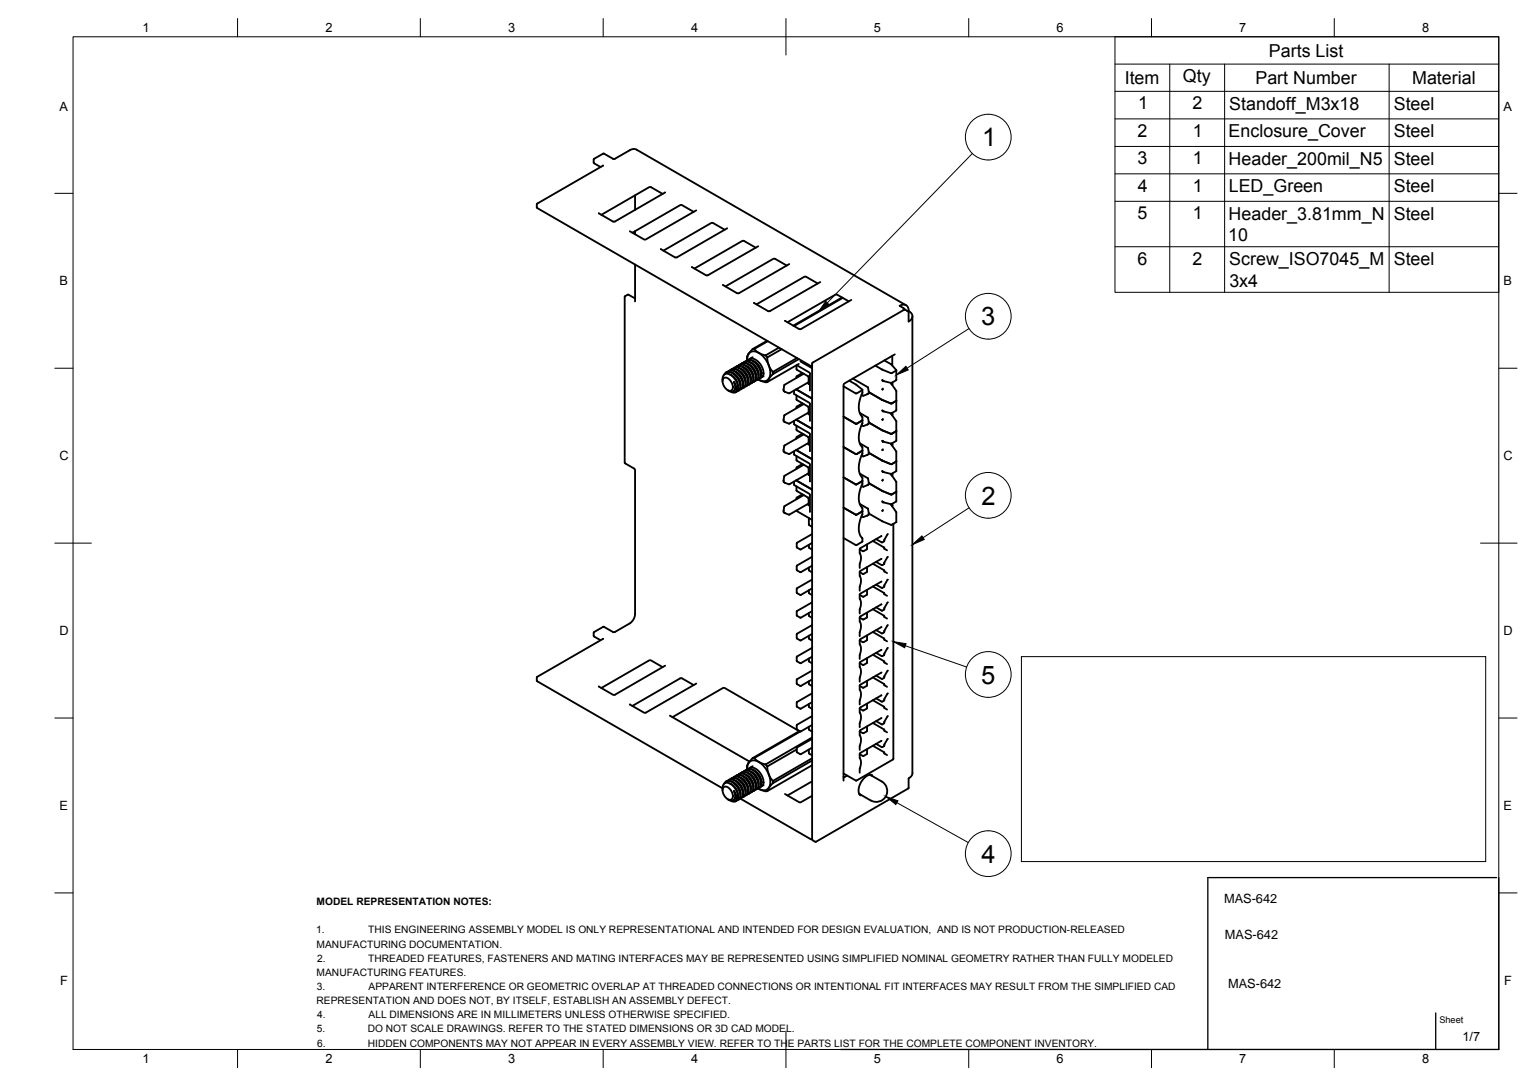
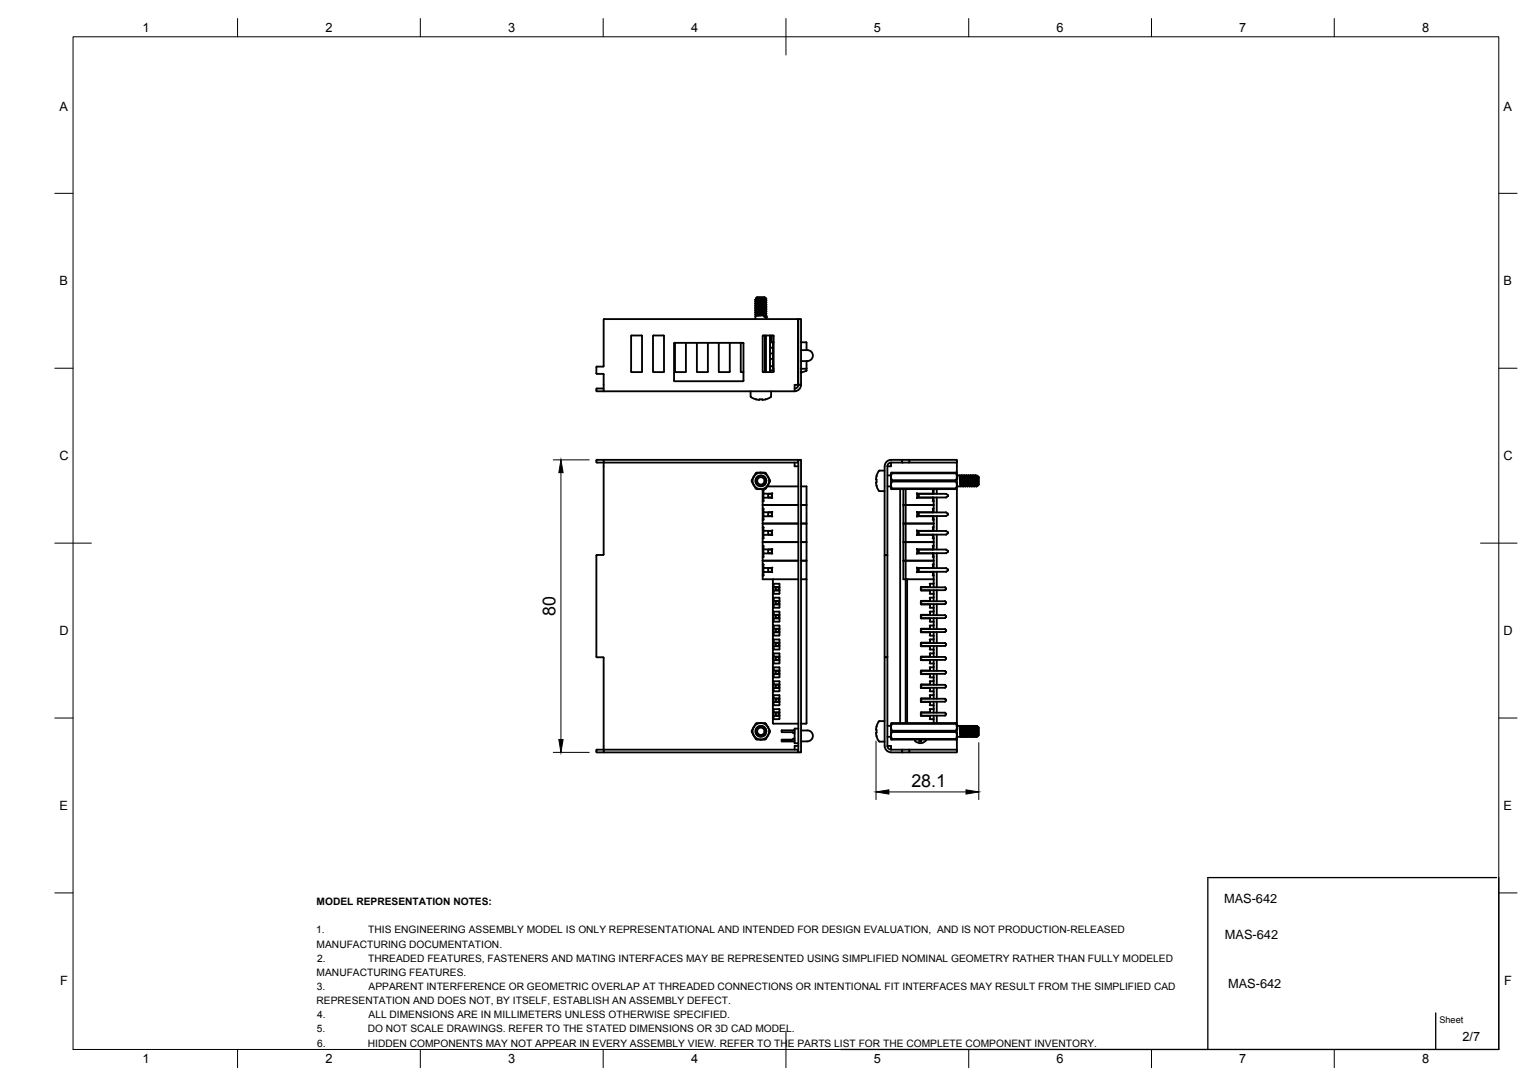
ISO-10303-21;
HEADER;
FILE_DESCRIPTION((''),'2;1');
FILE_NAME('MAS-642','2026-10-09T09:51:33-07:00',(''),(''),'','','');
FILE_SCHEMA (('AUTOMOTIVE_DESIGN { 1 0 10303 214 3 1 1 }'));
ENDSEC;
DATA;
#10 = MECHANICAL_DESIGN_GEOMETRIC_PRESENTATION_REPRESENTATION('',(#481,#482,
#483,#484,#485,#486,#487,#488,#489,#490,#491,#492,#493,#494,#495,#496,#497,
#498,#499,#500,#501,#502,#503,#504,#505,#506,#507,#508,#509,#510,#511,#512,
#513,#514,#515,#516,#517,#518,#519,#520,#521,#522,#523,#524,#525,#526,#527,
#528,#529,#530,#531,#532,#533,#534,#535,#536,#537,#538,#539,#540,#541,#542,
#543,#544,#545,#546,#547,#548,#549,#550,#551,#552,#553,#554,#555,#556,#557,
#558,#559,#560,#561,#562,#563,#564,#565,#566,#567,#568,#569,#570,#571,#572,
#573,#574,#575,#576,#577,#578,#579,#580,#581,#582,#583,#584,#585,#586,#587,
#588,#589,#590,#591,#592,#593,#594,#595,#596,#597,#598,#599,#600,#601,#602,
#603,#604,#605,#606,#607,#608,#609,#610,#611,#612,#613,#614,#615,#616,#617,
#618,#619,#620,#621,#622,#623,#624,#625,#626,#627,#628,#629,#630,#631,#632,
#633,#634,#635,#636,#637,#638,#639,#640,#641,#642,#643,#644,#645,#646,#647,
#648,#649,#650,#651,#652,#653,#654,#655,#656,#657,#658,#659,#660,#661,#662,
#663,#664,#665,#666,#667,#668,#669,#670,#671,#672,#673,#674,#675,#676,#677,
#678,#679,#680,#681,#682,#683,#684,#685,#686,#687,#688,#689,#690,#691,#692,
#693,#694,#695,#696,#697,#698,#699,#700,#701,#702,#703,#704,#705,#706,#707,
#708,#709,#710,#711,#712,#713,#714,#715,#716,#717,#718,#719,#720,#721,#722,
#723,#724,#725,#726,#727,#728,#729,#730,#731,#732,#733,#734,#735,#736,#737,
#738,#739,#740,#741,#742,#743,#744,#745,#746,#747,#748,#749,#750,#751,#752,
#753,#754,#755,#756,#757,#758,#759,#760,#761,#762,#763,#764,#765,#766,#767,
#768,#769,#770,#771,#772,#773,#774,#775,#776,#777,#778,#779,#780,#781,#782,
#783,#784,#785,#786,#787,#788,#789,#790,#791,#792,#793,#794,#795,#796,#797,
#798,#799,#800,#801,#802,#803,#804,#805,#806,#807,#808,#809,#810,#811,#812,
#813,#814,#815,#816,#817,#818,#819,#820,#821,#822,#823,#824,#825,#826,#827,
#828,#829,#830,#831,#832,#833,#834,#835,#836,#837,#838,#839,#840,#841,#842,
#843,#844,#845,#846,#847,#848,#849,#850,#851,#852,#853,#854,#855,#856,#857,
#858,#859,#860,#861,#862,#863,#864,#865,#866,#867,#868,#869,#870,#871,#872,
#873,#874,#875,#876,#877,#878,#879,#880,#881,#882,#883,#884,#885,#886,#887,
#888,#889,#890,#891,#892,#893,#894,#895,#896,#897,#898,#899,#900,#901,#902,
#903,#904,#905,#906,#907,#908,#909,#910,#911,#912,#913,#914,#915,#916,#917,
#918,#919,#920,#921,#922,#923,#924,#925,#926,#927,#928,#929,#930,#931,#932,
#933,#934,#935,#936,#937,#938,#939,#940,#941,#942,#943,#944,#945,#946,#947,
#948,#949,#950,#951,#952,#953,#954,#955,#956,#957,#958,#959,#960,#961,#962,
#963,#964,#965,#966,#967,#968,#969,#970,#971,#972,#973,#974,#975,#976,#977,
#978,#979,#980,#981,#982,#983,#984,#985,#986,#987,#988,#989,#990,#991,#992,
#993,#994,#995,#996,#997,#998,#999,#1000,#1001,#1002,#1003,#1004,#1005,
#1006,#1007,#1008,#1009,#1010,#1011,#1012,#1013,#1014,#1015,#1016,#1017,
#1018,#1019,#1020,#1021,#1022,#1023,#1024,#1025,#1026,#1027,#1028,#1029,
#1030,#1031,#1032,#1033,#1034,#1035,#1036,#1037,#1038,#1039,#1040,#1041,
#1042,#1043,#1044,#1045,#1046,#1047,#1048,#1049,#1050,#1051,#1052,#1053,
#1054,#1055,#1056,#1057,#1058,#1059,#1060,#1061,#1062,#1063,#1064,#1065,
#1066,#1067,#1068,#1069,#1070,#1071,#1072,#1073,#1074,#1075,#1076,#1077,
#1078,#1079,#1080,#1081,#1082,#1083,#1084,#1085,#1086,#1087,#1088,#1089,
#1090,#1091,#1092,#1093,#1094,#1095,#1096,#1097,#1098,#1099,#1100,#1101,
#1102,#1103,#1104,#1105,#1106,#1107,#1108,#1109,#1110,#1111,#1112,#1113,
#1114,#1115,#1116,#1117,#1118,#1119,#1120,#1121,#1122,#1123,#1124,#1125,
#1126,#1127,#1128,#1129,#1130,#1131,#1132,#1133,#1134,#1135,#1136,#1137,
#1138,#1139,#1140,#1141,#1142,#1143,#1144,#1145,#1146,#1147,#1148,#1149,
#1150,#1151,#1152,#1153,#1154,#1155,#1156,#1157,#1158,#1159,#1160,#1161,
#1162,#1163,#1164,#1165,#1166,#1167,#1168,#1169,#1170,#1171,#1172,#1173,
#1174,#1175,#1176,#1177,#1178,#1179,#1180,#1181,#1182,#1183,#1184,#1185,
#1186,#1187,#1188,#1189,#1190,#1191,#1192,#1193,#1194,#1195,#1196,#1197,
#1198,#1199,#1200,#1201,#1202,#1203,#1204,#1205,#1206,#1207,#1208,#1209,
#1210,#1211,#1212,#1213,#1214,#1215,#1216,#1217,#1218,#1219,#1220,#1221,
#1222,#1223,#1224,#1225,#1226,#1227,#1228,#1229,#1230,#1231,#1232,#1233,
#1234,#1235,#1236,#1237,#1238,#1239,#1240,#1241,#1242,#1243,#1244,#1245,
#1246,#1247,#1248,#1249,#1250,#1251,#1252,#1253,#1254,#1255,#1256,#1257,
#1258,#1259,#1260,#1261,#1262,#1263,#1264,#1265,#1266,#1267,#1268,#1269,
#1270,#1271,#1272,#1273,#1274,#1275,#1276,#1277,#1278,#1279,#1280,#1281,
#1282,#1283,#1284,#1285,#1286,#1287,#1288,#1289,#1290,#1291,#1292,#1293,
#1294,#1295,#1296,#1297,#1298,#1299,#1300,#1301,#1302,#1303,#1304,#1305,
#1306,#1307,#1308,#1309,#1310,#1311,#1312,#1313,#1314,#1315,#1316,#1317,
#1318,#1319,#1320,#1321,#1322,#1323,#1324,#1325,#1326,#1327,#1328,#1329,
#1330,#1331,#1332,#1333,#1334,#1335,#1336,#1337,#1338,#1339,#1340,#1341,
#1342,#1343,#1344,#1345,#1346,#1347,#1348,#1349,#1350,#1351,#1352,#1353,
#1354,#1355,#1356,#1357,#1358,#1359,#1360,#1361,#1362,#1363,#1364,#1365,
#1366,#1367,#1368,#1369,#1370,#1371,#1372,#1373,#1374,#1375,#1376,#1377,
#1378,#1379,#1380,#1381,#1382,#1383,#1384,#1385,#1386,#1387,#1388,#1389,
#1390,#1391,#1392,#1393,#1394,#1395,#1396,#1397,#1398,#1399,#1400,#1401,
#1402,#1403,#1404,#1405,#1406,#1407,#1408,#1409,#1410,#1411,#1412,#1413,
#1414,#1415,#1416,#1417,#1418,#1419,#1420,#1421,#1422,#1423,#1424,#1425,
#1426,#1427,#1428,#1429,#1430,#1431,#1432,#1433,#1434,#1435,#1436,#1437,
#1438,#1439,#1440,#1441,#1442,#1443,#1444,#1445,#1446,#1447,#1448,#1449,
#1450,#1451,#1452,#1453,#1454,#1455,#1456,#1457,#1458,#1459,#1460,#1461,
#1462,#1463,#1464,#1465,#1466,#1467,#1468,#1469,#1470,#1471,#1472,#1473,
#1474,#1475,#1476,#1477,#1478,#1479,#1480,#1481,#1482,#1483,#1484,#1485,
#1486,#1487,#1488,#1489,#1490,#1491,#1492,#1493,#1494,#1495,#1496,#1497,
#1498,#1499,#1500,#1501,#1502,#1503,#1504,#1505,#1506,#1507,#1508,#1509,
#1510,#1511,#1512,#1513,#1514,#1515,#1516,#1517,#1518,#1519,#1520,#1521,
#1522,#1523,#1524,#1525,#1526,#1527,#1528,#1529,#1530,#1531,#1532,#1533,
#1534,#1535,#1536,#1537,#1538,#1539,#1540,#1541,#1542,#1543,#1544,#1545,
#1546,#1547,#1548,#1549,#1550,#1551,#1552,#1553,#1554,#1555,#1556,#1557,
#1558,#1559,#1560,#1561,#1562,#1563,#1564,#1565,#1566,#1567,#1568,#1569,
#1570,#1571,#1572,#1573,#1574,#1575,#1576,#1577,#1578,#1579,#1580,#1581,
#1582,#1583,#1584,#1585,#1586,#1587,#1588,#1589,#1590,#1591,#1592,#1593,
#1594,#1595,#1596,#1597,#1598,#1599,#1600,#1601,#1602,#1603,#1604,#1605,
#1606,#1607,#1608,#1609,#1610,#1611,#1612,#1613,#1614,#1615,#1616,#1617,
#1618,#1619,#1620,#1621,#1622,#1623,#1624,#1625,#1626,#1627,#1628,#1629,
#1630,#1631,#1632,#1633,#1634,#1635,#1636,#1637,#1638,#1639,#1640,#1641,
#1642,#1643,#1644,#1645,#1646,#1647,#1648,#1649,#1650,#1651,#1652,#1653,
#1654,#1655,#1656,#1657,#1658,#1659,#1660,#1661,#1662,#1663,#1664,#1665,
#1666,#1667,#1668,#1669,#1670,#1671,#1672,#1673,#1674,#1675,#1676,#1677,
#1678,#1679,#1680,#1681,#1682,#1683,#1684,#1685,#1686,#1687,#1688,#1689,
#1690,#1691,#1692,#1693,#1694,#1695,#1696,#1697,#1698,#1699,#1700,#1701,
#1702,#1703,#1704,#1705,#1706,#1707,#1708,#1709,#1710,#1711,#1712,#1713,
#1714,#1715,#1716,#1717,#1718,#1719,#1720,#1721,#1722,#1723,#1724,#1725,
#1726,#1727,#1728,#1729,#1730,#1731,#1732,#1733,#1734,#1735,#1736,#1737,
#1738,#1739,#1740,#1741,#1742,#1743,#1744,#1745,#1746,#1747,#1748,#1749,
#1750,#1751,#1752,#1753,#1754,#1755,#1756,#1757,#1758,#1759,#1760,#1761,
#1762,#1763,#1764,#1765,#1766,#1767,#1768,#1769,#1770,#1771,#1772,#1773,
#1774,#1775,#1776,#1777,#1778,#1779,#1780,#1781,#1782,#1783,#1784,#1785,
#1786,#1787,#1788,#1789,#1790,#1791,#1792,#1793,#1794,#1795,#1796,#1797,
#1798,#1799,#1800,#1801,#1802,#1803,#1804,#1805,#1806,#1807,#1808,#1809,
#1810,#1811,#1812,#1813,#1814,#1815,#1816,#1817,#1818,#1819,#1820,#1821,
#1822,#1823,#1824,#1825,#1826,#1827,#1828,#1829,#1830,#1831,#1832,#1833,
#1834,#1835,#1836,#1837,#1838,#1839,#1840,#1841,#1842,#1843,#1844,#1845,
#1846,#1847,#1848,#1849,#1850,#1851,#1852,#1853,#1854,#1855,#1856,#1857,
#1858,#1859,#1860,#1861,#1862,#1863,#1864,#1865,#1866,#1867,#1868,#1869,
#1870,#1871,#1872,#1873,#1874,#1875,#1876,#1877,#1878,#1879,#1880,#1881,
#1882,#1883,#1884,#1885,#1886,#1887,#1888,#1889,#1890,#1891,#1892,#1893,
#1894,#1895,#1896,#1897,#1898,#1899,#1900,#1901,#1902,#1903,#1904,#1905,
#1906,#1907,#1908,#1909,#1910,#1911,#1912,#1913,#1914,#1915,#1916,#1917,
#1918,#1919,#1920,#1921,#1922,#1923,#1924,#1925,#1926,#1927,#1928,#1929,
#1930,#1931,#1932,#1933,#1934,#1935,#1936,#1937,#1938,#1939,#1940,#1941,
#1942,#1943,#1944,#1945,#1946,#1947,#1948,#1949,#1950,#1951,#1952,#1953,
#1954,#1955,#1956,#1957,#1958,#1959,#1960,#1961,#1962,#1963,#1964,#1965,
#1966,#1967,#1968,#1969,#1970,#1971,#1972,#1973,#1974,#1975,#1976,#1977,
#1978,#1979,#1980,#1981,#1982,#1983,#1984,#1985,#1986,#1987,#1988,#1989,
#1990,#1991,#1992,#1993,#1994,#1995,#1996,#1997,#1998,#1999,#2000,#2001,
#2002,#2003,#2004,#2005,#2006,#2007,#2008,#2009,#2010,#2011,#2012,#2013,
#2014,#2015,#2016,#2017,#2018,#2019,#2020,#2021,#2022,#2023,#2024,#2025,
#2026,#2027,#2028,#2029,#2030,#2031,#2032,#2033,#2034,#2035,#2036,#2037,
#2038,#2039,#2040,#2041,#2042,#2043,#2044,#2045,#2046,#2047,#2048,#2049,
#2050,#2051,#2052,#2053,#2054,#2055,#2056,#2057,#2058,#2059,#2060,#2061,
#2062,#2063,#2064,#2065,#2066,#2067,#2068,#2069,#2070,#2071,#2072,#2073,
#2074,#2075,#2076,#2077,#2078,#2079,#2080,#2081,#2082,#2083,#2084,#2085,
#2086,#2087,#2088,#2089,#2090,#2091,#2092,#2093,#2094,#2095,#2096,#2097,
#2098,#2099,#2100,#2101,#2102,#2103,#2104,#2105,#2106,#2107,#2108,#2109,
#2110,#2111,#2112,#2113,#2114,#2115,#2116,#2117,#2118,#2119,#2120,#2121,
#2122,#2123,#2124,#2125,#2126,#2127,#2128,#2129,#2130,#2131,#2132,#2133,
#2134,#2135,#2136,#2137,#2138,#2139,#2140,#2141,#2142,#2143,#2144,#2145,
#2146,#2147,#2148,#2149,#2150,#2151,#2152,#2153,#2154,#2155,#2156,#2157,
#2158,#2159,#2160,#2161,#2162,#2163,#2164,#2165,#2166,#2167,#2168,#2169,
#2170,#2171,#2172,#2173,#2174,#2175,#2176,#2177,#2178,#2179,#2180,#2181,
#2182,#2183,#2184,#2185,#2186,#2187,#2188,#2189,#2190,#2191,#2192,#2193,
#2194,#2195,#2196,#2197,#2198,#2199,#2200,#2201,#2202,#2203,#2204,#2205,
#2206,#2207,#2208,#2209,#2210,#2211,#2212,#2213,#2214,#2215,#2216,#2217,
#2218,#2219,#2220,#2221,#2222,#2223,#2224,#2225,#2226,#2227,#2228,#2229,
#2230,#2231,#2232,#2233,#2234,#2235,#2236,#2237,#2238,#2239,#2240,#2241,
#2242,#2243,#2244,#2245,#2246,#2247,#2248,#2249,#2250,#2251,#2252,#2253,
#2254,#2255,#2256,#2257,#2258,#2259,#2260,#2261,#2262,#2263,#2264,#2265,
#2266,#2267,#2268,#2269,#2270,#2271,#2272,#2273,#2274,#2275,#2276,#2277,
#2278,#2279,#2280,#2281,#2282,#2283,#2284,#2285,#2286,#2287,#2288,#2289,
#2290,#2291,#2292,#2293,#2294,#2295,#2296,#2297,#2298,#2299,#2300,#2301,
#2302,#2303,#2304,#2305,#2306,#2307,#2308,#2309,#2310,#2311,#2312,#2313,
#2314,#2315,#2316,#2317,#2318,#2319,#2320,#2321,#2322,#2323,#2324,#2325,
#2326,#2327,#2328,#2329,#2330,#2331,#2332,#2333,#2334,#2335,#2336,#2337,
#2338,#2339,#2340,#2341,#2342,#2343,#2344,#2345,#2346,#2347,#2348,#2349,
#2350,#2351,#2352,#2353,#2354,#2355,#2356,#2357,#2358,#2359,#2360,#2361,
#2362,#2363,#2364,#2365,#2366,#2367,#2368,#2369,#2370,#2371,#2372,#2373,
#2374,#2375,#2376,#2377,#2378,#2379,#2380,#2381,#2382,#2383,#2384,#2385,
#2386,#2387,#2388,#2389,#2390,#2391,#2392,#2393,#2394,#2395,#2396,#2397,
#2398,#2399,#2400,#2401,#2402,#2403,#2404,#2405,#2406,#2407,#2408,#2409,
#2410,#2411,#2412,#2413,#2414,#2415,#2416,#2417,#2418,#2419,#2420,#2421,
#2422,#2423,#2424,#2425,#2426,#2427,#2428,#2429,#2430,#2431,#2432,#2433,
#2434,#2435,#2436,#2437,#2438,#2439,#2440,#2441,#2442,#2443,#2444,#2445,
#2446,#2447,#2448,#2449,#2450,#2451,#2452,#2453,#2454,#2455,#2456,#2457,
#2458,#2459,#2460,#2461,#2462,#2463,#2464,#2465,#2466,#2467,#2468,#2469,
#2470,#2471,#2472,#2473,#2474,#2475,#2476,#2477,#2478,#2479,#2480,#2481,
#2482,#2483,#2484,#2485,#2486,#2487,#2488,#2489,#2490,#2491,#2492,#2493,
#2494,#2495,#2496,#2497,#2498,#2499,#2500,#2501,#2502,#2503,#2504,#2505,
#2506,#2507,#2508,#2509,#2510,#2511,#2512,#2513,#2514,#2515,#2516,#2517,
#2518,#2519,#2520,#2521,#2522,#2523,#2524,#2525,#2526,#2527,#2528,#2529,
#2530,#2531,#2532,#2533,#2534,#2535,#2536,#2537,#2538,#2539,#2540,#2541,
#2542,#2543,#2544,#2545,#2546,#2547,#2548,#2549,#2550,#2551,#2552,#2553,
#2554,#2555,#2556,#2557,#2558,#2559,#2560,#2561,#2562,#2563,#2564,#2565,
#2566,#2567,#2568,#2569,#2570,#2571,#2572,#2573,#2574,#2575,#2576,#2577,
#2578,#2579,#2580,#2581,#2582,#2583,#2584,#2585,#2586,#2587,#2588,#2589,
#2590,#2591,#2592,#2593,#2594,#2595,#2596,#2597,#2598,#2599,#2600,#2601,
#2602,#2603,#2604,#2605,#2606,#2607,#2608,#2609,#2610,#2611,#2612,#2613,
#2614,#2615,#2616,#2617,#2618,#2619,#2620,#2621,#2622,#2623,#2624,#2625,
#2626,#2627,#2628,#2629,#2630,#2631,#2632,#2633,#2634,#2635,#2636,#2637,
#2638,#2639,#2640,#2641,#2642,#2643,#2644,#2645,#2646,#2647,#2648,#2649,
#2650,#2651,#2652,#2653,#2654,#2655,#2656,#2657,#2658,#2659,#2660,#2661,
#2662,#2663,#2664,#2665,#2666,#2667,#2668,#2669,#2670,#2671,#2672,#2673,
#2674,#2675,#2676,#2677,#2678,#2679,#2680,#2681,#2682,#2683,#2684,#2685,
#2686,#2687,#2688,#2689,#2690,#2691,#2692,#2693,#2694,#2695,#2696,#2697,
#2698,#2699,#2700,#2701,#2702,#2703,#2704,#2705,#2706,#2707,#2708,#2709,
#2710,#2711,#2712,#2713,#2714,#2715,#2716,#2717,#2718,#2719,#2720,#2721,
#2722,#2723,#2724,#2725,#2726,#2727,#2728,#2729,#2730,#2731,#2732,#2733,
#2734,#2735,#2736,#2737,#2738,#2739,#2740,#2741,#2742,#2743,#2744,#2745,
#2746,#2747,#2748,#2749,#2750,#2751,#2752,#2753,#2754,#2755,#2756,#2757,
#2758,#2759,#2760,#2761,#2762,#2763,#2764,#2765,#2766,#2767,#2768,#2769,
#2770,#2771,#2772,#2773,#2774,#2775,#2776,#2777,#2778,#2779,#2780,#2781,
#2782,#2783,#2784,#2785,#2786,#2787,#2788,#2789,#2790,#2791,#2792,#2793,
#2794,#2795,#2796,#2797,#2798,#2799,#2800,#2801,#2802,#2803,#2804,#2805,
#2806,#2807,#2808,#2809,#2810,#2811,#2812,#2813,#2814,#2815,#2816,#2817,
#2818,#2819,#2820,#2821,#2822,#2823,#2824,#2825,#2826,#2827,#2828,#2829,
#2830,#2831,#2832,#2833,#2834,#2835,#2836,#2837,#2838,#2839,#2840,#2841,
#2842,#2843,#2844,#2845,#2846,#2847,#2848,#2849,#2850,#2851,#2852,#2853,
#2854,#2855,#2856,#2857,#2858,#2859,#2860,#2861,#2862,#2863,#2864,#2865,
#2866,#2867,#2868,#2869,#2870,#2871,#2872,#2873,#2874,#2875,#2876,#2877,
#2878,#2879,#2880,#2881,#2882,#2883,#2884,#2885,#2886,#2887,#2888,#2889,
#2890,#2891,#2892,#2893,#2894,#2895,#2896,#2897,#2898,#2899,#2900,#2901,
#2902,#2903,#2904,#2905,#2906,#2907,#2908,#2909,#2910,#2911,#2912,#2913,
#2914,#2915,#2916,#2917,#2918,#2919,#2920,#2921,#2922,#2923,#2924,#2925,
#2926,#2927,#2928,#2929,#2930,#2931,#2932,#2933,#2934,#2935,#2936,#2937,
#2938,#2939,#2940,#2941,#2942,#2943,#2944,#2945,#2946,#2947,#2948,#2949,
#2950,#2951,#2952,#2953,#2954,#2955,#2956,#2957,#2958,#2959,#2960,#2961,
#2962,#2963,#2964,#2965,#2966,#2967,#2968,#2969,#2970,#2971,#2972,#2973,
#2974,#2975,#2976,#2977,#2978,#2979,#2980,#2981,#2982,#2983,#2984,#2985,
#2986,#2987,#2988,#2989,#2990,#2991,#2992,#2993,#2994,#2995,#2996,#2997,
#2998,#2999,#3000,#3001,#3002,#3003,#3004,#3005,#3006,#3007,#3008,#3009,
#3010,#3011,#3012,#3013,#3014,#3015,#3016,#3017,#3018,#3019,#3020,#3021,
#3022,#3023,#3024,#3025,#3026,#3027,#3028,#3029,#3030,#3031,#3032,#3033,
#3034,#3035,#3036,#3037,#3038,#3039,#3040,#3041,#3042,#3043,#3044,#3045,
#3046,#3047,#3048,#3049,#3050,#3051,#3052,#3053,#3054,#3055,#3056,#3057,
#3058,#3059,#3060,#3061,#3062,#3063,#3064,#3065,#3066,#3067,#3068,#3069,
#3070,#3071,#3072,#3073,#3074,#3075,#3076,#3077,#3078,#3079,#3080,#3081,
#3082,#3083,#3084,#3085,#3086,#3087,#3088,#3089,#3090,#3091,#3092,#3093,
#3094,#3095,#3096,#3097,#3098,#3099,#3100,#3101,#3102,#3103,#3104,#3105,
#3106,#3107,#3108,#3109,#3110,#3111,#3112,#3113,#3114,#3115,#3116,#3117,
#3118,#3119,#3120,#3121,#3122,#3123,#3124,#3125,#3126,#3127,#3128,#3129,
#3130,#3131,#3132,#3133,#3134,#3135,#3136,#3137,#3138,#3139,#3140,#3141,
#3142,#3143,#3144,#3145,#3146,#3147,#3148,#3149,#3150,#3151,#3152,#3153,
#3154,#3155,#3156,#3157,#3158,#3159,#3160,#3161,#3162,#3163,#3164,#3165,
#3166,#3167,#3168,#3169,#3170,#3171,#3172,#3173,#3174,#3175,#3176,#3177,
#3178,#3179,#3180,#3181,#3182,#3183,#3184,#3185,#3186,#3187,#3188,#3189,
#3190,#3191,#3192,#3193,#3194,#3195,#3196,#3197,#3198,#3199,#3200,#3201,
#3202,#3203,#3204,#3205,#3206,#3207,#3208,#3209,#3210,#3211,#3212,#3213,
#3214,#3215,#3216,#3217,#3218,#3219,#3220,#3221,#3222,#3223,#3224,#3225,
#3226,#3227,#3228,#3229,#3230,#3231,#3232,#3233,#3234,#3235,#3236,#3237,
#3238,#3239,#3240,#3241,#3242,#3243,#3244,#3245,#3246,#3247,#3248,#3249,
#3250,#3251,#3252,#3253,#3254,#3255,#3256,#3257,#3258,#3259,#3260,#3261,
#3262,#3263,#3264,#3265,#3266,#3267,#3268,#3269,#3270,#3271,#3272,#3273,
#3274,#3275,#3276,#3277,#3278,#3279,#3280,#3281,#3282,#3283,#3284,#3285,
#3286,#3287,#3288,#3289,#3290,#3291,#3292,#3293,#3294,#3295,#3296,#3297,
#3298,#3299,#3300,#3301,#3302,#3303,#3304,#3305,#3306,#3307,#3308,#3309,
#3310,#3311,#3312,#3313,#3314,#3315,#3316,#3317,#3318,#3319,#3320,#3321,
#3322,#3323,#3324,#3325,#3326,#3327,#3328,#3329,#3330,#3331,#3332,#3333,
#3334,#3335,#3336,#3337,#3338,#3339,#3340,#3341,#3342,#3343,#3344,#3345,
#3346,#3347,#3348,#3349,#3350,#3351,#3352,#3353,#3354,#3355,#3356,#3357,
#3358,#3359,#3360,#3361,#3362,#3363,#3364,#3365,#3366,#3367,#3368,#3369,
#3370,#3371,#3372,#3373,#3374,#3375,#3376,#3377,#3378,#3379,#3380,#3381,
#3382,#3383,#3384,#3385,#3386,#3387,#3388,#3389,#3390,#3391,#3392,#3393,
#3394,#3395,#3396,#3397,#3398,#3399,#3400,#3401,#3402,#3403,#3404,#3405,
#3406,#3407,#3408,#3409,#3410,#3411,#3412,#3413,#3414,#3415,#3416,#3417,
#3418,#3419,#3420,#3421,#3422,#3423,#3424,#3425,#3426,#3427,#3428,#3429,
#3430,#3431,#3432,#3433,#3434,#3435,#3436,#3437,#3438,#3439,#3440,#3441,
#3442,#3443,#3444,#3445,#3446,#3447,#3448,#3449,#3450,#3451,#3452,#3453,
#3454,#3455,#3456,#3457,#3458,#3459,#3460,#3461,#3462,#3463,#3464,#3465,
#3466,#3467,#3468,#3469,#3470,#3471,#3472,#3473,#3474,#3475,#3476,#3477,
#3478,#3479,#3480,#3481,#3482,#3483,#3484,#3485,#3486,#3487,#3488,#3489,
#3490,#3491,#3492,#3493,#3494,#3495,#3496,#3497,#3498,#3499,#3500,#3501,
#3502,#3503,#3504,#3505,#3506,#3507,#3508,#3509,#3510,#3511,#3512,#3513,
#3514,#3515,#3516,#3517,#3518,#3519,#3520,#3521,#3522,#3523,#3524,#3525,
#3526,#3527,#3528,#3529,#3530,#3531,#3532,#3533,#3534,#3535,#3536,#3537,
#3538,#3539,#3540,#3541,#3542,#3543,#3544,#3545,#3546,#3547,#3548,#3549,
#3550,#3551,#3552,#3553,#3554,#3555,#3556,#3557,#3558,#3559,#3560,#3561,
#3562,#3563,#3564,#3565,#3566,#3567,#3568,#3569,#3570,#3571,#3572,#3573,
#3574,#3575,#3576,#3577,#3578,#3579,#3580,#3581,#3582,#3583,#3584,#3585,
#3586,#3587,#3588,#3589,#3590,#3591,#3592,#3593,#3594,#3595,#3596,#3597,
#3598,#3599,#3600,#3601,#3602,#3603,#3604,#3605,#3606,#3607,#3608,#3609,
#3610,#3611,#3612,#3613,#3614,#3615,#3616,#3617,#3618,#3619,#3620,#3621,
#3622,#3623,#3624,#3625,#3626,#3627,#3628,#3629,#3630,#3631,#3632,#3633,
#3634,#3635,#3636,#3637,#3638,#3639,#3640,#3641,#3642,#3643,#3644,#3645,
#3646,#3647,#3648,#3649,#3650,#3651,#3652,#3653,#3654,#3655,#3656,#3657,
#3658,#3659,#3660,#3661,#3662,#3663,#3664,#3665,#3666,#3667,#3668,#3669,
#3670,#3671,#3672,#3673,#3674,#3675,#3676,#3677,#3678,#3679,#3680,#3681,
#3682,#3683,#3684,#3685,#3686,#3687,#3688,#3689,#3690,#3691,#3692,#3693,
#3694,#3695,#3696,#3697,#3698,#3699,#3700,#3701,#3702,#3703,#3704,#3705,
#3706,#3707,#3708,#3709,#3710,#3711,#3712,#3713,#3714,#3715,#3716,#3717,
#3718,#3719,#3720,#3721,#3722,#3723,#3724,#3725,#3726,#3727,#3728,#3729,
#3730,#3731,#3732,#3733,#3734,#3735,#3736,#3737,#3738,#3739,#3740,#3741,
#3742,#3743,#3744,#3745,#3746,#3747,#3748,#3749,#3750,#3751,#3752,#3753,
#3754,#3755,#3756,#3757,#3758,#3759,#3760,#3761,#3762,#3763,#3764,#3765,
#3766,#3767,#3768,#3769,#3770,#3771,#3772,#3773,#3774,#3775,#3776,#3777,
#3778,#3779,#3780,#3781,#3782,#3783,#3784,#3785,#3786,#3787,#3788,#3789,
#3790,#3791,#3792,#3793,#3794,#3795,#3796,#3797,#3798,#3799,#3800,#3801,
#3802,#3803,#3804,#3805,#3806,#3807,#3808,#3809,#3810,#3811,#3812,#3813,
#3814,#3815,#3816,#3817,#3818,#3819,#3820,#3821,#3822,#3823,#3824,#3825,
#3826,#3827,#3828,#3829,#3830,#3831,#3832,#3833,#3834,#3835,#3836,#3837,
#3838,#3839,#3840,#3841,#3842,#3843,#3844,#3845,#3846,#3847,#3848,#3849,
#3850,#3851,#3852,#3853,#3854,#3855,#3856,#3857,#3858,#3859,#3860,#3861,
#3862,#3863,#3864,#3865,#3866,#3867,#3868,#3869,#3870,#3871,#3872,#3873,
#3874,#3875,#3876,#3877,#3878,#3879,#3880,#3881,#3882,#3883,#3884,#3885,
#3886,#3887,#3888,#3889,#3890,#3891,#3892,#3893,#3894,#3895,#3896,#3897,
#3898,#3899,#3900,#3901,#3902,#3903,#3904,#3905,#3906,#3907,#3908,#3909,
#3910,#3911,#3912,#3913,#3914,#3915,#3916,#3917,#3918,#3919,#3920,#3921,
#3922,#3923,#3924,#3925,#3926,#3927,#3928,#3929,#3930,#3931,#3932,#3933,
#3934,#3935,#3936,#3937,#3938,#3939,#3940,#3941,#3942,#3943,#3944,#3945,
#3946,#3947,#3948,#3949,#3950,#3951,#3952,#3953,#3954,#3955,#3956,#3957,
#3958,#3959,#3960,#3961,#3962,#3963,#3964,#3965,#3966,#3967,#3968,#3969,
#3970,#3971,#3972,#3973,#3974,#3975,#3976,#3977,#3978,#3979,#3980,#3981,
#3982,#3983,#3984,#3985,#3986,#3987,#3988,#3989,#3990,#3991,#3992,#3993,
#3994,#3995,#3996,#3997,#3998,#3999,#4000,#4001,#4002,#4003,#4004,#4005,
#4006,#4007,#4008,#4009,#4010,#4011,#4012,#4013,#4014,#4015,#4016,#4017,
#4018,#4019,#4020,#4021,#4022,#4023,#4024,#4025,#4026,#4027,#4028,#4029,
#4030,#4031,#4032,#4033,#4034,#4035,#4036,#4037,#4038,#4039,#4040,#4041,
#4042,#4043,#4044,#4045,#4046,#4047,#4048,#4049,#4050,#4051,#4052,#4053,
#4054,#4055,#4056,#4057,#4058,#4059,#4060,#4061,#4062,#4063,#4064,#4065,
#4066,#4067,#4068,#4069,#4070,#4071,#4072,#4073,#4074,#4075,#4076,#4077,
#4078,#4079,#4080,#4081,#4082,#4083,#4084,#4085,#4086,#4087,#4088,#4089,
#4090,#4091,#4092,#4093,#4094,#4095,#4096,#4097,#4098,#4099,#4100,#4101,
#4102,#4103,#4104,#4105,#4106,#4107,#4108,#4109,#4110,#4111,#4112,#4113,
#4114,#4115,#4116,#4117,#4118,#4119,#4120,#4121,#4122,#4123,#4124,#4125,
#4126,#4127,#4128,#4129,#4130,#4131,#4132,#4133,#4134,#4135,#4136,#4137,
#4138,#4139,#4140,#4141,#4142,#4143,#4144,#4145,#4146,#4147,#4148,#4149,
#4150,#4151,#4152,#4153,#4154,#4155,#4156,#4157,#4158,#4159,#4160,#4161,
#4162,#4163,#4164,#4165,#4166,#4167,#4168,#4169,#4170,#4171),#126571) ;
#11 = ITEM_DEFINED_TRANSFORMATION($,$,#76669,#76844) ;
#12 = ITEM_DEFINED_TRANSFORMATION($,$,#67764,#76845) ;
#13 = ITEM_DEFINED_TRANSFORMATION($,$,#68778,#76846) ;
#14 = ITEM_DEFINED_TRANSFORMATION($,$,#71829,#76847) ;
#15 = ITEM_DEFINED_TRANSFORMATION($,$,#71866,#76848) ;
#16 = ITEM_DEFINED_TRANSFORMATION($,$,#76762,#76849) ;
#17 = ITEM_DEFINED_TRANSFORMATION($,$,#76669,#76850) ;
#18 = ITEM_DEFINED_TRANSFORMATION($,$,#76762,#76851) ;
#19 = (
REPRESENTATION_RELATIONSHIP($,$,#126603,#126598)
REPRESENTATION_RELATIONSHIP_WITH_TRANSFORMATION(#11)
SHAPE_REPRESENTATION_RELATIONSHIP()
) ;
#20 = (
REPRESENTATION_RELATIONSHIP($,$,#126599,#126598)
REPRESENTATION_RELATIONSHIP_WITH_TRANSFORMATION(#12)
SHAPE_REPRESENTATION_RELATIONSHIP()
) ;
#21 = (
REPRESENTATION_RELATIONSHIP($,$,#126600,#126598)
REPRESENTATION_RELATIONSHIP_WITH_TRANSFORMATION(#13)
SHAPE_REPRESENTATION_RELATIONSHIP()
) ;
#22 = (
REPRESENTATION_RELATIONSHIP($,$,#126601,#126598)
REPRESENTATION_RELATIONSHIP_WITH_TRANSFORMATION(#14)
SHAPE_REPRESENTATION_RELATIONSHIP()
) ;
#23 = (
REPRESENTATION_RELATIONSHIP($,$,#126602,#126598)
REPRESENTATION_RELATIONSHIP_WITH_TRANSFORMATION(#15)
SHAPE_REPRESENTATION_RELATIONSHIP()
) ;
#24 = (
REPRESENTATION_RELATIONSHIP($,$,#126604,#126598)
REPRESENTATION_RELATIONSHIP_WITH_TRANSFORMATION(#16)
SHAPE_REPRESENTATION_RELATIONSHIP()
) ;
#25 = (
REPRESENTATION_RELATIONSHIP($,$,#126603,#126598)
REPRESENTATION_RELATIONSHIP_WITH_TRANSFORMATION(#17)
SHAPE_REPRESENTATION_RELATIONSHIP()
) ;
#26 = (
REPRESENTATION_RELATIONSHIP($,$,#126604,#126598)
REPRESENTATION_RELATIONSHIP_WITH_TRANSFORMATION(#18)
SHAPE_REPRESENTATION_RELATIONSHIP()
) ;
#27 = CONTEXT_DEPENDENT_SHAPE_REPRESENTATION(#19,#126590) ;
#28 = CONTEXT_DEPENDENT_SHAPE_REPRESENTATION(#20,#126591) ;
#29 = CONTEXT_DEPENDENT_SHAPE_REPRESENTATION(#21,#126592) ;
#30 = CONTEXT_DEPENDENT_SHAPE_REPRESENTATION(#22,#126593) ;
#31 = CONTEXT_DEPENDENT_SHAPE_REPRESENTATION(#23,#126594) ;
#32 = CONTEXT_DEPENDENT_SHAPE_REPRESENTATION(#24,#126595) ;
#33 = CONTEXT_DEPENDENT_SHAPE_REPRESENTATION(#25,#126596) ;
#34 = CONTEXT_DEPENDENT_SHAPE_REPRESENTATION(#26,#126597) ;
#35 = NEXT_ASSEMBLY_USAGE_OCCURRENCE('Standoff_M3x18:1',
'Standoff_M3x18:1','Standoff_M3x18:1',#126606,#126611,
'Standoff_M3x18:1') ;
#36 = NEXT_ASSEMBLY_USAGE_OCCURRENCE('Enclosure_Cover:1',
'Enclosure_Cover:1','Enclosure_Cover:1',#126606,#126607,
'Enclosure_Cover:1') ;
#37 = NEXT_ASSEMBLY_USAGE_OCCURRENCE('Header_200mil_N5:1',
'Header_200mil_N5:1','Header_200mil_N5:1',#126606,#126608,
'Header_200mil_N5:1') ;
#38 = NEXT_ASSEMBLY_USAGE_OCCURRENCE('LED_Green:1','LED_Green:1',
'LED_Green:1',#126606,#126609,'LED_Green:1') ;
#39 = NEXT_ASSEMBLY_USAGE_OCCURRENCE('Header_3.81mm_N10:1',
'Header_3.81mm_N10:1','Header_3.81mm_N10:1',#126606,#126610,
'Header_3.81mm_N10:1') ;
#40 = NEXT_ASSEMBLY_USAGE_OCCURRENCE('Screw_ISO7045_M3x4:1',
'Screw_ISO7045_M3x4:1','Screw_ISO7045_M3x4:1',#126606,#126612,
'Screw_ISO7045_M3x4:1') ;
#41 = NEXT_ASSEMBLY_USAGE_OCCURRENCE('Standoff_M3x18:2',
'Standoff_M3x18:2','Standoff_M3x18:2',#126606,#126611,
'Standoff_M3x18:2') ;
#42 = NEXT_ASSEMBLY_USAGE_OCCURRENCE('Screw_ISO7045_M3x4:2',
'Screw_ISO7045_M3x4:2','Screw_ISO7045_M3x4:2',#126606,#126612,
'Screw_ISO7045_M3x4:2') ;
#43 = (
BOUNDED_CURVE()
B_SPLINE_CURVE(2,(#125694,#125695,#125696),.UNSPECIFIED.,.F.,.F.)
B_SPLINE_CURVE_WITH_KNOTS((3,3),(2.11928043164924,2.84165444767657),
 .UNSPECIFIED.)
CURVE()
GEOMETRIC_REPRESENTATION_ITEM()
RATIONAL_B_SPLINE_CURVE((4.94937295736919,5.22222222222224,5.22222222222224))
REPRESENTATION_ITEM('')
) ;
#44 = (
BOUNDED_CURVE()
B_SPLINE_CURVE(2,(#125699,#125700,#125701),.UNSPECIFIED.,.F.,.F.)
B_SPLINE_CURVE_WITH_KNOTS((3,3),(2.84165444767658,3.56402846370389),
 .UNSPECIFIED.)
CURVE()
GEOMETRIC_REPRESENTATION_ITEM()
RATIONAL_B_SPLINE_CURVE((5.22222222222221,5.22222222222221,4.94937295736917))
REPRESENTATION_ITEM('')
) ;
#45 = (
BOUNDED_CURVE()
B_SPLINE_CURVE(2,(#125705,#125706,#125707),.UNSPECIFIED.,.F.,.F.)
B_SPLINE_CURVE_WITH_KNOTS((3,3),(2.84165444767657,3.56402846370389),
 .UNSPECIFIED.)
CURVE()
GEOMETRIC_REPRESENTATION_ITEM()
RATIONAL_B_SPLINE_CURVE((5.22222222222224,5.22222222222224,4.9493729573692))
REPRESENTATION_ITEM('')
) ;
#46 = (
BOUNDED_CURVE()
B_SPLINE_CURVE(2,(#125708,#125709,#125710),.UNSPECIFIED.,.F.,.F.)
B_SPLINE_CURVE_WITH_KNOTS((3,3),(2.11928043164924,2.84165444767655),
 .UNSPECIFIED.)
CURVE()
GEOMETRIC_REPRESENTATION_ITEM()
RATIONAL_B_SPLINE_CURVE((4.94937295736915,5.22222222222219,5.22222222222219))
REPRESENTATION_ITEM('')
) ;
#47 = (
BOUNDED_CURVE()
B_SPLINE_CURVE(2,(#125714,#125715,#125716),.UNSPECIFIED.,.F.,.F.)
B_SPLINE_CURVE_WITH_KNOTS((3,3),(2.84165444767655,3.56402846370389),
 .UNSPECIFIED.)
CURVE()
GEOMETRIC_REPRESENTATION_ITEM()
RATIONAL_B_SPLINE_CURVE((5.22222222222219,5.22222222222219,4.94937295736914))
REPRESENTATION_ITEM('')
) ;
#48 = (
BOUNDED_CURVE()
B_SPLINE_CURVE(2,(#125717,#125718,#125719),.UNSPECIFIED.,.F.,.F.)
B_SPLINE_CURVE_WITH_KNOTS((3,3),(2.11928043164923,2.84165444767657),
 .UNSPECIFIED.)
CURVE()
GEOMETRIC_REPRESENTATION_ITEM()
RATIONAL_B_SPLINE_CURVE((4.94937295736919,5.22222222222224,5.22222222222224))
REPRESENTATION_ITEM('')
) ;
#49 = (
BOUNDED_CURVE()
B_SPLINE_CURVE(2,(#125723,#125724,#125725),.UNSPECIFIED.,.F.,.F.)
B_SPLINE_CURVE_WITH_KNOTS((3,3),(2.84165444767657,3.5640284637039),
 .UNSPECIFIED.)
CURVE()
GEOMETRIC_REPRESENTATION_ITEM()
RATIONAL_B_SPLINE_CURVE((5.22222222222224,5.22222222222224,4.94937295736919))
REPRESENTATION_ITEM('')
) ;
#50 = (
BOUNDED_CURVE()
B_SPLINE_CURVE(2,(#125726,#125727,#125728),.UNSPECIFIED.,.F.,.F.)
B_SPLINE_CURVE_WITH_KNOTS((3,3),(2.11928043164923,2.84165444767656),
 .UNSPECIFIED.)
CURVE()
GEOMETRIC_REPRESENTATION_ITEM()
RATIONAL_B_SPLINE_CURVE((4.9493729573692,5.22222222222225,5.22222222222225))
REPRESENTATION_ITEM('')
) ;
#51 = (
BOUNDED_CURVE()
B_SPLINE_CURVE(2,(#125732,#125733,#125734),.UNSPECIFIED.,.F.,.F.)
B_SPLINE_CURVE_WITH_KNOTS((3,3),(2.84165444767656,3.56402846370389),
 .UNSPECIFIED.)
CURVE()
GEOMETRIC_REPRESENTATION_ITEM()
RATIONAL_B_SPLINE_CURVE((5.22222222222225,5.22222222222225,4.94937295736921))
REPRESENTATION_ITEM('')
) ;
#52 = (
BOUNDED_CURVE()
B_SPLINE_CURVE(2,(#125735,#125736,#125737),.UNSPECIFIED.,.F.,.F.)
B_SPLINE_CURVE_WITH_KNOTS((3,3),(2.11928043164924,2.84165444767656),
 .UNSPECIFIED.)
CURVE()
GEOMETRIC_REPRESENTATION_ITEM()
RATIONAL_B_SPLINE_CURVE((4.94937295736916,5.2222222222222,5.2222222222222))
REPRESENTATION_ITEM('')
) ;
#53 = (
BOUNDED_CURVE()
B_SPLINE_CURVE(2,(#125740,#125741,#125742),.UNSPECIFIED.,.F.,.F.)
B_SPLINE_CURVE_WITH_KNOTS((3,3),(2.84165444767656,3.56402846370389),
 .UNSPECIFIED.)
CURVE()
GEOMETRIC_REPRESENTATION_ITEM()
RATIONAL_B_SPLINE_CURVE((5.2222222222222,5.2222222222222,4.94937295736915))
REPRESENTATION_ITEM('')
) ;
#54 = (
BOUNDED_CURVE()
B_SPLINE_CURVE(2,(#125743,#125744,#125745),.UNSPECIFIED.,.F.,.F.)
B_SPLINE_CURVE_WITH_KNOTS((3,3),(2.11928043164924,2.84165444767658),
 .UNSPECIFIED.)
CURVE()
GEOMETRIC_REPRESENTATION_ITEM()
RATIONAL_B_SPLINE_CURVE((4.94937295736917,5.22222222222221,5.22222222222221))
REPRESENTATION_ITEM('')
) ;
#55 = (
BOUNDED_CURVE()
B_SPLINE_CURVE(2,(#125748,#125749,#125750),.UNSPECIFIED.,.F.,.F.)
B_SPLINE_CURVE_WITH_KNOTS((3,3),(2.11928043164923,2.84165444767652),
 .UNSPECIFIED.)
CURVE()
GEOMETRIC_REPRESENTATION_ITEM()
RATIONAL_B_SPLINE_CURVE((4.94937295736913,5.22222222222216,5.22222222222217))
REPRESENTATION_ITEM('')
) ;
#56 = (
BOUNDED_CURVE()
B_SPLINE_CURVE(2,(#125753,#125754,#125755),.UNSPECIFIED.,.F.,.F.)
B_SPLINE_CURVE_WITH_KNOTS((3,3),(2.84165444767653,3.56402846370387),
 .UNSPECIFIED.)
CURVE()
GEOMETRIC_REPRESENTATION_ITEM()
RATIONAL_B_SPLINE_CURVE((5.22222222222218,5.22222222222219,4.94937295736914))
REPRESENTATION_ITEM('')
) ;
#57 = (
BOUNDED_CURVE()
B_SPLINE_CURVE(2,(#125759,#125760,#125761),.UNSPECIFIED.,.F.,.F.)
B_SPLINE_CURVE_WITH_KNOTS((3,3),(2.84165444767652,3.56402846370389),
 .UNSPECIFIED.)
CURVE()
GEOMETRIC_REPRESENTATION_ITEM()
RATIONAL_B_SPLINE_CURVE((5.22222222222217,5.22222222222218,4.94937295736911))
REPRESENTATION_ITEM('')
) ;
#58 = (
BOUNDED_CURVE()
B_SPLINE_CURVE(2,(#125762,#125763,#125764),.UNSPECIFIED.,.F.,.F.)
B_SPLINE_CURVE_WITH_KNOTS((3,3),(2.11928043164923,2.8416544476765),
 .UNSPECIFIED.)
CURVE()
GEOMETRIC_REPRESENTATION_ITEM()
RATIONAL_B_SPLINE_CURVE((4.94937295736913,5.22222222222215,5.22222222222217))
REPRESENTATION_ITEM('')
) ;
#59 = (
BOUNDED_CURVE()
B_SPLINE_CURVE(2,(#125766,#125767,#125768),.UNSPECIFIED.,.F.,.F.)
B_SPLINE_CURVE_WITH_KNOTS((3,3),(2.11928043164914,2.84165444767653),
 .UNSPECIFIED.)
CURVE()
GEOMETRIC_REPRESENTATION_ITEM()
RATIONAL_B_SPLINE_CURVE((4.94937295736908,5.22222222222217,5.22222222222218))
REPRESENTATION_ITEM('')
) ;
#60 = (
BOUNDED_CURVE()
B_SPLINE_CURVE(2,(#125771,#125772,#125773),.UNSPECIFIED.,.F.,.F.)
B_SPLINE_CURVE_WITH_KNOTS((3,3),(2.84165444767655,3.5640284637039),
 .UNSPECIFIED.)
CURVE()
GEOMETRIC_REPRESENTATION_ITEM()
RATIONAL_B_SPLINE_CURVE((5.22222222222218,5.22222222222218,4.94937295736911))
REPRESENTATION_ITEM('')
) ;
#61 = (
BOUNDED_CURVE()
B_SPLINE_CURVE(2,(#125775,#125776,#125777),.UNSPECIFIED.,.F.,.F.)
B_SPLINE_CURVE_WITH_KNOTS((3,3),(2.11928043164924,2.84165444767655),
 .UNSPECIFIED.)
CURVE()
GEOMETRIC_REPRESENTATION_ITEM()
RATIONAL_B_SPLINE_CURVE((4.94937295736915,5.22222222222217,5.22222222222218))
REPRESENTATION_ITEM('')
) ;
#62 = (
BOUNDED_CURVE()
B_SPLINE_CURVE(2,(#125780,#125781,#125782),.UNSPECIFIED.,.F.,.F.)
B_SPLINE_CURVE_WITH_KNOTS((3,3),(2.84165444767655,3.56402846370386),
 .UNSPECIFIED.)
CURVE()
GEOMETRIC_REPRESENTATION_ITEM()
RATIONAL_B_SPLINE_CURVE((5.22222222222217,5.22222222222217,4.94937295736913))
REPRESENTATION_ITEM('')
) ;
#63 = (
BOUNDED_CURVE()
B_SPLINE_CURVE(2,(#125784,#125785,#125786),.UNSPECIFIED.,.F.,.F.)
B_SPLINE_CURVE_WITH_KNOTS((3,3),(2.11928043164924,2.84165444767655),
 .UNSPECIFIED.)
CURVE()
GEOMETRIC_REPRESENTATION_ITEM()
RATIONAL_B_SPLINE_CURVE((4.94937295736914,5.22222222222217,5.22222222222217))
REPRESENTATION_ITEM('')
) ;
#64 = (
BOUNDED_CURVE()
B_SPLINE_CURVE(2,(#125789,#125790,#125791),.UNSPECIFIED.,.F.,.F.)
B_SPLINE_CURVE_WITH_KNOTS((3,3),(2.84165444767657,3.56402846370392),
 .UNSPECIFIED.)
CURVE()
GEOMETRIC_REPRESENTATION_ITEM()
RATIONAL_B_SPLINE_CURVE((5.22222222222219,5.22222222222218,4.94937295736911))
REPRESENTATION_ITEM('')
) ;
#65 = (
BOUNDED_CURVE()
B_SPLINE_CURVE(2,(#125793,#125794,#125795),.UNSPECIFIED.,.F.,.F.)
B_SPLINE_CURVE_WITH_KNOTS((3,3),(2.11928043164923,2.84165444767657),
 .UNSPECIFIED.)
CURVE()
GEOMETRIC_REPRESENTATION_ITEM()
RATIONAL_B_SPLINE_CURVE((4.94937295736915,5.2222222222222,5.22222222222219))
REPRESENTATION_ITEM('')
) ;
#66 = (
BOUNDED_CURVE()
B_SPLINE_CURVE(2,(#125797,#125798,#125799),.UNSPECIFIED.,.F.,.F.)
B_SPLINE_CURVE_WITH_KNOTS((3,3),(2.8416544476765,3.56402846370386),
 .UNSPECIFIED.)
CURVE()
GEOMETRIC_REPRESENTATION_ITEM()
RATIONAL_B_SPLINE_CURVE((5.22222222222217,5.22222222222219,4.94937295736913))
REPRESENTATION_ITEM('')
) ;
#67 = (
BOUNDED_CURVE()
B_SPLINE_CURVE(2,(#126461,#126462,#126463),.UNSPECIFIED.,.F.,.F.)
B_SPLINE_CURVE_WITH_KNOTS((3,3),(-0.29451811881086,-0.129072001599117),
 .UNSPECIFIED.)
CURVE()
GEOMETRIC_REPRESENTATION_ITEM()
RATIONAL_B_SPLINE_CURVE((1.01263937277422,1.02259966004803,1.01738098005117))
REPRESENTATION_ITEM('')
) ;
#68 = (
BOUNDED_CURVE()
B_SPLINE_CURVE(2,(#126470,#126471,#126472),.UNSPECIFIED.,.F.,.F.)
B_SPLINE_CURVE_WITH_KNOTS((3,3),(-0.242836044574457,-0.0773899273627136),
 .UNSPECIFIED.)
CURVE()
GEOMETRIC_REPRESENTATION_ITEM()
RATIONAL_B_SPLINE_CURVE((1.01738098005117,1.02259966004803,1.01263937277422))
REPRESENTATION_ITEM('')
) ;
#69 = (
BOUNDED_CURVE()
B_SPLINE_CURVE(2,(#126477,#126478,#126479),.UNSPECIFIED.,.F.,.F.)
B_SPLINE_CURVE_WITH_KNOTS((3,3),(-0.242836044574458,-0.0773899273627143),
 .UNSPECIFIED.)
CURVE()
GEOMETRIC_REPRESENTATION_ITEM()
RATIONAL_B_SPLINE_CURVE((1.01738098005117,1.02259966004802,1.01263937277422))
REPRESENTATION_ITEM('')
) ;
#70 = (
BOUNDED_CURVE()
B_SPLINE_CURVE(2,(#126482,#126483,#126484),.UNSPECIFIED.,.F.,.F.)
B_SPLINE_CURVE_WITH_KNOTS((3,3),(-0.294518118810858,-0.129072001599116),
 .UNSPECIFIED.)
CURVE()
GEOMETRIC_REPRESENTATION_ITEM()
RATIONAL_B_SPLINE_CURVE((1.01263937277421,1.02259966004801,1.01738098005116))
REPRESENTATION_ITEM('')
) ;
#71 = (
BOUNDED_CURVE()
B_SPLINE_CURVE(2,(#126513,#126514,#126515),.UNSPECIFIED.,.F.,.F.)
B_SPLINE_CURVE_WITH_KNOTS((3,3),(-0.294518118811012,-0.129072001599294),
 .UNSPECIFIED.)
CURVE()
GEOMETRIC_REPRESENTATION_ITEM()
RATIONAL_B_SPLINE_CURVE((1.01263937277418,1.02259966004795,1.01738098005112))
REPRESENTATION_ITEM('')
) ;
#72 = (
BOUNDED_CURVE()
B_SPLINE_CURVE(2,(#126520,#126521,#126522),.UNSPECIFIED.,.F.,.F.)
B_SPLINE_CURVE_WITH_KNOTS((3,3),(-0.242836044574467,-0.0773899273627484),
 .UNSPECIFIED.)
CURVE()
GEOMETRIC_REPRESENTATION_ITEM()
RATIONAL_B_SPLINE_CURVE((1.01738098005112,1.02259966004794,1.01263937277417))
REPRESENTATION_ITEM('')
) ;
#73 = (
BOUNDED_CURVE()
B_SPLINE_CURVE(2,(#126531,#126532,#126533),.UNSPECIFIED.,.F.,.F.)
B_SPLINE_CURVE_WITH_KNOTS((3,3),(-0.242836044574484,-0.0773899273627661),
 .UNSPECIFIED.)
CURVE()
GEOMETRIC_REPRESENTATION_ITEM()
RATIONAL_B_SPLINE_CURVE((1.01738098005103,1.02259966004783,1.01263937277412))
REPRESENTATION_ITEM('')
) ;
#74 = (
BOUNDED_CURVE()
B_SPLINE_CURVE(2,(#126535,#126536,#126537),.UNSPECIFIED.,.F.,.F.)
B_SPLINE_CURVE_WITH_KNOTS((3,3),(-0.294518118811009,-0.129072001599291),
 .UNSPECIFIED.)
CURVE()
GEOMETRIC_REPRESENTATION_ITEM()
RATIONAL_B_SPLINE_CURVE((1.01263937277417,1.02259966004793,1.01738098005111))
REPRESENTATION_ITEM('')
) ;
#75 = B_SPLINE_CURVE_WITH_KNOTS('',3,(#101199,#101200,#101201,#101202,#101203,
#101204,#101205,#101206,#101207,#101208),.UNSPECIFIED.,.F.,.F.,(4,3,3,4),
(3.9738238267564E-15,3.94729529730257E-5,7.90727202189652E-5,0.000103003463696664),
 .UNSPECIFIED.) ;
#76 = B_SPLINE_CURVE_WITH_KNOTS('',3,(#101215,#101216,#101217,#101218,#101219,
#101220,#101221),.UNSPECIFIED.,.F.,.F.,(4,3,4),(0.000158223357507089,0.000179871364136711,
0.000191820073778124),.UNSPECIFIED.) ;
#77 = B_SPLINE_CURVE_WITH_KNOTS('',3,(#101236,#101237,#101238,#101239,#101240,
#101241,#101242,#101243,#101244,#101245,#101246,#101247,#101248,#101249,
#101250,#101251),.UNSPECIFIED.,.F.,.F.,(4,3,3,3,3,4),(2.2541451328491E-8,
3.71181381094363E-5,7.40234349159883E-5,0.000126639028433409,0.000171180683285943,
0.000173579731706481),.UNSPECIFIED.) ;
#78 = B_SPLINE_CURVE_WITH_KNOTS('',3,(#101307,#101308,#101309,#101310,#101311,
#101312),.UNSPECIFIED.,.F.,.F.,(4,2,4),(0.,0.000162685424844482,0.000325370849688964),
 .UNSPECIFIED.) ;
#79 = B_SPLINE_CURVE_WITH_KNOTS('',3,(#101315,#101316,#101317,#101318,#101319,
#101320),.UNSPECIFIED.,.F.,.F.,(4,2,4),(0.,0.000163438694679258,0.000326877389358517),
 .UNSPECIFIED.) ;
#80 = B_SPLINE_CURVE_WITH_KNOTS('',3,(#101331,#101332,#101333,#101334,#101335,
#101336),.UNSPECIFIED.,.F.,.F.,(4,2,4),(-0.00501427184001373,-0.00354643693242479,
0.),.UNSPECIFIED.) ;
#81 = B_SPLINE_CURVE_WITH_KNOTS('',3,(#101349,#101350,#101351,#101352,#101353,
#101354,#101355,#101356,#101357,#101358,#101359,#101360,#101361,#101362,
#101363,#101364,#101365,#101366,#101367,#101368,#101369,#101370,#101371,
#101372,#101373,#101374,#101375,#101376),.UNSPECIFIED.,.F.,.F.,(4,3,3,3,
3,3,3,3,3,4),(5.23810621123106E-9,5.84794260518929E-6,8.4966204178186E-6,
1.21937803558207E-5,1.76033670138093E-5,1.93092034273016E-5,2.55871453405733E-5,
3.03154216363468E-5,3.6851966035102E-5,3.92146766969322E-5),
 .UNSPECIFIED.) ;
#82 = B_SPLINE_CURVE_WITH_KNOTS('',3,(#101378,#101379,#101380,#101381,#101382,
#101383,#101384,#101385,#101386,#101387),.UNSPECIFIED.,.F.,.F.,(4,3,3,4),
(0.000144469795965456,0.000165397602015579,0.000173816468562374,0.000175865847906018),
 .UNSPECIFIED.) ;
#83 = B_SPLINE_CURVE_WITH_KNOTS('',3,(#101405,#101406,#101407,#101408,#101409,
#101410,#101411),.UNSPECIFIED.,.F.,.F.,(4,3,4),(-2.05331166616804E-6,2.04386714305399E-5,
3.16299855932264E-5),.UNSPECIFIED.) ;
#84 = B_SPLINE_CURVE_WITH_KNOTS('',3,(#101413,#101414,#101415,#101416,#101417,
#101418,#101419,#101420,#101421,#101422,#101423,#101424),.UNSPECIFIED.,
 .F.,.F.,(4,2,2,2,2,4),(9.00279448284787E-9,0.00183032786992351,0.0060774656661988,
0.0169681634641076,0.0216775195638031,0.0254454420779839),.UNSPECIFIED.) ;
#85 = B_SPLINE_CURVE_WITH_KNOTS('',3,(#101583,#101584,#101585,#101586,#101587,
#101588,#101589,#101590,#101591,#101592,#101593,#101594,#101595,#101596,
#101597,#101598,#101599,#101600,#101601,#101602,#101603,#101604,#101605,
#101606,#101607,#101608,#101609,#101610,#101611,#101612,#101613,#101614,
#101615,#101616,#101617,#101618,#101619,#101620,#101621,#101622),
 .UNSPECIFIED.,.F.,.F.,(4,3,3,3,3,3,3,3,3,3,3,3,3,4),(3.25260651745651E-19,
5.07173230207635E-5,0.000104017413485144,0.000124506719166644,0.000125249568192437,
0.000156566023859648,0.000186760078749966,0.000187880030991792,0.000203537318084802,
0.000211366035547456,0.000217886758541627,0.000219194644848635,0.000234851354133261,
0.000249013438333288),.UNSPECIFIED.) ;
#86 = B_SPLINE_CURVE_WITH_KNOTS('',3,(#101628,#101629,#101630,#101631,#101632,
#101633,#101634,#101635,#101636,#101637,#101638,#101639,#101640,#101641,
#101642,#101643,#101644,#101645,#101646,#101647,#101648,#101649,#101650,
#101651,#101652,#101653,#101654,#101655,#101656,#101657,#101658,#101659,
#101660,#101661,#101662,#101663,#101664,#101665,#101666,#101667),
 .UNSPECIFIED.,.F.,.F.,(4,3,3,3,3,3,3,3,3,3,3,3,3,4),(0.,1.43115567092604E-5,
3.01335133960367E-5,3.14552036774737E-5,3.8044751729729E-5,4.5956122251847E-5,
6.17788922892814E-5,6.29104073549473E-5,9.3421096696511E-5,0.000125066393795497,
0.000125820814709898,0.000179837268175291,0.000231469985683482,0.0002516416294198),
 .UNSPECIFIED.) ;
#87 = B_SPLINE_CURVE_WITH_KNOTS('',3,(#101672,#101673,#101674,#101675,#101676,
#101677,#101678),.UNSPECIFIED.,.F.,.F.,(4,3,4),(-2.04939766627081E-6,0.,
2.93835791072158E-5),.UNSPECIFIED.) ;
#88 = B_SPLINE_CURVE_WITH_KNOTS('',3,(#101693,#101694,#101695,#101696,#101697,
#101698,#101699,#101700,#101701,#101702,#101703,#101704,#101705,#101706),
 .UNSPECIFIED.,.F.,.F.,(4,2,2,2,2,2,4),(1.44901762830932E-6,0.00056162152378578,
0.00112173034328052,0.00210338619166554,0.00384452539466144,0.00473112295119629,
0.00541108585516142),.UNSPECIFIED.) ;
#89 = B_SPLINE_CURVE_WITH_KNOTS('',3,(#101715,#101716,#101717,#101718,#101719,
#101720,#101721,#101722,#101723,#101724,#101725,#101726,#101727,#101728,
#101729,#101730,#101731,#101732,#101733,#101734,#101735,#101736,#101737,
#101738,#101739,#101740,#101741,#101742,#101743,#101744,#101745,#101746,
#101747,#101748),.UNSPECIFIED.,.F.,.F.,(4,2,2,2,2,2,2,2,2,2,2,2,2,2,2,2,
4),(0.,1.67528894171223E-5,3.36326639087882E-5,3.53285003632596E-5,3.67766442981684E-5,
4.45936877500603E-5,5.25629171992643E-5,5.37833548713901E-5,5.51649664472508E-5,
7.22376444474067E-5,7.35532885963332E-5,0.000109240736296583,0.000146228640920627,
0.000147106577192663,0.000203359192947108,0.000258123601946057,0.000294213154385318),
 .UNSPECIFIED.) ;
#90 = B_SPLINE_CURVE_WITH_KNOTS('',3,(#101752,#101753,#101754,#101755,#101756,
#101757,#101758,#101759,#101760,#101761,#101762,#101763,#101764,#101765,
#101766,#101767,#101768,#101769,#101770,#101771,#101772,#101773,#101774,
#101775,#101776,#101777,#101778,#101779,#101780,#101781,#101782,#101783,
#101784,#101785,#101786,#101787,#101788,#101789,#101790,#101791,#101792,
#101793,#101794,#101795,#101796,#101797,#101798,#101799,#101800,#101801,
#101802,#101803),.UNSPECIFIED.,.F.,.F.,(4,3,3,3,3,3,3,3,3,3,3,3,3,3,3,3,
3,4),(0.,5.28180786082966E-5,0.000107888430275573,0.000143209193858987,
0.000144078242180707,0.000180086811859616,0.000214813790788481,0.00021545817026355,
0.000216102549738619,0.000232714940020855,0.000234106492510809,0.000238605983992194,
0.000240855729732887,0.00024310547547358,0.00025061608925323,0.000252108710851783,
0.000270124214172477,0.000286418387717979),.UNSPECIFIED.) ;
#91 = B_SPLINE_CURVE_WITH_KNOTS('',3,(#101948,#101949,#101950,#101951,#101952,
#101953,#101954,#101955),.UNSPECIFIED.,.F.,.F.,(4,2,2,4),(-0.0473604779370388,
-0.0461995546884435,-0.0447198409510953,-0.0410407833884838),
 .UNSPECIFIED.) ;
#92 = B_SPLINE_CURVE_WITH_KNOTS('',3,(#101963,#101964,#101965,#101966,#101967,
#101968,#101969,#101970),.UNSPECIFIED.,.F.,.F.,(4,2,2,4),(-0.0536801724855785,
-0.0500011149229822,-0.048521401185634,-0.0473604779370388),
 .UNSPECIFIED.) ;
#93 = B_SPLINE_CURVE_WITH_KNOTS('',3,(#102424,#102425,#102426,#102427,#102428,
#102429,#102430,#102431,#102432,#102433,#102434,#102435,#102436,#102437),
 .UNSPECIFIED.,.F.,.F.,(4,2,2,2,2,2,4),(4.71238898038469,4.8817580624518,
5.06763701998932,5.24337922965563,5.26451333208247,5.44874090582915,5.49822830854824),
 .UNSPECIFIED.) ;
#94 = B_SPLINE_CURVE_WITH_KNOTS('',3,(#102442,#102443,#102444,#102445,#102446,
#102447,#102448,#102449,#102450,#102451,#102452,#102453,#102454,#102455),
 .UNSPECIFIED.,.F.,.F.,(4,2,2,2,2,2,4),(0.784956998631334,0.96694169431193,
1.1431172121296,1.16348181627596,1.34745079132871,1.51752882030683,1.5707963267949),
 .UNSPECIFIED.) ;
#95 = B_SPLINE_CURVE_WITH_KNOTS('',3,(#102461,#102462,#102463,#102464,#102465,
#102466,#102467,#102468,#102469,#102470,#102471,#102472,#102473,#102474),
 .UNSPECIFIED.,.F.,.F.,(4,2,2,2,2,2,4),(0.784956998631337,0.966941694311871,
1.14311721213079,1.16348181627588,1.34745079132852,1.51752882030658,1.5707963267949),
 .UNSPECIFIED.) ;
#96 = B_SPLINE_CURVE_WITH_KNOTS('',3,(#102476,#102477,#102478,#102479,#102480,
#102481,#102482,#102483,#102484,#102485,#102486,#102487,#102488,#102489),
 .UNSPECIFIED.,.F.,.F.,(4,2,2,2,2,2,4),(4.71238898038469,4.88175806245191,
5.06763701998937,5.24337922965534,5.2645133320825,5.44874090582923,5.49822830854825),
 .UNSPECIFIED.) ;
#97 = B_SPLINE_CURVE_WITH_KNOTS('',3,(#102493,#102494,#102495,#102496,#102497,
#102498,#102499,#102500,#102501,#102502,#102503,#102504,#102505,#102506),
 .UNSPECIFIED.,.F.,.F.,(4,2,2,2,2,2,4),(4.71238898038469,4.88175806245175,
5.06763701998915,5.24337922965918,5.26451333208223,5.44874090582892,5.49822830854824),
 .UNSPECIFIED.) ;
#98 = B_SPLINE_CURVE_WITH_KNOTS('',3,(#102510,#102511,#102512,#102513,#102514,
#102515,#102516,#102517,#102518,#102519,#102520,#102521,#102522,#102523),
 .UNSPECIFIED.,.F.,.F.,(4,2,2,2,2,2,4),(0.784956998631348,0.96694169431196,
1.14311721213076,1.16348181627594,1.34745079132846,1.51752882030657,1.5707963267949),
 .UNSPECIFIED.) ;
#99 = B_SPLINE_CURVE_WITH_KNOTS('',3,(#102538,#102539,#102540,#102541,#102542,
#102543,#102544,#102545,#102546,#102547,#102548,#102549,#102550,#102551),
 .UNSPECIFIED.,.F.,.F.,(4,2,2,2,2,2,4),(0.784956998631344,0.966941694311673,
1.14311721213023,1.16348181627565,1.34745079132822,1.51752882030641,1.5707963267949),
 .UNSPECIFIED.) ;
#100 = B_SPLINE_CURVE_WITH_KNOTS('',3,(#102555,#102556,#102557,#102558,#102559,
#102560,#102561,#102562,#102563,#102564,#102565,#102566,#102567,#102568),
 .UNSPECIFIED.,.F.,.F.,(4,2,2,2,2,2,4),(4.71238898038469,4.88175806245189,
5.06763701998948,5.24337922965067,5.26451333208267,5.44874090582925,5.49822830854823),
 .UNSPECIFIED.) ;
#101 = B_SPLINE_CURVE_WITH_KNOTS('',3,(#102673,#102674,#102675,#102676,#102677,
#102678,#102679,#102680,#102681,#102682,#102683,#102684,#102685,#102686,
#102687,#102688),.UNSPECIFIED.,.F.,.F.,(4,3,3,3,3,4),(0.,3.26760986414936E-5,
6.60604127813368E-5,0.00010113572426573,0.000138237800333083,0.000166242991827322),
 .UNSPECIFIED.) ;
#102 = B_SPLINE_CURVE_WITH_KNOTS('',3,(#102750,#102751,#102752,#102753,#102754,
#102755,#102756,#102757,#102758,#102759,#102760,#102761,#102762,#102763,
#102764,#102765),.UNSPECIFIED.,.F.,.F.,(4,3,3,3,3,4),(0.,1.86901632150157E-5,
5.38940239621533E-5,9.13255451816924E-5,0.000129775966053829,0.000168373497604197),
 .UNSPECIFIED.) ;
#103 = B_SPLINE_CURVE_WITH_KNOTS('',3,(#102770,#102771,#102772,#102773,#102774,
#102775,#102776,#102777,#102778,#102779),.UNSPECIFIED.,.F.,.F.,(4,2,2,2,
4),(0.0288531015810606,0.0296205843579712,0.0328031056820271,0.0376042554622301,
0.0407130021445681),.UNSPECIFIED.) ;
#104 = B_SPLINE_CURVE_WITH_KNOTS('',3,(#102784,#102785,#102786,#102787,#102788,
#102789),.UNSPECIFIED.,.F.,.F.,(4,2,4),(0.0637474840427468,0.0675088661505087,
0.0720284409664136),.UNSPECIFIED.) ;
#105 = B_SPLINE_CURVE_WITH_KNOTS('',3,(#102795,#102796,#102797,#102798,#102799,
#102800,#102801,#102802,#102803,#102804),.UNSPECIFIED.,.F.,.F.,(4,2,2,2,
4),(0.0767275662247105,0.0771734766312244,0.0818220866843324,0.0868722195343171,
0.0892832637334449),.UNSPECIFIED.) ;
#106 = B_SPLINE_CURVE_WITH_KNOTS('',3,(#102839,#102840,#102841,#102842,#102843,
#102844),.UNSPECIFIED.,.F.,.F.,(4,2,4),(0.171679973604307,0.178707475947415,
0.186889989698882),.UNSPECIFIED.) ;
#107 = B_SPLINE_CURVE_WITH_KNOTS('',3,(#102884,#102885,#102886,#102887,#102888,
#102889,#102890,#102891,#102892,#102893,#102894,#102895,#102896,#102897,
#102898,#102899,#102900,#102901,#102902,#102903,#102904,#102905,#102906,
#102907,#102908,#102909,#102910,#102911,#102912,#102913),.UNSPECIFIED.,
 .F.,.F.,(4,2,2,2,2,2,2,2,2,2,2,2,2,2,4),(2.36970964942748,2.55498029688293,
2.73514427897862,2.74569929646372,2.92071305421519,2.93943382978511,3.11857096683926,
3.13197658032397,3.25399179664489,3.45054278261474,3.62794535800311,3.64606212534864,
3.82474099483969,3.83698255062518,3.9134742131524),.UNSPECIFIED.) ;
#108 = B_SPLINE_CURVE_WITH_KNOTS('',3,(#102924,#102925,#102926,#102927,#102928,
#102929,#102930,#102931,#102932,#102933,#102934,#102935,#102936,#102937,
#102938,#102939,#102940,#102941,#102942,#102943,#102944,#102945,#102946,
#102947,#102948,#102949),.UNSPECIFIED.,.F.,.F.,(4,2,2,2,2,2,2,2,2,2,2,2,
4),(2.70344464881052,2.89144352771273,3.06851986332525,3.0808108907457,
3.26996664970825,3.35940092938491,3.54587543017999,3.72254345721242,3.73903833379419,
3.91570024693591,3.93052100184837,4.1173551198632,4.22222897897866),
 .UNSPECIFIED.) ;
#109 = B_SPLINE_CURVE_WITH_KNOTS('',3,(#103107,#103108,#103109,#103110,#103111,
#103112,#103113,#103114,#103115,#103116,#103117,#103118,#103119,#103120,
#103121,#103122,#103123,#103124,#103125),.UNSPECIFIED.,.F.,.F.,(4,3,3,3,
3,3,4),(2.81004151652491E-8,3.99307614181575E-5,8.00540716903473E-5,0.000126830846822484,
0.000175618195186419,0.00021519314047228,0.000245220898756747),
 .UNSPECIFIED.) ;
#110 = B_SPLINE_CURVE_WITH_KNOTS('',3,(#103148,#103149,#103150,#103151,#103152,
#103153,#103154,#103155,#103156,#103157,#103158,#103159,#103160,#103161,
#103162,#103163,#103164,#103165,#103166,#103167,#103168,#103169,#103170,
#103171,#103172,#103173,#103174,#103175,#103176,#103177,#103178,#103179,
#103180,#103181,#103182,#103183,#103184,#103185,#103186,#103187,#103188,
#103189,#103190,#103191,#103192,#103193,#103194,#103195,#103196,#103197,
#103198,#103199,#103200,#103201,#103202,#103203,#103204,#103205,#103206,
#103207,#103208,#103209,#103210,#103211,#103212,#103213,#103214,#103215,
#103216,#103217,#103218,#103219,#103220,#103221,#103222,#103223,#103224,
#103225,#103226),.UNSPECIFIED.,.F.,.F.,(4,3,3,3,3,3,3,3,3,3,3,3,3,3,3,3,
3,3,3,3,3,3,3,3,3,3,4),(0.000152038190190966,0.00015489284140843,0.000155160464960067,
0.000160456565729287,0.000163456795060822,0.000166580092246913,0.000167751328691697,
0.000168007536663994,0.000168255738137156,0.000169267315291243,0.000175949983805187,
0.000178959298271468,0.000180334649023636,0.000187987241670312,0.000191981216408558,
0.000193065528939082,0.000193839174265184,0.000198143816207852,0.000212206269476803,
0.000226582370019584,0.000228143757087806,0.000228729277238389,0.000232827918292472,
0.000249109432819239,0.000250176797440921,0.000265881325829883,0.00026752567658937),
 .UNSPECIFIED.) ;
#111 = B_SPLINE_CURVE_WITH_KNOTS('',3,(#103228,#103229,#103230,#103231,#103232,
#103233,#103234,#103235,#103236,#103237),.UNSPECIFIED.,.F.,.F.,(4,3,3,4),
(0.000130631741230592,0.000139067346352972,0.000143554831048516,0.000152038189371529),
 .UNSPECIFIED.) ;
#112 = B_SPLINE_CURVE_WITH_KNOTS('',3,(#103239,#103240,#103241,#103242,#103243,
#103244,#103245,#103246,#103247,#103248,#103249,#103250,#103251,#103252,
#103253,#103254,#103255,#103256,#103257),.UNSPECIFIED.,.F.,.F.,(4,3,3,3,
3,3,4),(0.000104137230127885,0.000110259474166351,0.000116844366893157,
0.000120664217590229,0.000125429508057305,0.000130430624030388,0.000130630877722849),
 .UNSPECIFIED.) ;
#113 = B_SPLINE_CURVE_WITH_KNOTS('',3,(#103258,#103259,#103260,#103261,#103262,
#103263,#103264,#103265,#103266,#103267,#103268,#103269,#103270,#103271,
#103272,#103273,#103274,#103275,#103276,#103277,#103278,#103279,#103280,
#103281,#103282,#103283,#103284,#103285,#103286,#103287,#103288,#103289,
#103290,#103291,#103292,#103293,#103294,#103295,#103296,#103297,#103298,
#103299,#103300),.UNSPECIFIED.,.F.,.F.,(4,3,3,3,3,3,3,3,3,3,3,3,3,3,4),
(0.,4.7842153196409E-6,1.59977421330766E-5,1.7596526576931E-5,2.63603667654262E-5,
3.75047088104424E-5,4.29655082836412E-5,5.34507806651091E-5,6.17416442239024E-5,
6.3936053046577E-5,7.32944438956243E-5,8.49065978095127E-5,9.46209320477897E-5,
9.66050857869699E-5,0.000104137229466899),.UNSPECIFIED.) ;
#114 = B_SPLINE_CURVE_WITH_KNOTS('',3,(#103370,#103371,#103372,#103373,#103374,
#103375,#103376,#103377,#103378,#103379,#103380,#103381,#103382,#103383,
#103384,#103385,#103386,#103387,#103388,#103389,#103390,#103391,#103392,
#103393,#103394,#103395,#103396,#103397,#103398,#103399,#103400,#103401,
#103402,#103403),.UNSPECIFIED.,.F.,.F.,(4,3,3,3,3,3,3,3,3,3,3,4),(0.000173579735006479,
0.000179152672590571,0.000187122196212527,0.000190349677855674,0.000201571576239331,
0.000207505544696437,0.000209082158340111,0.000218112358783822,0.000219837174422831,
0.000228512621317844,0.000240802935331578,0.000245138123631296),
 .UNSPECIFIED.) ;
#115 = B_SPLINE_CURVE_WITH_KNOTS('',3,(#103465,#103466,#103467,#103468,#103469,
#103470,#103471,#103472,#103473,#103474,#103475,#103476,#103477,#103478,
#103479,#103480),.UNSPECIFIED.,.F.,.F.,(4,3,3,3,3,4),(0.00014982626823882,
0.000156541783273878,0.000187447062839771,0.000218157419331145,0.000251253590119498,
0.000263630362845943),.UNSPECIFIED.) ;
#116 = B_SPLINE_CURVE_WITH_KNOTS('',3,(#103482,#103483,#103484,#103485),
 .UNSPECIFIED.,.F.,.F.,(4,4),(0.000128945525003041,0.00014982626823882),
 .UNSPECIFIED.) ;
#117 = B_SPLINE_CURVE_WITH_KNOTS('',3,(#103486,#103487,#103488,#103489,#103490,
#103491,#103492,#103493,#103494,#103495,#103496,#103497,#103498,#103499,
#103500,#103501),.UNSPECIFIED.,.F.,.F.,(4,3,3,3,3,4),(0.000107977862661221,
0.000113849696954279,0.000116758640899991,0.000123355930725603,0.00012864932133829,
0.000128945525003041),.UNSPECIFIED.) ;
#118 = B_SPLINE_CURVE_WITH_KNOTS('',3,(#103711,#103712,#103713,#103714,#103715,
#103716,#103717,#103718,#103719,#103720),.UNSPECIFIED.,.F.,.F.,(4,3,3,4),
(3.97263228028543E-15,3.94729529730253E-5,7.90727202189645E-5,0.000103003463696544),
 .UNSPECIFIED.) ;
#119 = B_SPLINE_CURVE_WITH_KNOTS('',3,(#103727,#103728,#103729,#103730,#103731,
#103732,#103733),.UNSPECIFIED.,.F.,.F.,(4,3,4),(0.000158223357507079,0.000179871364137041,
0.000191820073778125),.UNSPECIFIED.) ;
#120 = B_SPLINE_CURVE_WITH_KNOTS('',3,(#103748,#103749,#103750,#103751,#103752,
#103753,#103754,#103755,#103756,#103757,#103758,#103759,#103760,#103761,
#103762,#103763),.UNSPECIFIED.,.F.,.F.,(4,3,3,3,3,4),(2.25414513312457E-8,
3.71181381094367E-5,7.40234349159884E-5,0.00012663902843341,0.000171180683285944,
0.000173579731706483),.UNSPECIFIED.) ;
#121 = B_SPLINE_CURVE_WITH_KNOTS('',3,(#103819,#103820,#103821,#103822,#103823,
#103824),.UNSPECIFIED.,.F.,.F.,(4,2,4),(0.,0.000162685424844482,0.000325370849688964),
 .UNSPECIFIED.) ;
#122 = B_SPLINE_CURVE_WITH_KNOTS('',3,(#103827,#103828,#103829,#103830,#103831,
#103832),.UNSPECIFIED.,.F.,.F.,(4,2,4),(0.,0.000163438694679258,0.000326877389358517),
 .UNSPECIFIED.) ;
#123 = B_SPLINE_CURVE_WITH_KNOTS('',3,(#103843,#103844,#103845,#103846,#103847,
#103848),.UNSPECIFIED.,.F.,.F.,(4,2,4),(-0.00501427184001364,-0.00354643693242477,
0.),.UNSPECIFIED.) ;
#124 = B_SPLINE_CURVE_WITH_KNOTS('',3,(#103861,#103862,#103863,#103864,#103865,
#103866,#103867,#103868,#103869,#103870,#103871,#103872,#103873,#103874,
#103875,#103876,#103877,#103878,#103879,#103880,#103881,#103882,#103883,
#103884,#103885,#103886,#103887,#103888),.UNSPECIFIED.,.F.,.F.,(4,3,3,3,
3,3,3,3,3,4),(5.23810620682237E-9,5.84794260519337E-6,8.49662041781855E-6,
1.2193780355802E-5,1.76033670137239E-5,1.93092034273018E-5,2.55871453405539E-5,
3.03154216363478E-5,3.68519660351436E-5,3.92146766969337E-5),
 .UNSPECIFIED.) ;
#125 = B_SPLINE_CURVE_WITH_KNOTS('',3,(#103890,#103891,#103892,#103893,#103894,
#103895,#103896,#103897,#103898,#103899),.UNSPECIFIED.,.F.,.F.,(4,3,3,4),
(0.000144469795965455,0.000165397602015561,0.000173816468562373,0.000175865847906015),
 .UNSPECIFIED.) ;
#126 = B_SPLINE_CURVE_WITH_KNOTS('',3,(#103917,#103918,#103919,#103920,#103921,
#103922,#103923),.UNSPECIFIED.,.F.,.F.,(4,3,4),(-2.05331166616703E-6,2.04386714305792E-5,
3.1629985593224E-5),.UNSPECIFIED.) ;
#127 = B_SPLINE_CURVE_WITH_KNOTS('',3,(#103925,#103926,#103927,#103928,#103929,
#103930,#103931,#103932,#103933,#103934,#103935,#103936),.UNSPECIFIED.,
 .F.,.F.,(4,2,2,2,2,4),(9.00279511935952E-9,0.00183032787015945,0.00607746566495241,
0.016968163415124,0.0216775194921712,0.025445441987748),.UNSPECIFIED.) ;
#128 = B_SPLINE_CURVE_WITH_KNOTS('',3,(#104095,#104096,#104097,#104098,#104099,
#104100,#104101,#104102,#104103,#104104,#104105,#104106,#104107,#104108,
#104109,#104110,#104111,#104112,#104113,#104114,#104115,#104116,#104117,
#104118,#104119,#104120,#104121,#104122,#104123,#104124,#104125,#104126,
#104127,#104128,#104129,#104130,#104131,#104132,#104133,#104134),
 .UNSPECIFIED.,.F.,.F.,(4,3,3,3,3,3,3,3,3,3,3,3,3,4),(0.,5.0717323021306E-5,
0.000104017413486267,0.000124506719166654,0.000125249568192443,0.000156566023859662,
0.000186760078749982,0.000187880030991811,0.000203537318084821,0.000211366035547473,
0.000217886758541643,0.000219194644848652,0.000234851354133276,0.000249013438333305),
 .UNSPECIFIED.) ;
#129 = B_SPLINE_CURVE_WITH_KNOTS('',3,(#104140,#104141,#104142,#104143,#104144,
#104145,#104146,#104147,#104148,#104149,#104150,#104151,#104152,#104153,
#104154,#104155,#104156,#104157,#104158,#104159,#104160,#104161,#104162,
#104163,#104164,#104165,#104166,#104167,#104168,#104169,#104170,#104171,
#104172,#104173,#104174,#104175,#104176,#104177,#104178,#104179),
 .UNSPECIFIED.,.F.,.F.,(4,3,3,3,3,3,3,3,3,3,3,3,3,4),(0.,1.43115567092614E-5,
3.01335133960405E-5,3.14552036774747E-5,3.80447517297348E-5,4.59561222518546E-5,
6.17788922892857E-5,6.29104073549493E-5,9.34210966965139E-5,0.000125066393795497,
0.000125820814709899,0.00017983726817215,0.000231469985677585,0.0002516416294198),
 .UNSPECIFIED.) ;
#130 = B_SPLINE_CURVE_WITH_KNOTS('',3,(#104184,#104185,#104186,#104187,#104188,
#104189,#104190),.UNSPECIFIED.,.F.,.F.,(4,3,4),(-2.04939766627066E-6,0.,
2.9383579107217E-5),.UNSPECIFIED.) ;
#131 = B_SPLINE_CURVE_WITH_KNOTS('',3,(#104205,#104206,#104207,#104208,#104209,
#104210,#104211,#104212,#104213,#104214,#104215,#104216,#104217,#104218),
 .UNSPECIFIED.,.F.,.F.,(4,2,2,2,2,2,4),(1.44901762819747E-6,0.000561621523735244,
0.00112173034317294,0.00210338619144832,0.00384452539459816,0.00473112295166382,
0.00541108585598296),.UNSPECIFIED.) ;
#132 = B_SPLINE_CURVE_WITH_KNOTS('',3,(#104227,#104228,#104229,#104230,#104231,
#104232,#104233,#104234,#104235,#104236,#104237,#104238,#104239,#104240,
#104241,#104242,#104243,#104244,#104245,#104246,#104247,#104248,#104249,
#104250,#104251,#104252,#104253,#104254,#104255,#104256,#104257,#104258,
#104259,#104260),.UNSPECIFIED.,.F.,.F.,(4,2,2,2,2,2,2,2,2,2,2,2,2,2,2,2,
4),(0.,1.67528894171568E-5,3.36326639087595E-5,3.532850036333E-5,3.67766442982351E-5,
4.45936877501458E-5,5.2562917199235E-5,5.37833548714877E-5,5.51649664473517E-5,
7.22376444475302E-5,7.35532885964682E-5,0.000109240736296779,0.000146228640920914,
0.000147106577192946,0.0002033591929484,0.000258123601948835,0.000294213154385907),
 .UNSPECIFIED.) ;
#133 = B_SPLINE_CURVE_WITH_KNOTS('',3,(#104264,#104265,#104266,#104267,#104268,
#104269,#104270,#104271,#104272,#104273,#104274,#104275,#104276,#104277,
#104278,#104279,#104280,#104281,#104282,#104283,#104284,#104285,#104286,
#104287,#104288,#104289,#104290,#104291,#104292,#104293,#104294,#104295,
#104296,#104297,#104298,#104299,#104300,#104301,#104302,#104303,#104304,
#104305,#104306,#104307,#104308,#104309,#104310,#104311,#104312,#104313,
#104314,#104315),.UNSPECIFIED.,.F.,.F.,(4,3,3,3,3,3,3,3,3,3,3,3,3,3,3,3,
3,4),(0.,5.28180786102637E-5,0.00010788843028001,0.000143209193858987,0.000144078242180701,
0.000180086811859617,0.000214813790788482,0.000215458170263551,0.00021610254973862,
0.000232714940020857,0.00023410649251081,0.000238605983992196,0.000240855729732889,
0.000243105475473582,0.000250616089253232,0.000252108710851784,0.000270124214172475,
0.00028641838771798),.UNSPECIFIED.) ;
#134 = B_SPLINE_CURVE_WITH_KNOTS('',3,(#104460,#104461,#104462,#104463,#104464,
#104465,#104466,#104467),.UNSPECIFIED.,.F.,.F.,(4,2,2,4),(-0.0473604779370388,
-0.0461995546884436,-0.0447198409510954,-0.0410407833884838),
 .UNSPECIFIED.) ;
#135 = B_SPLINE_CURVE_WITH_KNOTS('',3,(#104475,#104476,#104477,#104478,#104479,
#104480,#104481,#104482),.UNSPECIFIED.,.F.,.F.,(4,2,2,4),(-0.0536801724855784,
-0.0500011149229823,-0.048521401185634,-0.0473604779370388),
 .UNSPECIFIED.) ;
#136 = B_SPLINE_CURVE_WITH_KNOTS('',3,(#104936,#104937,#104938,#104939,#104940,
#104941,#104942,#104943,#104944,#104945,#104946,#104947,#104948,#104949),
 .UNSPECIFIED.,.F.,.F.,(4,2,2,2,2,2,4),(4.71238898038469,4.88175806245194,
5.06763701998947,5.24337922965538,5.26451333208261,5.4487409058292,5.49822830854821),
 .UNSPECIFIED.) ;
#137 = B_SPLINE_CURVE_WITH_KNOTS('',3,(#104954,#104955,#104956,#104957,#104958,
#104959,#104960,#104961,#104962,#104963,#104964,#104965,#104966,#104967),
 .UNSPECIFIED.,.F.,.F.,(4,2,2,2,2,2,4),(0.78495699863134,0.966941694312354,
1.14311721213096,1.16348181627614,1.34745079132807,1.51752882030578,1.5707963267949),
 .UNSPECIFIED.) ;
#138 = B_SPLINE_CURVE_WITH_KNOTS('',3,(#104973,#104974,#104975,#104976,#104977,
#104978,#104979,#104980,#104981,#104982,#104983,#104984,#104985,#104986),
 .UNSPECIFIED.,.F.,.F.,(4,2,2,2,2,2,4),(0.784956998631338,0.966941694312111,
1.14311721213157,1.16348181627597,1.34745079132821,1.51752882030615,1.5707963267949),
 .UNSPECIFIED.) ;
#139 = B_SPLINE_CURVE_WITH_KNOTS('',3,(#104988,#104989,#104990,#104991,#104992,
#104993,#104994,#104995,#104996,#104997,#104998,#104999,#105000,#105001),
 .UNSPECIFIED.,.F.,.F.,(4,2,2,2,2,2,4),(4.71238898038469,4.88175806245166,
5.06763701998869,5.24337922965497,5.26451333208185,5.44874090582888,5.49822830854824),
 .UNSPECIFIED.) ;
#140 = B_SPLINE_CURVE_WITH_KNOTS('',3,(#105005,#105006,#105007,#105008,#105009,
#105010,#105011,#105012,#105013,#105014,#105015,#105016,#105017,#105018),
 .UNSPECIFIED.,.F.,.F.,(4,2,2,2,2,2,4),(4.71238898038469,4.88175806245182,
5.06763701998925,5.24337922964886,5.26451333208237,5.44874090582905,5.49822830854823),
 .UNSPECIFIED.) ;
#141 = B_SPLINE_CURVE_WITH_KNOTS('',3,(#105022,#105023,#105024,#105025,#105026,
#105027,#105028,#105029,#105030,#105031,#105032,#105033,#105034,#105035),
 .UNSPECIFIED.,.F.,.F.,(4,2,2,2,2,2,4),(0.784956998631348,0.966941694311913,
1.14311721213295,1.16348181627588,1.34745079132843,1.51752882030647,1.5707963267949),
 .UNSPECIFIED.) ;
#142 = B_SPLINE_CURVE_WITH_KNOTS('',3,(#105050,#105051,#105052,#105053,#105054,
#105055,#105056,#105057,#105058,#105059,#105060,#105061,#105062,#105063),
 .UNSPECIFIED.,.F.,.F.,(4,2,2,2,2,2,4),(0.784956998631365,0.966941694311873,
1.14311721213002,1.16348181627585,1.34745079132852,1.51752882030655,1.5707963267949),
 .UNSPECIFIED.) ;
#143 = B_SPLINE_CURVE_WITH_KNOTS('',3,(#105067,#105068,#105069,#105070,#105071,
#105072,#105073,#105074,#105075,#105076,#105077,#105078,#105079,#105080),
 .UNSPECIFIED.,.F.,.F.,(4,2,2,2,2,2,4),(4.71238898038469,4.88175806245151,
5.06763701998819,5.24337922965584,5.26451333208124,5.4487409058285,5.49822830854824),
 .UNSPECIFIED.) ;
#144 = B_SPLINE_CURVE_WITH_KNOTS('',3,(#105185,#105186,#105187,#105188,#105189,
#105190,#105191,#105192,#105193,#105194,#105195,#105196,#105197,#105198,
#105199,#105200),.UNSPECIFIED.,.F.,.F.,(4,3,3,3,3,4),(0.,3.26760986414935E-5,
6.60604127813367E-5,0.00010113572426573,0.000138237800333083,0.000166242991827323),
 .UNSPECIFIED.) ;
#145 = B_SPLINE_CURVE_WITH_KNOTS('',3,(#105262,#105263,#105264,#105265,#105266,
#105267,#105268,#105269,#105270,#105271,#105272,#105273,#105274,#105275,
#105276,#105277),.UNSPECIFIED.,.F.,.F.,(4,3,3,3,3,4),(0.,1.86901632150157E-5,
5.38940239621529E-5,9.13255451816918E-5,0.000129775966053829,0.000168373497604196),
 .UNSPECIFIED.) ;
#146 = B_SPLINE_CURVE_WITH_KNOTS('',3,(#105282,#105283,#105284,#105285,#105286,
#105287,#105288,#105289,#105290,#105291),.UNSPECIFIED.,.F.,.F.,(4,2,2,2,
4),(0.0288531015801791,0.0296205843570608,0.0328031056810013,0.0376042554610398,
0.0407130021432729),.UNSPECIFIED.) ;
#147 = B_SPLINE_CURVE_WITH_KNOTS('',3,(#105296,#105297,#105298,#105299,#105300,
#105301),.UNSPECIFIED.,.F.,.F.,(4,2,4),(0.063747484019213,0.0675088661241108,
0.0720284409363993),.UNSPECIFIED.) ;
#148 = B_SPLINE_CURVE_WITH_KNOTS('',3,(#105307,#105308,#105309,#105310,#105311,
#105312,#105313,#105314,#105315,#105316),.UNSPECIFIED.,.F.,.F.,(4,2,2,2,
4),(0.0767275662235905,0.0771734766300911,0.0818220866830681,0.0868722195329092,
0.0892832637319672),.UNSPECIFIED.) ;
#149 = B_SPLINE_CURVE_WITH_KNOTS('',3,(#105351,#105352,#105353,#105354,#105355,
#105356),.UNSPECIFIED.,.F.,.F.,(4,2,4),(0.171679973604201,0.178707475947309,
0.186889989698777),.UNSPECIFIED.) ;
#150 = B_SPLINE_CURVE_WITH_KNOTS('',3,(#105396,#105397,#105398,#105399,#105400,
#105401,#105402,#105403,#105404,#105405,#105406,#105407,#105408,#105409,
#105410,#105411,#105412,#105413,#105414,#105415,#105416,#105417,#105418,
#105419,#105420,#105421,#105422,#105423,#105424,#105425),.UNSPECIFIED.,
 .F.,.F.,(4,2,2,2,2,2,2,2,2,2,2,2,2,2,4),(2.36970964942748,2.55498029688299,
2.73514427896706,2.74569929646378,2.92071305421126,2.93943382978513,3.11857096684179,
3.13197658032393,3.25399179664495,3.45054278261475,3.62794535799811,3.64606212534864,
3.82474099483732,3.83698255062522,3.91347421315246),.UNSPECIFIED.) ;
#151 = B_SPLINE_CURVE_WITH_KNOTS('',3,(#105436,#105437,#105438,#105439,#105440,
#105441,#105442,#105443,#105444,#105445,#105446,#105447,#105448,#105449,
#105450,#105451,#105452,#105453,#105454,#105455,#105456,#105457,#105458,
#105459,#105460,#105461),.UNSPECIFIED.,.F.,.F.,(4,2,2,2,2,2,2,2,2,2,2,2,
4),(2.70344464881055,2.89144352771225,3.06851986332573,3.08081089074492,
3.26996664970766,3.35940092938473,3.5458754301802,3.72254345721718,3.73903833379462,
3.91570024693468,3.93052100184901,4.11735511986399,4.22222897897866),
 .UNSPECIFIED.) ;
#152 = B_SPLINE_CURVE_WITH_KNOTS('',3,(#105619,#105620,#105621,#105622,#105623,
#105624,#105625,#105626,#105627,#105628,#105629,#105630,#105631,#105632,
#105633,#105634,#105635,#105636,#105637),.UNSPECIFIED.,.F.,.F.,(4,3,3,3,
3,3,4),(2.81004151703333E-8,3.99307614181576E-5,8.00540716903473E-5,0.000126830846822484,
0.00017561819518642,0.00021519314047228,0.000245220898756746),
 .UNSPECIFIED.) ;
#153 = B_SPLINE_CURVE_WITH_KNOTS('',3,(#105660,#105661,#105662,#105663,#105664,
#105665,#105666,#105667,#105668,#105669,#105670,#105671,#105672,#105673,
#105674,#105675,#105676,#105677,#105678,#105679,#105680,#105681,#105682,
#105683,#105684,#105685,#105686,#105687,#105688,#105689,#105690,#105691,
#105692,#105693,#105694,#105695,#105696,#105697,#105698,#105699,#105700,
#105701,#105702,#105703,#105704,#105705,#105706,#105707,#105708,#105709,
#105710,#105711,#105712,#105713,#105714,#105715,#105716,#105717,#105718,
#105719,#105720,#105721,#105722,#105723,#105724,#105725,#105726,#105727,
#105728,#105729,#105730,#105731,#105732,#105733,#105734,#105735,#105736,
#105737,#105738),.UNSPECIFIED.,.F.,.F.,(4,3,3,3,3,3,3,3,3,3,3,3,3,3,3,3,
3,3,3,3,3,3,3,3,3,3,4),(0.000152038190191021,0.000154892841408471,0.000155160464960107,
0.000160456565729371,0.000163456795060821,0.000166580092246908,0.00016775132869169,
0.000168007536663986,0.000168255738137148,0.000169267315291303,0.000175949983805168,
0.000178959298271447,0.000180334649023613,0.000187987241670282,0.00019198121640859,
0.000193065528939067,0.00019383917426517,0.000198143816207851,0.000212206269476815,
0.000226582370019607,0.000228143757087823,0.000228729277238404,0.000232827918292471,
0.00024910943281953,0.00025017679744092,0.000265881325830107,0.000267525676589369),
 .UNSPECIFIED.) ;
#154 = B_SPLINE_CURVE_WITH_KNOTS('',3,(#105740,#105741,#105742,#105743,#105744,
#105745,#105746,#105747,#105748,#105749),.UNSPECIFIED.,.F.,.F.,(4,3,3,4),
(0.000130631741230759,0.000139067346352796,0.000143554831048674,0.000152038189371587),
 .UNSPECIFIED.) ;
#155 = B_SPLINE_CURVE_WITH_KNOTS('',3,(#105751,#105752,#105753,#105754,#105755,
#105756,#105757,#105758,#105759,#105760,#105761,#105762,#105763,#105764,
#105765,#105766,#105767,#105768,#105769),.UNSPECIFIED.,.F.,.F.,(4,3,3,3,
3,3,4),(0.000104137230127934,0.000110259474166471,0.000116844366893148,
0.000120664217590266,0.000125429508057305,0.000130430624030549,0.000130630877723017),
 .UNSPECIFIED.) ;
#156 = B_SPLINE_CURVE_WITH_KNOTS('',3,(#105770,#105771,#105772,#105773,#105774,
#105775,#105776,#105777,#105778,#105779,#105780,#105781,#105782,#105783,
#105784,#105785,#105786,#105787,#105788,#105789,#105790,#105791,#105792,
#105793,#105794,#105795,#105796,#105797,#105798,#105799,#105800,#105801,
#105802,#105803,#105804,#105805,#105806,#105807,#105808,#105809,#105810,
#105811,#105812),.UNSPECIFIED.,.F.,.F.,(4,3,3,3,3,3,3,3,3,3,3,3,3,3,4),
(0.,4.78421531964037E-6,1.59977421331184E-5,1.75965265774506E-5,2.6360366765448E-5,
3.75047088104788E-5,4.29655082836413E-5,5.3450780665109E-5,6.17416442237089E-5,
6.39360530465768E-5,7.32944438958948E-5,8.49065978095123E-5,9.46209320474951E-5,
9.66050857869684E-5,0.000104137229466949),.UNSPECIFIED.) ;
#157 = B_SPLINE_CURVE_WITH_KNOTS('',3,(#105882,#105883,#105884,#105885,#105886,
#105887,#105888,#105889,#105890,#105891,#105892,#105893,#105894,#105895,
#105896,#105897,#105898,#105899,#105900,#105901,#105902,#105903,#105904,
#105905,#105906,#105907,#105908,#105909,#105910,#105911,#105912,#105913,
#105914,#105915),.UNSPECIFIED.,.F.,.F.,(4,3,3,3,3,3,3,3,3,3,3,4),(0.000173579735006482,
0.000179152672590559,0.000187122196212438,0.000190349677855741,0.000201571576239487,
0.000207505544696553,0.000209082158340111,0.000218112358783938,0.000219837174422809,
0.000228512621317814,0.000240802935332003,0.000245138123631297),
 .UNSPECIFIED.) ;
#158 = B_SPLINE_CURVE_WITH_KNOTS('',3,(#105977,#105978,#105979,#105980,#105981,
#105982,#105983,#105984,#105985,#105986,#105987,#105988,#105989,#105990,
#105991,#105992),.UNSPECIFIED.,.F.,.F.,(4,3,3,3,3,4),(0.000149826268238821,
0.000156541783273878,0.000187447062839771,0.000218157419331144,0.000251253590119497,
0.000263630362845938),.UNSPECIFIED.) ;
#159 = B_SPLINE_CURVE_WITH_KNOTS('',3,(#105994,#105995,#105996,#105997),
 .UNSPECIFIED.,.F.,.F.,(4,4),(0.000128945525003057,0.000149826268238821),
 .UNSPECIFIED.) ;
#160 = B_SPLINE_CURVE_WITH_KNOTS('',3,(#105998,#105999,#106000,#106001,#106002,
#106003,#106004,#106005,#106006,#106007,#106008,#106009,#106010,#106011,
#106012,#106013),.UNSPECIFIED.,.F.,.F.,(4,3,3,3,3,4),(0.000107977862661221,
0.000113849696954291,0.00011675864089999,0.000123355930725607,0.000128649321338309,
0.000128945525003057),.UNSPECIFIED.) ;
#161 = B_SPLINE_CURVE_WITH_KNOTS('',3,(#106223,#106224,#106225,#106226,#106227,
#106228,#106229,#106230,#106231,#106232),.UNSPECIFIED.,.F.,.F.,(4,3,3,4),
(3.97436543900202E-15,3.94729529730262E-5,7.90727202189655E-5,0.000103003463696588),
 .UNSPECIFIED.) ;
#162 = B_SPLINE_CURVE_WITH_KNOTS('',3,(#106239,#106240,#106241,#106242,#106243,
#106244,#106245),.UNSPECIFIED.,.F.,.F.,(4,3,4),(0.000158223357507084,0.000179871364136752,
0.000191820073778124),.UNSPECIFIED.) ;
#163 = B_SPLINE_CURVE_WITH_KNOTS('',3,(#106260,#106261,#106262,#106263,#106264,
#106265,#106266,#106267,#106268,#106269,#106270,#106271,#106272,#106273,
#106274,#106275),.UNSPECIFIED.,.F.,.F.,(4,3,3,3,3,4),(2.25414513257385E-8,
3.7118138109435E-5,7.40234349159874E-5,0.000126639028433408,0.000171180683285943,
0.000173579731706481),.UNSPECIFIED.) ;
#164 = B_SPLINE_CURVE_WITH_KNOTS('',3,(#106331,#106332,#106333,#106334,#106335,
#106336),.UNSPECIFIED.,.F.,.F.,(4,2,4),(0.,0.000162685424844482,0.000325370849688964),
 .UNSPECIFIED.) ;
#165 = B_SPLINE_CURVE_WITH_KNOTS('',3,(#106339,#106340,#106341,#106342,#106343,
#106344),.UNSPECIFIED.,.F.,.F.,(4,2,4),(0.,0.000163438694679259,0.000326877389358518),
 .UNSPECIFIED.) ;
#166 = B_SPLINE_CURVE_WITH_KNOTS('',3,(#106355,#106356,#106357,#106358,#106359,
#106360),.UNSPECIFIED.,.F.,.F.,(4,2,4),(-0.00501427184001376,-0.00354643693242498,
0.),.UNSPECIFIED.) ;
#167 = B_SPLINE_CURVE_WITH_KNOTS('',3,(#106373,#106374,#106375,#106376,#106377,
#106378,#106379,#106380,#106381,#106382,#106383,#106384,#106385,#106386,
#106387,#106388,#106389,#106390,#106391,#106392,#106393,#106394,#106395,
#106396,#106397,#106398,#106399,#106400),.UNSPECIFIED.,.F.,.F.,(4,3,3,3,
3,3,3,3,3,4),(5.2381062129225E-9,5.84794260519105E-6,8.49662041781866E-6,
1.21937803558578E-5,1.76033670137842E-5,1.93092034273014E-5,2.55871453405162E-5,
3.0315421636347E-5,3.68519660350372E-5,3.92146766969318E-5),
 .UNSPECIFIED.) ;
#168 = B_SPLINE_CURVE_WITH_KNOTS('',3,(#106402,#106403,#106404,#106405,#106406,
#106407,#106408,#106409,#106410,#106411),.UNSPECIFIED.,.F.,.F.,(4,3,3,4),
(0.000144469795965457,0.000165397602015722,0.000173816468562375,0.000175865847906017),
 .UNSPECIFIED.) ;
#169 = B_SPLINE_CURVE_WITH_KNOTS('',3,(#106429,#106430,#106431,#106432,#106433,
#106434,#106435),.UNSPECIFIED.,.F.,.F.,(4,3,4),(-2.05331166617142E-6,2.04386714309068E-5,
3.1629985593225E-5),.UNSPECIFIED.) ;
#170 = B_SPLINE_CURVE_WITH_KNOTS('',3,(#106437,#106438,#106439,#106440,#106441,
#106442,#106443,#106444,#106445,#106446,#106447,#106448),.UNSPECIFIED.,
 .F.,.F.,(4,2,2,2,2,4),(9.00279624299152E-9,0.00183032786957268,0.006077465667517,
0.0169681635237984,0.0216775196496615,0.0254454421850849),.UNSPECIFIED.) ;
#171 = B_SPLINE_CURVE_WITH_KNOTS('',3,(#106607,#106608,#106609,#106610,#106611,
#106612,#106613,#106614,#106615,#106616,#106617,#106618,#106619,#106620,
#106621,#106622,#106623,#106624,#106625,#106626,#106627,#106628,#106629,
#106630,#106631,#106632,#106633,#106634,#106635,#106636,#106637,#106638,
#106639,#106640,#106641,#106642,#106643,#106644,#106645,#106646),
 .UNSPECIFIED.,.F.,.F.,(4,3,3,3,3,3,3,3,3,3,3,3,3,4),(0.,5.07173230218452E-5,
0.00010401741348744,0.000124506719166651,0.000125249568192438,0.000156566023859653,
0.000186760078749975,0.000187880030991798,0.000203537318084809,0.000211366035547463,
0.000217886758541637,0.000219194644848643,0.000234851354133269,0.000249013438333299),
 .UNSPECIFIED.) ;
#172 = B_SPLINE_CURVE_WITH_KNOTS('',3,(#106652,#106653,#106654,#106655,#106656,
#106657,#106658,#106659,#106660,#106661,#106662,#106663,#106664,#106665,
#106666,#106667,#106668,#106669,#106670,#106671,#106672,#106673,#106674,
#106675,#106676,#106677,#106678,#106679,#106680,#106681,#106682,#106683,
#106684,#106685,#106686,#106687,#106688,#106689,#106690,#106691),
 .UNSPECIFIED.,.F.,.F.,(4,3,3,3,3,3,3,3,3,3,3,3,3,4),(0.,1.4311556709258E-5,
3.01335133960352E-5,3.14552036774726E-5,3.80447517297281E-5,4.59561222518464E-5,
6.17788922892798E-5,6.29104073549452E-5,9.34210966965093E-5,0.000125066393795483,
0.000125820814709883,0.000179837268173055,0.000231469985679291,0.000251641629419759),
 .UNSPECIFIED.) ;
#173 = B_SPLINE_CURVE_WITH_KNOTS('',3,(#106696,#106697,#106698,#106699,#106700,
#106701,#106702),.UNSPECIFIED.,.F.,.F.,(4,3,4),(-2.04939766627128E-6,0.,
2.93835791072157E-5),.UNSPECIFIED.) ;
#174 = B_SPLINE_CURVE_WITH_KNOTS('',3,(#106717,#106718,#106719,#106720,#106721,
#106722,#106723,#106724,#106725,#106726,#106727,#106728,#106729,#106730),
 .UNSPECIFIED.,.F.,.F.,(4,2,2,2,2,2,4),(1.44901762686856E-6,0.000561621523786212,
0.00112173034325288,0.00210338619152427,0.00384452539434926,0.00473112295079285,
0.00541108585487423),.UNSPECIFIED.) ;
#175 = B_SPLINE_CURVE_WITH_KNOTS('',3,(#106739,#106740,#106741,#106742,#106743,
#106744,#106745,#106746,#106747,#106748,#106749,#106750,#106751,#106752,
#106753,#106754,#106755,#106756,#106757,#106758,#106759,#106760,#106761,
#106762,#106763,#106764,#106765,#106766,#106767,#106768,#106769,#106770,
#106771,#106772),.UNSPECIFIED.,.F.,.F.,(4,2,2,2,2,2,2,2,2,2,2,2,2,2,2,2,
4),(0.,1.6752889417125E-5,3.36326639084849E-5,3.53285003632986E-5,3.67766442982582E-5,
4.4593687750131E-5,5.25629171995868E-5,5.37833548715131E-5,5.51649664473856E-5,
7.22376444476005E-5,7.35532885965131E-5,0.000109240736296885,0.000146228640921016,
0.000147106577193024,0.000203359192940443,0.000258123601934358,0.000294213154386043),
 .UNSPECIFIED.) ;
#176 = B_SPLINE_CURVE_WITH_KNOTS('',3,(#106776,#106777,#106778,#106779,#106780,
#106781,#106782,#106783,#106784,#106785,#106786,#106787,#106788,#106789,
#106790,#106791,#106792,#106793,#106794,#106795,#106796,#106797,#106798,
#106799,#106800,#106801,#106802,#106803,#106804,#106805,#106806,#106807,
#106808,#106809,#106810,#106811,#106812,#106813,#106814,#106815,#106816,
#106817,#106818,#106819,#106820,#106821,#106822,#106823,#106824,#106825,
#106826,#106827),.UNSPECIFIED.,.F.,.F.,(4,3,3,3,3,3,3,3,3,3,3,3,3,3,3,3,
3,4),(0.,5.28180786064093E-5,0.000107888430271973,0.000143209193858987,
0.00014407824218072,0.000180086811859619,0.00021481379078848,0.00021545817026355,
0.00021610254973862,0.000232714940020853,0.000234106492510808,0.000238605983992193,
0.000240855729732885,0.000243105475473578,0.000250616089253225,0.000252108710851782,
0.000270124214172477,0.000286418387717971),.UNSPECIFIED.) ;
#177 = B_SPLINE_CURVE_WITH_KNOTS('',3,(#106972,#106973,#106974,#106975,#106976,
#106977,#106978,#106979),.UNSPECIFIED.,.F.,.F.,(4,2,2,4),(-0.0473604779370388,
-0.0461995546884437,-0.0447198409510955,-0.0410407833884838),
 .UNSPECIFIED.) ;
#178 = B_SPLINE_CURVE_WITH_KNOTS('',3,(#106987,#106988,#106989,#106990,#106991,
#106992,#106993,#106994),.UNSPECIFIED.,.F.,.F.,(4,2,2,4),(-0.0536801724855783,
-0.0500011149229821,-0.0485214011856339,-0.0473604779370387),
 .UNSPECIFIED.) ;
#179 = B_SPLINE_CURVE_WITH_KNOTS('',3,(#107448,#107449,#107450,#107451,#107452,
#107453,#107454,#107455,#107456,#107457,#107458,#107459,#107460,#107461),
 .UNSPECIFIED.,.F.,.F.,(4,2,2,2,2,2,4),(4.71238898038469,4.88175806245169,
5.06763701998897,5.24337922960769,5.26451333208202,5.44874090582883,5.49822830854825),
 .UNSPECIFIED.) ;
#180 = B_SPLINE_CURVE_WITH_KNOTS('',3,(#107466,#107467,#107468,#107469,#107470,
#107471,#107472,#107473,#107474,#107475,#107476,#107477,#107478,#107479),
 .UNSPECIFIED.,.F.,.F.,(4,2,2,2,2,2,4),(0.784956998631304,0.966941694312144,
1.14311721221009,1.16348181627612,1.34745079132841,1.51752882030647,1.5707963267949),
 .UNSPECIFIED.) ;
#181 = B_SPLINE_CURVE_WITH_KNOTS('',3,(#107485,#107486,#107487,#107488,#107489,
#107490,#107491,#107492,#107493,#107494,#107495,#107496,#107497,#107498),
 .UNSPECIFIED.,.F.,.F.,(4,2,2,2,2,2,4),(0.784956998631347,0.966941694312202,
1.1431172121312,1.16348181627609,1.34745079132826,1.51752882030624,1.5707963267949),
 .UNSPECIFIED.) ;
#182 = B_SPLINE_CURVE_WITH_KNOTS('',3,(#107500,#107501,#107502,#107503,#107504,
#107505,#107506,#107507,#107508,#107509,#107510,#107511,#107512,#107513),
 .UNSPECIFIED.,.F.,.F.,(4,2,2,2,2,2,4),(4.71238898038469,4.88175806245171,
5.06763701998877,5.24337922965479,5.26451333208194,5.44874090582893,5.49822830854826),
 .UNSPECIFIED.) ;
#183 = B_SPLINE_CURVE_WITH_KNOTS('',3,(#107517,#107518,#107519,#107520,#107521,
#107522,#107523,#107524,#107525,#107526,#107527,#107528,#107529,#107530),
 .UNSPECIFIED.,.F.,.F.,(4,2,2,2,2,2,4),(4.71238898038469,4.88175806245169,
5.06763701998911,5.2433792296566,5.26451333208232,5.44874090582905,5.49822830854824),
 .UNSPECIFIED.) ;
#184 = B_SPLINE_CURVE_WITH_KNOTS('',3,(#107534,#107535,#107536,#107537,#107538,
#107539,#107540,#107541,#107542,#107543,#107544,#107545,#107546,#107547),
 .UNSPECIFIED.,.F.,.F.,(4,2,2,2,2,2,4),(0.784956998631345,0.966941694311759,
1.14311721212769,1.16348181627571,1.34745079132821,1.5175288203063,1.5707963267949),
 .UNSPECIFIED.) ;
#185 = B_SPLINE_CURVE_WITH_KNOTS('',3,(#107562,#107563,#107564,#107565,#107566,
#107567,#107568,#107569,#107570,#107571,#107572,#107573,#107574,#107575),
 .UNSPECIFIED.,.F.,.F.,(4,2,2,2,2,2,4),(0.784956998631335,0.966941694312017,
1.14311721212471,1.16348181627591,1.34745079132842,1.5175288203063,1.5707963267949),
 .UNSPECIFIED.) ;
#186 = B_SPLINE_CURVE_WITH_KNOTS('',3,(#107579,#107580,#107581,#107582,#107583,
#107584,#107585,#107586,#107587,#107588,#107589,#107590,#107591,#107592),
 .UNSPECIFIED.,.F.,.F.,(4,2,2,2,2,2,4),(4.71238898038469,4.88175806245169,
5.06763701998889,5.24337922965042,5.26451333208206,5.44874090582913,5.49822830854829),
 .UNSPECIFIED.) ;
#187 = B_SPLINE_CURVE_WITH_KNOTS('',3,(#107697,#107698,#107699,#107700,#107701,
#107702,#107703,#107704,#107705,#107706,#107707,#107708,#107709,#107710,
#107711,#107712),.UNSPECIFIED.,.F.,.F.,(4,3,3,3,3,4),(0.,3.26760986414935E-5,
6.60604127813372E-5,0.00010113572426573,0.000138237800333083,0.000166242991827321),
 .UNSPECIFIED.) ;
#188 = B_SPLINE_CURVE_WITH_KNOTS('',3,(#107774,#107775,#107776,#107777,#107778,
#107779,#107780,#107781,#107782,#107783,#107784,#107785,#107786,#107787,
#107788,#107789),.UNSPECIFIED.,.F.,.F.,(4,3,3,3,3,4),(0.,1.86901632150156E-5,
5.38940239621536E-5,9.1325545181693E-5,0.00012977596605383,0.000168373497604197),
 .UNSPECIFIED.) ;
#189 = B_SPLINE_CURVE_WITH_KNOTS('',3,(#107794,#107795,#107796,#107797,#107798,
#107799,#107800,#107801,#107802,#107803),.UNSPECIFIED.,.F.,.F.,(4,2,2,2,
4),(0.0288531015833118,0.0296205843603292,0.0328031056847702,0.0376042554655217,
0.0407130021481444),.UNSPECIFIED.) ;
#190 = B_SPLINE_CURVE_WITH_KNOTS('',3,(#107808,#107809,#107810,#107811,#107812,
#107813),.UNSPECIFIED.,.F.,.F.,(4,2,4),(0.0637474840407795,0.0675088661482764,
0.0720284409638634),.UNSPECIFIED.) ;
#191 = B_SPLINE_CURVE_WITH_KNOTS('',3,(#107819,#107820,#107821,#107822,#107823,
#107824,#107825,#107826,#107827,#107828),.UNSPECIFIED.,.F.,.F.,(4,2,2,2,
4),(0.0767275662236361,0.0771734766301334,0.0818220866832597,0.0868722195332896,
0.0892832637324438),.UNSPECIFIED.) ;
#192 = B_SPLINE_CURVE_WITH_KNOTS('',3,(#107863,#107864,#107865,#107866,#107867,
#107868),.UNSPECIFIED.,.F.,.F.,(4,2,4),(0.171679973605268,0.17870747594849,
0.186889989700107),.UNSPECIFIED.) ;
#193 = B_SPLINE_CURVE_WITH_KNOTS('',3,(#107908,#107909,#107910,#107911,#107912,
#107913,#107914,#107915,#107916,#107917,#107918,#107919,#107920,#107921,
#107922,#107923,#107924,#107925,#107926,#107927,#107928,#107929,#107930,
#107931,#107932,#107933,#107934,#107935,#107936,#107937),.UNSPECIFIED.,
 .F.,.F.,(4,2,2,2,2,2,2,2,2,2,2,2,2,2,4),(2.36970964942748,2.55498029688296,
2.73514427897508,2.74569929646384,2.92071305423067,2.9394338297853,3.11857096686515,
3.13197658032419,3.25399179664505,3.450542782615,3.62794535799348,3.64606212534887,
3.82474099482299,3.83698255062533,3.9134742131517),.UNSPECIFIED.) ;
#194 = B_SPLINE_CURVE_WITH_KNOTS('',3,(#107948,#107949,#107950,#107951,#107952,
#107953,#107954,#107955,#107956,#107957,#107958,#107959,#107960,#107961,
#107962,#107963,#107964,#107965,#107966,#107967,#107968,#107969,#107970,
#107971,#107972,#107973),.UNSPECIFIED.,.F.,.F.,(4,2,2,2,2,2,2,2,2,2,2,2,
4),(2.70344464881042,2.89144352771213,3.06851986339517,3.0808108907447,
3.26996664970742,3.35940092938473,3.54587543017995,3.72254345721779,3.73903833379426,
3.91570024691714,3.93052100184844,4.11735511986315,4.22222897897866),
 .UNSPECIFIED.) ;
#195 = B_SPLINE_CURVE_WITH_KNOTS('',3,(#108131,#108132,#108133,#108134,#108135,
#108136,#108137,#108138,#108139,#108140,#108141,#108142,#108143,#108144,
#108145,#108146,#108147,#108148,#108149),.UNSPECIFIED.,.F.,.F.,(4,3,3,3,
3,3,4),(2.81004151523444E-8,3.99307614181576E-5,8.00540716903464E-5,0.000126830846822483,
0.000175618195186419,0.000215193140472279,0.00024522089875675),
 .UNSPECIFIED.) ;
#196 = B_SPLINE_CURVE_WITH_KNOTS('',3,(#108172,#108173,#108174,#108175,#108176,
#108177,#108178,#108179,#108180,#108181,#108182,#108183,#108184,#108185,
#108186,#108187,#108188,#108189,#108190,#108191,#108192,#108193,#108194,
#108195,#108196,#108197,#108198,#108199,#108200,#108201,#108202,#108203,
#108204,#108205,#108206,#108207,#108208,#108209,#108210,#108211,#108212,
#108213,#108214,#108215,#108216,#108217,#108218,#108219,#108220,#108221,
#108222,#108223,#108224,#108225,#108226,#108227,#108228,#108229,#108230,
#108231,#108232,#108233,#108234,#108235,#108236,#108237,#108238,#108239,
#108240,#108241,#108242,#108243,#108244,#108245,#108246,#108247,#108248,
#108249,#108250),.UNSPECIFIED.,.F.,.F.,(4,3,3,3,3,3,3,3,3,3,3,3,3,3,3,3,
3,3,3,3,3,3,3,3,3,3,4),(0.000152038190191199,0.000154892841408555,0.000155160464960188,
0.000160456565729593,0.000163456795060823,0.000166580092246912,0.000167751328691695,
0.000168007536663992,0.000168255738137154,0.000169267315291292,0.000175949983805179,
0.000178959298271457,0.000180334649023622,0.000187987241670289,0.000191981216408587,
0.000193065528939071,0.000193839174265175,0.000198143816207854,0.000212206269476809,
0.000226582370019589,0.00022814375708781,0.000228729277238393,0.000232827918292474,
0.000249109432810095,0.000250176797440924,0.000265881325831287,0.000267525676589373),
 .UNSPECIFIED.) ;
#197 = B_SPLINE_CURVE_WITH_KNOTS('',3,(#108252,#108253,#108254,#108255,#108256,
#108257,#108258,#108259,#108260,#108261),.UNSPECIFIED.,.F.,.F.,(4,3,3,4),
(0.000130631741230765,0.000139067346353096,0.000143554831048713,0.000152038189371763),
 .UNSPECIFIED.) ;
#198 = B_SPLINE_CURVE_WITH_KNOTS('',3,(#108263,#108264,#108265,#108266,#108267,
#108268,#108269,#108270,#108271,#108272,#108273,#108274,#108275,#108276,
#108277,#108278,#108279,#108280,#108281),.UNSPECIFIED.,.F.,.F.,(4,3,3,3,
3,3,4),(0.000104137230128489,0.000110259474166938,0.000116844366893606,
0.00012066421759078,0.000125429508057306,0.000130430624030732,0.000130630877723054),
 .UNSPECIFIED.) ;
#199 = B_SPLINE_CURVE_WITH_KNOTS('',3,(#108282,#108283,#108284,#108285,#108286,
#108287,#108288,#108289,#108290,#108291,#108292,#108293,#108294,#108295,
#108296,#108297,#108298,#108299,#108300,#108301,#108302,#108303,#108304,
#108305,#108306,#108307,#108308,#108309,#108310,#108311,#108312,#108313,
#108314,#108315,#108316,#108317,#108318,#108319,#108320,#108321,#108322,
#108323,#108324),.UNSPECIFIED.,.F.,.F.,(4,3,3,3,3,3,3,3,3,3,3,3,3,3,4),
(0.,4.78421531964207E-6,1.5997742133728E-5,1.75965265776594E-5,2.63603667652772E-5,
3.75047088100453E-5,4.29655082836422E-5,5.34507806651101E-5,6.17416442235669E-5,
6.39360530465779E-5,7.32944438965259E-5,8.49065978095135E-5,9.46209320476381E-5,
9.66050857869696E-5,0.000104137229467517),.UNSPECIFIED.) ;
#200 = B_SPLINE_CURVE_WITH_KNOTS('',3,(#108394,#108395,#108396,#108397,#108398,
#108399,#108400,#108401,#108402,#108403,#108404,#108405,#108406,#108407,
#108408,#108409,#108410,#108411,#108412,#108413,#108414,#108415,#108416,
#108417,#108418,#108419,#108420,#108421,#108422,#108423,#108424,#108425,
#108426,#108427),.UNSPECIFIED.,.F.,.F.,(4,3,3,3,3,3,3,3,3,3,3,4),(0.00017357973500648,
0.000179152672590604,0.000187122196212524,0.000190349677855844,0.000201571576239683,
0.000207505544696743,0.00020908215834011,0.000218112358783795,0.000219837174422841,
0.000228512621317681,0.00024080293533128,0.000245138123631291),
 .UNSPECIFIED.) ;
#201 = B_SPLINE_CURVE_WITH_KNOTS('',3,(#108489,#108490,#108491,#108492,#108493,
#108494,#108495,#108496,#108497,#108498,#108499,#108500,#108501,#108502,
#108503,#108504),.UNSPECIFIED.,.F.,.F.,(4,3,3,3,3,4),(0.000149826268238863,
0.000156541783273878,0.000187447062839773,0.000218157419331147,0.0002512535901195,
0.000263630362845944),.UNSPECIFIED.) ;
#202 = B_SPLINE_CURVE_WITH_KNOTS('',3,(#108506,#108507,#108508,#108509),
 .UNSPECIFIED.,.F.,.F.,(4,4),(0.00012894552500308,0.000149826268238863),
 .UNSPECIFIED.) ;
#203 = B_SPLINE_CURVE_WITH_KNOTS('',3,(#108510,#108511,#108512,#108513,#108514,
#108515,#108516,#108517,#108518,#108519,#108520,#108521,#108522,#108523,
#108524,#108525),.UNSPECIFIED.,.F.,.F.,(4,3,3,3,3,4),(0.000107977862661225,
0.000113849696954203,0.00011675864089999,0.000123355930725642,0.000128649321338296,
0.00012894552500308),.UNSPECIFIED.) ;
#204 = B_SPLINE_CURVE_WITH_KNOTS('',3,(#108735,#108736,#108737,#108738,#108739,
#108740,#108741,#108742,#108743,#108744),.UNSPECIFIED.,.F.,.F.,(4,3,3,4),
(3.97436543900202E-15,3.94729529730262E-5,7.90727202189655E-5,0.000103003463696568),
 .UNSPECIFIED.) ;
#205 = B_SPLINE_CURVE_WITH_KNOTS('',3,(#108751,#108752,#108753,#108754,#108755,
#108756,#108757),.UNSPECIFIED.,.F.,.F.,(4,3,4),(0.000158223357507064,0.000179871364136604,
0.000191820073778122),.UNSPECIFIED.) ;
#206 = B_SPLINE_CURVE_WITH_KNOTS('',3,(#108772,#108773,#108774,#108775,#108776,
#108777,#108778,#108779,#108780,#108781,#108782,#108783,#108784,#108785,
#108786,#108787),.UNSPECIFIED.,.F.,.F.,(4,3,3,3,3,4),(2.25414513247713E-8,
3.7118138109435E-5,7.40234349159874E-5,0.000126639028433408,0.000171180683285943,
0.000173579731706481),.UNSPECIFIED.) ;
#207 = B_SPLINE_CURVE_WITH_KNOTS('',3,(#108843,#108844,#108845,#108846,#108847,
#108848),.UNSPECIFIED.,.F.,.F.,(4,2,4),(0.,0.000162685424844483,0.000325370849688965),
 .UNSPECIFIED.) ;
#208 = B_SPLINE_CURVE_WITH_KNOTS('',3,(#108851,#108852,#108853,#108854,#108855,
#108856),.UNSPECIFIED.,.F.,.F.,(4,2,4),(0.,0.000163438694679259,0.000326877389358518),
 .UNSPECIFIED.) ;
#209 = B_SPLINE_CURVE_WITH_KNOTS('',3,(#108867,#108868,#108869,#108870,#108871,
#108872),.UNSPECIFIED.,.F.,.F.,(4,2,4),(-0.00501427184001376,-0.00354643693242498,
0.),.UNSPECIFIED.) ;
#210 = B_SPLINE_CURVE_WITH_KNOTS('',3,(#108885,#108886,#108887,#108888,#108889,
#108890,#108891,#108892,#108893,#108894,#108895,#108896,#108897,#108898,
#108899,#108900,#108901,#108902,#108903,#108904,#108905,#108906,#108907,
#108908,#108909,#108910,#108911,#108912),.UNSPECIFIED.,.F.,.F.,(4,3,3,3,
3,3,3,3,3,4),(5.23810621265401E-9,5.84794260519711E-6,8.49662041781891E-6,
1.21937803558104E-5,1.76033670136906E-5,1.93092034273021E-5,2.55871453406251E-5,
3.0315421636348E-5,3.68519660352467E-5,3.92146766969314E-5),
 .UNSPECIFIED.) ;
#211 = B_SPLINE_CURVE_WITH_KNOTS('',3,(#108914,#108915,#108916,#108917,#108918,
#108919,#108920,#108921,#108922,#108923),.UNSPECIFIED.,.F.,.F.,(4,3,3,4),
(0.000144469795965455,0.000165397602015376,0.000173816468562374,0.000175865847906018),
 .UNSPECIFIED.) ;
#212 = B_SPLINE_CURVE_WITH_KNOTS('',3,(#108941,#108942,#108943,#108944,#108945,
#108946,#108947),.UNSPECIFIED.,.F.,.F.,(4,3,4),(-2.05331166616594E-6,2.04386714314149E-5,
3.16299855932266E-5),.UNSPECIFIED.) ;
#213 = B_SPLINE_CURVE_WITH_KNOTS('',3,(#108949,#108950,#108951,#108952,#108953,
#108954,#108955,#108956,#108957,#108958,#108959,#108960),.UNSPECIFIED.,
 .F.,.F.,(4,2,2,2,2,4),(9.00279528345874E-9,0.00183032786964776,0.00607746566718187,
0.0169681635075991,0.0216775196267783,0.0254454421566977),.UNSPECIFIED.) ;
#214 = B_SPLINE_CURVE_WITH_KNOTS('',3,(#109119,#109120,#109121,#109122,#109123,
#109124,#109125,#109126,#109127,#109128,#109129,#109130,#109131,#109132,
#109133,#109134,#109135,#109136,#109137,#109138,#109139,#109140,#109141,
#109142,#109143,#109144,#109145,#109146,#109147,#109148,#109149,#109150,
#109151,#109152,#109153,#109154,#109155,#109156,#109157,#109158),
 .UNSPECIFIED.,.F.,.F.,(4,3,3,3,3,3,3,3,3,3,3,3,3,4),(0.,5.0717323028302E-5,
0.00010401741350107,0.00012450671916665,0.000125249568192411,0.000156566023859649,
0.000186760078749971,0.000187880030991799,0.000203537318084808,0.000211366035547462,
0.000217886758541633,0.000219194644848641,0.000234851354133266,0.000249013438333296),
 .UNSPECIFIED.) ;
#215 = B_SPLINE_CURVE_WITH_KNOTS('',3,(#109164,#109165,#109166,#109167,#109168,
#109169,#109170,#109171,#109172,#109173,#109174,#109175,#109176,#109177,
#109178,#109179,#109180,#109181,#109182,#109183,#109184,#109185,#109186,
#109187,#109188,#109189,#109190,#109191,#109192,#109193,#109194,#109195,
#109196,#109197,#109198,#109199,#109200,#109201,#109202,#109203),
 .UNSPECIFIED.,.F.,.F.,(4,3,3,3,3,3,3,3,3,3,3,3,3,4),(0.,1.43115567092591E-5,
3.01335133960395E-5,3.14552036774756E-5,3.80447517297363E-5,4.59561222518582E-5,
6.17788922892867E-5,6.29104073549512E-5,9.34210966965043E-5,0.00012506639379551,
0.00012582081470991,0.000179837268177068,0.000231469985686737,0.00025164162941983),
 .UNSPECIFIED.) ;
#216 = B_SPLINE_CURVE_WITH_KNOTS('',3,(#109208,#109209,#109210,#109211,#109212,
#109213,#109214),.UNSPECIFIED.,.F.,.F.,(4,3,4),(-2.04939766627128E-6,0.,
2.93835791072157E-5),.UNSPECIFIED.) ;
#217 = B_SPLINE_CURVE_WITH_KNOTS('',3,(#109229,#109230,#109231,#109232,#109233,
#109234,#109235,#109236,#109237,#109238,#109239,#109240,#109241,#109242),
 .UNSPECIFIED.,.F.,.F.,(4,2,2,2,2,2,4),(1.44901763072086E-6,0.000561621523748031,
0.00112173034319911,0.00210338619150003,0.00384452539461507,0.00473112295159275,
0.00541108585601945),.UNSPECIFIED.) ;
#218 = B_SPLINE_CURVE_WITH_KNOTS('',3,(#109251,#109252,#109253,#109254,#109255,
#109256,#109257,#109258,#109259,#109260,#109261,#109262,#109263,#109264,
#109265,#109266,#109267,#109268,#109269,#109270,#109271,#109272,#109273,
#109274,#109275,#109276,#109277,#109278,#109279,#109280,#109281,#109282,
#109283,#109284),.UNSPECIFIED.,.F.,.F.,(4,2,2,2,2,2,2,2,2,2,2,2,2,2,2,2,
4),(0.,1.67528894171495E-5,3.36326639089867E-5,3.5328500363345E-5,3.67766442982523E-5,
4.45936877501694E-5,5.25629171990832E-5,5.37833548715101E-5,5.51649664473801E-5,
7.22376444475638E-5,7.35532885965079E-5,0.00010924073629687,0.000146228640921011,
0.000147106577193012,0.000203359192943554,0.000258123601940488,0.00029421315438602),
 .UNSPECIFIED.) ;
#219 = B_SPLINE_CURVE_WITH_KNOTS('',3,(#109288,#109289,#109290,#109291,#109292,
#109293,#109294,#109295,#109296,#109297,#109298,#109299,#109300,#109301,
#109302,#109303,#109304,#109305,#109306,#109307,#109308,#109309,#109310,
#109311,#109312,#109313,#109314,#109315,#109316,#109317,#109318,#109319,
#109320,#109321,#109322,#109323,#109324,#109325,#109326,#109327,#109328,
#109329,#109330,#109331,#109332,#109333,#109334,#109335,#109336,#109337,
#109338,#109339),.UNSPECIFIED.,.F.,.F.,(4,3,3,3,3,3,3,3,3,3,3,3,3,3,3,3,
3,4),(0.,5.28180786069338E-5,0.00010788843027313,0.000143209193858996,0.000144078242180727,
0.000180086811859628,0.000214813790788495,0.000215458170263561,0.000216102549738628,
0.000232714940020866,0.000234106492510818,0.000238605983992203,0.000240855729732896,
0.000243105475473589,0.000250616089253237,0.000252108710851791,0.000270124214172479,
0.000286418387717971),.UNSPECIFIED.) ;
#220 = B_SPLINE_CURVE_WITH_KNOTS('',3,(#109484,#109485,#109486,#109487,#109488,
#109489,#109490,#109491),.UNSPECIFIED.,.F.,.F.,(4,2,2,4),(-0.0473604779370388,
-0.0461995546884437,-0.0447198409510955,-0.0410407833884838),
 .UNSPECIFIED.) ;
#221 = B_SPLINE_CURVE_WITH_KNOTS('',3,(#109499,#109500,#109501,#109502,#109503,
#109504,#109505,#109506),.UNSPECIFIED.,.F.,.F.,(4,2,2,4),(-0.0536801724855779,
-0.0500011149229821,-0.048521401185634,-0.0473604779370388),
 .UNSPECIFIED.) ;
#222 = B_SPLINE_CURVE_WITH_KNOTS('',3,(#109960,#109961,#109962,#109963,#109964,
#109965,#109966,#109967,#109968,#109969,#109970,#109971,#109972,#109973),
 .UNSPECIFIED.,.F.,.F.,(4,2,2,2,2,2,4),(4.71238898038469,4.88175806245107,
5.06763701998695,5.2433792296077,5.26451333207962,5.44874090582719,5.49822830854814),
 .UNSPECIFIED.) ;
#223 = B_SPLINE_CURVE_WITH_KNOTS('',3,(#109978,#109979,#109980,#109981,#109982,
#109983,#109984,#109985,#109986,#109987,#109988,#109989,#109990,#109991),
 .UNSPECIFIED.,.F.,.F.,(4,2,2,2,2,2,4),(0.784956998631454,0.966941694311884,
1.1431172121161,1.16348181627568,1.34745079132797,1.51752882030577,1.5707963267949),
 .UNSPECIFIED.) ;
#224 = B_SPLINE_CURVE_WITH_KNOTS('',3,(#109997,#109998,#109999,#110000,#110001,
#110002,#110003,#110004,#110005,#110006,#110007,#110008,#110009,#110010),
 .UNSPECIFIED.,.F.,.F.,(4,2,2,2,2,2,4),(0.78495699863135,0.966941694311801,
1.14311721212949,1.16348181627581,1.34745079132849,1.51752882030664,1.5707963267949),
 .UNSPECIFIED.) ;
#225 = B_SPLINE_CURVE_WITH_KNOTS('',3,(#110012,#110013,#110014,#110015,#110016,
#110017,#110018,#110019,#110020,#110021,#110022,#110023,#110024,#110025),
 .UNSPECIFIED.,.F.,.F.,(4,2,2,2,2,2,4),(4.71238898038469,4.8817580624516,
5.06763701998866,5.24337922965485,5.26451333208181,5.44874090582897,5.49822830854826),
 .UNSPECIFIED.) ;
#226 = B_SPLINE_CURVE_WITH_KNOTS('',3,(#110029,#110030,#110031,#110032,#110033,
#110034,#110035,#110036,#110037,#110038,#110039,#110040,#110041,#110042),
 .UNSPECIFIED.,.F.,.F.,(4,2,2,2,2,2,4),(4.71238898038469,4.88175806245179,
5.06763701998917,5.24337922965321,5.26451333208237,5.44874090582905,5.49822830854822),
 .UNSPECIFIED.) ;
#227 = B_SPLINE_CURVE_WITH_KNOTS('',3,(#110046,#110047,#110048,#110049,#110050,
#110051,#110052,#110053,#110054,#110055,#110056,#110057,#110058,#110059),
 .UNSPECIFIED.,.F.,.F.,(4,2,2,2,2,2,4),(0.784956998631211,0.966941694311843,
1.14311721213428,1.16348181627569,1.3474507913286,1.51752882030718,1.5707963267949),
 .UNSPECIFIED.) ;
#228 = B_SPLINE_CURVE_WITH_KNOTS('',3,(#110074,#110075,#110076,#110077,#110078,
#110079,#110080,#110081,#110082,#110083,#110084,#110085,#110086,#110087),
 .UNSPECIFIED.,.F.,.F.,(4,2,2,2,2,2,4),(0.784956998631298,0.966941694311769,
1.14311721211431,1.1634818162758,1.3474507913284,1.51752882030656,1.5707963267949),
 .UNSPECIFIED.) ;
#229 = B_SPLINE_CURVE_WITH_KNOTS('',3,(#110091,#110092,#110093,#110094,#110095,
#110096,#110097,#110098,#110099,#110100,#110101,#110102,#110103,#110104),
 .UNSPECIFIED.,.F.,.F.,(4,2,2,2,2,2,4),(4.71238898038469,4.88175806245195,
5.06763701998927,5.24337922961088,5.26451333208257,5.44874090582964,5.49822830854831),
 .UNSPECIFIED.) ;
#230 = B_SPLINE_CURVE_WITH_KNOTS('',3,(#110209,#110210,#110211,#110212,#110213,
#110214,#110215,#110216,#110217,#110218,#110219,#110220,#110221,#110222,
#110223,#110224),.UNSPECIFIED.,.F.,.F.,(4,3,3,3,3,4),(0.,3.26760986414938E-5,
6.60604127813367E-5,0.000101135724265729,0.00013823780033308,0.00016624299182732),
 .UNSPECIFIED.) ;
#231 = B_SPLINE_CURVE_WITH_KNOTS('',3,(#110286,#110287,#110288,#110289,#110290,
#110291,#110292,#110293,#110294,#110295,#110296,#110297,#110298,#110299,
#110300,#110301),.UNSPECIFIED.,.F.,.F.,(4,3,3,3,3,4),(0.,1.86901632150156E-5,
5.38940239621536E-5,9.1325545181693E-5,0.00012977596605383,0.000168373497604197),
 .UNSPECIFIED.) ;
#232 = B_SPLINE_CURVE_WITH_KNOTS('',3,(#110306,#110307,#110308,#110309,#110310,
#110311,#110312,#110313,#110314,#110315),.UNSPECIFIED.,.F.,.F.,(4,2,2,2,
4),(0.0288531015809221,0.0296205843578462,0.0328031056819848,0.0376042554623528,
0.0407130021448623),.UNSPECIFIED.) ;
#233 = B_SPLINE_CURVE_WITH_KNOTS('',3,(#110320,#110321,#110322,#110323,#110324,
#110325),.UNSPECIFIED.,.F.,.F.,(4,2,4),(0.0637474840407795,0.0675088661482764,
0.0720284409638635),.UNSPECIFIED.) ;
#234 = B_SPLINE_CURVE_WITH_KNOTS('',3,(#110331,#110332,#110333,#110334,#110335,
#110336,#110337,#110338,#110339,#110340),.UNSPECIFIED.,.F.,.F.,(4,2,2,2,
4),(0.0767275662269652,0.0771734766335448,0.0818220866869972,0.0868722195372896,
0.0892832637365362),.UNSPECIFIED.) ;
#235 = B_SPLINE_CURVE_WITH_KNOTS('',3,(#110375,#110376,#110377,#110378,#110379,
#110380),.UNSPECIFIED.,.F.,.F.,(4,2,4),(0.171679973605596,0.178707475948804,
0.186889989700405),.UNSPECIFIED.) ;
#236 = B_SPLINE_CURVE_WITH_KNOTS('',3,(#110420,#110421,#110422,#110423,#110424,
#110425,#110426,#110427,#110428,#110429,#110430,#110431,#110432,#110433,
#110434,#110435,#110436,#110437,#110438,#110439,#110440,#110441,#110442,
#110443,#110444,#110445,#110446,#110447,#110448,#110449),.UNSPECIFIED.,
 .F.,.F.,(4,2,2,2,2,2,2,2,2,2,2,2,2,2,4),(2.36970964942748,2.55498029688329,
2.73514427898821,2.74569929646429,2.92071305420847,2.93943382978577,3.11857096685307,
3.13197658032462,3.25399179664507,3.45054278261492,3.62794535799599,3.64606212534882,
3.82474099482791,3.83698255062549,3.91347421315166),.UNSPECIFIED.) ;
#237 = B_SPLINE_CURVE_WITH_KNOTS('',3,(#110460,#110461,#110462,#110463,#110464,
#110465,#110466,#110467,#110468,#110469,#110470,#110471,#110472,#110473,
#110474,#110475,#110476,#110477,#110478,#110479,#110480,#110481,#110482,
#110483,#110484,#110485),.UNSPECIFIED.,.F.,.F.,(4,2,2,2,2,2,2,2,2,2,2,2,
4),(2.70344464880683,2.89144352771223,3.06851986340401,3.08081089074483,
3.26996664970738,3.35940092938476,3.54587543017967,3.72254345722124,3.73903833379381,
3.9157002469173,3.93052100184786,4.11735511986238,4.22222897897867),
 .UNSPECIFIED.) ;
#238 = B_SPLINE_CURVE_WITH_KNOTS('',3,(#110643,#110644,#110645,#110646,#110647,
#110648,#110649,#110650,#110651,#110652,#110653,#110654,#110655,#110656,
#110657,#110658,#110659,#110660,#110661),.UNSPECIFIED.,.F.,.F.,(4,3,3,3,
3,3,4),(2.81004151507315E-8,3.99307614181576E-5,8.00540716903477E-5,0.000126830846822483,
0.000175618195186418,0.000215193140472276,0.00024522089875673),
 .UNSPECIFIED.) ;
#239 = B_SPLINE_CURVE_WITH_KNOTS('',3,(#110684,#110685,#110686,#110687,#110688,
#110689,#110690,#110691,#110692,#110693,#110694,#110695,#110696,#110697,
#110698,#110699,#110700,#110701,#110702,#110703,#110704,#110705,#110706,
#110707,#110708,#110709,#110710,#110711,#110712,#110713,#110714,#110715,
#110716,#110717,#110718,#110719,#110720,#110721,#110722,#110723,#110724,
#110725,#110726,#110727,#110728,#110729,#110730,#110731,#110732,#110733,
#110734,#110735,#110736,#110737,#110738,#110739,#110740,#110741,#110742,
#110743,#110744,#110745,#110746,#110747,#110748,#110749,#110750,#110751,
#110752,#110753,#110754,#110755,#110756,#110757,#110758,#110759,#110760,
#110761,#110762),.UNSPECIFIED.,.F.,.F.,(4,3,3,3,3,3,3,3,3,3,3,3,3,3,3,3,
3,3,3,3,3,3,3,3,3,3,4),(0.000152038190190988,0.000154892841408446,0.000155160464960082,
0.000160456565729206,0.000163456795060818,0.0001665800922469,0.000167751328691681,
0.000168007536663977,0.000168255738137138,0.000169267315291294,0.000175949983805147,
0.000178959298271426,0.000180334649023592,0.000187987241670261,0.000191981216408588,
0.000193065528939054,0.000193839174265159,0.000198143816207847,0.000212206269476804,
0.000226582370019588,0.000228143757087808,0.000228729277238391,0.000232827918292468,
0.000249109432820284,0.000250176797440916,0.000265881325831968,0.000267525676589363),
 .UNSPECIFIED.) ;
#240 = B_SPLINE_CURVE_WITH_KNOTS('',3,(#110764,#110765,#110766,#110767,#110768,
#110769,#110770,#110771,#110772,#110773),.UNSPECIFIED.,.F.,.F.,(4,3,3,4),
(0.00013063174123083,0.000139067346351189,0.000143554831048705,0.00015203818937155),
 .UNSPECIFIED.) ;
#241 = B_SPLINE_CURVE_WITH_KNOTS('',3,(#110775,#110776,#110777,#110778,#110779,
#110780,#110781,#110782,#110783,#110784,#110785,#110786,#110787,#110788,
#110789,#110790,#110791,#110792,#110793),.UNSPECIFIED.,.F.,.F.,(4,3,3,3,
3,3,4),(0.000104137230128263,0.000110259474166881,0.000116844366893684,
0.000120664217590594,0.000125429508057303,0.000130430624030584,0.000130630877723054),
 .UNSPECIFIED.) ;
#242 = B_SPLINE_CURVE_WITH_KNOTS('',3,(#110794,#110795,#110796,#110797,#110798,
#110799,#110800,#110801,#110802,#110803,#110804,#110805,#110806,#110807,
#110808,#110809,#110810,#110811,#110812,#110813,#110814,#110815,#110816,
#110817,#110818,#110819,#110820,#110821,#110822,#110823,#110824,#110825,
#110826,#110827,#110828,#110829,#110830,#110831,#110832,#110833,#110834,
#110835,#110836),.UNSPECIFIED.,.F.,.F.,(4,3,3,3,3,3,3,3,3,3,3,3,3,3,4),
(0.,4.78421531964037E-6,1.59977421339088E-5,1.75965265776683E-5,2.63603667652888E-5,
3.75047088100213E-5,4.29655082836385E-5,5.3450780665107E-5,6.17416442233874E-5,
6.39360530465754E-5,7.32944438965348E-5,8.49065978095124E-5,9.46209320470023E-5,
9.66050857869651E-5,0.00010413722946728),.UNSPECIFIED.) ;
#243 = B_SPLINE_CURVE_WITH_KNOTS('',3,(#110906,#110907,#110908,#110909,#110910,
#110911,#110912,#110913,#110914,#110915,#110916,#110917,#110918,#110919,
#110920,#110921,#110922,#110923,#110924,#110925,#110926,#110927,#110928,
#110929,#110930,#110931,#110932,#110933,#110934,#110935,#110936,#110937,
#110938,#110939),.UNSPECIFIED.,.F.,.F.,(4,3,3,3,3,3,3,3,3,3,3,4),(0.000173579735006458,
0.000179152672590563,0.00018712219621297,0.000190349677855919,0.000201571576238784,
0.000207505544696865,0.00020908215834011,0.000218112358783792,0.000219837174422847,
0.000228512621317669,0.00024080293533235,0.000245138123631364),
 .UNSPECIFIED.) ;
#244 = B_SPLINE_CURVE_WITH_KNOTS('',3,(#111001,#111002,#111003,#111004,#111005,
#111006,#111007,#111008,#111009,#111010,#111011,#111012,#111013,#111014,
#111015,#111016),.UNSPECIFIED.,.F.,.F.,(4,3,3,3,3,4),(0.000149826268238874,
0.000156541783273878,0.000187447062839771,0.000218157419331147,0.0002512535901195,
0.000263630362845938),.UNSPECIFIED.) ;
#245 = B_SPLINE_CURVE_WITH_KNOTS('',3,(#111018,#111019,#111020,#111021),
 .UNSPECIFIED.,.F.,.F.,(4,4),(0.00012894552500308,0.000149826268238874),
 .UNSPECIFIED.) ;
#246 = B_SPLINE_CURVE_WITH_KNOTS('',3,(#111022,#111023,#111024,#111025,#111026,
#111027,#111028,#111029,#111030,#111031,#111032,#111033,#111034,#111035,
#111036,#111037),.UNSPECIFIED.,.F.,.F.,(4,3,3,3,3,4),(0.000107977862661226,
0.000113849696954328,0.00011675864089999,0.000123355930725867,0.000128649321338313,
0.00012894552500308),.UNSPECIFIED.) ;
#247 = B_SPLINE_CURVE_WITH_KNOTS('',3,(#111247,#111248,#111249,#111250,#111251,
#111252,#111253,#111254,#111255,#111256),.UNSPECIFIED.,.F.,.F.,(4,3,3,4),
(3.97263228028543E-15,3.94729529730244E-5,7.90727202189635E-5,0.00010300346369627),
 .UNSPECIFIED.) ;
#248 = B_SPLINE_CURVE_WITH_KNOTS('',3,(#111263,#111264,#111265,#111266,#111267,
#111268,#111269),.UNSPECIFIED.,.F.,.F.,(4,3,4),(0.00015822335750707,0.000179871364136697,
0.000191820073778123),.UNSPECIFIED.) ;
#249 = B_SPLINE_CURVE_WITH_KNOTS('',3,(#111284,#111285,#111286,#111287,#111288,
#111289,#111290,#111291,#111292,#111293,#111294,#111295,#111296,#111297,
#111298,#111299),.UNSPECIFIED.,.F.,.F.,(4,3,3,3,3,4),(2.25414513468041E-8,
3.71181381094367E-5,7.40234349159894E-5,0.000126639028433412,0.000171180683285944,
0.000173579731706482),.UNSPECIFIED.) ;
#250 = B_SPLINE_CURVE_WITH_KNOTS('',3,(#111355,#111356,#111357,#111358,#111359,
#111360),.UNSPECIFIED.,.F.,.F.,(4,2,4),(0.,0.000162685424844483,0.000325370849688965),
 .UNSPECIFIED.) ;
#251 = B_SPLINE_CURVE_WITH_KNOTS('',3,(#111363,#111364,#111365,#111366,#111367,
#111368),.UNSPECIFIED.,.F.,.F.,(4,2,4),(0.,0.000163438694679257,0.000326877389358514),
 .UNSPECIFIED.) ;
#252 = B_SPLINE_CURVE_WITH_KNOTS('',3,(#111379,#111380,#111381,#111382,#111383,
#111384),.UNSPECIFIED.,.F.,.F.,(4,2,4),(-0.00501427184001352,-0.00354643693242498,
0.),.UNSPECIFIED.) ;
#253 = B_SPLINE_CURVE_WITH_KNOTS('',3,(#111397,#111398,#111399,#111400,#111401,
#111402,#111403,#111404,#111405,#111406,#111407,#111408,#111409,#111410,
#111411,#111412,#111413,#111414,#111415,#111416,#111417,#111418,#111419,
#111420,#111421,#111422,#111423,#111424),.UNSPECIFIED.,.F.,.F.,(4,3,3,3,
3,3,3,3,3,4),(5.2381062116969E-9,5.84794260526809E-6,8.49662041781891E-6,
1.21937803558058E-5,1.7603367013667E-5,1.93092034273021E-5,2.55871453405969E-5,
3.0315421636348E-5,3.68519660351865E-5,3.92146766969307E-5),
 .UNSPECIFIED.) ;
#254 = B_SPLINE_CURVE_WITH_KNOTS('',3,(#111426,#111427,#111428,#111429,#111430,
#111431,#111432,#111433,#111434,#111435),.UNSPECIFIED.,.F.,.F.,(4,3,3,4),
(0.000144469795965455,0.000165397602015043,0.000173816468562374,0.000175865847906018),
 .UNSPECIFIED.) ;
#255 = B_SPLINE_CURVE_WITH_KNOTS('',3,(#111453,#111454,#111455,#111456,#111457,
#111458,#111459),.UNSPECIFIED.,.F.,.F.,(4,3,4),(-2.05331166616455E-6,2.04386714311757E-5,
3.16299855932218E-5),.UNSPECIFIED.) ;
#256 = B_SPLINE_CURVE_WITH_KNOTS('',3,(#111461,#111462,#111463,#111464,#111465,
#111466,#111467,#111468,#111469,#111470,#111471,#111472),.UNSPECIFIED.,
 .F.,.F.,(4,2,2,2,2,4),(9.00279523814192E-9,0.00183032786984177,0.0060774656662359,
0.0169681634717373,0.0216775195756215,0.0254454420933995),.UNSPECIFIED.) ;
#257 = B_SPLINE_CURVE_WITH_KNOTS('',3,(#111631,#111632,#111633,#111634,#111635,
#111636,#111637,#111638,#111639,#111640,#111641,#111642,#111643,#111644,
#111645,#111646,#111647,#111648,#111649,#111650,#111651,#111652,#111653,
#111654,#111655,#111656,#111657,#111658,#111659,#111660,#111661,#111662,
#111663,#111664,#111665,#111666,#111667,#111668,#111669,#111670),
 .UNSPECIFIED.,.F.,.F.,(4,3,3,3,3,3,3,3,3,3,3,3,3,4),(0.,5.0717323028292E-5,
0.000104017413501046,0.00012450671916665,0.00012524956819241,0.000156566023859647,
0.000186760078749971,0.000187880030991795,0.000203537318084806,0.00021136603554746,
0.000217886758541633,0.00021919464484864,0.000234851354133265,0.000249013438333296),
 .UNSPECIFIED.) ;
#258 = B_SPLINE_CURVE_WITH_KNOTS('',3,(#111676,#111677,#111678,#111679,#111680,
#111681,#111682,#111683,#111684,#111685,#111686,#111687,#111688,#111689,
#111690,#111691,#111692,#111693,#111694,#111695,#111696,#111697,#111698,
#111699,#111700,#111701,#111702,#111703,#111704,#111705,#111706,#111707,
#111708,#111709,#111710,#111711,#111712,#111713,#111714,#111715),
 .UNSPECIFIED.,.F.,.F.,(4,3,3,3,3,3,3,3,3,3,3,3,3,4),(0.,1.43115567092639E-5,
3.01335133960425E-5,3.14552036774813E-5,3.80447517297347E-5,4.59561222518525E-5,
6.17788922892923E-5,6.29104073549626E-5,9.34210966965285E-5,0.000125066393795525,
0.000125820814709921,0.000179837268182647,0.000231469985696588,0.000251641629419827),
 .UNSPECIFIED.) ;
#259 = B_SPLINE_CURVE_WITH_KNOTS('',3,(#111720,#111721,#111722,#111723,#111724,
#111725,#111726),.UNSPECIFIED.,.F.,.F.,(4,3,4),(-2.04939766627003E-6,0.,
2.93835791072157E-5),.UNSPECIFIED.) ;
#260 = B_SPLINE_CURVE_WITH_KNOTS('',3,(#111741,#111742,#111743,#111744,#111745,
#111746,#111747,#111748,#111749,#111750,#111751,#111752,#111753,#111754),
 .UNSPECIFIED.,.F.,.F.,(4,2,2,2,2,2,4),(1.44901763004144E-6,0.000561621523804037,
0.00112173034329354,0.00210338619163598,0.00384452539442495,0.00473112295062459,
0.00541108585437911),.UNSPECIFIED.) ;
#261 = B_SPLINE_CURVE_WITH_KNOTS('',3,(#111763,#111764,#111765,#111766,#111767,
#111768,#111769,#111770,#111771,#111772,#111773,#111774,#111775,#111776,
#111777,#111778,#111779,#111780,#111781,#111782,#111783,#111784,#111785,
#111786,#111787,#111788,#111789,#111790,#111791,#111792,#111793,#111794,
#111795,#111796),.UNSPECIFIED.,.F.,.F.,(4,2,2,2,2,2,2,2,2,2,2,2,2,2,2,2,
4),(0.,1.67528894171673E-5,3.36326639087995E-5,3.53285003633486E-5,3.67766442982523E-5,
4.45936877501694E-5,5.25629171991637E-5,5.37833548715111E-5,5.51649664473801E-5,
7.22376444475639E-5,7.35532885965079E-5,0.000109240736296815,0.000146228640920945,
0.000147106577193012,0.000203359192945594,0.000258123601943362,0.00029421315438602),
 .UNSPECIFIED.) ;
#262 = B_SPLINE_CURVE_WITH_KNOTS('',3,(#111800,#111801,#111802,#111803,#111804,
#111805,#111806,#111807,#111808,#111809,#111810,#111811,#111812,#111813,
#111814,#111815,#111816,#111817,#111818,#111819,#111820,#111821,#111822,
#111823,#111824,#111825,#111826,#111827,#111828,#111829,#111830,#111831,
#111832,#111833,#111834,#111835,#111836,#111837,#111838,#111839,#111840,
#111841,#111842,#111843,#111844,#111845,#111846,#111847,#111848,#111849,
#111850,#111851),.UNSPECIFIED.,.F.,.F.,(4,3,3,3,3,3,3,3,3,3,3,3,3,3,3,3,
3,4),(0.,5.28180786157377E-5,0.000107888430292485,0.000143209193859038,
0.000144078242180733,0.000180086811859676,0.000214813790788553,0.000215458170263625,
0.000216102549738696,0.000232714940020933,0.000234106492510888,0.000238605983992275,
0.000240855729732968,0.000243105475473661,0.000250616089253313,0.000252108710851866,
0.000270124214172563,0.000286418387718064),.UNSPECIFIED.) ;
#263 = B_SPLINE_CURVE_WITH_KNOTS('',3,(#111996,#111997,#111998,#111999,#112000,
#112001,#112002,#112003),.UNSPECIFIED.,.F.,.F.,(4,2,2,4),(-0.0473604779370388,
-0.0461995546884436,-0.0447198409510952,-0.0410407833884837),
 .UNSPECIFIED.) ;
#264 = B_SPLINE_CURVE_WITH_KNOTS('',3,(#112011,#112012,#112013,#112014,#112015,
#112016,#112017,#112018),.UNSPECIFIED.,.F.,.F.,(4,2,2,4),(-0.0536801724855783,
-0.0500011149229823,-0.0485214011856339,-0.0473604779370388),
 .UNSPECIFIED.) ;
#265 = B_SPLINE_CURVE_WITH_KNOTS('',3,(#112472,#112473,#112474,#112475,#112476,
#112477,#112478,#112479,#112480,#112481,#112482,#112483,#112484,#112485),
 .UNSPECIFIED.,.F.,.F.,(4,2,2,2,2,2,4),(4.71238898038469,4.88175806245101,
5.06763701998682,5.24337922961327,5.2645133320796,5.44874090582723,5.49822830854813),
 .UNSPECIFIED.) ;
#266 = B_SPLINE_CURVE_WITH_KNOTS('',3,(#112490,#112491,#112492,#112493,#112494,
#112495,#112496,#112497,#112498,#112499,#112500,#112501,#112502,#112503),
 .UNSPECIFIED.,.F.,.F.,(4,2,2,2,2,2,4),(0.78495699863145,0.966941694311798,
1.1431172121153,1.16348181627562,1.34745079132799,1.51752882030591,1.5707963267949),
 .UNSPECIFIED.) ;
#267 = B_SPLINE_CURVE_WITH_KNOTS('',3,(#112509,#112510,#112511,#112512,#112513,
#112514,#112515,#112516,#112517,#112518,#112519,#112520,#112521,#112522),
 .UNSPECIFIED.,.F.,.F.,(4,2,2,2,2,2,4),(0.784956998631343,0.966941694311655,
1.14311721212998,1.16348181627563,1.34745079132838,1.51752882030652,1.5707963267949),
 .UNSPECIFIED.) ;
#268 = B_SPLINE_CURVE_WITH_KNOTS('',3,(#112524,#112525,#112526,#112527,#112528,
#112529,#112530,#112531,#112532,#112533,#112534,#112535,#112536,#112537),
 .UNSPECIFIED.,.F.,.F.,(4,2,2,2,2,2,4),(4.71238898038469,4.88175806245179,
5.06763701998934,5.2433792296541,5.26451333208252,5.44874090582906,5.49822830854823),
 .UNSPECIFIED.) ;
#269 = B_SPLINE_CURVE_WITH_KNOTS('',3,(#112541,#112542,#112543,#112544,#112545,
#112546,#112547,#112548,#112549,#112550,#112551,#112552,#112553,#112554),
 .UNSPECIFIED.,.F.,.F.,(4,2,2,2,2,2,4),(4.71238898038469,4.88175806245174,
5.06763701998914,5.24337922964868,5.26451333208227,5.44874090582901,5.49822830854825),
 .UNSPECIFIED.) ;
#270 = B_SPLINE_CURVE_WITH_KNOTS('',3,(#112558,#112559,#112560,#112561,#112562,
#112563,#112564,#112565,#112566,#112567,#112568,#112569,#112570,#112571),
 .UNSPECIFIED.,.F.,.F.,(4,2,2,2,2,2,4),(0.784956998631379,0.966941694311961,
1.14311721212408,1.1634818162759,1.34745079132852,1.5175288203065,1.5707963267949),
 .UNSPECIFIED.) ;
#271 = B_SPLINE_CURVE_WITH_KNOTS('',3,(#112586,#112587,#112588,#112589,#112590,
#112591,#112592,#112593,#112594,#112595,#112596,#112597,#112598,#112599),
 .UNSPECIFIED.,.F.,.F.,(4,2,2,2,2,2,4),(0.784956998631469,0.966941694312593,
1.14311721209935,1.16348181627602,1.34745079132695,1.51752882030426,1.5707963267949),
 .UNSPECIFIED.) ;
#272 = B_SPLINE_CURVE_WITH_KNOTS('',3,(#112603,#112604,#112605,#112606,#112607,
#112608,#112609,#112610,#112611,#112612,#112613,#112614,#112615,#112616),
 .UNSPECIFIED.,.F.,.F.,(4,2,2,2,2,2,4),(4.71238898038469,4.88175806245153,
5.06763701998872,5.24337922961216,5.2645133320817,5.44874090582829,5.49822830854814),
 .UNSPECIFIED.) ;
#273 = B_SPLINE_CURVE_WITH_KNOTS('',3,(#112721,#112722,#112723,#112724,#112725,
#112726,#112727,#112728,#112729,#112730,#112731,#112732,#112733,#112734,
#112735,#112736),.UNSPECIFIED.,.F.,.F.,(4,3,3,3,3,4),(0.,3.26760986414938E-5,
6.60604127813367E-5,0.000101135724265729,0.00013823780033308,0.00016624299182732),
 .UNSPECIFIED.) ;
#274 = B_SPLINE_CURVE_WITH_KNOTS('',3,(#112798,#112799,#112800,#112801,#112802,
#112803,#112804,#112805,#112806,#112807,#112808,#112809,#112810,#112811,
#112812,#112813),.UNSPECIFIED.,.F.,.F.,(4,3,3,3,3,4),(0.,1.86901632150156E-5,
5.38940239621527E-5,9.13255451816914E-5,0.000129775966053829,0.000168373497604197),
 .UNSPECIFIED.) ;
#275 = B_SPLINE_CURVE_WITH_KNOTS('',3,(#112818,#112819,#112820,#112821,#112822,
#112823,#112824,#112825,#112826,#112827),.UNSPECIFIED.,.F.,.F.,(4,2,2,2,
4),(0.0288531015839766,0.0296205843610201,0.032803105685514,0.0376042554662768,
0.0407130021489537),.UNSPECIFIED.) ;
#276 = B_SPLINE_CURVE_WITH_KNOTS('',3,(#112832,#112833,#112834,#112835,#112836,
#112837),.UNSPECIFIED.,.F.,.F.,(4,2,4),(0.0637474840140125,0.0675088661184123,
0.0720284409301188),.UNSPECIFIED.) ;
#277 = B_SPLINE_CURVE_WITH_KNOTS('',3,(#112843,#112844,#112845,#112846,#112847,
#112848,#112849,#112850,#112851,#112852),.UNSPECIFIED.,.F.,.F.,(4,2,2,2,
4),(0.0767275662203977,0.0771734766269397,0.0818220866796455,0.0868722195290685,
0.0892832637278774),.UNSPECIFIED.) ;
#278 = B_SPLINE_CURVE_WITH_KNOTS('',3,(#112887,#112888,#112889,#112890,#112891,
#112892),.UNSPECIFIED.,.F.,.F.,(4,2,4),(0.171679973607292,0.178707475950603,
0.186889989702311),.UNSPECIFIED.) ;
#279 = B_SPLINE_CURVE_WITH_KNOTS('',3,(#112932,#112933,#112934,#112935,#112936,
#112937,#112938,#112939,#112940,#112941,#112942,#112943,#112944,#112945,
#112946,#112947,#112948,#112949,#112950,#112951,#112952,#112953,#112954,
#112955,#112956,#112957,#112958,#112959,#112960,#112961),.UNSPECIFIED.,
 .F.,.F.,(4,2,2,2,2,2,2,2,2,2,2,2,2,2,4),(2.36970964942748,2.55498029688324,
2.73514427898934,2.74569929646418,2.92071305420845,2.93943382978562,3.11857096684871,
3.13197658032441,3.25399179664502,3.4505427826148,3.6279453579965,3.64606212534862,
3.82474099481916,3.83698255062526,3.91347421315172),.UNSPECIFIED.) ;
#280 = B_SPLINE_CURVE_WITH_KNOTS('',3,(#112972,#112973,#112974,#112975,#112976,
#112977,#112978,#112979,#112980,#112981,#112982,#112983,#112984,#112985,
#112986,#112987,#112988,#112989,#112990,#112991,#112992,#112993,#112994,
#112995,#112996,#112997),.UNSPECIFIED.,.F.,.F.,(4,2,2,2,2,2,2,2,2,2,2,2,
4),(2.70344464881048,2.89144352771225,3.06851986339127,3.08081089074493,
3.2699666497075,3.35940092938474,3.54587543017978,3.72254345722052,3.73903833379394,
3.91570024691754,3.93052100184793,4.11735511986242,4.22222897897867),
 .UNSPECIFIED.) ;
#281 = B_SPLINE_CURVE_WITH_KNOTS('',3,(#113155,#113156,#113157,#113158,#113159,
#113160,#113161,#113162,#113163,#113164,#113165,#113166,#113167,#113168,
#113169,#113170,#113171,#113172,#113173),.UNSPECIFIED.,.F.,.F.,(4,3,3,3,
3,3,4),(2.8100415148163E-8,3.99307614181576E-5,8.00540716903477E-5,0.000126830846822483,
0.000175618195186418,0.000215193140472276,0.00024522089875673),
 .UNSPECIFIED.) ;
#282 = B_SPLINE_CURVE_WITH_KNOTS('',3,(#113196,#113197,#113198,#113199,#113200,
#113201,#113202,#113203,#113204,#113205,#113206,#113207,#113208,#113209,
#113210,#113211,#113212,#113213,#113214,#113215,#113216,#113217,#113218,
#113219,#113220,#113221,#113222,#113223,#113224,#113225,#113226,#113227,
#113228,#113229,#113230,#113231,#113232,#113233,#113234,#113235,#113236,
#113237,#113238,#113239,#113240,#113241,#113242,#113243,#113244,#113245,
#113246,#113247,#113248,#113249,#113250,#113251,#113252,#113253,#113254,
#113255,#113256,#113257,#113258,#113259,#113260,#113261,#113262,#113263,
#113264,#113265,#113266,#113267,#113268,#113269,#113270,#113271,#113272,
#113273,#113274),.UNSPECIFIED.,.F.,.F.,(4,3,3,3,3,3,3,3,3,3,3,3,3,3,3,3,
3,3,3,3,3,3,3,3,3,3,4),(0.000152038190190979,0.000154892841408439,0.000155160464960076,
0.00016045656572911,0.000163456795060818,0.000166580092246901,0.000167751328691683,
0.000168007536663979,0.00016825573813714,0.0001692673152913,0.000175949983805152,
0.000178959298271428,0.000180334649023594,0.000187987241670257,0.000191981216408588,
0.000193065528939052,0.000193839174265157,0.000198143816207847,0.000212206269476822,
0.000226582370019626,0.000228143757087837,0.000228729277238415,0.000232827918292468,
0.000249109432822923,0.000250176797440916,0.000265881325831446,0.000267525676589363),
 .UNSPECIFIED.) ;
#283 = B_SPLINE_CURVE_WITH_KNOTS('',3,(#113276,#113277,#113278,#113279,#113280,
#113281,#113282,#113283,#113284,#113285),.UNSPECIFIED.,.F.,.F.,(4,3,3,4),
(0.000130631741230824,0.000139067346351537,0.000143554831048706,0.000152038189371535),
 .UNSPECIFIED.) ;
#284 = B_SPLINE_CURVE_WITH_KNOTS('',3,(#113287,#113288,#113289,#113290,#113291,
#113292,#113293,#113294,#113295,#113296,#113297,#113298,#113299,#113300,
#113301,#113302,#113303,#113304,#113305),.UNSPECIFIED.,.F.,.F.,(4,3,3,3,
3,3,4),(0.000104137230128253,0.00011025947416687,0.000116844366893704,0.000120664217590573,
0.000125429508057303,0.00013043062403061,0.000130630877723054),
 .UNSPECIFIED.) ;
#285 = B_SPLINE_CURVE_WITH_KNOTS('',3,(#113306,#113307,#113308,#113309,#113310,
#113311,#113312,#113313,#113314,#113315,#113316,#113317,#113318,#113319,
#113320,#113321,#113322,#113323,#113324,#113325,#113326,#113327,#113328,
#113329,#113330,#113331,#113332,#113333,#113334,#113335,#113336,#113337,
#113338,#113339,#113340,#113341,#113342,#113343,#113344,#113345,#113346,
#113347,#113348),.UNSPECIFIED.,.F.,.F.,(4,3,3,3,3,3,3,3,3,3,3,3,3,3,4),
(0.,4.78421531964037E-6,1.5997742133367E-5,1.75965265776407E-5,2.63603667654138E-5,
3.75047088105756E-5,4.29655082836385E-5,5.3450780665107E-5,6.17416442233547E-5,
6.39360530465754E-5,7.32944438965254E-5,8.49065978095124E-5,9.4620932046832E-5,
9.6605085786969E-5,0.000104137229467266),.UNSPECIFIED.) ;
#286 = B_SPLINE_CURVE_WITH_KNOTS('',3,(#113418,#113419,#113420,#113421,#113422,
#113423,#113424,#113425,#113426,#113427,#113428,#113429,#113430,#113431,
#113432,#113433,#113434,#113435,#113436,#113437,#113438,#113439,#113440,
#113441,#113442,#113443,#113444,#113445,#113446,#113447,#113448,#113449,
#113450,#113451),.UNSPECIFIED.,.F.,.F.,(4,3,3,3,3,3,3,3,3,3,3,4),(0.00017357973500646,
0.000179152672590516,0.000187122196212348,0.000190349677855926,0.00020157157623905,
0.000207505544696952,0.000209082158340111,0.000218112358784159,0.00021983717442272,
0.000228512621317903,0.000240802935335257,0.000245138123631368),
 .UNSPECIFIED.) ;
#287 = B_SPLINE_CURVE_WITH_KNOTS('',3,(#113513,#113514,#113515,#113516,#113517,
#113518,#113519,#113520,#113521,#113522,#113523,#113524,#113525,#113526,
#113527,#113528),.UNSPECIFIED.,.F.,.F.,(4,3,3,3,3,4),(0.00014982626823866,
0.000156541783273877,0.000187447062839769,0.000218157419331144,0.000251253590119498,
0.000263630362845952),.UNSPECIFIED.) ;
#288 = B_SPLINE_CURVE_WITH_KNOTS('',3,(#113530,#113531,#113532,#113533),
 .UNSPECIFIED.,.F.,.F.,(4,4),(0.000128945525002973,0.00014982626823866),
 .UNSPECIFIED.) ;
#289 = B_SPLINE_CURVE_WITH_KNOTS('',3,(#113534,#113535,#113536,#113537,#113538,
#113539,#113540,#113541,#113542,#113543,#113544,#113545,#113546,#113547,
#113548,#113549),.UNSPECIFIED.,.F.,.F.,(4,3,3,3,3,4),(0.000107977862661223,
0.000113849696953733,0.000116758640899989,0.000123355930725824,0.000128649321338145,
0.000128945525002973),.UNSPECIFIED.) ;
#290 = B_SPLINE_CURVE_WITH_KNOTS('',3,(#113894,#113895,#113896,#113897,#113898,
#113899,#113900,#113901),.UNSPECIFIED.,.F.,.F.,(4,2,2,4),(-0.0212593174733862,
-0.0176486602253693,-0.0143243289552082,-0.0134403252720105),
 .UNSPECIFIED.) ;
#291 = B_SPLINE_CURVE_WITH_KNOTS('',3,(#113937,#113938,#113939,#113940,#113941,
#113942,#113943,#113944),.UNSPECIFIED.,.F.,.F.,(4,2,2,4),(-0.021259317482921,
-0.0176486602328459,-0.0143243289609224,-0.0134403252772803),
 .UNSPECIFIED.) ;
#292 = B_SPLINE_CURVE_WITH_KNOTS('',3,(#113980,#113981,#113982,#113983,#113984,
#113985,#113986,#113987),.UNSPECIFIED.,.F.,.F.,(4,2,2,4),(-0.0212593174877944,
-0.0176486602368674,-0.0143243289641644,-0.0134403252803157),
 .UNSPECIFIED.) ;
#293 = B_SPLINE_CURVE_WITH_KNOTS('',3,(#114023,#114024,#114025,#114026,#114027,
#114028,#114029,#114030),.UNSPECIFIED.,.F.,.F.,(4,2,2,4),(-0.0212593174829433,
-0.0176486602328601,-0.014324328960934,-0.0134403252772914),
 .UNSPECIFIED.) ;
#294 = B_SPLINE_CURVE_WITH_KNOTS('',3,(#114066,#114067,#114068,#114069,#114070,
#114071,#114072,#114073),.UNSPECIFIED.,.F.,.F.,(4,2,2,4),(-0.0212593174732112,
-0.0176486602254681,-0.0143243289554829,-0.0134403252723181),
 .UNSPECIFIED.) ;
#295 = B_SPLINE_CURVE_WITH_KNOTS('',3,(#114109,#114110,#114111,#114112,#114113,
#114114,#114115,#114116),.UNSPECIFIED.,.F.,.F.,(4,2,2,4),(-0.0212593174781932,
-0.0176486602293651,-0.0143243289584549,-0.0134403252750573),
 .UNSPECIFIED.) ;
#296 = B_SPLINE_CURVE_WITH_KNOTS('',3,(#114152,#114153,#114154,#114155,#114156,
#114157,#114158,#114159),.UNSPECIFIED.,.F.,.F.,(4,2,2,4),(-0.0212593174830444,
-0.0176486602331658,-0.0143243289613579,-0.0134403252777338),
 .UNSPECIFIED.) ;
#297 = B_SPLINE_CURVE_WITH_KNOTS('',3,(#114195,#114196,#114197,#114198,#114199,
#114200,#114201,#114202),.UNSPECIFIED.,.F.,.F.,(4,2,2,4),(-0.021259317485983,
-0.017648660235379,-0.0143243289629727,-0.0134403252792024),
 .UNSPECIFIED.) ;
#298 = B_SPLINE_CURVE_WITH_KNOTS('',3,(#114319,#114320,#114321,#114322,#114323,
#114324,#114325,#114326),.UNSPECIFIED.,.F.,.F.,(4,2,2,4),(-0.0212593174838741,
-0.0176486602337396,-0.0143243289617316,-0.0134403252780616),
 .UNSPECIFIED.) ;
#299 = B_SPLINE_CURVE_WITH_KNOTS('',3,(#114443,#114444,#114445,#114446,#114447,
#114448,#114449,#114450),.UNSPECIFIED.,.F.,.F.,(4,2,2,4),(-0.021259317485706,
-0.0176486602351398,-0.0143243289627718,-0.013440325279013),
 .UNSPECIFIED.) ;
#300 = B_SPLINE_CURVE_WITH_KNOTS('',3,(#116047,#116048,#116049,#116050,#116051,
#116052,#116053,#116054),.UNSPECIFIED.,.F.,.F.,(4,2,2,4),(-0.052701717162025,
-0.0518504523811948,-0.0480303917439054,-0.04467544736819),
 .UNSPECIFIED.) ;
#301 = B_SPLINE_CURVE_WITH_KNOTS('',3,(#116058,#116059,#116060,#116061,#116062,
#116063,#116064,#116065,#116066,#116067,#116068,#116069,#116070,#116071,
#116072,#116073,#116074,#116075,#116076,#116077,#116078,#116079,#116080,
#116081,#116082,#116083,#116084,#116085,#116086,#116087,#116088),
 .UNSPECIFIED.,.F.,.F.,(4,3,3,3,3,3,3,3,3,3,4),(0.,1.7911486298437E-5,3.35636550441565E-5,
5.14128838689559E-5,6.71346369544057E-5,8.50076921954425E-5,0.000100614915215922,
0.000118595988596762,0.000134133865285036,0.000151845157316713,0.0001565184788544),
 .UNSPECIFIED.) ;
#302 = B_SPLINE_CURVE_WITH_KNOTS('',3,(#116090,#116091,#116092,#116093,#116094,
#116095,#116096,#116097,#116098,#116099,#116100,#116101,#116102,#116103,
#116104,#116105,#116106,#116107,#116108,#116109,#116110,#116111),
 .UNSPECIFIED.,.F.,.F.,(4,2,2,2,2,2,2,2,2,2,4),(-0.0842935807175857,-0.0841564124762399,
-0.0836958438579189,-0.0829341784875174,-0.0805923611130053,-0.0773601159115686,
-0.0742136752654363,-0.071123820447877,-0.0675672289498007,-0.0637829215046486,
-0.0629274139192696),.UNSPECIFIED.) ;
#303 = B_SPLINE_CURVE_WITH_KNOTS('',3,(#119109,#119110,#119111,#119112,#119113,
#119114,#119115,#119116),.UNSPECIFIED.,.F.,.F.,(4,2,2,4),(-0.0527017171620382,
-0.0518504523812081,-0.0480303917439178,-0.0446754473682008),
 .UNSPECIFIED.) ;
#304 = B_SPLINE_CURVE_WITH_KNOTS('',3,(#119120,#119121,#119122,#119123,#119124,
#119125,#119126,#119127,#119128,#119129,#119130,#119131,#119132,#119133,
#119134,#119135,#119136,#119137,#119138,#119139,#119140,#119141,#119142,
#119143,#119144,#119145,#119146,#119147,#119148,#119149,#119150),
 .UNSPECIFIED.,.F.,.F.,(4,3,3,3,3,3,3,3,3,3,4),(0.,1.79114862984415E-5,
3.35636550441565E-5,5.14128838689557E-5,6.7134636954406E-5,8.50076921954395E-5,
0.000100614915215921,0.000118595988596772,0.000134133865285036,0.000151845157316653,
0.0001565184788544),.UNSPECIFIED.) ;
#305 = B_SPLINE_CURVE_WITH_KNOTS('',3,(#119152,#119153,#119154,#119155,#119156,
#119157,#119158,#119159,#119160,#119161,#119162,#119163,#119164,#119165,
#119166,#119167,#119168,#119169,#119170,#119171,#119172,#119173),
 .UNSPECIFIED.,.F.,.F.,(4,2,2,2,2,2,2,2,2,2,4),(-0.0842935807153196,-0.0841564124739783,
-0.0836958438556783,-0.0829341784853091,-0.0805923611108952,-0.0773601159095917,
-0.0742136752635866,-0.0711238204461505,-0.0675672289482145,-0.0637829215032092,
-0.062927413917864),.UNSPECIFIED.) ;
#306 = B_SPLINE_CURVE_WITH_KNOTS('',3,(#119813,#119814,#119815,#119816,#119817,
#119818,#119819,#119820),.UNSPECIFIED.,.F.,.F.,(4,2,2,4),(-0.0527017171621304,
-0.0518504523813015,-0.0480303917440028,-0.0446754473682719),
 .UNSPECIFIED.) ;
#307 = B_SPLINE_CURVE_WITH_KNOTS('',3,(#119824,#119825,#119826,#119827,#119828,
#119829,#119830,#119831,#119832,#119833,#119834,#119835,#119836,#119837,
#119838,#119839,#119840,#119841,#119842,#119843,#119844,#119845,#119846,
#119847,#119848,#119849,#119850,#119851,#119852,#119853,#119854),
 .UNSPECIFIED.,.F.,.F.,(4,3,3,3,3,3,3,3,3,3,4),(0.,1.79114862984384E-5,
3.35636550441566E-5,5.14128838689606E-5,6.7134636954406E-5,8.50076921954722E-5,
0.000100614915215922,0.000118595988596755,0.000134133865285036,0.00015184515731678,
0.0001565184788544),.UNSPECIFIED.) ;
#308 = B_SPLINE_CURVE_WITH_KNOTS('',3,(#119856,#119857,#119858,#119859,#119860,
#119861,#119862,#119863,#119864,#119865,#119866,#119867,#119868,#119869,
#119870,#119871,#119872,#119873,#119874,#119875,#119876,#119877),
 .UNSPECIFIED.,.F.,.F.,(4,2,2,2,2,2,2,2,2,2,4),(-0.0842935807419127,-0.0841564125005222,
-0.0836958438819682,-0.082934178511186,-0.0805923611355419,-0.0773601159325885,
-0.0742136752850249,-0.0711238204661043,-0.0675672289665108,-0.0637829215197928,
-0.0629274139340661),.UNSPECIFIED.) ;
#309 = B_SPLINE_CURVE_WITH_KNOTS('',3,(#120040,#120041,#120042,#120043,#120044,
#120045,#120046,#120047),.UNSPECIFIED.,.F.,.F.,(4,2,2,4),(-0.0527017171621393,
-0.0518504523813096,-0.0480303917440155,-0.0446754473682944),
 .UNSPECIFIED.) ;
#310 = B_SPLINE_CURVE_WITH_KNOTS('',3,(#120051,#120052,#120053,#120054,#120055,
#120056,#120057,#120058,#120059,#120060,#120061,#120062,#120063,#120064,
#120065,#120066,#120067,#120068,#120069,#120070,#120071,#120072,#120073,
#120074,#120075,#120076,#120077,#120078,#120079,#120080,#120081),
 .UNSPECIFIED.,.F.,.F.,(4,3,3,3,3,3,3,3,3,3,4),(0.,1.7911486298444E-5,3.35636550441567E-5,
5.14128838689174E-5,6.71346369544062E-5,8.50076921954515E-5,0.000100614915215921,
0.000118595988596814,0.000134133865285036,0.000151845157316771,0.0001565184788544),
 .UNSPECIFIED.) ;
#311 = B_SPLINE_CURVE_WITH_KNOTS('',3,(#120083,#120084,#120085,#120086,#120087,
#120088,#120089,#120090,#120091,#120092,#120093,#120094,#120095,#120096,
#120097,#120098,#120099,#120100,#120101,#120102,#120103,#120104),
 .UNSPECIFIED.,.F.,.F.,(4,2,2,2,2,2,2,2,2,2,4),(-0.0842935808351552,-0.0841564125935704,
-0.0836958439740798,-0.0829341786018125,-0.0805923612217205,-0.077360116012801,
-0.0742136753596006,-0.0711238205353107,-0.0675672290297288,-0.0637829215768355,
-0.0629274139897445),.UNSPECIFIED.) ;
#312 = B_SPLINE_CURVE_WITH_KNOTS('',3,(#120267,#120268,#120269,#120270,#120271,
#120272,#120273,#120274),.UNSPECIFIED.,.F.,.F.,(4,2,2,4),(-0.0527017171620452,
-0.0518504523812172,-0.0480303917439374,-0.04467544736823),
 .UNSPECIFIED.) ;
#313 = B_SPLINE_CURVE_WITH_KNOTS('',3,(#120278,#120279,#120280,#120281,#120282,
#120283,#120284,#120285,#120286,#120287,#120288,#120289,#120290,#120291,
#120292,#120293,#120294,#120295,#120296,#120297,#120298,#120299,#120300,
#120301,#120302,#120303,#120304,#120305,#120306,#120307,#120308),
 .UNSPECIFIED.,.F.,.F.,(4,3,3,3,3,3,3,3,3,3,4),(0.,1.79114862984569E-5,
3.35636550441567E-5,5.14128838689565E-5,6.71346369544062E-5,8.50076921954284E-5,
0.000100614915215921,0.000118595988596684,0.000134133865285036,0.000151845157316633,
0.0001565184788544),.UNSPECIFIED.) ;
#314 = B_SPLINE_CURVE_WITH_KNOTS('',3,(#120310,#120311,#120312,#120313,#120314,
#120315,#120316,#120317,#120318,#120319,#120320,#120321,#120322,#120323,
#120324,#120325,#120326,#120327,#120328,#120329,#120330,#120331),
 .UNSPECIFIED.,.F.,.F.,(4,2,2,2,2,2,2,2,2,2,4),(-0.0842935807861705,-0.0841564125446822,
-0.08369584392567,-0.0829341785541707,-0.0805923611763772,-0.0773601159705437,
-0.0742136753202586,-0.0711238204987475,-0.0675672289962676,-0.0637829215465878,
-0.0629274139602073),.UNSPECIFIED.) ;
#315 = B_SPLINE_CURVE_WITH_KNOTS('',3,(#120494,#120495,#120496,#120497,#120498,
#120499,#120500,#120501),.UNSPECIFIED.,.F.,.F.,(4,2,2,4),(-0.0527017171621833,
-0.0518504523813524,-0.0480303917440445,-0.044675447368305),
 .UNSPECIFIED.) ;
#316 = B_SPLINE_CURVE_WITH_KNOTS('',3,(#120505,#120506,#120507,#120508,#120509,
#120510,#120511,#120512,#120513,#120514,#120515,#120516,#120517,#120518,
#120519,#120520,#120521,#120522,#120523,#120524,#120525,#120526,#120527,
#120528,#120529,#120530,#120531,#120532,#120533,#120534,#120535),
 .UNSPECIFIED.,.F.,.F.,(4,3,3,3,3,3,3,3,3,3,4),(0.,1.791148629847E-5,3.35636550441561E-5,
5.14128838689644E-5,6.71346369544058E-5,8.50076921954764E-5,0.000100614915215921,
0.000118595988596817,0.000134133865285032,0.000151845157316703,0.000156518478854398),
 .UNSPECIFIED.) ;
#317 = B_SPLINE_CURVE_WITH_KNOTS('',3,(#120537,#120538,#120539,#120540,#120541,
#120542,#120543,#120544,#120545,#120546,#120547,#120548,#120549,#120550,
#120551,#120552,#120553,#120554,#120555,#120556,#120557,#120558),
 .UNSPECIFIED.,.F.,.F.,(4,2,2,2,2,2,2,2,2,2,4),(-0.0842935807861705,-0.0841564125446822,
-0.08369584392567,-0.0829341785541707,-0.0805923611763772,-0.0773601159705437,
-0.0742136753202586,-0.0711238204987475,-0.0675672289962676,-0.0637829215465878,
-0.0629274139602073),.UNSPECIFIED.) ;
#318 = B_SPLINE_CURVE_WITH_KNOTS('',3,(#120721,#120722,#120723,#120724,#120725,
#120726,#120727,#120728),.UNSPECIFIED.,.F.,.F.,(4,2,2,4),(-0.0527017171619057,
-0.0518504523810739,-0.0480303917437878,-0.0446754473680843),
 .UNSPECIFIED.) ;
#319 = B_SPLINE_CURVE_WITH_KNOTS('',3,(#120732,#120733,#120734,#120735,#120736,
#120737,#120738,#120739,#120740,#120741,#120742,#120743,#120744,#120745,
#120746,#120747,#120748,#120749,#120750,#120751,#120752,#120753,#120754,
#120755,#120756,#120757,#120758,#120759,#120760,#120761,#120762),
 .UNSPECIFIED.,.F.,.F.,(4,3,3,3,3,3,3,3,3,3,4),(0.,1.79114862984022E-5,
3.35636550441561E-5,5.14128838690747E-5,6.71346369544058E-5,8.50076921955029E-5,
0.000100614915215921,0.000118595988596949,0.000134133865285032,0.000151845157316721,
0.000156518478854398),.UNSPECIFIED.) ;
#320 = B_SPLINE_CURVE_WITH_KNOTS('',3,(#120764,#120765,#120766,#120767,#120768,
#120769,#120770,#120771,#120772,#120773,#120774,#120775,#120776,#120777,
#120778,#120779,#120780,#120781,#120782,#120783,#120784,#120785),
 .UNSPECIFIED.,.F.,.F.,(4,2,2,2,2,2,2,2,2,2,4),(-0.0842935806846017,-0.0841564124433096,
-0.0836958438252493,-0.0829341784552694,-0.0805923610820353,-0.0773601158823278,
-0.0742136752378489,-0.07112382042188,-0.0675672289255957,-0.0637829214823062,
-0.0629274138973503),.UNSPECIFIED.) ;
#321 = B_SPLINE_CURVE_WITH_KNOTS('',3,(#120948,#120949,#120950,#120951,#120952,
#120953,#120954,#120955),.UNSPECIFIED.,.F.,.F.,(4,2,2,4),(-0.0527017171620534,
-0.0518504523812236,-0.0480303917439217,-0.0446754473681886),
 .UNSPECIFIED.) ;
#322 = B_SPLINE_CURVE_WITH_KNOTS('',3,(#120959,#120960,#120961,#120962,#120963,
#120964,#120965,#120966,#120967,#120968,#120969,#120970,#120971,#120972,
#120973,#120974,#120975,#120976,#120977,#120978,#120979,#120980,#120981,
#120982,#120983,#120984,#120985,#120986,#120987,#120988,#120989),
 .UNSPECIFIED.,.F.,.F.,(4,3,3,3,3,3,3,3,3,3,4),(0.,1.79114862984111E-5,
3.35636550441561E-5,5.1412883869035E-5,6.71346369544058E-5,8.50076921954072E-5,
0.000100614915215921,0.000118595988596959,0.000134133865285032,0.000151845157317271,
0.000156518478854398),.UNSPECIFIED.) ;
#323 = B_SPLINE_CURVE_WITH_KNOTS('',3,(#120991,#120992,#120993,#120994,#120995,
#120996,#120997,#120998,#120999,#121000,#121001,#121002,#121003,#121004,
#121005,#121006,#121007,#121008,#121009,#121010,#121011,#121012),
 .UNSPECIFIED.,.F.,.F.,(4,2,2,2,2,2,2,2,2,2,4),(-0.0842935807784001,-0.0841564125369118,
-0.0836958439179285,-0.0829341785465007,-0.080592361168928,-0.0773601159633862,
-0.0742136753133782,-0.071123820492143,-0.0675672289899856,-0.063782921540619,
-0.0629274139542864),.UNSPECIFIED.) ;
#324 = B_SPLINE_CURVE_WITH_KNOTS('',3,(#121175,#121176,#121177,#121178,#121179,
#121180,#121181,#121182),.UNSPECIFIED.,.F.,.F.,(4,2,2,4),(-0.0527017171619366,
-0.0518504523811075,-0.0480303917438238,-0.0446754473681228),
 .UNSPECIFIED.) ;
#325 = B_SPLINE_CURVE_WITH_KNOTS('',3,(#121186,#121187,#121188,#121189,#121190,
#121191,#121192,#121193,#121194,#121195,#121196,#121197,#121198,#121199,
#121200,#121201,#121202,#121203,#121204,#121205,#121206,#121207,#121208,
#121209,#121210,#121211,#121212,#121213,#121214,#121215,#121216),
 .UNSPECIFIED.,.F.,.F.,(4,3,3,3,3,3,3,3,3,3,4),(0.,1.7911486298388E-5,3.35636550441561E-5,
5.14128838690249E-5,6.71346369544058E-5,8.50076921954834E-5,0.000100614915215921,
0.000118595988596784,0.000134133865285032,0.000151845157317113,0.000156518478854398),
 .UNSPECIFIED.) ;
#326 = B_SPLINE_CURVE_WITH_KNOTS('',3,(#121218,#121219,#121220,#121221,#121222,
#121223,#121224,#121225,#121226,#121227,#121228,#121229,#121230,#121231,
#121232,#121233,#121234,#121235,#121236,#121237,#121238,#121239),
 .UNSPECIFIED.,.F.,.F.,(4,2,2,2,2,2,2,2,2,2,4),(-0.0842935807784001,-0.0841564125369118,
-0.0836958439179285,-0.0829341785465007,-0.080592361168928,-0.0773601159633862,
-0.0742136753133782,-0.071123820492143,-0.0675672289899856,-0.063782921540619,
-0.0629274139542864),.UNSPECIFIED.) ;
#327 = B_SPLINE_CURVE_WITH_KNOTS('',3,(#121402,#121403,#121404,#121405,#121406,
#121407,#121408,#121409),.UNSPECIFIED.,.F.,.F.,(4,2,2,4),(-0.0527017171617456,
-0.0518504523809185,-0.0480303917436524,-0.0446754473679689),
 .UNSPECIFIED.) ;
#328 = B_SPLINE_CURVE_WITH_KNOTS('',3,(#121413,#121414,#121415,#121416,#121417,
#121418,#121419,#121420,#121421,#121422,#121423,#121424,#121425,#121426,
#121427,#121428,#121429,#121430,#121431,#121432,#121433,#121434,#121435,
#121436,#121437,#121438,#121439,#121440,#121441,#121442,#121443),
 .UNSPECIFIED.,.F.,.F.,(4,3,3,3,3,3,3,3,3,3,4),(0.,1.79114862983986E-5,
3.35636550441583E-5,5.14128838688763E-5,6.71346369544075E-5,8.5007692195462E-5,
0.000100614915215918,0.000118595988596873,0.000134133865285036,0.000151845157315814,
0.000156518478854401),.UNSPECIFIED.) ;
#329 = B_SPLINE_CURVE_WITH_KNOTS('',3,(#121445,#121446,#121447,#121448,#121449,
#121450,#121451,#121452,#121453,#121454,#121455,#121456,#121457,#121458,
#121459,#121460,#121461,#121462,#121463,#121464,#121465,#121466),
 .UNSPECIFIED.,.F.,.F.,(4,2,2,2,2,2,2,2,2,2,4),(-0.0842935807784001,-0.0841564125369118,
-0.0836958439179285,-0.0829341785465007,-0.080592361168928,-0.0773601159633862,
-0.0742136753133782,-0.071123820492143,-0.0675672289899856,-0.063782921540619,
-0.0629274139542864),.UNSPECIFIED.) ;
#330 = B_SPLINE_CURVE_WITH_KNOTS('',3,(#124047,#124048,#124049,#124050,#124051,
#124052,#124053,#124054,#124055,#124056,#124057,#124058,#124059,#124060,
#124061,#124062,#124063,#124064,#124065,#124066),.UNSPECIFIED.,.F.,.F.,
(4,2,2,2,2,2,2,2,2,4),(7.26097235916453,7.307487976323,7.35575594389105,
7.40257156416353,7.45158020939779,7.49931815600202,7.54681878982848,7.59584329786992,
7.64302175237609,7.68775617947263),.UNSPECIFIED.) ;
#331 = B_SPLINE_CURVE_WITH_KNOTS('',3,(#124069,#124070,#124071,#124072,#124073,
#124074,#124075,#124076,#124077,#124078,#124079,#124080,#124081,#124082,
#124083,#124084,#124085,#124086,#124087,#124088),.UNSPECIFIED.,.F.,.F.,
(4,2,2,2,2,2,2,2,2,4),(0.,0.0459875521653835,0.0932819628997698,0.142429322852028,
0.189908590414643,0.237761664358612,0.28683868989661,0.333704279409584,
0.382086034209551,0.427411498485805),.UNSPECIFIED.) ;
#332 = B_SPLINE_CURVE_WITH_KNOTS('',3,(#124093,#124094,#124095,#124096,#124097,
#124098,#124099,#124100,#124101,#124102,#124103,#124104,#124105,#124106,
#124107,#124108,#124109,#124110,#124111,#124112,#124113,#124114,#124115,
#124116,#124117,#124118,#124119,#124120,#124121,#124122,#124123,#124124,
#124125,#124126,#124127,#124128,#124129,#124130),.UNSPECIFIED.,.F.,.F.,
(4,2,2,2,2,2,2,2,2,2,2,2,2,2,2,2,2,2,4),(6.48467832939662,6.48870478558093,
6.53766507492409,6.58568550492772,6.63267823725172,6.68202082324882,6.72948815834683,
6.77759017644729,6.82630561099994,6.87323621682889,6.92225205593385,6.97046423370673,
7.01740641521615,7.06695661317869,7.11461532958629,7.16247212938834,7.21140015580506,
7.25849183169839,7.26097235916453),.UNSPECIFIED.) ;
#333 = B_SPLINE_CURVE_WITH_KNOTS('',3,(#124131,#124132,#124133,#124134,#124135,
#124136,#124137,#124138,#124139,#124140,#124141,#124142,#124143,#124144,
#124145,#124146,#124147,#124148,#124149,#124150,#124151,#124152,#124153,
#124154,#124155,#124156,#124157,#124158,#124159,#124160,#124161,#124162,
#124163,#124164,#124165,#124166,#124167,#124168),.UNSPECIFIED.,.F.,.F.,
(4,2,2,2,2,2,2,2,2,2,2,2,2,2,2,2,2,2,4),(0.427411498485805,0.431577036060463,
0.478789185503758,0.527845315274495,0.575603226460443,0.623379302822146,
0.672502619127436,0.719463017877226,0.767773403599721,0.816880465796082,
0.864021613138868,0.912997981216,0.961170824102338,1.00888581090197,1.0584891685082,
1.10562630736056,1.1538964673421,1.20305610785317,1.20577246230604),
 .UNSPECIFIED.) ;
#334 = B_SPLINE_CURVE_WITH_KNOTS('',3,(#124173,#124174,#124175,#124176,#124177,
#124178,#124179,#124180,#124181,#124182,#124183,#124184,#124185,#124186,
#124187,#124188,#124189,#124190,#124191,#124192,#124193,#124194,#124195,
#124196,#124197,#124198,#124199,#124200,#124201,#124202,#124203,#124204,
#124205,#124206,#124207,#124208),.UNSPECIFIED.,.F.,.F.,(4,2,2,2,2,2,2,2,
2,2,2,2,2,2,2,2,2,4),(5.70956420747771,5.72030972034507,5.76926273175053,
5.81700561122586,5.86434645191125,5.91338162506858,5.96056756496257,6.00942404361783,
6.05780748008125,6.10453345170252,6.15347366016584,6.20133669000566,6.24846500640859,
6.29763501900576,6.34494399136913,6.39338455386973,6.4419176261338,6.48467832939662),
 .UNSPECIFIED.) ;
#335 = B_SPLINE_CURVE_WITH_KNOTS('',3,(#124209,#124210,#124211,#124212,#124213,
#124214,#124215,#124216,#124217,#124218,#124219,#124220,#124221,#124222,
#124223,#124224,#124225,#124226,#124227,#124228,#124229,#124230,#124231,
#124232,#124233,#124234,#124235,#124236,#124237,#124238,#124239,#124240,
#124241,#124242,#124243,#124244),.UNSPECIFIED.,.F.,.F.,(4,2,2,2,2,2,2,2,
2,2,2,2,2,2,2,2,2,4),(1.20577246230604,1.2500637087132,1.29884493426391,
1.34732241102889,1.39486523697925,1.44428132500633,1.49152186175626,1.53962022531109,
1.58874613172205,1.63565991568587,1.68427775017929,1.73314474249065,1.78054992698739,
1.8298155429656,1.87724047764212,1.92520328493819,1.97432941645622,1.98383043851811),
 .UNSPECIFIED.) ;
#336 = B_SPLINE_CURVE_WITH_KNOTS('',3,(#124249,#124250,#124251,#124252,#124253,
#124254,#124255,#124256,#124257,#124258,#124259,#124260,#124261,#124262,
#124263,#124264,#124265,#124266,#124267,#124268,#124269,#124270,#124271,
#124272,#124273,#124274,#124275,#124276,#124277,#124278,#124279,#124280,
#124281,#124282,#124283,#124284),.UNSPECIFIED.,.F.,.F.,(4,2,2,2,2,2,2,2,
2,2,2,2,2,2,2,2,2,4),(4.93350849726113,4.95065313897434,5.0001367514161,
5.04773589353637,5.09575665066723,5.14461540943155,5.19164298059034,5.24062387411831,
5.28881904095715,5.33565288934101,5.38464956624476,5.43231220009687,5.4799267516029,
5.52886743736441,5.57596806240929,5.62529535397539,5.67356510724699,5.70956420747771),
 .UNSPECIFIED.) ;
#337 = B_SPLINE_CURVE_WITH_KNOTS('',3,(#124285,#124286,#124287,#124288,#124289,
#124290,#124291,#124292,#124293,#124294,#124295,#124296,#124297,#124298,
#124299,#124300,#124301,#124302,#124303,#124304,#124305,#124306,#124307,
#124308,#124309,#124310,#124311,#124312,#124313,#124314,#124315,#124316,
#124317,#124318,#124319,#124320),.UNSPECIFIED.,.F.,.F.,(4,2,2,2,2,2,2,2,
2,2,2,2,2,2,2,2,2,4),(1.98383043851811,2.021231364205,2.0697205926988,2.11904155289011,
2.1663460448574,2.21550071170308,2.26317878691631,2.31104512794968,2.36020318829153,
2.40716845964159,2.4555671563287,2.50471172270157,2.55193271124501,2.60099435417148,
2.64904317691366,2.69683410923425,2.74652048876617,2.76242745970405),
 .UNSPECIFIED.) ;
#338 = B_SPLINE_CURVE_WITH_KNOTS('',3,(#124325,#124326,#124327,#124328,#124329,
#124330,#124331,#124332,#124333,#124334,#124335,#124336,#124337,#124338,
#124339,#124340,#124341,#124342,#124343,#124344,#124345,#124346,#124347,
#124348,#124349,#124350,#124351,#124352,#124353,#124354,#124355,#124356,
#124357,#124358,#124359,#124360),.UNSPECIFIED.,.F.,.F.,(4,2,2,2,2,2,2,2,
2,2,2,2,2,2,2,2,2,4),(4.15738429453256,4.18139819511275,4.23053919796976,
4.27782394869024,4.32652355399284,4.37501975350424,4.42180928210789,4.47080187820887,
4.51878063593279,4.56588041443636,4.61517448159553,4.66259930855119,4.71091650689067,
4.7595782551651,4.80646789213435,4.8554969233847,4.90364974207811,4.93350849726113),
 .UNSPECIFIED.) ;
#339 = B_SPLINE_CURVE_WITH_KNOTS('',3,(#124361,#124362,#124363,#124364,#124365,
#124366,#124367,#124368,#124369,#124370,#124371,#124372,#124373,#124374,
#124375,#124376,#124377,#124378,#124379,#124380,#124381,#124382,#124383,
#124384,#124385,#124386,#124387,#124388,#124389,#124390,#124391,#124392,
#124393,#124394,#124395,#124396),.UNSPECIFIED.,.F.,.F.,(4,2,2,2,2,2,2,2,
2,2,2,2,2,2,2,2,2,4),(2.76242745970405,2.7936241020587,2.84197026691353,
2.89114229506907,2.93820657938614,2.98705917484022,3.03536824467617,3.08297180498013,
3.13245479128841,3.17962172814637,3.22778030392872,3.27690191435427,3.32383405210944,
3.3725082345208,3.421169403163,3.46861903657913,3.51793416507266,3.54067593133588),
 .UNSPECIFIED.) ;
#340 = B_SPLINE_CURVE_WITH_KNOTS('',3,(#124401,#124402,#124403,#124404,#124405,
#124406,#124407,#124408,#124409,#124410,#124411,#124412,#124413,#124414,
#124415,#124416,#124417,#124418,#124419,#124420,#124421,#124422,#124423,
#124424,#124425,#124426,#124427,#124428,#124429,#124430,#124431,#124432,
#124433,#124434,#124435,#124436),.UNSPECIFIED.,.F.,.F.,(4,2,2,2,2,2,2,2,
2,2,2,2,2,2,2,2,2,4),(3.3811260484289,3.41274900862816,3.46099351805033,
3.51004032645083,3.55700214539487,3.60575007739184,3.65387741150041,3.70137616908567,
3.75075153504194,3.79777167498976,3.84582386285438,3.89300519478398,3.94215330243098,
3.99051838064245,4.03728979359576,4.08628002368325,4.13412062890419,4.15738429453256),
 .UNSPECIFIED.) ;
#341 = B_SPLINE_CURVE_WITH_KNOTS('',3,(#124437,#124438,#124439,#124440,#124441,
#124442,#124443,#124444,#124445,#124446,#124447,#124448,#124449,#124450,
#124451,#124452,#124453,#124454,#124455,#124456,#124457,#124458,#124459,
#124460,#124461,#124462,#124463,#124464,#124465,#124466,#124467,#124468,
#124469,#124470,#124471,#124472),.UNSPECIFIED.,.F.,.F.,(4,2,2,2,2,2,2,2,
2,2,2,2,2,2,2,2,2,4),(3.54067593133588,3.56524889916681,3.6132547608121,
3.66236113995851,3.70924379097633,3.75777283633892,3.80686079772826,3.85419230870826,
3.90337783950468,3.95091591719774,4.0002920934568,4.0477975955105,4.09630989433075,
4.14504988690739,4.19202367440407,4.2411602470478,4.2893880427099,4.31858521036147),
 .UNSPECIFIED.) ;
#342 = B_SPLINE_CURVE_WITH_KNOTS('',3,(#124477,#124478,#124479,#124480,#124481,
#124482,#124483,#124484,#124485,#124486,#124487,#124488,#124489,#124490,
#124491,#124492,#124493,#124494,#124495,#124496,#124497,#124498,#124499,
#124500,#124501,#124502,#124503,#124504,#124505,#124506,#124507,#124508,
#124509,#124510,#124511,#124512),.UNSPECIFIED.,.F.,.F.,(4,2,2,2,2,2,2,2,
2,2,2,2,2,2,2,2,2,4),(2.60440000418254,2.64222091806599,2.69061789859203,
2.73975515555105,2.78696572159386,2.83602367520873,2.88355189021403,2.93132224967008,
2.98036249985887,3.02720769453067,3.07550834816351,3.12453618250826,3.17165958350625,
3.22062064308854,3.26850397351192,3.31619467232154,3.36577824481598,3.3811260484289),
 .UNSPECIFIED.) ;
#343 = B_SPLINE_CURVE_WITH_KNOTS('',3,(#124513,#124514,#124515,#124516,#124517,
#124518,#124519,#124520,#124521,#124522,#124523,#124524,#124525,#124526,
#124527,#124528,#124529,#124530,#124531,#124532,#124533,#124534,#124535,
#124536,#124537,#124538,#124539,#124540,#124541,#124542,#124543,#124544,
#124545,#124546,#124547,#124548),.UNSPECIFIED.,.F.,.F.,(4,2,2,2,2,2,2,2,
2,2,2,2,2,2,2,2,2,4),(4.31858521036147,4.33651923363743,4.38607754453018,
4.43375037804094,4.48194507407388,4.53087577616931,4.57797363563567,4.62704987194849,
4.67531370070556,4.72225592255632,4.77134912087816,4.81907824427662,4.86684436513085,
4.91585036470624,4.96301502121423,5.01254217112715,5.06087102345235,5.09618003538743),
 .UNSPECIFIED.) ;
#344 = B_SPLINE_CURVE_WITH_KNOTS('',3,(#124553,#124554,#124555,#124556,#124557,
#124558,#124559,#124560,#124561,#124562,#124563,#124564,#124565,#124566,
#124567,#124568,#124569,#124570,#124571,#124572,#124573,#124574,#124575,
#124576,#124577,#124578,#124579,#124580,#124581,#124582,#124583,#124584,
#124585,#124586,#124587,#124588),.UNSPECIFIED.,.F.,.F.,(4,2,2,2,2,2,2,2,
2,2,2,2,2,2,2,2,2,4),(1.82805130471776,1.87277646127533,1.92147530871624,
1.96979104419725,2.01725060263876,2.06658135847983,2.11369404932703,2.16170773952795,
2.2107256291696,2.25754243281317,2.30607324540708,2.35476584472025,2.40208265835429,
2.45125749765287,2.49854231366641,2.54641504154563,2.59542814286478,2.60440000418254),
 .UNSPECIFIED.) ;
#345 = B_SPLINE_CURVE_WITH_KNOTS('',3,(#124589,#124590,#124591,#124592,#124593,
#124594,#124595,#124596,#124597,#124598,#124599,#124600,#124601,#124602,
#124603,#124604,#124605,#124606,#124607,#124608,#124609,#124610,#124611,
#124612,#124613,#124614,#124615,#124616,#124617,#124618,#124619,#124620,
#124621,#124622,#124623,#124624),.UNSPECIFIED.,.F.,.F.,(4,2,2,2,2,2,2,2,
2,2,2,2,2,2,2,2,2,4),(5.09618003538743,5.10770893818563,5.15675128793345,
5.20455098500115,5.25203122076791,5.3011219283047,5.34836274788015,5.39740888690433,
5.44584255805835,5.49264392480102,5.54166593188317,5.58957668485638,5.63682763234505,
5.68604400914993,5.73339928464143,5.78201352428103,5.8305888160979,5.8725887638988),
 .UNSPECIFIED.) ;
#346 = B_SPLINE_CURVE_WITH_KNOTS('',3,(#124629,#124630,#124631,#124632,#124633,
#124634,#124635,#124636,#124637,#124638,#124639,#124640,#124641,#124642,
#124643,#124644,#124645,#124646,#124647,#124648,#124649,#124650,#124651,
#124652,#124653,#124654,#124655,#124656,#124657,#124658,#124659,#124660,
#124661,#124662,#124663,#124664,#124665,#124666),.UNSPECIFIED.,.F.,.F.,
(4,2,2,2,2,2,2,2,2,2,2,2,2,2,2,2,2,2,4),(1.05122908753305,1.05584848690386,
1.10298878125772,1.15197109295181,1.19959776737697,1.24730001658321,1.29632817220458,
1.34318726064785,1.39142201535752,1.44043479373918,1.48749995499297,1.536398131184,
1.58442418882633,1.63206057663025,1.68158354821496,1.72860610089148,1.77679646385941,
1.82585341919623,1.82805130471776),.UNSPECIFIED.) ;
#347 = B_SPLINE_CURVE_WITH_KNOTS('',3,(#124667,#124668,#124669,#124670,#124671,
#124672,#124673,#124674,#124675,#124676,#124677,#124678,#124679,#124680,
#124681,#124682,#124683,#124684,#124685,#124686,#124687,#124688,#124689,
#124690,#124691,#124692,#124693,#124694,#124695,#124696,#124697,#124698,
#124699,#124700,#124701,#124702,#124703,#124704),.UNSPECIFIED.,.F.,.F.,
(4,2,2,2,2,2,2,2,2,2,2,2,2,2,2,2,2,2,4),(5.8725887638988,5.87743194290884,
5.92646601185683,5.97452581587684,6.02162175582692,6.07100225132472,6.11850795426233,
6.1667628942196,6.21551331591218,6.2624807124907,6.31156171305631,6.35980565105167,
6.40683027516766,6.456410610302,6.50410033527444,6.55208641404564,6.6010427526743,
6.64816284268059,6.64991209706395),.UNSPECIFIED.) ;
#348 = B_SPLINE_CURVE_WITH_KNOTS('',3,(#124709,#124710,#124711,#124712,#124713,
#124714,#124715,#124716,#124717,#124718,#124719,#124720,#124721,#124722,
#124723,#124724,#124725,#124726,#124727,#124728,#124729,#124730,#124731,
#124732,#124733,#124734,#124735,#124736,#124737,#124738,#124739,#124740,
#124741,#124742,#124743,#124744),.UNSPECIFIED.,.F.,.F.,(4,2,2,2,2,2,2,2,
2,2,2,2,2,2,2,2,2,4),(0.275540243682509,0.286340819800539,0.333695388575774,
0.382913371187234,0.430062940631542,0.477971836820167,0.526948240257121,
0.573710230464671,0.622139368966846,0.670997426602599,0.718226071803216,
0.767306120243138,0.814662887431798,0.862448581964833,0.911435350682647,
0.958210116723726,1.00652260961773,1.05122908753305),.UNSPECIFIED.) ;
#349 = B_SPLINE_CURVE_WITH_KNOTS('',3,(#124745,#124746,#124747,#124748,#124749,
#124750,#124751,#124752,#124753,#124754,#124755,#124756,#124757,#124758,
#124759,#124760,#124761,#124762,#124763,#124764,#124765,#124766,#124767,
#124768,#124769,#124770,#124771,#124772,#124773,#124774,#124775,#124776,
#124777,#124778,#124779,#124780),.UNSPECIFIED.,.F.,.F.,(4,2,2,2,2,2,2,2,
2,2,2,2,2,2,2,2,2,4),(6.64991209706395,6.69721143233729,6.74550549456067,
6.79238454552838,6.84144720027061,6.88920947529323,6.93681673187035,6.98586340790173,
7.03306447569406,7.08232935533034,7.13071011437757,7.17751961704142,7.22654758629657,
7.27440241377778,7.32175171314648,7.37090535322958,7.41820339493711,7.42653426035933),
 .UNSPECIFIED.) ;
#350 = B_SPLINE_CURVE_WITH_KNOTS('',3,(#124786,#124787,#124788,#124789,#124790,
#124791,#124792,#124793,#124794,#124795,#124796,#124797),.UNSPECIFIED.,
 .F.,.F.,(4,2,2,2,2,4),(-0.236473027122006,-0.23458695710018,-0.176673006834002,
-0.118290109209632,-0.0588288584469845,-1.00000016489687E-6),
 .UNSPECIFIED.) ;
#351 = B_SPLINE_CURVE_WITH_KNOTS('',3,(#124800,#124801,#124802,#124803,#124804,
#124805,#124806,#124807),.UNSPECIFIED.,.F.,.F.,(4,2,2,4),(-9.35462171155631,
-9.30382148989728,-9.24635104762449,-9.23530418985942),.UNSPECIFIED.) ;
#352 = B_SPLINE_CURVE_WITH_KNOTS('',3,(#124812,#124813,#124814,#124815,#124816,
#124817,#124818,#124819,#124820,#124821,#124822,#124823,#124824,#124825,
#124826,#124827,#124828,#124829,#124830,#124831,#124832,#124833,#124834,
#124835,#124836,#124837,#124838,#124839,#124840,#124841,#124842,#124843,
#124844,#124845,#124846,#124847),.UNSPECIFIED.,.F.,.F.,(4,2,2,2,2,2,2,2,
2,2,2,2,2,2,2,2,2,4),(-1.1816466799126,-1.1711432489464,-1.11360549897867,
-1.05429971803153,-0.99527231100603,-0.938324784610826,-0.878701151729204,
-0.820319907036438,-0.763004488472792,-0.70301164166561,-0.645300597460547,
-0.586507743434059,-0.527276575096228,-0.470213578625258,-0.410561930645358,
-0.351974482019793,-0.294804872599786,-0.236473027122006),.UNSPECIFIED.) ;
#353 = B_SPLINE_CURVE_WITH_KNOTS('',3,(#124848,#124849,#124850,#124851,#124852,
#124853,#124854,#124855,#124856,#124857,#124858,#124859,#124860,#124861,
#124862,#124863,#124864,#124865,#124866,#124867,#124868,#124869,#124870,
#124871,#124872,#124873,#124874,#124875,#124876,#124877,#124878,#124879,
#124880,#124881,#124882,#124883),.UNSPECIFIED.,.F.,.F.,(4,2,2,2,2,2,2,2,
2,2,2,2,2,2,2,2,2,4),(-9.23530418985942,-9.18662207546147,-9.1290733058091,
-9.07093314408142,-9.01135436272492,-8.95446571047789,-8.89567746304653,
-8.83575191467067,-8.77841492190154,-8.71883583043751,-8.66095591767163,
-8.60294688747092,-8.54333582365895,-8.48636391838879,-8.42770437782455,
-8.3681122074522,-8.31090295919035,-8.29087925177368),.UNSPECIFIED.) ;
#354 = B_SPLINE_CURVE_WITH_KNOTS('',3,(#124888,#124889,#124890,#124891,#124892,
#124893,#124894,#124895,#124896,#124897,#124898,#124899,#124900,#124901,
#124902,#124903,#124904,#124905,#124906,#124907,#124908,#124909,#124910,
#124911,#124912,#124913,#124914,#124915,#124916,#124917,#124918,#124919,
#124920,#124921,#124922,#124923),.UNSPECIFIED.,.F.,.F.,(4,2,2,2,2,2,2,2,
2,2,2,2,2,2,2,2,2,4),(-2.12678122509193,-2.10729425304151,-2.05002580839115,
-1.99038909831469,-1.9316674048963,-1.87466417496185,-1.81501013841361,
-1.75693914324514,-1.69905824232611,-1.63941349055435,-1.58201455193184,
-1.52211994070396,-1.46326421662004,-1.40633380819462,-1.34670866487524,
-1.28850127053106,-1.2309432907053,-1.1816466799126),.UNSPECIFIED.) ;
#355 = B_SPLINE_CURVE_WITH_KNOTS('',3,(#124924,#124925,#124926,#124927,#124928,
#124929,#124930,#124931,#124932,#124933,#124934,#124935,#124936,#124937,
#124938,#124939,#124940,#124941,#124942,#124943,#124944,#124945,#124946,
#124947,#124948,#124949,#124950,#124951,#124952,#124953,#124954,#124955,
#124956,#124957,#124958,#124959),.UNSPECIFIED.,.F.,.F.,(4,2,2,2,2,2,2,2,
2,2,2,2,2,2,2,2,2,4),(-8.29087925177368,-8.25146774569309,-8.1931060140114,
-8.1352172805656,-8.07502593792519,-8.01787916182783,-7.95931748219078,
-7.89969072165382,-7.84265244666734,-7.78344729198975,-7.72467517694015,
-7.66698930483589,-7.60702272505567,-7.5497294421654,-7.4913736598247,-7.43177467302502,
-7.37485108389259,-7.3459015110284),.UNSPECIFIED.) ;
#356 = B_SPLINE_CURVE_WITH_KNOTS('',3,(#124964,#124965,#124966,#124967,#124968,
#124969,#124970,#124971,#124972,#124973,#124974,#124975,#124976,#124977,
#124978,#124979,#124980,#124981,#124982,#124983,#124984,#124985,#124986,
#124987,#124988,#124989,#124990,#124991,#124992,#124993,#124994,#124995,
#124996,#124997,#124998,#124999),.UNSPECIFIED.,.F.,.F.,(4,2,2,2,2,2,2,2,
2,2,2,2,2,2,2,2,2,4),(-3.07234930182782,-3.04396460692137,-2.98700170532857,
-2.92736930082992,-2.86895787619047,-2.81165872476739,-2.7516332217495,
-2.69389232736989,-2.63514802811358,-2.5758833604033,-2.51879305661577,
-2.45912888472762,-2.40050767619665,-2.34334201878956,-2.28308786627346,
-2.22514048990784,-2.16679217042194,-2.12678122509193),.UNSPECIFIED.) ;
#357 = B_SPLINE_CURVE_WITH_KNOTS('',3,(#125000,#125001,#125002,#125003,#125004,
#125005,#125006,#125007,#125008,#125009,#125010,#125011,#125012,#125013,
#125014,#125015,#125016,#125017,#125018,#125019,#125020,#125021,#125022,
#125023,#125024,#125025,#125026,#125027,#125028,#125029,#125030,#125031,
#125032,#125033,#125034,#125035),.UNSPECIFIED.,.F.,.F.,(4,2,2,2,2,2,2,2,
2,2,2,2,2,2,2,2,2,4),(-7.3459015110284,-7.31584938880444,-7.25656387817681,
-7.19905098889278,-7.13927687406326,-7.08174045168678,-7.02355818700801,
-6.9639574791867,-6.90705028583207,-6.84821994204823,-6.78834540215938,
-6.73097099328063,-6.67135180647426,-6.61349209399495,-6.55544587606107,
-6.49581608898128,-6.43883548963137,-6.40128325260829),.UNSPECIFIED.) ;
#358 = B_SPLINE_CURVE_WITH_KNOTS('',3,(#125040,#125041,#125042,#125043,#125044,
#125045,#125046,#125047,#125048,#125049,#125050,#125051,#125052,#125053,
#125054,#125055,#125056,#125057,#125058,#125059,#125060,#125061,#125062,
#125063,#125064,#125065,#125066,#125067,#125068,#125069,#125070,#125071,
#125072,#125073,#125074,#125075),.UNSPECIFIED.,.F.,.F.,(4,2,2,2,2,2,2,2,
2,2,2,2,2,2,2,2,2,4),(-4.01743446108088,-3.98037711695305,-3.92338026613865,
-3.86372411788194,-3.80563194583232,-3.74778671319995,-3.68811833045966,
-3.63069784236149,-3.57087032386455,-3.51198882129594,-3.45505470154523,
-3.39542422850156,-3.33719086850357,-3.27966026017497,-3.21983177136984,
-3.1622680481908,-3.10302199988204,-3.07234930182782),.UNSPECIFIED.) ;
#359 = B_SPLINE_CURVE_WITH_KNOTS('',3,(#125076,#125077,#125078,#125079,#125080,
#125081,#125082,#125083,#125084,#125085,#125086,#125087,#125088,#125089,
#125090,#125091,#125092,#125093,#125094,#125095,#125096,#125097,#125098,
#125099,#125100,#125101,#125102,#125103,#125104,#125105,#125106,#125107,
#125108,#125109,#125110,#125111),.UNSPECIFIED.,.F.,.F.,(4,2,2,2,2,2,2,2,
2,2,2,2,2,2,2,2,2,4),(-6.40128325260829,-6.38013882187402,-6.32052644786668,
-6.26328232847502,-6.20380975384858,-6.14548195466263,-6.08755912059145,
-6.0273305946859,-5.97018690671393,-5.91159053837258,-5.85195029651196,
-5.79488386817085,-5.73564427374236,-5.67691979083501,-5.61920315388539,
-5.5592029693765,-5.50192507313698,-5.45600166496054),.UNSPECIFIED.) ;
#360 = B_SPLINE_CURVE_WITH_KNOTS('',3,(#125116,#125117,#125118,#125119,#125120,
#125121,#125122,#125123,#125124,#125125,#125126,#125127,#125128,#125129,
#125130,#125131,#125132,#125133,#125134,#125135,#125136,#125137,#125138,
#125139,#125140,#125141,#125142,#125143,#125144,#125145,#125146,#125147,
#125148,#125149,#125150,#125151),.UNSPECIFIED.,.F.,.F.,(4,2,2,2,2,2,2,2,
2,2,2,2,2,2,2,2,2,4),(-4.96307563769018,-4.91813866664957,-4.86025738965345,
-4.80218793930441,-4.74253483237101,-4.68553219539954,-4.62681204815797,
-4.5671763186103,-4.50990933760739,-4.45041297938131,-4.3920638222817,-4.33411788796424,
-4.27386529354949,-4.21556664620729,-4.15604769936401,-4.0987601299753,
-4.03911975185839,-4.01743446108088),.UNSPECIFIED.) ;
#361 = B_SPLINE_CURVE_WITH_KNOTS('',3,(#125152,#125153,#125154,#125155,#125156,
#125157,#125158,#125159,#125160,#125161,#125162,#125163,#125164,#125165,
#125166,#125167,#125168,#125169,#125170,#125171,#125172,#125173,#125174,
#125175,#125176,#125177,#125178,#125179,#125180,#125181,#125182,#125183,
#125184,#125185,#125186,#125187),.UNSPECIFIED.,.F.,.F.,(4,2,2,2,2,2,2,2,
2,2,2,2,2,2,2,2,2,4),(-5.45600166496054,-5.44353818748178,-5.38392946676581,
-5.32698965292687,-5.26795703729325,-5.20873029520478,-5.15119052229069,
-5.09138701680441,-5.03387705745448,-4.97566790823344,-4.916060903816,-4.85914913392717,
-4.80029208196713,-4.74048362398375,-4.68308675803797,-4.62463408755934,
-4.56743411515897,-4.51134022964834),.UNSPECIFIED.) ;
#362 = B_SPLINE_CURVE_WITH_KNOTS('',3,(#125192,#125193,#125194,#125195,#125196,
#125197,#125198,#125199,#125200,#125201,#125202,#125203,#125204,#125205,
#125206,#125207,#125208,#125209,#125210,#125211,#125212,#125213,#125214,
#125215,#125216,#125217,#125218,#125219,#125220,#125221,#125222,#125223,
#125224,#125225,#125226,#125227),.UNSPECIFIED.,.F.,.F.,(4,2,2,2,2,2,2,2,
2,2,2,2,2,2,2,2,2,4),(-5.90797790587752,-5.85417655914304,-5.79686139893281,
-5.73848200916043,-5.67885952882914,-5.62191332079682,-5.56288777161221,
-5.50358081908249,-5.44604476955684,-5.38624654359381,-5.32868845608922,
-5.27048277087713,-5.21085866475879,-5.15392918370283,-5.0950751718008,
-5.03517915849782,-4.97778176824204,-4.96307563769018),.UNSPECIFIED.) ;
#363 = B_SPLINE_CURVE_WITH_KNOTS('',3,(#125228,#125229,#125230,#125231,#125232,
#125233,#125234,#125235,#125236,#125237,#125238,#125239,#125240,#125241,
#125242,#125243,#125244,#125245,#125246,#125247,#125248,#125249,#125250,
#125251,#125252,#125253,#125254,#125255,#125256,#125257,#125258,#125259,
#125260,#125261,#125262,#125263,#125264,#125265),.UNSPECIFIED.,.F.,.F.,
(4,2,2,2,2,2,2,2,2,2,2,2,2,2,2,2,2,2,4),(-4.51134022964834,-4.50736107889285,
-4.44957955522536,-4.39103805795909,-4.33172296596087,-4.27459313534948,
-4.21494515138725,-4.15627197557177,-4.09916570838644,-4.03885333731966,
-3.98085531235153,-3.92266438621144,-3.86310737388169,-3.80578556710095,
-3.74614371498309,-3.68736332860037,-3.63038329021729,-3.57072909156752,
-3.56587391815655),.UNSPECIFIED.) ;
#364 = B_SPLINE_CURVE_WITH_KNOTS('',3,(#125270,#125271,#125272,#125273,#125274,
#125275,#125276,#125277,#125278,#125279,#125280,#125281,#125282,#125283,
#125284,#125285,#125286,#125287,#125288,#125289,#125290,#125291,#125292,
#125293,#125294,#125295,#125296,#125297,#125298,#125299,#125300,#125301,
#125302,#125303,#125304,#125305,#125306,#125307),.UNSPECIFIED.,.F.,.F.,
(4,2,2,2,2,2,2,2,2,2,2,2,2,2,2,2,2,2,4),(-6.85333016178901,-6.85049761572826,
-6.79086280145887,-6.7338684673792,-6.67518502916102,-6.61556907483254,
-6.55833655807044,-6.49887713904935,-6.44049363778125,-6.38258139356379,
-6.32236555670732,-6.26519661684873,-6.20661114802352,-6.14696077866283,
-6.08989950504226,-6.03067031724312,-5.97187665370647,-5.91416744423235,
-5.90797790587752),.UNSPECIFIED.) ;
#365 = B_SPLINE_CURVE_WITH_KNOTS('',3,(#125308,#125309,#125310,#125311,#125312,
#125313,#125314,#125315,#125316,#125317,#125318,#125319,#125320,#125321,
#125322,#125323,#125324,#125325,#125326,#125327,#125328,#125329,#125330,
#125331,#125332,#125333,#125334,#125335,#125336,#125337,#125338,#125339,
#125340,#125341,#125342,#125343),.UNSPECIFIED.,.F.,.F.,(4,2,2,2,2,2,2,2,
2,2,2,2,2,2,2,2,2,4),(-3.56587391815655,-3.51259862586625,-3.4548315841227,
-3.39512002261551,-3.33766052431138,-3.27797683666954,-3.21904783493571,
-3.16210893490559,-3.10247369370918,-3.04419237234846,-2.98672132744669,
-2.92683995638948,-2.86922830950958,-2.8101092431121,-2.75099595568126,
-2.69400388512544,-2.63435950322405,-2.62073726926079),.UNSPECIFIED.) ;
#366 = B_SPLINE_CURVE_WITH_KNOTS('',3,(#125350,#125351,#125352,#125353,#125354,
#125355,#125356,#125357,#125358,#125359,#125360,#125361,#125362,#125363,
#125364,#125365,#125366,#125367,#125368,#125369,#125370,#125371,#125372,
#125373,#125374,#125375,#125376,#125377),.UNSPECIFIED.,.F.,.F.,(4,2,2,2,
2,2,2,2,2,2,2,2,2,4),(-0.729144904376339,-0.701294765627904,-0.644290240572763,
-0.584622721852303,-0.526155163852952,-0.468846061685899,-0.408761237620433,
-0.350964868034901,-0.292242330555774,-0.23291790866579,-0.175774000270549,
-0.116070886581869,-0.0573899304566333,0.),.UNSPECIFIED.) ;
#367 = B_SPLINE_CURVE_WITH_KNOTS('',3,(#125385,#125386,#125387,#125388,#125389,
#125390,#125391,#125392,#125393,#125394,#125395,#125396,#125397,#125398,
#125399,#125400,#125401,#125402,#125403,#125404,#125405,#125406,#125407,
#125408,#125409,#125410,#125411,#125412,#125413,#125414),.UNSPECIFIED.,
 .F.,.F.,(4,2,2,2,2,2,2,2,2,2,2,2,2,2,4),(-8.55374923263164,-8.52045997548488,
-8.48812186400397,-8.43025873621608,-8.37009569721686,-8.31293715613035,
-8.25440154797182,-8.19477991623858,-8.1377605421172,-8.07858114325935,
-8.01975349658949,-7.96208993347597,-7.90214811438955,-7.84483111171218,
-7.79788942893258),.UNSPECIFIED.) ;
#368 = B_SPLINE_CURVE_WITH_KNOTS('',3,(#125417,#125418,#125419,#125420,#125421,
#125422,#125423,#125424,#125425,#125426,#125427,#125428,#125429,#125430,
#125431,#125432,#125433,#125434,#125435,#125436,#125437,#125438,#125439,
#125440,#125441,#125442,#125443,#125444,#125445,#125446,#125447,#125448,
#125449,#125450,#125451,#125452),.UNSPECIFIED.,.F.,.F.,(4,2,2,2,2,2,2,2,
2,2,2,2,2,2,2,2,2,4),(-1.67472695159199,-1.63814253054756,-1.58112626326033,
-1.52144174075491,-1.46330248400391,-1.40546717323888,-1.34574854931093,
-1.28828093672951,-1.228494242623,-1.1695607477854,-1.11259684987605,-1.05293475628546,
-0.994649499089507,-0.937120115226852,-0.877236543088398,-0.819621249528116,
-0.760408371557094,-0.729144904376339),.UNSPECIFIED.) ;
#369 = B_SPLINE_CURVE_WITH_KNOTS('',3,(#125454,#125455,#125456,#125457,#125458,
#125459,#125460,#125461,#125462,#125463,#125464,#125465,#125466,#125467,
#125468,#125469,#125470,#125471,#125472,#125473,#125474,#125475,#125476,
#125477,#125478,#125479,#125480,#125481,#125482,#125483,#125484,#125485,
#125486,#125487,#125488,#125489),.UNSPECIFIED.,.F.,.F.,(4,2,2,2,2,2,2,2,
2,2,2,2,2,2,2,2,2,4),(-7.79788942893258,-7.7864978331053,-7.72690027532479,
-7.66998381914493,-7.61100430828218,-7.55165262671408,-7.49415813115462,
-7.434404527004,-7.37683370109388,-7.31866970220167,-7.25906709251872,-7.20215576863061,
-7.14334343176941,-7.08339598828515,-7.02603560425023,-6.96643217276498,
-6.9085302919768,-6.85333016178901),.UNSPECIFIED.) ;
#370 = B_SPLINE_CURVE_WITH_KNOTS('',3,(#125490,#125491,#125492,#125493,#125494,
#125495,#125496,#125497,#125498,#125499,#125500,#125501,#125502,#125503,
#125504,#125505,#125506,#125507,#125508,#125509,#125510,#125511,#125512,
#125513,#125514,#125515,#125516,#125517,#125518,#125519,#125520,#125521,
#125522,#125523,#125524,#125525),.UNSPECIFIED.,.F.,.F.,(4,2,2,2,2,2,2,2,
2,2,2,2,2,2,2,2,2,4),(-2.62073726926079,-2.57589168419096,-2.51862873581428,
-2.45854193473685,-2.40074535328825,-2.34210369906827,-2.28277616139501,
-2.22563231373495,-2.16594829107943,-2.10726356038932,-2.05010847618233,
-1.98978591242265,-1.93177619281583,-1.87350153298898,-1.81393494970357,
-1.75660268268265,-1.69693230395467,-1.67472695159199),.UNSPECIFIED.) ;
#371 = B_SPLINE_CURVE_WITH_KNOTS('',3,(#125528,#125529,#125530,#125531,#125532,
#125533,#125534,#125535,#125536,#125537,#125538,#125539,#125540,#125541,
#125542,#125543,#125544,#125545,#125546,#125547,#125548,#125549),
 .UNSPECIFIED.,.F.,.F.,(4,2,2,2,2,2,2,2,2,2,4),(7.42653426035933,7.46701042314504,
7.51551605666961,7.56232997551886,7.61135461607121,7.65934114232017,7.70649931554284,
7.75579949517463,7.80323150261535,7.848007974901,7.89462988945302),
 .UNSPECIFIED.) ;
#372 = B_SPLINE_CURVE_WITH_KNOTS('',3,(#125552,#125553,#125554,#125555,#125556,
#125557,#125558,#125559,#125560,#125561,#125562,#125563,#125564,#125565),
 .UNSPECIFIED.,.F.,.F.,(4,2,2,2,2,2,4),(9.99999999993084E-7,0.0454152741647829,
0.0934842511977,0.142483198960695,0.189312581462748,0.237893912869686,0.275540243682509),
 .UNSPECIFIED.) ;
#373 = B_SPLINE_CURVE_WITH_KNOTS('',3,(#125585,#125586,#125587,#125588,#125589,
#125590,#125591,#125592,#125593,#125594,#125595,#125596,#125597,#125598,
#125599,#125600,#125601,#125602,#125603,#125604,#125605,#125606,#125607,
#125608,#125609,#125610,#125611,#125612,#125613,#125614),.UNSPECIFIED.,
 .F.,.F.,(4,2,2,2,2,2,2,2,2,2,2,2,2,2,4),(0.102793946330879,0.14065908540827,
0.207546049472987,0.277181081921595,0.341925843104979,0.425232051113792,
0.529553206832786,0.635138456761143,0.687061075445346,0.791098170318975,
0.901479157744014,1.02330053588931,1.15825935025609,1.22953088710868,1.29476085683451),
 .UNSPECIFIED.) ;
#374 = B_SPLINE_CURVE_WITH_KNOTS('',3,(#125618,#125619,#125620,#125621,#125622,
#125623,#125624,#125625),.UNSPECIFIED.,.F.,.F.,(4,2,2,4),(0.,0.0368526993038302,
0.0772866279385214,0.102793946330879),.UNSPECIFIED.) ;
#375 = B_SPLINE_CURVE_WITH_KNOTS('',3,(#125626,#125627,#125628,#125629,#125630,
#125631,#125632,#125633,#125634,#125635,#125636,#125637),.UNSPECIFIED.,
 .F.,.F.,(4,2,2,2,2,4),(-0.166237454912908,-0.14614759649084,-0.124790609402371,
-0.083627563805611,-0.0424146450456111,0.),.UNSPECIFIED.) ;
#376 = B_SPLINE_CURVE_WITH_KNOTS('',3,(#126352,#126353,#126354,#126355,#126356,
#126357,#126358,#126359,#126360,#126361),.UNSPECIFIED.,.F.,.F.,(4,3,3,4),
(0.,8.73464104464917E-5,0.000174692824679549,0.000283410104056903),
 .UNSPECIFIED.) ;
#377 = (
BOUNDED_SURFACE()
B_SPLINE_SURFACE(3,2,((#101185,#101186,#101187),(#101188,#101189,#101190),
(#101191,#101192,#101193),(#101194,#101195,#101196)),.UNSPECIFIED.,.F.,
 .F.,.F.)
B_SPLINE_SURFACE_WITH_KNOTS((4,4),(3,3),(-8.88178419700125E-16,1.00173611575494),
(0.800638603120404,1.),.UNSPECIFIED.)
GEOMETRIC_REPRESENTATION_ITEM()
RATIONAL_B_SPLINE_SURFACE(((0.931056261594764,0.956944532691445,1.),(0.931106613485821,
0.956975977522396,1.),(0.926966069646249,0.954390201728277,1.),(0.920044734228405,
0.950067817452233,1.)))
REPRESENTATION_ITEM('')
SURFACE()
) ;
#378 = (
BOUNDED_SURFACE()
B_SPLINE_SURFACE(3,2,((#101222,#101223,#101224),(#101225,#101226,#101227),
(#101228,#101229,#101230),(#101231,#101232,#101233)),.UNSPECIFIED.,.F.,
 .F.,.F.)
B_SPLINE_SURFACE_WITH_KNOTS((4,4),(3,3),(1.8295911660693E-15,1.08063632538888),
(0.,1.),.UNSPECIFIED.)
GEOMETRIC_REPRESENTATION_ITEM()
RATIONAL_B_SPLINE_SURFACE(((1.,0.821344978643199,1.),(1.,0.821618737292292,
1.),(1.,0.799663084581839,1.),(1.,0.763019982472727,1.)))
REPRESENTATION_ITEM('')
SURFACE()
) ;
#379 = (
BOUNDED_SURFACE()
B_SPLINE_SURFACE(3,2,((#102700,#102701,#102702),(#102703,#102704,#102705),
(#102706,#102707,#102708),(#102709,#102710,#102711),(#102712,#102713,#102714),
(#102715,#102716,#102717)),.UNSPECIFIED.,.F.,.F.,.F.)
B_SPLINE_SURFACE_WITH_KNOTS((4,2,4),(3,3),(9.07204043127161E-5,0.000289236237441534,
0.000487752070570359),(-0.000844756555527479,1.00064307855265),
 .UNSPECIFIED.)
GEOMETRIC_REPRESENTATION_ITEM()
RATIONAL_B_SPLINE_SURFACE(((1.0006785336953,0.598126578821808,1.00051643581316),
(1.00070177595156,0.584360946986066,1.00053412562517),(1.00066498743049,
0.606149590529446,1.00050612567481),(1.00056632625581,0.664583392836326,
1.00043103409964),(1.00050548323107,0.700618735924288,1.0003847261312),
(1.00047271456519,0.720026550084155,1.00035978571524)))
REPRESENTATION_ITEM('')
SURFACE()
) ;
#380 = (
BOUNDED_SURFACE()
B_SPLINE_SURFACE(3,2,((#102732,#102733,#102734),(#102735,#102736,#102737),
(#102738,#102739,#102740),(#102741,#102742,#102743),(#102744,#102745,#102746),
(#102747,#102748,#102749)),.UNSPECIFIED.,.F.,.F.,.F.)
B_SPLINE_SURFACE_WITH_KNOTS((4,2,4),(3,3),(0.000107162911540598,0.000298022515767418,
0.000488882119994237),(-0.000759939855646165,1.00062534339576),
 .UNSPECIFIED.)
GEOMETRIC_REPRESENTATION_ITEM()
RATIONAL_B_SPLINE_SURFACE(((1.000428625731,0.717810580914592,1.00035266240945),
(1.00045905072597,0.697780025035142,1.00037769532571),(1.00051114946329,
0.663480375353458,1.00042056084894),(1.00059665225219,0.607188882365371,
1.00049091038087),(1.00062840114513,0.586286726926422,1.0005170325669),
(1.00061268510755,0.596633514797481,1.00050410180871)))
REPRESENTATION_ITEM('')
SURFACE()
) ;
#381 = (
BOUNDED_SURFACE()
B_SPLINE_SURFACE(3,2,((#102979,#102980,#102981),(#102982,#102983,#102984),
(#102985,#102986,#102987),(#102988,#102989,#102990),(#102991,#102992,#102993),
(#102994,#102995,#102996),(#102997,#102998,#102999),(#103000,#103001,#103002)),
 .UNSPECIFIED.,.F.,.F.,.F.)
B_SPLINE_SURFACE_WITH_KNOTS((4,2,2,4),(3,3),(6.28318530717959,6.67588438887831,
7.06858347057703,7.85398163397448),(0.,1.),.UNSPECIFIED.)
GEOMETRIC_REPRESENTATION_ITEM()
RATIONAL_B_SPLINE_SURFACE(((1.,0.707106781186548,1.),(1.,0.706675310150437,
1.),(1.,0.726552333979981,1.),(1.,0.787677905717223,1.),(1.,0.828238301901761,
1.),(1.,0.941599607549792,1.),(1.,1.00267605951746,1.),(1.,1.,1.)))
REPRESENTATION_ITEM('')
SURFACE()
) ;
#382 = (
BOUNDED_SURFACE()
B_SPLINE_SURFACE(3,2,((#103010,#103011,#103012),(#103013,#103014,#103015),
(#103016,#103017,#103018),(#103019,#103020,#103021),(#103022,#103023,#103024),
(#103025,#103026,#103027),(#103028,#103029,#103030),(#103031,#103032,#103033)),
 .UNSPECIFIED.,.F.,.F.,.F.)
B_SPLINE_SURFACE_WITH_KNOTS((4,2,2,4),(3,3),(4.71238898038469,5.49778714378214,
5.89048622548086,6.28318530717959),(0.,1.),.UNSPECIFIED.)
GEOMETRIC_REPRESENTATION_ITEM()
RATIONAL_B_SPLINE_SURFACE(((1.,1.,1.),(1.,1.00267605951745,1.),(1.,0.941599607549811,
1.),(1.,0.828238301901754,1.),(1.,0.787677905717215,1.),(1.,0.72655233397999,
1.),(1.,0.706675310150431,1.),(1.,0.707106781186547,1.)))
REPRESENTATION_ITEM('')
SURFACE()
) ;
#383 = (
BOUNDED_SURFACE()
B_SPLINE_SURFACE(3,2,((#103034,#103035,#103036),(#103037,#103038,#103039),
(#103040,#103041,#103042),(#103043,#103044,#103045),(#103046,#103047,#103048),
(#103049,#103050,#103051),(#103052,#103053,#103054),(#103055,#103056,#103057)),
 .UNSPECIFIED.,.F.,.F.,.F.)
B_SPLINE_SURFACE_WITH_KNOTS((4,2,2,4),(3,3),(4.71238898038469,5.49778714378214,
5.89048622548086,6.28318530717959),(0.,1.),.UNSPECIFIED.)
GEOMETRIC_REPRESENTATION_ITEM()
RATIONAL_B_SPLINE_SURFACE(((1.,1.,1.),(1.,1.00267605951745,1.),(1.,0.941599607549811,
1.),(1.,0.828238301901754,1.),(1.,0.787677905717212,1.),(1.,0.726552333979993,
1.),(1.,0.706675310150429,1.),(1.,0.707106781186548,1.)))
REPRESENTATION_ITEM('')
SURFACE()
) ;
#384 = (
BOUNDED_SURFACE()
B_SPLINE_SURFACE(3,2,((#103065,#103066,#103067),(#103068,#103069,#103070),
(#103071,#103072,#103073),(#103074,#103075,#103076),(#103077,#103078,#103079),
(#103080,#103081,#103082),(#103083,#103084,#103085),(#103086,#103087,#103088)),
 .UNSPECIFIED.,.F.,.F.,.F.)
B_SPLINE_SURFACE_WITH_KNOTS((4,2,2,4),(3,3),(6.28318530717959,6.67588438887831,
7.06858347057703,7.85398163397448),(0.,1.),.UNSPECIFIED.)
GEOMETRIC_REPRESENTATION_ITEM()
RATIONAL_B_SPLINE_SURFACE(((1.,0.707106781186548,1.),(1.,0.70667531015044,
1.),(1.,0.726552333979978,1.),(1.,0.787677905717225,1.),(1.,0.828238301901761,
1.),(1.,0.941599607549792,1.),(1.,1.00267605951746,1.),(1.,1.,1.)))
REPRESENTATION_ITEM('')
SURFACE()
) ;
#385 = (
BOUNDED_SURFACE()
B_SPLINE_SURFACE(3,2,((#103089,#103090,#103091),(#103092,#103093,#103094),
(#103095,#103096,#103097),(#103098,#103099,#103100),(#103101,#103102,#103103),
(#103104,#103105,#103106)),.UNSPECIFIED.,.F.,.F.,.F.)
B_SPLINE_SURFACE_WITH_KNOTS((4,2,4),(3,3),(2.06095632820092,2.9281173096476,
3.79527829109429),(0.,1.),.UNSPECIFIED.)
GEOMETRIC_REPRESENTATION_ITEM()
RATIONAL_B_SPLINE_SURFACE(((1.,0.763019982472727,1.),(1.,0.792403856906193,
1.),(1.,0.812400188579439,1.),(1.,0.825457041220947,1.),(1.,0.818529518851321,
1.),(1.,0.799131938862213,1.)))
REPRESENTATION_ITEM('')
SURFACE()
) ;
#386 = (
BOUNDED_SURFACE()
B_SPLINE_SURFACE(3,2,((#103129,#103130,#103131),(#103132,#103133,#103134),
(#103135,#103136,#103137),(#103138,#103139,#103140),(#103141,#103142,#103143),
(#103144,#103145,#103146)),.UNSPECIFIED.,.F.,.F.,.F.)
B_SPLINE_SURFACE_WITH_KNOTS((4,2,4),(3,3),(2.13522523980987,3.02435044878099,
3.9134756577521),(0.,1.),.UNSPECIFIED.)
GEOMETRIC_REPRESENTATION_ITEM()
RATIONAL_B_SPLINE_SURFACE(((1.,0.749240327740277,1.),(1.,0.768579562596357,
1.),(1.,0.780993049743008,1.),(1.,0.78606840104594,1.),(1.,0.778729916329032,
1.),(1.,0.763019982472727,1.)))
REPRESENTATION_ITEM('')
SURFACE()
) ;
#387 = (
BOUNDED_SURFACE()
B_SPLINE_SURFACE(3,2,((#103303,#103304,#103305),(#103306,#103307,#103308),
(#103309,#103310,#103311),(#103312,#103313,#103314),(#103315,#103316,#103317),
(#103318,#103319,#103320),(#103321,#103322,#103323),(#103324,#103325,#103326),
(#103327,#103328,#103329),(#103330,#103331,#103332),(#103333,#103334,#103335),
(#103336,#103337,#103338),(#103339,#103340,#103341),(#103342,#103343,#103344),
(#103345,#103346,#103347),(#103348,#103349,#103350),(#103351,#103352,#103353),
(#103354,#103355,#103356)),.UNSPECIFIED.,.F.,.F.,.F.)
B_SPLINE_SURFACE_WITH_KNOTS((4,2,2,2,2,2,2,2,4),(3,3),(-2.88136898045006E-5,
0.000144068449022501,0.000180085561278126,0.000216102673533752,0.000234111229661564,
0.000243115507725471,0.000252119785789377,0.00027012834191719,0.000315232069289129),
(-0.00230043332376221,1.00649231299482),.UNSPECIFIED.)
GEOMETRIC_REPRESENTATION_ITEM()
RATIONAL_B_SPLINE_SURFACE(((1.00137797387137,0.698547958833496,1.00390520040674),
(1.00130996746141,0.713425360736485,1.00371246913268),(1.0013392130407,
0.707027460342999,1.00379535158098),(1.00112343332548,0.754232445100877,
1.00318382835174),(1.00107694244916,0.76440300773299,1.00305207245063),
(1.00092854904644,0.796866246024035,1.00263152312912),(1.00083723042777,
0.816843536281347,1.00237272467569),(1.0005249519753,0.885159038384459,
1.00148772245255),(1.0003623858312,0.920722772198159,1.00102700735102),
(1.00013066612431,0.97141486445937,1.00037030992561),(1.00008161134638,
0.982146318257361,1.00023128788558),(1.00010185218186,0.977718337948078,
1.00028865074315),(1.00015066464696,0.967039893643917,1.00042698606469),
(1.00027150756266,0.94060372939002,1.00076945685705),(1.00035349548867,
0.922667665317858,1.00100181197542),(1.00060974665136,0.866608956479207,
1.0017280319463),(1.00075148156369,0.8356023608425,1.00212971099755),(1.00085165739564,
0.813687424976079,1.00241361093774)))
REPRESENTATION_ITEM('')
SURFACE()
) ;
#388 = (
BOUNDED_SURFACE()
B_SPLINE_SURFACE(3,2,((#103358,#103359,#103360),(#103361,#103362,#103363),
(#103364,#103365,#103366),(#103367,#103368,#103369)),.UNSPECIFIED.,.F.,
 .F.,.F.)
B_SPLINE_SURFACE_WITH_KNOTS((4,4),(3,3),(5.63598348762742,6.28318530717959),
(0.792338840560963,1.),.UNSPECIFIED.)
GEOMETRIC_REPRESENTATION_ITEM()
RATIONAL_B_SPLINE_SURFACE(((0.934040253948343,0.958376553896462,1.),(0.938725627259265,
0.961333226642434,1.),(0.941220250254381,0.962907441402214,1.),(0.941208919370365,
0.962900291125441,1.)))
REPRESENTATION_ITEM('')
SURFACE()
) ;
#389 = (
BOUNDED_SURFACE()
B_SPLINE_SURFACE(3,2,((#103410,#103411,#103412),(#103413,#103414,#103415),
(#103416,#103417,#103418),(#103419,#103420,#103421),(#103422,#103423,#103424),
(#103425,#103426,#103427),(#103428,#103429,#103430),(#103431,#103432,#103433),
(#103434,#103435,#103436),(#103437,#103438,#103439),(#103440,#103441,#103442),
(#103443,#103444,#103445),(#103446,#103447,#103448),(#103449,#103450,#103451),
(#103452,#103453,#103454),(#103455,#103456,#103457),(#103458,#103459,#103460),
(#103461,#103462,#103463)),.UNSPECIFIED.,.F.,.F.,.F.)
B_SPLINE_SURFACE_WITH_KNOTS((4,2,2,2,2,2,2,2,4),(3,3),(-3.19743590576754E-5,
0.000144068449022546,0.000180085561278183,0.000216102673533819,0.000234111229661638,
0.000243115507725547,0.000252119785789456,0.000270128341917274,0.000288136898045092),
(-0.00668341897260021,1.00019683226132),.UNSPECIFIED.)
GEOMETRIC_REPRESENTATION_ITEM()
RATIONAL_B_SPLINE_SURFACE(((1.00403209003396,0.698291475893957,1.00011798325541),
(1.00381915098312,0.714225030505444,1.00011175243164),(1.00391733895236,
0.706877935813784,1.00011462551636),(1.00327816898458,0.754704999695385,
1.0000959227213),(1.00314250899891,0.764856006670135,1.00009195316541),
(1.00270949829923,0.797256825605574,1.00007928281045),(1.00244303133882,
0.817195704120572,1.00007148570295),(1.0015318054439,0.885379851192721,
1.00004482226126),(1.0010574388042,0.920875204110099,1.00003094178738),
(1.00038128265054,0.971469827113991,1.00001115673707),(1.00023814122158,
0.98218064678933,1.00000696826617),(1.00029720380908,0.97776118046934,1.00000869650048),
(1.00043963817124,0.967103268362387,1.00001286428185),(1.0007922567818,
0.940717934784036,1.00002318227853),(1.00103149685957,0.922816357646008,
1.00003018269841),(1.00145821870303,0.890886113898632,1.00004266903473),
(1.00165232267982,0.87636192821199,1.00004834872414),(1.00182713963607,
0.863280929173223,1.00005346405476)))
REPRESENTATION_ITEM('')
SURFACE()
) ;
#390 = (
BOUNDED_SURFACE()
B_SPLINE_SURFACE(3,2,((#103502,#103503,#103504),(#103505,#103506,#103507),
(#103508,#103509,#103510),(#103511,#103512,#103513)),.UNSPECIFIED.,.F.,
 .F.,.F.)
B_SPLINE_SURFACE_WITH_KNOTS((4,4),(3,3),(5.51130230301728,6.28318530717959),
(0.,1.),.UNSPECIFIED.)
GEOMETRIC_REPRESENTATION_ITEM()
RATIONAL_B_SPLINE_SURFACE(((1.,0.763019982472727,1.),(1.,0.776565014072566,
1.),(1.,0.78408875836913,1.),(1.,0.784033077704815,1.)))
REPRESENTATION_ITEM('')
SURFACE()
) ;
#391 = (
BOUNDED_SURFACE()
B_SPLINE_SURFACE(3,2,((#103518,#103519,#103520),(#103521,#103522,#103523),
(#103524,#103525,#103526),(#103527,#103528,#103529)),.UNSPECIFIED.,.F.,
 .F.,.F.)
B_SPLINE_SURFACE_WITH_KNOTS((4,4),(3,3),(0.0051446850272488,0.00657473287039649),
(0.,1.),.UNSPECIFIED.)
GEOMETRIC_REPRESENTATION_ITEM()
RATIONAL_B_SPLINE_SURFACE(((1.,0.943476662524758,1.),(1.,0.944945702024752,
1.),(1.,0.946300916277096,1.),(1.,0.947565352018496,1.)))
REPRESENTATION_ITEM('')
SURFACE()
) ;
#392 = (
BOUNDED_SURFACE()
B_SPLINE_SURFACE(3,2,((#103568,#103569,#103570),(#103571,#103572,#103573),
(#103574,#103575,#103576),(#103577,#103578,#103579)),.UNSPECIFIED.,.F.,
 .F.,.F.)
B_SPLINE_SURFACE_WITH_KNOTS((4,4),(3,3),(0.0051446850272488,0.00657473287039648),
(0.,1.),.UNSPECIFIED.)
GEOMETRIC_REPRESENTATION_ITEM()
RATIONAL_B_SPLINE_SURFACE(((1.,0.943476662524758,1.),(1.,0.944945702024752,
1.),(1.,0.946300916277096,1.),(1.,0.947565352018496,1.)))
REPRESENTATION_ITEM('')
SURFACE()
) ;
#393 = (
BOUNDED_SURFACE()
B_SPLINE_SURFACE(3,2,((#103584,#103585,#103586),(#103587,#103588,#103589),
(#103590,#103591,#103592),(#103593,#103594,#103595),(#103596,#103597,#103598),
(#103599,#103600,#103601),(#103602,#103603,#103604),(#103605,#103606,#103607),
(#103608,#103609,#103610),(#103611,#103612,#103613),(#103614,#103615,#103616),
(#103617,#103618,#103619),(#103620,#103621,#103622),(#103623,#103624,#103625),
(#103626,#103627,#103628),(#103629,#103630,#103631),(#103632,#103633,#103634),
(#103635,#103636,#103637)),.UNSPECIFIED.,.F.,.F.,.F.)
B_SPLINE_SURFACE_WITH_KNOTS((4,2,2,2,2,2,2,2,4),(3,3),(-2.77591379149742E-5,
0.000125253167969377,0.000156566459961721,0.000187879751954065,0.000203536397950237,
0.000211364720948323,0.000219193043946409,0.000234849689942581,0.000250506335938753),
(0.,1.00287807885248),.UNSPECIFIED.)
GEOMETRIC_REPRESENTATION_ITEM()
RATIONAL_B_SPLINE_SURFACE(((1.,0.698587265144072,1.00173497923611),(1.,
0.713937574732587,1.0016466204333),(1.,0.719549163949171,1.00161431924079),
(1.,0.771808112009009,1.00131350849427),(1.,0.782482243723509,1.00125206650876),
(1.,0.810804881627976,1.00108903693836),(1.,0.827824808964379,1.00099106755248),
(1.,0.868687526094284,1.00075585530843),(1.,0.885097717150239,1.00066139566074),
(1.,0.918597380148661,1.00046856631746),(1.,0.931968622959475,1.00039159933513),
(1.,0.95574199467466,1.00025475605836),(1.,0.963776461019218,1.00020850840301),
(1.,0.96542172890934,1.00019903798156),(1.,0.949947468785993,1.0002881102632),
(1.,0.927474619202833,1.00041746752948),(1.,0.916335140210118,1.00048158812731),
(1.,0.906010523700252,1.00054101824819)))
REPRESENTATION_ITEM('')
SURFACE()
) ;
#394 = (
BOUNDED_SURFACE()
B_SPLINE_SURFACE(3,2,((#103641,#103642,#103643),(#103644,#103645,#103646),
(#103647,#103648,#103649),(#103650,#103651,#103652),(#103653,#103654,#103655),
(#103656,#103657,#103658),(#103659,#103660,#103661),(#103662,#103663,#103664),
(#103665,#103666,#103667),(#103668,#103669,#103670),(#103671,#103672,#103673),
(#103674,#103675,#103676),(#103677,#103678,#103679),(#103680,#103681,#103682),
(#103683,#103684,#103685),(#103686,#103687,#103688),(#103689,#103690,#103691),
(#103692,#103693,#103694)),.UNSPECIFIED.,.F.,.F.,.F.)
B_SPLINE_SURFACE_WITH_KNOTS((4,2,2,2,2,2,2,2,4),(3,3),(-2.79610875103897E-5,
0.000125253167969368,0.00015656645996171,0.000187879751954052,0.000203536397950223,
0.000211364720948308,0.000219193043946394,0.000234849689942565,0.000253195388096685),
(-0.00314610977262661,1.),.UNSPECIFIED.)
GEOMETRIC_REPRESENTATION_ITEM()
RATIONAL_B_SPLINE_SURFACE(((1.00189744483735,0.698445862592737,1.),(1.00180054146108,
0.713846370407001,1.),(1.0017654902188,0.719416939270283,1.),(1.001436217201,
0.771747125052562,1.),(1.00136903527044,0.782424109553829,1.),(1.00119077538533,
0.810754317015262,1.),(1.00108365364399,0.82777879312693,1.),(1.00082646773902,
0.868652431296543,1.),(1.0007231836176,0.885067008168521,1.),(1.00051234004796,
0.918575624344433,1.),(1.00042818276659,0.931950440776527,1.),(1.00027855551348,
0.955730166204014,1.),(1.00022798737599,0.963766779853875,1.),(1.00021763222242,
0.965412487461153,1.),(1.00031502568701,0.949934091660457,1.),(1.00046861400988,
0.92552484754986,1.),(1.00055064362451,0.912488173602249,1.),(1.00062456604608,
0.900739946914071,0.999999999999999)))
REPRESENTATION_ITEM('')
SURFACE()
) ;
#395 = (
BOUNDED_SURFACE()
B_SPLINE_SURFACE(3,2,((#103697,#103698,#103699),(#103700,#103701,#103702),
(#103703,#103704,#103705),(#103706,#103707,#103708)),.UNSPECIFIED.,.F.,
 .F.,.F.)
B_SPLINE_SURFACE_WITH_KNOTS((4,4),(3,3),(-1.77635683940025E-15,1.00173611575493),
(0.800638603120394,1.),.UNSPECIFIED.)
GEOMETRIC_REPRESENTATION_ITEM()
RATIONAL_B_SPLINE_SURFACE(((0.931056261594762,0.956944532691443,1.),(0.931106613485818,
0.956975977522394,1.),(0.926966069646246,0.954390201728275,1.),(0.920044734228402,
0.95006781745223,1.)))
REPRESENTATION_ITEM('')
SURFACE()
) ;
#396 = (
BOUNDED_SURFACE()
B_SPLINE_SURFACE(3,2,((#103734,#103735,#103736),(#103737,#103738,#103739),
(#103740,#103741,#103742),(#103743,#103744,#103745)),.UNSPECIFIED.,.F.,
 .F.,.F.)
B_SPLINE_SURFACE_WITH_KNOTS((4,4),(3,3),(3.32036915323687E-15,1.08063632538888),
(0.,1.),.UNSPECIFIED.)
GEOMETRIC_REPRESENTATION_ITEM()
RATIONAL_B_SPLINE_SURFACE(((1.,0.821344978643199,1.),(1.,0.821618737292291,
1.),(1.,0.79966308458184,1.),(1.,0.763019982472727,1.)))
REPRESENTATION_ITEM('')
SURFACE()
) ;
#397 = (
BOUNDED_SURFACE()
B_SPLINE_SURFACE(3,2,((#105212,#105213,#105214),(#105215,#105216,#105217),
(#105218,#105219,#105220),(#105221,#105222,#105223),(#105224,#105225,#105226),
(#105227,#105228,#105229)),.UNSPECIFIED.,.F.,.F.,.F.)
B_SPLINE_SURFACE_WITH_KNOTS((4,2,4),(3,3),(9.07204043127111E-5,0.000289236237441535,
0.000487752070570357),(-0.000844756555506173,1.00064307855256),
 .UNSPECIFIED.)
GEOMETRIC_REPRESENTATION_ITEM()
RATIONAL_B_SPLINE_SURFACE(((1.00067853369529,0.598126578821862,1.00051643581309),
(1.00070177595154,0.5843609469861,1.00053412562509),(1.00066498743048,0.606149590529492,
1.00050612567475),(1.0005663262558,0.664583392836358,1.00043103409958),
(1.00050548323105,0.700618735924326,1.00038472613115),(1.00047271456518,
0.720026550084179,1.00035978571519)))
REPRESENTATION_ITEM('')
SURFACE()
) ;
#398 = (
BOUNDED_SURFACE()
B_SPLINE_SURFACE(3,2,((#105244,#105245,#105246),(#105247,#105248,#105249),
(#105250,#105251,#105252),(#105253,#105254,#105255),(#105256,#105257,#105258),
(#105259,#105260,#105261)),.UNSPECIFIED.,.F.,.F.,.F.)
B_SPLINE_SURFACE_WITH_KNOTS((4,2,4),(3,3),(0.000107162911540596,0.000298022515767417,
0.000488882119994237),(-0.00075993985561925,1.00062534339583),
 .UNSPECIFIED.)
GEOMETRIC_REPRESENTATION_ITEM()
RATIONAL_B_SPLINE_SURFACE(((1.00042862573099,0.717810580914598,1.00035266240949),
(1.00045905072595,0.697780025035093,1.00037769532575),(1.00051114946327,
0.663480375353471,1.00042056084899),(1.00059665225217,0.607188882365325,
1.00049091038093),(1.0006284011451,0.586286726926441,1.00051703256696),
(1.00061268510753,0.596633514797444,1.00050410180877)))
REPRESENTATION_ITEM('')
SURFACE()
) ;
#399 = (
BOUNDED_SURFACE()
B_SPLINE_SURFACE(3,2,((#105491,#105492,#105493),(#105494,#105495,#105496),
(#105497,#105498,#105499),(#105500,#105501,#105502),(#105503,#105504,#105505),
(#105506,#105507,#105508),(#105509,#105510,#105511),(#105512,#105513,#105514)),
 .UNSPECIFIED.,.F.,.F.,.F.)
B_SPLINE_SURFACE_WITH_KNOTS((4,2,2,4),(3,3),(6.28318530717959,6.67588438887831,
7.06858347057703,7.85398163397448),(0.,1.),.UNSPECIFIED.)
GEOMETRIC_REPRESENTATION_ITEM()
RATIONAL_B_SPLINE_SURFACE(((1.,0.707106781186548,1.),(1.,0.706675310150414,
1.),(1.,0.726552333980012,1.),(1.,0.787677905717191,1.),(1.,0.828238301901766,
1.),(1.,0.941599607549786,1.),(1.,1.00267605951747,1.),(1.,1.,1.)))
REPRESENTATION_ITEM('')
SURFACE()
) ;
#400 = (
BOUNDED_SURFACE()
B_SPLINE_SURFACE(3,2,((#105522,#105523,#105524),(#105525,#105526,#105527),
(#105528,#105529,#105530),(#105531,#105532,#105533),(#105534,#105535,#105536),
(#105537,#105538,#105539),(#105540,#105541,#105542),(#105543,#105544,#105545)),
 .UNSPECIFIED.,.F.,.F.,.F.)
B_SPLINE_SURFACE_WITH_KNOTS((4,2,2,4),(3,3),(4.71238898038469,5.49778714378214,
5.89048622548086,6.28318530717959),(0.,1.),.UNSPECIFIED.)
GEOMETRIC_REPRESENTATION_ITEM()
RATIONAL_B_SPLINE_SURFACE(((1.,1.,1.),(1.,1.00267605951742,1.),(1.,0.941599607549841,
1.),(1.,0.82823830190174,1.),(1.,0.787677905717214,1.),(1.,0.726552333979992,
1.),(1.,0.706675310150431,1.),(1.,0.707106781186548,1.)))
REPRESENTATION_ITEM('')
SURFACE()
) ;
#401 = (
BOUNDED_SURFACE()
B_SPLINE_SURFACE(3,2,((#105546,#105547,#105548),(#105549,#105550,#105551),
(#105552,#105553,#105554),(#105555,#105556,#105557),(#105558,#105559,#105560),
(#105561,#105562,#105563),(#105564,#105565,#105566),(#105567,#105568,#105569)),
 .UNSPECIFIED.,.F.,.F.,.F.)
B_SPLINE_SURFACE_WITH_KNOTS((4,2,2,4),(3,3),(4.71238898038469,5.49778714378214,
5.89048622548086,6.28318530717959),(0.,1.),.UNSPECIFIED.)
GEOMETRIC_REPRESENTATION_ITEM()
RATIONAL_B_SPLINE_SURFACE(((1.,1.,1.),(1.,1.00267605951742,1.),(1.,0.94159960754984,
1.),(1.,0.828238301901739,1.),(1.,0.787677905717214,1.),(1.,0.726552333979992,
1.),(1.,0.70667531015043,1.),(1.,0.707106781186548,1.)))
REPRESENTATION_ITEM('')
SURFACE()
) ;
#402 = (
BOUNDED_SURFACE()
B_SPLINE_SURFACE(3,2,((#105577,#105578,#105579),(#105580,#105581,#105582),
(#105583,#105584,#105585),(#105586,#105587,#105588),(#105589,#105590,#105591),
(#105592,#105593,#105594),(#105595,#105596,#105597),(#105598,#105599,#105600)),
 .UNSPECIFIED.,.F.,.F.,.F.)
B_SPLINE_SURFACE_WITH_KNOTS((4,2,2,4),(3,3),(6.28318530717959,6.67588438887831,
7.06858347057703,7.85398163397448),(0.,1.),.UNSPECIFIED.)
GEOMETRIC_REPRESENTATION_ITEM()
RATIONAL_B_SPLINE_SURFACE(((1.,0.707106781186548,1.),(1.,0.706675310150437,
1.),(1.,0.726552333979981,1.),(1.,0.787677905717222,1.),(1.,0.828238301901765,
1.),(1.,0.941599607549785,1.),(1.,1.00267605951747,1.),(1.,1.,1.)))
REPRESENTATION_ITEM('')
SURFACE()
) ;
#403 = (
BOUNDED_SURFACE()
B_SPLINE_SURFACE(3,2,((#105601,#105602,#105603),(#105604,#105605,#105606),
(#105607,#105608,#105609),(#105610,#105611,#105612),(#105613,#105614,#105615),
(#105616,#105617,#105618)),.UNSPECIFIED.,.F.,.F.,.F.)
B_SPLINE_SURFACE_WITH_KNOTS((4,2,4),(3,3),(2.06095632820092,2.9281173096476,
3.79527829109429),(0.,1.),.UNSPECIFIED.)
GEOMETRIC_REPRESENTATION_ITEM()
RATIONAL_B_SPLINE_SURFACE(((1.,0.763019982472727,1.),(1.,0.792403856906172,
1.),(1.,0.812400188579468,1.),(1.,0.825457041220918,1.),(1.,0.818529518851342,
1.),(1.,0.799131938862213,1.)))
REPRESENTATION_ITEM('')
SURFACE()
) ;
#404 = (
BOUNDED_SURFACE()
B_SPLINE_SURFACE(3,2,((#105641,#105642,#105643),(#105644,#105645,#105646),
(#105647,#105648,#105649),(#105650,#105651,#105652),(#105653,#105654,#105655),
(#105656,#105657,#105658)),.UNSPECIFIED.,.F.,.F.,.F.)
B_SPLINE_SURFACE_WITH_KNOTS((4,2,4),(3,3),(2.13522523980988,3.02435044878099,
3.9134756577521),(0.,1.),.UNSPECIFIED.)
GEOMETRIC_REPRESENTATION_ITEM()
RATIONAL_B_SPLINE_SURFACE(((1.,0.749240327740277,1.),(1.,0.76857956259632,
1.),(1.,0.780993049743057,1.),(1.,0.786068401045891,1.),(1.,0.778729916329069,
1.),(1.,0.763019982472727,1.)))
REPRESENTATION_ITEM('')
SURFACE()
) ;
#405 = (
BOUNDED_SURFACE()
B_SPLINE_SURFACE(3,2,((#105815,#105816,#105817),(#105818,#105819,#105820),
(#105821,#105822,#105823),(#105824,#105825,#105826),(#105827,#105828,#105829),
(#105830,#105831,#105832),(#105833,#105834,#105835),(#105836,#105837,#105838),
(#105839,#105840,#105841),(#105842,#105843,#105844),(#105845,#105846,#105847),
(#105848,#105849,#105850),(#105851,#105852,#105853),(#105854,#105855,#105856),
(#105857,#105858,#105859),(#105860,#105861,#105862),(#105863,#105864,#105865),
(#105866,#105867,#105868)),.UNSPECIFIED.,.F.,.F.,.F.)
B_SPLINE_SURFACE_WITH_KNOTS((4,2,2,2,2,2,2,2,4),(3,3),(-2.88136898044879E-5,
0.000144068449022439,0.000180085561278049,0.000216102673533659,0.000234111229661463,
0.000243115507725366,0.000252119785789268,0.000270128341917073,0.000315232069288994),
(-0.00230043332309208,1.00649231299495),.UNSPECIFIED.)
GEOMETRIC_REPRESENTATION_ITEM()
RATIONAL_B_SPLINE_SURFACE(((1.00137797387097,0.698547958833687,1.00390520040681),
(1.00130996746102,0.71342536073659,1.00371246913275),(1.00133921304031,
0.707027460343199,1.00379535158106),(1.00112343332516,0.754232445100949,
1.0031838283518),(1.00107694244884,0.764403007733067,1.00305207245068),
(1.00092854904617,0.796866246023982,1.00263152312917),(1.00083723042752,
0.81684353628167,1.00237272467573),(1.00052495197515,0.885159038383876,
1.00148772245259),(1.0003623858311,0.920722772198335,1.00102700735104),
(1.00013066612427,0.971414864458886,1.00037030992563),(1.00008161134636,
0.98214631825728,1.00023128788558),(1.00010185218183,0.977718337948346,
1.00028865074315),(1.00015066464691,0.967039893644153,1.00042698606469),
(1.00027150756258,0.940603729390226,1.00076945685706),(1.00035349548857,
0.922667665318029,1.00100181197544),(1.00060974665118,0.866608956479267,
1.00172803194633),(1.00075148156347,0.835602360842649,1.00212971099759),
(1.0008516573954,0.813687424975539,1.0024136109378)))
REPRESENTATION_ITEM('')
SURFACE()
) ;
#406 = (
BOUNDED_SURFACE()
B_SPLINE_SURFACE(3,2,((#105870,#105871,#105872),(#105873,#105874,#105875),
(#105876,#105877,#105878),(#105879,#105880,#105881)),.UNSPECIFIED.,.F.,
 .F.,.F.)
B_SPLINE_SURFACE_WITH_KNOTS((4,4),(3,3),(5.63598348762742,6.28318530717959),
(0.792338840560958,1.),.UNSPECIFIED.)
GEOMETRIC_REPRESENTATION_ITEM()
RATIONAL_B_SPLINE_SURFACE(((0.934040253948341,0.958376553896461,1.),(0.938725627259263,
0.961333226642432,1.),(0.94122025025438,0.962907441402213,1.),(0.941208919370364,
0.96290029112544,1.)))
REPRESENTATION_ITEM('')
SURFACE()
) ;
#407 = (
BOUNDED_SURFACE()
B_SPLINE_SURFACE(3,2,((#105922,#105923,#105924),(#105925,#105926,#105927),
(#105928,#105929,#105930),(#105931,#105932,#105933),(#105934,#105935,#105936),
(#105937,#105938,#105939),(#105940,#105941,#105942),(#105943,#105944,#105945),
(#105946,#105947,#105948),(#105949,#105950,#105951),(#105952,#105953,#105954),
(#105955,#105956,#105957),(#105958,#105959,#105960),(#105961,#105962,#105963),
(#105964,#105965,#105966),(#105967,#105968,#105969),(#105970,#105971,#105972),
(#105973,#105974,#105975)),.UNSPECIFIED.,.F.,.F.,.F.)
B_SPLINE_SURFACE_WITH_KNOTS((4,2,2,2,2,2,2,2,4),(3,3),(-3.19743590576624E-5,
0.000144068449022547,0.000180085561278184,0.000216102673533821,0.000234111229661639,
0.000243115507725548,0.000252119785789458,0.000270128341917276,0.000288136898045094),
(-0.0066834189723838,1.00019683226129),.UNSPECIFIED.)
GEOMETRIC_REPRESENTATION_ITEM()
RATIONAL_B_SPLINE_SURFACE(((1.00403209003383,0.698291475894096,1.00011798325539),
(1.003819150983,0.714225030505405,1.00011175243162),(1.00391733895223,0.706877935813939,
1.00011462551634),(1.00327816898448,0.75470499969543,1.00009592272129),
(1.00314250899881,0.764856006670175,1.0000919531654),(1.00270949829915,
0.797256825605654,1.00007928281044),(1.00244303133874,0.817195704120573,
1.00007148570294),(1.00153180544385,0.885379851192701,1.00004482226125),
(1.00105743880416,0.920875204110361,1.00003094178737),(1.00038128265052,
0.971469827114154,1.00001115673707),(1.00023814122157,0.982180646789333,
1.00000696826617),(1.00029720380907,0.977761180469344,1.00000869650048),
(1.00043963817123,0.967103268362389,1.00001286428185),(1.00079225678177,
0.940717934784047,1.00002318227853),(1.00103149685954,0.922816357646006,
1.0000301826984),(1.00145821870299,0.890886113898669,1.00004266903472),
(1.00165232267976,0.876361928212014,1.00004834872413),(1.00182713963601,
0.863280929173256,1.00005346405475)))
REPRESENTATION_ITEM('')
SURFACE()
) ;
#408 = (
BOUNDED_SURFACE()
B_SPLINE_SURFACE(3,2,((#106014,#106015,#106016),(#106017,#106018,#106019),
(#106020,#106021,#106022),(#106023,#106024,#106025)),.UNSPECIFIED.,.F.,
 .F.,.F.)
B_SPLINE_SURFACE_WITH_KNOTS((4,4),(3,3),(5.51130230301728,6.28318530717958),
(0.,1.),.UNSPECIFIED.)
GEOMETRIC_REPRESENTATION_ITEM()
RATIONAL_B_SPLINE_SURFACE(((1.,0.763019982472727,1.),(1.,0.776565014072565,
1.),(1.,0.784088758369132,1.),(1.,0.784033077704815,1.)))
REPRESENTATION_ITEM('')
SURFACE()
) ;
#409 = (
BOUNDED_SURFACE()
B_SPLINE_SURFACE(3,2,((#106030,#106031,#106032),(#106033,#106034,#106035),
(#106036,#106037,#106038),(#106039,#106040,#106041)),.UNSPECIFIED.,.F.,
 .F.,.F.)
B_SPLINE_SURFACE_WITH_KNOTS((4,4),(3,3),(0.0051446850272488,0.00657473287039649),
(0.,1.),.UNSPECIFIED.)
GEOMETRIC_REPRESENTATION_ITEM()
RATIONAL_B_SPLINE_SURFACE(((1.,0.943476662524758,1.),(1.,0.944945702024752,
1.),(1.,0.946300916277095,1.),(1.,0.947565352018496,1.)))
REPRESENTATION_ITEM('')
SURFACE()
) ;
#410 = (
BOUNDED_SURFACE()
B_SPLINE_SURFACE(3,2,((#106080,#106081,#106082),(#106083,#106084,#106085),
(#106086,#106087,#106088),(#106089,#106090,#106091)),.UNSPECIFIED.,.F.,
 .F.,.F.)
B_SPLINE_SURFACE_WITH_KNOTS((4,4),(3,3),(0.0051446850272488,0.00657473287039648),
(0.,1.),.UNSPECIFIED.)
GEOMETRIC_REPRESENTATION_ITEM()
RATIONAL_B_SPLINE_SURFACE(((1.,0.943476662524758,1.),(1.,0.944945702024752,
1.),(1.,0.946300916277093,1.),(1.,0.947565352018496,1.)))
REPRESENTATION_ITEM('')
SURFACE()
) ;
#411 = (
BOUNDED_SURFACE()
B_SPLINE_SURFACE(3,2,((#106096,#106097,#106098),(#106099,#106100,#106101),
(#106102,#106103,#106104),(#106105,#106106,#106107),(#106108,#106109,#106110),
(#106111,#106112,#106113),(#106114,#106115,#106116),(#106117,#106118,#106119),
(#106120,#106121,#106122),(#106123,#106124,#106125),(#106126,#106127,#106128),
(#106129,#106130,#106131),(#106132,#106133,#106134),(#106135,#106136,#106137),
(#106138,#106139,#106140),(#106141,#106142,#106143),(#106144,#106145,#106146),
(#106147,#106148,#106149)),.UNSPECIFIED.,.F.,.F.,.F.)
B_SPLINE_SURFACE_WITH_KNOTS((4,2,2,2,2,2,2,2,4),(3,3),(-2.77591379149735E-5,
0.000125253167969377,0.000156566459961721,0.000187879751954065,0.000203536397950237,
0.000211364720948323,0.000219193043946409,0.000234849689942581,0.000250506335938753),
(0.,1.00287807885233),.UNSPECIFIED.)
GEOMETRIC_REPRESENTATION_ITEM()
RATIONAL_B_SPLINE_SURFACE(((1.,0.698587265144123,1.00173497923602),(1.,
0.713937574732621,1.00164662043321),(1.,0.719549163949218,1.00161431924071),
(1.,0.771808112009042,1.0013135084942),(1.,0.782482243723491,1.00125206650869),
(1.,0.810804881628056,1.0010890369383),(1.,0.82782480896442,1.00099106755243),
(1.,0.868687526094324,1.00075585530839),(1.,0.885097717150333,1.00066139566071),
(1.,0.918597380148702,1.00046856631744),(1.,0.931968622959456,1.00039159933511),
(1.,0.955741994674696,1.00025475605835),(1.,0.963776461019225,1.00020850840299),
(1.,0.965421728909339,1.00019903798155),(1.,0.949947468785964,1.00028811026319),
(1.,0.927474619202864,1.00041746752946),(1.,0.91633514021013,1.00048158812729),
(1.,0.906010523700257,1.00054101824816)))
REPRESENTATION_ITEM('')
SURFACE()
) ;
#412 = (
BOUNDED_SURFACE()
B_SPLINE_SURFACE(3,2,((#106153,#106154,#106155),(#106156,#106157,#106158),
(#106159,#106160,#106161),(#106162,#106163,#106164),(#106165,#106166,#106167),
(#106168,#106169,#106170),(#106171,#106172,#106173),(#106174,#106175,#106176),
(#106177,#106178,#106179),(#106180,#106181,#106182),(#106183,#106184,#106185),
(#106186,#106187,#106188),(#106189,#106190,#106191),(#106192,#106193,#106194),
(#106195,#106196,#106197),(#106198,#106199,#106200),(#106201,#106202,#106203),
(#106204,#106205,#106206)),.UNSPECIFIED.,.F.,.F.,.F.)
B_SPLINE_SURFACE_WITH_KNOTS((4,2,2,2,2,2,2,2,4),(3,3),(-2.79610875103821E-5,
0.000125253167969377,0.000156566459961721,0.000187879751954065,0.000203536397950237,
0.000211364720948323,0.000219193043946409,0.000234849689942581,0.00025319538809668),
(-0.00314610977277591,1.),.UNSPECIFIED.)
GEOMETRIC_REPRESENTATION_ITEM()
RATIONAL_B_SPLINE_SURFACE(((1.00189744483744,0.698445862592552,0.999999999999999),
(1.00180054146116,0.713846370407211,1.),(1.00176549021887,0.719416939270069,
1.),(1.00143621720107,0.771747125052571,1.),(1.00136903527051,0.782424109553791,
1.),(1.00119077538539,0.810754317015272,1.),(1.00108365364405,0.827778793126799,
1.),(1.00082646773906,0.868652431296628,1.),(1.00072318361763,0.885067008168634,
1.),(1.00051234004798,0.918575624344512,1.),(1.00042818276661,0.931950440776572,
1.),(1.00027855551349,0.955730166204094,1.),(1.000227987376,0.96376677985388,
1.),(1.00021763222243,0.965412487461141,1.),(1.00031502568702,0.949934091660348,
1.),(1.0004686140099,0.925524847549937,1.),(1.00055064362453,0.912488173602174,
1.),(1.00062456604613,0.90073994691414,1.)))
REPRESENTATION_ITEM('')
SURFACE()
) ;
#413 = (
BOUNDED_SURFACE()
B_SPLINE_SURFACE(3,2,((#106209,#106210,#106211),(#106212,#106213,#106214),
(#106215,#106216,#106217),(#106218,#106219,#106220)),.UNSPECIFIED.,.F.,
 .F.,.F.)
B_SPLINE_SURFACE_WITH_KNOTS((4,4),(3,3),(-1.77635683940025E-15,1.00173611575494),
(0.800638603120415,1.),.UNSPECIFIED.)
GEOMETRIC_REPRESENTATION_ITEM()
RATIONAL_B_SPLINE_SURFACE(((0.931056261594767,0.956944532691447,1.),(0.931106613485823,
0.956975977522398,1.),(0.926966069646252,0.95439020172828,1.),(0.920044734228408,
0.950067817452235,1.)))
REPRESENTATION_ITEM('')
SURFACE()
) ;
#414 = (
BOUNDED_SURFACE()
B_SPLINE_SURFACE(3,2,((#106246,#106247,#106248),(#106249,#106250,#106251),
(#106252,#106253,#106254),(#106255,#106256,#106257)),.UNSPECIFIED.,.F.,
 .F.,.F.)
B_SPLINE_SURFACE_WITH_KNOTS((4,4),(3,3),(-8.88178419700125E-16,1.08063632538888),
(0.,1.),.UNSPECIFIED.)
GEOMETRIC_REPRESENTATION_ITEM()
RATIONAL_B_SPLINE_SURFACE(((1.,0.821344978643199,1.),(1.,0.821618737292292,
1.),(1.,0.799663084581839,1.),(1.,0.763019982472728,1.)))
REPRESENTATION_ITEM('')
SURFACE()
) ;
#415 = (
BOUNDED_SURFACE()
B_SPLINE_SURFACE(3,2,((#107724,#107725,#107726),(#107727,#107728,#107729),
(#107730,#107731,#107732),(#107733,#107734,#107735),(#107736,#107737,#107738),
(#107739,#107740,#107741)),.UNSPECIFIED.,.F.,.F.,.F.)
B_SPLINE_SURFACE_WITH_KNOTS((4,2,4),(3,3),(9.07204043127126E-5,0.000289236237441534,
0.000487752070570335),(-0.000844756556539755,1.00064307855249),
 .UNSPECIFIED.)
GEOMETRIC_REPRESENTATION_ITEM()
RATIONAL_B_SPLINE_SURFACE(((1.00067853369612,0.598126578821559,1.00051643581304),
(1.0007017759524,0.584360946985556,1.00053412562504),(1.00066498743129,
0.60614959052921,1.00050612567469),(1.00056632625649,0.664583392835936,
1.00043103409954),(1.00050548323167,0.700618735924161,1.00038472613111),
(1.00047271456577,0.720026550083823,1.00035978571515)))
REPRESENTATION_ITEM('')
SURFACE()
) ;
#416 = (
BOUNDED_SURFACE()
B_SPLINE_SURFACE(3,2,((#107756,#107757,#107758),(#107759,#107760,#107761),
(#107762,#107763,#107764),(#107765,#107766,#107767),(#107768,#107769,#107770),
(#107771,#107772,#107773)),.UNSPECIFIED.,.F.,.F.,.F.)
B_SPLINE_SURFACE_WITH_KNOTS((4,2,4),(3,3),(0.000107162911540598,0.000298022515767418,
0.000488882119994237),(-0.000759939855667643,1.00062534339582),
 .UNSPECIFIED.)
GEOMETRIC_REPRESENTATION_ITEM()
RATIONAL_B_SPLINE_SURFACE(((1.00042862573101,0.717810580914495,1.00035266240948),
(1.00045905072598,0.697780025035261,1.00037769532575),(1.0005111494633,
0.663480375353317,1.00042056084899),(1.00059665225221,0.607188882365452,
1.00049091038093),(1.00062840114514,0.586286726926244,1.00051703256695),
(1.00061268510756,0.596633514797517,1.00050410180877)))
REPRESENTATION_ITEM('')
SURFACE()
) ;
#417 = (
BOUNDED_SURFACE()
B_SPLINE_SURFACE(3,2,((#108003,#108004,#108005),(#108006,#108007,#108008),
(#108009,#108010,#108011),(#108012,#108013,#108014),(#108015,#108016,#108017),
(#108018,#108019,#108020),(#108021,#108022,#108023),(#108024,#108025,#108026)),
 .UNSPECIFIED.,.F.,.F.,.F.)
B_SPLINE_SURFACE_WITH_KNOTS((4,2,2,4),(3,3),(6.28318530717959,6.67588438887831,
7.06858347057703,7.85398163397448),(0.,1.),.UNSPECIFIED.)
GEOMETRIC_REPRESENTATION_ITEM()
RATIONAL_B_SPLINE_SURFACE(((1.,0.707106781186548,1.),(1.,0.706675310150441,
1.),(1.,0.726552333979978,1.),(1.,0.787677905717226,1.),(1.,0.828238301901708,
1.),(1.,0.941599607549899,1.),(1.,1.00267605951738,1.),(1.,1.,1.)))
REPRESENTATION_ITEM('')
SURFACE()
) ;
#418 = (
BOUNDED_SURFACE()
B_SPLINE_SURFACE(3,2,((#108034,#108035,#108036),(#108037,#108038,#108039),
(#108040,#108041,#108042),(#108043,#108044,#108045),(#108046,#108047,#108048),
(#108049,#108050,#108051),(#108052,#108053,#108054),(#108055,#108056,#108057)),
 .UNSPECIFIED.,.F.,.F.,.F.)
B_SPLINE_SURFACE_WITH_KNOTS((4,2,2,4),(3,3),(4.71238898038469,5.49778714378214,
5.89048622548086,6.28318530717959),(0.,1.),.UNSPECIFIED.)
GEOMETRIC_REPRESENTATION_ITEM()
RATIONAL_B_SPLINE_SURFACE(((1.,1.,1.),(1.,1.0026760595174,1.),(1.,0.94159960754987,
1.),(1.,0.828238301901727,1.),(1.,0.787677905717214,1.),(1.,0.726552333979982,
1.),(1.,0.706675310150449,1.),(1.,0.707106781186548,1.)))
REPRESENTATION_ITEM('')
SURFACE()
) ;
#419 = (
BOUNDED_SURFACE()
B_SPLINE_SURFACE(3,2,((#108058,#108059,#108060),(#108061,#108062,#108063),
(#108064,#108065,#108066),(#108067,#108068,#108069),(#108070,#108071,#108072),
(#108073,#108074,#108075),(#108076,#108077,#108078),(#108079,#108080,#108081)),
 .UNSPECIFIED.,.F.,.F.,.F.)
B_SPLINE_SURFACE_WITH_KNOTS((4,2,2,4),(3,3),(4.71238898038469,5.49778714378214,
5.89048622548086,6.28318530717959),(0.,1.),.UNSPECIFIED.)
GEOMETRIC_REPRESENTATION_ITEM()
RATIONAL_B_SPLINE_SURFACE(((1.,1.,1.),(1.,1.00267605951745,1.),(1.,0.941599607549811,
1.),(1.,0.828238301901754,1.),(1.,0.787677905717219,1.),(1.,0.726552333979987,
1.),(1.,0.706675310150434,1.),(1.,0.707106781186548,1.)))
REPRESENTATION_ITEM('')
SURFACE()
) ;
#420 = (
BOUNDED_SURFACE()
B_SPLINE_SURFACE(3,2,((#108089,#108090,#108091),(#108092,#108093,#108094),
(#108095,#108096,#108097),(#108098,#108099,#108100),(#108101,#108102,#108103),
(#108104,#108105,#108106),(#108107,#108108,#108109),(#108110,#108111,#108112)),
 .UNSPECIFIED.,.F.,.F.,.F.)
B_SPLINE_SURFACE_WITH_KNOTS((4,2,2,4),(3,3),(6.28318530717959,6.67588438887831,
7.06858347057703,7.85398163397448),(0.,1.),.UNSPECIFIED.)
GEOMETRIC_REPRESENTATION_ITEM()
RATIONAL_B_SPLINE_SURFACE(((1.,0.707106781186548,1.),(1.,0.70667531015044,
1.),(1.,0.726552333979978,1.),(1.,0.787677905717226,1.),(1.,0.828238301901736,
1.),(1.,0.941599607549842,1.),(1.,1.00267605951742,1.),(1.,1.,1.)))
REPRESENTATION_ITEM('')
SURFACE()
) ;
#421 = (
BOUNDED_SURFACE()
B_SPLINE_SURFACE(3,2,((#108113,#108114,#108115),(#108116,#108117,#108118),
(#108119,#108120,#108121),(#108122,#108123,#108124),(#108125,#108126,#108127),
(#108128,#108129,#108130)),.UNSPECIFIED.,.F.,.F.,.F.)
B_SPLINE_SURFACE_WITH_KNOTS((4,2,4),(3,3),(2.06095632820092,2.9281173096476,
3.79527829109429),(0.,1.),.UNSPECIFIED.)
GEOMETRIC_REPRESENTATION_ITEM()
RATIONAL_B_SPLINE_SURFACE(((1.,0.763019982472728,1.),(1.,0.792403856906196,
1.),(1.,0.812400188579439,1.),(1.,0.825457041220947,1.),(1.,0.818529518851322,
1.),(1.,0.799131938862213,1.)))
REPRESENTATION_ITEM('')
SURFACE()
) ;
#422 = (
BOUNDED_SURFACE()
B_SPLINE_SURFACE(3,2,((#108153,#108154,#108155),(#108156,#108157,#108158),
(#108159,#108160,#108161),(#108162,#108163,#108164),(#108165,#108166,#108167),
(#108168,#108169,#108170)),.UNSPECIFIED.,.F.,.F.,.F.)
B_SPLINE_SURFACE_WITH_KNOTS((4,2,4),(3,3),(2.13522523980986,3.02435044878098,
3.91347565775211),(0.,1.),.UNSPECIFIED.)
GEOMETRIC_REPRESENTATION_ITEM()
RATIONAL_B_SPLINE_SURFACE(((1.,0.749240327740271,1.),(1.,0.768579562596362,
1.),(1.,0.780993049743008,1.),(1.,0.78606840104594,1.),(1.,0.778729916329028,
1.),(1.,0.763019982472728,1.)))
REPRESENTATION_ITEM('')
SURFACE()
) ;
#423 = (
BOUNDED_SURFACE()
B_SPLINE_SURFACE(3,2,((#108327,#108328,#108329),(#108330,#108331,#108332),
(#108333,#108334,#108335),(#108336,#108337,#108338),(#108339,#108340,#108341),
(#108342,#108343,#108344),(#108345,#108346,#108347),(#108348,#108349,#108350),
(#108351,#108352,#108353),(#108354,#108355,#108356),(#108357,#108358,#108359),
(#108360,#108361,#108362),(#108363,#108364,#108365),(#108366,#108367,#108368),
(#108369,#108370,#108371),(#108372,#108373,#108374),(#108375,#108376,#108377),
(#108378,#108379,#108380)),.UNSPECIFIED.,.F.,.F.,.F.)
B_SPLINE_SURFACE_WITH_KNOTS((4,2,2,2,2,2,2,2,4),(3,3),(-2.88136898044851E-5,
0.000144068449022425,0.000180085561278031,0.000216102673533637,0.00023411122966144,
0.000243115507725342,0.000252119785789243,0.000270128341917046,0.000315232069288961),
(-0.00230043332275091,1.00649231299441),.UNSPECIFIED.)
GEOMETRIC_REPRESENTATION_ITEM()
RATIONAL_B_SPLINE_SURFACE(((1.00137797387076,0.698547958833899,1.00390520040649),
(1.00130996746083,0.713425360736938,1.00371246913244),(1.00133921304011,
0.70702746034338,1.00379535158075),(1.00112343332499,0.754232445101169,
1.00318382835154),(1.00107694244868,0.764403007733155,1.00305207245044),
(1.00092854904603,0.796866246024235,1.00263152312896),(1.0008372304274,
0.816843536281796,1.00237272467553),(1.00052495197507,0.885159038383831,
1.00148772245247),(1.00036238583105,0.920722772197686,1.00102700735096),
(1.00013066612426,0.97141486445809,1.0003703099256),(1.00008161134635,0.982146318257279,
1.00023128788556),(1.00010185218181,0.977718337948419,1.00028865074314),
(1.00015066464689,0.967039893644228,1.00042698606465),(1.00027150756254,
0.940603729390326,1.00076945685699),(1.00035349548852,0.922667665318131,
1.00100181197535),(1.00060974665109,0.866608956479371,1.00172803194619),
(1.00075148156336,0.835602360842761,1.00212971099741),(1.00085165739527,
0.813687424975854,1.00241361093759)))
REPRESENTATION_ITEM('')
SURFACE()
) ;
#424 = (
BOUNDED_SURFACE()
B_SPLINE_SURFACE(3,2,((#108382,#108383,#108384),(#108385,#108386,#108387),
(#108388,#108389,#108390),(#108391,#108392,#108393)),.UNSPECIFIED.,.F.,
 .F.,.F.)
B_SPLINE_SURFACE_WITH_KNOTS((4,4),(3,3),(5.63598348762741,6.28318530717959),
(0.792338840560947,1.),.UNSPECIFIED.)
GEOMETRIC_REPRESENTATION_ITEM()
RATIONAL_B_SPLINE_SURFACE(((0.934040253948337,0.958376553896458,1.),(0.938725627259263,
0.961333226642432,1.),(0.941220250254377,0.96290744140221,1.),(0.941208919370362,
0.962900291125438,1.)))
REPRESENTATION_ITEM('')
SURFACE()
) ;
#425 = (
BOUNDED_SURFACE()
B_SPLINE_SURFACE(3,2,((#108434,#108435,#108436),(#108437,#108438,#108439),
(#108440,#108441,#108442),(#108443,#108444,#108445),(#108446,#108447,#108448),
(#108449,#108450,#108451),(#108452,#108453,#108454),(#108455,#108456,#108457),
(#108458,#108459,#108460),(#108461,#108462,#108463),(#108464,#108465,#108466),
(#108467,#108468,#108469),(#108470,#108471,#108472),(#108473,#108474,#108475),
(#108476,#108477,#108478),(#108479,#108480,#108481),(#108482,#108483,#108484),
(#108485,#108486,#108487)),.UNSPECIFIED.,.F.,.F.,.F.)
B_SPLINE_SURFACE_WITH_KNOTS((4,2,2,2,2,2,2,2,4),(3,3),(-3.19743590576725E-5,
0.000144068449022543,0.000180085561278178,0.000216102673533814,0.000234111229661632,
0.000243115507725541,0.00025211978578945,0.000270128341917267,0.000288136898045085),
(-0.0066834189729316,1.00019683226125),.UNSPECIFIED.)
GEOMETRIC_REPRESENTATION_ITEM()
RATIONAL_B_SPLINE_SURFACE(((1.00403209003416,0.69829147589393,1.00011798325537),
(1.00381915098331,0.714225030505279,1.0001117524316),(1.00391733895256,
0.706877935813777,1.00011462551633),(1.00327816898475,0.754704999695305,
1.00009592272127),(1.00314250899907,0.764856006670041,1.00009195316538),
(1.00270949829937,0.797256825605557,1.00007928281042),(1.00244303133896,
0.817195704119684,1.00007148570292),(1.00153180544397,0.885379851193009,
1.00004482226124),(1.00105743880425,0.920875204110236,1.00003094178737),
(1.00038128265055,0.971469827114243,1.00001115673706),(1.00023814122159,
0.982180646789321,1.00000696826617),(1.0002972038091,0.977761180469343,
1.00000869650048),(1.00043963817126,0.967103268362385,1.00001286428185),
(1.00079225678184,0.940717934784041,1.00002318227853),(1.00103149685962,
0.922816357645972,1.0000301826984),(1.00145821870311,0.890886113898623,
1.00004266903471),(1.0016523226799,0.876361928211943,1.00004834872412),
(1.00182713963616,0.863280929173184,1.00005346405474)))
REPRESENTATION_ITEM('')
SURFACE()
) ;
#426 = (
BOUNDED_SURFACE()
B_SPLINE_SURFACE(3,2,((#108526,#108527,#108528),(#108529,#108530,#108531),
(#108532,#108533,#108534),(#108535,#108536,#108537)),.UNSPECIFIED.,.F.,
 .F.,.F.)
B_SPLINE_SURFACE_WITH_KNOTS((4,4),(3,3),(5.51130230301727,6.28318530717958),
(0.,1.),.UNSPECIFIED.)
GEOMETRIC_REPRESENTATION_ITEM()
RATIONAL_B_SPLINE_SURFACE(((1.,0.763019982472728,1.),(1.,0.776565014072567,
1.),(1.,0.78408875836913,1.),(1.,0.784033077704815,1.)))
REPRESENTATION_ITEM('')
SURFACE()
) ;
#427 = (
BOUNDED_SURFACE()
B_SPLINE_SURFACE(3,2,((#108542,#108543,#108544),(#108545,#108546,#108547),
(#108548,#108549,#108550),(#108551,#108552,#108553)),.UNSPECIFIED.,.F.,
 .F.,.F.)
B_SPLINE_SURFACE_WITH_KNOTS((4,4),(3,3),(0.0051446850272488,0.00657473287039649),
(0.,1.),.UNSPECIFIED.)
GEOMETRIC_REPRESENTATION_ITEM()
RATIONAL_B_SPLINE_SURFACE(((1.,0.943476662524758,1.),(1.,0.94494570202475,
1.),(1.,0.946300916277098,1.),(1.,0.947565352018496,1.)))
REPRESENTATION_ITEM('')
SURFACE()
) ;
#428 = (
BOUNDED_SURFACE()
B_SPLINE_SURFACE(3,2,((#108592,#108593,#108594),(#108595,#108596,#108597),
(#108598,#108599,#108600),(#108601,#108602,#108603)),.UNSPECIFIED.,.F.,
 .F.,.F.)
B_SPLINE_SURFACE_WITH_KNOTS((4,4),(3,3),(0.0051446850272488,0.00657473287039648),
(0.,1.),.UNSPECIFIED.)
GEOMETRIC_REPRESENTATION_ITEM()
RATIONAL_B_SPLINE_SURFACE(((1.,0.943476662524758,1.),(1.,0.944945702024751,
1.),(1.,0.946300916277097,1.),(1.,0.947565352018496,1.)))
REPRESENTATION_ITEM('')
SURFACE()
) ;
#429 = (
BOUNDED_SURFACE()
B_SPLINE_SURFACE(3,2,((#108608,#108609,#108610),(#108611,#108612,#108613),
(#108614,#108615,#108616),(#108617,#108618,#108619),(#108620,#108621,#108622),
(#108623,#108624,#108625),(#108626,#108627,#108628),(#108629,#108630,#108631),
(#108632,#108633,#108634),(#108635,#108636,#108637),(#108638,#108639,#108640),
(#108641,#108642,#108643),(#108644,#108645,#108646),(#108647,#108648,#108649),
(#108650,#108651,#108652),(#108653,#108654,#108655),(#108656,#108657,#108658),
(#108659,#108660,#108661)),.UNSPECIFIED.,.F.,.F.,.F.)
B_SPLINE_SURFACE_WITH_KNOTS((4,2,2,2,2,2,2,2,4),(3,3),(-2.77591379149846E-5,
0.00012525316796938,0.000156566459961724,0.000187879751954069,0.000203536397950241,
0.000211364720948327,0.000219193043946413,0.000234849689942586,0.000250506335938758),
(0.,1.00287807885244),.UNSPECIFIED.)
GEOMETRIC_REPRESENTATION_ITEM()
RATIONAL_B_SPLINE_SURFACE(((1.,0.6985872651442,1.00173497923609),(1.,0.713937574732387,
1.00164662043327),(1.,0.719549163949333,1.00161431924077),(1.,0.771808112008987,
1.00131350849425),(1.,0.78248224372348,1.00125206650874),(1.,0.810804881628055,
1.00108903693834),(1.,0.82782480896445,1.00099106755247),(1.,0.868687526094294,
1.00075585530842),(1.,0.885097717150226,1.00066139566073),(1.,0.918597380148776,
1.00046856631745),(1.,0.931968622959474,1.00039159933513),(1.,0.955741994674726,
1.00025475605836),(1.,0.963776461019231,1.000208508403),(1.,0.965421728909319,
1.00019903798156),(1.,0.949947468785985,1.0002881102632),(1.,0.92747461920283,
1.00041746752947),(1.,0.916335140210132,1.00048158812731),(1.,0.906010523700246,
1.00054101824818)))
REPRESENTATION_ITEM('')
SURFACE()
) ;
#430 = (
BOUNDED_SURFACE()
B_SPLINE_SURFACE(3,2,((#108665,#108666,#108667),(#108668,#108669,#108670),
(#108671,#108672,#108673),(#108674,#108675,#108676),(#108677,#108678,#108679),
(#108680,#108681,#108682),(#108683,#108684,#108685),(#108686,#108687,#108688),
(#108689,#108690,#108691),(#108692,#108693,#108694),(#108695,#108696,#108697),
(#108698,#108699,#108700),(#108701,#108702,#108703),(#108704,#108705,#108706),
(#108707,#108708,#108709),(#108710,#108711,#108712),(#108713,#108714,#108715),
(#108716,#108717,#108718)),.UNSPECIFIED.,.F.,.F.,.F.)
B_SPLINE_SURFACE_WITH_KNOTS((4,2,2,2,2,2,2,2,4),(3,3),(-2.79610875103729E-5,
0.000125253167969372,0.000156566459961715,0.000187879751954059,0.00020353639795023,
0.000211364720948316,0.000219193043946402,0.000234849689942574,0.000253195388096673),
(-0.00314610977265889,1.),.UNSPECIFIED.)
GEOMETRIC_REPRESENTATION_ITEM()
RATIONAL_B_SPLINE_SURFACE(((1.00189744483737,0.698445862592838,0.999999999999999),
(1.00180054146109,0.713846370406803,1.),(1.0017654902188,0.719416939270416,
1.),(1.00143621720102,0.771747125052534,1.),(1.00136903527045,0.782424109553835,
1.),(1.00119077538534,0.810754317015274,1.),(1.00108365364401,0.827778793126865,
1.),(1.00082646773903,0.868652431296584,1.),(1.0007231836176,0.885067008168485,
1.),(1.00051234004796,0.91857562434451,1.),(1.0004281827666,0.931950440776612,
1.),(1.00027855551348,0.955730166203988,1.),(1.00022798737599,0.963766779853886,
1.),(1.00021763222242,0.965412487461145,1.),(1.00031502568701,0.949934091660368,
1.),(1.00046861400989,0.925524847549974,1.),(1.00055064362451,0.912488173602136,
1.),(1.00062456604611,0.900739946914172,1.)))
REPRESENTATION_ITEM('')
SURFACE()
) ;
#431 = (
BOUNDED_SURFACE()
B_SPLINE_SURFACE(3,2,((#108721,#108722,#108723),(#108724,#108725,#108726),
(#108727,#108728,#108729),(#108730,#108731,#108732)),.UNSPECIFIED.,.F.,
 .F.,.F.)
B_SPLINE_SURFACE_WITH_KNOTS((4,4),(3,3),(-1.77635683940025E-15,1.00173611575494),
(0.800638603120396,1.),.UNSPECIFIED.)
GEOMETRIC_REPRESENTATION_ITEM()
RATIONAL_B_SPLINE_SURFACE(((0.931056261594762,0.956944532691443,1.),(0.931106613485818,
0.956975977522394,1.),(0.926966069646247,0.954390201728275,1.),(0.920044734228403,
0.950067817452231,1.)))
REPRESENTATION_ITEM('')
SURFACE()
) ;
#432 = (
BOUNDED_SURFACE()
B_SPLINE_SURFACE(3,2,((#108758,#108759,#108760),(#108761,#108762,#108763),
(#108764,#108765,#108766),(#108767,#108768,#108769)),.UNSPECIFIED.,.F.,
 .F.,.F.)
B_SPLINE_SURFACE_WITH_KNOTS((4,4),(3,3),(-8.88178419700125E-16,1.08063632538888),
(0.,1.),.UNSPECIFIED.)
GEOMETRIC_REPRESENTATION_ITEM()
RATIONAL_B_SPLINE_SURFACE(((1.,0.8213449786432,1.),(1.,0.821618737292288,
1.),(1.,0.799663084581846,1.),(1.,0.763019982472728,1.)))
REPRESENTATION_ITEM('')
SURFACE()
) ;
#433 = (
BOUNDED_SURFACE()
B_SPLINE_SURFACE(3,2,((#110236,#110237,#110238),(#110239,#110240,#110241),
(#110242,#110243,#110244),(#110245,#110246,#110247),(#110248,#110249,#110250),
(#110251,#110252,#110253)),.UNSPECIFIED.,.F.,.F.,.F.)
B_SPLINE_SURFACE_WITH_KNOTS((4,2,4),(3,3),(9.07204043127176E-5,0.000289236237441533,
0.000487752070570311),(-0.000844756555347329,1.00064307855269),
 .UNSPECIFIED.)
GEOMETRIC_REPRESENTATION_ITEM()
RATIONAL_B_SPLINE_SURFACE(((1.00067853369516,0.598126578821866,1.0005164358132),
(1.00070177595141,0.584360946986094,1.0005341256252),(1.00066498743035,
0.606149590529527,1.00050612567485),(1.00056632625569,0.66458339283634,
1.00043103409967),(1.00050548323096,0.700618735924348,1.00038472613123),
(1.00047271456509,0.720026550084158,1.00035978571527)))
REPRESENTATION_ITEM('')
SURFACE()
) ;
#434 = (
BOUNDED_SURFACE()
B_SPLINE_SURFACE(3,2,((#110268,#110269,#110270),(#110271,#110272,#110273),
(#110274,#110275,#110276),(#110277,#110278,#110279),(#110280,#110281,#110282),
(#110283,#110284,#110285)),.UNSPECIFIED.,.F.,.F.,.F.)
B_SPLINE_SURFACE_WITH_KNOTS((4,2,4),(3,3),(0.000107162911540598,0.000298022515767418,
0.000488882119994237),(-0.00075993985566105,1.00062534339582),
 .UNSPECIFIED.)
GEOMETRIC_REPRESENTATION_ITEM()
RATIONAL_B_SPLINE_SURFACE(((1.00042862573101,0.717810580914573,1.00035266240948),
(1.00045905072598,0.697780025035115,1.00037769532575),(1.0005111494633,
0.663480375353433,1.00042056084899),(1.0005966522522,0.607188882365342,
1.00049091038092),(1.00062840114514,0.586286726926399,1.00051703256695),
(1.00061268510756,0.596633514797443,1.00050410180877)))
REPRESENTATION_ITEM('')
SURFACE()
) ;
#435 = (
BOUNDED_SURFACE()
B_SPLINE_SURFACE(3,2,((#110515,#110516,#110517),(#110518,#110519,#110520),
(#110521,#110522,#110523),(#110524,#110525,#110526),(#110527,#110528,#110529),
(#110530,#110531,#110532),(#110533,#110534,#110535),(#110536,#110537,#110538)),
 .UNSPECIFIED.,.F.,.F.,.F.)
B_SPLINE_SURFACE_WITH_KNOTS((4,2,2,4),(3,3),(6.28318530717959,6.67588438887831,
7.06858347057703,7.85398163397448),(0.,1.),.UNSPECIFIED.)
GEOMETRIC_REPRESENTATION_ITEM()
RATIONAL_B_SPLINE_SURFACE(((1.,0.707106781186548,1.),(1.,0.706675310150436,
1.),(1.,0.726552333979984,1.),(1.,0.787677905717219,1.),(1.,0.828238301901734,
1.),(1.,0.94159960754984,1.),(1.,1.00267605951742,1.),(1.,1.,1.)))
REPRESENTATION_ITEM('')
SURFACE()
) ;
#436 = (
BOUNDED_SURFACE()
B_SPLINE_SURFACE(3,2,((#110546,#110547,#110548),(#110549,#110550,#110551),
(#110552,#110553,#110554),(#110555,#110556,#110557),(#110558,#110559,#110560),
(#110561,#110562,#110563),(#110564,#110565,#110566),(#110567,#110568,#110569)),
 .UNSPECIFIED.,.F.,.F.,.F.)
B_SPLINE_SURFACE_WITH_KNOTS((4,2,2,4),(3,3),(4.71238898038469,5.49778714378214,
5.89048622548086,6.28318530717959),(0.,1.),.UNSPECIFIED.)
GEOMETRIC_REPRESENTATION_ITEM()
RATIONAL_B_SPLINE_SURFACE(((1.,1.,1.),(1.,1.0026760595174,1.),(1.,0.94159960754987,
1.),(1.,0.828238301901727,1.),(1.,0.787677905717213,1.),(1.,0.726552333979991,
1.),(1.,0.706675310150431,1.),(1.,0.707106781186548,1.)))
REPRESENTATION_ITEM('')
SURFACE()
) ;
#437 = (
BOUNDED_SURFACE()
B_SPLINE_SURFACE(3,2,((#110570,#110571,#110572),(#110573,#110574,#110575),
(#110576,#110577,#110578),(#110579,#110580,#110581),(#110582,#110583,#110584),
(#110585,#110586,#110587),(#110588,#110589,#110590),(#110591,#110592,#110593)),
 .UNSPECIFIED.,.F.,.F.,.F.)
B_SPLINE_SURFACE_WITH_KNOTS((4,2,2,4),(3,3),(4.71238898038469,5.49778714378214,
5.89048622548086,6.28318530717959),(0.,1.),.UNSPECIFIED.)
GEOMETRIC_REPRESENTATION_ITEM()
RATIONAL_B_SPLINE_SURFACE(((1.,1.,1.),(1.,1.00267605951744,1.),(1.,0.941599607549825,
1.),(1.,0.828238301901746,1.),(1.,0.787677905717283,1.),(1.,0.726552333979923,
1.),(1.,0.706675310150477,1.),(1.,0.707106781186554,1.)))
REPRESENTATION_ITEM('')
SURFACE()
) ;
#438 = (
BOUNDED_SURFACE()
B_SPLINE_SURFACE(3,2,((#110601,#110602,#110603),(#110604,#110605,#110606),
(#110607,#110608,#110609),(#110610,#110611,#110612),(#110613,#110614,#110615),
(#110616,#110617,#110618),(#110619,#110620,#110621),(#110622,#110623,#110624)),
 .UNSPECIFIED.,.F.,.F.,.F.)
B_SPLINE_SURFACE_WITH_KNOTS((4,2,2,4),(3,3),(6.28318530717959,6.67588438887831,
7.06858347057703,7.85398163397448),(0.,1.),.UNSPECIFIED.)
GEOMETRIC_REPRESENTATION_ITEM()
RATIONAL_B_SPLINE_SURFACE(((1.,0.707106781186548,1.),(1.,0.706675310150428,
1.),(1.,0.726552333979983,1.),(1.,0.78767790571723,1.),(1.,0.828238301901763,
1.),(1.,0.941599607549783,1.),(1.,1.00267605951747,1.),(1.,1.,1.)))
REPRESENTATION_ITEM('')
SURFACE()
) ;
#439 = (
BOUNDED_SURFACE()
B_SPLINE_SURFACE(3,2,((#110625,#110626,#110627),(#110628,#110629,#110630),
(#110631,#110632,#110633),(#110634,#110635,#110636),(#110637,#110638,#110639),
(#110640,#110641,#110642)),.UNSPECIFIED.,.F.,.F.,.F.)
B_SPLINE_SURFACE_WITH_KNOTS((4,2,4),(3,3),(2.06095632820092,2.92811730964759,
3.79527829109427),(0.,1.),.UNSPECIFIED.)
GEOMETRIC_REPRESENTATION_ITEM()
RATIONAL_B_SPLINE_SURFACE(((1.,0.763019982472728,1.),(1.,0.792403856906218,
1.),(1.,0.812400188579406,1.),(1.,0.825457041220978,1.),(1.,0.818529518851298,
1.),(1.,0.799131938862213,1.)))
REPRESENTATION_ITEM('')
SURFACE()
) ;
#440 = (
BOUNDED_SURFACE()
B_SPLINE_SURFACE(3,2,((#110665,#110666,#110667),(#110668,#110669,#110670),
(#110671,#110672,#110673),(#110674,#110675,#110676),(#110677,#110678,#110679),
(#110680,#110681,#110682)),.UNSPECIFIED.,.F.,.F.,.F.)
B_SPLINE_SURFACE_WITH_KNOTS((4,2,4),(3,3),(2.13522523980989,3.02435044878099,
3.9134756577521),(0.,1.),.UNSPECIFIED.)
GEOMETRIC_REPRESENTATION_ITEM()
RATIONAL_B_SPLINE_SURFACE(((1.,0.749240327740279,1.),(1.,0.768579562596332,
1.),(1.,0.780993049743038,1.),(1.,0.78606840104591,1.),(1.,0.778729916329054,
1.),(1.,0.763019982472728,1.)))
REPRESENTATION_ITEM('')
SURFACE()
) ;
#441 = (
BOUNDED_SURFACE()
B_SPLINE_SURFACE(3,2,((#110839,#110840,#110841),(#110842,#110843,#110844),
(#110845,#110846,#110847),(#110848,#110849,#110850),(#110851,#110852,#110853),
(#110854,#110855,#110856),(#110857,#110858,#110859),(#110860,#110861,#110862),
(#110863,#110864,#110865),(#110866,#110867,#110868),(#110869,#110870,#110871),
(#110872,#110873,#110874),(#110875,#110876,#110877),(#110878,#110879,#110880),
(#110881,#110882,#110883),(#110884,#110885,#110886),(#110887,#110888,#110889),
(#110890,#110891,#110892)),.UNSPECIFIED.,.F.,.F.,.F.)
B_SPLINE_SURFACE_WITH_KNOTS((4,2,2,2,2,2,2,2,4),(3,3),(-2.88136898044833E-5,
0.000144068449022426,0.000180085561278032,0.000216102673533639,0.000234111229661442,
0.000243115507725343,0.000252119785789245,0.000270128341917048,0.000315232069288965),
(-0.00230043332394133,1.00649231299454),.UNSPECIFIED.)
GEOMETRIC_REPRESENTATION_ITEM()
RATIONAL_B_SPLINE_SURFACE(((1.00137797387148,0.69854795883355,1.00390520040657),
(1.00130996746151,0.71342536073646,1.00371246913252),(1.00133921304081,
0.707027460343067,1.00379535158082),(1.00112343332557,0.754232445100828,
1.0031838283516),(1.00107694244924,0.764403007732966,1.0030520724505),(1.00092854904651,
0.796866246023831,1.00263152312901),(1.00083723042783,0.816843536281475,
1.00237272467558),(1.00052495197535,0.885159038383718,1.0014877224525),
(1.00036238583123,0.920722772198033,1.00102700735098),(1.00013066612433,
0.971414864457831,1.00037030992562),(1.00008161134639,0.982146318257256,
1.00023128788557),(1.00010185218186,0.977718337948391,1.00028865074313),
(1.00015066464697,0.96703989364419,1.00042698606466),(1.00027150756269,
0.940603729390218,1.00076945685701),(1.0003534954887,0.922667665318,1.00100181197537),
(1.00060974665141,0.866608956479275,1.00172803194623),(1.00075148156375,
0.835602360842203,1.00212971099746),(1.00085165739571,0.813687424976644,
1.00241361093764)))
REPRESENTATION_ITEM('')
SURFACE()
) ;
#442 = (
BOUNDED_SURFACE()
B_SPLINE_SURFACE(3,2,((#110894,#110895,#110896),(#110897,#110898,#110899),
(#110900,#110901,#110902),(#110903,#110904,#110905)),.UNSPECIFIED.,.F.,
 .F.,.F.)
B_SPLINE_SURFACE_WITH_KNOTS((4,4),(3,3),(5.63598348762741,6.28318530717959),
(0.792338840560962,1.),.UNSPECIFIED.)
GEOMETRIC_REPRESENTATION_ITEM()
RATIONAL_B_SPLINE_SURFACE(((0.934040253948341,0.958376553896461,1.),(0.938725627259267,
0.961333226642435,1.),(0.941220250254379,0.962907441402212,1.),(0.941208919370365,
0.962900291125441,1.)))
REPRESENTATION_ITEM('')
SURFACE()
) ;
#443 = (
BOUNDED_SURFACE()
B_SPLINE_SURFACE(3,2,((#110946,#110947,#110948),(#110949,#110950,#110951),
(#110952,#110953,#110954),(#110955,#110956,#110957),(#110958,#110959,#110960),
(#110961,#110962,#110963),(#110964,#110965,#110966),(#110967,#110968,#110969),
(#110970,#110971,#110972),(#110973,#110974,#110975),(#110976,#110977,#110978),
(#110979,#110980,#110981),(#110982,#110983,#110984),(#110985,#110986,#110987),
(#110988,#110989,#110990),(#110991,#110992,#110993),(#110994,#110995,#110996),
(#110997,#110998,#110999)),.UNSPECIFIED.,.F.,.F.,.F.)
B_SPLINE_SURFACE_WITH_KNOTS((4,2,2,2,2,2,2,2,4),(3,3),(-3.1974359057668E-5,
0.000144068449022543,0.000180085561278178,0.000216102673533814,0.000234111229661632,
0.000243115507725541,0.00025211978578945,0.000270128341917267,0.000288136898045085),
(-0.00668341897303802,1.00019683226125),.UNSPECIFIED.)
GEOMETRIC_REPRESENTATION_ITEM()
RATIONAL_B_SPLINE_SURFACE(((1.00403209003423,0.698291475893822,1.00011798325538),
(1.00381915098337,0.714225030505383,1.00011175243161),(1.00391733895262,
0.706877935813645,1.00011462551632),(1.0032781689848,0.754704999695298,
1.00009592272127),(1.00314250899912,0.764856006669979,1.00009195316538),
(1.00270949829941,0.79725682560557,1.00007928281042),(1.00244303133899,
0.817195704119653,1.00007148570293),(1.001531805444,0.885379851193002,1.00004482226125),
(1.00105743880427,0.920875204110228,1.00003094178737),(1.00038128265056,
0.971469827114239,1.00001115673706),(1.0002381412216,0.982180646789319,
1.00000696826617),(1.0002972038091,0.97776118046934,1.00000869650048),(1.00043963817127,
0.967103268362382,1.00001286428185),(1.00079225678185,0.940717934784034,
1.00002318227853),(1.00103149685964,0.922816357645954,1.0000301826984),
(1.00145821870313,0.890886113898608,1.00004266903471),(1.00165232267993,
0.876361928211933,1.00004834872412),(1.00182713963619,0.863280929173169,
1.00005346405474)))
REPRESENTATION_ITEM('')
SURFACE()
) ;
#444 = (
BOUNDED_SURFACE()
B_SPLINE_SURFACE(3,2,((#111038,#111039,#111040),(#111041,#111042,#111043),
(#111044,#111045,#111046),(#111047,#111048,#111049)),.UNSPECIFIED.,.F.,
 .F.,.F.)
B_SPLINE_SURFACE_WITH_KNOTS((4,4),(3,3),(5.51130230301728,6.28318530717958),
(0.,1.),.UNSPECIFIED.)
GEOMETRIC_REPRESENTATION_ITEM()
RATIONAL_B_SPLINE_SURFACE(((1.,0.763019982472728,1.),(1.,0.776565014072563,
1.),(1.,0.78408875836913,1.),(1.,0.784033077704815,1.)))
REPRESENTATION_ITEM('')
SURFACE()
) ;
#445 = (
BOUNDED_SURFACE()
B_SPLINE_SURFACE(3,2,((#111054,#111055,#111056),(#111057,#111058,#111059),
(#111060,#111061,#111062),(#111063,#111064,#111065)),.UNSPECIFIED.,.F.,
 .F.,.F.)
B_SPLINE_SURFACE_WITH_KNOTS((4,4),(3,3),(0.0051446850272488,0.00657473287039649),
(0.,1.),.UNSPECIFIED.)
GEOMETRIC_REPRESENTATION_ITEM()
RATIONAL_B_SPLINE_SURFACE(((1.,0.943476662524758,1.),(1.,0.944945702024748,
1.),(1.,0.946300916277099,1.),(1.,0.947565352018495,1.)))
REPRESENTATION_ITEM('')
SURFACE()
) ;
#446 = (
BOUNDED_SURFACE()
B_SPLINE_SURFACE(3,2,((#111104,#111105,#111106),(#111107,#111108,#111109),
(#111110,#111111,#111112),(#111113,#111114,#111115)),.UNSPECIFIED.,.F.,
 .F.,.F.)
B_SPLINE_SURFACE_WITH_KNOTS((4,4),(3,3),(0.0051446850272488,0.00657473287039648),
(0.,1.),.UNSPECIFIED.)
GEOMETRIC_REPRESENTATION_ITEM()
RATIONAL_B_SPLINE_SURFACE(((1.,0.943476662524758,1.),(1.,0.944945702024752,
1.),(1.,0.946300916277091,1.),(1.,0.947565352018496,1.)))
REPRESENTATION_ITEM('')
SURFACE()
) ;
#447 = (
BOUNDED_SURFACE()
B_SPLINE_SURFACE(3,2,((#111120,#111121,#111122),(#111123,#111124,#111125),
(#111126,#111127,#111128),(#111129,#111130,#111131),(#111132,#111133,#111134),
(#111135,#111136,#111137),(#111138,#111139,#111140),(#111141,#111142,#111143),
(#111144,#111145,#111146),(#111147,#111148,#111149),(#111150,#111151,#111152),
(#111153,#111154,#111155),(#111156,#111157,#111158),(#111159,#111160,#111161),
(#111162,#111163,#111164),(#111165,#111166,#111167),(#111168,#111169,#111170),
(#111171,#111172,#111173)),.UNSPECIFIED.,.F.,.F.,.F.)
B_SPLINE_SURFACE_WITH_KNOTS((4,2,2,2,2,2,2,2,4),(3,3),(-2.77591379148802E-5,
0.000125253167969374,0.000156566459961717,0.000187879751954061,0.000203536397950232,
0.000211364720948318,0.000219193043946404,0.000234849689942576,0.000250506335938747),
(0.,1.00287807885236),.UNSPECIFIED.)
GEOMETRIC_REPRESENTATION_ITEM()
RATIONAL_B_SPLINE_SURFACE(((1.,0.698587265144137,1.00173497923604),(1.,
0.713937574732619,1.00164662043323),(1.,0.719549163949235,1.00161431924073),
(1.,0.771808112009033,1.00131350849422),(1.,0.782482243723513,1.00125206650871),
(1.,0.810804881628019,1.00108903693831),(1.,0.827824808964515,1.00099106755244),
(1.,0.868687526094263,1.0007558553084),(1.,0.885097717150305,1.00066139566072),
(1.,0.918597380148718,1.00046856631744),(1.,0.931968622959399,1.00039159933512),
(1.,0.955741994674697,1.00025475605835),(1.,0.963776461019228,1.000208508403),
(1.,0.965421728909335,1.00019903798155),(1.,0.949947468785963,1.00028811026319),
(1.,0.927474619202861,1.00041746752946),(1.,0.916335140210129,1.00048158812729),
(1.,0.906010523700251,1.00054101824817)))
REPRESENTATION_ITEM('')
SURFACE()
) ;
#448 = (
BOUNDED_SURFACE()
B_SPLINE_SURFACE(3,2,((#111177,#111178,#111179),(#111180,#111181,#111182),
(#111183,#111184,#111185),(#111186,#111187,#111188),(#111189,#111190,#111191),
(#111192,#111193,#111194),(#111195,#111196,#111197),(#111198,#111199,#111200),
(#111201,#111202,#111203),(#111204,#111205,#111206),(#111207,#111208,#111209),
(#111210,#111211,#111212),(#111213,#111214,#111215),(#111216,#111217,#111218),
(#111219,#111220,#111221),(#111222,#111223,#111224),(#111225,#111226,#111227),
(#111228,#111229,#111230)),.UNSPECIFIED.,.F.,.F.,.F.)
B_SPLINE_SURFACE_WITH_KNOTS((4,2,2,2,2,2,2,2,4),(3,3),(-2.7961087510372E-5,
0.000125253167969371,0.000156566459961714,0.000187879751954057,0.000203536397950228,
0.000211364720948314,0.000219193043946399,0.000234849689942571,0.000253195388096718),
(-0.00314610977256982,1.),.UNSPECIFIED.)
GEOMETRIC_REPRESENTATION_ITEM()
RATIONAL_B_SPLINE_SURFACE(((1.00189744483732,0.698445862592752,0.999999999999999),
(1.00180054146104,0.713846370407033,1.),(1.00176549021876,0.71941693927029,
1.),(1.00143621720098,0.771747125052584,1.),(1.00136903527042,0.78242410955385,
1.),(1.00119077538531,0.810754317015277,1.),(1.00108365364397,0.827778793126865,
1.),(1.000826467739,0.868652431296581,1.),(1.00072318361758,0.885067008168526,
1.),(1.00051234004795,0.9185756243445,1.),(1.00042818276658,0.931950440776531,
1.),(1.00027855551347,0.95573016620407,1.),(1.00022798737599,0.963766779853886,
1.),(1.00021763222241,0.965412487461147,1.),(1.000315025687,0.949934091660343,
1.),(1.00046861400987,0.925524847549985,1.),(1.0005506436245,0.912488173602062,
1.),(1.00062456604607,0.900739946914099,1.)))
REPRESENTATION_ITEM('')
SURFACE()
) ;
#449 = (
BOUNDED_SURFACE()
B_SPLINE_SURFACE(3,2,((#111233,#111234,#111235),(#111236,#111237,#111238),
(#111239,#111240,#111241),(#111242,#111243,#111244)),.UNSPECIFIED.,.F.,
 .F.,.F.)
B_SPLINE_SURFACE_WITH_KNOTS((4,4),(3,3),(-1.77635683940025E-15,1.00173611575493),
(0.800638603120408,1.),.UNSPECIFIED.)
GEOMETRIC_REPRESENTATION_ITEM()
RATIONAL_B_SPLINE_SURFACE(((0.931056261594765,0.956944532691446,1.),(0.931106613485821,
0.956975977522397,1.),(0.92696606964625,0.954390201728278,1.),(0.920044734228406,
0.950067817452234,1.)))
REPRESENTATION_ITEM('')
SURFACE()
) ;
#450 = (
BOUNDED_SURFACE()
B_SPLINE_SURFACE(3,2,((#111270,#111271,#111272),(#111273,#111274,#111275),
(#111276,#111277,#111278),(#111279,#111280,#111281)),.UNSPECIFIED.,.F.,
 .F.,.F.)
B_SPLINE_SURFACE_WITH_KNOTS((4,4),(3,3),(7.18283939271647E-15,1.08063632538888),
(0.,1.),.UNSPECIFIED.)
GEOMETRIC_REPRESENTATION_ITEM()
RATIONAL_B_SPLINE_SURFACE(((1.,0.821344978643199,1.),(1.,0.821618737292293,
1.),(1.,0.799663084581839,1.),(1.,0.763019982472728,1.)))
REPRESENTATION_ITEM('')
SURFACE()
) ;
#451 = (
BOUNDED_SURFACE()
B_SPLINE_SURFACE(3,2,((#112748,#112749,#112750),(#112751,#112752,#112753),
(#112754,#112755,#112756),(#112757,#112758,#112759),(#112760,#112761,#112762),
(#112763,#112764,#112765)),.UNSPECIFIED.,.F.,.F.,.F.)
B_SPLINE_SURFACE_WITH_KNOTS((4,2,4),(3,3),(9.07204043127144E-5,0.000289236237441533,
0.000487752070570316),(-0.000844756555295823,1.00064307855252),
 .UNSPECIFIED.)
GEOMETRIC_REPRESENTATION_ITEM()
RATIONAL_B_SPLINE_SURFACE(((1.00067853369511,0.598126578822019,1.00051643581306),
(1.00070177595137,0.58436094698614,1.00053412562506),(1.0006649874303,0.606149590529623,
1.00050612567471),(1.00056632625566,0.664583392836423,1.00043103409956),
(1.00050548323092,0.700618735924398,1.00038472613112),(1.00047271456507,
0.720026550084235,1.00035978571517)))
REPRESENTATION_ITEM('')
SURFACE()
) ;
#452 = (
BOUNDED_SURFACE()
B_SPLINE_SURFACE(3,2,((#112780,#112781,#112782),(#112783,#112784,#112785),
(#112786,#112787,#112788),(#112789,#112790,#112791),(#112792,#112793,#112794),
(#112795,#112796,#112797)),.UNSPECIFIED.,.F.,.F.,.F.)
B_SPLINE_SURFACE_WITH_KNOTS((4,2,4),(3,3),(0.000107162911540599,0.000298022515767417,
0.000488882119994238),(-0.000759939855676642,1.00062534339577),
 .UNSPECIFIED.)
GEOMETRIC_REPRESENTATION_ITEM()
RATIONAL_B_SPLINE_SURFACE(((1.00042862573102,0.717810580914605,1.00035266240945),
(1.00045905072599,0.697780025035077,1.00037769532572),(1.00051114946331,
0.663480375353483,1.00042056084895),(1.00059665225221,0.607188882365318,
1.00049091038088),(1.00062840114515,0.586286726926443,1.00051703256691),
(1.00061268510757,0.596633514797456,1.00050410180872)))
REPRESENTATION_ITEM('')
SURFACE()
) ;
#453 = (
BOUNDED_SURFACE()
B_SPLINE_SURFACE(3,2,((#113027,#113028,#113029),(#113030,#113031,#113032),
(#113033,#113034,#113035),(#113036,#113037,#113038),(#113039,#113040,#113041),
(#113042,#113043,#113044),(#113045,#113046,#113047),(#113048,#113049,#113050)),
 .UNSPECIFIED.,.F.,.F.,.F.)
B_SPLINE_SURFACE_WITH_KNOTS((4,2,2,4),(3,3),(6.28318530717959,6.67588438887831,
7.06858347057703,7.85398163397448),(0.,1.),.UNSPECIFIED.)
GEOMETRIC_REPRESENTATION_ITEM()
RATIONAL_B_SPLINE_SURFACE(((1.,0.707106781186548,1.),(1.,0.706675310150436,
1.),(1.,0.726552333979984,1.),(1.,0.787677905717219,1.),(1.,0.828238301901734,
1.),(1.,0.94159960754984,1.),(1.,1.00267605951742,1.),(1.,1.,1.)))
REPRESENTATION_ITEM('')
SURFACE()
) ;
#454 = (
BOUNDED_SURFACE()
B_SPLINE_SURFACE(3,2,((#113058,#113059,#113060),(#113061,#113062,#113063),
(#113064,#113065,#113066),(#113067,#113068,#113069),(#113070,#113071,#113072),
(#113073,#113074,#113075),(#113076,#113077,#113078),(#113079,#113080,#113081)),
 .UNSPECIFIED.,.F.,.F.,.F.)
B_SPLINE_SURFACE_WITH_KNOTS((4,2,2,4),(3,3),(4.71238898038469,5.49778714378214,
5.89048622548086,6.28318530717959),(0.,1.),.UNSPECIFIED.)
GEOMETRIC_REPRESENTATION_ITEM()
RATIONAL_B_SPLINE_SURFACE(((1.,1.,1.),(1.,1.0026760595174,1.),(1.,0.94159960754987,
1.),(1.,0.828238301901727,1.),(1.,0.787677905717213,1.),(1.,0.726552333979991,
1.),(1.,0.706675310150431,1.),(1.,0.707106781186548,1.)))
REPRESENTATION_ITEM('')
SURFACE()
) ;
#455 = (
BOUNDED_SURFACE()
B_SPLINE_SURFACE(3,2,((#113082,#113083,#113084),(#113085,#113086,#113087),
(#113088,#113089,#113090),(#113091,#113092,#113093),(#113094,#113095,#113096),
(#113097,#113098,#113099),(#113100,#113101,#113102),(#113103,#113104,#113105)),
 .UNSPECIFIED.,.F.,.F.,.F.)
B_SPLINE_SURFACE_WITH_KNOTS((4,2,2,4),(3,3),(4.71238898038469,5.49778714378214,
5.89048622548086,6.28318530717959),(0.,1.),.UNSPECIFIED.)
GEOMETRIC_REPRESENTATION_ITEM()
RATIONAL_B_SPLINE_SURFACE(((1.,1.,1.),(1.,1.0026760595174,1.),(1.,0.94159960754987,
1.),(1.,0.828238301901727,1.),(1.,0.787677905717213,1.),(1.,0.726552333979991,
1.),(1.,0.706675310150431,1.),(1.,0.707106781186548,1.)))
REPRESENTATION_ITEM('')
SURFACE()
) ;
#456 = (
BOUNDED_SURFACE()
B_SPLINE_SURFACE(3,2,((#113113,#113114,#113115),(#113116,#113117,#113118),
(#113119,#113120,#113121),(#113122,#113123,#113124),(#113125,#113126,#113127),
(#113128,#113129,#113130),(#113131,#113132,#113133),(#113134,#113135,#113136)),
 .UNSPECIFIED.,.F.,.F.,.F.)
B_SPLINE_SURFACE_WITH_KNOTS((4,2,2,4),(3,3),(6.28318530717959,6.67588438887831,
7.06858347057703,7.85398163397448),(0.,1.),.UNSPECIFIED.)
GEOMETRIC_REPRESENTATION_ITEM()
RATIONAL_B_SPLINE_SURFACE(((1.,0.707106781186548,1.),(1.,0.706675310150436,
1.),(1.,0.726552333979984,1.),(1.,0.787677905717219,1.),(1.,0.828238301901734,
1.),(1.,0.94159960754984,1.),(1.,1.00267605951742,1.),(1.,1.,1.)))
REPRESENTATION_ITEM('')
SURFACE()
) ;
#457 = (
BOUNDED_SURFACE()
B_SPLINE_SURFACE(3,2,((#113137,#113138,#113139),(#113140,#113141,#113142),
(#113143,#113144,#113145),(#113146,#113147,#113148),(#113149,#113150,#113151),
(#113152,#113153,#113154)),.UNSPECIFIED.,.F.,.F.,.F.)
B_SPLINE_SURFACE_WITH_KNOTS((4,2,4),(3,3),(2.06095632820092,2.92811730964759,
3.79527829109427),(0.,1.),.UNSPECIFIED.)
GEOMETRIC_REPRESENTATION_ITEM()
RATIONAL_B_SPLINE_SURFACE(((1.,0.763019982472728,1.),(1.,0.792403856906318,
1.),(1.,0.812400188579283,1.),(1.,0.825457041221101,1.),(1.,0.818529518851208,
1.),(1.,0.799131938862211,1.)))
REPRESENTATION_ITEM('')
SURFACE()
) ;
#458 = (
BOUNDED_SURFACE()
B_SPLINE_SURFACE(3,2,((#113177,#113178,#113179),(#113180,#113181,#113182),
(#113183,#113184,#113185),(#113186,#113187,#113188),(#113189,#113190,#113191),
(#113192,#113193,#113194)),.UNSPECIFIED.,.F.,.F.,.F.)
B_SPLINE_SURFACE_WITH_KNOTS((4,2,4),(3,3),(2.13522523980989,3.02435044878099,
3.9134756577521),(0.,1.),.UNSPECIFIED.)
GEOMETRIC_REPRESENTATION_ITEM()
RATIONAL_B_SPLINE_SURFACE(((1.,0.749240327740277,1.),(1.,0.768579562596332,
1.),(1.,0.780993049743038,1.),(1.,0.78606840104591,1.),(1.,0.778729916329044,
1.),(1.,0.763019982472728,1.)))
REPRESENTATION_ITEM('')
SURFACE()
) ;
#459 = (
BOUNDED_SURFACE()
B_SPLINE_SURFACE(3,2,((#113351,#113352,#113353),(#113354,#113355,#113356),
(#113357,#113358,#113359),(#113360,#113361,#113362),(#113363,#113364,#113365),
(#113366,#113367,#113368),(#113369,#113370,#113371),(#113372,#113373,#113374),
(#113375,#113376,#113377),(#113378,#113379,#113380),(#113381,#113382,#113383),
(#113384,#113385,#113386),(#113387,#113388,#113389),(#113390,#113391,#113392),
(#113393,#113394,#113395),(#113396,#113397,#113398),(#113399,#113400,#113401),
(#113402,#113403,#113404)),.UNSPECIFIED.,.F.,.F.,.F.)
B_SPLINE_SURFACE_WITH_KNOTS((4,2,2,2,2,2,2,2,4),(3,3),(-2.88136898044833E-5,
0.000144068449022426,0.000180085561278032,0.000216102673533639,0.000234111229661442,
0.000243115507725343,0.000252119785789245,0.000270128341917048,0.000315232069288961),
(-0.00230043332395591,1.00649231299463),.UNSPECIFIED.)
GEOMETRIC_REPRESENTATION_ITEM()
RATIONAL_B_SPLINE_SURFACE(((1.00137797387149,0.698547958833521,1.00390520040663),
(1.00130996746152,0.713425360736431,1.00371246913257),(1.00133921304082,
0.707027460343038,1.00379535158087),(1.00112343332558,0.754232445100804,
1.00318382835165),(1.00107694244925,0.764403007732903,1.00305207245053),
(1.00092854904652,0.79686624602385,1.00263152312904),(1.00083723042784,
0.816843536281434,1.00237272467562),(1.00052495197535,0.885159038383718,
1.00148772245252),(1.00036238583123,0.920722772198024,1.00102700735099),
(1.00013066612433,0.971414864457828,1.00037030992562),(1.00008161134639,
0.982146318257254,1.00023128788557),(1.00010185218186,0.977718337948389,
1.00028865074314),(1.00015066464697,0.967039893644187,1.00042698606467),
(1.00027150756269,0.940603729390212,1.00076945685701),(1.0003534954887,
0.922667665317993,1.00100181197539),(1.00060974665141,0.866608956479265,
1.00172803194625),(1.00075148156376,0.835602360842176,1.00212971099749),
(1.00085165739571,0.813687424976746,1.00241361093766)))
REPRESENTATION_ITEM('')
SURFACE()
) ;
#460 = (
BOUNDED_SURFACE()
B_SPLINE_SURFACE(3,2,((#113406,#113407,#113408),(#113409,#113410,#113411),
(#113412,#113413,#113414),(#113415,#113416,#113417)),.UNSPECIFIED.,.F.,
 .F.,.F.)
B_SPLINE_SURFACE_WITH_KNOTS((4,4),(3,3),(5.63598348762743,6.28318530717959),
(0.792338840560947,1.),.UNSPECIFIED.)
GEOMETRIC_REPRESENTATION_ITEM()
RATIONAL_B_SPLINE_SURFACE(((0.934040253948338,0.958376553896459,1.),(0.938725627259262,
0.961333226642431,1.),(0.941220250254377,0.962907441402211,1.),(0.941208919370362,
0.962900291125438,1.)))
REPRESENTATION_ITEM('')
SURFACE()
) ;
#461 = (
BOUNDED_SURFACE()
B_SPLINE_SURFACE(3,2,((#113458,#113459,#113460),(#113461,#113462,#113463),
(#113464,#113465,#113466),(#113467,#113468,#113469),(#113470,#113471,#113472),
(#113473,#113474,#113475),(#113476,#113477,#113478),(#113479,#113480,#113481),
(#113482,#113483,#113484),(#113485,#113486,#113487),(#113488,#113489,#113490),
(#113491,#113492,#113493),(#113494,#113495,#113496),(#113497,#113498,#113499),
(#113500,#113501,#113502),(#113503,#113504,#113505),(#113506,#113507,#113508),
(#113509,#113510,#113511)),.UNSPECIFIED.,.F.,.F.,.F.)
B_SPLINE_SURFACE_WITH_KNOTS((4,2,2,2,2,2,2,2,4),(3,3),(-3.19743590575723E-5,
0.000144068449022591,0.000180085561278238,0.000216102673533885,0.000234111229661708,
0.00024311550772562,0.000252119785789532,0.000270128341917355,0.000288136898045179),
(-0.0066834189728382,1.00019683226058),.UNSPECIFIED.)
GEOMETRIC_REPRESENTATION_ITEM()
RATIONAL_B_SPLINE_SURFACE(((1.00403209003411,0.69829147589406,1.00011798325497),
(1.00381915098325,0.714225030505723,1.00011175243122),(1.0039173389525,
0.706877935813847,1.00011462551593),(1.0032781689847,0.754704999695571,
1.00009592272094),(1.00314250899902,0.764856006670268,1.00009195316507),
(1.00270949829933,0.797256825605796,1.00007928281015),(1.00244303133891,
0.817195704120733,1.00007148570268),(1.00153180544395,0.885379851192955,
1.00004482226109),(1.00105743880421,0.920875204111829,1.00003094178726),
(1.00038128265055,0.971469827113733,1.00001115673703),(1.00023814122159,
0.982180646789395,1.00000696826614),(1.00029720380909,0.977761180469183,
1.00000869650045),(1.00043963817126,0.967103268362262,1.0000128642818),
(1.00079225678183,0.940717934783944,1.00002318227845),(1.00103149685961,
0.922816357645932,1.00003018269829),(1.00145821870309,0.890886113898687,
1.00004266903457),(1.00165232267988,0.876361928212012,1.00004834872396),
(1.00182713963613,0.863280929173305,1.00005346405456)))
REPRESENTATION_ITEM('')
SURFACE()
) ;
#462 = (
BOUNDED_SURFACE()
B_SPLINE_SURFACE(3,2,((#113550,#113551,#113552),(#113553,#113554,#113555),
(#113556,#113557,#113558),(#113559,#113560,#113561)),.UNSPECIFIED.,.F.,
 .F.,.F.)
B_SPLINE_SURFACE_WITH_KNOTS((4,4),(3,3),(5.51130230301728,6.28318530717958),
(0.,1.),.UNSPECIFIED.)
GEOMETRIC_REPRESENTATION_ITEM()
RATIONAL_B_SPLINE_SURFACE(((1.,0.763019982472728,1.),(1.,0.776565014072567,
1.),(1.,0.784088758369131,1.),(1.,0.784033077704815,1.)))
REPRESENTATION_ITEM('')
SURFACE()
) ;
#463 = (
BOUNDED_SURFACE()
B_SPLINE_SURFACE(3,2,((#113566,#113567,#113568),(#113569,#113570,#113571),
(#113572,#113573,#113574),(#113575,#113576,#113577)),.UNSPECIFIED.,.F.,
 .F.,.F.)
B_SPLINE_SURFACE_WITH_KNOTS((4,4),(3,3),(0.0051446850272488,0.00657473287039649),
(0.,1.),.UNSPECIFIED.)
GEOMETRIC_REPRESENTATION_ITEM()
RATIONAL_B_SPLINE_SURFACE(((1.,0.943476662524759,1.),(1.,0.944945702024751,
1.),(1.,0.946300916277093,1.),(1.,0.947565352018496,1.)))
REPRESENTATION_ITEM('')
SURFACE()
) ;
#464 = (
BOUNDED_SURFACE()
B_SPLINE_SURFACE(3,2,((#113616,#113617,#113618),(#113619,#113620,#113621),
(#113622,#113623,#113624),(#113625,#113626,#113627)),.UNSPECIFIED.,.F.,
 .F.,.F.)
B_SPLINE_SURFACE_WITH_KNOTS((4,4),(3,3),(0.0051446850272488,0.00657473287039648),
(0.,1.),.UNSPECIFIED.)
GEOMETRIC_REPRESENTATION_ITEM()
RATIONAL_B_SPLINE_SURFACE(((1.,0.94347666252476,1.),(1.,0.94494570202475,
1.),(1.,0.946300916277093,1.),(1.,0.947565352018496,1.)))
REPRESENTATION_ITEM('')
SURFACE()
) ;
#465 = (
BOUNDED_SURFACE()
B_SPLINE_SURFACE(3,2,((#113632,#113633,#113634),(#113635,#113636,#113637),
(#113638,#113639,#113640),(#113641,#113642,#113643),(#113644,#113645,#113646),
(#113647,#113648,#113649),(#113650,#113651,#113652),(#113653,#113654,#113655),
(#113656,#113657,#113658),(#113659,#113660,#113661),(#113662,#113663,#113664),
(#113665,#113666,#113667),(#113668,#113669,#113670),(#113671,#113672,#113673),
(#113674,#113675,#113676),(#113677,#113678,#113679),(#113680,#113681,#113682),
(#113683,#113684,#113685)),.UNSPECIFIED.,.F.,.F.,.F.)
B_SPLINE_SURFACE_WITH_KNOTS((4,2,2,2,2,2,2,2,4),(3,3),(-2.77591379149701E-5,
0.000125253167969375,0.000156566459961718,0.000187879751954062,0.000203536397950234,
0.00021136472094832,0.000219193043946406,0.000234849689942578,0.00025050633593875),
(0.,1.00287807885242),.UNSPECIFIED.)
GEOMETRIC_REPRESENTATION_ITEM()
RATIONAL_B_SPLINE_SURFACE(((1.,0.698587265143979,1.00173497923608),(1.,
0.713937574732811,1.00164662043326),(1.,0.719549163949031,1.00161431924076),
(1.,0.771808112009055,1.00131350849424),(1.,0.782482243723506,1.00125206650873),
(1.,0.810804881628005,1.00108903693833),(1.,0.827824808964385,1.00099106755246),
(1.,0.868687526094324,1.00075585530841),(1.,0.885097717150309,1.00066139566073),
(1.,0.91859738014868,1.00046856631745),(1.,0.931968622959436,1.00039159933512),
(1.,0.955741994674629,1.00025475605835),(1.,0.963776461019212,1.000208508403),
(1.,0.965421728909353,1.00019903798156),(1.,0.949947468785925,1.00028811026319),
(1.,0.927474619202907,1.00041746752947),(1.,0.916335140210081,1.0004815881273),
(1.,0.906010523700247,1.00054101824818)))
REPRESENTATION_ITEM('')
SURFACE()
) ;
#466 = (
BOUNDED_SURFACE()
B_SPLINE_SURFACE(3,2,((#113689,#113690,#113691),(#113692,#113693,#113694),
(#113695,#113696,#113697),(#113698,#113699,#113700),(#113701,#113702,#113703),
(#113704,#113705,#113706),(#113707,#113708,#113709),(#113710,#113711,#113712),
(#113713,#113714,#113715),(#113716,#113717,#113718),(#113719,#113720,#113721),
(#113722,#113723,#113724),(#113725,#113726,#113727),(#113728,#113729,#113730),
(#113731,#113732,#113733),(#113734,#113735,#113736),(#113737,#113738,#113739),
(#113740,#113741,#113742)),.UNSPECIFIED.,.F.,.F.,.F.)
B_SPLINE_SURFACE_WITH_KNOTS((4,2,2,2,2,2,2,2,4),(3,3),(-2.79610875104704E-5,
0.000125253167969371,0.000156566459961714,0.000187879751954057,0.000203536397950228,
0.000211364720948314,0.000219193043946399,0.000234849689942571,0.000253195388096719),
(-0.00314610977255892,1.),.UNSPECIFIED.)
GEOMETRIC_REPRESENTATION_ITEM()
RATIONAL_B_SPLINE_SURFACE(((1.00189744483731,0.698445862592619,1.),(1.00180054146103,
0.713846370407217,1.),(1.00176549021876,0.719416939270132,1.),(1.00143621720097,
0.771747125052614,1.),(1.00136903527041,0.782424109553879,1.),(1.00119077538531,
0.810754317015252,1.),(1.00108365364397,0.827778793126867,1.),(1.000826467739,
0.868652431296582,1.),(1.00072318361758,0.885067008168527,1.),(1.00051234004795,
0.918575624344501,1.),(1.00042818276658,0.931950440776532,1.),(1.00027855551347,
0.955730166204071,1.),(1.00022798737599,0.963766779853886,1.),(1.00021763222241,
0.965412487461148,1.),(1.000315025687,0.949934091660343,1.),(1.00046861400987,
0.925524847549986,1.),(1.0005506436245,0.912488173602064,1.),(1.00062456604607,
0.900739946914099,1.)))
REPRESENTATION_ITEM('')
SURFACE()
) ;
#467 = (
BOUNDED_SURFACE()
B_SPLINE_SURFACE(1,2,((#125809,#125810,#125811,#125812,#125813,#125814,
#125815,#125816,#125817,#125818,#125819,#125820,#125821,#125822,#125823,
#125824,#125825,#125826,#125827,#125828,#125829,#125830,#125831,#125832,
#125833,#125834,#125835,#125836,#125837,#125838,#125839,#125840,#125841,
#125842,#125843,#125844,#125845,#125846,#125847,#125848,#125849,#125850,
#125851,#125852,#125853,#125854,#125855,#125856,#125857,#125858,#125859,
#125860,#125861,#125862,#125863,#125864,#125865,#125866,#125867,#125868,
#125869,#125870,#125871,#125872,#125873,#125874,#125875,#125876,#125877,
#125878,#125879,#125880,#125881,#125882,#125883,#125884,#125885,#125886,
#125887,#125888,#125889,#125890,#125891,#125892,#125893,#125894,#125895,
#125896,#125897,#125898,#125899,#125900,#125901,#125902,#125903,#125904,
#125905,#125906,#125907,#125908,#125909,#125910,#125911,#125912,#125913,
#125914,#125915,#125916,#125917,#125918,#125919,#125920,#125921,#125922,
#125923,#125924,#125925,#125926,#125927,#125928,#125929,#125930,#125931,
#125932,#125933,#125934,#125935,#125936,#125937,#125938,#125939,#125940,
#125941,#125942,#125943),(#125944,#125945,#125946,#125947,#125948,#125949,
#125950,#125951,#125952,#125953,#125954,#125955,#125956,#125957,#125958,
#125959,#125960,#125961,#125962,#125963,#125964,#125965,#125966,#125967,
#125968,#125969,#125970,#125971,#125972,#125973,#125974,#125975,#125976,
#125977,#125978,#125979,#125980,#125981,#125982,#125983,#125984,#125985,
#125986,#125987,#125988,#125989,#125990,#125991,#125992,#125993,#125994,
#125995,#125996,#125997,#125998,#125999,#126000,#126001,#126002,#126003,
#126004,#126005,#126006,#126007,#126008,#126009,#126010,#126011,#126012,
#126013,#126014,#126015,#126016,#126017,#126018,#126019,#126020,#126021,
#126022,#126023,#126024,#126025,#126026,#126027,#126028,#126029,#126030,
#126031,#126032,#126033,#126034,#126035,#126036,#126037,#126038,#126039,
#126040,#126041,#126042,#126043,#126044,#126045,#126046,#126047,#126048,
#126049,#126050,#126051,#126052,#126053,#126054,#126055,#126056,#126057,
#126058,#126059,#126060,#126061,#126062,#126063,#126064,#126065,#126066,
#126067,#126068,#126069,#126070,#126071,#126072,#126073,#126074,#126075,
#126076,#126077,#126078)),.UNSPECIFIED.,.F.,.F.,.F.)
B_SPLINE_SURFACE_WITH_KNOTS((2,2),(3,2,2,2,2,2,2,2,2,2,2,2,2,2,2,2,2,2,
2,2,2,2,2,2,2,2,2,2,2,2,2,2,2,2,2,2,2,2,2,2,2,2,2,2,2,2,2,2,2,2,2,2,2,2,
2,2,2,2,2,2,2,2,2,2,2,2,2,3),(0.,1.00006111776867),(0.,0.0138888888888889,
0.0277777777777778,0.0416666666666667,0.0555555555555556,0.0694444444444444,
0.0833333333333333,0.0972222222222222,0.111111111111111,0.125,0.138888888888889,
0.152777777777778,0.166666666666667,0.180555555555556,0.194444444444444,
0.208333333333333,0.222222222222222,0.236111111111111,0.25,0.263888888888889,
0.277777777777778,0.291666666666667,0.305555555555556,0.319444444444444,
0.333333333333333,0.347222222222222,0.361111111111111,0.375,0.388888888888889,
0.402777777777778,0.416666666666667,0.430555555555556,0.444444444444444,
0.458333333333333,0.472222222222222,0.486111111111111,0.5,0.513888888888889,
0.527777777777778,0.541666666666667,0.555555555555556,0.569444444444444,
0.583333333333333,0.597222222222222,0.611111111111111,0.625,0.638888888888889,
0.652777777777778,0.666666666666667,0.680555555555556,0.694444444444444,
0.708333333333333,0.722222222222222,0.736111111111111,0.75,0.763888888888889,
0.777777777777778,0.791666666666667,0.805555555555556,0.819444444444444,
0.833333333333333,0.847222222222222,0.861111111111111,0.875,0.888888888888889,
0.902777777777778,0.916666666666667,0.920887586444199),.UNSPECIFIED.)
GEOMETRIC_REPRESENTATION_ITEM()
RATIONAL_B_SPLINE_SURFACE(((1.,0.866025403784439,1.,0.866025403784439,1.,
0.866025403784439,1.,0.866025403784439,1.,0.866025403784439,1.,0.866025403784439,
1.,0.866025403784439,1.,0.866025403784439,1.,0.866025403784439,1.,0.866025403784439,
1.,0.866025403784439,1.,0.866025403784439,1.,0.866025403784439,1.,0.866025403784439,
1.,0.866025403784439,1.,0.866025403784439,1.,0.866025403784439,1.,0.866025403784439,
1.,0.866025403784439,1.,0.866025403784439,1.,0.866025403784439,1.,0.866025403784439,
1.,0.866025403784439,1.,0.866025403784439,1.,0.866025403784439,1.,0.866025403784439,
1.,0.866025403784439,1.,0.866025403784439,1.,0.866025403784439,1.,0.866025403784439,
1.,0.866025403784439,1.,0.866025403784439,1.,0.866025403784439,1.,0.866025403784439,
1.,0.866025403784439,1.,0.866025403784439,1.,0.866025403784439,1.,0.866025403784439,
1.,0.866025403784439,1.,0.866025403784439,1.,0.866025403784439,1.,0.866025403784439,
1.,0.866025403784439,1.,0.866025403784439,1.,0.866025403784439,1.,0.866025403784439,
1.,0.866025403784439,1.,0.866025403784439,1.,0.866025403784439,1.,0.866025403784439,
1.,0.866025403784439,1.,0.866025403784439,1.,0.866025403784439,1.,0.866025403784439,
1.,0.866025403784439,1.,0.866025403784439,1.,0.866025403784439,1.,0.866025403784439,
1.,0.866025403784439,1.,0.866025403784439,1.,0.866025403784439,1.,0.866025403784439,
1.,0.866025403784439,1.,0.866025403784439,1.,0.866025403784439,1.,0.866025403784439,
1.,0.959284286354576,0.943316090290602),(1.,0.866025403784439,1.,0.866025403784439,
1.,0.866025403784439,1.,0.866025403784439,1.,0.866025403784439,1.,0.866025403784439,
1.,0.866025403784439,1.,0.866025403784439,1.,0.866025403784439,1.,0.866025403784439,
1.,0.866025403784439,1.,0.866025403784439,1.,0.866025403784439,1.,0.866025403784439,
1.,0.866025403784439,1.,0.866025403784439,1.,0.866025403784439,1.,0.866025403784439,
1.,0.866025403784439,1.,0.866025403784439,1.,0.866025403784439,1.,0.866025403784439,
1.,0.866025403784439,1.,0.866025403784439,1.,0.866025403784439,1.,0.866025403784439,
1.,0.866025403784439,1.,0.866025403784439,1.,0.866025403784439,1.,0.866025403784439,
1.,0.866025403784439,1.,0.866025403784439,1.,0.866025403784439,1.,0.866025403784439,
1.,0.866025403784439,1.,0.866025403784439,1.,0.866025403784439,1.,0.866025403784439,
1.,0.866025403784439,1.,0.866025403784439,1.,0.866025403784439,1.,0.866025403784439,
1.,0.866025403784439,1.,0.866025403784439,1.,0.866025403784439,1.,0.866025403784439,
1.,0.866025403784439,1.,0.866025403784439,1.,0.866025403784439,1.,0.866025403784439,
1.,0.866025403784439,1.,0.866025403784439,1.,0.866025403784439,1.,0.866025403784439,
1.,0.866025403784439,1.,0.866025403784439,1.,0.866025403784439,1.,0.866025403784439,
1.,0.866025403784439,1.,0.866025403784439,1.,0.866025403784439,1.,0.866025403784439,
1.,0.866025403784439,1.,0.866025403784439,1.,0.866025403784439,1.,0.866025403784439,
1.,0.959284286354576,0.943316090290602)))
REPRESENTATION_ITEM('')
SURFACE()
) ;
#468 = (
BOUNDED_SURFACE()
B_SPLINE_SURFACE(1,2,((#126080,#126081,#126082,#126083,#126084,#126085,
#126086,#126087,#126088,#126089,#126090,#126091,#126092,#126093,#126094,
#126095,#126096,#126097,#126098,#126099,#126100,#126101,#126102,#126103,
#126104,#126105,#126106,#126107,#126108,#126109,#126110,#126111,#126112,
#126113,#126114,#126115,#126116,#126117,#126118,#126119,#126120,#126121,
#126122,#126123,#126124,#126125,#126126,#126127,#126128,#126129,#126130,
#126131,#126132,#126133,#126134,#126135,#126136,#126137,#126138,#126139,
#126140,#126141,#126142,#126143,#126144,#126145,#126146,#126147,#126148,
#126149,#126150,#126151,#126152,#126153,#126154,#126155,#126156,#126157,
#126158,#126159,#126160,#126161,#126162,#126163,#126164,#126165,#126166,
#126167,#126168,#126169,#126170,#126171,#126172,#126173,#126174,#126175,
#126176,#126177,#126178,#126179,#126180,#126181,#126182,#126183,#126184,
#126185,#126186,#126187,#126188,#126189,#126190,#126191,#126192,#126193,
#126194,#126195,#126196,#126197,#126198,#126199,#126200,#126201,#126202,
#126203,#126204,#126205,#126206,#126207,#126208,#126209,#126210,#126211,
#126212,#126213,#126214),(#126215,#126216,#126217,#126218,#126219,#126220,
#126221,#126222,#126223,#126224,#126225,#126226,#126227,#126228,#126229,
#126230,#126231,#126232,#126233,#126234,#126235,#126236,#126237,#126238,
#126239,#126240,#126241,#126242,#126243,#126244,#126245,#126246,#126247,
#126248,#126249,#126250,#126251,#126252,#126253,#126254,#126255,#126256,
#126257,#126258,#126259,#126260,#126261,#126262,#126263,#126264,#126265,
#126266,#126267,#126268,#126269,#126270,#126271,#126272,#126273,#126274,
#126275,#126276,#126277,#126278,#126279,#126280,#126281,#126282,#126283,
#126284,#126285,#126286,#126287,#126288,#126289,#126290,#126291,#126292,
#126293,#126294,#126295,#126296,#126297,#126298,#126299,#126300,#126301,
#126302,#126303,#126304,#126305,#126306,#126307,#126308,#126309,#126310,
#126311,#126312,#126313,#126314,#126315,#126316,#126317,#126318,#126319,
#126320,#126321,#126322,#126323,#126324,#126325,#126326,#126327,#126328,
#126329,#126330,#126331,#126332,#126333,#126334,#126335,#126336,#126337,
#126338,#126339,#126340,#126341,#126342,#126343,#126344,#126345,#126346,
#126347,#126348,#126349)),.UNSPECIFIED.,.F.,.F.,.F.)
B_SPLINE_SURFACE_WITH_KNOTS((2,2),(3,2,2,2,2,2,2,2,2,2,2,2,2,2,2,2,2,2,
2,2,2,2,2,2,2,2,2,2,2,2,2,2,2,2,2,2,2,2,2,2,2,2,2,2,2,2,2,2,2,2,2,2,2,2,
2,2,2,2,2,2,2,2,2,2,2,2,2,3),(0.,1.),(0.,0.0138888888888889,0.0277777777777778,
0.0416666666666667,0.0555555555555556,0.0694444444444444,0.0833333333333333,
0.0972222222222222,0.111111111111111,0.125,0.138888888888889,0.152777777777778,
0.166666666666667,0.180555555555556,0.194444444444444,0.208333333333333,
0.222222222222222,0.236111111111111,0.25,0.263888888888889,0.277777777777778,
0.291666666666667,0.305555555555556,0.319444444444444,0.333333333333333,
0.347222222222222,0.361111111111111,0.375,0.388888888888889,0.402777777777778,
0.416666666666667,0.430555555555556,0.444444444444444,0.458333333333333,
0.472222222222222,0.486111111111111,0.5,0.513888888888889,0.527777777777778,
0.541666666666667,0.555555555555556,0.569444444444444,0.583333333333333,
0.597222222222222,0.611111111111111,0.625,0.638888888888889,0.652777777777778,
0.666666666666667,0.680555555555556,0.694444444444444,0.708333333333333,
0.722222222222222,0.736111111111111,0.75,0.763888888888889,0.777777777777778,
0.791666666666667,0.805555555555556,0.819444444444444,0.833333333333333,
0.847222222222222,0.861111111111111,0.875,0.888888888888889,0.902777777777778,
0.916666666666667,0.920887434615967),.UNSPECIFIED.)
GEOMETRIC_REPRESENTATION_ITEM()
RATIONAL_B_SPLINE_SURFACE(((1.,0.866025403784439,1.,0.866025403784439,1.,
0.866025403784439,1.,0.866025403784439,1.,0.866025403784439,1.,0.866025403784439,
1.,0.866025403784439,1.,0.866025403784439,1.,0.866025403784439,1.,0.866025403784439,
1.,0.866025403784439,1.,0.866025403784439,1.,0.866025403784439,1.,0.866025403784439,
1.,0.866025403784439,1.,0.866025403784439,1.,0.866025403784439,1.,0.866025403784439,
1.,0.866025403784439,1.,0.866025403784439,1.,0.866025403784439,1.,0.866025403784439,
1.,0.866025403784439,1.,0.866025403784439,1.,0.866025403784439,1.,0.866025403784439,
1.,0.866025403784439,1.,0.866025403784439,1.,0.866025403784439,1.,0.866025403784439,
1.,0.866025403784439,1.,0.866025403784439,1.,0.866025403784439,1.,0.866025403784439,
1.,0.866025403784439,1.,0.866025403784439,1.,0.866025403784439,1.,0.866025403784439,
1.,0.866025403784439,1.,0.866025403784439,1.,0.866025403784439,1.,0.866025403784439,
1.,0.866025403784439,1.,0.866025403784439,1.,0.866025403784439,1.,0.866025403784439,
1.,0.866025403784439,1.,0.866025403784439,1.,0.866025403784439,1.,0.866025403784439,
1.,0.866025403784439,1.,0.866025403784439,1.,0.866025403784439,1.,0.866025403784439,
1.,0.866025403784439,1.,0.866025403784439,1.,0.866025403784439,1.,0.866025403784439,
1.,0.866025403784439,1.,0.866025403784439,1.,0.866025403784439,1.,0.866025403784439,
1.,0.866025403784439,1.,0.866025403784439,1.,0.866025403784439,1.,0.866025403784439,
1.,0.959285750915652,0.943317239087869),(1.,0.866025403784439,1.,0.866025403784439,
1.,0.866025403784439,1.,0.866025403784439,1.,0.866025403784439,1.,0.866025403784439,
1.,0.866025403784439,1.,0.866025403784439,1.,0.866025403784439,1.,0.866025403784439,
1.,0.866025403784439,1.,0.866025403784439,1.,0.866025403784439,1.,0.866025403784439,
1.,0.866025403784439,1.,0.866025403784439,1.,0.866025403784439,1.,0.866025403784439,
1.,0.866025403784439,1.,0.866025403784439,1.,0.866025403784439,1.,0.866025403784439,
1.,0.866025403784439,1.,0.866025403784439,1.,0.866025403784439,1.,0.866025403784439,
1.,0.866025403784439,1.,0.866025403784439,1.,0.866025403784439,1.,0.866025403784439,
1.,0.866025403784439,1.,0.866025403784439,1.,0.866025403784439,1.,0.866025403784439,
1.,0.866025403784439,1.,0.866025403784439,1.,0.866025403784439,1.,0.866025403784439,
1.,0.866025403784439,1.,0.866025403784439,1.,0.866025403784439,1.,0.866025403784439,
1.,0.866025403784439,1.,0.866025403784439,1.,0.866025403784439,1.,0.866025403784439,
1.,0.866025403784439,1.,0.866025403784439,1.,0.866025403784439,1.,0.866025403784439,
1.,0.866025403784439,1.,0.866025403784439,1.,0.866025403784439,1.,0.866025403784439,
1.,0.866025403784439,1.,0.866025403784439,1.,0.866025403784439,1.,0.866025403784439,
1.,0.866025403784439,1.,0.866025403784439,1.,0.866025403784439,1.,0.866025403784439,
1.,0.866025403784439,1.,0.866025403784439,1.,0.866025403784439,1.,0.866025403784439,
1.,0.959285750915652,0.943317239087869)))
REPRESENTATION_ITEM('')
SURFACE()
) ;
#469 = SHAPE_REPRESENTATION_RELATIONSHIP('SRR','None',#126599,#475) ;
#470 = SHAPE_REPRESENTATION_RELATIONSHIP('SRR','None',#126600,#476) ;
#471 = SHAPE_REPRESENTATION_RELATIONSHIP('SRR','None',#126601,#477) ;
#472 = SHAPE_REPRESENTATION_RELATIONSHIP('SRR','None',#126602,#478) ;
#473 = SHAPE_REPRESENTATION_RELATIONSHIP('SRR','None',#126603,#479) ;
#474 = SHAPE_REPRESENTATION_RELATIONSHIP('SRR','None',#126604,#480) ;
#475 = ADVANCED_BREP_SHAPE_REPRESENTATION('',(#4172),#126565) ;
#476 = ADVANCED_BREP_SHAPE_REPRESENTATION('',(#4173,#4174,#4175,#4176,#4177),
#126566) ;
#477 = ADVANCED_BREP_SHAPE_REPRESENTATION('',(#4178),#126567) ;
#478 = ADVANCED_BREP_SHAPE_REPRESENTATION('',(#4179),#126568) ;
#479 = ADVANCED_BREP_SHAPE_REPRESENTATION('',(#4180),#126569) ;
#480 = ADVANCED_BREP_SHAPE_REPRESENTATION('',(#4181),#126570) ;
#481 = STYLED_ITEM('',(#126638),#4172) ;
#482 = STYLED_ITEM('',(#126640),#63895) ;
#483 = STYLED_ITEM('',(#126640),#63896) ;
#484 = STYLED_ITEM('',(#126640),#63897) ;
#485 = STYLED_ITEM('',(#126640),#63898) ;
#486 = STYLED_ITEM('',(#126640),#63899) ;
#487 = STYLED_ITEM('',(#126640),#63900) ;
#488 = STYLED_ITEM('',(#126640),#63901) ;
#489 = STYLED_ITEM('',(#126640),#63902) ;
#490 = STYLED_ITEM('',(#126640),#63903) ;
#491 = STYLED_ITEM('',(#126640),#63904) ;
#492 = STYLED_ITEM('',(#126640),#63905) ;
#493 = STYLED_ITEM('',(#126640),#63906) ;
#494 = STYLED_ITEM('',(#126640),#63907) ;
#495 = STYLED_ITEM('',(#126640),#63908) ;
#496 = STYLED_ITEM('',(#126640),#63909) ;
#497 = STYLED_ITEM('',(#126640),#63910) ;
#498 = STYLED_ITEM('',(#126640),#63911) ;
#499 = STYLED_ITEM('',(#126640),#63912) ;
#500 = STYLED_ITEM('',(#126640),#63913) ;
#501 = STYLED_ITEM('',(#126640),#63914) ;
#502 = STYLED_ITEM('',(#126640),#63915) ;
#503 = STYLED_ITEM('',(#126640),#63916) ;
#504 = STYLED_ITEM('',(#126640),#63917) ;
#505 = STYLED_ITEM('',(#126640),#63918) ;
#506 = STYLED_ITEM('',(#126640),#63919) ;
#507 = STYLED_ITEM('',(#126640),#63920) ;
#508 = STYLED_ITEM('',(#126640),#63921) ;
#509 = STYLED_ITEM('',(#126640),#63922) ;
#510 = STYLED_ITEM('',(#126640),#63923) ;
#511 = STYLED_ITEM('',(#126640),#63924) ;
#512 = STYLED_ITEM('',(#126640),#63925) ;
#513 = STYLED_ITEM('',(#126640),#63926) ;
#514 = STYLED_ITEM('',(#126640),#63927) ;
#515 = STYLED_ITEM('',(#126640),#63928) ;
#516 = STYLED_ITEM('',(#126640),#63929) ;
#517 = STYLED_ITEM('',(#126640),#63930) ;
#518 = STYLED_ITEM('',(#126640),#63931) ;
#519 = STYLED_ITEM('',(#126640),#63932) ;
#520 = STYLED_ITEM('',(#126640),#63933) ;
#521 = STYLED_ITEM('',(#126640),#63934) ;
#522 = STYLED_ITEM('',(#126640),#63935) ;
#523 = STYLED_ITEM('',(#126640),#63936) ;
#524 = STYLED_ITEM('',(#126640),#63937) ;
#525 = STYLED_ITEM('',(#126640),#63938) ;
#526 = STYLED_ITEM('',(#126640),#63939) ;
#527 = STYLED_ITEM('',(#126640),#63940) ;
#528 = STYLED_ITEM('',(#126640),#63941) ;
#529 = STYLED_ITEM('',(#126640),#63942) ;
#530 = STYLED_ITEM('',(#126640),#63943) ;
#531 = STYLED_ITEM('',(#126640),#63944) ;
#532 = STYLED_ITEM('',(#126640),#63945) ;
#533 = STYLED_ITEM('',(#126640),#63946) ;
#534 = STYLED_ITEM('',(#126640),#63947) ;
#535 = STYLED_ITEM('',(#126640),#63948) ;
#536 = STYLED_ITEM('',(#126640),#63949) ;
#537 = STYLED_ITEM('',(#126640),#63950) ;
#538 = STYLED_ITEM('',(#126641),#63951) ;
#539 = STYLED_ITEM('',(#126641),#63952) ;
#540 = STYLED_ITEM('',(#126641),#63953) ;
#541 = STYLED_ITEM('',(#126641),#63954) ;
#542 = STYLED_ITEM('',(#126641),#63955) ;
#543 = STYLED_ITEM('',(#126641),#63956) ;
#544 = STYLED_ITEM('',(#126641),#63957) ;
#545 = STYLED_ITEM('',(#126641),#63958) ;
#546 = STYLED_ITEM('',(#126641),#63959) ;
#547 = STYLED_ITEM('',(#126641),#63960) ;
#548 = STYLED_ITEM('',(#126641),#63961) ;
#549 = STYLED_ITEM('',(#126641),#63962) ;
#550 = STYLED_ITEM('',(#126641),#63963) ;
#551 = STYLED_ITEM('',(#126641),#63964) ;
#552 = STYLED_ITEM('',(#126641),#63965) ;
#553 = STYLED_ITEM('',(#126641),#63966) ;
#554 = STYLED_ITEM('',(#126641),#63967) ;
#555 = STYLED_ITEM('',(#126641),#63968) ;
#556 = STYLED_ITEM('',(#126641),#63969) ;
#557 = STYLED_ITEM('',(#126641),#63970) ;
#558 = STYLED_ITEM('',(#126640),#63971) ;
#559 = STYLED_ITEM('',(#126640),#63972) ;
#560 = STYLED_ITEM('',(#126640),#63973) ;
#561 = STYLED_ITEM('',(#126640),#63974) ;
#562 = STYLED_ITEM('',(#126640),#63975) ;
#563 = STYLED_ITEM('',(#126640),#63976) ;
#564 = STYLED_ITEM('',(#126640),#63977) ;
#565 = STYLED_ITEM('',(#126640),#63978) ;
#566 = STYLED_ITEM('',(#126640),#63979) ;
#567 = STYLED_ITEM('',(#126640),#63980) ;
#568 = STYLED_ITEM('',(#126640),#63981) ;
#569 = STYLED_ITEM('',(#126640),#63982) ;
#570 = STYLED_ITEM('',(#126640),#63983) ;
#571 = STYLED_ITEM('',(#126640),#63984) ;
#572 = STYLED_ITEM('',(#126640),#63985) ;
#573 = STYLED_ITEM('',(#126640),#63986) ;
#574 = STYLED_ITEM('',(#126640),#63987) ;
#575 = STYLED_ITEM('',(#126640),#63988) ;
#576 = STYLED_ITEM('',(#126640),#63989) ;
#577 = STYLED_ITEM('',(#126640),#63990) ;
#578 = STYLED_ITEM('',(#126640),#63991) ;
#579 = STYLED_ITEM('',(#126640),#63992) ;
#580 = STYLED_ITEM('',(#126640),#63993) ;
#581 = STYLED_ITEM('',(#126640),#63994) ;
#582 = STYLED_ITEM('',(#126640),#63995) ;
#583 = STYLED_ITEM('',(#126640),#63996) ;
#584 = STYLED_ITEM('',(#126640),#63997) ;
#585 = STYLED_ITEM('',(#126640),#63998) ;
#586 = STYLED_ITEM('',(#126640),#63999) ;
#587 = STYLED_ITEM('',(#126640),#64000) ;
#588 = STYLED_ITEM('',(#126640),#64001) ;
#589 = STYLED_ITEM('',(#126640),#64002) ;
#590 = STYLED_ITEM('',(#126640),#64003) ;
#591 = STYLED_ITEM('',(#126640),#64004) ;
#592 = STYLED_ITEM('',(#126640),#64005) ;
#593 = STYLED_ITEM('',(#126640),#64006) ;
#594 = STYLED_ITEM('',(#126640),#64007) ;
#595 = STYLED_ITEM('',(#126640),#64008) ;
#596 = STYLED_ITEM('',(#126640),#64009) ;
#597 = STYLED_ITEM('',(#126640),#64010) ;
#598 = STYLED_ITEM('',(#126640),#64011) ;
#599 = STYLED_ITEM('',(#126640),#64012) ;
#600 = STYLED_ITEM('',(#126640),#64013) ;
#601 = STYLED_ITEM('',(#126640),#64014) ;
#602 = STYLED_ITEM('',(#126640),#64015) ;
#603 = STYLED_ITEM('',(#126640),#64016) ;
#604 = STYLED_ITEM('',(#126640),#64017) ;
#605 = STYLED_ITEM('',(#126640),#64018) ;
#606 = STYLED_ITEM('',(#126640),#64019) ;
#607 = STYLED_ITEM('',(#126640),#64020) ;
#608 = STYLED_ITEM('',(#126640),#64021) ;
#609 = STYLED_ITEM('',(#126640),#64022) ;
#610 = STYLED_ITEM('',(#126640),#64023) ;
#611 = STYLED_ITEM('',(#126640),#64024) ;
#612 = STYLED_ITEM('',(#126640),#64025) ;
#613 = STYLED_ITEM('',(#126640),#64026) ;
#614 = STYLED_ITEM('',(#126640),#64027) ;
#615 = STYLED_ITEM('',(#126640),#64028) ;
#616 = STYLED_ITEM('',(#126640),#64029) ;
#617 = STYLED_ITEM('',(#126640),#64030) ;
#618 = STYLED_ITEM('',(#126640),#64031) ;
#619 = STYLED_ITEM('',(#126640),#64032) ;
#620 = STYLED_ITEM('',(#126640),#64033) ;
#621 = STYLED_ITEM('',(#126640),#64034) ;
#622 = STYLED_ITEM('',(#126640),#64035) ;
#623 = STYLED_ITEM('',(#126640),#64036) ;
#624 = STYLED_ITEM('',(#126640),#64037) ;
#625 = STYLED_ITEM('',(#126640),#64038) ;
#626 = STYLED_ITEM('',(#126640),#64039) ;
#627 = STYLED_ITEM('',(#126640),#64040) ;
#628 = STYLED_ITEM('',(#126640),#64041) ;
#629 = STYLED_ITEM('',(#126640),#64042) ;
#630 = STYLED_ITEM('',(#126640),#64043) ;
#631 = STYLED_ITEM('',(#126640),#64044) ;
#632 = STYLED_ITEM('',(#126640),#64045) ;
#633 = STYLED_ITEM('',(#126640),#64046) ;
#634 = STYLED_ITEM('',(#126640),#64047) ;
#635 = STYLED_ITEM('',(#126640),#64048) ;
#636 = STYLED_ITEM('',(#126640),#64049) ;
#637 = STYLED_ITEM('',(#126640),#64050) ;
#638 = STYLED_ITEM('',(#126640),#64051) ;
#639 = STYLED_ITEM('',(#126640),#64052) ;
#640 = STYLED_ITEM('',(#126640),#64053) ;
#641 = STYLED_ITEM('',(#126640),#64054) ;
#642 = STYLED_ITEM('',(#126640),#64055) ;
#643 = STYLED_ITEM('',(#126640),#64056) ;
#644 = STYLED_ITEM('',(#126640),#64057) ;
#645 = STYLED_ITEM('',(#126640),#64058) ;
#646 = STYLED_ITEM('',(#126640),#64059) ;
#647 = STYLED_ITEM('',(#126640),#64060) ;
#648 = STYLED_ITEM('',(#126640),#64061) ;
#649 = STYLED_ITEM('',(#126640),#64062) ;
#650 = STYLED_ITEM('',(#126640),#64063) ;
#651 = STYLED_ITEM('',(#126640),#64064) ;
#652 = STYLED_ITEM('',(#126640),#64065) ;
#653 = STYLED_ITEM('',(#126640),#64066) ;
#654 = STYLED_ITEM('',(#126640),#64067) ;
#655 = STYLED_ITEM('',(#126640),#64068) ;
#656 = STYLED_ITEM('',(#126640),#64069) ;
#657 = STYLED_ITEM('',(#126640),#64070) ;
#658 = STYLED_ITEM('',(#126640),#64071) ;
#659 = STYLED_ITEM('',(#126640),#64072) ;
#660 = STYLED_ITEM('',(#126640),#64073) ;
#661 = STYLED_ITEM('',(#126640),#64074) ;
#662 = STYLED_ITEM('',(#126640),#64075) ;
#663 = STYLED_ITEM('',(#126641),#64076) ;
#664 = STYLED_ITEM('',(#126641),#64077) ;
#665 = STYLED_ITEM('',(#126641),#64078) ;
#666 = STYLED_ITEM('',(#126641),#64079) ;
#667 = STYLED_ITEM('',(#126641),#64080) ;
#668 = STYLED_ITEM('',(#126641),#64081) ;
#669 = STYLED_ITEM('',(#126641),#64082) ;
#670 = STYLED_ITEM('',(#126641),#64083) ;
#671 = STYLED_ITEM('',(#126641),#64084) ;
#672 = STYLED_ITEM('',(#126641),#64085) ;
#673 = STYLED_ITEM('',(#126641),#64086) ;
#674 = STYLED_ITEM('',(#126641),#64087) ;
#675 = STYLED_ITEM('',(#126641),#64088) ;
#676 = STYLED_ITEM('',(#126641),#64089) ;
#677 = STYLED_ITEM('',(#126641),#64090) ;
#678 = STYLED_ITEM('',(#126641),#64091) ;
#679 = STYLED_ITEM('',(#126641),#64092) ;
#680 = STYLED_ITEM('',(#126641),#64093) ;
#681 = STYLED_ITEM('',(#126641),#64094) ;
#682 = STYLED_ITEM('',(#126641),#64095) ;
#683 = STYLED_ITEM('',(#126641),#64096) ;
#684 = STYLED_ITEM('',(#126641),#64097) ;
#685 = STYLED_ITEM('',(#126641),#64098) ;
#686 = STYLED_ITEM('',(#126641),#64099) ;
#687 = STYLED_ITEM('',(#126641),#64100) ;
#688 = STYLED_ITEM('',(#126641),#64101) ;
#689 = STYLED_ITEM('',(#126641),#64102) ;
#690 = STYLED_ITEM('',(#126641),#64103) ;
#691 = STYLED_ITEM('',(#126641),#64104) ;
#692 = STYLED_ITEM('',(#126641),#64105) ;
#693 = STYLED_ITEM('',(#126641),#64106) ;
#694 = STYLED_ITEM('',(#126641),#64107) ;
#695 = STYLED_ITEM('',(#126641),#64108) ;
#696 = STYLED_ITEM('',(#126641),#64109) ;
#697 = STYLED_ITEM('',(#126641),#64110) ;
#698 = STYLED_ITEM('',(#126641),#64111) ;
#699 = STYLED_ITEM('',(#126640),#64112) ;
#700 = STYLED_ITEM('',(#126640),#64113) ;
#701 = STYLED_ITEM('',(#126640),#64114) ;
#702 = STYLED_ITEM('',(#126640),#64115) ;
#703 = STYLED_ITEM('',(#126640),#64116) ;
#704 = STYLED_ITEM('',(#126640),#64117) ;
#705 = STYLED_ITEM('',(#126640),#64118) ;
#706 = STYLED_ITEM('',(#126640),#64119) ;
#707 = STYLED_ITEM('',(#126640),#64120) ;
#708 = STYLED_ITEM('',(#126640),#64121) ;
#709 = STYLED_ITEM('',(#126640),#64122) ;
#710 = STYLED_ITEM('',(#126640),#64123) ;
#711 = STYLED_ITEM('',(#126640),#64124) ;
#712 = STYLED_ITEM('',(#126640),#64125) ;
#713 = STYLED_ITEM('',(#126640),#64126) ;
#714 = STYLED_ITEM('',(#126640),#64127) ;
#715 = STYLED_ITEM('',(#126640),#64128) ;
#716 = STYLED_ITEM('',(#126640),#64129) ;
#717 = STYLED_ITEM('',(#126640),#64130) ;
#718 = STYLED_ITEM('',(#126640),#64131) ;
#719 = STYLED_ITEM('',(#126640),#64132) ;
#720 = STYLED_ITEM('',(#126640),#64133) ;
#721 = STYLED_ITEM('',(#126640),#64134) ;
#722 = STYLED_ITEM('',(#126640),#64135) ;
#723 = STYLED_ITEM('',(#126640),#64136) ;
#724 = STYLED_ITEM('',(#126640),#64137) ;
#725 = STYLED_ITEM('',(#126640),#64138) ;
#726 = STYLED_ITEM('',(#126640),#64139) ;
#727 = STYLED_ITEM('',(#126640),#64140) ;
#728 = STYLED_ITEM('',(#126640),#64141) ;
#729 = STYLED_ITEM('',(#126640),#64142) ;
#730 = STYLED_ITEM('',(#126640),#64143) ;
#731 = STYLED_ITEM('',(#126640),#64144) ;
#732 = STYLED_ITEM('',(#126640),#64145) ;
#733 = STYLED_ITEM('',(#126640),#64146) ;
#734 = STYLED_ITEM('',(#126640),#64147) ;
#735 = STYLED_ITEM('',(#126640),#64148) ;
#736 = STYLED_ITEM('',(#126640),#64149) ;
#737 = STYLED_ITEM('',(#126640),#64150) ;
#738 = STYLED_ITEM('',(#126640),#64151) ;
#739 = STYLED_ITEM('',(#126640),#64152) ;
#740 = STYLED_ITEM('',(#126640),#64153) ;
#741 = STYLED_ITEM('',(#126640),#64154) ;
#742 = STYLED_ITEM('',(#126640),#64155) ;
#743 = STYLED_ITEM('',(#126640),#64156) ;
#744 = STYLED_ITEM('',(#126640),#64157) ;
#745 = STYLED_ITEM('',(#126640),#64158) ;
#746 = STYLED_ITEM('',(#126641),#64159) ;
#747 = STYLED_ITEM('',(#126641),#64160) ;
#748 = STYLED_ITEM('',(#126641),#64161) ;
#749 = STYLED_ITEM('',(#126641),#64162) ;
#750 = STYLED_ITEM('',(#126641),#64163) ;
#751 = STYLED_ITEM('',(#126641),#64164) ;
#752 = STYLED_ITEM('',(#126641),#64165) ;
#753 = STYLED_ITEM('',(#126641),#64166) ;
#754 = STYLED_ITEM('',(#126641),#64167) ;
#755 = STYLED_ITEM('',(#126641),#64168) ;
#756 = STYLED_ITEM('',(#126641),#64169) ;
#757 = STYLED_ITEM('',(#126641),#64170) ;
#758 = STYLED_ITEM('',(#126641),#64171) ;
#759 = STYLED_ITEM('',(#126641),#64172) ;
#760 = STYLED_ITEM('',(#126641),#64173) ;
#761 = STYLED_ITEM('',(#126641),#64174) ;
#762 = STYLED_ITEM('',(#126640),#64175) ;
#763 = STYLED_ITEM('',(#126640),#64176) ;
#764 = STYLED_ITEM('',(#126640),#64177) ;
#765 = STYLED_ITEM('',(#126640),#64178) ;
#766 = STYLED_ITEM('',(#126640),#64179) ;
#767 = STYLED_ITEM('',(#126640),#64180) ;
#768 = STYLED_ITEM('',(#126640),#64181) ;
#769 = STYLED_ITEM('',(#126640),#64182) ;
#770 = STYLED_ITEM('',(#126640),#64183) ;
#771 = STYLED_ITEM('',(#126639),#4173) ;
#772 = STYLED_ITEM('',(#126640),#64184) ;
#773 = STYLED_ITEM('',(#126640),#64185) ;
#774 = STYLED_ITEM('',(#126640),#64186) ;
#775 = STYLED_ITEM('',(#126640),#64187) ;
#776 = STYLED_ITEM('',(#126640),#64188) ;
#777 = STYLED_ITEM('',(#126640),#64189) ;
#778 = STYLED_ITEM('',(#126640),#64190) ;
#779 = STYLED_ITEM('',(#126640),#64191) ;
#780 = STYLED_ITEM('',(#126640),#64192) ;
#781 = STYLED_ITEM('',(#126640),#64193) ;
#782 = STYLED_ITEM('',(#126640),#64194) ;
#783 = STYLED_ITEM('',(#126640),#64195) ;
#784 = STYLED_ITEM('',(#126640),#64196) ;
#785 = STYLED_ITEM('',(#126640),#64197) ;
#786 = STYLED_ITEM('',(#126640),#64198) ;
#787 = STYLED_ITEM('',(#126640),#64199) ;
#788 = STYLED_ITEM('',(#126640),#64200) ;
#789 = STYLED_ITEM('',(#126640),#64201) ;
#790 = STYLED_ITEM('',(#126640),#64202) ;
#791 = STYLED_ITEM('',(#126640),#64203) ;
#792 = STYLED_ITEM('',(#126640),#64204) ;
#793 = STYLED_ITEM('',(#126640),#64205) ;
#794 = STYLED_ITEM('',(#126640),#64206) ;
#795 = STYLED_ITEM('',(#126640),#64207) ;
#796 = STYLED_ITEM('',(#126640),#64208) ;
#797 = STYLED_ITEM('',(#126640),#64209) ;
#798 = STYLED_ITEM('',(#126640),#64210) ;
#799 = STYLED_ITEM('',(#126640),#64211) ;
#800 = STYLED_ITEM('',(#126640),#64212) ;
#801 = STYLED_ITEM('',(#126640),#64213) ;
#802 = STYLED_ITEM('',(#126640),#64214) ;
#803 = STYLED_ITEM('',(#126640),#64215) ;
#804 = STYLED_ITEM('',(#126640),#64216) ;
#805 = STYLED_ITEM('',(#126640),#64217) ;
#806 = STYLED_ITEM('',(#126640),#64218) ;
#807 = STYLED_ITEM('',(#126640),#64219) ;
#808 = STYLED_ITEM('',(#126640),#64220) ;
#809 = STYLED_ITEM('',(#126640),#64221) ;
#810 = STYLED_ITEM('',(#126640),#64222) ;
#811 = STYLED_ITEM('',(#126640),#64223) ;
#812 = STYLED_ITEM('',(#126640),#64224) ;
#813 = STYLED_ITEM('',(#126640),#64225) ;
#814 = STYLED_ITEM('',(#126640),#64226) ;
#815 = STYLED_ITEM('',(#126640),#64227) ;
#816 = STYLED_ITEM('',(#126640),#64228) ;
#817 = STYLED_ITEM('',(#126640),#64229) ;
#818 = STYLED_ITEM('',(#126640),#64230) ;
#819 = STYLED_ITEM('',(#126640),#64231) ;
#820 = STYLED_ITEM('',(#126640),#64232) ;
#821 = STYLED_ITEM('',(#126640),#64233) ;
#822 = STYLED_ITEM('',(#126640),#64234) ;
#823 = STYLED_ITEM('',(#126640),#64235) ;
#824 = STYLED_ITEM('',(#126640),#64236) ;
#825 = STYLED_ITEM('',(#126640),#64237) ;
#826 = STYLED_ITEM('',(#126640),#64238) ;
#827 = STYLED_ITEM('',(#126640),#64239) ;
#828 = STYLED_ITEM('',(#126641),#64240) ;
#829 = STYLED_ITEM('',(#126641),#64241) ;
#830 = STYLED_ITEM('',(#126641),#64242) ;
#831 = STYLED_ITEM('',(#126641),#64243) ;
#832 = STYLED_ITEM('',(#126641),#64244) ;
#833 = STYLED_ITEM('',(#126641),#64245) ;
#834 = STYLED_ITEM('',(#126641),#64246) ;
#835 = STYLED_ITEM('',(#126641),#64247) ;
#836 = STYLED_ITEM('',(#126641),#64248) ;
#837 = STYLED_ITEM('',(#126641),#64249) ;
#838 = STYLED_ITEM('',(#126641),#64250) ;
#839 = STYLED_ITEM('',(#126641),#64251) ;
#840 = STYLED_ITEM('',(#126641),#64252) ;
#841 = STYLED_ITEM('',(#126641),#64253) ;
#842 = STYLED_ITEM('',(#126641),#64254) ;
#843 = STYLED_ITEM('',(#126641),#64255) ;
#844 = STYLED_ITEM('',(#126641),#64256) ;
#845 = STYLED_ITEM('',(#126641),#64257) ;
#846 = STYLED_ITEM('',(#126641),#64258) ;
#847 = STYLED_ITEM('',(#126641),#64259) ;
#848 = STYLED_ITEM('',(#126640),#64260) ;
#849 = STYLED_ITEM('',(#126640),#64261) ;
#850 = STYLED_ITEM('',(#126640),#64262) ;
#851 = STYLED_ITEM('',(#126640),#64263) ;
#852 = STYLED_ITEM('',(#126640),#64264) ;
#853 = STYLED_ITEM('',(#126640),#64265) ;
#854 = STYLED_ITEM('',(#126640),#64266) ;
#855 = STYLED_ITEM('',(#126640),#64267) ;
#856 = STYLED_ITEM('',(#126640),#64268) ;
#857 = STYLED_ITEM('',(#126640),#64269) ;
#858 = STYLED_ITEM('',(#126640),#64270) ;
#859 = STYLED_ITEM('',(#126640),#64271) ;
#860 = STYLED_ITEM('',(#126640),#64272) ;
#861 = STYLED_ITEM('',(#126640),#64273) ;
#862 = STYLED_ITEM('',(#126640),#64274) ;
#863 = STYLED_ITEM('',(#126640),#64275) ;
#864 = STYLED_ITEM('',(#126640),#64276) ;
#865 = STYLED_ITEM('',(#126640),#64277) ;
#866 = STYLED_ITEM('',(#126640),#64278) ;
#867 = STYLED_ITEM('',(#126640),#64279) ;
#868 = STYLED_ITEM('',(#126640),#64280) ;
#869 = STYLED_ITEM('',(#126640),#64281) ;
#870 = STYLED_ITEM('',(#126640),#64282) ;
#871 = STYLED_ITEM('',(#126640),#64283) ;
#872 = STYLED_ITEM('',(#126640),#64284) ;
#873 = STYLED_ITEM('',(#126640),#64285) ;
#874 = STYLED_ITEM('',(#126640),#64286) ;
#875 = STYLED_ITEM('',(#126640),#64287) ;
#876 = STYLED_ITEM('',(#126640),#64288) ;
#877 = STYLED_ITEM('',(#126640),#64289) ;
#878 = STYLED_ITEM('',(#126640),#64290) ;
#879 = STYLED_ITEM('',(#126640),#64291) ;
#880 = STYLED_ITEM('',(#126640),#64292) ;
#881 = STYLED_ITEM('',(#126640),#64293) ;
#882 = STYLED_ITEM('',(#126640),#64294) ;
#883 = STYLED_ITEM('',(#126640),#64295) ;
#884 = STYLED_ITEM('',(#126640),#64296) ;
#885 = STYLED_ITEM('',(#126640),#64297) ;
#886 = STYLED_ITEM('',(#126640),#64298) ;
#887 = STYLED_ITEM('',(#126640),#64299) ;
#888 = STYLED_ITEM('',(#126640),#64300) ;
#889 = STYLED_ITEM('',(#126640),#64301) ;
#890 = STYLED_ITEM('',(#126640),#64302) ;
#891 = STYLED_ITEM('',(#126640),#64303) ;
#892 = STYLED_ITEM('',(#126640),#64304) ;
#893 = STYLED_ITEM('',(#126640),#64305) ;
#894 = STYLED_ITEM('',(#126640),#64306) ;
#895 = STYLED_ITEM('',(#126640),#64307) ;
#896 = STYLED_ITEM('',(#126640),#64308) ;
#897 = STYLED_ITEM('',(#126640),#64309) ;
#898 = STYLED_ITEM('',(#126640),#64310) ;
#899 = STYLED_ITEM('',(#126640),#64311) ;
#900 = STYLED_ITEM('',(#126640),#64312) ;
#901 = STYLED_ITEM('',(#126640),#64313) ;
#902 = STYLED_ITEM('',(#126640),#64314) ;
#903 = STYLED_ITEM('',(#126640),#64315) ;
#904 = STYLED_ITEM('',(#126640),#64316) ;
#905 = STYLED_ITEM('',(#126640),#64317) ;
#906 = STYLED_ITEM('',(#126640),#64318) ;
#907 = STYLED_ITEM('',(#126640),#64319) ;
#908 = STYLED_ITEM('',(#126640),#64320) ;
#909 = STYLED_ITEM('',(#126640),#64321) ;
#910 = STYLED_ITEM('',(#126640),#64322) ;
#911 = STYLED_ITEM('',(#126640),#64323) ;
#912 = STYLED_ITEM('',(#126640),#64324) ;
#913 = STYLED_ITEM('',(#126640),#64325) ;
#914 = STYLED_ITEM('',(#126640),#64326) ;
#915 = STYLED_ITEM('',(#126640),#64327) ;
#916 = STYLED_ITEM('',(#126640),#64328) ;
#917 = STYLED_ITEM('',(#126640),#64329) ;
#918 = STYLED_ITEM('',(#126640),#64330) ;
#919 = STYLED_ITEM('',(#126640),#64331) ;
#920 = STYLED_ITEM('',(#126640),#64332) ;
#921 = STYLED_ITEM('',(#126640),#64333) ;
#922 = STYLED_ITEM('',(#126640),#64334) ;
#923 = STYLED_ITEM('',(#126640),#64335) ;
#924 = STYLED_ITEM('',(#126640),#64336) ;
#925 = STYLED_ITEM('',(#126640),#64337) ;
#926 = STYLED_ITEM('',(#126640),#64338) ;
#927 = STYLED_ITEM('',(#126640),#64339) ;
#928 = STYLED_ITEM('',(#126640),#64340) ;
#929 = STYLED_ITEM('',(#126640),#64341) ;
#930 = STYLED_ITEM('',(#126640),#64342) ;
#931 = STYLED_ITEM('',(#126640),#64343) ;
#932 = STYLED_ITEM('',(#126640),#64344) ;
#933 = STYLED_ITEM('',(#126640),#64345) ;
#934 = STYLED_ITEM('',(#126640),#64346) ;
#935 = STYLED_ITEM('',(#126640),#64347) ;
#936 = STYLED_ITEM('',(#126640),#64348) ;
#937 = STYLED_ITEM('',(#126640),#64349) ;
#938 = STYLED_ITEM('',(#126640),#64350) ;
#939 = STYLED_ITEM('',(#126640),#64351) ;
#940 = STYLED_ITEM('',(#126640),#64352) ;
#941 = STYLED_ITEM('',(#126640),#64353) ;
#942 = STYLED_ITEM('',(#126640),#64354) ;
#943 = STYLED_ITEM('',(#126640),#64355) ;
#944 = STYLED_ITEM('',(#126640),#64356) ;
#945 = STYLED_ITEM('',(#126640),#64357) ;
#946 = STYLED_ITEM('',(#126640),#64358) ;
#947 = STYLED_ITEM('',(#126640),#64359) ;
#948 = STYLED_ITEM('',(#126640),#64360) ;
#949 = STYLED_ITEM('',(#126640),#64361) ;
#950 = STYLED_ITEM('',(#126640),#64362) ;
#951 = STYLED_ITEM('',(#126640),#64363) ;
#952 = STYLED_ITEM('',(#126640),#64364) ;
#953 = STYLED_ITEM('',(#126641),#64365) ;
#954 = STYLED_ITEM('',(#126641),#64366) ;
#955 = STYLED_ITEM('',(#126641),#64367) ;
#956 = STYLED_ITEM('',(#126641),#64368) ;
#957 = STYLED_ITEM('',(#126641),#64369) ;
#958 = STYLED_ITEM('',(#126641),#64370) ;
#959 = STYLED_ITEM('',(#126640),#64371) ;
#960 = STYLED_ITEM('',(#126641),#64372) ;
#961 = STYLED_ITEM('',(#126641),#64373) ;
#962 = STYLED_ITEM('',(#126641),#64374) ;
#963 = STYLED_ITEM('',(#126641),#64375) ;
#964 = STYLED_ITEM('',(#126641),#64376) ;
#965 = STYLED_ITEM('',(#126640),#64377) ;
#966 = STYLED_ITEM('',(#126640),#64378) ;
#967 = STYLED_ITEM('',(#126641),#64379) ;
#968 = STYLED_ITEM('',(#126641),#64380) ;
#969 = STYLED_ITEM('',(#126640),#64381) ;
#970 = STYLED_ITEM('',(#126641),#64382) ;
#971 = STYLED_ITEM('',(#126641),#64383) ;
#972 = STYLED_ITEM('',(#126641),#64384) ;
#973 = STYLED_ITEM('',(#126641),#64385) ;
#974 = STYLED_ITEM('',(#126641),#64386) ;
#975 = STYLED_ITEM('',(#126641),#64387) ;
#976 = STYLED_ITEM('',(#126641),#64388) ;
#977 = STYLED_ITEM('',(#126641),#64389) ;
#978 = STYLED_ITEM('',(#126640),#64390) ;
#979 = STYLED_ITEM('',(#126641),#64391) ;
#980 = STYLED_ITEM('',(#126641),#64392) ;
#981 = STYLED_ITEM('',(#126640),#64393) ;
#982 = STYLED_ITEM('',(#126641),#64394) ;
#983 = STYLED_ITEM('',(#126641),#64395) ;
#984 = STYLED_ITEM('',(#126641),#64396) ;
#985 = STYLED_ITEM('',(#126641),#64397) ;
#986 = STYLED_ITEM('',(#126640),#64398) ;
#987 = STYLED_ITEM('',(#126640),#64399) ;
#988 = STYLED_ITEM('',(#126641),#64400) ;
#989 = STYLED_ITEM('',(#126640),#64401) ;
#990 = STYLED_ITEM('',(#126640),#64402) ;
#991 = STYLED_ITEM('',(#126640),#64403) ;
#992 = STYLED_ITEM('',(#126640),#64404) ;
#993 = STYLED_ITEM('',(#126640),#64405) ;
#994 = STYLED_ITEM('',(#126640),#64406) ;
#995 = STYLED_ITEM('',(#126640),#64407) ;
#996 = STYLED_ITEM('',(#126640),#64408) ;
#997 = STYLED_ITEM('',(#126640),#64409) ;
#998 = STYLED_ITEM('',(#126640),#64410) ;
#999 = STYLED_ITEM('',(#126640),#64411) ;
#1000 = STYLED_ITEM('',(#126640),#64412) ;
#1001 = STYLED_ITEM('',(#126640),#64413) ;
#1002 = STYLED_ITEM('',(#126640),#64414) ;
#1003 = STYLED_ITEM('',(#126640),#64415) ;
#1004 = STYLED_ITEM('',(#126640),#64416) ;
#1005 = STYLED_ITEM('',(#126640),#64417) ;
#1006 = STYLED_ITEM('',(#126640),#64418) ;
#1007 = STYLED_ITEM('',(#126640),#64419) ;
#1008 = STYLED_ITEM('',(#126640),#64420) ;
#1009 = STYLED_ITEM('',(#126640),#64421) ;
#1010 = STYLED_ITEM('',(#126640),#64422) ;
#1011 = STYLED_ITEM('',(#126640),#64423) ;
#1012 = STYLED_ITEM('',(#126640),#64424) ;
#1013 = STYLED_ITEM('',(#126640),#64425) ;
#1014 = STYLED_ITEM('',(#126640),#64426) ;
#1015 = STYLED_ITEM('',(#126640),#64427) ;
#1016 = STYLED_ITEM('',(#126640),#64428) ;
#1017 = STYLED_ITEM('',(#126640),#64429) ;
#1018 = STYLED_ITEM('',(#126640),#64430) ;
#1019 = STYLED_ITEM('',(#126640),#64431) ;
#1020 = STYLED_ITEM('',(#126640),#64432) ;
#1021 = STYLED_ITEM('',(#126640),#64433) ;
#1022 = STYLED_ITEM('',(#126640),#64434) ;
#1023 = STYLED_ITEM('',(#126640),#64435) ;
#1024 = STYLED_ITEM('',(#126640),#64436) ;
#1025 = STYLED_ITEM('',(#126640),#64437) ;
#1026 = STYLED_ITEM('',(#126640),#64438) ;
#1027 = STYLED_ITEM('',(#126640),#64439) ;
#1028 = STYLED_ITEM('',(#126640),#64440) ;
#1029 = STYLED_ITEM('',(#126640),#64441) ;
#1030 = STYLED_ITEM('',(#126640),#64442) ;
#1031 = STYLED_ITEM('',(#126640),#64443) ;
#1032 = STYLED_ITEM('',(#126640),#64444) ;
#1033 = STYLED_ITEM('',(#126640),#64445) ;
#1034 = STYLED_ITEM('',(#126640),#64446) ;
#1035 = STYLED_ITEM('',(#126640),#64447) ;
#1036 = STYLED_ITEM('',(#126641),#64448) ;
#1037 = STYLED_ITEM('',(#126641),#64449) ;
#1038 = STYLED_ITEM('',(#126641),#64450) ;
#1039 = STYLED_ITEM('',(#126641),#64451) ;
#1040 = STYLED_ITEM('',(#126641),#64452) ;
#1041 = STYLED_ITEM('',(#126641),#64453) ;
#1042 = STYLED_ITEM('',(#126641),#64454) ;
#1043 = STYLED_ITEM('',(#126641),#64455) ;
#1044 = STYLED_ITEM('',(#126641),#64456) ;
#1045 = STYLED_ITEM('',(#126641),#64457) ;
#1046 = STYLED_ITEM('',(#126641),#64458) ;
#1047 = STYLED_ITEM('',(#126641),#64459) ;
#1048 = STYLED_ITEM('',(#126641),#64460) ;
#1049 = STYLED_ITEM('',(#126641),#64461) ;
#1050 = STYLED_ITEM('',(#126641),#64462) ;
#1051 = STYLED_ITEM('',(#126641),#64463) ;
#1052 = STYLED_ITEM('',(#126640),#64464) ;
#1053 = STYLED_ITEM('',(#126640),#64465) ;
#1054 = STYLED_ITEM('',(#126640),#64466) ;
#1055 = STYLED_ITEM('',(#126640),#64467) ;
#1056 = STYLED_ITEM('',(#126640),#64468) ;
#1057 = STYLED_ITEM('',(#126640),#64469) ;
#1058 = STYLED_ITEM('',(#126640),#64470) ;
#1059 = STYLED_ITEM('',(#126640),#64471) ;
#1060 = STYLED_ITEM('',(#126640),#64472) ;
#1061 = STYLED_ITEM('',(#126639),#4174) ;
#1062 = STYLED_ITEM('',(#126640),#64473) ;
#1063 = STYLED_ITEM('',(#126640),#64474) ;
#1064 = STYLED_ITEM('',(#126640),#64475) ;
#1065 = STYLED_ITEM('',(#126640),#64476) ;
#1066 = STYLED_ITEM('',(#126640),#64477) ;
#1067 = STYLED_ITEM('',(#126640),#64478) ;
#1068 = STYLED_ITEM('',(#126640),#64479) ;
#1069 = STYLED_ITEM('',(#126640),#64480) ;
#1070 = STYLED_ITEM('',(#126640),#64481) ;
#1071 = STYLED_ITEM('',(#126640),#64482) ;
#1072 = STYLED_ITEM('',(#126640),#64483) ;
#1073 = STYLED_ITEM('',(#126640),#64484) ;
#1074 = STYLED_ITEM('',(#126640),#64485) ;
#1075 = STYLED_ITEM('',(#126640),#64486) ;
#1076 = STYLED_ITEM('',(#126640),#64487) ;
#1077 = STYLED_ITEM('',(#126640),#64488) ;
#1078 = STYLED_ITEM('',(#126640),#64489) ;
#1079 = STYLED_ITEM('',(#126640),#64490) ;
#1080 = STYLED_ITEM('',(#126640),#64491) ;
#1081 = STYLED_ITEM('',(#126640),#64492) ;
#1082 = STYLED_ITEM('',(#126640),#64493) ;
#1083 = STYLED_ITEM('',(#126640),#64494) ;
#1084 = STYLED_ITEM('',(#126640),#64495) ;
#1085 = STYLED_ITEM('',(#126640),#64496) ;
#1086 = STYLED_ITEM('',(#126640),#64497) ;
#1087 = STYLED_ITEM('',(#126640),#64498) ;
#1088 = STYLED_ITEM('',(#126640),#64499) ;
#1089 = STYLED_ITEM('',(#126640),#64500) ;
#1090 = STYLED_ITEM('',(#126640),#64501) ;
#1091 = STYLED_ITEM('',(#126640),#64502) ;
#1092 = STYLED_ITEM('',(#126640),#64503) ;
#1093 = STYLED_ITEM('',(#126640),#64504) ;
#1094 = STYLED_ITEM('',(#126640),#64505) ;
#1095 = STYLED_ITEM('',(#126640),#64506) ;
#1096 = STYLED_ITEM('',(#126640),#64507) ;
#1097 = STYLED_ITEM('',(#126640),#64508) ;
#1098 = STYLED_ITEM('',(#126640),#64509) ;
#1099 = STYLED_ITEM('',(#126640),#64510) ;
#1100 = STYLED_ITEM('',(#126640),#64511) ;
#1101 = STYLED_ITEM('',(#126640),#64512) ;
#1102 = STYLED_ITEM('',(#126640),#64513) ;
#1103 = STYLED_ITEM('',(#126640),#64514) ;
#1104 = STYLED_ITEM('',(#126640),#64515) ;
#1105 = STYLED_ITEM('',(#126640),#64516) ;
#1106 = STYLED_ITEM('',(#126640),#64517) ;
#1107 = STYLED_ITEM('',(#126640),#64518) ;
#1108 = STYLED_ITEM('',(#126640),#64519) ;
#1109 = STYLED_ITEM('',(#126640),#64520) ;
#1110 = STYLED_ITEM('',(#126640),#64521) ;
#1111 = STYLED_ITEM('',(#126640),#64522) ;
#1112 = STYLED_ITEM('',(#126640),#64523) ;
#1113 = STYLED_ITEM('',(#126640),#64524) ;
#1114 = STYLED_ITEM('',(#126640),#64525) ;
#1115 = STYLED_ITEM('',(#126640),#64526) ;
#1116 = STYLED_ITEM('',(#126640),#64527) ;
#1117 = STYLED_ITEM('',(#126640),#64528) ;
#1118 = STYLED_ITEM('',(#126641),#64529) ;
#1119 = STYLED_ITEM('',(#126641),#64530) ;
#1120 = STYLED_ITEM('',(#126641),#64531) ;
#1121 = STYLED_ITEM('',(#126641),#64532) ;
#1122 = STYLED_ITEM('',(#126641),#64533) ;
#1123 = STYLED_ITEM('',(#126641),#64534) ;
#1124 = STYLED_ITEM('',(#126641),#64535) ;
#1125 = STYLED_ITEM('',(#126641),#64536) ;
#1126 = STYLED_ITEM('',(#126641),#64537) ;
#1127 = STYLED_ITEM('',(#126641),#64538) ;
#1128 = STYLED_ITEM('',(#126641),#64539) ;
#1129 = STYLED_ITEM('',(#126641),#64540) ;
#1130 = STYLED_ITEM('',(#126641),#64541) ;
#1131 = STYLED_ITEM('',(#126641),#64542) ;
#1132 = STYLED_ITEM('',(#126641),#64543) ;
#1133 = STYLED_ITEM('',(#126641),#64544) ;
#1134 = STYLED_ITEM('',(#126641),#64545) ;
#1135 = STYLED_ITEM('',(#126641),#64546) ;
#1136 = STYLED_ITEM('',(#126641),#64547) ;
#1137 = STYLED_ITEM('',(#126641),#64548) ;
#1138 = STYLED_ITEM('',(#126640),#64549) ;
#1139 = STYLED_ITEM('',(#126640),#64550) ;
#1140 = STYLED_ITEM('',(#126640),#64551) ;
#1141 = STYLED_ITEM('',(#126640),#64552) ;
#1142 = STYLED_ITEM('',(#126640),#64553) ;
#1143 = STYLED_ITEM('',(#126640),#64554) ;
#1144 = STYLED_ITEM('',(#126640),#64555) ;
#1145 = STYLED_ITEM('',(#126640),#64556) ;
#1146 = STYLED_ITEM('',(#126640),#64557) ;
#1147 = STYLED_ITEM('',(#126640),#64558) ;
#1148 = STYLED_ITEM('',(#126640),#64559) ;
#1149 = STYLED_ITEM('',(#126640),#64560) ;
#1150 = STYLED_ITEM('',(#126640),#64561) ;
#1151 = STYLED_ITEM('',(#126640),#64562) ;
#1152 = STYLED_ITEM('',(#126640),#64563) ;
#1153 = STYLED_ITEM('',(#126640),#64564) ;
#1154 = STYLED_ITEM('',(#126640),#64565) ;
#1155 = STYLED_ITEM('',(#126640),#64566) ;
#1156 = STYLED_ITEM('',(#126640),#64567) ;
#1157 = STYLED_ITEM('',(#126640),#64568) ;
#1158 = STYLED_ITEM('',(#126640),#64569) ;
#1159 = STYLED_ITEM('',(#126640),#64570) ;
#1160 = STYLED_ITEM('',(#126640),#64571) ;
#1161 = STYLED_ITEM('',(#126640),#64572) ;
#1162 = STYLED_ITEM('',(#126640),#64573) ;
#1163 = STYLED_ITEM('',(#126640),#64574) ;
#1164 = STYLED_ITEM('',(#126640),#64575) ;
#1165 = STYLED_ITEM('',(#126640),#64576) ;
#1166 = STYLED_ITEM('',(#126640),#64577) ;
#1167 = STYLED_ITEM('',(#126640),#64578) ;
#1168 = STYLED_ITEM('',(#126640),#64579) ;
#1169 = STYLED_ITEM('',(#126640),#64580) ;
#1170 = STYLED_ITEM('',(#126640),#64581) ;
#1171 = STYLED_ITEM('',(#126640),#64582) ;
#1172 = STYLED_ITEM('',(#126640),#64583) ;
#1173 = STYLED_ITEM('',(#126640),#64584) ;
#1174 = STYLED_ITEM('',(#126640),#64585) ;
#1175 = STYLED_ITEM('',(#126640),#64586) ;
#1176 = STYLED_ITEM('',(#126640),#64587) ;
#1177 = STYLED_ITEM('',(#126640),#64588) ;
#1178 = STYLED_ITEM('',(#126640),#64589) ;
#1179 = STYLED_ITEM('',(#126640),#64590) ;
#1180 = STYLED_ITEM('',(#126640),#64591) ;
#1181 = STYLED_ITEM('',(#126640),#64592) ;
#1182 = STYLED_ITEM('',(#126640),#64593) ;
#1183 = STYLED_ITEM('',(#126640),#64594) ;
#1184 = STYLED_ITEM('',(#126640),#64595) ;
#1185 = STYLED_ITEM('',(#126640),#64596) ;
#1186 = STYLED_ITEM('',(#126640),#64597) ;
#1187 = STYLED_ITEM('',(#126640),#64598) ;
#1188 = STYLED_ITEM('',(#126640),#64599) ;
#1189 = STYLED_ITEM('',(#126640),#64600) ;
#1190 = STYLED_ITEM('',(#126640),#64601) ;
#1191 = STYLED_ITEM('',(#126640),#64602) ;
#1192 = STYLED_ITEM('',(#126640),#64603) ;
#1193 = STYLED_ITEM('',(#126640),#64604) ;
#1194 = STYLED_ITEM('',(#126640),#64605) ;
#1195 = STYLED_ITEM('',(#126640),#64606) ;
#1196 = STYLED_ITEM('',(#126640),#64607) ;
#1197 = STYLED_ITEM('',(#126640),#64608) ;
#1198 = STYLED_ITEM('',(#126640),#64609) ;
#1199 = STYLED_ITEM('',(#126640),#64610) ;
#1200 = STYLED_ITEM('',(#126640),#64611) ;
#1201 = STYLED_ITEM('',(#126640),#64612) ;
#1202 = STYLED_ITEM('',(#126640),#64613) ;
#1203 = STYLED_ITEM('',(#126640),#64614) ;
#1204 = STYLED_ITEM('',(#126640),#64615) ;
#1205 = STYLED_ITEM('',(#126640),#64616) ;
#1206 = STYLED_ITEM('',(#126640),#64617) ;
#1207 = STYLED_ITEM('',(#126640),#64618) ;
#1208 = STYLED_ITEM('',(#126640),#64619) ;
#1209 = STYLED_ITEM('',(#126640),#64620) ;
#1210 = STYLED_ITEM('',(#126640),#64621) ;
#1211 = STYLED_ITEM('',(#126640),#64622) ;
#1212 = STYLED_ITEM('',(#126640),#64623) ;
#1213 = STYLED_ITEM('',(#126640),#64624) ;
#1214 = STYLED_ITEM('',(#126640),#64625) ;
#1215 = STYLED_ITEM('',(#126640),#64626) ;
#1216 = STYLED_ITEM('',(#126640),#64627) ;
#1217 = STYLED_ITEM('',(#126640),#64628) ;
#1218 = STYLED_ITEM('',(#126640),#64629) ;
#1219 = STYLED_ITEM('',(#126640),#64630) ;
#1220 = STYLED_ITEM('',(#126640),#64631) ;
#1221 = STYLED_ITEM('',(#126640),#64632) ;
#1222 = STYLED_ITEM('',(#126640),#64633) ;
#1223 = STYLED_ITEM('',(#126640),#64634) ;
#1224 = STYLED_ITEM('',(#126640),#64635) ;
#1225 = STYLED_ITEM('',(#126640),#64636) ;
#1226 = STYLED_ITEM('',(#126640),#64637) ;
#1227 = STYLED_ITEM('',(#126640),#64638) ;
#1228 = STYLED_ITEM('',(#126640),#64639) ;
#1229 = STYLED_ITEM('',(#126640),#64640) ;
#1230 = STYLED_ITEM('',(#126640),#64641) ;
#1231 = STYLED_ITEM('',(#126640),#64642) ;
#1232 = STYLED_ITEM('',(#126640),#64643) ;
#1233 = STYLED_ITEM('',(#126640),#64644) ;
#1234 = STYLED_ITEM('',(#126640),#64645) ;
#1235 = STYLED_ITEM('',(#126640),#64646) ;
#1236 = STYLED_ITEM('',(#126640),#64647) ;
#1237 = STYLED_ITEM('',(#126640),#64648) ;
#1238 = STYLED_ITEM('',(#126640),#64649) ;
#1239 = STYLED_ITEM('',(#126640),#64650) ;
#1240 = STYLED_ITEM('',(#126640),#64651) ;
#1241 = STYLED_ITEM('',(#126640),#64652) ;
#1242 = STYLED_ITEM('',(#126640),#64653) ;
#1243 = STYLED_ITEM('',(#126641),#64654) ;
#1244 = STYLED_ITEM('',(#126641),#64655) ;
#1245 = STYLED_ITEM('',(#126641),#64656) ;
#1246 = STYLED_ITEM('',(#126641),#64657) ;
#1247 = STYLED_ITEM('',(#126641),#64658) ;
#1248 = STYLED_ITEM('',(#126641),#64659) ;
#1249 = STYLED_ITEM('',(#126640),#64660) ;
#1250 = STYLED_ITEM('',(#126641),#64661) ;
#1251 = STYLED_ITEM('',(#126641),#64662) ;
#1252 = STYLED_ITEM('',(#126641),#64663) ;
#1253 = STYLED_ITEM('',(#126641),#64664) ;
#1254 = STYLED_ITEM('',(#126641),#64665) ;
#1255 = STYLED_ITEM('',(#126640),#64666) ;
#1256 = STYLED_ITEM('',(#126640),#64667) ;
#1257 = STYLED_ITEM('',(#126641),#64668) ;
#1258 = STYLED_ITEM('',(#126641),#64669) ;
#1259 = STYLED_ITEM('',(#126640),#64670) ;
#1260 = STYLED_ITEM('',(#126641),#64671) ;
#1261 = STYLED_ITEM('',(#126641),#64672) ;
#1262 = STYLED_ITEM('',(#126641),#64673) ;
#1263 = STYLED_ITEM('',(#126641),#64674) ;
#1264 = STYLED_ITEM('',(#126641),#64675) ;
#1265 = STYLED_ITEM('',(#126641),#64676) ;
#1266 = STYLED_ITEM('',(#126641),#64677) ;
#1267 = STYLED_ITEM('',(#126641),#64678) ;
#1268 = STYLED_ITEM('',(#126640),#64679) ;
#1269 = STYLED_ITEM('',(#126641),#64680) ;
#1270 = STYLED_ITEM('',(#126641),#64681) ;
#1271 = STYLED_ITEM('',(#126640),#64682) ;
#1272 = STYLED_ITEM('',(#126641),#64683) ;
#1273 = STYLED_ITEM('',(#126641),#64684) ;
#1274 = STYLED_ITEM('',(#126641),#64685) ;
#1275 = STYLED_ITEM('',(#126641),#64686) ;
#1276 = STYLED_ITEM('',(#126640),#64687) ;
#1277 = STYLED_ITEM('',(#126640),#64688) ;
#1278 = STYLED_ITEM('',(#126641),#64689) ;
#1279 = STYLED_ITEM('',(#126640),#64690) ;
#1280 = STYLED_ITEM('',(#126640),#64691) ;
#1281 = STYLED_ITEM('',(#126640),#64692) ;
#1282 = STYLED_ITEM('',(#126640),#64693) ;
#1283 = STYLED_ITEM('',(#126640),#64694) ;
#1284 = STYLED_ITEM('',(#126640),#64695) ;
#1285 = STYLED_ITEM('',(#126640),#64696) ;
#1286 = STYLED_ITEM('',(#126640),#64697) ;
#1287 = STYLED_ITEM('',(#126640),#64698) ;
#1288 = STYLED_ITEM('',(#126640),#64699) ;
#1289 = STYLED_ITEM('',(#126640),#64700) ;
#1290 = STYLED_ITEM('',(#126640),#64701) ;
#1291 = STYLED_ITEM('',(#126640),#64702) ;
#1292 = STYLED_ITEM('',(#126640),#64703) ;
#1293 = STYLED_ITEM('',(#126640),#64704) ;
#1294 = STYLED_ITEM('',(#126640),#64705) ;
#1295 = STYLED_ITEM('',(#126640),#64706) ;
#1296 = STYLED_ITEM('',(#126640),#64707) ;
#1297 = STYLED_ITEM('',(#126640),#64708) ;
#1298 = STYLED_ITEM('',(#126640),#64709) ;
#1299 = STYLED_ITEM('',(#126640),#64710) ;
#1300 = STYLED_ITEM('',(#126640),#64711) ;
#1301 = STYLED_ITEM('',(#126640),#64712) ;
#1302 = STYLED_ITEM('',(#126640),#64713) ;
#1303 = STYLED_ITEM('',(#126640),#64714) ;
#1304 = STYLED_ITEM('',(#126640),#64715) ;
#1305 = STYLED_ITEM('',(#126640),#64716) ;
#1306 = STYLED_ITEM('',(#126640),#64717) ;
#1307 = STYLED_ITEM('',(#126640),#64718) ;
#1308 = STYLED_ITEM('',(#126640),#64719) ;
#1309 = STYLED_ITEM('',(#126640),#64720) ;
#1310 = STYLED_ITEM('',(#126640),#64721) ;
#1311 = STYLED_ITEM('',(#126640),#64722) ;
#1312 = STYLED_ITEM('',(#126640),#64723) ;
#1313 = STYLED_ITEM('',(#126640),#64724) ;
#1314 = STYLED_ITEM('',(#126640),#64725) ;
#1315 = STYLED_ITEM('',(#126640),#64726) ;
#1316 = STYLED_ITEM('',(#126640),#64727) ;
#1317 = STYLED_ITEM('',(#126640),#64728) ;
#1318 = STYLED_ITEM('',(#126640),#64729) ;
#1319 = STYLED_ITEM('',(#126640),#64730) ;
#1320 = STYLED_ITEM('',(#126640),#64731) ;
#1321 = STYLED_ITEM('',(#126640),#64732) ;
#1322 = STYLED_ITEM('',(#126640),#64733) ;
#1323 = STYLED_ITEM('',(#126640),#64734) ;
#1324 = STYLED_ITEM('',(#126640),#64735) ;
#1325 = STYLED_ITEM('',(#126640),#64736) ;
#1326 = STYLED_ITEM('',(#126641),#64737) ;
#1327 = STYLED_ITEM('',(#126641),#64738) ;
#1328 = STYLED_ITEM('',(#126641),#64739) ;
#1329 = STYLED_ITEM('',(#126641),#64740) ;
#1330 = STYLED_ITEM('',(#126641),#64741) ;
#1331 = STYLED_ITEM('',(#126641),#64742) ;
#1332 = STYLED_ITEM('',(#126641),#64743) ;
#1333 = STYLED_ITEM('',(#126641),#64744) ;
#1334 = STYLED_ITEM('',(#126641),#64745) ;
#1335 = STYLED_ITEM('',(#126641),#64746) ;
#1336 = STYLED_ITEM('',(#126641),#64747) ;
#1337 = STYLED_ITEM('',(#126641),#64748) ;
#1338 = STYLED_ITEM('',(#126641),#64749) ;
#1339 = STYLED_ITEM('',(#126641),#64750) ;
#1340 = STYLED_ITEM('',(#126641),#64751) ;
#1341 = STYLED_ITEM('',(#126641),#64752) ;
#1342 = STYLED_ITEM('',(#126640),#64753) ;
#1343 = STYLED_ITEM('',(#126640),#64754) ;
#1344 = STYLED_ITEM('',(#126640),#64755) ;
#1345 = STYLED_ITEM('',(#126640),#64756) ;
#1346 = STYLED_ITEM('',(#126640),#64757) ;
#1347 = STYLED_ITEM('',(#126640),#64758) ;
#1348 = STYLED_ITEM('',(#126640),#64759) ;
#1349 = STYLED_ITEM('',(#126640),#64760) ;
#1350 = STYLED_ITEM('',(#126640),#64761) ;
#1351 = STYLED_ITEM('',(#126639),#4175) ;
#1352 = STYLED_ITEM('',(#126640),#64762) ;
#1353 = STYLED_ITEM('',(#126640),#64763) ;
#1354 = STYLED_ITEM('',(#126640),#64764) ;
#1355 = STYLED_ITEM('',(#126640),#64765) ;
#1356 = STYLED_ITEM('',(#126640),#64766) ;
#1357 = STYLED_ITEM('',(#126640),#64767) ;
#1358 = STYLED_ITEM('',(#126640),#64768) ;
#1359 = STYLED_ITEM('',(#126640),#64769) ;
#1360 = STYLED_ITEM('',(#126640),#64770) ;
#1361 = STYLED_ITEM('',(#126640),#64771) ;
#1362 = STYLED_ITEM('',(#126640),#64772) ;
#1363 = STYLED_ITEM('',(#126640),#64773) ;
#1364 = STYLED_ITEM('',(#126640),#64774) ;
#1365 = STYLED_ITEM('',(#126640),#64775) ;
#1366 = STYLED_ITEM('',(#126640),#64776) ;
#1367 = STYLED_ITEM('',(#126640),#64777) ;
#1368 = STYLED_ITEM('',(#126640),#64778) ;
#1369 = STYLED_ITEM('',(#126640),#64779) ;
#1370 = STYLED_ITEM('',(#126640),#64780) ;
#1371 = STYLED_ITEM('',(#126640),#64781) ;
#1372 = STYLED_ITEM('',(#126640),#64782) ;
#1373 = STYLED_ITEM('',(#126640),#64783) ;
#1374 = STYLED_ITEM('',(#126640),#64784) ;
#1375 = STYLED_ITEM('',(#126640),#64785) ;
#1376 = STYLED_ITEM('',(#126640),#64786) ;
#1377 = STYLED_ITEM('',(#126640),#64787) ;
#1378 = STYLED_ITEM('',(#126640),#64788) ;
#1379 = STYLED_ITEM('',(#126640),#64789) ;
#1380 = STYLED_ITEM('',(#126640),#64790) ;
#1381 = STYLED_ITEM('',(#126640),#64791) ;
#1382 = STYLED_ITEM('',(#126640),#64792) ;
#1383 = STYLED_ITEM('',(#126640),#64793) ;
#1384 = STYLED_ITEM('',(#126640),#64794) ;
#1385 = STYLED_ITEM('',(#126640),#64795) ;
#1386 = STYLED_ITEM('',(#126640),#64796) ;
#1387 = STYLED_ITEM('',(#126640),#64797) ;
#1388 = STYLED_ITEM('',(#126640),#64798) ;
#1389 = STYLED_ITEM('',(#126640),#64799) ;
#1390 = STYLED_ITEM('',(#126640),#64800) ;
#1391 = STYLED_ITEM('',(#126640),#64801) ;
#1392 = STYLED_ITEM('',(#126640),#64802) ;
#1393 = STYLED_ITEM('',(#126640),#64803) ;
#1394 = STYLED_ITEM('',(#126640),#64804) ;
#1395 = STYLED_ITEM('',(#126640),#64805) ;
#1396 = STYLED_ITEM('',(#126640),#64806) ;
#1397 = STYLED_ITEM('',(#126640),#64807) ;
#1398 = STYLED_ITEM('',(#126640),#64808) ;
#1399 = STYLED_ITEM('',(#126640),#64809) ;
#1400 = STYLED_ITEM('',(#126640),#64810) ;
#1401 = STYLED_ITEM('',(#126640),#64811) ;
#1402 = STYLED_ITEM('',(#126640),#64812) ;
#1403 = STYLED_ITEM('',(#126640),#64813) ;
#1404 = STYLED_ITEM('',(#126640),#64814) ;
#1405 = STYLED_ITEM('',(#126640),#64815) ;
#1406 = STYLED_ITEM('',(#126640),#64816) ;
#1407 = STYLED_ITEM('',(#126640),#64817) ;
#1408 = STYLED_ITEM('',(#126641),#64818) ;
#1409 = STYLED_ITEM('',(#126641),#64819) ;
#1410 = STYLED_ITEM('',(#126641),#64820) ;
#1411 = STYLED_ITEM('',(#126641),#64821) ;
#1412 = STYLED_ITEM('',(#126641),#64822) ;
#1413 = STYLED_ITEM('',(#126641),#64823) ;
#1414 = STYLED_ITEM('',(#126641),#64824) ;
#1415 = STYLED_ITEM('',(#126641),#64825) ;
#1416 = STYLED_ITEM('',(#126641),#64826) ;
#1417 = STYLED_ITEM('',(#126641),#64827) ;
#1418 = STYLED_ITEM('',(#126641),#64828) ;
#1419 = STYLED_ITEM('',(#126641),#64829) ;
#1420 = STYLED_ITEM('',(#126641),#64830) ;
#1421 = STYLED_ITEM('',(#126641),#64831) ;
#1422 = STYLED_ITEM('',(#126641),#64832) ;
#1423 = STYLED_ITEM('',(#126641),#64833) ;
#1424 = STYLED_ITEM('',(#126641),#64834) ;
#1425 = STYLED_ITEM('',(#126641),#64835) ;
#1426 = STYLED_ITEM('',(#126641),#64836) ;
#1427 = STYLED_ITEM('',(#126641),#64837) ;
#1428 = STYLED_ITEM('',(#126640),#64838) ;
#1429 = STYLED_ITEM('',(#126640),#64839) ;
#1430 = STYLED_ITEM('',(#126640),#64840) ;
#1431 = STYLED_ITEM('',(#126640),#64841) ;
#1432 = STYLED_ITEM('',(#126640),#64842) ;
#1433 = STYLED_ITEM('',(#126640),#64843) ;
#1434 = STYLED_ITEM('',(#126640),#64844) ;
#1435 = STYLED_ITEM('',(#126640),#64845) ;
#1436 = STYLED_ITEM('',(#126640),#64846) ;
#1437 = STYLED_ITEM('',(#126640),#64847) ;
#1438 = STYLED_ITEM('',(#126640),#64848) ;
#1439 = STYLED_ITEM('',(#126640),#64849) ;
#1440 = STYLED_ITEM('',(#126640),#64850) ;
#1441 = STYLED_ITEM('',(#126640),#64851) ;
#1442 = STYLED_ITEM('',(#126640),#64852) ;
#1443 = STYLED_ITEM('',(#126640),#64853) ;
#1444 = STYLED_ITEM('',(#126640),#64854) ;
#1445 = STYLED_ITEM('',(#126640),#64855) ;
#1446 = STYLED_ITEM('',(#126640),#64856) ;
#1447 = STYLED_ITEM('',(#126640),#64857) ;
#1448 = STYLED_ITEM('',(#126640),#64858) ;
#1449 = STYLED_ITEM('',(#126640),#64859) ;
#1450 = STYLED_ITEM('',(#126640),#64860) ;
#1451 = STYLED_ITEM('',(#126640),#64861) ;
#1452 = STYLED_ITEM('',(#126640),#64862) ;
#1453 = STYLED_ITEM('',(#126640),#64863) ;
#1454 = STYLED_ITEM('',(#126640),#64864) ;
#1455 = STYLED_ITEM('',(#126640),#64865) ;
#1456 = STYLED_ITEM('',(#126640),#64866) ;
#1457 = STYLED_ITEM('',(#126640),#64867) ;
#1458 = STYLED_ITEM('',(#126640),#64868) ;
#1459 = STYLED_ITEM('',(#126640),#64869) ;
#1460 = STYLED_ITEM('',(#126640),#64870) ;
#1461 = STYLED_ITEM('',(#126640),#64871) ;
#1462 = STYLED_ITEM('',(#126640),#64872) ;
#1463 = STYLED_ITEM('',(#126640),#64873) ;
#1464 = STYLED_ITEM('',(#126640),#64874) ;
#1465 = STYLED_ITEM('',(#126640),#64875) ;
#1466 = STYLED_ITEM('',(#126640),#64876) ;
#1467 = STYLED_ITEM('',(#126640),#64877) ;
#1468 = STYLED_ITEM('',(#126640),#64878) ;
#1469 = STYLED_ITEM('',(#126640),#64879) ;
#1470 = STYLED_ITEM('',(#126640),#64880) ;
#1471 = STYLED_ITEM('',(#126640),#64881) ;
#1472 = STYLED_ITEM('',(#126640),#64882) ;
#1473 = STYLED_ITEM('',(#126640),#64883) ;
#1474 = STYLED_ITEM('',(#126640),#64884) ;
#1475 = STYLED_ITEM('',(#126640),#64885) ;
#1476 = STYLED_ITEM('',(#126640),#64886) ;
#1477 = STYLED_ITEM('',(#126640),#64887) ;
#1478 = STYLED_ITEM('',(#126640),#64888) ;
#1479 = STYLED_ITEM('',(#126640),#64889) ;
#1480 = STYLED_ITEM('',(#126640),#64890) ;
#1481 = STYLED_ITEM('',(#126640),#64891) ;
#1482 = STYLED_ITEM('',(#126640),#64892) ;
#1483 = STYLED_ITEM('',(#126640),#64893) ;
#1484 = STYLED_ITEM('',(#126640),#64894) ;
#1485 = STYLED_ITEM('',(#126640),#64895) ;
#1486 = STYLED_ITEM('',(#126640),#64896) ;
#1487 = STYLED_ITEM('',(#126640),#64897) ;
#1488 = STYLED_ITEM('',(#126640),#64898) ;
#1489 = STYLED_ITEM('',(#126640),#64899) ;
#1490 = STYLED_ITEM('',(#126640),#64900) ;
#1491 = STYLED_ITEM('',(#126640),#64901) ;
#1492 = STYLED_ITEM('',(#126640),#64902) ;
#1493 = STYLED_ITEM('',(#126640),#64903) ;
#1494 = STYLED_ITEM('',(#126640),#64904) ;
#1495 = STYLED_ITEM('',(#126640),#64905) ;
#1496 = STYLED_ITEM('',(#126640),#64906) ;
#1497 = STYLED_ITEM('',(#126640),#64907) ;
#1498 = STYLED_ITEM('',(#126640),#64908) ;
#1499 = STYLED_ITEM('',(#126640),#64909) ;
#1500 = STYLED_ITEM('',(#126640),#64910) ;
#1501 = STYLED_ITEM('',(#126640),#64911) ;
#1502 = STYLED_ITEM('',(#126640),#64912) ;
#1503 = STYLED_ITEM('',(#126640),#64913) ;
#1504 = STYLED_ITEM('',(#126640),#64914) ;
#1505 = STYLED_ITEM('',(#126640),#64915) ;
#1506 = STYLED_ITEM('',(#126640),#64916) ;
#1507 = STYLED_ITEM('',(#126640),#64917) ;
#1508 = STYLED_ITEM('',(#126640),#64918) ;
#1509 = STYLED_ITEM('',(#126640),#64919) ;
#1510 = STYLED_ITEM('',(#126640),#64920) ;
#1511 = STYLED_ITEM('',(#126640),#64921) ;
#1512 = STYLED_ITEM('',(#126640),#64922) ;
#1513 = STYLED_ITEM('',(#126640),#64923) ;
#1514 = STYLED_ITEM('',(#126640),#64924) ;
#1515 = STYLED_ITEM('',(#126640),#64925) ;
#1516 = STYLED_ITEM('',(#126640),#64926) ;
#1517 = STYLED_ITEM('',(#126640),#64927) ;
#1518 = STYLED_ITEM('',(#126640),#64928) ;
#1519 = STYLED_ITEM('',(#126640),#64929) ;
#1520 = STYLED_ITEM('',(#126640),#64930) ;
#1521 = STYLED_ITEM('',(#126640),#64931) ;
#1522 = STYLED_ITEM('',(#126640),#64932) ;
#1523 = STYLED_ITEM('',(#126640),#64933) ;
#1524 = STYLED_ITEM('',(#126640),#64934) ;
#1525 = STYLED_ITEM('',(#126640),#64935) ;
#1526 = STYLED_ITEM('',(#126640),#64936) ;
#1527 = STYLED_ITEM('',(#126640),#64937) ;
#1528 = STYLED_ITEM('',(#126640),#64938) ;
#1529 = STYLED_ITEM('',(#126640),#64939) ;
#1530 = STYLED_ITEM('',(#126640),#64940) ;
#1531 = STYLED_ITEM('',(#126640),#64941) ;
#1532 = STYLED_ITEM('',(#126640),#64942) ;
#1533 = STYLED_ITEM('',(#126641),#64943) ;
#1534 = STYLED_ITEM('',(#126641),#64944) ;
#1535 = STYLED_ITEM('',(#126641),#64945) ;
#1536 = STYLED_ITEM('',(#126641),#64946) ;
#1537 = STYLED_ITEM('',(#126641),#64947) ;
#1538 = STYLED_ITEM('',(#126641),#64948) ;
#1539 = STYLED_ITEM('',(#126640),#64949) ;
#1540 = STYLED_ITEM('',(#126641),#64950) ;
#1541 = STYLED_ITEM('',(#126641),#64951) ;
#1542 = STYLED_ITEM('',(#126641),#64952) ;
#1543 = STYLED_ITEM('',(#126641),#64953) ;
#1544 = STYLED_ITEM('',(#126641),#64954) ;
#1545 = STYLED_ITEM('',(#126640),#64955) ;
#1546 = STYLED_ITEM('',(#126640),#64956) ;
#1547 = STYLED_ITEM('',(#126641),#64957) ;
#1548 = STYLED_ITEM('',(#126641),#64958) ;
#1549 = STYLED_ITEM('',(#126640),#64959) ;
#1550 = STYLED_ITEM('',(#126641),#64960) ;
#1551 = STYLED_ITEM('',(#126641),#64961) ;
#1552 = STYLED_ITEM('',(#126641),#64962) ;
#1553 = STYLED_ITEM('',(#126641),#64963) ;
#1554 = STYLED_ITEM('',(#126641),#64964) ;
#1555 = STYLED_ITEM('',(#126641),#64965) ;
#1556 = STYLED_ITEM('',(#126641),#64966) ;
#1557 = STYLED_ITEM('',(#126641),#64967) ;
#1558 = STYLED_ITEM('',(#126640),#64968) ;
#1559 = STYLED_ITEM('',(#126641),#64969) ;
#1560 = STYLED_ITEM('',(#126641),#64970) ;
#1561 = STYLED_ITEM('',(#126640),#64971) ;
#1562 = STYLED_ITEM('',(#126641),#64972) ;
#1563 = STYLED_ITEM('',(#126641),#64973) ;
#1564 = STYLED_ITEM('',(#126641),#64974) ;
#1565 = STYLED_ITEM('',(#126641),#64975) ;
#1566 = STYLED_ITEM('',(#126640),#64976) ;
#1567 = STYLED_ITEM('',(#126640),#64977) ;
#1568 = STYLED_ITEM('',(#126641),#64978) ;
#1569 = STYLED_ITEM('',(#126640),#64979) ;
#1570 = STYLED_ITEM('',(#126640),#64980) ;
#1571 = STYLED_ITEM('',(#126640),#64981) ;
#1572 = STYLED_ITEM('',(#126640),#64982) ;
#1573 = STYLED_ITEM('',(#126640),#64983) ;
#1574 = STYLED_ITEM('',(#126640),#64984) ;
#1575 = STYLED_ITEM('',(#126640),#64985) ;
#1576 = STYLED_ITEM('',(#126640),#64986) ;
#1577 = STYLED_ITEM('',(#126640),#64987) ;
#1578 = STYLED_ITEM('',(#126640),#64988) ;
#1579 = STYLED_ITEM('',(#126640),#64989) ;
#1580 = STYLED_ITEM('',(#126640),#64990) ;
#1581 = STYLED_ITEM('',(#126640),#64991) ;
#1582 = STYLED_ITEM('',(#126640),#64992) ;
#1583 = STYLED_ITEM('',(#126640),#64993) ;
#1584 = STYLED_ITEM('',(#126640),#64994) ;
#1585 = STYLED_ITEM('',(#126640),#64995) ;
#1586 = STYLED_ITEM('',(#126640),#64996) ;
#1587 = STYLED_ITEM('',(#126640),#64997) ;
#1588 = STYLED_ITEM('',(#126640),#64998) ;
#1589 = STYLED_ITEM('',(#126640),#64999) ;
#1590 = STYLED_ITEM('',(#126640),#65000) ;
#1591 = STYLED_ITEM('',(#126640),#65001) ;
#1592 = STYLED_ITEM('',(#126640),#65002) ;
#1593 = STYLED_ITEM('',(#126640),#65003) ;
#1594 = STYLED_ITEM('',(#126640),#65004) ;
#1595 = STYLED_ITEM('',(#126640),#65005) ;
#1596 = STYLED_ITEM('',(#126640),#65006) ;
#1597 = STYLED_ITEM('',(#126640),#65007) ;
#1598 = STYLED_ITEM('',(#126640),#65008) ;
#1599 = STYLED_ITEM('',(#126640),#65009) ;
#1600 = STYLED_ITEM('',(#126640),#65010) ;
#1601 = STYLED_ITEM('',(#126640),#65011) ;
#1602 = STYLED_ITEM('',(#126640),#65012) ;
#1603 = STYLED_ITEM('',(#126640),#65013) ;
#1604 = STYLED_ITEM('',(#126640),#65014) ;
#1605 = STYLED_ITEM('',(#126640),#65015) ;
#1606 = STYLED_ITEM('',(#126640),#65016) ;
#1607 = STYLED_ITEM('',(#126640),#65017) ;
#1608 = STYLED_ITEM('',(#126640),#65018) ;
#1609 = STYLED_ITEM('',(#126640),#65019) ;
#1610 = STYLED_ITEM('',(#126640),#65020) ;
#1611 = STYLED_ITEM('',(#126640),#65021) ;
#1612 = STYLED_ITEM('',(#126640),#65022) ;
#1613 = STYLED_ITEM('',(#126640),#65023) ;
#1614 = STYLED_ITEM('',(#126640),#65024) ;
#1615 = STYLED_ITEM('',(#126640),#65025) ;
#1616 = STYLED_ITEM('',(#126641),#65026) ;
#1617 = STYLED_ITEM('',(#126641),#65027) ;
#1618 = STYLED_ITEM('',(#126641),#65028) ;
#1619 = STYLED_ITEM('',(#126641),#65029) ;
#1620 = STYLED_ITEM('',(#126641),#65030) ;
#1621 = STYLED_ITEM('',(#126641),#65031) ;
#1622 = STYLED_ITEM('',(#126641),#65032) ;
#1623 = STYLED_ITEM('',(#126641),#65033) ;
#1624 = STYLED_ITEM('',(#126641),#65034) ;
#1625 = STYLED_ITEM('',(#126641),#65035) ;
#1626 = STYLED_ITEM('',(#126641),#65036) ;
#1627 = STYLED_ITEM('',(#126641),#65037) ;
#1628 = STYLED_ITEM('',(#126641),#65038) ;
#1629 = STYLED_ITEM('',(#126641),#65039) ;
#1630 = STYLED_ITEM('',(#126641),#65040) ;
#1631 = STYLED_ITEM('',(#126641),#65041) ;
#1632 = STYLED_ITEM('',(#126640),#65042) ;
#1633 = STYLED_ITEM('',(#126640),#65043) ;
#1634 = STYLED_ITEM('',(#126640),#65044) ;
#1635 = STYLED_ITEM('',(#126640),#65045) ;
#1636 = STYLED_ITEM('',(#126640),#65046) ;
#1637 = STYLED_ITEM('',(#126640),#65047) ;
#1638 = STYLED_ITEM('',(#126640),#65048) ;
#1639 = STYLED_ITEM('',(#126640),#65049) ;
#1640 = STYLED_ITEM('',(#126640),#65050) ;
#1641 = STYLED_ITEM('',(#126639),#4176) ;
#1642 = STYLED_ITEM('',(#126640),#65051) ;
#1643 = STYLED_ITEM('',(#126640),#65052) ;
#1644 = STYLED_ITEM('',(#126640),#65053) ;
#1645 = STYLED_ITEM('',(#126640),#65054) ;
#1646 = STYLED_ITEM('',(#126640),#65055) ;
#1647 = STYLED_ITEM('',(#126640),#65056) ;
#1648 = STYLED_ITEM('',(#126640),#65057) ;
#1649 = STYLED_ITEM('',(#126640),#65058) ;
#1650 = STYLED_ITEM('',(#126640),#65059) ;
#1651 = STYLED_ITEM('',(#126640),#65060) ;
#1652 = STYLED_ITEM('',(#126640),#65061) ;
#1653 = STYLED_ITEM('',(#126640),#65062) ;
#1654 = STYLED_ITEM('',(#126640),#65063) ;
#1655 = STYLED_ITEM('',(#126640),#65064) ;
#1656 = STYLED_ITEM('',(#126640),#65065) ;
#1657 = STYLED_ITEM('',(#126640),#65066) ;
#1658 = STYLED_ITEM('',(#126640),#65067) ;
#1659 = STYLED_ITEM('',(#126640),#65068) ;
#1660 = STYLED_ITEM('',(#126640),#65069) ;
#1661 = STYLED_ITEM('',(#126640),#65070) ;
#1662 = STYLED_ITEM('',(#126640),#65071) ;
#1663 = STYLED_ITEM('',(#126640),#65072) ;
#1664 = STYLED_ITEM('',(#126640),#65073) ;
#1665 = STYLED_ITEM('',(#126640),#65074) ;
#1666 = STYLED_ITEM('',(#126640),#65075) ;
#1667 = STYLED_ITEM('',(#126640),#65076) ;
#1668 = STYLED_ITEM('',(#126640),#65077) ;
#1669 = STYLED_ITEM('',(#126640),#65078) ;
#1670 = STYLED_ITEM('',(#126640),#65079) ;
#1671 = STYLED_ITEM('',(#126640),#65080) ;
#1672 = STYLED_ITEM('',(#126640),#65081) ;
#1673 = STYLED_ITEM('',(#126640),#65082) ;
#1674 = STYLED_ITEM('',(#126640),#65083) ;
#1675 = STYLED_ITEM('',(#126640),#65084) ;
#1676 = STYLED_ITEM('',(#126640),#65085) ;
#1677 = STYLED_ITEM('',(#126640),#65086) ;
#1678 = STYLED_ITEM('',(#126640),#65087) ;
#1679 = STYLED_ITEM('',(#126640),#65088) ;
#1680 = STYLED_ITEM('',(#126640),#65089) ;
#1681 = STYLED_ITEM('',(#126640),#65090) ;
#1682 = STYLED_ITEM('',(#126640),#65091) ;
#1683 = STYLED_ITEM('',(#126640),#65092) ;
#1684 = STYLED_ITEM('',(#126640),#65093) ;
#1685 = STYLED_ITEM('',(#126640),#65094) ;
#1686 = STYLED_ITEM('',(#126640),#65095) ;
#1687 = STYLED_ITEM('',(#126640),#65096) ;
#1688 = STYLED_ITEM('',(#126640),#65097) ;
#1689 = STYLED_ITEM('',(#126640),#65098) ;
#1690 = STYLED_ITEM('',(#126640),#65099) ;
#1691 = STYLED_ITEM('',(#126640),#65100) ;
#1692 = STYLED_ITEM('',(#126640),#65101) ;
#1693 = STYLED_ITEM('',(#126640),#65102) ;
#1694 = STYLED_ITEM('',(#126640),#65103) ;
#1695 = STYLED_ITEM('',(#126640),#65104) ;
#1696 = STYLED_ITEM('',(#126640),#65105) ;
#1697 = STYLED_ITEM('',(#126640),#65106) ;
#1698 = STYLED_ITEM('',(#126641),#65107) ;
#1699 = STYLED_ITEM('',(#126641),#65108) ;
#1700 = STYLED_ITEM('',(#126641),#65109) ;
#1701 = STYLED_ITEM('',(#126641),#65110) ;
#1702 = STYLED_ITEM('',(#126641),#65111) ;
#1703 = STYLED_ITEM('',(#126641),#65112) ;
#1704 = STYLED_ITEM('',(#126641),#65113) ;
#1705 = STYLED_ITEM('',(#126641),#65114) ;
#1706 = STYLED_ITEM('',(#126641),#65115) ;
#1707 = STYLED_ITEM('',(#126641),#65116) ;
#1708 = STYLED_ITEM('',(#126641),#65117) ;
#1709 = STYLED_ITEM('',(#126641),#65118) ;
#1710 = STYLED_ITEM('',(#126641),#65119) ;
#1711 = STYLED_ITEM('',(#126641),#65120) ;
#1712 = STYLED_ITEM('',(#126641),#65121) ;
#1713 = STYLED_ITEM('',(#126641),#65122) ;
#1714 = STYLED_ITEM('',(#126641),#65123) ;
#1715 = STYLED_ITEM('',(#126641),#65124) ;
#1716 = STYLED_ITEM('',(#126641),#65125) ;
#1717 = STYLED_ITEM('',(#126641),#65126) ;
#1718 = STYLED_ITEM('',(#126640),#65127) ;
#1719 = STYLED_ITEM('',(#126640),#65128) ;
#1720 = STYLED_ITEM('',(#126640),#65129) ;
#1721 = STYLED_ITEM('',(#126640),#65130) ;
#1722 = STYLED_ITEM('',(#126640),#65131) ;
#1723 = STYLED_ITEM('',(#126640),#65132) ;
#1724 = STYLED_ITEM('',(#126640),#65133) ;
#1725 = STYLED_ITEM('',(#126640),#65134) ;
#1726 = STYLED_ITEM('',(#126640),#65135) ;
#1727 = STYLED_ITEM('',(#126640),#65136) ;
#1728 = STYLED_ITEM('',(#126640),#65137) ;
#1729 = STYLED_ITEM('',(#126640),#65138) ;
#1730 = STYLED_ITEM('',(#126640),#65139) ;
#1731 = STYLED_ITEM('',(#126640),#65140) ;
#1732 = STYLED_ITEM('',(#126640),#65141) ;
#1733 = STYLED_ITEM('',(#126640),#65142) ;
#1734 = STYLED_ITEM('',(#126640),#65143) ;
#1735 = STYLED_ITEM('',(#126640),#65144) ;
#1736 = STYLED_ITEM('',(#126640),#65145) ;
#1737 = STYLED_ITEM('',(#126640),#65146) ;
#1738 = STYLED_ITEM('',(#126640),#65147) ;
#1739 = STYLED_ITEM('',(#126640),#65148) ;
#1740 = STYLED_ITEM('',(#126640),#65149) ;
#1741 = STYLED_ITEM('',(#126640),#65150) ;
#1742 = STYLED_ITEM('',(#126640),#65151) ;
#1743 = STYLED_ITEM('',(#126640),#65152) ;
#1744 = STYLED_ITEM('',(#126640),#65153) ;
#1745 = STYLED_ITEM('',(#126640),#65154) ;
#1746 = STYLED_ITEM('',(#126640),#65155) ;
#1747 = STYLED_ITEM('',(#126640),#65156) ;
#1748 = STYLED_ITEM('',(#126640),#65157) ;
#1749 = STYLED_ITEM('',(#126640),#65158) ;
#1750 = STYLED_ITEM('',(#126640),#65159) ;
#1751 = STYLED_ITEM('',(#126640),#65160) ;
#1752 = STYLED_ITEM('',(#126640),#65161) ;
#1753 = STYLED_ITEM('',(#126640),#65162) ;
#1754 = STYLED_ITEM('',(#126640),#65163) ;
#1755 = STYLED_ITEM('',(#126640),#65164) ;
#1756 = STYLED_ITEM('',(#126640),#65165) ;
#1757 = STYLED_ITEM('',(#126640),#65166) ;
#1758 = STYLED_ITEM('',(#126640),#65167) ;
#1759 = STYLED_ITEM('',(#126640),#65168) ;
#1760 = STYLED_ITEM('',(#126640),#65169) ;
#1761 = STYLED_ITEM('',(#126640),#65170) ;
#1762 = STYLED_ITEM('',(#126640),#65171) ;
#1763 = STYLED_ITEM('',(#126640),#65172) ;
#1764 = STYLED_ITEM('',(#126640),#65173) ;
#1765 = STYLED_ITEM('',(#126640),#65174) ;
#1766 = STYLED_ITEM('',(#126640),#65175) ;
#1767 = STYLED_ITEM('',(#126640),#65176) ;
#1768 = STYLED_ITEM('',(#126640),#65177) ;
#1769 = STYLED_ITEM('',(#126640),#65178) ;
#1770 = STYLED_ITEM('',(#126640),#65179) ;
#1771 = STYLED_ITEM('',(#126640),#65180) ;
#1772 = STYLED_ITEM('',(#126640),#65181) ;
#1773 = STYLED_ITEM('',(#126640),#65182) ;
#1774 = STYLED_ITEM('',(#126640),#65183) ;
#1775 = STYLED_ITEM('',(#126640),#65184) ;
#1776 = STYLED_ITEM('',(#126640),#65185) ;
#1777 = STYLED_ITEM('',(#126640),#65186) ;
#1778 = STYLED_ITEM('',(#126640),#65187) ;
#1779 = STYLED_ITEM('',(#126640),#65188) ;
#1780 = STYLED_ITEM('',(#126640),#65189) ;
#1781 = STYLED_ITEM('',(#126640),#65190) ;
#1782 = STYLED_ITEM('',(#126640),#65191) ;
#1783 = STYLED_ITEM('',(#126640),#65192) ;
#1784 = STYLED_ITEM('',(#126640),#65193) ;
#1785 = STYLED_ITEM('',(#126640),#65194) ;
#1786 = STYLED_ITEM('',(#126640),#65195) ;
#1787 = STYLED_ITEM('',(#126640),#65196) ;
#1788 = STYLED_ITEM('',(#126640),#65197) ;
#1789 = STYLED_ITEM('',(#126640),#65198) ;
#1790 = STYLED_ITEM('',(#126640),#65199) ;
#1791 = STYLED_ITEM('',(#126640),#65200) ;
#1792 = STYLED_ITEM('',(#126640),#65201) ;
#1793 = STYLED_ITEM('',(#126640),#65202) ;
#1794 = STYLED_ITEM('',(#126640),#65203) ;
#1795 = STYLED_ITEM('',(#126640),#65204) ;
#1796 = STYLED_ITEM('',(#126640),#65205) ;
#1797 = STYLED_ITEM('',(#126640),#65206) ;
#1798 = STYLED_ITEM('',(#126640),#65207) ;
#1799 = STYLED_ITEM('',(#126640),#65208) ;
#1800 = STYLED_ITEM('',(#126640),#65209) ;
#1801 = STYLED_ITEM('',(#126640),#65210) ;
#1802 = STYLED_ITEM('',(#126640),#65211) ;
#1803 = STYLED_ITEM('',(#126640),#65212) ;
#1804 = STYLED_ITEM('',(#126640),#65213) ;
#1805 = STYLED_ITEM('',(#126640),#65214) ;
#1806 = STYLED_ITEM('',(#126640),#65215) ;
#1807 = STYLED_ITEM('',(#126640),#65216) ;
#1808 = STYLED_ITEM('',(#126640),#65217) ;
#1809 = STYLED_ITEM('',(#126640),#65218) ;
#1810 = STYLED_ITEM('',(#126640),#65219) ;
#1811 = STYLED_ITEM('',(#126640),#65220) ;
#1812 = STYLED_ITEM('',(#126640),#65221) ;
#1813 = STYLED_ITEM('',(#126640),#65222) ;
#1814 = STYLED_ITEM('',(#126640),#65223) ;
#1815 = STYLED_ITEM('',(#126640),#65224) ;
#1816 = STYLED_ITEM('',(#126640),#65225) ;
#1817 = STYLED_ITEM('',(#126640),#65226) ;
#1818 = STYLED_ITEM('',(#126640),#65227) ;
#1819 = STYLED_ITEM('',(#126640),#65228) ;
#1820 = STYLED_ITEM('',(#126640),#65229) ;
#1821 = STYLED_ITEM('',(#126640),#65230) ;
#1822 = STYLED_ITEM('',(#126640),#65231) ;
#1823 = STYLED_ITEM('',(#126641),#65232) ;
#1824 = STYLED_ITEM('',(#126641),#65233) ;
#1825 = STYLED_ITEM('',(#126641),#65234) ;
#1826 = STYLED_ITEM('',(#126641),#65235) ;
#1827 = STYLED_ITEM('',(#126641),#65236) ;
#1828 = STYLED_ITEM('',(#126641),#65237) ;
#1829 = STYLED_ITEM('',(#126640),#65238) ;
#1830 = STYLED_ITEM('',(#126641),#65239) ;
#1831 = STYLED_ITEM('',(#126641),#65240) ;
#1832 = STYLED_ITEM('',(#126641),#65241) ;
#1833 = STYLED_ITEM('',(#126641),#65242) ;
#1834 = STYLED_ITEM('',(#126641),#65243) ;
#1835 = STYLED_ITEM('',(#126640),#65244) ;
#1836 = STYLED_ITEM('',(#126640),#65245) ;
#1837 = STYLED_ITEM('',(#126641),#65246) ;
#1838 = STYLED_ITEM('',(#126641),#65247) ;
#1839 = STYLED_ITEM('',(#126640),#65248) ;
#1840 = STYLED_ITEM('',(#126641),#65249) ;
#1841 = STYLED_ITEM('',(#126641),#65250) ;
#1842 = STYLED_ITEM('',(#126641),#65251) ;
#1843 = STYLED_ITEM('',(#126641),#65252) ;
#1844 = STYLED_ITEM('',(#126641),#65253) ;
#1845 = STYLED_ITEM('',(#126641),#65254) ;
#1846 = STYLED_ITEM('',(#126641),#65255) ;
#1847 = STYLED_ITEM('',(#126641),#65256) ;
#1848 = STYLED_ITEM('',(#126640),#65257) ;
#1849 = STYLED_ITEM('',(#126641),#65258) ;
#1850 = STYLED_ITEM('',(#126641),#65259) ;
#1851 = STYLED_ITEM('',(#126640),#65260) ;
#1852 = STYLED_ITEM('',(#126641),#65261) ;
#1853 = STYLED_ITEM('',(#126641),#65262) ;
#1854 = STYLED_ITEM('',(#126641),#65263) ;
#1855 = STYLED_ITEM('',(#126641),#65264) ;
#1856 = STYLED_ITEM('',(#126640),#65265) ;
#1857 = STYLED_ITEM('',(#126640),#65266) ;
#1858 = STYLED_ITEM('',(#126641),#65267) ;
#1859 = STYLED_ITEM('',(#126640),#65268) ;
#1860 = STYLED_ITEM('',(#126640),#65269) ;
#1861 = STYLED_ITEM('',(#126640),#65270) ;
#1862 = STYLED_ITEM('',(#126640),#65271) ;
#1863 = STYLED_ITEM('',(#126640),#65272) ;
#1864 = STYLED_ITEM('',(#126640),#65273) ;
#1865 = STYLED_ITEM('',(#126640),#65274) ;
#1866 = STYLED_ITEM('',(#126640),#65275) ;
#1867 = STYLED_ITEM('',(#126640),#65276) ;
#1868 = STYLED_ITEM('',(#126640),#65277) ;
#1869 = STYLED_ITEM('',(#126640),#65278) ;
#1870 = STYLED_ITEM('',(#126640),#65279) ;
#1871 = STYLED_ITEM('',(#126640),#65280) ;
#1872 = STYLED_ITEM('',(#126640),#65281) ;
#1873 = STYLED_ITEM('',(#126640),#65282) ;
#1874 = STYLED_ITEM('',(#126640),#65283) ;
#1875 = STYLED_ITEM('',(#126640),#65284) ;
#1876 = STYLED_ITEM('',(#126640),#65285) ;
#1877 = STYLED_ITEM('',(#126640),#65286) ;
#1878 = STYLED_ITEM('',(#126640),#65287) ;
#1879 = STYLED_ITEM('',(#126640),#65288) ;
#1880 = STYLED_ITEM('',(#126640),#65289) ;
#1881 = STYLED_ITEM('',(#126640),#65290) ;
#1882 = STYLED_ITEM('',(#126640),#65291) ;
#1883 = STYLED_ITEM('',(#126640),#65292) ;
#1884 = STYLED_ITEM('',(#126640),#65293) ;
#1885 = STYLED_ITEM('',(#126640),#65294) ;
#1886 = STYLED_ITEM('',(#126640),#65295) ;
#1887 = STYLED_ITEM('',(#126640),#65296) ;
#1888 = STYLED_ITEM('',(#126640),#65297) ;
#1889 = STYLED_ITEM('',(#126640),#65298) ;
#1890 = STYLED_ITEM('',(#126640),#65299) ;
#1891 = STYLED_ITEM('',(#126640),#65300) ;
#1892 = STYLED_ITEM('',(#126640),#65301) ;
#1893 = STYLED_ITEM('',(#126640),#65302) ;
#1894 = STYLED_ITEM('',(#126640),#65303) ;
#1895 = STYLED_ITEM('',(#126640),#65304) ;
#1896 = STYLED_ITEM('',(#126640),#65305) ;
#1897 = STYLED_ITEM('',(#126640),#65306) ;
#1898 = STYLED_ITEM('',(#126640),#65307) ;
#1899 = STYLED_ITEM('',(#126640),#65308) ;
#1900 = STYLED_ITEM('',(#126640),#65309) ;
#1901 = STYLED_ITEM('',(#126640),#65310) ;
#1902 = STYLED_ITEM('',(#126640),#65311) ;
#1903 = STYLED_ITEM('',(#126640),#65312) ;
#1904 = STYLED_ITEM('',(#126640),#65313) ;
#1905 = STYLED_ITEM('',(#126640),#65314) ;
#1906 = STYLED_ITEM('',(#126641),#65315) ;
#1907 = STYLED_ITEM('',(#126641),#65316) ;
#1908 = STYLED_ITEM('',(#126641),#65317) ;
#1909 = STYLED_ITEM('',(#126641),#65318) ;
#1910 = STYLED_ITEM('',(#126641),#65319) ;
#1911 = STYLED_ITEM('',(#126641),#65320) ;
#1912 = STYLED_ITEM('',(#126641),#65321) ;
#1913 = STYLED_ITEM('',(#126641),#65322) ;
#1914 = STYLED_ITEM('',(#126641),#65323) ;
#1915 = STYLED_ITEM('',(#126641),#65324) ;
#1916 = STYLED_ITEM('',(#126641),#65325) ;
#1917 = STYLED_ITEM('',(#126641),#65326) ;
#1918 = STYLED_ITEM('',(#126641),#65327) ;
#1919 = STYLED_ITEM('',(#126641),#65328) ;
#1920 = STYLED_ITEM('',(#126641),#65329) ;
#1921 = STYLED_ITEM('',(#126641),#65330) ;
#1922 = STYLED_ITEM('',(#126640),#65331) ;
#1923 = STYLED_ITEM('',(#126640),#65332) ;
#1924 = STYLED_ITEM('',(#126640),#65333) ;
#1925 = STYLED_ITEM('',(#126640),#65334) ;
#1926 = STYLED_ITEM('',(#126640),#65335) ;
#1927 = STYLED_ITEM('',(#126640),#65336) ;
#1928 = STYLED_ITEM('',(#126640),#65337) ;
#1929 = STYLED_ITEM('',(#126640),#65338) ;
#1930 = STYLED_ITEM('',(#126640),#65339) ;
#1931 = STYLED_ITEM('',(#126639),#4177) ;
#1932 = STYLED_ITEM('',(#126643),#65340) ;
#1933 = STYLED_ITEM('',(#126643),#65341) ;
#1934 = STYLED_ITEM('',(#126643),#65356) ;
#1935 = STYLED_ITEM('',(#126643),#65357) ;
#1936 = STYLED_ITEM('',(#126643),#65358) ;
#1937 = STYLED_ITEM('',(#126643),#65359) ;
#1938 = STYLED_ITEM('',(#126642),#4178) ;
#1939 = STYLED_ITEM('',(#126640),#65362) ;
#1940 = STYLED_ITEM('',(#126640),#65363) ;
#1941 = STYLED_ITEM('',(#126640),#65364) ;
#1942 = STYLED_ITEM('',(#126640),#65365) ;
#1943 = STYLED_ITEM('',(#126640),#65366) ;
#1944 = STYLED_ITEM('',(#126640),#65367) ;
#1945 = STYLED_ITEM('',(#126640),#65368) ;
#1946 = STYLED_ITEM('',(#126640),#65369) ;
#1947 = STYLED_ITEM('',(#126640),#65370) ;
#1948 = STYLED_ITEM('',(#126640),#65371) ;
#1949 = STYLED_ITEM('',(#126640),#65372) ;
#1950 = STYLED_ITEM('',(#126640),#65373) ;
#1951 = STYLED_ITEM('',(#126640),#65374) ;
#1952 = STYLED_ITEM('',(#126640),#65375) ;
#1953 = STYLED_ITEM('',(#126640),#65376) ;
#1954 = STYLED_ITEM('',(#126640),#65377) ;
#1955 = STYLED_ITEM('',(#126640),#65378) ;
#1956 = STYLED_ITEM('',(#126640),#65379) ;
#1957 = STYLED_ITEM('',(#126640),#65380) ;
#1958 = STYLED_ITEM('',(#126640),#65381) ;
#1959 = STYLED_ITEM('',(#126640),#65382) ;
#1960 = STYLED_ITEM('',(#126640),#65383) ;
#1961 = STYLED_ITEM('',(#126640),#65384) ;
#1962 = STYLED_ITEM('',(#126640),#65385) ;
#1963 = STYLED_ITEM('',(#126640),#65386) ;
#1964 = STYLED_ITEM('',(#126640),#65387) ;
#1965 = STYLED_ITEM('',(#126640),#65388) ;
#1966 = STYLED_ITEM('',(#126640),#65389) ;
#1967 = STYLED_ITEM('',(#126640),#65390) ;
#1968 = STYLED_ITEM('',(#126640),#65391) ;
#1969 = STYLED_ITEM('',(#126640),#65392) ;
#1970 = STYLED_ITEM('',(#126640),#65393) ;
#1971 = STYLED_ITEM('',(#126640),#65394) ;
#1972 = STYLED_ITEM('',(#126640),#65395) ;
#1973 = STYLED_ITEM('',(#126640),#65396) ;
#1974 = STYLED_ITEM('',(#126640),#65397) ;
#1975 = STYLED_ITEM('',(#126640),#65398) ;
#1976 = STYLED_ITEM('',(#126640),#65399) ;
#1977 = STYLED_ITEM('',(#126640),#65400) ;
#1978 = STYLED_ITEM('',(#126640),#65401) ;
#1979 = STYLED_ITEM('',(#126640),#65402) ;
#1980 = STYLED_ITEM('',(#126640),#65403) ;
#1981 = STYLED_ITEM('',(#126640),#65404) ;
#1982 = STYLED_ITEM('',(#126640),#65405) ;
#1983 = STYLED_ITEM('',(#126640),#65406) ;
#1984 = STYLED_ITEM('',(#126640),#65407) ;
#1985 = STYLED_ITEM('',(#126640),#65408) ;
#1986 = STYLED_ITEM('',(#126640),#65409) ;
#1987 = STYLED_ITEM('',(#126640),#65410) ;
#1988 = STYLED_ITEM('',(#126640),#65411) ;
#1989 = STYLED_ITEM('',(#126640),#65412) ;
#1990 = STYLED_ITEM('',(#126640),#65413) ;
#1991 = STYLED_ITEM('',(#126640),#65414) ;
#1992 = STYLED_ITEM('',(#126640),#65415) ;
#1993 = STYLED_ITEM('',(#126640),#65416) ;
#1994 = STYLED_ITEM('',(#126640),#65417) ;
#1995 = STYLED_ITEM('',(#126640),#65418) ;
#1996 = STYLED_ITEM('',(#126640),#65419) ;
#1997 = STYLED_ITEM('',(#126640),#65420) ;
#1998 = STYLED_ITEM('',(#126640),#65421) ;
#1999 = STYLED_ITEM('',(#126640),#65422) ;
#2000 = STYLED_ITEM('',(#126640),#65423) ;
#2001 = STYLED_ITEM('',(#126640),#65424) ;
#2002 = STYLED_ITEM('',(#126640),#65425) ;
#2003 = STYLED_ITEM('',(#126640),#65426) ;
#2004 = STYLED_ITEM('',(#126640),#65427) ;
#2005 = STYLED_ITEM('',(#126640),#65428) ;
#2006 = STYLED_ITEM('',(#126640),#65429) ;
#2007 = STYLED_ITEM('',(#126640),#65430) ;
#2008 = STYLED_ITEM('',(#126640),#65431) ;
#2009 = STYLED_ITEM('',(#126640),#65432) ;
#2010 = STYLED_ITEM('',(#126640),#65433) ;
#2011 = STYLED_ITEM('',(#126640),#65434) ;
#2012 = STYLED_ITEM('',(#126640),#65435) ;
#2013 = STYLED_ITEM('',(#126640),#65436) ;
#2014 = STYLED_ITEM('',(#126640),#65437) ;
#2015 = STYLED_ITEM('',(#126640),#65438) ;
#2016 = STYLED_ITEM('',(#126640),#65439) ;
#2017 = STYLED_ITEM('',(#126640),#65440) ;
#2018 = STYLED_ITEM('',(#126640),#65441) ;
#2019 = STYLED_ITEM('',(#126640),#65442) ;
#2020 = STYLED_ITEM('',(#126640),#65443) ;
#2021 = STYLED_ITEM('',(#126640),#65444) ;
#2022 = STYLED_ITEM('',(#126640),#65445) ;
#2023 = STYLED_ITEM('',(#126640),#65446) ;
#2024 = STYLED_ITEM('',(#126640),#65447) ;
#2025 = STYLED_ITEM('',(#126640),#65448) ;
#2026 = STYLED_ITEM('',(#126640),#65449) ;
#2027 = STYLED_ITEM('',(#126640),#65450) ;
#2028 = STYLED_ITEM('',(#126640),#65451) ;
#2029 = STYLED_ITEM('',(#126640),#65452) ;
#2030 = STYLED_ITEM('',(#126640),#65453) ;
#2031 = STYLED_ITEM('',(#126640),#65454) ;
#2032 = STYLED_ITEM('',(#126640),#65455) ;
#2033 = STYLED_ITEM('',(#126640),#65456) ;
#2034 = STYLED_ITEM('',(#126640),#65457) ;
#2035 = STYLED_ITEM('',(#126640),#65458) ;
#2036 = STYLED_ITEM('',(#126640),#65459) ;
#2037 = STYLED_ITEM('',(#126640),#65460) ;
#2038 = STYLED_ITEM('',(#126640),#65461) ;
#2039 = STYLED_ITEM('',(#126640),#65462) ;
#2040 = STYLED_ITEM('',(#126640),#65463) ;
#2041 = STYLED_ITEM('',(#126640),#65464) ;
#2042 = STYLED_ITEM('',(#126640),#65465) ;
#2043 = STYLED_ITEM('',(#126640),#65466) ;
#2044 = STYLED_ITEM('',(#126640),#65467) ;
#2045 = STYLED_ITEM('',(#126640),#65468) ;
#2046 = STYLED_ITEM('',(#126640),#65469) ;
#2047 = STYLED_ITEM('',(#126640),#65470) ;
#2048 = STYLED_ITEM('',(#126640),#65471) ;
#2049 = STYLED_ITEM('',(#126640),#65472) ;
#2050 = STYLED_ITEM('',(#126640),#65473) ;
#2051 = STYLED_ITEM('',(#126640),#65474) ;
#2052 = STYLED_ITEM('',(#126640),#65475) ;
#2053 = STYLED_ITEM('',(#126640),#65476) ;
#2054 = STYLED_ITEM('',(#126640),#65477) ;
#2055 = STYLED_ITEM('',(#126640),#65478) ;
#2056 = STYLED_ITEM('',(#126640),#65479) ;
#2057 = STYLED_ITEM('',(#126640),#65480) ;
#2058 = STYLED_ITEM('',(#126640),#65481) ;
#2059 = STYLED_ITEM('',(#126640),#65482) ;
#2060 = STYLED_ITEM('',(#126640),#65483) ;
#2061 = STYLED_ITEM('',(#126640),#65484) ;
#2062 = STYLED_ITEM('',(#126640),#65485) ;
#2063 = STYLED_ITEM('',(#126640),#65486) ;
#2064 = STYLED_ITEM('',(#126640),#65487) ;
#2065 = STYLED_ITEM('',(#126640),#65488) ;
#2066 = STYLED_ITEM('',(#126640),#65489) ;
#2067 = STYLED_ITEM('',(#126640),#65490) ;
#2068 = STYLED_ITEM('',(#126640),#65491) ;
#2069 = STYLED_ITEM('',(#126640),#65492) ;
#2070 = STYLED_ITEM('',(#126640),#65493) ;
#2071 = STYLED_ITEM('',(#126640),#65494) ;
#2072 = STYLED_ITEM('',(#126640),#65495) ;
#2073 = STYLED_ITEM('',(#126640),#65496) ;
#2074 = STYLED_ITEM('',(#126640),#65497) ;
#2075 = STYLED_ITEM('',(#126640),#65498) ;
#2076 = STYLED_ITEM('',(#126640),#65499) ;
#2077 = STYLED_ITEM('',(#126640),#65500) ;
#2078 = STYLED_ITEM('',(#126640),#65501) ;
#2079 = STYLED_ITEM('',(#126640),#65502) ;
#2080 = STYLED_ITEM('',(#126640),#65503) ;
#2081 = STYLED_ITEM('',(#126640),#65504) ;
#2082 = STYLED_ITEM('',(#126640),#65505) ;
#2083 = STYLED_ITEM('',(#126640),#65506) ;
#2084 = STYLED_ITEM('',(#126640),#65507) ;
#2085 = STYLED_ITEM('',(#126640),#65508) ;
#2086 = STYLED_ITEM('',(#126640),#65509) ;
#2087 = STYLED_ITEM('',(#126640),#65510) ;
#2088 = STYLED_ITEM('',(#126640),#65511) ;
#2089 = STYLED_ITEM('',(#126640),#65512) ;
#2090 = STYLED_ITEM('',(#126640),#65513) ;
#2091 = STYLED_ITEM('',(#126640),#65514) ;
#2092 = STYLED_ITEM('',(#126640),#65515) ;
#2093 = STYLED_ITEM('',(#126640),#65516) ;
#2094 = STYLED_ITEM('',(#126640),#65517) ;
#2095 = STYLED_ITEM('',(#126640),#65518) ;
#2096 = STYLED_ITEM('',(#126640),#65519) ;
#2097 = STYLED_ITEM('',(#126640),#65520) ;
#2098 = STYLED_ITEM('',(#126640),#65521) ;
#2099 = STYLED_ITEM('',(#126640),#65522) ;
#2100 = STYLED_ITEM('',(#126640),#65523) ;
#2101 = STYLED_ITEM('',(#126640),#65524) ;
#2102 = STYLED_ITEM('',(#126640),#65525) ;
#2103 = STYLED_ITEM('',(#126640),#65526) ;
#2104 = STYLED_ITEM('',(#126640),#65527) ;
#2105 = STYLED_ITEM('',(#126640),#65528) ;
#2106 = STYLED_ITEM('',(#126640),#65529) ;
#2107 = STYLED_ITEM('',(#126640),#65530) ;
#2108 = STYLED_ITEM('',(#126640),#65531) ;
#2109 = STYLED_ITEM('',(#126640),#65532) ;
#2110 = STYLED_ITEM('',(#126640),#65533) ;
#2111 = STYLED_ITEM('',(#126640),#65534) ;
#2112 = STYLED_ITEM('',(#126640),#65535) ;
#2113 = STYLED_ITEM('',(#126640),#65536) ;
#2114 = STYLED_ITEM('',(#126640),#65537) ;
#2115 = STYLED_ITEM('',(#126640),#65538) ;
#2116 = STYLED_ITEM('',(#126640),#65539) ;
#2117 = STYLED_ITEM('',(#126640),#65540) ;
#2118 = STYLED_ITEM('',(#126640),#65541) ;
#2119 = STYLED_ITEM('',(#126640),#65542) ;
#2120 = STYLED_ITEM('',(#126640),#65543) ;
#2121 = STYLED_ITEM('',(#126640),#65544) ;
#2122 = STYLED_ITEM('',(#126640),#65545) ;
#2123 = STYLED_ITEM('',(#126640),#65546) ;
#2124 = STYLED_ITEM('',(#126640),#65547) ;
#2125 = STYLED_ITEM('',(#126640),#65548) ;
#2126 = STYLED_ITEM('',(#126640),#65549) ;
#2127 = STYLED_ITEM('',(#126640),#65550) ;
#2128 = STYLED_ITEM('',(#126640),#65551) ;
#2129 = STYLED_ITEM('',(#126640),#65552) ;
#2130 = STYLED_ITEM('',(#126640),#65553) ;
#2131 = STYLED_ITEM('',(#126640),#65554) ;
#2132 = STYLED_ITEM('',(#126640),#65555) ;
#2133 = STYLED_ITEM('',(#126640),#65556) ;
#2134 = STYLED_ITEM('',(#126640),#65557) ;
#2135 = STYLED_ITEM('',(#126640),#65558) ;
#2136 = STYLED_ITEM('',(#126640),#65559) ;
#2137 = STYLED_ITEM('',(#126640),#65560) ;
#2138 = STYLED_ITEM('',(#126640),#65561) ;
#2139 = STYLED_ITEM('',(#126640),#65562) ;
#2140 = STYLED_ITEM('',(#126640),#65563) ;
#2141 = STYLED_ITEM('',(#126640),#65564) ;
#2142 = STYLED_ITEM('',(#126640),#65565) ;
#2143 = STYLED_ITEM('',(#126640),#65566) ;
#2144 = STYLED_ITEM('',(#126640),#65567) ;
#2145 = STYLED_ITEM('',(#126640),#65568) ;
#2146 = STYLED_ITEM('',(#126640),#65569) ;
#2147 = STYLED_ITEM('',(#126640),#65570) ;
#2148 = STYLED_ITEM('',(#126640),#65571) ;
#2149 = STYLED_ITEM('',(#126640),#65572) ;
#2150 = STYLED_ITEM('',(#126640),#65573) ;
#2151 = STYLED_ITEM('',(#126640),#65574) ;
#2152 = STYLED_ITEM('',(#126640),#65575) ;
#2153 = STYLED_ITEM('',(#126640),#65576) ;
#2154 = STYLED_ITEM('',(#126640),#65577) ;
#2155 = STYLED_ITEM('',(#126640),#65578) ;
#2156 = STYLED_ITEM('',(#126640),#65579) ;
#2157 = STYLED_ITEM('',(#126640),#65580) ;
#2158 = STYLED_ITEM('',(#126640),#65581) ;
#2159 = STYLED_ITEM('',(#126640),#65582) ;
#2160 = STYLED_ITEM('',(#126640),#65583) ;
#2161 = STYLED_ITEM('',(#126640),#65584) ;
#2162 = STYLED_ITEM('',(#126640),#65585) ;
#2163 = STYLED_ITEM('',(#126640),#65586) ;
#2164 = STYLED_ITEM('',(#126640),#65587) ;
#2165 = STYLED_ITEM('',(#126640),#65588) ;
#2166 = STYLED_ITEM('',(#126640),#65589) ;
#2167 = STYLED_ITEM('',(#126640),#65590) ;
#2168 = STYLED_ITEM('',(#126640),#65591) ;
#2169 = STYLED_ITEM('',(#126640),#65592) ;
#2170 = STYLED_ITEM('',(#126640),#65593) ;
#2171 = STYLED_ITEM('',(#126640),#65594) ;
#2172 = STYLED_ITEM('',(#126640),#65595) ;
#2173 = STYLED_ITEM('',(#126640),#65596) ;
#2174 = STYLED_ITEM('',(#126640),#65597) ;
#2175 = STYLED_ITEM('',(#126640),#65598) ;
#2176 = STYLED_ITEM('',(#126640),#65599) ;
#2177 = STYLED_ITEM('',(#126640),#65600) ;
#2178 = STYLED_ITEM('',(#126640),#65601) ;
#2179 = STYLED_ITEM('',(#126640),#65602) ;
#2180 = STYLED_ITEM('',(#126640),#65603) ;
#2181 = STYLED_ITEM('',(#126640),#65604) ;
#2182 = STYLED_ITEM('',(#126640),#65605) ;
#2183 = STYLED_ITEM('',(#126640),#65606) ;
#2184 = STYLED_ITEM('',(#126640),#65607) ;
#2185 = STYLED_ITEM('',(#126640),#65608) ;
#2186 = STYLED_ITEM('',(#126640),#65609) ;
#2187 = STYLED_ITEM('',(#126640),#65610) ;
#2188 = STYLED_ITEM('',(#126640),#65611) ;
#2189 = STYLED_ITEM('',(#126640),#65612) ;
#2190 = STYLED_ITEM('',(#126640),#65613) ;
#2191 = STYLED_ITEM('',(#126640),#65614) ;
#2192 = STYLED_ITEM('',(#126640),#65615) ;
#2193 = STYLED_ITEM('',(#126640),#65616) ;
#2194 = STYLED_ITEM('',(#126640),#65617) ;
#2195 = STYLED_ITEM('',(#126640),#65618) ;
#2196 = STYLED_ITEM('',(#126640),#65619) ;
#2197 = STYLED_ITEM('',(#126640),#65620) ;
#2198 = STYLED_ITEM('',(#126640),#65621) ;
#2199 = STYLED_ITEM('',(#126640),#65622) ;
#2200 = STYLED_ITEM('',(#126640),#65623) ;
#2201 = STYLED_ITEM('',(#126640),#65624) ;
#2202 = STYLED_ITEM('',(#126640),#65625) ;
#2203 = STYLED_ITEM('',(#126640),#65626) ;
#2204 = STYLED_ITEM('',(#126640),#65627) ;
#2205 = STYLED_ITEM('',(#126640),#65628) ;
#2206 = STYLED_ITEM('',(#126640),#65629) ;
#2207 = STYLED_ITEM('',(#126640),#65630) ;
#2208 = STYLED_ITEM('',(#126640),#65631) ;
#2209 = STYLED_ITEM('',(#126640),#65632) ;
#2210 = STYLED_ITEM('',(#126640),#65633) ;
#2211 = STYLED_ITEM('',(#126640),#65634) ;
#2212 = STYLED_ITEM('',(#126640),#65635) ;
#2213 = STYLED_ITEM('',(#126640),#65636) ;
#2214 = STYLED_ITEM('',(#126640),#65637) ;
#2215 = STYLED_ITEM('',(#126640),#65638) ;
#2216 = STYLED_ITEM('',(#126640),#65639) ;
#2217 = STYLED_ITEM('',(#126640),#65640) ;
#2218 = STYLED_ITEM('',(#126640),#65641) ;
#2219 = STYLED_ITEM('',(#126640),#65642) ;
#2220 = STYLED_ITEM('',(#126640),#65643) ;
#2221 = STYLED_ITEM('',(#126640),#65644) ;
#2222 = STYLED_ITEM('',(#126640),#65645) ;
#2223 = STYLED_ITEM('',(#126640),#65646) ;
#2224 = STYLED_ITEM('',(#126640),#65647) ;
#2225 = STYLED_ITEM('',(#126640),#65648) ;
#2226 = STYLED_ITEM('',(#126640),#65649) ;
#2227 = STYLED_ITEM('',(#126640),#65650) ;
#2228 = STYLED_ITEM('',(#126640),#65651) ;
#2229 = STYLED_ITEM('',(#126640),#65652) ;
#2230 = STYLED_ITEM('',(#126640),#65653) ;
#2231 = STYLED_ITEM('',(#126640),#65654) ;
#2232 = STYLED_ITEM('',(#126640),#65655) ;
#2233 = STYLED_ITEM('',(#126640),#65656) ;
#2234 = STYLED_ITEM('',(#126641),#65657) ;
#2235 = STYLED_ITEM('',(#126641),#65658) ;
#2236 = STYLED_ITEM('',(#126641),#65659) ;
#2237 = STYLED_ITEM('',(#126641),#65660) ;
#2238 = STYLED_ITEM('',(#126641),#65661) ;
#2239 = STYLED_ITEM('',(#126641),#65662) ;
#2240 = STYLED_ITEM('',(#126641),#65663) ;
#2241 = STYLED_ITEM('',(#126641),#65664) ;
#2242 = STYLED_ITEM('',(#126641),#65665) ;
#2243 = STYLED_ITEM('',(#126641),#65666) ;
#2244 = STYLED_ITEM('',(#126641),#65667) ;
#2245 = STYLED_ITEM('',(#126641),#65668) ;
#2246 = STYLED_ITEM('',(#126641),#65669) ;
#2247 = STYLED_ITEM('',(#126641),#65670) ;
#2248 = STYLED_ITEM('',(#126641),#65671) ;
#2249 = STYLED_ITEM('',(#126641),#65672) ;
#2250 = STYLED_ITEM('',(#126641),#65673) ;
#2251 = STYLED_ITEM('',(#126641),#65674) ;
#2252 = STYLED_ITEM('',(#126641),#65675) ;
#2253 = STYLED_ITEM('',(#126641),#65676) ;
#2254 = STYLED_ITEM('',(#126641),#65677) ;
#2255 = STYLED_ITEM('',(#126641),#65678) ;
#2256 = STYLED_ITEM('',(#126641),#65679) ;
#2257 = STYLED_ITEM('',(#126641),#65680) ;
#2258 = STYLED_ITEM('',(#126641),#65681) ;
#2259 = STYLED_ITEM('',(#126641),#65682) ;
#2260 = STYLED_ITEM('',(#126641),#65683) ;
#2261 = STYLED_ITEM('',(#126641),#65684) ;
#2262 = STYLED_ITEM('',(#126641),#65685) ;
#2263 = STYLED_ITEM('',(#126641),#65686) ;
#2264 = STYLED_ITEM('',(#126641),#65687) ;
#2265 = STYLED_ITEM('',(#126641),#65688) ;
#2266 = STYLED_ITEM('',(#126641),#65689) ;
#2267 = STYLED_ITEM('',(#126641),#65690) ;
#2268 = STYLED_ITEM('',(#126641),#65691) ;
#2269 = STYLED_ITEM('',(#126641),#65692) ;
#2270 = STYLED_ITEM('',(#126641),#65693) ;
#2271 = STYLED_ITEM('',(#126641),#65694) ;
#2272 = STYLED_ITEM('',(#126641),#65695) ;
#2273 = STYLED_ITEM('',(#126641),#65696) ;
#2274 = STYLED_ITEM('',(#126641),#65697) ;
#2275 = STYLED_ITEM('',(#126641),#65698) ;
#2276 = STYLED_ITEM('',(#126641),#65699) ;
#2277 = STYLED_ITEM('',(#126641),#65700) ;
#2278 = STYLED_ITEM('',(#126641),#65701) ;
#2279 = STYLED_ITEM('',(#126641),#65702) ;
#2280 = STYLED_ITEM('',(#126641),#65703) ;
#2281 = STYLED_ITEM('',(#126641),#65704) ;
#2282 = STYLED_ITEM('',(#126641),#65705) ;
#2283 = STYLED_ITEM('',(#126641),#65706) ;
#2284 = STYLED_ITEM('',(#126641),#65707) ;
#2285 = STYLED_ITEM('',(#126641),#65708) ;
#2286 = STYLED_ITEM('',(#126641),#65709) ;
#2287 = STYLED_ITEM('',(#126641),#65710) ;
#2288 = STYLED_ITEM('',(#126641),#65711) ;
#2289 = STYLED_ITEM('',(#126641),#65712) ;
#2290 = STYLED_ITEM('',(#126641),#65713) ;
#2291 = STYLED_ITEM('',(#126641),#65714) ;
#2292 = STYLED_ITEM('',(#126641),#65715) ;
#2293 = STYLED_ITEM('',(#126641),#65716) ;
#2294 = STYLED_ITEM('',(#126641),#65717) ;
#2295 = STYLED_ITEM('',(#126641),#65718) ;
#2296 = STYLED_ITEM('',(#126641),#65719) ;
#2297 = STYLED_ITEM('',(#126641),#65720) ;
#2298 = STYLED_ITEM('',(#126641),#65721) ;
#2299 = STYLED_ITEM('',(#126641),#65722) ;
#2300 = STYLED_ITEM('',(#126641),#65723) ;
#2301 = STYLED_ITEM('',(#126641),#65724) ;
#2302 = STYLED_ITEM('',(#126641),#65725) ;
#2303 = STYLED_ITEM('',(#126641),#65726) ;
#2304 = STYLED_ITEM('',(#126641),#65727) ;
#2305 = STYLED_ITEM('',(#126641),#65728) ;
#2306 = STYLED_ITEM('',(#126640),#65729) ;
#2307 = STYLED_ITEM('',(#126640),#65730) ;
#2308 = STYLED_ITEM('',(#126640),#65731) ;
#2309 = STYLED_ITEM('',(#126640),#65732) ;
#2310 = STYLED_ITEM('',(#126640),#65733) ;
#2311 = STYLED_ITEM('',(#126640),#65734) ;
#2312 = STYLED_ITEM('',(#126640),#65735) ;
#2313 = STYLED_ITEM('',(#126640),#65736) ;
#2314 = STYLED_ITEM('',(#126640),#65737) ;
#2315 = STYLED_ITEM('',(#126640),#65738) ;
#2316 = STYLED_ITEM('',(#126640),#65739) ;
#2317 = STYLED_ITEM('',(#126640),#65740) ;
#2318 = STYLED_ITEM('',(#126640),#65741) ;
#2319 = STYLED_ITEM('',(#126640),#65742) ;
#2320 = STYLED_ITEM('',(#126640),#65743) ;
#2321 = STYLED_ITEM('',(#126640),#65744) ;
#2322 = STYLED_ITEM('',(#126640),#65745) ;
#2323 = STYLED_ITEM('',(#126640),#65746) ;
#2324 = STYLED_ITEM('',(#126640),#65747) ;
#2325 = STYLED_ITEM('',(#126640),#65748) ;
#2326 = STYLED_ITEM('',(#126640),#65749) ;
#2327 = STYLED_ITEM('',(#126640),#65750) ;
#2328 = STYLED_ITEM('',(#126640),#65751) ;
#2329 = STYLED_ITEM('',(#126640),#65752) ;
#2330 = STYLED_ITEM('',(#126640),#65753) ;
#2331 = STYLED_ITEM('',(#126640),#65754) ;
#2332 = STYLED_ITEM('',(#126640),#65755) ;
#2333 = STYLED_ITEM('',(#126640),#65756) ;
#2334 = STYLED_ITEM('',(#126640),#65757) ;
#2335 = STYLED_ITEM('',(#126640),#65758) ;
#2336 = STYLED_ITEM('',(#126640),#65759) ;
#2337 = STYLED_ITEM('',(#126640),#65760) ;
#2338 = STYLED_ITEM('',(#126640),#65761) ;
#2339 = STYLED_ITEM('',(#126640),#65762) ;
#2340 = STYLED_ITEM('',(#126640),#65763) ;
#2341 = STYLED_ITEM('',(#126640),#65764) ;
#2342 = STYLED_ITEM('',(#126640),#65765) ;
#2343 = STYLED_ITEM('',(#126640),#65766) ;
#2344 = STYLED_ITEM('',(#126640),#65767) ;
#2345 = STYLED_ITEM('',(#126640),#65768) ;
#2346 = STYLED_ITEM('',(#126640),#65769) ;
#2347 = STYLED_ITEM('',(#126640),#65770) ;
#2348 = STYLED_ITEM('',(#126640),#65771) ;
#2349 = STYLED_ITEM('',(#126640),#65772) ;
#2350 = STYLED_ITEM('',(#126640),#65773) ;
#2351 = STYLED_ITEM('',(#126640),#65774) ;
#2352 = STYLED_ITEM('',(#126640),#65775) ;
#2353 = STYLED_ITEM('',(#126640),#65776) ;
#2354 = STYLED_ITEM('',(#126640),#65777) ;
#2355 = STYLED_ITEM('',(#126640),#65778) ;
#2356 = STYLED_ITEM('',(#126640),#65779) ;
#2357 = STYLED_ITEM('',(#126640),#65780) ;
#2358 = STYLED_ITEM('',(#126640),#65781) ;
#2359 = STYLED_ITEM('',(#126640),#65782) ;
#2360 = STYLED_ITEM('',(#126640),#65783) ;
#2361 = STYLED_ITEM('',(#126640),#65784) ;
#2362 = STYLED_ITEM('',(#126640),#65785) ;
#2363 = STYLED_ITEM('',(#126640),#65786) ;
#2364 = STYLED_ITEM('',(#126640),#65787) ;
#2365 = STYLED_ITEM('',(#126640),#65788) ;
#2366 = STYLED_ITEM('',(#126640),#65789) ;
#2367 = STYLED_ITEM('',(#126640),#65790) ;
#2368 = STYLED_ITEM('',(#126640),#65791) ;
#2369 = STYLED_ITEM('',(#126640),#65792) ;
#2370 = STYLED_ITEM('',(#126640),#65793) ;
#2371 = STYLED_ITEM('',(#126640),#65794) ;
#2372 = STYLED_ITEM('',(#126640),#65795) ;
#2373 = STYLED_ITEM('',(#126640),#65796) ;
#2374 = STYLED_ITEM('',(#126640),#65797) ;
#2375 = STYLED_ITEM('',(#126640),#65798) ;
#2376 = STYLED_ITEM('',(#126640),#65799) ;
#2377 = STYLED_ITEM('',(#126640),#65800) ;
#2378 = STYLED_ITEM('',(#126640),#65801) ;
#2379 = STYLED_ITEM('',(#126640),#65802) ;
#2380 = STYLED_ITEM('',(#126640),#65803) ;
#2381 = STYLED_ITEM('',(#126640),#65804) ;
#2382 = STYLED_ITEM('',(#126640),#65805) ;
#2383 = STYLED_ITEM('',(#126640),#65806) ;
#2384 = STYLED_ITEM('',(#126640),#65807) ;
#2385 = STYLED_ITEM('',(#126640),#65808) ;
#2386 = STYLED_ITEM('',(#126640),#65809) ;
#2387 = STYLED_ITEM('',(#126640),#65810) ;
#2388 = STYLED_ITEM('',(#126640),#65811) ;
#2389 = STYLED_ITEM('',(#126640),#65812) ;
#2390 = STYLED_ITEM('',(#126640),#65813) ;
#2391 = STYLED_ITEM('',(#126640),#65814) ;
#2392 = STYLED_ITEM('',(#126640),#65815) ;
#2393 = STYLED_ITEM('',(#126640),#65816) ;
#2394 = STYLED_ITEM('',(#126640),#65817) ;
#2395 = STYLED_ITEM('',(#126640),#65818) ;
#2396 = STYLED_ITEM('',(#126640),#65819) ;
#2397 = STYLED_ITEM('',(#126640),#65820) ;
#2398 = STYLED_ITEM('',(#126640),#65821) ;
#2399 = STYLED_ITEM('',(#126640),#65822) ;
#2400 = STYLED_ITEM('',(#126640),#65823) ;
#2401 = STYLED_ITEM('',(#126640),#65824) ;
#2402 = STYLED_ITEM('',(#126640),#65825) ;
#2403 = STYLED_ITEM('',(#126640),#65826) ;
#2404 = STYLED_ITEM('',(#126640),#65827) ;
#2405 = STYLED_ITEM('',(#126640),#65828) ;
#2406 = STYLED_ITEM('',(#126640),#65829) ;
#2407 = STYLED_ITEM('',(#126640),#65830) ;
#2408 = STYLED_ITEM('',(#126640),#65831) ;
#2409 = STYLED_ITEM('',(#126640),#65832) ;
#2410 = STYLED_ITEM('',(#126640),#65833) ;
#2411 = STYLED_ITEM('',(#126640),#65834) ;
#2412 = STYLED_ITEM('',(#126640),#65835) ;
#2413 = STYLED_ITEM('',(#126640),#65836) ;
#2414 = STYLED_ITEM('',(#126640),#65837) ;
#2415 = STYLED_ITEM('',(#126640),#65838) ;
#2416 = STYLED_ITEM('',(#126640),#65839) ;
#2417 = STYLED_ITEM('',(#126640),#65840) ;
#2418 = STYLED_ITEM('',(#126640),#65841) ;
#2419 = STYLED_ITEM('',(#126640),#65842) ;
#2420 = STYLED_ITEM('',(#126640),#65843) ;
#2421 = STYLED_ITEM('',(#126640),#65844) ;
#2422 = STYLED_ITEM('',(#126640),#65845) ;
#2423 = STYLED_ITEM('',(#126640),#65846) ;
#2424 = STYLED_ITEM('',(#126640),#65847) ;
#2425 = STYLED_ITEM('',(#126640),#65848) ;
#2426 = STYLED_ITEM('',(#126640),#65849) ;
#2427 = STYLED_ITEM('',(#126640),#65850) ;
#2428 = STYLED_ITEM('',(#126640),#65851) ;
#2429 = STYLED_ITEM('',(#126640),#65852) ;
#2430 = STYLED_ITEM('',(#126640),#65853) ;
#2431 = STYLED_ITEM('',(#126640),#65854) ;
#2432 = STYLED_ITEM('',(#126640),#65855) ;
#2433 = STYLED_ITEM('',(#126640),#65856) ;
#2434 = STYLED_ITEM('',(#126640),#65857) ;
#2435 = STYLED_ITEM('',(#126640),#65858) ;
#2436 = STYLED_ITEM('',(#126640),#65859) ;
#2437 = STYLED_ITEM('',(#126640),#65860) ;
#2438 = STYLED_ITEM('',(#126640),#65861) ;
#2439 = STYLED_ITEM('',(#126640),#65862) ;
#2440 = STYLED_ITEM('',(#126640),#65863) ;
#2441 = STYLED_ITEM('',(#126640),#65864) ;
#2442 = STYLED_ITEM('',(#126640),#65865) ;
#2443 = STYLED_ITEM('',(#126640),#65866) ;
#2444 = STYLED_ITEM('',(#126640),#65867) ;
#2445 = STYLED_ITEM('',(#126640),#65868) ;
#2446 = STYLED_ITEM('',(#126640),#65869) ;
#2447 = STYLED_ITEM('',(#126640),#65870) ;
#2448 = STYLED_ITEM('',(#126640),#65871) ;
#2449 = STYLED_ITEM('',(#126640),#65872) ;
#2450 = STYLED_ITEM('',(#126640),#65873) ;
#2451 = STYLED_ITEM('',(#126640),#65874) ;
#2452 = STYLED_ITEM('',(#126640),#65875) ;
#2453 = STYLED_ITEM('',(#126640),#65876) ;
#2454 = STYLED_ITEM('',(#126640),#65877) ;
#2455 = STYLED_ITEM('',(#126640),#65878) ;
#2456 = STYLED_ITEM('',(#126640),#65879) ;
#2457 = STYLED_ITEM('',(#126640),#65880) ;
#2458 = STYLED_ITEM('',(#126640),#65881) ;
#2459 = STYLED_ITEM('',(#126640),#65882) ;
#2460 = STYLED_ITEM('',(#126640),#65883) ;
#2461 = STYLED_ITEM('',(#126640),#65884) ;
#2462 = STYLED_ITEM('',(#126640),#65885) ;
#2463 = STYLED_ITEM('',(#126640),#65886) ;
#2464 = STYLED_ITEM('',(#126640),#65887) ;
#2465 = STYLED_ITEM('',(#126640),#65888) ;
#2466 = STYLED_ITEM('',(#126640),#65889) ;
#2467 = STYLED_ITEM('',(#126640),#65890) ;
#2468 = STYLED_ITEM('',(#126640),#65891) ;
#2469 = STYLED_ITEM('',(#126640),#65892) ;
#2470 = STYLED_ITEM('',(#126640),#65893) ;
#2471 = STYLED_ITEM('',(#126640),#65894) ;
#2472 = STYLED_ITEM('',(#126640),#65895) ;
#2473 = STYLED_ITEM('',(#126640),#65896) ;
#2474 = STYLED_ITEM('',(#126640),#65897) ;
#2475 = STYLED_ITEM('',(#126640),#65898) ;
#2476 = STYLED_ITEM('',(#126640),#65899) ;
#2477 = STYLED_ITEM('',(#126640),#65900) ;
#2478 = STYLED_ITEM('',(#126640),#65901) ;
#2479 = STYLED_ITEM('',(#126640),#65902) ;
#2480 = STYLED_ITEM('',(#126640),#65903) ;
#2481 = STYLED_ITEM('',(#126640),#65904) ;
#2482 = STYLED_ITEM('',(#126640),#65905) ;
#2483 = STYLED_ITEM('',(#126640),#65906) ;
#2484 = STYLED_ITEM('',(#126640),#65907) ;
#2485 = STYLED_ITEM('',(#126640),#65908) ;
#2486 = STYLED_ITEM('',(#126640),#65909) ;
#2487 = STYLED_ITEM('',(#126640),#65910) ;
#2488 = STYLED_ITEM('',(#126640),#65911) ;
#2489 = STYLED_ITEM('',(#126640),#65912) ;
#2490 = STYLED_ITEM('',(#126640),#65913) ;
#2491 = STYLED_ITEM('',(#126640),#65914) ;
#2492 = STYLED_ITEM('',(#126640),#65915) ;
#2493 = STYLED_ITEM('',(#126640),#65916) ;
#2494 = STYLED_ITEM('',(#126640),#65917) ;
#2495 = STYLED_ITEM('',(#126640),#65918) ;
#2496 = STYLED_ITEM('',(#126640),#65919) ;
#2497 = STYLED_ITEM('',(#126640),#65920) ;
#2498 = STYLED_ITEM('',(#126640),#65921) ;
#2499 = STYLED_ITEM('',(#126640),#65922) ;
#2500 = STYLED_ITEM('',(#126640),#65923) ;
#2501 = STYLED_ITEM('',(#126640),#65924) ;
#2502 = STYLED_ITEM('',(#126640),#65925) ;
#2503 = STYLED_ITEM('',(#126640),#65926) ;
#2504 = STYLED_ITEM('',(#126640),#65927) ;
#2505 = STYLED_ITEM('',(#126640),#65928) ;
#2506 = STYLED_ITEM('',(#126640),#65929) ;
#2507 = STYLED_ITEM('',(#126640),#65930) ;
#2508 = STYLED_ITEM('',(#126640),#65931) ;
#2509 = STYLED_ITEM('',(#126640),#65932) ;
#2510 = STYLED_ITEM('',(#126640),#65933) ;
#2511 = STYLED_ITEM('',(#126640),#65934) ;
#2512 = STYLED_ITEM('',(#126640),#65935) ;
#2513 = STYLED_ITEM('',(#126640),#65936) ;
#2514 = STYLED_ITEM('',(#126640),#65937) ;
#2515 = STYLED_ITEM('',(#126640),#65938) ;
#2516 = STYLED_ITEM('',(#126640),#65939) ;
#2517 = STYLED_ITEM('',(#126640),#65940) ;
#2518 = STYLED_ITEM('',(#126640),#65941) ;
#2519 = STYLED_ITEM('',(#126640),#65942) ;
#2520 = STYLED_ITEM('',(#126640),#65943) ;
#2521 = STYLED_ITEM('',(#126640),#65944) ;
#2522 = STYLED_ITEM('',(#126640),#65945) ;
#2523 = STYLED_ITEM('',(#126640),#65946) ;
#2524 = STYLED_ITEM('',(#126640),#65947) ;
#2525 = STYLED_ITEM('',(#126640),#65948) ;
#2526 = STYLED_ITEM('',(#126640),#65949) ;
#2527 = STYLED_ITEM('',(#126640),#65950) ;
#2528 = STYLED_ITEM('',(#126640),#65951) ;
#2529 = STYLED_ITEM('',(#126640),#65952) ;
#2530 = STYLED_ITEM('',(#126640),#65953) ;
#2531 = STYLED_ITEM('',(#126640),#65954) ;
#2532 = STYLED_ITEM('',(#126640),#65955) ;
#2533 = STYLED_ITEM('',(#126640),#65956) ;
#2534 = STYLED_ITEM('',(#126640),#65957) ;
#2535 = STYLED_ITEM('',(#126640),#65958) ;
#2536 = STYLED_ITEM('',(#126640),#65959) ;
#2537 = STYLED_ITEM('',(#126640),#65960) ;
#2538 = STYLED_ITEM('',(#126640),#65961) ;
#2539 = STYLED_ITEM('',(#126640),#65962) ;
#2540 = STYLED_ITEM('',(#126640),#65963) ;
#2541 = STYLED_ITEM('',(#126640),#65964) ;
#2542 = STYLED_ITEM('',(#126640),#65965) ;
#2543 = STYLED_ITEM('',(#126640),#65966) ;
#2544 = STYLED_ITEM('',(#126640),#65967) ;
#2545 = STYLED_ITEM('',(#126640),#65968) ;
#2546 = STYLED_ITEM('',(#126640),#65969) ;
#2547 = STYLED_ITEM('',(#126640),#65970) ;
#2548 = STYLED_ITEM('',(#126640),#65971) ;
#2549 = STYLED_ITEM('',(#126640),#65972) ;
#2550 = STYLED_ITEM('',(#126640),#65973) ;
#2551 = STYLED_ITEM('',(#126640),#65974) ;
#2552 = STYLED_ITEM('',(#126640),#65975) ;
#2553 = STYLED_ITEM('',(#126640),#65976) ;
#2554 = STYLED_ITEM('',(#126640),#65977) ;
#2555 = STYLED_ITEM('',(#126640),#65978) ;
#2556 = STYLED_ITEM('',(#126640),#65979) ;
#2557 = STYLED_ITEM('',(#126640),#65980) ;
#2558 = STYLED_ITEM('',(#126640),#65981) ;
#2559 = STYLED_ITEM('',(#126640),#65982) ;
#2560 = STYLED_ITEM('',(#126640),#65983) ;
#2561 = STYLED_ITEM('',(#126640),#65984) ;
#2562 = STYLED_ITEM('',(#126640),#65985) ;
#2563 = STYLED_ITEM('',(#126640),#65986) ;
#2564 = STYLED_ITEM('',(#126640),#65987) ;
#2565 = STYLED_ITEM('',(#126640),#65988) ;
#2566 = STYLED_ITEM('',(#126640),#65989) ;
#2567 = STYLED_ITEM('',(#126640),#65990) ;
#2568 = STYLED_ITEM('',(#126640),#65991) ;
#2569 = STYLED_ITEM('',(#126640),#65992) ;
#2570 = STYLED_ITEM('',(#126640),#65993) ;
#2571 = STYLED_ITEM('',(#126640),#65994) ;
#2572 = STYLED_ITEM('',(#126640),#65995) ;
#2573 = STYLED_ITEM('',(#126640),#65996) ;
#2574 = STYLED_ITEM('',(#126640),#65997) ;
#2575 = STYLED_ITEM('',(#126640),#65998) ;
#2576 = STYLED_ITEM('',(#126640),#65999) ;
#2577 = STYLED_ITEM('',(#126640),#66000) ;
#2578 = STYLED_ITEM('',(#126640),#66001) ;
#2579 = STYLED_ITEM('',(#126640),#66002) ;
#2580 = STYLED_ITEM('',(#126640),#66003) ;
#2581 = STYLED_ITEM('',(#126640),#66004) ;
#2582 = STYLED_ITEM('',(#126640),#66005) ;
#2583 = STYLED_ITEM('',(#126640),#66006) ;
#2584 = STYLED_ITEM('',(#126640),#66007) ;
#2585 = STYLED_ITEM('',(#126640),#66008) ;
#2586 = STYLED_ITEM('',(#126640),#66009) ;
#2587 = STYLED_ITEM('',(#126640),#66010) ;
#2588 = STYLED_ITEM('',(#126640),#66011) ;
#2589 = STYLED_ITEM('',(#126640),#66012) ;
#2590 = STYLED_ITEM('',(#126640),#66013) ;
#2591 = STYLED_ITEM('',(#126640),#66014) ;
#2592 = STYLED_ITEM('',(#126640),#66015) ;
#2593 = STYLED_ITEM('',(#126640),#66016) ;
#2594 = STYLED_ITEM('',(#126640),#66017) ;
#2595 = STYLED_ITEM('',(#126640),#66018) ;
#2596 = STYLED_ITEM('',(#126640),#66019) ;
#2597 = STYLED_ITEM('',(#126640),#66020) ;
#2598 = STYLED_ITEM('',(#126640),#66021) ;
#2599 = STYLED_ITEM('',(#126640),#66022) ;
#2600 = STYLED_ITEM('',(#126640),#66023) ;
#2601 = STYLED_ITEM('',(#126640),#66024) ;
#2602 = STYLED_ITEM('',(#126640),#66025) ;
#2603 = STYLED_ITEM('',(#126640),#66026) ;
#2604 = STYLED_ITEM('',(#126640),#66027) ;
#2605 = STYLED_ITEM('',(#126640),#66028) ;
#2606 = STYLED_ITEM('',(#126640),#66029) ;
#2607 = STYLED_ITEM('',(#126640),#66030) ;
#2608 = STYLED_ITEM('',(#126640),#66031) ;
#2609 = STYLED_ITEM('',(#126640),#66032) ;
#2610 = STYLED_ITEM('',(#126640),#66033) ;
#2611 = STYLED_ITEM('',(#126640),#66034) ;
#2612 = STYLED_ITEM('',(#126640),#66035) ;
#2613 = STYLED_ITEM('',(#126640),#66036) ;
#2614 = STYLED_ITEM('',(#126640),#66037) ;
#2615 = STYLED_ITEM('',(#126640),#66038) ;
#2616 = STYLED_ITEM('',(#126640),#66039) ;
#2617 = STYLED_ITEM('',(#126640),#66040) ;
#2618 = STYLED_ITEM('',(#126640),#66041) ;
#2619 = STYLED_ITEM('',(#126640),#66042) ;
#2620 = STYLED_ITEM('',(#126640),#66043) ;
#2621 = STYLED_ITEM('',(#126640),#66044) ;
#2622 = STYLED_ITEM('',(#126640),#66045) ;
#2623 = STYLED_ITEM('',(#126640),#66046) ;
#2624 = STYLED_ITEM('',(#126640),#66047) ;
#2625 = STYLED_ITEM('',(#126640),#66048) ;
#2626 = STYLED_ITEM('',(#126640),#66049) ;
#2627 = STYLED_ITEM('',(#126640),#66050) ;
#2628 = STYLED_ITEM('',(#126640),#66051) ;
#2629 = STYLED_ITEM('',(#126640),#66052) ;
#2630 = STYLED_ITEM('',(#126640),#66053) ;
#2631 = STYLED_ITEM('',(#126640),#66054) ;
#2632 = STYLED_ITEM('',(#126640),#66055) ;
#2633 = STYLED_ITEM('',(#126640),#66056) ;
#2634 = STYLED_ITEM('',(#126640),#66057) ;
#2635 = STYLED_ITEM('',(#126640),#66058) ;
#2636 = STYLED_ITEM('',(#126640),#66059) ;
#2637 = STYLED_ITEM('',(#126640),#66060) ;
#2638 = STYLED_ITEM('',(#126640),#66061) ;
#2639 = STYLED_ITEM('',(#126640),#66062) ;
#2640 = STYLED_ITEM('',(#126640),#66063) ;
#2641 = STYLED_ITEM('',(#126640),#66064) ;
#2642 = STYLED_ITEM('',(#126640),#66065) ;
#2643 = STYLED_ITEM('',(#126640),#66066) ;
#2644 = STYLED_ITEM('',(#126640),#66067) ;
#2645 = STYLED_ITEM('',(#126640),#66068) ;
#2646 = STYLED_ITEM('',(#126640),#66069) ;
#2647 = STYLED_ITEM('',(#126640),#66070) ;
#2648 = STYLED_ITEM('',(#126640),#66071) ;
#2649 = STYLED_ITEM('',(#126640),#66072) ;
#2650 = STYLED_ITEM('',(#126640),#66073) ;
#2651 = STYLED_ITEM('',(#126640),#66074) ;
#2652 = STYLED_ITEM('',(#126640),#66075) ;
#2653 = STYLED_ITEM('',(#126640),#66076) ;
#2654 = STYLED_ITEM('',(#126640),#66077) ;
#2655 = STYLED_ITEM('',(#126640),#66078) ;
#2656 = STYLED_ITEM('',(#126640),#66079) ;
#2657 = STYLED_ITEM('',(#126640),#66080) ;
#2658 = STYLED_ITEM('',(#126640),#66081) ;
#2659 = STYLED_ITEM('',(#126640),#66082) ;
#2660 = STYLED_ITEM('',(#126640),#66083) ;
#2661 = STYLED_ITEM('',(#126640),#66084) ;
#2662 = STYLED_ITEM('',(#126640),#66085) ;
#2663 = STYLED_ITEM('',(#126640),#66086) ;
#2664 = STYLED_ITEM('',(#126640),#66087) ;
#2665 = STYLED_ITEM('',(#126640),#66088) ;
#2666 = STYLED_ITEM('',(#126640),#66089) ;
#2667 = STYLED_ITEM('',(#126640),#66090) ;
#2668 = STYLED_ITEM('',(#126640),#66091) ;
#2669 = STYLED_ITEM('',(#126640),#66092) ;
#2670 = STYLED_ITEM('',(#126640),#66093) ;
#2671 = STYLED_ITEM('',(#126640),#66094) ;
#2672 = STYLED_ITEM('',(#126640),#66095) ;
#2673 = STYLED_ITEM('',(#126640),#66096) ;
#2674 = STYLED_ITEM('',(#126640),#66097) ;
#2675 = STYLED_ITEM('',(#126640),#66098) ;
#2676 = STYLED_ITEM('',(#126640),#66099) ;
#2677 = STYLED_ITEM('',(#126640),#66100) ;
#2678 = STYLED_ITEM('',(#126640),#66101) ;
#2679 = STYLED_ITEM('',(#126640),#66102) ;
#2680 = STYLED_ITEM('',(#126640),#66103) ;
#2681 = STYLED_ITEM('',(#126640),#66104) ;
#2682 = STYLED_ITEM('',(#126640),#66105) ;
#2683 = STYLED_ITEM('',(#126640),#66106) ;
#2684 = STYLED_ITEM('',(#126640),#66107) ;
#2685 = STYLED_ITEM('',(#126640),#66108) ;
#2686 = STYLED_ITEM('',(#126640),#66109) ;
#2687 = STYLED_ITEM('',(#126640),#66110) ;
#2688 = STYLED_ITEM('',(#126640),#66111) ;
#2689 = STYLED_ITEM('',(#126640),#66112) ;
#2690 = STYLED_ITEM('',(#126640),#66113) ;
#2691 = STYLED_ITEM('',(#126640),#66114) ;
#2692 = STYLED_ITEM('',(#126640),#66115) ;
#2693 = STYLED_ITEM('',(#126640),#66116) ;
#2694 = STYLED_ITEM('',(#126640),#66117) ;
#2695 = STYLED_ITEM('',(#126640),#66118) ;
#2696 = STYLED_ITEM('',(#126640),#66119) ;
#2697 = STYLED_ITEM('',(#126640),#66120) ;
#2698 = STYLED_ITEM('',(#126640),#66121) ;
#2699 = STYLED_ITEM('',(#126640),#66122) ;
#2700 = STYLED_ITEM('',(#126640),#66123) ;
#2701 = STYLED_ITEM('',(#126640),#66124) ;
#2702 = STYLED_ITEM('',(#126640),#66125) ;
#2703 = STYLED_ITEM('',(#126640),#66126) ;
#2704 = STYLED_ITEM('',(#126640),#66127) ;
#2705 = STYLED_ITEM('',(#126640),#66128) ;
#2706 = STYLED_ITEM('',(#126640),#66129) ;
#2707 = STYLED_ITEM('',(#126640),#66130) ;
#2708 = STYLED_ITEM('',(#126640),#66131) ;
#2709 = STYLED_ITEM('',(#126640),#66132) ;
#2710 = STYLED_ITEM('',(#126640),#66133) ;
#2711 = STYLED_ITEM('',(#126640),#66134) ;
#2712 = STYLED_ITEM('',(#126640),#66135) ;
#2713 = STYLED_ITEM('',(#126640),#66136) ;
#2714 = STYLED_ITEM('',(#126640),#66137) ;
#2715 = STYLED_ITEM('',(#126640),#66138) ;
#2716 = STYLED_ITEM('',(#126640),#66139) ;
#2717 = STYLED_ITEM('',(#126640),#66140) ;
#2718 = STYLED_ITEM('',(#126640),#66141) ;
#2719 = STYLED_ITEM('',(#126640),#66142) ;
#2720 = STYLED_ITEM('',(#126640),#66143) ;
#2721 = STYLED_ITEM('',(#126640),#66144) ;
#2722 = STYLED_ITEM('',(#126640),#66145) ;
#2723 = STYLED_ITEM('',(#126640),#66146) ;
#2724 = STYLED_ITEM('',(#126640),#66147) ;
#2725 = STYLED_ITEM('',(#126640),#66148) ;
#2726 = STYLED_ITEM('',(#126640),#66149) ;
#2727 = STYLED_ITEM('',(#126640),#66150) ;
#2728 = STYLED_ITEM('',(#126640),#66151) ;
#2729 = STYLED_ITEM('',(#126640),#66152) ;
#2730 = STYLED_ITEM('',(#126640),#66153) ;
#2731 = STYLED_ITEM('',(#126640),#66154) ;
#2732 = STYLED_ITEM('',(#126640),#66155) ;
#2733 = STYLED_ITEM('',(#126640),#66156) ;
#2734 = STYLED_ITEM('',(#126640),#66157) ;
#2735 = STYLED_ITEM('',(#126640),#66158) ;
#2736 = STYLED_ITEM('',(#126640),#66159) ;
#2737 = STYLED_ITEM('',(#126640),#66160) ;
#2738 = STYLED_ITEM('',(#126640),#66161) ;
#2739 = STYLED_ITEM('',(#126640),#66162) ;
#2740 = STYLED_ITEM('',(#126640),#66163) ;
#2741 = STYLED_ITEM('',(#126640),#66164) ;
#2742 = STYLED_ITEM('',(#126640),#66165) ;
#2743 = STYLED_ITEM('',(#126640),#66166) ;
#2744 = STYLED_ITEM('',(#126640),#66167) ;
#2745 = STYLED_ITEM('',(#126640),#66168) ;
#2746 = STYLED_ITEM('',(#126640),#66169) ;
#2747 = STYLED_ITEM('',(#126640),#66170) ;
#2748 = STYLED_ITEM('',(#126640),#66171) ;
#2749 = STYLED_ITEM('',(#126640),#66172) ;
#2750 = STYLED_ITEM('',(#126640),#66173) ;
#2751 = STYLED_ITEM('',(#126640),#66174) ;
#2752 = STYLED_ITEM('',(#126640),#66175) ;
#2753 = STYLED_ITEM('',(#126640),#66176) ;
#2754 = STYLED_ITEM('',(#126640),#66177) ;
#2755 = STYLED_ITEM('',(#126640),#66178) ;
#2756 = STYLED_ITEM('',(#126640),#66179) ;
#2757 = STYLED_ITEM('',(#126640),#66180) ;
#2758 = STYLED_ITEM('',(#126640),#66181) ;
#2759 = STYLED_ITEM('',(#126640),#66182) ;
#2760 = STYLED_ITEM('',(#126640),#66183) ;
#2761 = STYLED_ITEM('',(#126640),#66184) ;
#2762 = STYLED_ITEM('',(#126640),#66185) ;
#2763 = STYLED_ITEM('',(#126640),#66186) ;
#2764 = STYLED_ITEM('',(#126640),#66187) ;
#2765 = STYLED_ITEM('',(#126640),#66188) ;
#2766 = STYLED_ITEM('',(#126640),#66189) ;
#2767 = STYLED_ITEM('',(#126640),#66190) ;
#2768 = STYLED_ITEM('',(#126640),#66191) ;
#2769 = STYLED_ITEM('',(#126640),#66192) ;
#2770 = STYLED_ITEM('',(#126640),#66193) ;
#2771 = STYLED_ITEM('',(#126640),#66194) ;
#2772 = STYLED_ITEM('',(#126640),#66195) ;
#2773 = STYLED_ITEM('',(#126640),#66196) ;
#2774 = STYLED_ITEM('',(#126640),#66197) ;
#2775 = STYLED_ITEM('',(#126640),#66198) ;
#2776 = STYLED_ITEM('',(#126640),#66199) ;
#2777 = STYLED_ITEM('',(#126640),#66200) ;
#2778 = STYLED_ITEM('',(#126640),#66201) ;
#2779 = STYLED_ITEM('',(#126640),#66202) ;
#2780 = STYLED_ITEM('',(#126640),#66203) ;
#2781 = STYLED_ITEM('',(#126640),#66204) ;
#2782 = STYLED_ITEM('',(#126640),#66205) ;
#2783 = STYLED_ITEM('',(#126640),#66206) ;
#2784 = STYLED_ITEM('',(#126640),#66207) ;
#2785 = STYLED_ITEM('',(#126640),#66208) ;
#2786 = STYLED_ITEM('',(#126640),#66209) ;
#2787 = STYLED_ITEM('',(#126640),#66210) ;
#2788 = STYLED_ITEM('',(#126640),#66211) ;
#2789 = STYLED_ITEM('',(#126640),#66212) ;
#2790 = STYLED_ITEM('',(#126640),#66213) ;
#2791 = STYLED_ITEM('',(#126640),#66214) ;
#2792 = STYLED_ITEM('',(#126640),#66215) ;
#2793 = STYLED_ITEM('',(#126640),#66216) ;
#2794 = STYLED_ITEM('',(#126640),#66217) ;
#2795 = STYLED_ITEM('',(#126640),#66218) ;
#2796 = STYLED_ITEM('',(#126640),#66219) ;
#2797 = STYLED_ITEM('',(#126640),#66220) ;
#2798 = STYLED_ITEM('',(#126640),#66221) ;
#2799 = STYLED_ITEM('',(#126640),#66222) ;
#2800 = STYLED_ITEM('',(#126640),#66223) ;
#2801 = STYLED_ITEM('',(#126640),#66224) ;
#2802 = STYLED_ITEM('',(#126640),#66225) ;
#2803 = STYLED_ITEM('',(#126640),#66226) ;
#2804 = STYLED_ITEM('',(#126640),#66227) ;
#2805 = STYLED_ITEM('',(#126640),#66228) ;
#2806 = STYLED_ITEM('',(#126640),#66229) ;
#2807 = STYLED_ITEM('',(#126640),#66230) ;
#2808 = STYLED_ITEM('',(#126640),#66231) ;
#2809 = STYLED_ITEM('',(#126640),#66232) ;
#2810 = STYLED_ITEM('',(#126640),#66233) ;
#2811 = STYLED_ITEM('',(#126640),#66234) ;
#2812 = STYLED_ITEM('',(#126640),#66235) ;
#2813 = STYLED_ITEM('',(#126640),#66236) ;
#2814 = STYLED_ITEM('',(#126640),#66237) ;
#2815 = STYLED_ITEM('',(#126640),#66238) ;
#2816 = STYLED_ITEM('',(#126640),#66239) ;
#2817 = STYLED_ITEM('',(#126640),#66240) ;
#2818 = STYLED_ITEM('',(#126640),#66241) ;
#2819 = STYLED_ITEM('',(#126640),#66242) ;
#2820 = STYLED_ITEM('',(#126640),#66243) ;
#2821 = STYLED_ITEM('',(#126640),#66244) ;
#2822 = STYLED_ITEM('',(#126640),#66245) ;
#2823 = STYLED_ITEM('',(#126640),#66246) ;
#2824 = STYLED_ITEM('',(#126640),#66247) ;
#2825 = STYLED_ITEM('',(#126640),#66248) ;
#2826 = STYLED_ITEM('',(#126640),#66249) ;
#2827 = STYLED_ITEM('',(#126640),#66250) ;
#2828 = STYLED_ITEM('',(#126640),#66251) ;
#2829 = STYLED_ITEM('',(#126640),#66252) ;
#2830 = STYLED_ITEM('',(#126640),#66253) ;
#2831 = STYLED_ITEM('',(#126640),#66254) ;
#2832 = STYLED_ITEM('',(#126640),#66255) ;
#2833 = STYLED_ITEM('',(#126640),#66256) ;
#2834 = STYLED_ITEM('',(#126640),#66257) ;
#2835 = STYLED_ITEM('',(#126640),#66258) ;
#2836 = STYLED_ITEM('',(#126640),#66259) ;
#2837 = STYLED_ITEM('',(#126640),#66260) ;
#2838 = STYLED_ITEM('',(#126640),#66261) ;
#2839 = STYLED_ITEM('',(#126640),#66262) ;
#2840 = STYLED_ITEM('',(#126640),#66263) ;
#2841 = STYLED_ITEM('',(#126640),#66264) ;
#2842 = STYLED_ITEM('',(#126640),#66265) ;
#2843 = STYLED_ITEM('',(#126640),#66266) ;
#2844 = STYLED_ITEM('',(#126640),#66267) ;
#2845 = STYLED_ITEM('',(#126640),#66268) ;
#2846 = STYLED_ITEM('',(#126640),#66269) ;
#2847 = STYLED_ITEM('',(#126640),#66270) ;
#2848 = STYLED_ITEM('',(#126640),#66271) ;
#2849 = STYLED_ITEM('',(#126640),#66272) ;
#2850 = STYLED_ITEM('',(#126640),#66273) ;
#2851 = STYLED_ITEM('',(#126640),#66274) ;
#2852 = STYLED_ITEM('',(#126640),#66275) ;
#2853 = STYLED_ITEM('',(#126640),#66276) ;
#2854 = STYLED_ITEM('',(#126640),#66277) ;
#2855 = STYLED_ITEM('',(#126640),#66278) ;
#2856 = STYLED_ITEM('',(#126640),#66279) ;
#2857 = STYLED_ITEM('',(#126640),#66280) ;
#2858 = STYLED_ITEM('',(#126640),#66281) ;
#2859 = STYLED_ITEM('',(#126640),#66282) ;
#2860 = STYLED_ITEM('',(#126640),#66283) ;
#2861 = STYLED_ITEM('',(#126640),#66284) ;
#2862 = STYLED_ITEM('',(#126640),#66285) ;
#2863 = STYLED_ITEM('',(#126640),#66286) ;
#2864 = STYLED_ITEM('',(#126640),#66287) ;
#2865 = STYLED_ITEM('',(#126640),#66288) ;
#2866 = STYLED_ITEM('',(#126640),#66289) ;
#2867 = STYLED_ITEM('',(#126640),#66290) ;
#2868 = STYLED_ITEM('',(#126640),#66291) ;
#2869 = STYLED_ITEM('',(#126640),#66292) ;
#2870 = STYLED_ITEM('',(#126640),#66293) ;
#2871 = STYLED_ITEM('',(#126640),#66294) ;
#2872 = STYLED_ITEM('',(#126640),#66295) ;
#2873 = STYLED_ITEM('',(#126640),#66296) ;
#2874 = STYLED_ITEM('',(#126640),#66297) ;
#2875 = STYLED_ITEM('',(#126640),#66298) ;
#2876 = STYLED_ITEM('',(#126640),#66299) ;
#2877 = STYLED_ITEM('',(#126640),#66300) ;
#2878 = STYLED_ITEM('',(#126640),#66301) ;
#2879 = STYLED_ITEM('',(#126640),#66302) ;
#2880 = STYLED_ITEM('',(#126640),#66303) ;
#2881 = STYLED_ITEM('',(#126640),#66304) ;
#2882 = STYLED_ITEM('',(#126640),#66305) ;
#2883 = STYLED_ITEM('',(#126640),#66306) ;
#2884 = STYLED_ITEM('',(#126640),#66307) ;
#2885 = STYLED_ITEM('',(#126640),#66308) ;
#2886 = STYLED_ITEM('',(#126640),#66309) ;
#2887 = STYLED_ITEM('',(#126640),#66310) ;
#2888 = STYLED_ITEM('',(#126640),#66311) ;
#2889 = STYLED_ITEM('',(#126640),#66312) ;
#2890 = STYLED_ITEM('',(#126640),#66313) ;
#2891 = STYLED_ITEM('',(#126640),#66314) ;
#2892 = STYLED_ITEM('',(#126640),#66315) ;
#2893 = STYLED_ITEM('',(#126640),#66316) ;
#2894 = STYLED_ITEM('',(#126640),#66317) ;
#2895 = STYLED_ITEM('',(#126640),#66318) ;
#2896 = STYLED_ITEM('',(#126640),#66319) ;
#2897 = STYLED_ITEM('',(#126640),#66320) ;
#2898 = STYLED_ITEM('',(#126640),#66321) ;
#2899 = STYLED_ITEM('',(#126640),#66322) ;
#2900 = STYLED_ITEM('',(#126640),#66323) ;
#2901 = STYLED_ITEM('',(#126640),#66324) ;
#2902 = STYLED_ITEM('',(#126640),#66325) ;
#2903 = STYLED_ITEM('',(#126640),#66326) ;
#2904 = STYLED_ITEM('',(#126640),#66327) ;
#2905 = STYLED_ITEM('',(#126640),#66328) ;
#2906 = STYLED_ITEM('',(#126640),#66329) ;
#2907 = STYLED_ITEM('',(#126640),#66330) ;
#2908 = STYLED_ITEM('',(#126640),#66331) ;
#2909 = STYLED_ITEM('',(#126640),#66332) ;
#2910 = STYLED_ITEM('',(#126640),#66333) ;
#2911 = STYLED_ITEM('',(#126640),#66334) ;
#2912 = STYLED_ITEM('',(#126640),#66335) ;
#2913 = STYLED_ITEM('',(#126640),#66336) ;
#2914 = STYLED_ITEM('',(#126640),#66337) ;
#2915 = STYLED_ITEM('',(#126640),#66338) ;
#2916 = STYLED_ITEM('',(#126640),#66339) ;
#2917 = STYLED_ITEM('',(#126640),#66340) ;
#2918 = STYLED_ITEM('',(#126640),#66341) ;
#2919 = STYLED_ITEM('',(#126640),#66342) ;
#2920 = STYLED_ITEM('',(#126640),#66343) ;
#2921 = STYLED_ITEM('',(#126640),#66344) ;
#2922 = STYLED_ITEM('',(#126640),#66345) ;
#2923 = STYLED_ITEM('',(#126640),#66346) ;
#2924 = STYLED_ITEM('',(#126640),#66347) ;
#2925 = STYLED_ITEM('',(#126640),#66348) ;
#2926 = STYLED_ITEM('',(#126640),#66349) ;
#2927 = STYLED_ITEM('',(#126640),#66350) ;
#2928 = STYLED_ITEM('',(#126640),#66351) ;
#2929 = STYLED_ITEM('',(#126640),#66352) ;
#2930 = STYLED_ITEM('',(#126640),#66353) ;
#2931 = STYLED_ITEM('',(#126640),#66354) ;
#2932 = STYLED_ITEM('',(#126640),#66355) ;
#2933 = STYLED_ITEM('',(#126640),#66356) ;
#2934 = STYLED_ITEM('',(#126640),#66357) ;
#2935 = STYLED_ITEM('',(#126640),#66358) ;
#2936 = STYLED_ITEM('',(#126640),#66359) ;
#2937 = STYLED_ITEM('',(#126640),#66360) ;
#2938 = STYLED_ITEM('',(#126640),#66361) ;
#2939 = STYLED_ITEM('',(#126640),#66362) ;
#2940 = STYLED_ITEM('',(#126640),#66363) ;
#2941 = STYLED_ITEM('',(#126640),#66364) ;
#2942 = STYLED_ITEM('',(#126640),#66365) ;
#2943 = STYLED_ITEM('',(#126640),#66366) ;
#2944 = STYLED_ITEM('',(#126640),#66367) ;
#2945 = STYLED_ITEM('',(#126640),#66368) ;
#2946 = STYLED_ITEM('',(#126640),#66369) ;
#2947 = STYLED_ITEM('',(#126640),#66370) ;
#2948 = STYLED_ITEM('',(#126640),#66371) ;
#2949 = STYLED_ITEM('',(#126640),#66372) ;
#2950 = STYLED_ITEM('',(#126640),#66373) ;
#2951 = STYLED_ITEM('',(#126640),#66374) ;
#2952 = STYLED_ITEM('',(#126640),#66375) ;
#2953 = STYLED_ITEM('',(#126640),#66376) ;
#2954 = STYLED_ITEM('',(#126640),#66377) ;
#2955 = STYLED_ITEM('',(#126640),#66378) ;
#2956 = STYLED_ITEM('',(#126640),#66379) ;
#2957 = STYLED_ITEM('',(#126640),#66380) ;
#2958 = STYLED_ITEM('',(#126640),#66381) ;
#2959 = STYLED_ITEM('',(#126640),#66382) ;
#2960 = STYLED_ITEM('',(#126640),#66383) ;
#2961 = STYLED_ITEM('',(#126640),#66384) ;
#2962 = STYLED_ITEM('',(#126640),#66385) ;
#2963 = STYLED_ITEM('',(#126640),#66386) ;
#2964 = STYLED_ITEM('',(#126640),#66387) ;
#2965 = STYLED_ITEM('',(#126640),#66388) ;
#2966 = STYLED_ITEM('',(#126640),#66389) ;
#2967 = STYLED_ITEM('',(#126640),#66390) ;
#2968 = STYLED_ITEM('',(#126640),#66391) ;
#2969 = STYLED_ITEM('',(#126640),#66392) ;
#2970 = STYLED_ITEM('',(#126640),#66393) ;
#2971 = STYLED_ITEM('',(#126640),#66394) ;
#2972 = STYLED_ITEM('',(#126640),#66395) ;
#2973 = STYLED_ITEM('',(#126640),#66396) ;
#2974 = STYLED_ITEM('',(#126640),#66397) ;
#2975 = STYLED_ITEM('',(#126640),#66398) ;
#2976 = STYLED_ITEM('',(#126640),#66399) ;
#2977 = STYLED_ITEM('',(#126640),#66400) ;
#2978 = STYLED_ITEM('',(#126640),#66401) ;
#2979 = STYLED_ITEM('',(#126640),#66402) ;
#2980 = STYLED_ITEM('',(#126640),#66403) ;
#2981 = STYLED_ITEM('',(#126640),#66404) ;
#2982 = STYLED_ITEM('',(#126640),#66405) ;
#2983 = STYLED_ITEM('',(#126640),#66406) ;
#2984 = STYLED_ITEM('',(#126640),#66407) ;
#2985 = STYLED_ITEM('',(#126640),#66408) ;
#2986 = STYLED_ITEM('',(#126640),#66409) ;
#2987 = STYLED_ITEM('',(#126640),#66410) ;
#2988 = STYLED_ITEM('',(#126640),#66411) ;
#2989 = STYLED_ITEM('',(#126640),#66412) ;
#2990 = STYLED_ITEM('',(#126640),#66413) ;
#2991 = STYLED_ITEM('',(#126640),#66414) ;
#2992 = STYLED_ITEM('',(#126640),#66415) ;
#2993 = STYLED_ITEM('',(#126640),#66416) ;
#2994 = STYLED_ITEM('',(#126640),#66417) ;
#2995 = STYLED_ITEM('',(#126640),#66418) ;
#2996 = STYLED_ITEM('',(#126640),#66419) ;
#2997 = STYLED_ITEM('',(#126640),#66420) ;
#2998 = STYLED_ITEM('',(#126640),#66421) ;
#2999 = STYLED_ITEM('',(#126640),#66422) ;
#3000 = STYLED_ITEM('',(#126640),#66423) ;
#3001 = STYLED_ITEM('',(#126640),#66424) ;
#3002 = STYLED_ITEM('',(#126640),#66425) ;
#3003 = STYLED_ITEM('',(#126640),#66426) ;
#3004 = STYLED_ITEM('',(#126640),#66427) ;
#3005 = STYLED_ITEM('',(#126640),#66428) ;
#3006 = STYLED_ITEM('',(#126640),#66429) ;
#3007 = STYLED_ITEM('',(#126640),#66430) ;
#3008 = STYLED_ITEM('',(#126640),#66431) ;
#3009 = STYLED_ITEM('',(#126640),#66432) ;
#3010 = STYLED_ITEM('',(#126640),#66433) ;
#3011 = STYLED_ITEM('',(#126640),#66434) ;
#3012 = STYLED_ITEM('',(#126640),#66435) ;
#3013 = STYLED_ITEM('',(#126640),#66436) ;
#3014 = STYLED_ITEM('',(#126640),#66437) ;
#3015 = STYLED_ITEM('',(#126640),#66438) ;
#3016 = STYLED_ITEM('',(#126640),#66439) ;
#3017 = STYLED_ITEM('',(#126640),#66440) ;
#3018 = STYLED_ITEM('',(#126640),#66441) ;
#3019 = STYLED_ITEM('',(#126640),#66442) ;
#3020 = STYLED_ITEM('',(#126640),#66443) ;
#3021 = STYLED_ITEM('',(#126640),#66444) ;
#3022 = STYLED_ITEM('',(#126640),#66445) ;
#3023 = STYLED_ITEM('',(#126640),#66446) ;
#3024 = STYLED_ITEM('',(#126640),#66447) ;
#3025 = STYLED_ITEM('',(#126640),#66448) ;
#3026 = STYLED_ITEM('',(#126640),#66449) ;
#3027 = STYLED_ITEM('',(#126640),#66450) ;
#3028 = STYLED_ITEM('',(#126640),#66451) ;
#3029 = STYLED_ITEM('',(#126640),#66452) ;
#3030 = STYLED_ITEM('',(#126640),#66453) ;
#3031 = STYLED_ITEM('',(#126640),#66454) ;
#3032 = STYLED_ITEM('',(#126640),#66455) ;
#3033 = STYLED_ITEM('',(#126640),#66456) ;
#3034 = STYLED_ITEM('',(#126640),#66457) ;
#3035 = STYLED_ITEM('',(#126640),#66458) ;
#3036 = STYLED_ITEM('',(#126640),#66459) ;
#3037 = STYLED_ITEM('',(#126640),#66460) ;
#3038 = STYLED_ITEM('',(#126640),#66461) ;
#3039 = STYLED_ITEM('',(#126640),#66462) ;
#3040 = STYLED_ITEM('',(#126640),#66463) ;
#3041 = STYLED_ITEM('',(#126640),#66464) ;
#3042 = STYLED_ITEM('',(#126640),#66465) ;
#3043 = STYLED_ITEM('',(#126640),#66466) ;
#3044 = STYLED_ITEM('',(#126640),#66467) ;
#3045 = STYLED_ITEM('',(#126640),#66468) ;
#3046 = STYLED_ITEM('',(#126640),#66469) ;
#3047 = STYLED_ITEM('',(#126640),#66470) ;
#3048 = STYLED_ITEM('',(#126640),#66471) ;
#3049 = STYLED_ITEM('',(#126640),#66472) ;
#3050 = STYLED_ITEM('',(#126640),#66473) ;
#3051 = STYLED_ITEM('',(#126640),#66474) ;
#3052 = STYLED_ITEM('',(#126640),#66475) ;
#3053 = STYLED_ITEM('',(#126640),#66476) ;
#3054 = STYLED_ITEM('',(#126640),#66477) ;
#3055 = STYLED_ITEM('',(#126640),#66478) ;
#3056 = STYLED_ITEM('',(#126640),#66479) ;
#3057 = STYLED_ITEM('',(#126640),#66480) ;
#3058 = STYLED_ITEM('',(#126640),#66481) ;
#3059 = STYLED_ITEM('',(#126640),#66482) ;
#3060 = STYLED_ITEM('',(#126640),#66483) ;
#3061 = STYLED_ITEM('',(#126640),#66484) ;
#3062 = STYLED_ITEM('',(#126640),#66485) ;
#3063 = STYLED_ITEM('',(#126640),#66486) ;
#3064 = STYLED_ITEM('',(#126640),#66487) ;
#3065 = STYLED_ITEM('',(#126640),#66488) ;
#3066 = STYLED_ITEM('',(#126640),#66489) ;
#3067 = STYLED_ITEM('',(#126640),#66490) ;
#3068 = STYLED_ITEM('',(#126640),#66491) ;
#3069 = STYLED_ITEM('',(#126640),#66492) ;
#3070 = STYLED_ITEM('',(#126640),#66493) ;
#3071 = STYLED_ITEM('',(#126640),#66494) ;
#3072 = STYLED_ITEM('',(#126640),#66495) ;
#3073 = STYLED_ITEM('',(#126640),#66496) ;
#3074 = STYLED_ITEM('',(#126640),#66497) ;
#3075 = STYLED_ITEM('',(#126640),#66498) ;
#3076 = STYLED_ITEM('',(#126640),#66499) ;
#3077 = STYLED_ITEM('',(#126640),#66500) ;
#3078 = STYLED_ITEM('',(#126640),#66501) ;
#3079 = STYLED_ITEM('',(#126640),#66502) ;
#3080 = STYLED_ITEM('',(#126640),#66503) ;
#3081 = STYLED_ITEM('',(#126640),#66504) ;
#3082 = STYLED_ITEM('',(#126640),#66505) ;
#3083 = STYLED_ITEM('',(#126640),#66506) ;
#3084 = STYLED_ITEM('',(#126640),#66507) ;
#3085 = STYLED_ITEM('',(#126640),#66508) ;
#3086 = STYLED_ITEM('',(#126640),#66509) ;
#3087 = STYLED_ITEM('',(#126640),#66510) ;
#3088 = STYLED_ITEM('',(#126640),#66511) ;
#3089 = STYLED_ITEM('',(#126640),#66512) ;
#3090 = STYLED_ITEM('',(#126640),#66513) ;
#3091 = STYLED_ITEM('',(#126640),#66514) ;
#3092 = STYLED_ITEM('',(#126640),#66515) ;
#3093 = STYLED_ITEM('',(#126640),#66516) ;
#3094 = STYLED_ITEM('',(#126640),#66517) ;
#3095 = STYLED_ITEM('',(#126640),#66518) ;
#3096 = STYLED_ITEM('',(#126640),#66519) ;
#3097 = STYLED_ITEM('',(#126640),#66520) ;
#3098 = STYLED_ITEM('',(#126640),#66521) ;
#3099 = STYLED_ITEM('',(#126640),#66522) ;
#3100 = STYLED_ITEM('',(#126640),#66523) ;
#3101 = STYLED_ITEM('',(#126640),#66524) ;
#3102 = STYLED_ITEM('',(#126640),#66525) ;
#3103 = STYLED_ITEM('',(#126640),#66526) ;
#3104 = STYLED_ITEM('',(#126640),#66527) ;
#3105 = STYLED_ITEM('',(#126640),#66528) ;
#3106 = STYLED_ITEM('',(#126640),#66529) ;
#3107 = STYLED_ITEM('',(#126640),#66530) ;
#3108 = STYLED_ITEM('',(#126640),#66531) ;
#3109 = STYLED_ITEM('',(#126640),#66532) ;
#3110 = STYLED_ITEM('',(#126640),#66533) ;
#3111 = STYLED_ITEM('',(#126640),#66534) ;
#3112 = STYLED_ITEM('',(#126640),#66535) ;
#3113 = STYLED_ITEM('',(#126640),#66536) ;
#3114 = STYLED_ITEM('',(#126640),#66537) ;
#3115 = STYLED_ITEM('',(#126640),#66538) ;
#3116 = STYLED_ITEM('',(#126640),#66539) ;
#3117 = STYLED_ITEM('',(#126640),#66540) ;
#3118 = STYLED_ITEM('',(#126640),#66541) ;
#3119 = STYLED_ITEM('',(#126640),#66542) ;
#3120 = STYLED_ITEM('',(#126640),#66543) ;
#3121 = STYLED_ITEM('',(#126640),#66544) ;
#3122 = STYLED_ITEM('',(#126640),#66545) ;
#3123 = STYLED_ITEM('',(#126640),#66546) ;
#3124 = STYLED_ITEM('',(#126640),#66547) ;
#3125 = STYLED_ITEM('',(#126640),#66548) ;
#3126 = STYLED_ITEM('',(#126640),#66549) ;
#3127 = STYLED_ITEM('',(#126640),#66550) ;
#3128 = STYLED_ITEM('',(#126640),#66551) ;
#3129 = STYLED_ITEM('',(#126640),#66552) ;
#3130 = STYLED_ITEM('',(#126640),#66553) ;
#3131 = STYLED_ITEM('',(#126640),#66554) ;
#3132 = STYLED_ITEM('',(#126640),#66555) ;
#3133 = STYLED_ITEM('',(#126640),#66556) ;
#3134 = STYLED_ITEM('',(#126640),#66557) ;
#3135 = STYLED_ITEM('',(#126640),#66558) ;
#3136 = STYLED_ITEM('',(#126640),#66559) ;
#3137 = STYLED_ITEM('',(#126640),#66560) ;
#3138 = STYLED_ITEM('',(#126640),#66561) ;
#3139 = STYLED_ITEM('',(#126640),#66562) ;
#3140 = STYLED_ITEM('',(#126640),#66563) ;
#3141 = STYLED_ITEM('',(#126640),#66564) ;
#3142 = STYLED_ITEM('',(#126640),#66565) ;
#3143 = STYLED_ITEM('',(#126640),#66566) ;
#3144 = STYLED_ITEM('',(#126640),#66567) ;
#3145 = STYLED_ITEM('',(#126640),#66568) ;
#3146 = STYLED_ITEM('',(#126640),#66569) ;
#3147 = STYLED_ITEM('',(#126640),#66570) ;
#3148 = STYLED_ITEM('',(#126640),#66571) ;
#3149 = STYLED_ITEM('',(#126640),#66572) ;
#3150 = STYLED_ITEM('',(#126640),#66573) ;
#3151 = STYLED_ITEM('',(#126640),#66574) ;
#3152 = STYLED_ITEM('',(#126640),#66575) ;
#3153 = STYLED_ITEM('',(#126640),#66576) ;
#3154 = STYLED_ITEM('',(#126640),#66577) ;
#3155 = STYLED_ITEM('',(#126640),#66578) ;
#3156 = STYLED_ITEM('',(#126640),#66579) ;
#3157 = STYLED_ITEM('',(#126640),#66580) ;
#3158 = STYLED_ITEM('',(#126640),#66581) ;
#3159 = STYLED_ITEM('',(#126640),#66582) ;
#3160 = STYLED_ITEM('',(#126640),#66583) ;
#3161 = STYLED_ITEM('',(#126640),#66584) ;
#3162 = STYLED_ITEM('',(#126640),#66585) ;
#3163 = STYLED_ITEM('',(#126640),#66586) ;
#3164 = STYLED_ITEM('',(#126640),#66587) ;
#3165 = STYLED_ITEM('',(#126640),#66588) ;
#3166 = STYLED_ITEM('',(#126640),#66589) ;
#3167 = STYLED_ITEM('',(#126640),#66590) ;
#3168 = STYLED_ITEM('',(#126640),#66591) ;
#3169 = STYLED_ITEM('',(#126640),#66592) ;
#3170 = STYLED_ITEM('',(#126640),#66593) ;
#3171 = STYLED_ITEM('',(#126640),#66594) ;
#3172 = STYLED_ITEM('',(#126640),#66595) ;
#3173 = STYLED_ITEM('',(#126640),#66596) ;
#3174 = STYLED_ITEM('',(#126640),#66597) ;
#3175 = STYLED_ITEM('',(#126640),#66598) ;
#3176 = STYLED_ITEM('',(#126640),#66599) ;
#3177 = STYLED_ITEM('',(#126640),#66600) ;
#3178 = STYLED_ITEM('',(#126640),#66601) ;
#3179 = STYLED_ITEM('',(#126640),#66602) ;
#3180 = STYLED_ITEM('',(#126640),#66603) ;
#3181 = STYLED_ITEM('',(#126640),#66604) ;
#3182 = STYLED_ITEM('',(#126640),#66605) ;
#3183 = STYLED_ITEM('',(#126640),#66606) ;
#3184 = STYLED_ITEM('',(#126640),#66607) ;
#3185 = STYLED_ITEM('',(#126640),#66608) ;
#3186 = STYLED_ITEM('',(#126640),#66609) ;
#3187 = STYLED_ITEM('',(#126640),#66610) ;
#3188 = STYLED_ITEM('',(#126640),#66611) ;
#3189 = STYLED_ITEM('',(#126640),#66612) ;
#3190 = STYLED_ITEM('',(#126640),#66613) ;
#3191 = STYLED_ITEM('',(#126640),#66614) ;
#3192 = STYLED_ITEM('',(#126640),#66615) ;
#3193 = STYLED_ITEM('',(#126640),#66616) ;
#3194 = STYLED_ITEM('',(#126640),#66617) ;
#3195 = STYLED_ITEM('',(#126640),#66618) ;
#3196 = STYLED_ITEM('',(#126640),#66619) ;
#3197 = STYLED_ITEM('',(#126640),#66620) ;
#3198 = STYLED_ITEM('',(#126640),#66621) ;
#3199 = STYLED_ITEM('',(#126640),#66622) ;
#3200 = STYLED_ITEM('',(#126640),#66623) ;
#3201 = STYLED_ITEM('',(#126640),#66624) ;
#3202 = STYLED_ITEM('',(#126640),#66625) ;
#3203 = STYLED_ITEM('',(#126640),#66626) ;
#3204 = STYLED_ITEM('',(#126640),#66627) ;
#3205 = STYLED_ITEM('',(#126640),#66628) ;
#3206 = STYLED_ITEM('',(#126640),#66629) ;
#3207 = STYLED_ITEM('',(#126640),#66630) ;
#3208 = STYLED_ITEM('',(#126640),#66631) ;
#3209 = STYLED_ITEM('',(#126640),#66632) ;
#3210 = STYLED_ITEM('',(#126640),#66633) ;
#3211 = STYLED_ITEM('',(#126640),#66634) ;
#3212 = STYLED_ITEM('',(#126640),#66635) ;
#3213 = STYLED_ITEM('',(#126640),#66636) ;
#3214 = STYLED_ITEM('',(#126640),#66637) ;
#3215 = STYLED_ITEM('',(#126640),#66638) ;
#3216 = STYLED_ITEM('',(#126640),#66639) ;
#3217 = STYLED_ITEM('',(#126640),#66640) ;
#3218 = STYLED_ITEM('',(#126640),#66641) ;
#3219 = STYLED_ITEM('',(#126640),#66642) ;
#3220 = STYLED_ITEM('',(#126640),#66643) ;
#3221 = STYLED_ITEM('',(#126640),#66644) ;
#3222 = STYLED_ITEM('',(#126640),#66645) ;
#3223 = STYLED_ITEM('',(#126640),#66646) ;
#3224 = STYLED_ITEM('',(#126640),#66647) ;
#3225 = STYLED_ITEM('',(#126640),#66648) ;
#3226 = STYLED_ITEM('',(#126640),#66649) ;
#3227 = STYLED_ITEM('',(#126640),#66650) ;
#3228 = STYLED_ITEM('',(#126640),#66651) ;
#3229 = STYLED_ITEM('',(#126640),#66652) ;
#3230 = STYLED_ITEM('',(#126640),#66653) ;
#3231 = STYLED_ITEM('',(#126640),#66654) ;
#3232 = STYLED_ITEM('',(#126640),#66655) ;
#3233 = STYLED_ITEM('',(#126640),#66656) ;
#3234 = STYLED_ITEM('',(#126640),#66657) ;
#3235 = STYLED_ITEM('',(#126640),#66658) ;
#3236 = STYLED_ITEM('',(#126640),#66659) ;
#3237 = STYLED_ITEM('',(#126640),#66660) ;
#3238 = STYLED_ITEM('',(#126640),#66661) ;
#3239 = STYLED_ITEM('',(#126640),#66662) ;
#3240 = STYLED_ITEM('',(#126640),#66663) ;
#3241 = STYLED_ITEM('',(#126640),#66664) ;
#3242 = STYLED_ITEM('',(#126640),#66665) ;
#3243 = STYLED_ITEM('',(#126640),#66666) ;
#3244 = STYLED_ITEM('',(#126640),#66667) ;
#3245 = STYLED_ITEM('',(#126640),#66668) ;
#3246 = STYLED_ITEM('',(#126640),#66669) ;
#3247 = STYLED_ITEM('',(#126640),#66670) ;
#3248 = STYLED_ITEM('',(#126640),#66671) ;
#3249 = STYLED_ITEM('',(#126640),#66672) ;
#3250 = STYLED_ITEM('',(#126640),#66673) ;
#3251 = STYLED_ITEM('',(#126640),#66674) ;
#3252 = STYLED_ITEM('',(#126640),#66675) ;
#3253 = STYLED_ITEM('',(#126640),#66676) ;
#3254 = STYLED_ITEM('',(#126640),#66677) ;
#3255 = STYLED_ITEM('',(#126640),#66678) ;
#3256 = STYLED_ITEM('',(#126640),#66679) ;
#3257 = STYLED_ITEM('',(#126640),#66680) ;
#3258 = STYLED_ITEM('',(#126640),#66681) ;
#3259 = STYLED_ITEM('',(#126640),#66682) ;
#3260 = STYLED_ITEM('',(#126640),#66683) ;
#3261 = STYLED_ITEM('',(#126640),#66684) ;
#3262 = STYLED_ITEM('',(#126640),#66685) ;
#3263 = STYLED_ITEM('',(#126640),#66686) ;
#3264 = STYLED_ITEM('',(#126640),#66687) ;
#3265 = STYLED_ITEM('',(#126640),#66688) ;
#3266 = STYLED_ITEM('',(#126640),#66689) ;
#3267 = STYLED_ITEM('',(#126640),#66690) ;
#3268 = STYLED_ITEM('',(#126640),#66691) ;
#3269 = STYLED_ITEM('',(#126640),#66692) ;
#3270 = STYLED_ITEM('',(#126640),#66693) ;
#3271 = STYLED_ITEM('',(#126640),#66694) ;
#3272 = STYLED_ITEM('',(#126640),#66695) ;
#3273 = STYLED_ITEM('',(#126640),#66696) ;
#3274 = STYLED_ITEM('',(#126640),#66697) ;
#3275 = STYLED_ITEM('',(#126640),#66698) ;
#3276 = STYLED_ITEM('',(#126640),#66699) ;
#3277 = STYLED_ITEM('',(#126640),#66700) ;
#3278 = STYLED_ITEM('',(#126640),#66701) ;
#3279 = STYLED_ITEM('',(#126640),#66702) ;
#3280 = STYLED_ITEM('',(#126640),#66703) ;
#3281 = STYLED_ITEM('',(#126640),#66704) ;
#3282 = STYLED_ITEM('',(#126640),#66705) ;
#3283 = STYLED_ITEM('',(#126640),#66706) ;
#3284 = STYLED_ITEM('',(#126640),#66707) ;
#3285 = STYLED_ITEM('',(#126640),#66708) ;
#3286 = STYLED_ITEM('',(#126640),#66709) ;
#3287 = STYLED_ITEM('',(#126640),#66710) ;
#3288 = STYLED_ITEM('',(#126640),#66711) ;
#3289 = STYLED_ITEM('',(#126640),#66712) ;
#3290 = STYLED_ITEM('',(#126640),#66713) ;
#3291 = STYLED_ITEM('',(#126640),#66714) ;
#3292 = STYLED_ITEM('',(#126640),#66715) ;
#3293 = STYLED_ITEM('',(#126640),#66716) ;
#3294 = STYLED_ITEM('',(#126640),#66717) ;
#3295 = STYLED_ITEM('',(#126640),#66718) ;
#3296 = STYLED_ITEM('',(#126640),#66719) ;
#3297 = STYLED_ITEM('',(#126640),#66720) ;
#3298 = STYLED_ITEM('',(#126640),#66721) ;
#3299 = STYLED_ITEM('',(#126640),#66722) ;
#3300 = STYLED_ITEM('',(#126640),#66723) ;
#3301 = STYLED_ITEM('',(#126640),#66724) ;
#3302 = STYLED_ITEM('',(#126640),#66725) ;
#3303 = STYLED_ITEM('',(#126640),#66726) ;
#3304 = STYLED_ITEM('',(#126640),#66727) ;
#3305 = STYLED_ITEM('',(#126640),#66728) ;
#3306 = STYLED_ITEM('',(#126640),#66729) ;
#3307 = STYLED_ITEM('',(#126640),#66730) ;
#3308 = STYLED_ITEM('',(#126640),#66731) ;
#3309 = STYLED_ITEM('',(#126640),#66732) ;
#3310 = STYLED_ITEM('',(#126640),#66733) ;
#3311 = STYLED_ITEM('',(#126640),#66734) ;
#3312 = STYLED_ITEM('',(#126640),#66735) ;
#3313 = STYLED_ITEM('',(#126640),#66736) ;
#3314 = STYLED_ITEM('',(#126640),#66737) ;
#3315 = STYLED_ITEM('',(#126640),#66738) ;
#3316 = STYLED_ITEM('',(#126640),#66739) ;
#3317 = STYLED_ITEM('',(#126640),#66740) ;
#3318 = STYLED_ITEM('',(#126640),#66741) ;
#3319 = STYLED_ITEM('',(#126640),#66742) ;
#3320 = STYLED_ITEM('',(#126640),#66743) ;
#3321 = STYLED_ITEM('',(#126640),#66744) ;
#3322 = STYLED_ITEM('',(#126640),#66745) ;
#3323 = STYLED_ITEM('',(#126640),#66746) ;
#3324 = STYLED_ITEM('',(#126640),#66747) ;
#3325 = STYLED_ITEM('',(#126640),#66748) ;
#3326 = STYLED_ITEM('',(#126640),#66749) ;
#3327 = STYLED_ITEM('',(#126640),#66750) ;
#3328 = STYLED_ITEM('',(#126640),#66751) ;
#3329 = STYLED_ITEM('',(#126640),#66752) ;
#3330 = STYLED_ITEM('',(#126640),#66753) ;
#3331 = STYLED_ITEM('',(#126640),#66754) ;
#3332 = STYLED_ITEM('',(#126640),#66755) ;
#3333 = STYLED_ITEM('',(#126640),#66756) ;
#3334 = STYLED_ITEM('',(#126640),#66757) ;
#3335 = STYLED_ITEM('',(#126640),#66758) ;
#3336 = STYLED_ITEM('',(#126640),#66759) ;
#3337 = STYLED_ITEM('',(#126640),#66760) ;
#3338 = STYLED_ITEM('',(#126640),#66761) ;
#3339 = STYLED_ITEM('',(#126640),#66762) ;
#3340 = STYLED_ITEM('',(#126640),#66763) ;
#3341 = STYLED_ITEM('',(#126640),#66764) ;
#3342 = STYLED_ITEM('',(#126640),#66765) ;
#3343 = STYLED_ITEM('',(#126640),#66766) ;
#3344 = STYLED_ITEM('',(#126640),#66767) ;
#3345 = STYLED_ITEM('',(#126640),#66768) ;
#3346 = STYLED_ITEM('',(#126640),#66769) ;
#3347 = STYLED_ITEM('',(#126640),#66770) ;
#3348 = STYLED_ITEM('',(#126640),#66771) ;
#3349 = STYLED_ITEM('',(#126640),#66772) ;
#3350 = STYLED_ITEM('',(#126640),#66773) ;
#3351 = STYLED_ITEM('',(#126640),#66774) ;
#3352 = STYLED_ITEM('',(#126640),#66775) ;
#3353 = STYLED_ITEM('',(#126640),#66776) ;
#3354 = STYLED_ITEM('',(#126640),#66777) ;
#3355 = STYLED_ITEM('',(#126640),#66778) ;
#3356 = STYLED_ITEM('',(#126640),#66779) ;
#3357 = STYLED_ITEM('',(#126640),#66780) ;
#3358 = STYLED_ITEM('',(#126640),#66781) ;
#3359 = STYLED_ITEM('',(#126640),#66782) ;
#3360 = STYLED_ITEM('',(#126640),#66783) ;
#3361 = STYLED_ITEM('',(#126640),#66784) ;
#3362 = STYLED_ITEM('',(#126640),#66785) ;
#3363 = STYLED_ITEM('',(#126640),#66786) ;
#3364 = STYLED_ITEM('',(#126640),#66787) ;
#3365 = STYLED_ITEM('',(#126640),#66788) ;
#3366 = STYLED_ITEM('',(#126640),#66789) ;
#3367 = STYLED_ITEM('',(#126640),#66790) ;
#3368 = STYLED_ITEM('',(#126640),#66791) ;
#3369 = STYLED_ITEM('',(#126640),#66792) ;
#3370 = STYLED_ITEM('',(#126640),#66793) ;
#3371 = STYLED_ITEM('',(#126640),#66794) ;
#3372 = STYLED_ITEM('',(#126640),#66795) ;
#3373 = STYLED_ITEM('',(#126640),#66796) ;
#3374 = STYLED_ITEM('',(#126640),#66797) ;
#3375 = STYLED_ITEM('',(#126640),#66798) ;
#3376 = STYLED_ITEM('',(#126640),#66799) ;
#3377 = STYLED_ITEM('',(#126640),#66800) ;
#3378 = STYLED_ITEM('',(#126640),#66801) ;
#3379 = STYLED_ITEM('',(#126640),#66802) ;
#3380 = STYLED_ITEM('',(#126640),#66803) ;
#3381 = STYLED_ITEM('',(#126640),#66804) ;
#3382 = STYLED_ITEM('',(#126640),#66805) ;
#3383 = STYLED_ITEM('',(#126640),#66806) ;
#3384 = STYLED_ITEM('',(#126640),#66807) ;
#3385 = STYLED_ITEM('',(#126640),#66808) ;
#3386 = STYLED_ITEM('',(#126640),#66809) ;
#3387 = STYLED_ITEM('',(#126640),#66810) ;
#3388 = STYLED_ITEM('',(#126640),#66811) ;
#3389 = STYLED_ITEM('',(#126640),#66812) ;
#3390 = STYLED_ITEM('',(#126640),#66813) ;
#3391 = STYLED_ITEM('',(#126640),#66814) ;
#3392 = STYLED_ITEM('',(#126640),#66815) ;
#3393 = STYLED_ITEM('',(#126640),#66816) ;
#3394 = STYLED_ITEM('',(#126640),#66817) ;
#3395 = STYLED_ITEM('',(#126640),#66818) ;
#3396 = STYLED_ITEM('',(#126640),#66819) ;
#3397 = STYLED_ITEM('',(#126640),#66820) ;
#3398 = STYLED_ITEM('',(#126640),#66821) ;
#3399 = STYLED_ITEM('',(#126640),#66822) ;
#3400 = STYLED_ITEM('',(#126640),#66823) ;
#3401 = STYLED_ITEM('',(#126640),#66824) ;
#3402 = STYLED_ITEM('',(#126640),#66825) ;
#3403 = STYLED_ITEM('',(#126640),#66826) ;
#3404 = STYLED_ITEM('',(#126640),#66827) ;
#3405 = STYLED_ITEM('',(#126640),#66828) ;
#3406 = STYLED_ITEM('',(#126640),#66829) ;
#3407 = STYLED_ITEM('',(#126640),#66830) ;
#3408 = STYLED_ITEM('',(#126640),#66831) ;
#3409 = STYLED_ITEM('',(#126640),#66832) ;
#3410 = STYLED_ITEM('',(#126640),#66833) ;
#3411 = STYLED_ITEM('',(#126640),#66834) ;
#3412 = STYLED_ITEM('',(#126640),#66835) ;
#3413 = STYLED_ITEM('',(#126640),#66836) ;
#3414 = STYLED_ITEM('',(#126640),#66837) ;
#3415 = STYLED_ITEM('',(#126640),#66838) ;
#3416 = STYLED_ITEM('',(#126640),#66839) ;
#3417 = STYLED_ITEM('',(#126640),#66840) ;
#3418 = STYLED_ITEM('',(#126640),#66841) ;
#3419 = STYLED_ITEM('',(#126640),#66842) ;
#3420 = STYLED_ITEM('',(#126640),#66843) ;
#3421 = STYLED_ITEM('',(#126640),#66844) ;
#3422 = STYLED_ITEM('',(#126640),#66845) ;
#3423 = STYLED_ITEM('',(#126640),#66846) ;
#3424 = STYLED_ITEM('',(#126640),#66847) ;
#3425 = STYLED_ITEM('',(#126640),#66848) ;
#3426 = STYLED_ITEM('',(#126640),#66849) ;
#3427 = STYLED_ITEM('',(#126640),#66850) ;
#3428 = STYLED_ITEM('',(#126640),#66851) ;
#3429 = STYLED_ITEM('',(#126640),#66852) ;
#3430 = STYLED_ITEM('',(#126640),#66853) ;
#3431 = STYLED_ITEM('',(#126640),#66854) ;
#3432 = STYLED_ITEM('',(#126640),#66855) ;
#3433 = STYLED_ITEM('',(#126640),#66856) ;
#3434 = STYLED_ITEM('',(#126640),#66857) ;
#3435 = STYLED_ITEM('',(#126640),#66858) ;
#3436 = STYLED_ITEM('',(#126640),#66859) ;
#3437 = STYLED_ITEM('',(#126640),#66860) ;
#3438 = STYLED_ITEM('',(#126640),#66861) ;
#3439 = STYLED_ITEM('',(#126640),#66862) ;
#3440 = STYLED_ITEM('',(#126640),#66863) ;
#3441 = STYLED_ITEM('',(#126640),#66864) ;
#3442 = STYLED_ITEM('',(#126640),#66865) ;
#3443 = STYLED_ITEM('',(#126640),#66866) ;
#3444 = STYLED_ITEM('',(#126640),#66867) ;
#3445 = STYLED_ITEM('',(#126640),#66868) ;
#3446 = STYLED_ITEM('',(#126640),#66869) ;
#3447 = STYLED_ITEM('',(#126640),#66870) ;
#3448 = STYLED_ITEM('',(#126640),#66871) ;
#3449 = STYLED_ITEM('',(#126640),#66872) ;
#3450 = STYLED_ITEM('',(#126640),#66873) ;
#3451 = STYLED_ITEM('',(#126640),#66874) ;
#3452 = STYLED_ITEM('',(#126640),#66875) ;
#3453 = STYLED_ITEM('',(#126640),#66876) ;
#3454 = STYLED_ITEM('',(#126640),#66877) ;
#3455 = STYLED_ITEM('',(#126640),#66878) ;
#3456 = STYLED_ITEM('',(#126640),#66879) ;
#3457 = STYLED_ITEM('',(#126640),#66880) ;
#3458 = STYLED_ITEM('',(#126640),#66881) ;
#3459 = STYLED_ITEM('',(#126640),#66882) ;
#3460 = STYLED_ITEM('',(#126640),#66883) ;
#3461 = STYLED_ITEM('',(#126640),#66884) ;
#3462 = STYLED_ITEM('',(#126640),#66885) ;
#3463 = STYLED_ITEM('',(#126640),#66886) ;
#3464 = STYLED_ITEM('',(#126640),#66887) ;
#3465 = STYLED_ITEM('',(#126640),#66888) ;
#3466 = STYLED_ITEM('',(#126640),#66889) ;
#3467 = STYLED_ITEM('',(#126640),#66890) ;
#3468 = STYLED_ITEM('',(#126640),#66891) ;
#3469 = STYLED_ITEM('',(#126640),#66892) ;
#3470 = STYLED_ITEM('',(#126640),#66893) ;
#3471 = STYLED_ITEM('',(#126640),#66894) ;
#3472 = STYLED_ITEM('',(#126640),#66895) ;
#3473 = STYLED_ITEM('',(#126640),#66896) ;
#3474 = STYLED_ITEM('',(#126640),#66897) ;
#3475 = STYLED_ITEM('',(#126640),#66898) ;
#3476 = STYLED_ITEM('',(#126640),#66899) ;
#3477 = STYLED_ITEM('',(#126640),#66900) ;
#3478 = STYLED_ITEM('',(#126640),#66901) ;
#3479 = STYLED_ITEM('',(#126640),#66902) ;
#3480 = STYLED_ITEM('',(#126640),#66903) ;
#3481 = STYLED_ITEM('',(#126640),#66904) ;
#3482 = STYLED_ITEM('',(#126640),#66905) ;
#3483 = STYLED_ITEM('',(#126640),#66906) ;
#3484 = STYLED_ITEM('',(#126640),#66907) ;
#3485 = STYLED_ITEM('',(#126640),#66908) ;
#3486 = STYLED_ITEM('',(#126640),#66909) ;
#3487 = STYLED_ITEM('',(#126640),#66910) ;
#3488 = STYLED_ITEM('',(#126640),#66911) ;
#3489 = STYLED_ITEM('',(#126640),#66912) ;
#3490 = STYLED_ITEM('',(#126640),#66913) ;
#3491 = STYLED_ITEM('',(#126640),#66914) ;
#3492 = STYLED_ITEM('',(#126640),#66915) ;
#3493 = STYLED_ITEM('',(#126640),#66916) ;
#3494 = STYLED_ITEM('',(#126640),#66917) ;
#3495 = STYLED_ITEM('',(#126640),#66918) ;
#3496 = STYLED_ITEM('',(#126640),#66919) ;
#3497 = STYLED_ITEM('',(#126640),#66920) ;
#3498 = STYLED_ITEM('',(#126640),#66921) ;
#3499 = STYLED_ITEM('',(#126640),#66922) ;
#3500 = STYLED_ITEM('',(#126640),#66923) ;
#3501 = STYLED_ITEM('',(#126640),#66924) ;
#3502 = STYLED_ITEM('',(#126640),#66925) ;
#3503 = STYLED_ITEM('',(#126640),#66926) ;
#3504 = STYLED_ITEM('',(#126640),#66927) ;
#3505 = STYLED_ITEM('',(#126640),#66928) ;
#3506 = STYLED_ITEM('',(#126640),#66929) ;
#3507 = STYLED_ITEM('',(#126640),#66930) ;
#3508 = STYLED_ITEM('',(#126640),#66931) ;
#3509 = STYLED_ITEM('',(#126640),#66932) ;
#3510 = STYLED_ITEM('',(#126640),#66933) ;
#3511 = STYLED_ITEM('',(#126640),#66934) ;
#3512 = STYLED_ITEM('',(#126640),#66935) ;
#3513 = STYLED_ITEM('',(#126640),#66936) ;
#3514 = STYLED_ITEM('',(#126640),#66937) ;
#3515 = STYLED_ITEM('',(#126640),#66938) ;
#3516 = STYLED_ITEM('',(#126640),#66939) ;
#3517 = STYLED_ITEM('',(#126640),#66940) ;
#3518 = STYLED_ITEM('',(#126640),#66941) ;
#3519 = STYLED_ITEM('',(#126640),#66942) ;
#3520 = STYLED_ITEM('',(#126640),#66943) ;
#3521 = STYLED_ITEM('',(#126641),#66944) ;
#3522 = STYLED_ITEM('',(#126641),#66945) ;
#3523 = STYLED_ITEM('',(#126641),#66946) ;
#3524 = STYLED_ITEM('',(#126641),#66947) ;
#3525 = STYLED_ITEM('',(#126641),#66948) ;
#3526 = STYLED_ITEM('',(#126641),#66949) ;
#3527 = STYLED_ITEM('',(#126641),#66950) ;
#3528 = STYLED_ITEM('',(#126641),#66951) ;
#3529 = STYLED_ITEM('',(#126641),#66952) ;
#3530 = STYLED_ITEM('',(#126641),#66953) ;
#3531 = STYLED_ITEM('',(#126641),#66954) ;
#3532 = STYLED_ITEM('',(#126641),#66955) ;
#3533 = STYLED_ITEM('',(#126641),#66956) ;
#3534 = STYLED_ITEM('',(#126641),#66957) ;
#3535 = STYLED_ITEM('',(#126641),#66958) ;
#3536 = STYLED_ITEM('',(#126641),#66959) ;
#3537 = STYLED_ITEM('',(#126641),#66960) ;
#3538 = STYLED_ITEM('',(#126641),#66961) ;
#3539 = STYLED_ITEM('',(#126641),#66962) ;
#3540 = STYLED_ITEM('',(#126641),#66963) ;
#3541 = STYLED_ITEM('',(#126641),#66964) ;
#3542 = STYLED_ITEM('',(#126641),#66965) ;
#3543 = STYLED_ITEM('',(#126641),#66966) ;
#3544 = STYLED_ITEM('',(#126641),#66967) ;
#3545 = STYLED_ITEM('',(#126641),#66968) ;
#3546 = STYLED_ITEM('',(#126641),#66969) ;
#3547 = STYLED_ITEM('',(#126641),#66970) ;
#3548 = STYLED_ITEM('',(#126641),#66971) ;
#3549 = STYLED_ITEM('',(#126641),#66972) ;
#3550 = STYLED_ITEM('',(#126641),#66973) ;
#3551 = STYLED_ITEM('',(#126641),#66974) ;
#3552 = STYLED_ITEM('',(#126641),#66975) ;
#3553 = STYLED_ITEM('',(#126641),#66976) ;
#3554 = STYLED_ITEM('',(#126641),#66977) ;
#3555 = STYLED_ITEM('',(#126641),#66978) ;
#3556 = STYLED_ITEM('',(#126641),#66979) ;
#3557 = STYLED_ITEM('',(#126641),#66980) ;
#3558 = STYLED_ITEM('',(#126641),#66981) ;
#3559 = STYLED_ITEM('',(#126641),#66982) ;
#3560 = STYLED_ITEM('',(#126641),#66983) ;
#3561 = STYLED_ITEM('',(#126641),#66984) ;
#3562 = STYLED_ITEM('',(#126641),#66985) ;
#3563 = STYLED_ITEM('',(#126641),#66986) ;
#3564 = STYLED_ITEM('',(#126641),#66987) ;
#3565 = STYLED_ITEM('',(#126641),#66988) ;
#3566 = STYLED_ITEM('',(#126641),#66989) ;
#3567 = STYLED_ITEM('',(#126641),#66990) ;
#3568 = STYLED_ITEM('',(#126641),#66991) ;
#3569 = STYLED_ITEM('',(#126641),#66992) ;
#3570 = STYLED_ITEM('',(#126641),#66993) ;
#3571 = STYLED_ITEM('',(#126641),#66994) ;
#3572 = STYLED_ITEM('',(#126641),#66995) ;
#3573 = STYLED_ITEM('',(#126641),#66996) ;
#3574 = STYLED_ITEM('',(#126641),#66997) ;
#3575 = STYLED_ITEM('',(#126641),#66998) ;
#3576 = STYLED_ITEM('',(#126641),#66999) ;
#3577 = STYLED_ITEM('',(#126641),#67000) ;
#3578 = STYLED_ITEM('',(#126641),#67001) ;
#3579 = STYLED_ITEM('',(#126641),#67002) ;
#3580 = STYLED_ITEM('',(#126641),#67003) ;
#3581 = STYLED_ITEM('',(#126641),#67004) ;
#3582 = STYLED_ITEM('',(#126641),#67005) ;
#3583 = STYLED_ITEM('',(#126641),#67006) ;
#3584 = STYLED_ITEM('',(#126641),#67007) ;
#3585 = STYLED_ITEM('',(#126641),#67008) ;
#3586 = STYLED_ITEM('',(#126641),#67009) ;
#3587 = STYLED_ITEM('',(#126641),#67010) ;
#3588 = STYLED_ITEM('',(#126641),#67011) ;
#3589 = STYLED_ITEM('',(#126641),#67012) ;
#3590 = STYLED_ITEM('',(#126641),#67013) ;
#3591 = STYLED_ITEM('',(#126641),#67014) ;
#3592 = STYLED_ITEM('',(#126641),#67015) ;
#3593 = STYLED_ITEM('',(#126641),#67016) ;
#3594 = STYLED_ITEM('',(#126641),#67017) ;
#3595 = STYLED_ITEM('',(#126641),#67018) ;
#3596 = STYLED_ITEM('',(#126641),#67019) ;
#3597 = STYLED_ITEM('',(#126641),#67020) ;
#3598 = STYLED_ITEM('',(#126641),#67021) ;
#3599 = STYLED_ITEM('',(#126641),#67022) ;
#3600 = STYLED_ITEM('',(#126641),#67023) ;
#3601 = STYLED_ITEM('',(#126641),#67024) ;
#3602 = STYLED_ITEM('',(#126641),#67025) ;
#3603 = STYLED_ITEM('',(#126641),#67026) ;
#3604 = STYLED_ITEM('',(#126641),#67027) ;
#3605 = STYLED_ITEM('',(#126641),#67028) ;
#3606 = STYLED_ITEM('',(#126641),#67029) ;
#3607 = STYLED_ITEM('',(#126641),#67030) ;
#3608 = STYLED_ITEM('',(#126641),#67031) ;
#3609 = STYLED_ITEM('',(#126641),#67032) ;
#3610 = STYLED_ITEM('',(#126641),#67033) ;
#3611 = STYLED_ITEM('',(#126641),#67034) ;
#3612 = STYLED_ITEM('',(#126641),#67035) ;
#3613 = STYLED_ITEM('',(#126641),#67036) ;
#3614 = STYLED_ITEM('',(#126641),#67037) ;
#3615 = STYLED_ITEM('',(#126641),#67038) ;
#3616 = STYLED_ITEM('',(#126641),#67039) ;
#3617 = STYLED_ITEM('',(#126641),#67040) ;
#3618 = STYLED_ITEM('',(#126641),#67041) ;
#3619 = STYLED_ITEM('',(#126641),#67042) ;
#3620 = STYLED_ITEM('',(#126641),#67043) ;
#3621 = STYLED_ITEM('',(#126641),#67044) ;
#3622 = STYLED_ITEM('',(#126641),#67045) ;
#3623 = STYLED_ITEM('',(#126641),#67046) ;
#3624 = STYLED_ITEM('',(#126641),#67047) ;
#3625 = STYLED_ITEM('',(#126641),#67048) ;
#3626 = STYLED_ITEM('',(#126641),#67049) ;
#3627 = STYLED_ITEM('',(#126641),#67050) ;
#3628 = STYLED_ITEM('',(#126641),#67051) ;
#3629 = STYLED_ITEM('',(#126641),#67052) ;
#3630 = STYLED_ITEM('',(#126641),#67053) ;
#3631 = STYLED_ITEM('',(#126641),#67054) ;
#3632 = STYLED_ITEM('',(#126641),#67055) ;
#3633 = STYLED_ITEM('',(#126641),#67056) ;
#3634 = STYLED_ITEM('',(#126641),#67057) ;
#3635 = STYLED_ITEM('',(#126641),#67058) ;
#3636 = STYLED_ITEM('',(#126641),#67059) ;
#3637 = STYLED_ITEM('',(#126641),#67060) ;
#3638 = STYLED_ITEM('',(#126641),#67061) ;
#3639 = STYLED_ITEM('',(#126641),#67062) ;
#3640 = STYLED_ITEM('',(#126641),#67063) ;
#3641 = STYLED_ITEM('',(#126641),#67064) ;
#3642 = STYLED_ITEM('',(#126641),#67065) ;
#3643 = STYLED_ITEM('',(#126641),#67066) ;
#3644 = STYLED_ITEM('',(#126641),#67067) ;
#3645 = STYLED_ITEM('',(#126641),#67068) ;
#3646 = STYLED_ITEM('',(#126641),#67069) ;
#3647 = STYLED_ITEM('',(#126641),#67070) ;
#3648 = STYLED_ITEM('',(#126641),#67071) ;
#3649 = STYLED_ITEM('',(#126641),#67072) ;
#3650 = STYLED_ITEM('',(#126641),#67073) ;
#3651 = STYLED_ITEM('',(#126641),#67074) ;
#3652 = STYLED_ITEM('',(#126641),#67075) ;
#3653 = STYLED_ITEM('',(#126641),#67076) ;
#3654 = STYLED_ITEM('',(#126641),#67077) ;
#3655 = STYLED_ITEM('',(#126641),#67078) ;
#3656 = STYLED_ITEM('',(#126641),#67079) ;
#3657 = STYLED_ITEM('',(#126641),#67080) ;
#3658 = STYLED_ITEM('',(#126641),#67081) ;
#3659 = STYLED_ITEM('',(#126641),#67082) ;
#3660 = STYLED_ITEM('',(#126641),#67083) ;
#3661 = STYLED_ITEM('',(#126641),#67084) ;
#3662 = STYLED_ITEM('',(#126641),#67085) ;
#3663 = STYLED_ITEM('',(#126641),#67086) ;
#3664 = STYLED_ITEM('',(#126641),#67087) ;
#3665 = STYLED_ITEM('',(#126641),#67088) ;
#3666 = STYLED_ITEM('',(#126641),#67089) ;
#3667 = STYLED_ITEM('',(#126641),#67090) ;
#3668 = STYLED_ITEM('',(#126641),#67091) ;
#3669 = STYLED_ITEM('',(#126641),#67092) ;
#3670 = STYLED_ITEM('',(#126641),#67093) ;
#3671 = STYLED_ITEM('',(#126641),#67094) ;
#3672 = STYLED_ITEM('',(#126641),#67095) ;
#3673 = STYLED_ITEM('',(#126641),#67096) ;
#3674 = STYLED_ITEM('',(#126641),#67097) ;
#3675 = STYLED_ITEM('',(#126641),#67098) ;
#3676 = STYLED_ITEM('',(#126641),#67099) ;
#3677 = STYLED_ITEM('',(#126641),#67100) ;
#3678 = STYLED_ITEM('',(#126641),#67101) ;
#3679 = STYLED_ITEM('',(#126641),#67102) ;
#3680 = STYLED_ITEM('',(#126641),#67103) ;
#3681 = STYLED_ITEM('',(#126641),#67104) ;
#3682 = STYLED_ITEM('',(#126641),#67105) ;
#3683 = STYLED_ITEM('',(#126641),#67106) ;
#3684 = STYLED_ITEM('',(#126641),#67107) ;
#3685 = STYLED_ITEM('',(#126641),#67108) ;
#3686 = STYLED_ITEM('',(#126641),#67109) ;
#3687 = STYLED_ITEM('',(#126641),#67110) ;
#3688 = STYLED_ITEM('',(#126641),#67111) ;
#3689 = STYLED_ITEM('',(#126641),#67112) ;
#3690 = STYLED_ITEM('',(#126641),#67113) ;
#3691 = STYLED_ITEM('',(#126641),#67114) ;
#3692 = STYLED_ITEM('',(#126641),#67115) ;
#3693 = STYLED_ITEM('',(#126641),#67116) ;
#3694 = STYLED_ITEM('',(#126641),#67117) ;
#3695 = STYLED_ITEM('',(#126641),#67118) ;
#3696 = STYLED_ITEM('',(#126641),#67119) ;
#3697 = STYLED_ITEM('',(#126641),#67120) ;
#3698 = STYLED_ITEM('',(#126641),#67121) ;
#3699 = STYLED_ITEM('',(#126641),#67122) ;
#3700 = STYLED_ITEM('',(#126641),#67123) ;
#3701 = STYLED_ITEM('',(#126641),#67124) ;
#3702 = STYLED_ITEM('',(#126641),#67125) ;
#3703 = STYLED_ITEM('',(#126641),#67126) ;
#3704 = STYLED_ITEM('',(#126641),#67127) ;
#3705 = STYLED_ITEM('',(#126641),#67128) ;
#3706 = STYLED_ITEM('',(#126641),#67129) ;
#3707 = STYLED_ITEM('',(#126641),#67130) ;
#3708 = STYLED_ITEM('',(#126641),#67131) ;
#3709 = STYLED_ITEM('',(#126641),#67132) ;
#3710 = STYLED_ITEM('',(#126641),#67133) ;
#3711 = STYLED_ITEM('',(#126641),#67134) ;
#3712 = STYLED_ITEM('',(#126641),#67135) ;
#3713 = STYLED_ITEM('',(#126641),#67136) ;
#3714 = STYLED_ITEM('',(#126641),#67137) ;
#3715 = STYLED_ITEM('',(#126641),#67138) ;
#3716 = STYLED_ITEM('',(#126641),#67139) ;
#3717 = STYLED_ITEM('',(#126641),#67140) ;
#3718 = STYLED_ITEM('',(#126641),#67141) ;
#3719 = STYLED_ITEM('',(#126641),#67142) ;
#3720 = STYLED_ITEM('',(#126641),#67143) ;
#3721 = STYLED_ITEM('',(#126641),#67144) ;
#3722 = STYLED_ITEM('',(#126641),#67145) ;
#3723 = STYLED_ITEM('',(#126641),#67146) ;
#3724 = STYLED_ITEM('',(#126641),#67147) ;
#3725 = STYLED_ITEM('',(#126641),#67148) ;
#3726 = STYLED_ITEM('',(#126641),#67149) ;
#3727 = STYLED_ITEM('',(#126641),#67150) ;
#3728 = STYLED_ITEM('',(#126641),#67151) ;
#3729 = STYLED_ITEM('',(#126641),#67152) ;
#3730 = STYLED_ITEM('',(#126641),#67153) ;
#3731 = STYLED_ITEM('',(#126641),#67154) ;
#3732 = STYLED_ITEM('',(#126641),#67155) ;
#3733 = STYLED_ITEM('',(#126641),#67156) ;
#3734 = STYLED_ITEM('',(#126641),#67157) ;
#3735 = STYLED_ITEM('',(#126641),#67158) ;
#3736 = STYLED_ITEM('',(#126641),#67159) ;
#3737 = STYLED_ITEM('',(#126641),#67160) ;
#3738 = STYLED_ITEM('',(#126641),#67161) ;
#3739 = STYLED_ITEM('',(#126641),#67162) ;
#3740 = STYLED_ITEM('',(#126641),#67163) ;
#3741 = STYLED_ITEM('',(#126641),#67164) ;
#3742 = STYLED_ITEM('',(#126641),#67165) ;
#3743 = STYLED_ITEM('',(#126641),#67166) ;
#3744 = STYLED_ITEM('',(#126641),#67167) ;
#3745 = STYLED_ITEM('',(#126641),#67168) ;
#3746 = STYLED_ITEM('',(#126641),#67169) ;
#3747 = STYLED_ITEM('',(#126641),#67170) ;
#3748 = STYLED_ITEM('',(#126641),#67171) ;
#3749 = STYLED_ITEM('',(#126641),#67172) ;
#3750 = STYLED_ITEM('',(#126641),#67173) ;
#3751 = STYLED_ITEM('',(#126641),#67174) ;
#3752 = STYLED_ITEM('',(#126641),#67175) ;
#3753 = STYLED_ITEM('',(#126641),#67176) ;
#3754 = STYLED_ITEM('',(#126641),#67177) ;
#3755 = STYLED_ITEM('',(#126641),#67178) ;
#3756 = STYLED_ITEM('',(#126641),#67179) ;
#3757 = STYLED_ITEM('',(#126641),#67180) ;
#3758 = STYLED_ITEM('',(#126641),#67181) ;
#3759 = STYLED_ITEM('',(#126641),#67182) ;
#3760 = STYLED_ITEM('',(#126641),#67183) ;
#3761 = STYLED_ITEM('',(#126641),#67184) ;
#3762 = STYLED_ITEM('',(#126641),#67185) ;
#3763 = STYLED_ITEM('',(#126641),#67186) ;
#3764 = STYLED_ITEM('',(#126641),#67187) ;
#3765 = STYLED_ITEM('',(#126641),#67188) ;
#3766 = STYLED_ITEM('',(#126641),#67189) ;
#3767 = STYLED_ITEM('',(#126641),#67190) ;
#3768 = STYLED_ITEM('',(#126641),#67191) ;
#3769 = STYLED_ITEM('',(#126641),#67192) ;
#3770 = STYLED_ITEM('',(#126641),#67193) ;
#3771 = STYLED_ITEM('',(#126641),#67194) ;
#3772 = STYLED_ITEM('',(#126641),#67195) ;
#3773 = STYLED_ITEM('',(#126641),#67196) ;
#3774 = STYLED_ITEM('',(#126641),#67197) ;
#3775 = STYLED_ITEM('',(#126641),#67198) ;
#3776 = STYLED_ITEM('',(#126641),#67199) ;
#3777 = STYLED_ITEM('',(#126641),#67200) ;
#3778 = STYLED_ITEM('',(#126641),#67201) ;
#3779 = STYLED_ITEM('',(#126641),#67202) ;
#3780 = STYLED_ITEM('',(#126641),#67203) ;
#3781 = STYLED_ITEM('',(#126641),#67204) ;
#3782 = STYLED_ITEM('',(#126641),#67205) ;
#3783 = STYLED_ITEM('',(#126641),#67206) ;
#3784 = STYLED_ITEM('',(#126641),#67207) ;
#3785 = STYLED_ITEM('',(#126641),#67208) ;
#3786 = STYLED_ITEM('',(#126641),#67209) ;
#3787 = STYLED_ITEM('',(#126641),#67210) ;
#3788 = STYLED_ITEM('',(#126641),#67211) ;
#3789 = STYLED_ITEM('',(#126641),#67212) ;
#3790 = STYLED_ITEM('',(#126641),#67213) ;
#3791 = STYLED_ITEM('',(#126641),#67214) ;
#3792 = STYLED_ITEM('',(#126641),#67215) ;
#3793 = STYLED_ITEM('',(#126641),#67216) ;
#3794 = STYLED_ITEM('',(#126641),#67217) ;
#3795 = STYLED_ITEM('',(#126641),#67218) ;
#3796 = STYLED_ITEM('',(#126641),#67219) ;
#3797 = STYLED_ITEM('',(#126641),#67220) ;
#3798 = STYLED_ITEM('',(#126641),#67221) ;
#3799 = STYLED_ITEM('',(#126641),#67222) ;
#3800 = STYLED_ITEM('',(#126641),#67223) ;
#3801 = STYLED_ITEM('',(#126641),#67224) ;
#3802 = STYLED_ITEM('',(#126641),#67225) ;
#3803 = STYLED_ITEM('',(#126641),#67226) ;
#3804 = STYLED_ITEM('',(#126641),#67227) ;
#3805 = STYLED_ITEM('',(#126641),#67228) ;
#3806 = STYLED_ITEM('',(#126641),#67229) ;
#3807 = STYLED_ITEM('',(#126641),#67230) ;
#3808 = STYLED_ITEM('',(#126641),#67231) ;
#3809 = STYLED_ITEM('',(#126641),#67232) ;
#3810 = STYLED_ITEM('',(#126641),#67233) ;
#3811 = STYLED_ITEM('',(#126641),#67234) ;
#3812 = STYLED_ITEM('',(#126641),#67235) ;
#3813 = STYLED_ITEM('',(#126641),#67236) ;
#3814 = STYLED_ITEM('',(#126641),#67237) ;
#3815 = STYLED_ITEM('',(#126641),#67238) ;
#3816 = STYLED_ITEM('',(#126641),#67239) ;
#3817 = STYLED_ITEM('',(#126641),#67240) ;
#3818 = STYLED_ITEM('',(#126641),#67241) ;
#3819 = STYLED_ITEM('',(#126641),#67242) ;
#3820 = STYLED_ITEM('',(#126641),#67243) ;
#3821 = STYLED_ITEM('',(#126641),#67244) ;
#3822 = STYLED_ITEM('',(#126641),#67245) ;
#3823 = STYLED_ITEM('',(#126641),#67246) ;
#3824 = STYLED_ITEM('',(#126641),#67247) ;
#3825 = STYLED_ITEM('',(#126641),#67248) ;
#3826 = STYLED_ITEM('',(#126641),#67249) ;
#3827 = STYLED_ITEM('',(#126641),#67250) ;
#3828 = STYLED_ITEM('',(#126641),#67251) ;
#3829 = STYLED_ITEM('',(#126641),#67252) ;
#3830 = STYLED_ITEM('',(#126641),#67253) ;
#3831 = STYLED_ITEM('',(#126641),#67254) ;
#3832 = STYLED_ITEM('',(#126641),#67255) ;
#3833 = STYLED_ITEM('',(#126641),#67256) ;
#3834 = STYLED_ITEM('',(#126641),#67257) ;
#3835 = STYLED_ITEM('',(#126641),#67258) ;
#3836 = STYLED_ITEM('',(#126641),#67259) ;
#3837 = STYLED_ITEM('',(#126641),#67260) ;
#3838 = STYLED_ITEM('',(#126641),#67261) ;
#3839 = STYLED_ITEM('',(#126641),#67262) ;
#3840 = STYLED_ITEM('',(#126641),#67263) ;
#3841 = STYLED_ITEM('',(#126641),#67264) ;
#3842 = STYLED_ITEM('',(#126641),#67265) ;
#3843 = STYLED_ITEM('',(#126641),#67266) ;
#3844 = STYLED_ITEM('',(#126641),#67267) ;
#3845 = STYLED_ITEM('',(#126641),#67268) ;
#3846 = STYLED_ITEM('',(#126641),#67269) ;
#3847 = STYLED_ITEM('',(#126641),#67270) ;
#3848 = STYLED_ITEM('',(#126641),#67271) ;
#3849 = STYLED_ITEM('',(#126641),#67272) ;
#3850 = STYLED_ITEM('',(#126641),#67273) ;
#3851 = STYLED_ITEM('',(#126641),#67274) ;
#3852 = STYLED_ITEM('',(#126641),#67275) ;
#3853 = STYLED_ITEM('',(#126641),#67276) ;
#3854 = STYLED_ITEM('',(#126641),#67277) ;
#3855 = STYLED_ITEM('',(#126641),#67278) ;
#3856 = STYLED_ITEM('',(#126641),#67279) ;
#3857 = STYLED_ITEM('',(#126641),#67280) ;
#3858 = STYLED_ITEM('',(#126641),#67281) ;
#3859 = STYLED_ITEM('',(#126641),#67282) ;
#3860 = STYLED_ITEM('',(#126641),#67283) ;
#3861 = STYLED_ITEM('',(#126641),#67284) ;
#3862 = STYLED_ITEM('',(#126641),#67285) ;
#3863 = STYLED_ITEM('',(#126641),#67286) ;
#3864 = STYLED_ITEM('',(#126641),#67287) ;
#3865 = STYLED_ITEM('',(#126641),#67288) ;
#3866 = STYLED_ITEM('',(#126641),#67289) ;
#3867 = STYLED_ITEM('',(#126641),#67290) ;
#3868 = STYLED_ITEM('',(#126641),#67291) ;
#3869 = STYLED_ITEM('',(#126641),#67292) ;
#3870 = STYLED_ITEM('',(#126641),#67293) ;
#3871 = STYLED_ITEM('',(#126641),#67294) ;
#3872 = STYLED_ITEM('',(#126641),#67295) ;
#3873 = STYLED_ITEM('',(#126641),#67296) ;
#3874 = STYLED_ITEM('',(#126641),#67297) ;
#3875 = STYLED_ITEM('',(#126641),#67298) ;
#3876 = STYLED_ITEM('',(#126641),#67299) ;
#3877 = STYLED_ITEM('',(#126641),#67300) ;
#3878 = STYLED_ITEM('',(#126641),#67301) ;
#3879 = STYLED_ITEM('',(#126641),#67302) ;
#3880 = STYLED_ITEM('',(#126641),#67303) ;
#3881 = STYLED_ITEM('',(#126641),#67304) ;
#3882 = STYLED_ITEM('',(#126641),#67305) ;
#3883 = STYLED_ITEM('',(#126641),#67306) ;
#3884 = STYLED_ITEM('',(#126641),#67307) ;
#3885 = STYLED_ITEM('',(#126641),#67308) ;
#3886 = STYLED_ITEM('',(#126641),#67309) ;
#3887 = STYLED_ITEM('',(#126641),#67310) ;
#3888 = STYLED_ITEM('',(#126641),#67311) ;
#3889 = STYLED_ITEM('',(#126641),#67312) ;
#3890 = STYLED_ITEM('',(#126641),#67313) ;
#3891 = STYLED_ITEM('',(#126641),#67314) ;
#3892 = STYLED_ITEM('',(#126641),#67315) ;
#3893 = STYLED_ITEM('',(#126641),#67316) ;
#3894 = STYLED_ITEM('',(#126641),#67317) ;
#3895 = STYLED_ITEM('',(#126641),#67318) ;
#3896 = STYLED_ITEM('',(#126641),#67319) ;
#3897 = STYLED_ITEM('',(#126641),#67320) ;
#3898 = STYLED_ITEM('',(#126641),#67321) ;
#3899 = STYLED_ITEM('',(#126641),#67322) ;
#3900 = STYLED_ITEM('',(#126641),#67323) ;
#3901 = STYLED_ITEM('',(#126641),#67324) ;
#3902 = STYLED_ITEM('',(#126641),#67325) ;
#3903 = STYLED_ITEM('',(#126641),#67326) ;
#3904 = STYLED_ITEM('',(#126641),#67327) ;
#3905 = STYLED_ITEM('',(#126641),#67328) ;
#3906 = STYLED_ITEM('',(#126641),#67329) ;
#3907 = STYLED_ITEM('',(#126641),#67330) ;
#3908 = STYLED_ITEM('',(#126641),#67331) ;
#3909 = STYLED_ITEM('',(#126641),#67332) ;
#3910 = STYLED_ITEM('',(#126641),#67333) ;
#3911 = STYLED_ITEM('',(#126641),#67334) ;
#3912 = STYLED_ITEM('',(#126641),#67335) ;
#3913 = STYLED_ITEM('',(#126641),#67336) ;
#3914 = STYLED_ITEM('',(#126641),#67337) ;
#3915 = STYLED_ITEM('',(#126641),#67338) ;
#3916 = STYLED_ITEM('',(#126641),#67339) ;
#3917 = STYLED_ITEM('',(#126641),#67340) ;
#3918 = STYLED_ITEM('',(#126641),#67341) ;
#3919 = STYLED_ITEM('',(#126641),#67342) ;
#3920 = STYLED_ITEM('',(#126641),#67343) ;
#3921 = STYLED_ITEM('',(#126641),#67344) ;
#3922 = STYLED_ITEM('',(#126641),#67345) ;
#3923 = STYLED_ITEM('',(#126641),#67346) ;
#3924 = STYLED_ITEM('',(#126641),#67347) ;
#3925 = STYLED_ITEM('',(#126641),#67348) ;
#3926 = STYLED_ITEM('',(#126641),#67349) ;
#3927 = STYLED_ITEM('',(#126641),#67350) ;
#3928 = STYLED_ITEM('',(#126641),#67351) ;
#3929 = STYLED_ITEM('',(#126641),#67352) ;
#3930 = STYLED_ITEM('',(#126641),#67353) ;
#3931 = STYLED_ITEM('',(#126641),#67354) ;
#3932 = STYLED_ITEM('',(#126641),#67355) ;
#3933 = STYLED_ITEM('',(#126641),#67356) ;
#3934 = STYLED_ITEM('',(#126641),#67357) ;
#3935 = STYLED_ITEM('',(#126641),#67358) ;
#3936 = STYLED_ITEM('',(#126641),#67359) ;
#3937 = STYLED_ITEM('',(#126641),#67360) ;
#3938 = STYLED_ITEM('',(#126641),#67361) ;
#3939 = STYLED_ITEM('',(#126641),#67362) ;
#3940 = STYLED_ITEM('',(#126641),#67363) ;
#3941 = STYLED_ITEM('',(#126641),#67364) ;
#3942 = STYLED_ITEM('',(#126641),#67365) ;
#3943 = STYLED_ITEM('',(#126641),#67366) ;
#3944 = STYLED_ITEM('',(#126641),#67367) ;
#3945 = STYLED_ITEM('',(#126641),#67368) ;
#3946 = STYLED_ITEM('',(#126641),#67369) ;
#3947 = STYLED_ITEM('',(#126641),#67370) ;
#3948 = STYLED_ITEM('',(#126641),#67371) ;
#3949 = STYLED_ITEM('',(#126641),#67372) ;
#3950 = STYLED_ITEM('',(#126641),#67373) ;
#3951 = STYLED_ITEM('',(#126641),#67374) ;
#3952 = STYLED_ITEM('',(#126641),#67375) ;
#3953 = STYLED_ITEM('',(#126641),#67376) ;
#3954 = STYLED_ITEM('',(#126641),#67377) ;
#3955 = STYLED_ITEM('',(#126641),#67378) ;
#3956 = STYLED_ITEM('',(#126641),#67379) ;
#3957 = STYLED_ITEM('',(#126641),#67380) ;
#3958 = STYLED_ITEM('',(#126641),#67381) ;
#3959 = STYLED_ITEM('',(#126641),#67382) ;
#3960 = STYLED_ITEM('',(#126641),#67383) ;
#3961 = STYLED_ITEM('',(#126641),#67384) ;
#3962 = STYLED_ITEM('',(#126641),#67385) ;
#3963 = STYLED_ITEM('',(#126641),#67386) ;
#3964 = STYLED_ITEM('',(#126641),#67387) ;
#3965 = STYLED_ITEM('',(#126641),#67388) ;
#3966 = STYLED_ITEM('',(#126641),#67389) ;
#3967 = STYLED_ITEM('',(#126641),#67390) ;
#3968 = STYLED_ITEM('',(#126641),#67391) ;
#3969 = STYLED_ITEM('',(#126641),#67392) ;
#3970 = STYLED_ITEM('',(#126641),#67393) ;
#3971 = STYLED_ITEM('',(#126641),#67394) ;
#3972 = STYLED_ITEM('',(#126641),#67395) ;
#3973 = STYLED_ITEM('',(#126641),#67396) ;
#3974 = STYLED_ITEM('',(#126641),#67397) ;
#3975 = STYLED_ITEM('',(#126641),#67398) ;
#3976 = STYLED_ITEM('',(#126641),#67399) ;
#3977 = STYLED_ITEM('',(#126641),#67400) ;
#3978 = STYLED_ITEM('',(#126641),#67401) ;
#3979 = STYLED_ITEM('',(#126641),#67402) ;
#3980 = STYLED_ITEM('',(#126641),#67403) ;
#3981 = STYLED_ITEM('',(#126641),#67404) ;
#3982 = STYLED_ITEM('',(#126641),#67405) ;
#3983 = STYLED_ITEM('',(#126641),#67406) ;
#3984 = STYLED_ITEM('',(#126641),#67407) ;
#3985 = STYLED_ITEM('',(#126641),#67408) ;
#3986 = STYLED_ITEM('',(#126641),#67409) ;
#3987 = STYLED_ITEM('',(#126641),#67410) ;
#3988 = STYLED_ITEM('',(#126641),#67411) ;
#3989 = STYLED_ITEM('',(#126641),#67412) ;
#3990 = STYLED_ITEM('',(#126641),#67413) ;
#3991 = STYLED_ITEM('',(#126641),#67414) ;
#3992 = STYLED_ITEM('',(#126641),#67415) ;
#3993 = STYLED_ITEM('',(#126641),#67416) ;
#3994 = STYLED_ITEM('',(#126641),#67417) ;
#3995 = STYLED_ITEM('',(#126641),#67418) ;
#3996 = STYLED_ITEM('',(#126641),#67419) ;
#3997 = STYLED_ITEM('',(#126641),#67420) ;
#3998 = STYLED_ITEM('',(#126641),#67421) ;
#3999 = STYLED_ITEM('',(#126641),#67422) ;
#4000 = STYLED_ITEM('',(#126641),#67423) ;
#4001 = STYLED_ITEM('',(#126641),#67424) ;
#4002 = STYLED_ITEM('',(#126641),#67425) ;
#4003 = STYLED_ITEM('',(#126641),#67426) ;
#4004 = STYLED_ITEM('',(#126641),#67427) ;
#4005 = STYLED_ITEM('',(#126641),#67428) ;
#4006 = STYLED_ITEM('',(#126641),#67429) ;
#4007 = STYLED_ITEM('',(#126641),#67430) ;
#4008 = STYLED_ITEM('',(#126641),#67431) ;
#4009 = STYLED_ITEM('',(#126641),#67432) ;
#4010 = STYLED_ITEM('',(#126641),#67433) ;
#4011 = STYLED_ITEM('',(#126641),#67434) ;
#4012 = STYLED_ITEM('',(#126641),#67435) ;
#4013 = STYLED_ITEM('',(#126641),#67436) ;
#4014 = STYLED_ITEM('',(#126641),#67437) ;
#4015 = STYLED_ITEM('',(#126641),#67438) ;
#4016 = STYLED_ITEM('',(#126641),#67439) ;
#4017 = STYLED_ITEM('',(#126641),#67440) ;
#4018 = STYLED_ITEM('',(#126641),#67441) ;
#4019 = STYLED_ITEM('',(#126641),#67442) ;
#4020 = STYLED_ITEM('',(#126641),#67443) ;
#4021 = STYLED_ITEM('',(#126641),#67444) ;
#4022 = STYLED_ITEM('',(#126641),#67445) ;
#4023 = STYLED_ITEM('',(#126641),#67446) ;
#4024 = STYLED_ITEM('',(#126641),#67447) ;
#4025 = STYLED_ITEM('',(#126641),#67448) ;
#4026 = STYLED_ITEM('',(#126641),#67449) ;
#4027 = STYLED_ITEM('',(#126641),#67450) ;
#4028 = STYLED_ITEM('',(#126641),#67451) ;
#4029 = STYLED_ITEM('',(#126641),#67452) ;
#4030 = STYLED_ITEM('',(#126641),#67453) ;
#4031 = STYLED_ITEM('',(#126641),#67454) ;
#4032 = STYLED_ITEM('',(#126641),#67455) ;
#4033 = STYLED_ITEM('',(#126641),#67456) ;
#4034 = STYLED_ITEM('',(#126641),#67457) ;
#4035 = STYLED_ITEM('',(#126641),#67458) ;
#4036 = STYLED_ITEM('',(#126641),#67459) ;
#4037 = STYLED_ITEM('',(#126641),#67460) ;
#4038 = STYLED_ITEM('',(#126641),#67461) ;
#4039 = STYLED_ITEM('',(#126641),#67462) ;
#4040 = STYLED_ITEM('',(#126641),#67463) ;
#4041 = STYLED_ITEM('',(#126641),#67464) ;
#4042 = STYLED_ITEM('',(#126641),#67465) ;
#4043 = STYLED_ITEM('',(#126641),#67466) ;
#4044 = STYLED_ITEM('',(#126641),#67467) ;
#4045 = STYLED_ITEM('',(#126641),#67468) ;
#4046 = STYLED_ITEM('',(#126641),#67469) ;
#4047 = STYLED_ITEM('',(#126641),#67470) ;
#4048 = STYLED_ITEM('',(#126641),#67471) ;
#4049 = STYLED_ITEM('',(#126641),#67472) ;
#4050 = STYLED_ITEM('',(#126641),#67473) ;
#4051 = STYLED_ITEM('',(#126641),#67474) ;
#4052 = STYLED_ITEM('',(#126641),#67475) ;
#4053 = STYLED_ITEM('',(#126641),#67476) ;
#4054 = STYLED_ITEM('',(#126641),#67477) ;
#4055 = STYLED_ITEM('',(#126641),#67478) ;
#4056 = STYLED_ITEM('',(#126641),#67479) ;
#4057 = STYLED_ITEM('',(#126641),#67480) ;
#4058 = STYLED_ITEM('',(#126641),#67481) ;
#4059 = STYLED_ITEM('',(#126641),#67482) ;
#4060 = STYLED_ITEM('',(#126641),#67483) ;
#4061 = STYLED_ITEM('',(#126641),#67484) ;
#4062 = STYLED_ITEM('',(#126641),#67485) ;
#4063 = STYLED_ITEM('',(#126641),#67486) ;
#4064 = STYLED_ITEM('',(#126641),#67487) ;
#4065 = STYLED_ITEM('',(#126641),#67488) ;
#4066 = STYLED_ITEM('',(#126641),#67489) ;
#4067 = STYLED_ITEM('',(#126641),#67490) ;
#4068 = STYLED_ITEM('',(#126641),#67491) ;
#4069 = STYLED_ITEM('',(#126641),#67492) ;
#4070 = STYLED_ITEM('',(#126641),#67493) ;
#4071 = STYLED_ITEM('',(#126641),#67494) ;
#4072 = STYLED_ITEM('',(#126641),#67495) ;
#4073 = STYLED_ITEM('',(#126641),#67496) ;
#4074 = STYLED_ITEM('',(#126641),#67497) ;
#4075 = STYLED_ITEM('',(#126641),#67498) ;
#4076 = STYLED_ITEM('',(#126641),#67499) ;
#4077 = STYLED_ITEM('',(#126641),#67500) ;
#4078 = STYLED_ITEM('',(#126641),#67501) ;
#4079 = STYLED_ITEM('',(#126641),#67502) ;
#4080 = STYLED_ITEM('',(#126641),#67503) ;
#4081 = STYLED_ITEM('',(#126641),#67504) ;
#4082 = STYLED_ITEM('',(#126641),#67505) ;
#4083 = STYLED_ITEM('',(#126641),#67506) ;
#4084 = STYLED_ITEM('',(#126641),#67507) ;
#4085 = STYLED_ITEM('',(#126641),#67508) ;
#4086 = STYLED_ITEM('',(#126641),#67509) ;
#4087 = STYLED_ITEM('',(#126641),#67510) ;
#4088 = STYLED_ITEM('',(#126641),#67511) ;
#4089 = STYLED_ITEM('',(#126641),#67512) ;
#4090 = STYLED_ITEM('',(#126641),#67513) ;
#4091 = STYLED_ITEM('',(#126641),#67514) ;
#4092 = STYLED_ITEM('',(#126641),#67515) ;
#4093 = STYLED_ITEM('',(#126641),#67516) ;
#4094 = STYLED_ITEM('',(#126641),#67517) ;
#4095 = STYLED_ITEM('',(#126641),#67518) ;
#4096 = STYLED_ITEM('',(#126641),#67519) ;
#4097 = STYLED_ITEM('',(#126641),#67520) ;
#4098 = STYLED_ITEM('',(#126641),#67521) ;
#4099 = STYLED_ITEM('',(#126641),#67522) ;
#4100 = STYLED_ITEM('',(#126641),#67523) ;
#4101 = STYLED_ITEM('',(#126641),#67524) ;
#4102 = STYLED_ITEM('',(#126641),#67525) ;
#4103 = STYLED_ITEM('',(#126641),#67526) ;
#4104 = STYLED_ITEM('',(#126641),#67527) ;
#4105 = STYLED_ITEM('',(#126641),#67528) ;
#4106 = STYLED_ITEM('',(#126641),#67529) ;
#4107 = STYLED_ITEM('',(#126641),#67530) ;
#4108 = STYLED_ITEM('',(#126641),#67531) ;
#4109 = STYLED_ITEM('',(#126641),#67532) ;
#4110 = STYLED_ITEM('',(#126641),#67533) ;
#4111 = STYLED_ITEM('',(#126641),#67534) ;
#4112 = STYLED_ITEM('',(#126641),#67535) ;
#4113 = STYLED_ITEM('',(#126641),#67536) ;
#4114 = STYLED_ITEM('',(#126641),#67537) ;
#4115 = STYLED_ITEM('',(#126641),#67538) ;
#4116 = STYLED_ITEM('',(#126641),#67539) ;
#4117 = STYLED_ITEM('',(#126641),#67540) ;
#4118 = STYLED_ITEM('',(#126641),#67541) ;
#4119 = STYLED_ITEM('',(#126641),#67542) ;
#4120 = STYLED_ITEM('',(#126641),#67543) ;
#4121 = STYLED_ITEM('',(#126641),#67544) ;
#4122 = STYLED_ITEM('',(#126641),#67545) ;
#4123 = STYLED_ITEM('',(#126641),#67546) ;
#4124 = STYLED_ITEM('',(#126641),#67547) ;
#4125 = STYLED_ITEM('',(#126641),#67548) ;
#4126 = STYLED_ITEM('',(#126641),#67549) ;
#4127 = STYLED_ITEM('',(#126641),#67550) ;
#4128 = STYLED_ITEM('',(#126641),#67551) ;
#4129 = STYLED_ITEM('',(#126641),#67552) ;
#4130 = STYLED_ITEM('',(#126641),#67553) ;
#4131 = STYLED_ITEM('',(#126641),#67554) ;
#4132 = STYLED_ITEM('',(#126641),#67555) ;
#4133 = STYLED_ITEM('',(#126641),#67556) ;
#4134 = STYLED_ITEM('',(#126641),#67557) ;
#4135 = STYLED_ITEM('',(#126641),#67558) ;
#4136 = STYLED_ITEM('',(#126641),#67559) ;
#4137 = STYLED_ITEM('',(#126641),#67560) ;
#4138 = STYLED_ITEM('',(#126641),#67561) ;
#4139 = STYLED_ITEM('',(#126641),#67562) ;
#4140 = STYLED_ITEM('',(#126641),#67563) ;
#4141 = STYLED_ITEM('',(#126641),#67564) ;
#4142 = STYLED_ITEM('',(#126641),#67565) ;
#4143 = STYLED_ITEM('',(#126641),#67566) ;
#4144 = STYLED_ITEM('',(#126641),#67567) ;
#4145 = STYLED_ITEM('',(#126641),#67568) ;
#4146 = STYLED_ITEM('',(#126641),#67569) ;
#4147 = STYLED_ITEM('',(#126641),#67570) ;
#4148 = STYLED_ITEM('',(#126641),#67571) ;
#4149 = STYLED_ITEM('',(#126641),#67572) ;
#4150 = STYLED_ITEM('',(#126641),#67573) ;
#4151 = STYLED_ITEM('',(#126641),#67574) ;
#4152 = STYLED_ITEM('',(#126641),#67575) ;
#4153 = STYLED_ITEM('',(#126641),#67576) ;
#4154 = STYLED_ITEM('',(#126641),#67577) ;
#4155 = STYLED_ITEM('',(#126641),#67578) ;
#4156 = STYLED_ITEM('',(#126641),#67579) ;
#4157 = STYLED_ITEM('',(#126641),#67580) ;
#4158 = STYLED_ITEM('',(#126641),#67581) ;
#4159 = STYLED_ITEM('',(#126641),#67582) ;
#4160 = STYLED_ITEM('',(#126641),#67583) ;
#4161 = STYLED_ITEM('',(#126641),#67584) ;
#4162 = STYLED_ITEM('',(#126641),#67585) ;
#4163 = STYLED_ITEM('',(#126641),#67586) ;
#4164 = STYLED_ITEM('',(#126641),#67587) ;
#4165 = STYLED_ITEM('',(#126641),#67588) ;
#4166 = STYLED_ITEM('',(#126641),#67589) ;
#4167 = STYLED_ITEM('',(#126641),#67590) ;
#4168 = STYLED_ITEM('',(#126641),#67591) ;
#4169 = STYLED_ITEM('',(#126639),#4179) ;
#4170 = STYLED_ITEM('',(#126644),#4180) ;
#4171 = STYLED_ITEM('',(#126645),#4181) ;
#4172 = MANIFOLD_SOLID_BREP('Body1',#67686) ;
#4173 = MANIFOLD_SOLID_BREP('Body1',#67687) ;
#4174 = MANIFOLD_SOLID_BREP('Body2',#67688) ;
#4175 = MANIFOLD_SOLID_BREP('Body3',#67689) ;
#4176 = MANIFOLD_SOLID_BREP('Body4',#67690) ;
#4177 = MANIFOLD_SOLID_BREP('Body5',#67691) ;
#4178 = MANIFOLD_SOLID_BREP('Body1',#67692) ;
#4179 = MANIFOLD_SOLID_BREP('Body1',#67693) ;
#4180 = MANIFOLD_SOLID_BREP('Body1',#67694) ;
#4181 = MANIFOLD_SOLID_BREP('Body1',#67695) ;
#4182 = SPHERICAL_SURFACE('',#68025,0.15) ;
#4183 = SPHERICAL_SURFACE('',#68034,0.15) ;
#4184 = SPHERICAL_SURFACE('',#68036,0.15) ;
#4185 = SPHERICAL_SURFACE('',#68045,0.15) ;
#4186 = SPHERICAL_SURFACE('',#68058,0.15) ;
#4187 = SPHERICAL_SURFACE('',#68067,0.15) ;
#4188 = SPHERICAL_SURFACE('',#68069,0.15) ;
#4189 = SPHERICAL_SURFACE('',#68081,0.15) ;
#4190 = SPHERICAL_SURFACE('',#68086,0.15) ;
#4191 = SPHERICAL_SURFACE('',#68107,0.15) ;
#4192 = SPHERICAL_SURFACE('',#68110,0.15) ;
#4193 = SPHERICAL_SURFACE('',#68130,0.15) ;
#4194 = SPHERICAL_SURFACE('',#68146,0.15) ;
#4195 = SPHERICAL_SURFACE('',#68149,0.15) ;
#4196 = SPHERICAL_SURFACE('',#68166,0.15) ;
#4197 = SPHERICAL_SURFACE('',#68168,0.15) ;
#4198 = SPHERICAL_SURFACE('',#68174,0.15) ;
#4199 = SPHERICAL_SURFACE('',#68177,0.15) ;
#4200 = SPHERICAL_SURFACE('',#68195,0.15) ;
#4201 = SPHERICAL_SURFACE('',#68201,0.15) ;
#4202 = SPHERICAL_SURFACE('',#68757,0.15) ;
#4203 = SPHERICAL_SURFACE('',#68763,0.15) ;
#4204 = SPHERICAL_SURFACE('',#68773,0.15) ;
#4205 = SPHERICAL_SURFACE('',#68775,0.15) ;
#4206 = SPHERICAL_SURFACE('',#68975,0.1) ;
#4207 = SPHERICAL_SURFACE('',#68986,0.1) ;
#4208 = SPHERICAL_SURFACE('',#69004,0.1) ;
#4209 = SPHERICAL_SURFACE('',#69010,0.1) ;
#4210 = SPHERICAL_SURFACE('',#69023,0.1) ;
#4211 = SPHERICAL_SURFACE('',#69037,0.1) ;
#4212 = SPHERICAL_SURFACE('',#69042,0.1) ;
#4213 = SPHERICAL_SURFACE('',#69063,0.1) ;
#4214 = SPHERICAL_SURFACE('',#69081,0.1) ;
#4215 = SPHERICAL_SURFACE('',#69083,0.1) ;
#4216 = SPHERICAL_SURFACE('',#69090,0.1) ;
#4217 = SPHERICAL_SURFACE('',#69105,0.1) ;
#4218 = SPHERICAL_SURFACE('',#69118,0.1) ;
#4219 = SPHERICAL_SURFACE('',#69134,0.1) ;
#4220 = SPHERICAL_SURFACE('',#69156,0.1) ;
#4221 = SPHERICAL_SURFACE('',#69159,0.1) ;
#4222 = SPHERICAL_SURFACE('',#69175,0.1) ;
#4223 = SPHERICAL_SURFACE('',#69177,0.1) ;
#4224 = SPHERICAL_SURFACE('',#69203,0.1) ;
#4225 = SPHERICAL_SURFACE('',#69218,0.1) ;
#4226 = SPHERICAL_SURFACE('',#69220,0.1) ;
#4227 = SPHERICAL_SURFACE('',#69226,0.1) ;
#4228 = SPHERICAL_SURFACE('',#69247,0.1) ;
#4229 = SPHERICAL_SURFACE('',#69253,0.1) ;
#4230 = SPHERICAL_SURFACE('',#69265,0.1) ;
#4231 = SPHERICAL_SURFACE('',#69267,0.1) ;
#4232 = SPHERICAL_SURFACE('',#69274,0.1) ;
#4233 = SPHERICAL_SURFACE('',#69280,0.1) ;
#4234 = SPHERICAL_SURFACE('',#69288,0.1) ;
#4235 = SPHERICAL_SURFACE('',#69294,0.1) ;
#4236 = SPHERICAL_SURFACE('',#69315,0.1) ;
#4237 = SPHERICAL_SURFACE('',#69322,0.1) ;
#4238 = SPHERICAL_SURFACE('',#69340,0.1) ;
#4239 = SPHERICAL_SURFACE('',#69343,0.1) ;
#4240 = SPHERICAL_SURFACE('',#69344,0.1) ;
#4241 = SPHERICAL_SURFACE('',#69351,0.1) ;
#4242 = SPHERICAL_SURFACE('',#69353,0.1) ;
#4243 = SPHERICAL_SURFACE('',#69359,0.1) ;
#4244 = SPHERICAL_SURFACE('',#69360,0.1) ;
#4245 = SPHERICAL_SURFACE('',#69367,0.1) ;
#4246 = SPHERICAL_SURFACE('',#69369,0.1) ;
#4247 = SPHERICAL_SURFACE('',#69375,0.1) ;
#4248 = SPHERICAL_SURFACE('',#69378,0.1) ;
#4249 = SPHERICAL_SURFACE('',#69381,0.1) ;
#4250 = SPHERICAL_SURFACE('',#69585,0.1) ;
#4251 = SPHERICAL_SURFACE('',#69596,0.1) ;
#4252 = SPHERICAL_SURFACE('',#69614,0.1) ;
#4253 = SPHERICAL_SURFACE('',#69620,0.1) ;
#4254 = SPHERICAL_SURFACE('',#69633,0.1) ;
#4255 = SPHERICAL_SURFACE('',#69647,0.1) ;
#4256 = SPHERICAL_SURFACE('',#69652,0.1) ;
#4257 = SPHERICAL_SURFACE('',#69673,0.1) ;
#4258 = SPHERICAL_SURFACE('',#69691,0.1) ;
#4259 = SPHERICAL_SURFACE('',#69693,0.1) ;
#4260 = SPHERICAL_SURFACE('',#69700,0.1) ;
#4261 = SPHERICAL_SURFACE('',#69715,0.1) ;
#4262 = SPHERICAL_SURFACE('',#69728,0.1) ;
#4263 = SPHERICAL_SURFACE('',#69744,0.1) ;
#4264 = SPHERICAL_SURFACE('',#69766,0.1) ;
#4265 = SPHERICAL_SURFACE('',#69769,0.1) ;
#4266 = SPHERICAL_SURFACE('',#69785,0.1) ;
#4267 = SPHERICAL_SURFACE('',#69787,0.1) ;
#4268 = SPHERICAL_SURFACE('',#69813,0.1) ;
#4269 = SPHERICAL_SURFACE('',#69828,0.1) ;
#4270 = SPHERICAL_SURFACE('',#69830,0.1) ;
#4271 = SPHERICAL_SURFACE('',#69836,0.1) ;
#4272 = SPHERICAL_SURFACE('',#69857,0.1) ;
#4273 = SPHERICAL_SURFACE('',#69863,0.1) ;
#4274 = SPHERICAL_SURFACE('',#69875,0.1) ;
#4275 = SPHERICAL_SURFACE('',#69877,0.1) ;
#4276 = SPHERICAL_SURFACE('',#69884,0.1) ;
#4277 = SPHERICAL_SURFACE('',#69890,0.1) ;
#4278 = SPHERICAL_SURFACE('',#69898,0.1) ;
#4279 = SPHERICAL_SURFACE('',#69904,0.1) ;
#4280 = SPHERICAL_SURFACE('',#69925,0.1) ;
#4281 = SPHERICAL_SURFACE('',#69932,0.1) ;
#4282 = SPHERICAL_SURFACE('',#69950,0.1) ;
#4283 = SPHERICAL_SURFACE('',#69953,0.1) ;
#4284 = SPHERICAL_SURFACE('',#69954,0.1) ;
#4285 = SPHERICAL_SURFACE('',#69961,0.1) ;
#4286 = SPHERICAL_SURFACE('',#69963,0.1) ;
#4287 = SPHERICAL_SURFACE('',#69969,0.1) ;
#4288 = SPHERICAL_SURFACE('',#69970,0.1) ;
#4289 = SPHERICAL_SURFACE('',#69977,0.1) ;
#4290 = SPHERICAL_SURFACE('',#69979,0.1) ;
#4291 = SPHERICAL_SURFACE('',#69985,0.1) ;
#4292 = SPHERICAL_SURFACE('',#69988,0.1) ;
#4293 = SPHERICAL_SURFACE('',#69991,0.1) ;
#4294 = SPHERICAL_SURFACE('',#70195,0.1) ;
#4295 = SPHERICAL_SURFACE('',#70206,0.1) ;
#4296 = SPHERICAL_SURFACE('',#70224,0.1) ;
#4297 = SPHERICAL_SURFACE('',#70230,0.1) ;
#4298 = SPHERICAL_SURFACE('',#70243,0.1) ;
#4299 = SPHERICAL_SURFACE('',#70257,0.1) ;
#4300 = SPHERICAL_SURFACE('',#70262,0.1) ;
#4301 = SPHERICAL_SURFACE('',#70283,0.1) ;
#4302 = SPHERICAL_SURFACE('',#70301,0.1) ;
#4303 = SPHERICAL_SURFACE('',#70303,0.1) ;
#4304 = SPHERICAL_SURFACE('',#70310,0.1) ;
#4305 = SPHERICAL_SURFACE('',#70325,0.1) ;
#4306 = SPHERICAL_SURFACE('',#70338,0.1) ;
#4307 = SPHERICAL_SURFACE('',#70354,0.1) ;
#4308 = SPHERICAL_SURFACE('',#70376,0.1) ;
#4309 = SPHERICAL_SURFACE('',#70379,0.1) ;
#4310 = SPHERICAL_SURFACE('',#70395,0.1) ;
#4311 = SPHERICAL_SURFACE('',#70397,0.1) ;
#4312 = SPHERICAL_SURFACE('',#70423,0.1) ;
#4313 = SPHERICAL_SURFACE('',#70438,0.1) ;
#4314 = SPHERICAL_SURFACE('',#70440,0.1) ;
#4315 = SPHERICAL_SURFACE('',#70446,0.1) ;
#4316 = SPHERICAL_SURFACE('',#70467,0.1) ;
#4317 = SPHERICAL_SURFACE('',#70473,0.1) ;
#4318 = SPHERICAL_SURFACE('',#70485,0.1) ;
#4319 = SPHERICAL_SURFACE('',#70487,0.1) ;
#4320 = SPHERICAL_SURFACE('',#70494,0.1) ;
#4321 = SPHERICAL_SURFACE('',#70500,0.1) ;
#4322 = SPHERICAL_SURFACE('',#70508,0.1) ;
#4323 = SPHERICAL_SURFACE('',#70514,0.1) ;
#4324 = SPHERICAL_SURFACE('',#70535,0.1) ;
#4325 = SPHERICAL_SURFACE('',#70542,0.1) ;
#4326 = SPHERICAL_SURFACE('',#70560,0.1) ;
#4327 = SPHERICAL_SURFACE('',#70563,0.1) ;
#4328 = SPHERICAL_SURFACE('',#70564,0.1) ;
#4329 = SPHERICAL_SURFACE('',#70571,0.1) ;
#4330 = SPHERICAL_SURFACE('',#70573,0.1) ;
#4331 = SPHERICAL_SURFACE('',#70579,0.1) ;
#4332 = SPHERICAL_SURFACE('',#70580,0.1) ;
#4333 = SPHERICAL_SURFACE('',#70587,0.1) ;
#4334 = SPHERICAL_SURFACE('',#70589,0.1) ;
#4335 = SPHERICAL_SURFACE('',#70595,0.1) ;
#4336 = SPHERICAL_SURFACE('',#70598,0.1) ;
#4337 = SPHERICAL_SURFACE('',#70601,0.1) ;
#4338 = SPHERICAL_SURFACE('',#70805,0.1) ;
#4339 = SPHERICAL_SURFACE('',#70816,0.1) ;
#4340 = SPHERICAL_SURFACE('',#70834,0.1) ;
#4341 = SPHERICAL_SURFACE('',#70840,0.1) ;
#4342 = SPHERICAL_SURFACE('',#70853,0.1) ;
#4343 = SPHERICAL_SURFACE('',#70867,0.1) ;
#4344 = SPHERICAL_SURFACE('',#70872,0.1) ;
#4345 = SPHERICAL_SURFACE('',#70893,0.1) ;
#4346 = SPHERICAL_SURFACE('',#70911,0.1) ;
#4347 = SPHERICAL_SURFACE('',#70913,0.1) ;
#4348 = SPHERICAL_SURFACE('',#70920,0.1) ;
#4349 = SPHERICAL_SURFACE('',#70935,0.1) ;
#4350 = SPHERICAL_SURFACE('',#70948,0.1) ;
#4351 = SPHERICAL_SURFACE('',#70964,0.1) ;
#4352 = SPHERICAL_SURFACE('',#70986,0.1) ;
#4353 = SPHERICAL_SURFACE('',#70989,0.1) ;
#4354 = SPHERICAL_SURFACE('',#71005,0.1) ;
#4355 = SPHERICAL_SURFACE('',#71007,0.1) ;
#4356 = SPHERICAL_SURFACE('',#71033,0.1) ;
#4357 = SPHERICAL_SURFACE('',#71048,0.1) ;
#4358 = SPHERICAL_SURFACE('',#71050,0.1) ;
#4359 = SPHERICAL_SURFACE('',#71056,0.1) ;
#4360 = SPHERICAL_SURFACE('',#71077,0.1) ;
#4361 = SPHERICAL_SURFACE('',#71083,0.1) ;
#4362 = SPHERICAL_SURFACE('',#71095,0.1) ;
#4363 = SPHERICAL_SURFACE('',#71097,0.1) ;
#4364 = SPHERICAL_SURFACE('',#71104,0.1) ;
#4365 = SPHERICAL_SURFACE('',#71110,0.1) ;
#4366 = SPHERICAL_SURFACE('',#71118,0.1) ;
#4367 = SPHERICAL_SURFACE('',#71124,0.1) ;
#4368 = SPHERICAL_SURFACE('',#71145,0.1) ;
#4369 = SPHERICAL_SURFACE('',#71152,0.1) ;
#4370 = SPHERICAL_SURFACE('',#71170,0.1) ;
#4371 = SPHERICAL_SURFACE('',#71173,0.1) ;
#4372 = SPHERICAL_SURFACE('',#71174,0.1) ;
#4373 = SPHERICAL_SURFACE('',#71181,0.1) ;
#4374 = SPHERICAL_SURFACE('',#71183,0.1) ;
#4375 = SPHERICAL_SURFACE('',#71189,0.1) ;
#4376 = SPHERICAL_SURFACE('',#71190,0.1) ;
#4377 = SPHERICAL_SURFACE('',#71197,0.1) ;
#4378 = SPHERICAL_SURFACE('',#71199,0.1) ;
#4379 = SPHERICAL_SURFACE('',#71205,0.1) ;
#4380 = SPHERICAL_SURFACE('',#71208,0.1) ;
#4381 = SPHERICAL_SURFACE('',#71211,0.1) ;
#4382 = SPHERICAL_SURFACE('',#71415,0.1) ;
#4383 = SPHERICAL_SURFACE('',#71426,0.1) ;
#4384 = SPHERICAL_SURFACE('',#71444,0.1) ;
#4385 = SPHERICAL_SURFACE('',#71450,0.1) ;
#4386 = SPHERICAL_SURFACE('',#71463,0.1) ;
#4387 = SPHERICAL_SURFACE('',#71477,0.1) ;
#4388 = SPHERICAL_SURFACE('',#71482,0.1) ;
#4389 = SPHERICAL_SURFACE('',#71503,0.1) ;
#4390 = SPHERICAL_SURFACE('',#71521,0.1) ;
#4391 = SPHERICAL_SURFACE('',#71523,0.1) ;
#4392 = SPHERICAL_SURFACE('',#71530,0.1) ;
#4393 = SPHERICAL_SURFACE('',#71545,0.1) ;
#4394 = SPHERICAL_SURFACE('',#71558,0.1) ;
#4395 = SPHERICAL_SURFACE('',#71574,0.1) ;
#4396 = SPHERICAL_SURFACE('',#71596,0.1) ;
#4397 = SPHERICAL_SURFACE('',#71599,0.1) ;
#4398 = SPHERICAL_SURFACE('',#71615,0.1) ;
#4399 = SPHERICAL_SURFACE('',#71617,0.1) ;
#4400 = SPHERICAL_SURFACE('',#71643,0.1) ;
#4401 = SPHERICAL_SURFACE('',#71658,0.1) ;
#4402 = SPHERICAL_SURFACE('',#71660,0.1) ;
#4403 = SPHERICAL_SURFACE('',#71666,0.1) ;
#4404 = SPHERICAL_SURFACE('',#71687,0.1) ;
#4405 = SPHERICAL_SURFACE('',#71693,0.1) ;
#4406 = SPHERICAL_SURFACE('',#71705,0.1) ;
#4407 = SPHERICAL_SURFACE('',#71707,0.1) ;
#4408 = SPHERICAL_SURFACE('',#71714,0.1) ;
#4409 = SPHERICAL_SURFACE('',#71720,0.1) ;
#4410 = SPHERICAL_SURFACE('',#71728,0.1) ;
#4411 = SPHERICAL_SURFACE('',#71734,0.1) ;
#4412 = SPHERICAL_SURFACE('',#71755,0.1) ;
#4413 = SPHERICAL_SURFACE('',#71762,0.1) ;
#4414 = SPHERICAL_SURFACE('',#71780,0.1) ;
#4415 = SPHERICAL_SURFACE('',#71783,0.1) ;
#4416 = SPHERICAL_SURFACE('',#71784,0.1) ;
#4417 = SPHERICAL_SURFACE('',#71791,0.1) ;
#4418 = SPHERICAL_SURFACE('',#71793,0.1) ;
#4419 = SPHERICAL_SURFACE('',#71799,0.1) ;
#4420 = SPHERICAL_SURFACE('',#71800,0.1) ;
#4421 = SPHERICAL_SURFACE('',#71807,0.1) ;
#4422 = SPHERICAL_SURFACE('',#71809,0.1) ;
#4423 = SPHERICAL_SURFACE('',#71815,0.1) ;
#4424 = SPHERICAL_SURFACE('',#71818,0.1) ;
#4425 = SPHERICAL_SURFACE('',#71821,0.1) ;
#4426 = SPHERICAL_SURFACE('',#71862,1.4986) ;
#4427 = SPHERICAL_SURFACE('',#71876,0.1) ;
#4428 = SPHERICAL_SURFACE('',#71893,0.1) ;
#4429 = SPHERICAL_SURFACE('',#71910,0.1) ;
#4430 = SPHERICAL_SURFACE('',#71927,0.1) ;
#4431 = SPHERICAL_SURFACE('',#71944,0.1) ;
#4432 = SPHERICAL_SURFACE('',#71961,0.1) ;
#4433 = SPHERICAL_SURFACE('',#71978,0.1) ;
#4434 = SPHERICAL_SURFACE('',#71995,0.1) ;
#4435 = SPHERICAL_SURFACE('',#72057,0.1) ;
#4436 = SPHERICAL_SURFACE('',#72106,0.1) ;
#4437 = SPHERICAL_SURFACE('',#72494,0.1) ;
#4438 = SPHERICAL_SURFACE('',#72497,0.1) ;
#4439 = SPHERICAL_SURFACE('',#72515,0.1) ;
#4440 = SPHERICAL_SURFACE('',#72536,0.1) ;
#4441 = SPHERICAL_SURFACE('',#72538,0.1) ;
#4442 = SPHERICAL_SURFACE('',#72543,0.1) ;
#4443 = SPHERICAL_SURFACE('',#72546,0.1) ;
#4444 = SPHERICAL_SURFACE('',#72563,0.1) ;
#4445 = SPHERICAL_SURFACE('',#72569,0.1) ;
#4446 = SPHERICAL_SURFACE('',#72587,0.1) ;
#4447 = SPHERICAL_SURFACE('',#72588,0.1) ;
#4448 = SPHERICAL_SURFACE('',#72597,0.1) ;
#4449 = SPHERICAL_SURFACE('',#72603,0.1) ;
#4450 = SPHERICAL_SURFACE('',#72611,0.1) ;
#4451 = SPHERICAL_SURFACE('',#72613,0.1) ;
#4452 = SPHERICAL_SURFACE('',#72619,0.1) ;
#4453 = SPHERICAL_SURFACE('',#72620,0.1) ;
#4454 = SPHERICAL_SURFACE('',#72629,0.1) ;
#4455 = SPHERICAL_SURFACE('',#72635,0.1) ;
#4456 = SPHERICAL_SURFACE('',#72643,0.1) ;
#4457 = SPHERICAL_SURFACE('',#72645,0.1) ;
#4458 = SPHERICAL_SURFACE('',#72651,0.1) ;
#4459 = SPHERICAL_SURFACE('',#72657,0.1) ;
#4460 = SPHERICAL_SURFACE('',#72665,0.1) ;
#4461 = SPHERICAL_SURFACE('',#72671,0.1) ;
#4462 = SPHERICAL_SURFACE('',#72673,0.1) ;
#4463 = SPHERICAL_SURFACE('',#72679,0.1) ;
#4464 = SPHERICAL_SURFACE('',#72681,0.1) ;
#4465 = SPHERICAL_SURFACE('',#72686,0.1) ;
#4466 = SPHERICAL_SURFACE('',#72692,0.1) ;
#4467 = SPHERICAL_SURFACE('',#72694,0.1) ;
#4468 = SPHERICAL_SURFACE('',#72708,0.1) ;
#4469 = SPHERICAL_SURFACE('',#72710,0.1) ;
#4470 = SPHERICAL_SURFACE('',#72745,0.1) ;
#4471 = SPHERICAL_SURFACE('',#72753,0.1) ;
#4472 = SPHERICAL_SURFACE('',#72792,0.1) ;
#4473 = SPHERICAL_SURFACE('',#72802,0.1) ;
#4474 = SPHERICAL_SURFACE('',#72804,0.1) ;
#4475 = SPHERICAL_SURFACE('',#72813,0.1) ;
#4476 = SPHERICAL_SURFACE('',#72826,0.1) ;
#4477 = SPHERICAL_SURFACE('',#72836,0.1) ;
#4478 = SPHERICAL_SURFACE('',#72838,0.1) ;
#4479 = SPHERICAL_SURFACE('',#72847,0.1) ;
#4480 = SPHERICAL_SURFACE('',#72858,0.1) ;
#4481 = SPHERICAL_SURFACE('',#72862,0.1) ;
#4482 = SPHERICAL_SURFACE('',#72871,0.1) ;
#4483 = SPHERICAL_SURFACE('',#72875,0.1) ;
#4484 = SPHERICAL_SURFACE('',#72882,0.1) ;
#4485 = SPHERICAL_SURFACE('',#72886,0.1) ;
#4486 = SPHERICAL_SURFACE('',#72891,0.1) ;
#4487 = SPHERICAL_SURFACE('',#72897,0.1) ;
#4488 = SPHERICAL_SURFACE('',#73561,0.1) ;
#4489 = SPHERICAL_SURFACE('',#73564,0.1) ;
#4490 = SPHERICAL_SURFACE('',#73582,0.1) ;
#4491 = SPHERICAL_SURFACE('',#73603,0.1) ;
#4492 = SPHERICAL_SURFACE('',#73605,0.1) ;
#4493 = SPHERICAL_SURFACE('',#73610,0.1) ;
#4494 = SPHERICAL_SURFACE('',#73613,0.1) ;
#4495 = SPHERICAL_SURFACE('',#73630,0.1) ;
#4496 = SPHERICAL_SURFACE('',#73636,0.1) ;
#4497 = SPHERICAL_SURFACE('',#73654,0.1) ;
#4498 = SPHERICAL_SURFACE('',#73660,0.1) ;
#4499 = SPHERICAL_SURFACE('',#73668,0.1) ;
#4500 = SPHERICAL_SURFACE('',#73674,0.1) ;
#4501 = SPHERICAL_SURFACE('',#73676,0.1) ;
#4502 = SPHERICAL_SURFACE('',#73682,0.1) ;
#4503 = SPHERICAL_SURFACE('',#73684,0.1) ;
#4504 = SPHERICAL_SURFACE('',#73689,0.1) ;
#4505 = SPHERICAL_SURFACE('',#73695,0.1) ;
#4506 = SPHERICAL_SURFACE('',#73697,0.1) ;
#4507 = SPHERICAL_SURFACE('',#73711,0.1) ;
#4508 = SPHERICAL_SURFACE('',#73713,0.1) ;
#4509 = SPHERICAL_SURFACE('',#73748,0.1) ;
#4510 = SPHERICAL_SURFACE('',#73756,0.1) ;
#4511 = SPHERICAL_SURFACE('',#73764,0.1) ;
#4512 = SPHERICAL_SURFACE('',#73766,0.1) ;
#4513 = SPHERICAL_SURFACE('',#73801,0.1) ;
#4514 = SPHERICAL_SURFACE('',#73809,0.1) ;
#4515 = SPHERICAL_SURFACE('',#73817,0.1) ;
#4516 = SPHERICAL_SURFACE('',#73819,0.1) ;
#4517 = SPHERICAL_SURFACE('',#73854,0.1) ;
#4518 = SPHERICAL_SURFACE('',#73862,0.1) ;
#4519 = SPHERICAL_SURFACE('',#73870,0.1) ;
#4520 = SPHERICAL_SURFACE('',#73872,0.1) ;
#4521 = SPHERICAL_SURFACE('',#73907,0.1) ;
#4522 = SPHERICAL_SURFACE('',#73915,0.1) ;
#4523 = SPHERICAL_SURFACE('',#73923,0.1) ;
#4524 = SPHERICAL_SURFACE('',#73925,0.1) ;
#4525 = SPHERICAL_SURFACE('',#73960,0.1) ;
#4526 = SPHERICAL_SURFACE('',#73968,0.1) ;
#4527 = SPHERICAL_SURFACE('',#73976,0.1) ;
#4528 = SPHERICAL_SURFACE('',#73978,0.1) ;
#4529 = SPHERICAL_SURFACE('',#74013,0.1) ;
#4530 = SPHERICAL_SURFACE('',#74021,0.1) ;
#4531 = SPHERICAL_SURFACE('',#74029,0.1) ;
#4532 = SPHERICAL_SURFACE('',#74031,0.1) ;
#4533 = SPHERICAL_SURFACE('',#74066,0.1) ;
#4534 = SPHERICAL_SURFACE('',#74074,0.1) ;
#4535 = SPHERICAL_SURFACE('',#74082,0.1) ;
#4536 = SPHERICAL_SURFACE('',#74084,0.1) ;
#4537 = SPHERICAL_SURFACE('',#74119,0.1) ;
#4538 = SPHERICAL_SURFACE('',#74127,0.1) ;
#4539 = SPHERICAL_SURFACE('',#74135,0.1) ;
#4540 = SPHERICAL_SURFACE('',#74137,0.1) ;
#4541 = SPHERICAL_SURFACE('',#74172,0.1) ;
#4542 = SPHERICAL_SURFACE('',#74180,0.1) ;
#4543 = SPHERICAL_SURFACE('',#74191,0.1) ;
#4544 = SPHERICAL_SURFACE('',#74194,0.1) ;
#4545 = SPHERICAL_SURFACE('',#74212,0.1) ;
#4546 = SPHERICAL_SURFACE('',#74233,0.1) ;
#4547 = SPHERICAL_SURFACE('',#74235,0.1) ;
#4548 = SPHERICAL_SURFACE('',#74240,0.1) ;
#4549 = SPHERICAL_SURFACE('',#74243,0.1) ;
#4550 = SPHERICAL_SURFACE('',#74260,0.1) ;
#4551 = SPHERICAL_SURFACE('',#74266,0.1) ;
#4552 = SPHERICAL_SURFACE('',#74284,0.1) ;
#4553 = SPHERICAL_SURFACE('',#74290,0.1) ;
#4554 = SPHERICAL_SURFACE('',#74298,0.1) ;
#4555 = SPHERICAL_SURFACE('',#74304,0.1) ;
#4556 = SPHERICAL_SURFACE('',#74306,0.1) ;
#4557 = SPHERICAL_SURFACE('',#74312,0.1) ;
#4558 = SPHERICAL_SURFACE('',#74314,0.1) ;
#4559 = SPHERICAL_SURFACE('',#74319,0.1) ;
#4560 = SPHERICAL_SURFACE('',#74325,0.1) ;
#4561 = SPHERICAL_SURFACE('',#74327,0.1) ;
#4562 = SPHERICAL_SURFACE('',#74344,0.1) ;
#4563 = SPHERICAL_SURFACE('',#74347,0.1) ;
#4564 = SPHERICAL_SURFACE('',#74365,0.1) ;
#4565 = SPHERICAL_SURFACE('',#74386,0.1) ;
#4566 = SPHERICAL_SURFACE('',#74388,0.1) ;
#4567 = SPHERICAL_SURFACE('',#74393,0.1) ;
#4568 = SPHERICAL_SURFACE('',#74396,0.1) ;
#4569 = SPHERICAL_SURFACE('',#74413,0.1) ;
#4570 = SPHERICAL_SURFACE('',#74419,0.1) ;
#4571 = SPHERICAL_SURFACE('',#74437,0.1) ;
#4572 = SPHERICAL_SURFACE('',#74443,0.1) ;
#4573 = SPHERICAL_SURFACE('',#74451,0.1) ;
#4574 = SPHERICAL_SURFACE('',#74457,0.1) ;
#4575 = SPHERICAL_SURFACE('',#74459,0.1) ;
#4576 = SPHERICAL_SURFACE('',#74465,0.1) ;
#4577 = SPHERICAL_SURFACE('',#74467,0.1) ;
#4578 = SPHERICAL_SURFACE('',#74472,0.1) ;
#4579 = SPHERICAL_SURFACE('',#74478,0.1) ;
#4580 = SPHERICAL_SURFACE('',#74480,0.1) ;
#4581 = SPHERICAL_SURFACE('',#74497,0.1) ;
#4582 = SPHERICAL_SURFACE('',#74500,0.1) ;
#4583 = SPHERICAL_SURFACE('',#74518,0.1) ;
#4584 = SPHERICAL_SURFACE('',#74539,0.1) ;
#4585 = SPHERICAL_SURFACE('',#74541,0.1) ;
#4586 = SPHERICAL_SURFACE('',#74546,0.1) ;
#4587 = SPHERICAL_SURFACE('',#74549,0.1) ;
#4588 = SPHERICAL_SURFACE('',#74566,0.1) ;
#4589 = SPHERICAL_SURFACE('',#74572,0.1) ;
#4590 = SPHERICAL_SURFACE('',#74590,0.1) ;
#4591 = SPHERICAL_SURFACE('',#74596,0.1) ;
#4592 = SPHERICAL_SURFACE('',#74604,0.1) ;
#4593 = SPHERICAL_SURFACE('',#74610,0.1) ;
#4594 = SPHERICAL_SURFACE('',#74612,0.1) ;
#4595 = SPHERICAL_SURFACE('',#74618,0.1) ;
#4596 = SPHERICAL_SURFACE('',#74620,0.1) ;
#4597 = SPHERICAL_SURFACE('',#74625,0.1) ;
#4598 = SPHERICAL_SURFACE('',#74631,0.1) ;
#4599 = SPHERICAL_SURFACE('',#74633,0.1) ;
#4600 = SPHERICAL_SURFACE('',#74650,0.1) ;
#4601 = SPHERICAL_SURFACE('',#74653,0.1) ;
#4602 = SPHERICAL_SURFACE('',#74671,0.1) ;
#4603 = SPHERICAL_SURFACE('',#74692,0.1) ;
#4604 = SPHERICAL_SURFACE('',#74694,0.1) ;
#4605 = SPHERICAL_SURFACE('',#74699,0.1) ;
#4606 = SPHERICAL_SURFACE('',#74702,0.1) ;
#4607 = SPHERICAL_SURFACE('',#74719,0.1) ;
#4608 = SPHERICAL_SURFACE('',#74725,0.1) ;
#4609 = SPHERICAL_SURFACE('',#74743,0.1) ;
#4610 = SPHERICAL_SURFACE('',#74749,0.1) ;
#4611 = SPHERICAL_SURFACE('',#74757,0.1) ;
#4612 = SPHERICAL_SURFACE('',#74763,0.1) ;
#4613 = SPHERICAL_SURFACE('',#74765,0.1) ;
#4614 = SPHERICAL_SURFACE('',#74771,0.1) ;
#4615 = SPHERICAL_SURFACE('',#74773,0.1) ;
#4616 = SPHERICAL_SURFACE('',#74778,0.1) ;
#4617 = SPHERICAL_SURFACE('',#74784,0.1) ;
#4618 = SPHERICAL_SURFACE('',#74786,0.1) ;
#4619 = SPHERICAL_SURFACE('',#74803,0.1) ;
#4620 = SPHERICAL_SURFACE('',#74806,0.1) ;
#4621 = SPHERICAL_SURFACE('',#74824,0.1) ;
#4622 = SPHERICAL_SURFACE('',#74845,0.1) ;
#4623 = SPHERICAL_SURFACE('',#74847,0.1) ;
#4624 = SPHERICAL_SURFACE('',#74852,0.1) ;
#4625 = SPHERICAL_SURFACE('',#74855,0.1) ;
#4626 = SPHERICAL_SURFACE('',#74872,0.1) ;
#4627 = SPHERICAL_SURFACE('',#74878,0.1) ;
#4628 = SPHERICAL_SURFACE('',#74896,0.1) ;
#4629 = SPHERICAL_SURFACE('',#74902,0.1) ;
#4630 = SPHERICAL_SURFACE('',#74910,0.1) ;
#4631 = SPHERICAL_SURFACE('',#74916,0.1) ;
#4632 = SPHERICAL_SURFACE('',#74918,0.1) ;
#4633 = SPHERICAL_SURFACE('',#74924,0.1) ;
#4634 = SPHERICAL_SURFACE('',#74926,0.1) ;
#4635 = SPHERICAL_SURFACE('',#74931,0.1) ;
#4636 = SPHERICAL_SURFACE('',#74937,0.1) ;
#4637 = SPHERICAL_SURFACE('',#74939,0.1) ;
#4638 = SPHERICAL_SURFACE('',#74956,0.1) ;
#4639 = SPHERICAL_SURFACE('',#74959,0.1) ;
#4640 = SPHERICAL_SURFACE('',#74977,0.1) ;
#4641 = SPHERICAL_SURFACE('',#74998,0.1) ;
#4642 = SPHERICAL_SURFACE('',#75000,0.1) ;
#4643 = SPHERICAL_SURFACE('',#75005,0.1) ;
#4644 = SPHERICAL_SURFACE('',#75008,0.1) ;
#4645 = SPHERICAL_SURFACE('',#75025,0.1) ;
#4646 = SPHERICAL_SURFACE('',#75031,0.1) ;
#4647 = SPHERICAL_SURFACE('',#75049,0.1) ;
#4648 = SPHERICAL_SURFACE('',#75055,0.1) ;
#4649 = SPHERICAL_SURFACE('',#75063,0.1) ;
#4650 = SPHERICAL_SURFACE('',#75069,0.1) ;
#4651 = SPHERICAL_SURFACE('',#75071,0.1) ;
#4652 = SPHERICAL_SURFACE('',#75077,0.1) ;
#4653 = SPHERICAL_SURFACE('',#75079,0.1) ;
#4654 = SPHERICAL_SURFACE('',#75084,0.1) ;
#4655 = SPHERICAL_SURFACE('',#75090,0.1) ;
#4656 = SPHERICAL_SURFACE('',#75092,0.1) ;
#4657 = SPHERICAL_SURFACE('',#75109,0.1) ;
#4658 = SPHERICAL_SURFACE('',#75112,0.1) ;
#4659 = SPHERICAL_SURFACE('',#75130,0.1) ;
#4660 = SPHERICAL_SURFACE('',#75151,0.1) ;
#4661 = SPHERICAL_SURFACE('',#75153,0.1) ;
#4662 = SPHERICAL_SURFACE('',#75158,0.1) ;
#4663 = SPHERICAL_SURFACE('',#75161,0.1) ;
#4664 = SPHERICAL_SURFACE('',#75178,0.1) ;
#4665 = SPHERICAL_SURFACE('',#75184,0.1) ;
#4666 = SPHERICAL_SURFACE('',#75202,0.1) ;
#4667 = SPHERICAL_SURFACE('',#75208,0.1) ;
#4668 = SPHERICAL_SURFACE('',#75216,0.1) ;
#4669 = SPHERICAL_SURFACE('',#75222,0.1) ;
#4670 = SPHERICAL_SURFACE('',#75224,0.1) ;
#4671 = SPHERICAL_SURFACE('',#75230,0.1) ;
#4672 = SPHERICAL_SURFACE('',#75232,0.1) ;
#4673 = SPHERICAL_SURFACE('',#75237,0.1) ;
#4674 = SPHERICAL_SURFACE('',#75243,0.1) ;
#4675 = SPHERICAL_SURFACE('',#75245,0.1) ;
#4676 = SPHERICAL_SURFACE('',#75262,0.1) ;
#4677 = SPHERICAL_SURFACE('',#75265,0.1) ;
#4678 = SPHERICAL_SURFACE('',#75283,0.1) ;
#4679 = SPHERICAL_SURFACE('',#75304,0.1) ;
#4680 = SPHERICAL_SURFACE('',#75306,0.1) ;
#4681 = SPHERICAL_SURFACE('',#75311,0.1) ;
#4682 = SPHERICAL_SURFACE('',#75314,0.1) ;
#4683 = SPHERICAL_SURFACE('',#75331,0.1) ;
#4684 = SPHERICAL_SURFACE('',#75337,0.1) ;
#4685 = SPHERICAL_SURFACE('',#75355,0.1) ;
#4686 = SPHERICAL_SURFACE('',#75361,0.1) ;
#4687 = SPHERICAL_SURFACE('',#75369,0.1) ;
#4688 = SPHERICAL_SURFACE('',#75375,0.1) ;
#4689 = SPHERICAL_SURFACE('',#75377,0.1) ;
#4690 = SPHERICAL_SURFACE('',#75383,0.1) ;
#4691 = SPHERICAL_SURFACE('',#75385,0.1) ;
#4692 = SPHERICAL_SURFACE('',#75390,0.1) ;
#4693 = SPHERICAL_SURFACE('',#75396,0.1) ;
#4694 = SPHERICAL_SURFACE('',#75398,0.1) ;
#4695 = SPHERICAL_SURFACE('',#75667,0.1) ;
#4696 = SPHERICAL_SURFACE('',#75677,0.1) ;
#4697 = SPHERICAL_SURFACE('',#75679,0.1) ;
#4698 = SPHERICAL_SURFACE('',#75688,0.1) ;
#4699 = SPHERICAL_SURFACE('',#75701,0.1) ;
#4700 = SPHERICAL_SURFACE('',#75711,0.1) ;
#4701 = SPHERICAL_SURFACE('',#75713,0.1) ;
#4702 = SPHERICAL_SURFACE('',#75722,0.1) ;
#4703 = SPHERICAL_SURFACE('',#75735,0.1) ;
#4704 = SPHERICAL_SURFACE('',#75745,0.1) ;
#4705 = SPHERICAL_SURFACE('',#75747,0.1) ;
#4706 = SPHERICAL_SURFACE('',#75756,0.1) ;
#4707 = SPHERICAL_SURFACE('',#75769,0.1) ;
#4708 = SPHERICAL_SURFACE('',#75779,0.1) ;
#4709 = SPHERICAL_SURFACE('',#75781,0.1) ;
#4710 = SPHERICAL_SURFACE('',#75790,0.1) ;
#4711 = SPHERICAL_SURFACE('',#75803,0.1) ;
#4712 = SPHERICAL_SURFACE('',#75813,0.1) ;
#4713 = SPHERICAL_SURFACE('',#75815,0.1) ;
#4714 = SPHERICAL_SURFACE('',#75824,0.1) ;
#4715 = SPHERICAL_SURFACE('',#75837,0.1) ;
#4716 = SPHERICAL_SURFACE('',#75847,0.1) ;
#4717 = SPHERICAL_SURFACE('',#75849,0.1) ;
#4718 = SPHERICAL_SURFACE('',#75858,0.1) ;
#4719 = SPHERICAL_SURFACE('',#75871,0.1) ;
#4720 = SPHERICAL_SURFACE('',#75881,0.1) ;
#4721 = SPHERICAL_SURFACE('',#75883,0.1) ;
#4722 = SPHERICAL_SURFACE('',#75892,0.1) ;
#4723 = SPHERICAL_SURFACE('',#75905,0.1) ;
#4724 = SPHERICAL_SURFACE('',#75915,0.1) ;
#4725 = SPHERICAL_SURFACE('',#75917,0.1) ;
#4726 = SPHERICAL_SURFACE('',#75926,0.1) ;
#4727 = SPHERICAL_SURFACE('',#75939,0.1) ;
#4728 = SPHERICAL_SURFACE('',#75949,0.1) ;
#4729 = SPHERICAL_SURFACE('',#75951,0.1) ;
#4730 = SPHERICAL_SURFACE('',#75960,0.1) ;
#4731 = SPHERICAL_SURFACE('',#75973,0.1) ;
#4732 = SPHERICAL_SURFACE('',#75983,0.1) ;
#4733 = SPHERICAL_SURFACE('',#75985,0.1) ;
#4734 = SPHERICAL_SURFACE('',#75994,0.1) ;
#4735 = SPHERICAL_SURFACE('',#76007,0.1) ;
#4736 = SPHERICAL_SURFACE('',#76017,0.1) ;
#4737 = SPHERICAL_SURFACE('',#76019,0.1) ;
#4738 = SPHERICAL_SURFACE('',#76028,0.1) ;
#4739 = SPHERICAL_SURFACE('',#76041,0.1) ;
#4740 = SPHERICAL_SURFACE('',#76051,0.1) ;
#4741 = SPHERICAL_SURFACE('',#76053,0.1) ;
#4742 = SPHERICAL_SURFACE('',#76062,0.1) ;
#4743 = SPHERICAL_SURFACE('',#76075,0.1) ;
#4744 = SPHERICAL_SURFACE('',#76085,0.1) ;
#4745 = SPHERICAL_SURFACE('',#76087,0.1) ;
#4746 = SPHERICAL_SURFACE('',#76096,0.1) ;
#4747 = SPHERICAL_SURFACE('',#76109,0.1) ;
#4748 = SPHERICAL_SURFACE('',#76119,0.1) ;
#4749 = SPHERICAL_SURFACE('',#76121,0.1) ;
#4750 = SPHERICAL_SURFACE('',#76130,0.1) ;
#4751 = SPHERICAL_SURFACE('',#76143,0.1) ;
#4752 = SPHERICAL_SURFACE('',#76153,0.1) ;
#4753 = SPHERICAL_SURFACE('',#76155,0.1) ;
#4754 = SPHERICAL_SURFACE('',#76164,0.1) ;
#4755 = SPHERICAL_SURFACE('',#76177,0.1) ;
#4756 = SPHERICAL_SURFACE('',#76187,0.1) ;
#4757 = SPHERICAL_SURFACE('',#76189,0.1) ;
#4758 = SPHERICAL_SURFACE('',#76198,0.1) ;
#4759 = SPHERICAL_SURFACE('',#76211,0.1) ;
#4760 = SPHERICAL_SURFACE('',#76221,0.1) ;
#4761 = SPHERICAL_SURFACE('',#76223,0.1) ;
#4762 = SPHERICAL_SURFACE('',#76232,0.1) ;
#4763 = SPHERICAL_SURFACE('',#76245,0.1) ;
#4764 = SPHERICAL_SURFACE('',#76255,0.1) ;
#4765 = SPHERICAL_SURFACE('',#76257,0.1) ;
#4766 = SPHERICAL_SURFACE('',#76266,0.1) ;
#4767 = SPHERICAL_SURFACE('',#76277,0.1) ;
#4768 = SPHERICAL_SURFACE('',#76281,0.1) ;
#4769 = SPHERICAL_SURFACE('',#76290,0.1) ;
#4770 = SPHERICAL_SURFACE('',#76294,0.1) ;
#4771 = SPHERICAL_SURFACE('',#76301,0.1) ;
#4772 = SPHERICAL_SURFACE('',#76305,0.1) ;
#4773 = SPHERICAL_SURFACE('',#76310,0.1) ;
#4774 = SPHERICAL_SURFACE('',#76316,0.1) ;
#4775 = SPHERICAL_SURFACE('',#76321,0.1) ;
#4776 = SPHERICAL_SURFACE('',#76325,0.1) ;
#4777 = SPHERICAL_SURFACE('',#76334,0.1) ;
#4778 = SPHERICAL_SURFACE('',#76338,0.1) ;
#4779 = SPHERICAL_SURFACE('',#76345,0.1) ;
#4780 = SPHERICAL_SURFACE('',#76349,0.1) ;
#4781 = SPHERICAL_SURFACE('',#76354,0.1) ;
#4782 = SPHERICAL_SURFACE('',#76360,0.1) ;
#4783 = SPHERICAL_SURFACE('',#76365,0.1) ;
#4784 = SPHERICAL_SURFACE('',#76369,0.1) ;
#4785 = SPHERICAL_SURFACE('',#76378,0.1) ;
#4786 = SPHERICAL_SURFACE('',#76382,0.1) ;
#4787 = SPHERICAL_SURFACE('',#76389,0.1) ;
#4788 = SPHERICAL_SURFACE('',#76393,0.1) ;
#4789 = SPHERICAL_SURFACE('',#76398,0.1) ;
#4790 = SPHERICAL_SURFACE('',#76404,0.1) ;
#4791 = SPHERICAL_SURFACE('',#76409,0.1) ;
#4792 = SPHERICAL_SURFACE('',#76413,0.1) ;
#4793 = SPHERICAL_SURFACE('',#76422,0.1) ;
#4794 = SPHERICAL_SURFACE('',#76426,0.1) ;
#4795 = SPHERICAL_SURFACE('',#76433,0.1) ;
#4796 = SPHERICAL_SURFACE('',#76437,0.1) ;
#4797 = SPHERICAL_SURFACE('',#76442,0.1) ;
#4798 = SPHERICAL_SURFACE('',#76448,0.1) ;
#4799 = SPHERICAL_SURFACE('',#76453,0.1) ;
#4800 = SPHERICAL_SURFACE('',#76457,0.1) ;
#4801 = SPHERICAL_SURFACE('',#76466,0.1) ;
#4802 = SPHERICAL_SURFACE('',#76470,0.1) ;
#4803 = SPHERICAL_SURFACE('',#76477,0.1) ;
#4804 = SPHERICAL_SURFACE('',#76481,0.1) ;
#4805 = SPHERICAL_SURFACE('',#76486,0.1) ;
#4806 = SPHERICAL_SURFACE('',#76492,0.1) ;
#4807 = SPHERICAL_SURFACE('',#76497,0.1) ;
#4808 = SPHERICAL_SURFACE('',#76501,0.1) ;
#4809 = SPHERICAL_SURFACE('',#76510,0.1) ;
#4810 = SPHERICAL_SURFACE('',#76514,0.1) ;
#4811 = SPHERICAL_SURFACE('',#76521,0.1) ;
#4812 = SPHERICAL_SURFACE('',#76525,0.1) ;
#4813 = SPHERICAL_SURFACE('',#76530,0.1) ;
#4814 = SPHERICAL_SURFACE('',#76536,0.1) ;
#4815 = SPHERICAL_SURFACE('',#76541,0.1) ;
#4816 = SPHERICAL_SURFACE('',#76545,0.1) ;
#4817 = SPHERICAL_SURFACE('',#76554,0.1) ;
#4818 = SPHERICAL_SURFACE('',#76558,0.1) ;
#4819 = SPHERICAL_SURFACE('',#76565,0.1) ;
#4820 = SPHERICAL_SURFACE('',#76569,0.1) ;
#4821 = SPHERICAL_SURFACE('',#76574,0.1) ;
#4822 = SPHERICAL_SURFACE('',#76580,0.1) ;
#4823 = SPHERICAL_SURFACE('',#76585,0.1) ;
#4824 = SPHERICAL_SURFACE('',#76589,0.1) ;
#4825 = SPHERICAL_SURFACE('',#76598,0.1) ;
#4826 = SPHERICAL_SURFACE('',#76602,0.1) ;
#4827 = SPHERICAL_SURFACE('',#76609,0.1) ;
#4828 = SPHERICAL_SURFACE('',#76613,0.1) ;
#4829 = SPHERICAL_SURFACE('',#76618,0.1) ;
#4830 = SPHERICAL_SURFACE('',#76624,0.1) ;
#4831 = SPHERICAL_SURFACE('',#76629,0.1) ;
#4832 = SPHERICAL_SURFACE('',#76633,0.1) ;
#4833 = SPHERICAL_SURFACE('',#76642,0.1) ;
#4834 = SPHERICAL_SURFACE('',#76646,0.1) ;
#4835 = SPHERICAL_SURFACE('',#76653,0.1) ;
#4836 = SPHERICAL_SURFACE('',#76657,0.1) ;
#4837 = SPHERICAL_SURFACE('',#76662,0.1) ;
#4838 = SPHERICAL_SURFACE('',#76668,0.1) ;
#4839 = SPHERICAL_SURFACE('',#76795,5.) ;
#4840 = ELLIPSE('',#68022,0.212132034355858,0.149999999999913) ;
#4841 = ELLIPSE('',#68024,0.212132034356981,0.150000000000627) ;
#4842 = ELLIPSE('',#68079,0.21213203435611,0.150000000000114) ;
#4843 = ELLIPSE('',#68090,0.212132034356462,0.150000000000298) ;
#4844 = ELLIPSE('',#68749,0.212132034356202,0.150000000000162) ;
#4845 = ELLIPSE('',#68753,0.212132034355904,0.149999999999933) ;
#4846 = ELLIPSE('',#68760,0.212132034354929,0.149999999999304) ;
#4847 = ELLIPSE('',#68762,0.212132034356004,0.150000000000028) ;
#4848 = ELLIPSE('',#68779,0.0809537756926331,0.0568957747646781) ;
#4849 = ELLIPSE('',#68781,0.100391322057661,0.0922176205486333) ;
#4850 = ELLIPSE('',#68783,0.113377229734873,0.0929834630466229) ;
#4851 = ELLIPSE('',#68785,0.223917610441093,0.216142984077905) ;
#4852 = ELLIPSE('',#68812,0.121362326126752,0.103679679516972) ;
#4853 = ELLIPSE('',#68858,0.0267230623193982,0.018714321485574) ;
#4854 = ELLIPSE('',#68933,0.199399949088646,0.187786165419954) ;
#4855 = ELLIPSE('',#68934,0.199099081511402,0.194604184805257) ;
#4856 = ELLIPSE('',#68935,0.201529676353064,0.190129099365806) ;
#4857 = ELLIPSE('',#69047,0.239594752729702,0.10422367698916) ;
#4858 = ELLIPSE('',#69049,0.239471272532979,0.104190452488474) ;
#4859 = ELLIPSE('',#69053,0.239471272536741,0.104190452489493) ;
#4860 = ELLIPSE('',#69054,0.239594752729914,0.104223676989188) ;
#4861 = ELLIPSE('',#69056,0.239594752728089,0.104223676988759) ;
#4862 = ELLIPSE('',#69057,0.239471272538988,0.104190452490065) ;
#4863 = ELLIPSE('',#69067,0.239471272536946,0.10419045248958) ;
#4864 = ELLIPSE('',#69070,0.239594752723292,0.104223676987398) ;
#4865 = ELLIPSE('',#69075,0.14142135623732,0.100000000000004) ;
#4866 = ELLIPSE('',#69111,0.141421356237308,0.0999999999999974) ;
#4867 = ELLIPSE('',#69284,0.097021650614293,0.0903313095003513) ;
#4868 = ELLIPSE('',#69297,0.0951423444618738,0.0854984019584871) ;
#4869 = ELLIPSE('',#69330,0.104054226887004,0.0879291201711123) ;
#4870 = ELLIPSE('',#69335,0.104149278807314,0.0880903460854034) ;
#4871 = ELLIPSE('',#69383,0.107757087311018,0.0995628413317711) ;
#4872 = ELLIPSE('',#69387,0.107757092531729,0.0995628480425321) ;
#4873 = ELLIPSE('',#69389,0.0809537320004613,0.0568957137241202) ;
#4874 = ELLIPSE('',#69391,0.10039132205649,0.0922176205475765) ;
#4875 = ELLIPSE('',#69393,0.113377229735081,0.0929834630467951) ;
#4876 = ELLIPSE('',#69395,0.223917611676684,0.216142984782922) ;
#4877 = ELLIPSE('',#69422,0.121362326117636,0.10367967951289) ;
#4878 = ELLIPSE('',#69468,0.0267230623194912,0.0187143214857259) ;
#4879 = ELLIPSE('',#69543,0.19939994910193,0.187786165441026) ;
#4880 = ELLIPSE('',#69544,0.199099083267325,0.194604186778209) ;
#4881 = ELLIPSE('',#69545,0.201529680428943,0.190129102907909) ;
#4882 = ELLIPSE('',#69657,0.23959475272645,0.104223676988348) ;
#4883 = ELLIPSE('',#69659,0.23947127252868,0.104190452487282) ;
#4884 = ELLIPSE('',#69663,0.239471272523845,0.104190452486007) ;
#4885 = ELLIPSE('',#69664,0.239594752719793,0.104223676986401) ;
#4886 = ELLIPSE('',#69666,0.239594752718529,0.104223676986274) ;
#4887 = ELLIPSE('',#69667,0.239471272528616,0.10419045248741) ;
#4888 = ELLIPSE('',#69677,0.239471272535145,0.104190452489145) ;
#4889 = ELLIPSE('',#69680,0.239594752726162,0.104223676988029) ;
#4890 = ELLIPSE('',#69685,0.141421356237384,0.100000000000052) ;
#4891 = ELLIPSE('',#69721,0.141421356237348,0.100000000000022) ;
#4892 = ELLIPSE('',#69894,0.0970216506148374,0.0903313095008944) ;
#4893 = ELLIPSE('',#69907,0.0951423444627011,0.0854984019587331) ;
#4894 = ELLIPSE('',#69940,0.104054227208667,0.0879291207156953) ;
#4895 = ELLIPSE('',#69945,0.10414927820719,0.0880903450688493) ;
#4896 = ELLIPSE('',#69993,0.107757087370127,0.0995628414091742) ;
#4897 = ELLIPSE('',#69997,0.107757092560179,0.0995628480825893) ;
#4898 = ELLIPSE('',#69999,0.0809537150131407,0.0568956899993869) ;
#4899 = ELLIPSE('',#70001,0.100391322056624,0.0922176205478182) ;
#4900 = ELLIPSE('',#70003,0.11337722973501,0.0929834630467645) ;
#4901 = ELLIPSE('',#70005,0.223917608546806,0.216142982996952) ;
#4902 = ELLIPSE('',#70032,0.121362326128888,0.103679679517888) ;
#4903 = ELLIPSE('',#70078,0.0267230623192196,0.018714321485282) ;
#4904 = ELLIPSE('',#70153,0.199399948440172,0.187786164286963) ;
#4905 = ELLIPSE('',#70154,0.19909908761073,0.194604191600843) ;
#4906 = ELLIPSE('',#70155,0.201529663713424,0.190129088416408) ;
#4907 = ELLIPSE('',#70267,0.239594752713108,0.104223676985137) ;
#4908 = ELLIPSE('',#70269,0.239471272519053,0.10419045248485) ;
#4909 = ELLIPSE('',#70273,0.239471272510231,0.104190452482661) ;
#4910 = ELLIPSE('',#70274,0.239594752744898,0.104223676993171) ;
#4911 = ELLIPSE('',#70276,0.239594752804206,0.104223677008282) ;
#4912 = ELLIPSE('',#70277,0.239471272554278,0.104190452494285) ;
#4913 = ELLIPSE('',#70287,0.239471272532213,0.10419045248842) ;
#4914 = ELLIPSE('',#70290,0.239594752728355,0.104223676988648) ;
#4915 = ELLIPSE('',#70295,0.141421356237532,0.100000000000142) ;
#4916 = ELLIPSE('',#70331,0.141421356237283,0.0999999999999815) ;
#4917 = ELLIPSE('',#70504,0.097021650613777,0.0903313094997654) ;
#4918 = ELLIPSE('',#70517,0.0951423444666796,0.0854984019616217) ;
#4919 = ELLIPSE('',#70550,0.104054228132819,0.0879291222802139) ;
#4920 = ELLIPSE('',#70555,0.104149278173856,0.0880903450126872) ;
#4921 = ELLIPSE('',#70603,0.107757087301598,0.0995628413185721) ;
#4922 = ELLIPSE('',#70607,0.107757092599453,0.0995628481342478) ;
#4923 = ELLIPSE('',#70609,0.0809537387857418,0.0568957231926316) ;
#4924 = ELLIPSE('',#70611,0.10039132205777,0.092217620548776) ;
#4925 = ELLIPSE('',#70613,0.113377229735182,0.0929834630469383) ;
#4926 = ELLIPSE('',#70615,0.223917610559684,0.216142984153567) ;
#4927 = ELLIPSE('',#70642,0.121362326124367,0.103679679515825) ;
#4928 = ELLIPSE('',#70688,0.026723062320724,0.0187143214878425) ;
#4929 = ELLIPSE('',#70763,0.199399948145838,0.187786163779416) ;
#4930 = ELLIPSE('',#70764,0.199099054947908,0.194604155307638) ;
#4931 = ELLIPSE('',#70765,0.201529689838765,0.190129111016764) ;
#4932 = ELLIPSE('',#70877,0.239594752707325,0.104223676983421) ;
#4933 = ELLIPSE('',#70879,0.239471272497778,0.104190452479804) ;
#4934 = ELLIPSE('',#70883,0.239471272515141,0.104190452483868) ;
#4935 = ELLIPSE('',#70884,0.239594752753233,0.10422367699537) ;
#4936 = ELLIPSE('',#70886,0.239594752695653,0.104223676980216) ;
#4937 = ELLIPSE('',#70887,0.239471272540246,0.10419045249087) ;
#4938 = ELLIPSE('',#70897,0.239471272540333,0.104190452490452) ;
#4939 = ELLIPSE('',#70900,0.239594752729595,0.10422367698884) ;
#4940 = ELLIPSE('',#70905,0.141421356237619,0.100000000000176) ;
#4941 = ELLIPSE('',#70941,0.14142135623723,0.0999999999999436) ;
#4942 = ELLIPSE('',#71114,0.0970216506126833,0.0903313094987464) ;
#4943 = ELLIPSE('',#71127,0.0951423444690284,0.0854984019628288) ;
#4944 = ELLIPSE('',#71160,0.104054227520181,0.0879291212428128) ;
#4945 = ELLIPSE('',#71165,0.104149278514073,0.0880903455891445) ;
#4946 = ELLIPSE('',#71213,0.107757082275427,0.0995628348635113) ;
#4947 = ELLIPSE('',#71217,0.107757087537776,0.0995628416311376) ;
#4948 = ELLIPSE('',#71219,0.0809537573847507,0.0568957491961901) ;
#4949 = ELLIPSE('',#71221,0.100391322057649,0.0922176205486138) ;
#4950 = ELLIPSE('',#71223,0.113377229735276,0.0929834630468768) ;
#4951 = ELLIPSE('',#71225,0.22391761061454,0.216142984175044) ;
#4952 = ELLIPSE('',#71252,0.121362326124309,0.103679679515832) ;
#4953 = ELLIPSE('',#71298,0.0267230623209999,0.0187143214882515) ;
#4954 = ELLIPSE('',#71373,0.199399950265729,0.187786167479822) ;
#4955 = ELLIPSE('',#71374,0.199099063433144,0.194604164642533) ;
#4956 = ELLIPSE('',#71375,0.201529637184767,0.190129065311698) ;
#4957 = ELLIPSE('',#71487,0.239594752727344,0.104223676988237) ;
#4958 = ELLIPSE('',#71489,0.239471272520672,0.104190452485608) ;
#4959 = ELLIPSE('',#71493,0.239471272484206,0.104190452475713) ;
#4960 = ELLIPSE('',#71494,0.239594752698159,0.104223676980846) ;
#4961 = ELLIPSE('',#71496,0.239594752701739,0.104223676981937) ;
#4962 = ELLIPSE('',#71497,0.239471272477747,0.104190452474144) ;
#4963 = ELLIPSE('',#71507,0.239471272525481,0.104190452486512) ;
#4964 = ELLIPSE('',#71510,0.239594752715511,0.104223676985684) ;
#4965 = ELLIPSE('',#71515,0.141421356237514,0.100000000000115) ;
#4966 = ELLIPSE('',#71551,0.141421356237124,0.0999999999998686) ;
#4967 = ELLIPSE('',#71724,0.0970216506112587,0.0903313094971849) ;
#4968 = ELLIPSE('',#71737,0.0951423444596952,0.0854984019571455) ;
#4969 = ELLIPSE('',#71770,0.104054227648042,0.0879291214596957) ;
#4970 = ELLIPSE('',#71775,0.104149278744974,0.0880903459807416) ;
#4971 = ELLIPSE('',#71823,0.107757087317353,0.0995628413381732) ;
#4972 = ELLIPSE('',#71827,0.107757082308246,0.0995628349076281) ;
#4973 = ELLIPSE('',#71881,0.141421356226833,0.0999999999854714) ;
#4974 = ELLIPSE('',#71898,0.141421356205715,0.0999999999561054) ;
#4975 = ELLIPSE('',#71915,0.141421356206211,0.0999999999568741) ;
#4976 = ELLIPSE('',#71932,0.14142135619891,0.0999999999469108) ;
#4977 = ELLIPSE('',#71949,0.14142135620716,0.0999999999583245) ;
#4978 = ELLIPSE('',#71966,0.141421356264666,0.100000000037862) ;
#4979 = ELLIPSE('',#71983,0.141421356235352,0.0999999999972513) ;
#4980 = ELLIPSE('',#72000,0.141421356240128,0.100000000003844) ;
#4981 = ELLIPSE('',#72062,0.141421356242718,0.100000000007393) ;
#4982 = ELLIPSE('',#72111,0.141421356244824,0.100000000010334) ;
#4983 = ELLIPSE('',#76691,1.73204548364451,1.5) ;
#4984 = ELLIPSE('',#76692,1.73205681329418,1.5) ;
#4985 = ELLIPSE('',#76782,1.10195897608265,0.486831694836699) ;
#4986 = ELLIPSE('',#76817,1.10195897609098,0.486831694838641) ;
#4987 = ELLIPSE('',#76819,1.10195897609068,0.486831694838579) ;
#4988 = ELLIPSE('',#76831,1.1019589760921,0.486831694838885) ;
#4989 = FACE_BOUND('',#20413,.T.) ;
#4990 = FACE_BOUND('',#20414,.T.) ;
#4991 = FACE_BOUND('',#20416,.T.) ;
#4992 = FACE_BOUND('',#20417,.T.) ;
#4993 = FACE_BOUND('',#20419,.T.) ;
#4994 = FACE_BOUND('',#20420,.T.) ;
#4995 = FACE_BOUND('',#20421,.T.) ;
#4996 = FACE_BOUND('',#20422,.T.) ;
#4997 = FACE_BOUND('',#20424,.T.) ;
#4998 = FACE_BOUND('',#20425,.T.) ;
#4999 = FACE_BOUND('',#20426,.T.) ;
#5000 = FACE_BOUND('',#20427,.T.) ;
#5001 = FACE_BOUND('',#20429,.T.) ;
#5002 = FACE_BOUND('',#20430,.T.) ;
#5003 = FACE_BOUND('',#20431,.T.) ;
#5004 = FACE_BOUND('',#20432,.T.) ;
#5005 = FACE_BOUND('',#20433,.T.) ;
#5006 = FACE_BOUND('',#20434,.T.) ;
#5007 = FACE_BOUND('',#20435,.T.) ;
#5008 = FACE_BOUND('',#20437,.T.) ;
#5009 = FACE_BOUND('',#20438,.T.) ;
#5010 = FACE_BOUND('',#20439,.T.) ;
#5011 = FACE_BOUND('',#20440,.T.) ;
#5012 = FACE_BOUND('',#20441,.T.) ;
#5013 = FACE_BOUND('',#20442,.T.) ;
#5014 = FACE_BOUND('',#20443,.T.) ;
#5015 = FACE_BOUND('',#20445,.T.) ;
#5016 = FACE_BOUND('',#20446,.T.) ;
#5017 = FACE_BOUND('',#20448,.T.) ;
#5018 = FACE_BOUND('',#20449,.T.) ;
#5019 = FACE_BOUND('',#20908,.T.) ;
#5020 = FACE_BOUND('',#20920,.T.) ;
#5021 = FACE_BOUND('',#21199,.T.) ;
#5022 = FACE_BOUND('',#21211,.T.) ;
#5023 = FACE_BOUND('',#21490,.T.) ;
#5024 = FACE_BOUND('',#21502,.T.) ;
#5025 = FACE_BOUND('',#21781,.T.) ;
#5026 = FACE_BOUND('',#21793,.T.) ;
#5027 = FACE_BOUND('',#22072,.T.) ;
#5028 = FACE_BOUND('',#22084,.T.) ;
#5029 = FACE_BOUND('',#22354,.T.) ;
#5030 = FACE_BOUND('',#22355,.T.) ;
#5031 = FACE_BOUND('',#22487,.T.) ;
#5032 = FACE_BOUND('',#22488,.T.) ;
#5033 = FACE_BOUND('',#22489,.T.) ;
#5034 = FACE_BOUND('',#22490,.T.) ;
#5035 = FACE_BOUND('',#22491,.T.) ;
#5036 = FACE_BOUND('',#22492,.T.) ;
#5037 = FACE_BOUND('',#22493,.T.) ;
#5038 = FACE_BOUND('',#22494,.T.) ;
#5039 = FACE_BOUND('',#22495,.T.) ;
#5040 = FACE_BOUND('',#22496,.T.) ;
#5041 = FACE_BOUND('',#22533,.T.) ;
#5042 = FACE_BOUND('',#22535,.T.) ;
#5043 = FACE_BOUND('',#22822,.T.) ;
#5044 = FACE_BOUND('',#22851,.T.) ;
#5045 = FACE_BOUND('',#22880,.T.) ;
#5046 = FACE_BOUND('',#22909,.T.) ;
#5047 = FACE_BOUND('',#22938,.T.) ;
#5048 = FACE_BOUND('',#22967,.T.) ;
#5049 = FACE_BOUND('',#22996,.T.) ;
#5050 = FACE_BOUND('',#23025,.T.) ;
#5051 = FACE_BOUND('',#23054,.T.) ;
#5052 = FACE_BOUND('',#23056,.T.) ;
#5053 = FACE_BOUND('',#23058,.T.) ;
#5054 = FACE_BOUND('',#23060,.T.) ;
#5055 = FACE_BOUND('',#23062,.T.) ;
#5056 = FACE_BOUND('',#23064,.T.) ;
#5057 = FACE_BOUND('',#23066,.T.) ;
#5058 = FACE_BOUND('',#23068,.T.) ;
#5059 = FACE_BOUND('',#23070,.T.) ;
#5060 = FACE_BOUND('',#23072,.T.) ;
#5061 = FACE_BOUND('',#24666,.T.) ;
#5062 = FACE_BOUND('',#24668,.T.) ;
#5063 = FACE_BOUND('',#24688,.T.) ;
#5064 = FACE_BOUND('',#24709,.T.) ;
#5065 = PLANE('',#67802) ;
#5066 = PLANE('',#67807) ;
#5067 = PLANE('',#67812) ;
#5068 = PLANE('',#67831) ;
#5069 = PLANE('',#67850) ;
#5070 = PLANE('',#67881) ;
#5071 = PLANE('',#67912) ;
#5072 = PLANE('',#67915) ;
#5073 = PLANE('',#67918) ;
#5074 = PLANE('',#67919) ;
#5075 = PLANE('',#67920) ;
#5076 = PLANE('',#67921) ;
#5077 = PLANE('',#67922) ;
#5078 = PLANE('',#67923) ;
#5079 = PLANE('',#67926) ;
#5080 = PLANE('',#67933) ;
#5081 = PLANE('',#67934) ;
#5082 = PLANE('',#67935) ;
#5083 = PLANE('',#67936) ;
#5084 = PLANE('',#67937) ;
#5085 = PLANE('',#67938) ;
#5086 = PLANE('',#67939) ;
#5087 = PLANE('',#67940) ;
#5088 = PLANE('',#67941) ;
#5089 = PLANE('',#67942) ;
#5090 = PLANE('',#67943) ;
#5091 = PLANE('',#67944) ;
#5092 = PLANE('',#67945) ;
#5093 = PLANE('',#67946) ;
#5094 = PLANE('',#67949) ;
#5095 = PLANE('',#67954) ;
#5096 = PLANE('',#67957) ;
#5097 = PLANE('',#67964) ;
#5098 = PLANE('',#67965) ;
#5099 = PLANE('',#67966) ;
#5100 = PLANE('',#67967) ;
#5101 = PLANE('',#67968) ;
#5102 = PLANE('',#67969) ;
#5103 = PLANE('',#67970) ;
#5104 = PLANE('',#67971) ;
#5105 = PLANE('',#67972) ;
#5106 = PLANE('',#67973) ;
#5107 = PLANE('',#67974) ;
#5108 = PLANE('',#67975) ;
#5109 = PLANE('',#67976) ;
#5110 = PLANE('',#67977) ;
#5111 = PLANE('',#67978) ;
#5112 = PLANE('',#67979) ;
#5113 = PLANE('',#67980) ;
#5114 = PLANE('',#67981) ;
#5115 = PLANE('',#67982) ;
#5116 = PLANE('',#67983) ;
#5117 = PLANE('',#67984) ;
#5118 = PLANE('',#67985) ;
#5119 = PLANE('',#67986) ;
#5120 = PLANE('',#67987) ;
#5121 = PLANE('',#67988) ;
#5122 = PLANE('',#67989) ;
#5123 = PLANE('',#67990) ;
#5124 = PLANE('',#67991) ;
#5125 = PLANE('',#67992) ;
#5126 = PLANE('',#67993) ;
#5127 = PLANE('',#67994) ;
#5128 = PLANE('',#67995) ;
#5129 = PLANE('',#67996) ;
#5130 = PLANE('',#67997) ;
#5131 = PLANE('',#67998) ;
#5132 = PLANE('',#67999) ;
#5133 = PLANE('',#68000) ;
#5134 = PLANE('',#68001) ;
#5135 = PLANE('',#68002) ;
#5136 = PLANE('',#68003) ;
#5137 = PLANE('',#68004) ;
#5138 = PLANE('',#68005) ;
#5139 = PLANE('',#68006) ;
#5140 = PLANE('',#68007) ;
#5141 = PLANE('',#68008) ;
#5142 = PLANE('',#68009) ;
#5143 = PLANE('',#68010) ;
#5144 = PLANE('',#68011) ;
#5145 = PLANE('',#68012) ;
#5146 = PLANE('',#68013) ;
#5147 = PLANE('',#68014) ;
#5148 = PLANE('',#68015) ;
#5149 = PLANE('',#68016) ;
#5150 = PLANE('',#68017) ;
#5151 = PLANE('',#68018) ;
#5152 = PLANE('',#68019) ;
#5153 = PLANE('',#68811) ;
#5154 = PLANE('',#68813) ;
#5155 = PLANE('',#68814) ;
#5156 = PLANE('',#68815) ;
#5157 = PLANE('',#68816) ;
#5158 = PLANE('',#68817) ;
#5159 = PLANE('',#68818) ;
#5160 = PLANE('',#68820) ;
#5161 = PLANE('',#68837) ;
#5162 = PLANE('',#68854) ;
#5163 = PLANE('',#68855) ;
#5164 = PLANE('',#68856) ;
#5165 = PLANE('',#68857) ;
#5166 = PLANE('',#68859) ;
#5167 = PLANE('',#68860) ;
#5168 = PLANE('',#68861) ;
#5169 = PLANE('',#68864) ;
#5170 = PLANE('',#68878) ;
#5171 = PLANE('',#68881) ;
#5172 = PLANE('',#68884) ;
#5173 = PLANE('',#68886) ;
#5174 = PLANE('',#68888) ;
#5175 = PLANE('',#68889) ;
#5176 = PLANE('',#68890) ;
#5177 = PLANE('',#68891) ;
#5178 = PLANE('',#68892) ;
#5179 = PLANE('',#68893) ;
#5180 = PLANE('',#68894) ;
#5181 = PLANE('',#68899) ;
#5182 = PLANE('',#68903) ;
#5183 = PLANE('',#68904) ;
#5184 = PLANE('',#68911) ;
#5185 = PLANE('',#68912) ;
#5186 = PLANE('',#68913) ;
#5187 = PLANE('',#68917) ;
#5188 = PLANE('',#68919) ;
#5189 = PLANE('',#68923) ;
#5190 = PLANE('',#68927) ;
#5191 = PLANE('',#68928) ;
#5192 = PLANE('',#68929) ;
#5193 = PLANE('',#68931) ;
#5194 = PLANE('',#68932) ;
#5195 = PLANE('',#68936) ;
#5196 = PLANE('',#68937) ;
#5197 = PLANE('',#68938) ;
#5198 = PLANE('',#68939) ;
#5199 = PLANE('',#68940) ;
#5200 = PLANE('',#68941) ;
#5201 = PLANE('',#68942) ;
#5202 = PLANE('',#68943) ;
#5203 = PLANE('',#68944) ;
#5204 = PLANE('',#68947) ;
#5205 = PLANE('',#68953) ;
#5206 = PLANE('',#68954) ;
#5207 = PLANE('',#68955) ;
#5208 = PLANE('',#68956) ;
#5209 = PLANE('',#68957) ;
#5210 = PLANE('',#68961) ;
#5211 = PLANE('',#68962) ;
#5212 = PLANE('',#68963) ;
#5213 = PLANE('',#68964) ;
#5214 = PLANE('',#68965) ;
#5215 = PLANE('',#68971) ;
#5216 = PLANE('',#69421) ;
#5217 = PLANE('',#69423) ;
#5218 = PLANE('',#69424) ;
#5219 = PLANE('',#69425) ;
#5220 = PLANE('',#69426) ;
#5221 = PLANE('',#69427) ;
#5222 = PLANE('',#69428) ;
#5223 = PLANE('',#69430) ;
#5224 = PLANE('',#69447) ;
#5225 = PLANE('',#69464) ;
#5226 = PLANE('',#69465) ;
#5227 = PLANE('',#69466) ;
#5228 = PLANE('',#69467) ;
#5229 = PLANE('',#69469) ;
#5230 = PLANE('',#69470) ;
#5231 = PLANE('',#69471) ;
#5232 = PLANE('',#69474) ;
#5233 = PLANE('',#69488) ;
#5234 = PLANE('',#69491) ;
#5235 = PLANE('',#69494) ;
#5236 = PLANE('',#69496) ;
#5237 = PLANE('',#69498) ;
#5238 = PLANE('',#69499) ;
#5239 = PLANE('',#69500) ;
#5240 = PLANE('',#69501) ;
#5241 = PLANE('',#69502) ;
#5242 = PLANE('',#69503) ;
#5243 = PLANE('',#69504) ;
#5244 = PLANE('',#69509) ;
#5245 = PLANE('',#69513) ;
#5246 = PLANE('',#69514) ;
#5247 = PLANE('',#69521) ;
#5248 = PLANE('',#69522) ;
#5249 = PLANE('',#69523) ;
#5250 = PLANE('',#69527) ;
#5251 = PLANE('',#69529) ;
#5252 = PLANE('',#69533) ;
#5253 = PLANE('',#69537) ;
#5254 = PLANE('',#69538) ;
#5255 = PLANE('',#69539) ;
#5256 = PLANE('',#69541) ;
#5257 = PLANE('',#69542) ;
#5258 = PLANE('',#69546) ;
#5259 = PLANE('',#69547) ;
#5260 = PLANE('',#69548) ;
#5261 = PLANE('',#69549) ;
#5262 = PLANE('',#69550) ;
#5263 = PLANE('',#69551) ;
#5264 = PLANE('',#69552) ;
#5265 = PLANE('',#69553) ;
#5266 = PLANE('',#69554) ;
#5267 = PLANE('',#69557) ;
#5268 = PLANE('',#69563) ;
#5269 = PLANE('',#69564) ;
#5270 = PLANE('',#69565) ;
#5271 = PLANE('',#69566) ;
#5272 = PLANE('',#69567) ;
#5273 = PLANE('',#69571) ;
#5274 = PLANE('',#69572) ;
#5275 = PLANE('',#69573) ;
#5276 = PLANE('',#69574) ;
#5277 = PLANE('',#69575) ;
#5278 = PLANE('',#69581) ;
#5279 = PLANE('',#70031) ;
#5280 = PLANE('',#70033) ;
#5281 = PLANE('',#70034) ;
#5282 = PLANE('',#70035) ;
#5283 = PLANE('',#70036) ;
#5284 = PLANE('',#70037) ;
#5285 = PLANE('',#70038) ;
#5286 = PLANE('',#70040) ;
#5287 = PLANE('',#70057) ;
#5288 = PLANE('',#70074) ;
#5289 = PLANE('',#70075) ;
#5290 = PLANE('',#70076) ;
#5291 = PLANE('',#70077) ;
#5292 = PLANE('',#70079) ;
#5293 = PLANE('',#70080) ;
#5294 = PLANE('',#70081) ;
#5295 = PLANE('',#70084) ;
#5296 = PLANE('',#70098) ;
#5297 = PLANE('',#70101) ;
#5298 = PLANE('',#70104) ;
#5299 = PLANE('',#70106) ;
#5300 = PLANE('',#70108) ;
#5301 = PLANE('',#70109) ;
#5302 = PLANE('',#70110) ;
#5303 = PLANE('',#70111) ;
#5304 = PLANE('',#70112) ;
#5305 = PLANE('',#70113) ;
#5306 = PLANE('',#70114) ;
#5307 = PLANE('',#70119) ;
#5308 = PLANE('',#70123) ;
#5309 = PLANE('',#70124) ;
#5310 = PLANE('',#70131) ;
#5311 = PLANE('',#70132) ;
#5312 = PLANE('',#70133) ;
#5313 = PLANE('',#70137) ;
#5314 = PLANE('',#70139) ;
#5315 = PLANE('',#70143) ;
#5316 = PLANE('',#70147) ;
#5317 = PLANE('',#70148) ;
#5318 = PLANE('',#70149) ;
#5319 = PLANE('',#70151) ;
#5320 = PLANE('',#70152) ;
#5321 = PLANE('',#70156) ;
#5322 = PLANE('',#70157) ;
#5323 = PLANE('',#70158) ;
#5324 = PLANE('',#70159) ;
#5325 = PLANE('',#70160) ;
#5326 = PLANE('',#70161) ;
#5327 = PLANE('',#70162) ;
#5328 = PLANE('',#70163) ;
#5329 = PLANE('',#70164) ;
#5330 = PLANE('',#70167) ;
#5331 = PLANE('',#70173) ;
#5332 = PLANE('',#70174) ;
#5333 = PLANE('',#70175) ;
#5334 = PLANE('',#70176) ;
#5335 = PLANE('',#70177) ;
#5336 = PLANE('',#70181) ;
#5337 = PLANE('',#70182) ;
#5338 = PLANE('',#70183) ;
#5339 = PLANE('',#70184) ;
#5340 = PLANE('',#70185) ;
#5341 = PLANE('',#70191) ;
#5342 = PLANE('',#70641) ;
#5343 = PLANE('',#70643) ;
#5344 = PLANE('',#70644) ;
#5345 = PLANE('',#70645) ;
#5346 = PLANE('',#70646) ;
#5347 = PLANE('',#70647) ;
#5348 = PLANE('',#70648) ;
#5349 = PLANE('',#70650) ;
#5350 = PLANE('',#70667) ;
#5351 = PLANE('',#70684) ;
#5352 = PLANE('',#70685) ;
#5353 = PLANE('',#70686) ;
#5354 = PLANE('',#70687) ;
#5355 = PLANE('',#70689) ;
#5356 = PLANE('',#70690) ;
#5357 = PLANE('',#70691) ;
#5358 = PLANE('',#70694) ;
#5359 = PLANE('',#70708) ;
#5360 = PLANE('',#70711) ;
#5361 = PLANE('',#70714) ;
#5362 = PLANE('',#70716) ;
#5363 = PLANE('',#70718) ;
#5364 = PLANE('',#70719) ;
#5365 = PLANE('',#70720) ;
#5366 = PLANE('',#70721) ;
#5367 = PLANE('',#70722) ;
#5368 = PLANE('',#70723) ;
#5369 = PLANE('',#70724) ;
#5370 = PLANE('',#70729) ;
#5371 = PLANE('',#70733) ;
#5372 = PLANE('',#70734) ;
#5373 = PLANE('',#70741) ;
#5374 = PLANE('',#70742) ;
#5375 = PLANE('',#70743) ;
#5376 = PLANE('',#70747) ;
#5377 = PLANE('',#70749) ;
#5378 = PLANE('',#70753) ;
#5379 = PLANE('',#70757) ;
#5380 = PLANE('',#70758) ;
#5381 = PLANE('',#70759) ;
#5382 = PLANE('',#70761) ;
#5383 = PLANE('',#70762) ;
#5384 = PLANE('',#70766) ;
#5385 = PLANE('',#70767) ;
#5386 = PLANE('',#70768) ;
#5387 = PLANE('',#70769) ;
#5388 = PLANE('',#70770) ;
#5389 = PLANE('',#70771) ;
#5390 = PLANE('',#70772) ;
#5391 = PLANE('',#70773) ;
#5392 = PLANE('',#70774) ;
#5393 = PLANE('',#70777) ;
#5394 = PLANE('',#70783) ;
#5395 = PLANE('',#70784) ;
#5396 = PLANE('',#70785) ;
#5397 = PLANE('',#70786) ;
#5398 = PLANE('',#70787) ;
#5399 = PLANE('',#70791) ;
#5400 = PLANE('',#70792) ;
#5401 = PLANE('',#70793) ;
#5402 = PLANE('',#70794) ;
#5403 = PLANE('',#70795) ;
#5404 = PLANE('',#70801) ;
#5405 = PLANE('',#71251) ;
#5406 = PLANE('',#71253) ;
#5407 = PLANE('',#71254) ;
#5408 = PLANE('',#71255) ;
#5409 = PLANE('',#71256) ;
#5410 = PLANE('',#71257) ;
#5411 = PLANE('',#71258) ;
#5412 = PLANE('',#71260) ;
#5413 = PLANE('',#71277) ;
#5414 = PLANE('',#71294) ;
#5415 = PLANE('',#71295) ;
#5416 = PLANE('',#71296) ;
#5417 = PLANE('',#71297) ;
#5418 = PLANE('',#71299) ;
#5419 = PLANE('',#71300) ;
#5420 = PLANE('',#71301) ;
#5421 = PLANE('',#71304) ;
#5422 = PLANE('',#71318) ;
#5423 = PLANE('',#71321) ;
#5424 = PLANE('',#71324) ;
#5425 = PLANE('',#71326) ;
#5426 = PLANE('',#71328) ;
#5427 = PLANE('',#71329) ;
#5428 = PLANE('',#71330) ;
#5429 = PLANE('',#71331) ;
#5430 = PLANE('',#71332) ;
#5431 = PLANE('',#71333) ;
#5432 = PLANE('',#71334) ;
#5433 = PLANE('',#71339) ;
#5434 = PLANE('',#71343) ;
#5435 = PLANE('',#71344) ;
#5436 = PLANE('',#71351) ;
#5437 = PLANE('',#71352) ;
#5438 = PLANE('',#71353) ;
#5439 = PLANE('',#71357) ;
#5440 = PLANE('',#71359) ;
#5441 = PLANE('',#71363) ;
#5442 = PLANE('',#71367) ;
#5443 = PLANE('',#71368) ;
#5444 = PLANE('',#71369) ;
#5445 = PLANE('',#71371) ;
#5446 = PLANE('',#71372) ;
#5447 = PLANE('',#71376) ;
#5448 = PLANE('',#71377) ;
#5449 = PLANE('',#71378) ;
#5450 = PLANE('',#71379) ;
#5451 = PLANE('',#71380) ;
#5452 = PLANE('',#71381) ;
#5453 = PLANE('',#71382) ;
#5454 = PLANE('',#71383) ;
#5455 = PLANE('',#71384) ;
#5456 = PLANE('',#71387) ;
#5457 = PLANE('',#71393) ;
#5458 = PLANE('',#71394) ;
#5459 = PLANE('',#71395) ;
#5460 = PLANE('',#71396) ;
#5461 = PLANE('',#71397) ;
#5462 = PLANE('',#71401) ;
#5463 = PLANE('',#71402) ;
#5464 = PLANE('',#71403) ;
#5465 = PLANE('',#71404) ;
#5466 = PLANE('',#71405) ;
#5467 = PLANE('',#71411) ;
#5468 = PLANE('',#71837) ;
#5469 = PLANE('',#71840) ;
#5470 = PLANE('',#71843) ;
#5471 = PLANE('',#71844) ;
#5472 = PLANE('',#71847) ;
#5473 = PLANE('',#71848) ;
#5474 = PLANE('',#71851) ;
#5475 = PLANE('',#71852) ;
#5476 = PLANE('',#71853) ;
#5477 = PLANE('',#71854) ;
#5478 = PLANE('',#71859) ;
#5479 = PLANE('',#71860) ;
#5480 = PLANE('',#71861) ;
#5481 = PLANE('',#71864) ;
#5482 = PLANE('',#71865) ;
#5483 = PLANE('',#72117) ;
#5484 = PLANE('',#72122) ;
#5485 = PLANE('',#72127) ;
#5486 = PLANE('',#72132) ;
#5487 = PLANE('',#72137) ;
#5488 = PLANE('',#72142) ;
#5489 = PLANE('',#72147) ;
#5490 = PLANE('',#72152) ;
#5491 = PLANE('',#72157) ;
#5492 = PLANE('',#72162) ;
#5493 = PLANE('',#72164) ;
#5494 = PLANE('',#72166) ;
#5495 = PLANE('',#72168) ;
#5496 = PLANE('',#72170) ;
#5497 = PLANE('',#72172) ;
#5498 = PLANE('',#72174) ;
#5499 = PLANE('',#72176) ;
#5500 = PLANE('',#72178) ;
#5501 = PLANE('',#72180) ;
#5502 = PLANE('',#72182) ;
#5503 = PLANE('',#72184) ;
#5504 = PLANE('',#72186) ;
#5505 = PLANE('',#72188) ;
#5506 = PLANE('',#72190) ;
#5507 = PLANE('',#72192) ;
#5508 = PLANE('',#72194) ;
#5509 = PLANE('',#72196) ;
#5510 = PLANE('',#72225) ;
#5511 = PLANE('',#72230) ;
#5512 = PLANE('',#72232) ;
#5513 = PLANE('',#72240) ;
#5514 = PLANE('',#72264) ;
#5515 = PLANE('',#72288) ;
#5516 = PLANE('',#72292) ;
#5517 = PLANE('',#72296) ;
#5518 = PLANE('',#72300) ;
#5519 = PLANE('',#72304) ;
#5520 = PLANE('',#72308) ;
#5521 = PLANE('',#72409) ;
#5522 = PLANE('',#72412) ;
#5523 = PLANE('',#72415) ;
#5524 = PLANE('',#72418) ;
#5525 = PLANE('',#72419) ;
#5526 = PLANE('',#72420) ;
#5527 = PLANE('',#72421) ;
#5528 = PLANE('',#72422) ;
#5529 = PLANE('',#72426) ;
#5530 = PLANE('',#72430) ;
#5531 = PLANE('',#72434) ;
#5532 = PLANE('',#72437) ;
#5533 = PLANE('',#72438) ;
#5534 = PLANE('',#72442) ;
#5535 = PLANE('',#72446) ;
#5536 = PLANE('',#72450) ;
#5537 = PLANE('',#72454) ;
#5538 = PLANE('',#72458) ;
#5539 = PLANE('',#72468) ;
#5540 = PLANE('',#72472) ;
#5541 = PLANE('',#72476) ;
#5542 = PLANE('',#72477) ;
#5543 = PLANE('',#72483) ;
#5544 = PLANE('',#72758) ;
#5545 = PLANE('',#72759) ;
#5546 = PLANE('',#72760) ;
#5547 = PLANE('',#72761) ;
#5548 = PLANE('',#72762) ;
#5549 = PLANE('',#72763) ;
#5550 = PLANE('',#72766) ;
#5551 = PLANE('',#72775) ;
#5552 = PLANE('',#72776) ;
#5553 = PLANE('',#72777) ;
#5554 = PLANE('',#72778) ;
#5555 = PLANE('',#72779) ;
#5556 = PLANE('',#72780) ;
#5557 = PLANE('',#72781) ;
#5558 = PLANE('',#72782) ;
#5559 = PLANE('',#72783) ;
#5560 = PLANE('',#72784) ;
#5561 = PLANE('',#72785) ;
#5562 = PLANE('',#72898) ;
#5563 = PLANE('',#72901) ;
#5564 = PLANE('',#72904) ;
#5565 = PLANE('',#72907) ;
#5566 = PLANE('',#72910) ;
#5567 = PLANE('',#72913) ;
#5568 = PLANE('',#72916) ;
#5569 = PLANE('',#72919) ;
#5570 = PLANE('',#72922) ;
#5571 = PLANE('',#72925) ;
#5572 = PLANE('',#72926) ;
#5573 = PLANE('',#72927) ;
#5574 = PLANE('',#72928) ;
#5575 = PLANE('',#72929) ;
#5576 = PLANE('',#72930) ;
#5577 = PLANE('',#72931) ;
#5578 = PLANE('',#72932) ;
#5579 = PLANE('',#72933) ;
#5580 = PLANE('',#72934) ;
#5581 = PLANE('',#72935) ;
#5582 = PLANE('',#72936) ;
#5583 = PLANE('',#72937) ;
#5584 = PLANE('',#72938) ;
#5585 = PLANE('',#72939) ;
#5586 = PLANE('',#72940) ;
#5587 = PLANE('',#72941) ;
#5588 = PLANE('',#72942) ;
#5589 = PLANE('',#72943) ;
#5590 = PLANE('',#72944) ;
#5591 = PLANE('',#72945) ;
#5592 = PLANE('',#72946) ;
#5593 = PLANE('',#72947) ;
#5594 = PLANE('',#72948) ;
#5595 = PLANE('',#72949) ;
#5596 = PLANE('',#72950) ;
#5597 = PLANE('',#72951) ;
#5598 = PLANE('',#72952) ;
#5599 = PLANE('',#72953) ;
#5600 = PLANE('',#72954) ;
#5601 = PLANE('',#72955) ;
#5602 = PLANE('',#72956) ;
#5603 = PLANE('',#72957) ;
#5604 = PLANE('',#72958) ;
#5605 = PLANE('',#72959) ;
#5606 = PLANE('',#72960) ;
#5607 = PLANE('',#72961) ;
#5608 = PLANE('',#72962) ;
#5609 = PLANE('',#72963) ;
#5610 = PLANE('',#72964) ;
#5611 = PLANE('',#72965) ;
#5612 = PLANE('',#72966) ;
#5613 = PLANE('',#72967) ;
#5614 = PLANE('',#72968) ;
#5615 = PLANE('',#72969) ;
#5616 = PLANE('',#72973) ;
#5617 = PLANE('',#72977) ;
#5618 = PLANE('',#72981) ;
#5619 = PLANE('',#72984) ;
#5620 = PLANE('',#72985) ;
#5621 = PLANE('',#72989) ;
#5622 = PLANE('',#72993) ;
#5623 = PLANE('',#72997) ;
#5624 = PLANE('',#73001) ;
#5625 = PLANE('',#73005) ;
#5626 = PLANE('',#73015) ;
#5627 = PLANE('',#73019) ;
#5628 = PLANE('',#73023) ;
#5629 = PLANE('',#73024) ;
#5630 = PLANE('',#73033) ;
#5631 = PLANE('',#73037) ;
#5632 = PLANE('',#73041) ;
#5633 = PLANE('',#73044) ;
#5634 = PLANE('',#73045) ;
#5635 = PLANE('',#73049) ;
#5636 = PLANE('',#73053) ;
#5637 = PLANE('',#73057) ;
#5638 = PLANE('',#73061) ;
#5639 = PLANE('',#73065) ;
#5640 = PLANE('',#73075) ;
#5641 = PLANE('',#73079) ;
#5642 = PLANE('',#73083) ;
#5643 = PLANE('',#73084) ;
#5644 = PLANE('',#73093) ;
#5645 = PLANE('',#73097) ;
#5646 = PLANE('',#73101) ;
#5647 = PLANE('',#73104) ;
#5648 = PLANE('',#73105) ;
#5649 = PLANE('',#73109) ;
#5650 = PLANE('',#73113) ;
#5651 = PLANE('',#73117) ;
#5652 = PLANE('',#73121) ;
#5653 = PLANE('',#73125) ;
#5654 = PLANE('',#73135) ;
#5655 = PLANE('',#73139) ;
#5656 = PLANE('',#73143) ;
#5657 = PLANE('',#73144) ;
#5658 = PLANE('',#73153) ;
#5659 = PLANE('',#73157) ;
#5660 = PLANE('',#73161) ;
#5661 = PLANE('',#73164) ;
#5662 = PLANE('',#73165) ;
#5663 = PLANE('',#73169) ;
#5664 = PLANE('',#73173) ;
#5665 = PLANE('',#73177) ;
#5666 = PLANE('',#73181) ;
#5667 = PLANE('',#73185) ;
#5668 = PLANE('',#73195) ;
#5669 = PLANE('',#73199) ;
#5670 = PLANE('',#73203) ;
#5671 = PLANE('',#73204) ;
#5672 = PLANE('',#73213) ;
#5673 = PLANE('',#73217) ;
#5674 = PLANE('',#73221) ;
#5675 = PLANE('',#73224) ;
#5676 = PLANE('',#73225) ;
#5677 = PLANE('',#73229) ;
#5678 = PLANE('',#73233) ;
#5679 = PLANE('',#73237) ;
#5680 = PLANE('',#73241) ;
#5681 = PLANE('',#73245) ;
#5682 = PLANE('',#73255) ;
#5683 = PLANE('',#73259) ;
#5684 = PLANE('',#73263) ;
#5685 = PLANE('',#73264) ;
#5686 = PLANE('',#73273) ;
#5687 = PLANE('',#73277) ;
#5688 = PLANE('',#73281) ;
#5689 = PLANE('',#73284) ;
#5690 = PLANE('',#73285) ;
#5691 = PLANE('',#73289) ;
#5692 = PLANE('',#73293) ;
#5693 = PLANE('',#73297) ;
#5694 = PLANE('',#73301) ;
#5695 = PLANE('',#73305) ;
#5696 = PLANE('',#73315) ;
#5697 = PLANE('',#73319) ;
#5698 = PLANE('',#73323) ;
#5699 = PLANE('',#73324) ;
#5700 = PLANE('',#73333) ;
#5701 = PLANE('',#73337) ;
#5702 = PLANE('',#73341) ;
#5703 = PLANE('',#73344) ;
#5704 = PLANE('',#73345) ;
#5705 = PLANE('',#73349) ;
#5706 = PLANE('',#73353) ;
#5707 = PLANE('',#73357) ;
#5708 = PLANE('',#73361) ;
#5709 = PLANE('',#73365) ;
#5710 = PLANE('',#73375) ;
#5711 = PLANE('',#73379) ;
#5712 = PLANE('',#73383) ;
#5713 = PLANE('',#73384) ;
#5714 = PLANE('',#73393) ;
#5715 = PLANE('',#73397) ;
#5716 = PLANE('',#73401) ;
#5717 = PLANE('',#73404) ;
#5718 = PLANE('',#73405) ;
#5719 = PLANE('',#73409) ;
#5720 = PLANE('',#73413) ;
#5721 = PLANE('',#73417) ;
#5722 = PLANE('',#73421) ;
#5723 = PLANE('',#73425) ;
#5724 = PLANE('',#73435) ;
#5725 = PLANE('',#73439) ;
#5726 = PLANE('',#73443) ;
#5727 = PLANE('',#73444) ;
#5728 = PLANE('',#73453) ;
#5729 = PLANE('',#73457) ;
#5730 = PLANE('',#73461) ;
#5731 = PLANE('',#73464) ;
#5732 = PLANE('',#73465) ;
#5733 = PLANE('',#73469) ;
#5734 = PLANE('',#73473) ;
#5735 = PLANE('',#73477) ;
#5736 = PLANE('',#73481) ;
#5737 = PLANE('',#73485) ;
#5738 = PLANE('',#73495) ;
#5739 = PLANE('',#73499) ;
#5740 = PLANE('',#73503) ;
#5741 = PLANE('',#73504) ;
#5742 = PLANE('',#73510) ;
#5743 = PLANE('',#73515) ;
#5744 = PLANE('',#73520) ;
#5745 = PLANE('',#73525) ;
#5746 = PLANE('',#73530) ;
#5747 = PLANE('',#73535) ;
#5748 = PLANE('',#73540) ;
#5749 = PLANE('',#73545) ;
#5750 = PLANE('',#73550) ;
#5751 = PLANE('',#75409) ;
#5752 = PLANE('',#75410) ;
#5753 = PLANE('',#75411) ;
#5754 = PLANE('',#75412) ;
#5755 = PLANE('',#75413) ;
#5756 = PLANE('',#75414) ;
#5757 = PLANE('',#75417) ;
#5758 = PLANE('',#75426) ;
#5759 = PLANE('',#75427) ;
#5760 = PLANE('',#75428) ;
#5761 = PLANE('',#75429) ;
#5762 = PLANE('',#75430) ;
#5763 = PLANE('',#75431) ;
#5764 = PLANE('',#75432) ;
#5765 = PLANE('',#75433) ;
#5766 = PLANE('',#75434) ;
#5767 = PLANE('',#75435) ;
#5768 = PLANE('',#75436) ;
#5769 = PLANE('',#75437) ;
#5770 = PLANE('',#75438) ;
#5771 = PLANE('',#75441) ;
#5772 = PLANE('',#75450) ;
#5773 = PLANE('',#75451) ;
#5774 = PLANE('',#75452) ;
#5775 = PLANE('',#75453) ;
#5776 = PLANE('',#75454) ;
#5777 = PLANE('',#75455) ;
#5778 = PLANE('',#75456) ;
#5779 = PLANE('',#75457) ;
#5780 = PLANE('',#75458) ;
#5781 = PLANE('',#75459) ;
#5782 = PLANE('',#75460) ;
#5783 = PLANE('',#75461) ;
#5784 = PLANE('',#75462) ;
#5785 = PLANE('',#75465) ;
#5786 = PLANE('',#75474) ;
#5787 = PLANE('',#75475) ;
#5788 = PLANE('',#75476) ;
#5789 = PLANE('',#75477) ;
#5790 = PLANE('',#75478) ;
#5791 = PLANE('',#75479) ;
#5792 = PLANE('',#75480) ;
#5793 = PLANE('',#75481) ;
#5794 = PLANE('',#75482) ;
#5795 = PLANE('',#75483) ;
#5796 = PLANE('',#75484) ;
#5797 = PLANE('',#75485) ;
#5798 = PLANE('',#75486) ;
#5799 = PLANE('',#75489) ;
#5800 = PLANE('',#75498) ;
#5801 = PLANE('',#75499) ;
#5802 = PLANE('',#75500) ;
#5803 = PLANE('',#75501) ;
#5804 = PLANE('',#75502) ;
#5805 = PLANE('',#75503) ;
#5806 = PLANE('',#75504) ;
#5807 = PLANE('',#75505) ;
#5808 = PLANE('',#75506) ;
#5809 = PLANE('',#75507) ;
#5810 = PLANE('',#75508) ;
#5811 = PLANE('',#75509) ;
#5812 = PLANE('',#75510) ;
#5813 = PLANE('',#75513) ;
#5814 = PLANE('',#75522) ;
#5815 = PLANE('',#75523) ;
#5816 = PLANE('',#75524) ;
#5817 = PLANE('',#75525) ;
#5818 = PLANE('',#75526) ;
#5819 = PLANE('',#75527) ;
#5820 = PLANE('',#75528) ;
#5821 = PLANE('',#75529) ;
#5822 = PLANE('',#75530) ;
#5823 = PLANE('',#75531) ;
#5824 = PLANE('',#75532) ;
#5825 = PLANE('',#75533) ;
#5826 = PLANE('',#75534) ;
#5827 = PLANE('',#75537) ;
#5828 = PLANE('',#75546) ;
#5829 = PLANE('',#75547) ;
#5830 = PLANE('',#75548) ;
#5831 = PLANE('',#75549) ;
#5832 = PLANE('',#75550) ;
#5833 = PLANE('',#75551) ;
#5834 = PLANE('',#75552) ;
#5835 = PLANE('',#75553) ;
#5836 = PLANE('',#75554) ;
#5837 = PLANE('',#75555) ;
#5838 = PLANE('',#75556) ;
#5839 = PLANE('',#75557) ;
#5840 = PLANE('',#75558) ;
#5841 = PLANE('',#75561) ;
#5842 = PLANE('',#75570) ;
#5843 = PLANE('',#75571) ;
#5844 = PLANE('',#75572) ;
#5845 = PLANE('',#75573) ;
#5846 = PLANE('',#75574) ;
#5847 = PLANE('',#75575) ;
#5848 = PLANE('',#75576) ;
#5849 = PLANE('',#75577) ;
#5850 = PLANE('',#75578) ;
#5851 = PLANE('',#75579) ;
#5852 = PLANE('',#75580) ;
#5853 = PLANE('',#75581) ;
#5854 = PLANE('',#75582) ;
#5855 = PLANE('',#75585) ;
#5856 = PLANE('',#75594) ;
#5857 = PLANE('',#75595) ;
#5858 = PLANE('',#75596) ;
#5859 = PLANE('',#75597) ;
#5860 = PLANE('',#75598) ;
#5861 = PLANE('',#75599) ;
#5862 = PLANE('',#75600) ;
#5863 = PLANE('',#75601) ;
#5864 = PLANE('',#75602) ;
#5865 = PLANE('',#75603) ;
#5866 = PLANE('',#75604) ;
#5867 = PLANE('',#75605) ;
#5868 = PLANE('',#75606) ;
#5869 = PLANE('',#75609) ;
#5870 = PLANE('',#75618) ;
#5871 = PLANE('',#75619) ;
#5872 = PLANE('',#75620) ;
#5873 = PLANE('',#75621) ;
#5874 = PLANE('',#75622) ;
#5875 = PLANE('',#75623) ;
#5876 = PLANE('',#75624) ;
#5877 = PLANE('',#75625) ;
#5878 = PLANE('',#75626) ;
#5879 = PLANE('',#75627) ;
#5880 = PLANE('',#75628) ;
#5881 = PLANE('',#75629) ;
#5882 = PLANE('',#75630) ;
#5883 = PLANE('',#75631) ;
#5884 = PLANE('',#75632) ;
#5885 = PLANE('',#75633) ;
#5886 = PLANE('',#75634) ;
#5887 = PLANE('',#75635) ;
#5888 = PLANE('',#75636) ;
#5889 = PLANE('',#75637) ;
#5890 = PLANE('',#75638) ;
#5891 = PLANE('',#75639) ;
#5892 = PLANE('',#75640) ;
#5893 = PLANE('',#75641) ;
#5894 = PLANE('',#75642) ;
#5895 = PLANE('',#75643) ;
#5896 = PLANE('',#75644) ;
#5897 = PLANE('',#75645) ;
#5898 = PLANE('',#75646) ;
#5899 = PLANE('',#75647) ;
#5900 = PLANE('',#75648) ;
#5901 = PLANE('',#75649) ;
#5902 = PLANE('',#75650) ;
#5903 = PLANE('',#75651) ;
#5904 = PLANE('',#75652) ;
#5905 = PLANE('',#75653) ;
#5906 = PLANE('',#75654) ;
#5907 = PLANE('',#75655) ;
#5908 = PLANE('',#75656) ;
#5909 = PLANE('',#75657) ;
#5910 = PLANE('',#75658) ;
#5911 = PLANE('',#75659) ;
#5912 = PLANE('',#75660) ;
#5913 = PLANE('',#76749) ;
#5914 = PLANE('',#76750) ;
#5915 = PLANE('',#76751) ;
#5916 = PLANE('',#76752) ;
#5917 = PLANE('',#76753) ;
#5918 = PLANE('',#76754) ;
#5919 = PLANE('',#76755) ;
#5920 = PLANE('',#76756) ;
#5921 = PLANE('',#76757) ;
#5922 = PLANE('',#76759) ;
#5923 = PLANE('',#76760) ;
#5924 = PLANE('',#76761) ;
#5925 = PLANE('',#76812) ;
#5926 = PLANE('',#76813) ;
#5927 = PLANE('',#76814) ;
#5928 = PLANE('',#76815) ;
#5929 = PLANE('',#76816) ;
#5930 = PLANE('',#76818) ;
#5931 = PLANE('',#76820) ;
#5932 = PLANE('',#76821) ;
#5933 = PLANE('',#76822) ;
#5934 = PLANE('',#76823) ;
#5935 = PLANE('',#76824) ;
#5936 = PLANE('',#76825) ;
#5937 = PLANE('',#76826) ;
#5938 = PLANE('',#76827) ;
#5939 = PLANE('',#76828) ;
#5940 = PLANE('',#76829) ;
#5941 = PLANE('',#76830) ;
#5942 = PLANE('',#76832) ;
#5943 = PLANE('',#76833) ;
#5944 = PLANE('',#76834) ;
#5945 = PLANE('',#76835) ;
#5946 = PLANE('',#76836) ;
#5947 = CYLINDRICAL_SURFACE('',#67797,1.49999999999999) ;
#5948 = CYLINDRICAL_SURFACE('',#67800,1.49999999999999) ;
#5949 = CYLINDRICAL_SURFACE('',#67801,1.6) ;
#5950 = CYLINDRICAL_SURFACE('',#67929,1.75) ;
#5951 = CYLINDRICAL_SURFACE('',#67931,1.) ;
#5952 = CYLINDRICAL_SURFACE('',#67952,1.75) ;
#5953 = CYLINDRICAL_SURFACE('',#67953,1.) ;
#5954 = CYLINDRICAL_SURFACE('',#67960,1.75) ;
#5955 = CYLINDRICAL_SURFACE('',#67962,1.) ;
#5956 = CYLINDRICAL_SURFACE('',#68020,0.149999999999997) ;
#5957 = CYLINDRICAL_SURFACE('',#68023,0.15) ;
#5958 = CYLINDRICAL_SURFACE('',#68028,0.149999999999997) ;
#5959 = CYLINDRICAL_SURFACE('',#68030,0.149999999999997) ;
#5960 = CYLINDRICAL_SURFACE('',#68032,0.149999999999997) ;
#5961 = CYLINDRICAL_SURFACE('',#68039,0.149999999999997) ;
#5962 = CYLINDRICAL_SURFACE('',#68041,0.15) ;
#5963 = CYLINDRICAL_SURFACE('',#68043,0.149999999999997) ;
#5964 = CYLINDRICAL_SURFACE('',#68050,0.149999999999997) ;
#5965 = CYLINDRICAL_SURFACE('',#68052,0.15) ;
#5966 = CYLINDRICAL_SURFACE('',#68054,0.149999999999997) ;
#5967 = CYLINDRICAL_SURFACE('',#68061,0.149999999999997) ;
#5968 = CYLINDRICAL_SURFACE('',#68063,0.15) ;
#5969 = CYLINDRICAL_SURFACE('',#68065,0.149999999999997) ;
#5970 = CYLINDRICAL_SURFACE('',#68072,0.149999999999997) ;
#5971 = CYLINDRICAL_SURFACE('',#68074,0.15) ;
#5972 = CYLINDRICAL_SURFACE('',#68076,0.149999999999997) ;
#5973 = CYLINDRICAL_SURFACE('',#68078,0.149999999999997) ;
#5974 = CYLINDRICAL_SURFACE('',#68089,0.15) ;
#5975 = CYLINDRICAL_SURFACE('',#68091,0.149999999999997) ;
#5976 = CYLINDRICAL_SURFACE('',#68093,0.15) ;
#5977 = CYLINDRICAL_SURFACE('',#68095,0.149999999999997) ;
#5978 = CYLINDRICAL_SURFACE('',#68097,0.150000000000001) ;
#5979 = CYLINDRICAL_SURFACE('',#68099,0.150000000000001) ;
#5980 = CYLINDRICAL_SURFACE('',#68101,0.149999999999997) ;
#5981 = CYLINDRICAL_SURFACE('',#68112,0.149999999999997) ;
#5982 = CYLINDRICAL_SURFACE('',#68114,0.15) ;
#5983 = CYLINDRICAL_SURFACE('',#68116,0.15) ;
#5984 = CYLINDRICAL_SURFACE('',#68118,0.15) ;
#5985 = CYLINDRICAL_SURFACE('',#68120,0.150000000000001) ;
#5986 = CYLINDRICAL_SURFACE('',#68132,0.15) ;
#5987 = CYLINDRICAL_SURFACE('',#68134,0.150000000000001) ;
#5988 = CYLINDRICAL_SURFACE('',#68136,0.15) ;
#5989 = CYLINDRICAL_SURFACE('',#68138,0.15) ;
#5990 = CYLINDRICAL_SURFACE('',#68140,0.15) ;
#5991 = CYLINDRICAL_SURFACE('',#68142,0.15) ;
#5992 = CYLINDRICAL_SURFACE('',#68154,0.15) ;
#5993 = CYLINDRICAL_SURFACE('',#68156,0.150000000000001) ;
#5994 = CYLINDRICAL_SURFACE('',#68158,0.15) ;
#5995 = CYLINDRICAL_SURFACE('',#68160,0.15) ;
#5996 = CYLINDRICAL_SURFACE('',#68162,0.15) ;
#5997 = CYLINDRICAL_SURFACE('',#68164,0.15) ;
#5998 = CYLINDRICAL_SURFACE('',#68179,0.15) ;
#5999 = CYLINDRICAL_SURFACE('',#68181,0.150000000000001) ;
#6000 = CYLINDRICAL_SURFACE('',#68183,0.15) ;
#6001 = CYLINDRICAL_SURFACE('',#68185,0.15) ;
#6002 = CYLINDRICAL_SURFACE('',#68187,0.15) ;
#6003 = CYLINDRICAL_SURFACE('',#68189,0.15) ;
#6004 = CYLINDRICAL_SURFACE('',#68191,0.15) ;
#6005 = CYLINDRICAL_SURFACE('',#68193,0.15) ;
#6006 = CYLINDRICAL_SURFACE('',#68203,0.15) ;
#6007 = CYLINDRICAL_SURFACE('',#68205,0.150000000000001) ;
#6008 = CYLINDRICAL_SURFACE('',#68207,0.15) ;
#6009 = CYLINDRICAL_SURFACE('',#68209,0.15) ;
#6010 = CYLINDRICAL_SURFACE('',#68215,0.15) ;
#6011 = CYLINDRICAL_SURFACE('',#68217,0.15) ;
#6012 = CYLINDRICAL_SURFACE('',#68220,0.149999999999997) ;
#6013 = CYLINDRICAL_SURFACE('',#68229,0.15) ;
#6014 = CYLINDRICAL_SURFACE('',#68231,0.149999999999997) ;
#6015 = CYLINDRICAL_SURFACE('',#68233,0.149999999999997) ;
#6016 = CYLINDRICAL_SURFACE('',#68236,0.149999999999997) ;
#6017 = CYLINDRICAL_SURFACE('',#68238,0.15) ;
#6018 = CYLINDRICAL_SURFACE('',#68240,0.149999999999997) ;
#6019 = CYLINDRICAL_SURFACE('',#68251,0.149999999999997) ;
#6020 = CYLINDRICAL_SURFACE('',#68253,0.150000000000001) ;
#6021 = CYLINDRICAL_SURFACE('',#68255,0.150000000000001) ;
#6022 = CYLINDRICAL_SURFACE('',#68257,0.149999999999997) ;
#6023 = CYLINDRICAL_SURFACE('',#68263,0.149999999999997) ;
#6024 = CYLINDRICAL_SURFACE('',#68264,0.149999999999997) ;
#6025 = CYLINDRICAL_SURFACE('',#68273,0.150000000000001) ;
#6026 = CYLINDRICAL_SURFACE('',#68275,0.149999999999997) ;
#6027 = CYLINDRICAL_SURFACE('',#68277,0.149999999999997) ;
#6028 = CYLINDRICAL_SURFACE('',#68280,0.149999999999997) ;
#6029 = CYLINDRICAL_SURFACE('',#68282,0.150000000000001) ;
#6030 = CYLINDRICAL_SURFACE('',#68284,0.149999999999997) ;
#6031 = CYLINDRICAL_SURFACE('',#68295,0.149999999999997) ;
#6032 = CYLINDRICAL_SURFACE('',#68297,0.15) ;
#6033 = CYLINDRICAL_SURFACE('',#68299,0.15) ;
#6034 = CYLINDRICAL_SURFACE('',#68301,0.149999999999997) ;
#6035 = CYLINDRICAL_SURFACE('',#68307,0.149999999999997) ;
#6036 = CYLINDRICAL_SURFACE('',#68308,0.149999999999997) ;
#6037 = CYLINDRICAL_SURFACE('',#68317,0.15) ;
#6038 = CYLINDRICAL_SURFACE('',#68319,0.149999999999997) ;
#6039 = CYLINDRICAL_SURFACE('',#68321,0.149999999999997) ;
#6040 = CYLINDRICAL_SURFACE('',#68324,0.149999999999997) ;
#6041 = CYLINDRICAL_SURFACE('',#68326,0.15) ;
#6042 = CYLINDRICAL_SURFACE('',#68328,0.149999999999997) ;
#6043 = CYLINDRICAL_SURFACE('',#68339,0.149999999999997) ;
#6044 = CYLINDRICAL_SURFACE('',#68341,0.150000000000001) ;
#6045 = CYLINDRICAL_SURFACE('',#68343,0.150000000000001) ;
#6046 = CYLINDRICAL_SURFACE('',#68345,0.149999999999997) ;
#6047 = CYLINDRICAL_SURFACE('',#68351,0.149999999999997) ;
#6048 = CYLINDRICAL_SURFACE('',#68352,0.149999999999997) ;
#6049 = CYLINDRICAL_SURFACE('',#68361,0.150000000000001) ;
#6050 = CYLINDRICAL_SURFACE('',#68363,0.149999999999997) ;
#6051 = CYLINDRICAL_SURFACE('',#68365,0.149999999999997) ;
#6052 = CYLINDRICAL_SURFACE('',#68368,0.149999999999997) ;
#6053 = CYLINDRICAL_SURFACE('',#68370,0.150000000000001) ;
#6054 = CYLINDRICAL_SURFACE('',#68372,0.149999999999997) ;
#6055 = CYLINDRICAL_SURFACE('',#68383,0.149999999999997) ;
#6056 = CYLINDRICAL_SURFACE('',#68385,0.15) ;
#6057 = CYLINDRICAL_SURFACE('',#68387,0.15) ;
#6058 = CYLINDRICAL_SURFACE('',#68389,0.149999999999997) ;
#6059 = CYLINDRICAL_SURFACE('',#68395,0.149999999999997) ;
#6060 = CYLINDRICAL_SURFACE('',#68396,0.149999999999997) ;
#6061 = CYLINDRICAL_SURFACE('',#68405,0.149999999999997) ;
#6062 = CYLINDRICAL_SURFACE('',#68407,0.150000000000001) ;
#6063 = CYLINDRICAL_SURFACE('',#68409,0.149999999999997) ;
#6064 = CYLINDRICAL_SURFACE('',#68412,0.150000000000001) ;
#6065 = CYLINDRICAL_SURFACE('',#68414,0.149999999999997) ;
#6066 = CYLINDRICAL_SURFACE('',#68416,0.149999999999997) ;
#6067 = CYLINDRICAL_SURFACE('',#68427,0.15) ;
#6068 = CYLINDRICAL_SURFACE('',#68429,0.149999999999997) ;
#6069 = CYLINDRICAL_SURFACE('',#68431,0.149999999999997) ;
#6070 = CYLINDRICAL_SURFACE('',#68433,0.15) ;
#6071 = CYLINDRICAL_SURFACE('',#68439,0.149999999999997) ;
#6072 = CYLINDRICAL_SURFACE('',#68440,0.149999999999997) ;
#6073 = CYLINDRICAL_SURFACE('',#68449,0.149999999999997) ;
#6074 = CYLINDRICAL_SURFACE('',#68451,0.149999999999997) ;
#6075 = CYLINDRICAL_SURFACE('',#68453,0.149999999999997) ;
#6076 = CYLINDRICAL_SURFACE('',#68456,0.149999999999997) ;
#6077 = CYLINDRICAL_SURFACE('',#68458,0.149999999999997) ;
#6078 = CYLINDRICAL_SURFACE('',#68460,0.149999999999997) ;
#6079 = CYLINDRICAL_SURFACE('',#68471,0.149999999999997) ;
#6080 = CYLINDRICAL_SURFACE('',#68473,0.149999999999997) ;
#6081 = CYLINDRICAL_SURFACE('',#68475,0.149999999999997) ;
#6082 = CYLINDRICAL_SURFACE('',#68477,0.149999999999997) ;
#6083 = CYLINDRICAL_SURFACE('',#68483,0.149999999999997) ;
#6084 = CYLINDRICAL_SURFACE('',#68484,0.149999999999997) ;
#6085 = CYLINDRICAL_SURFACE('',#68493,0.149999999999997) ;
#6086 = CYLINDRICAL_SURFACE('',#68495,0.149999999999997) ;
#6087 = CYLINDRICAL_SURFACE('',#68497,0.149999999999997) ;
#6088 = CYLINDRICAL_SURFACE('',#68500,0.149999999999997) ;
#6089 = CYLINDRICAL_SURFACE('',#68502,0.149999999999997) ;
#6090 = CYLINDRICAL_SURFACE('',#68504,0.149999999999997) ;
#6091 = CYLINDRICAL_SURFACE('',#68515,0.149999999999997) ;
#6092 = CYLINDRICAL_SURFACE('',#68517,0.149999999999997) ;
#6093 = CYLINDRICAL_SURFACE('',#68519,0.149999999999997) ;
#6094 = CYLINDRICAL_SURFACE('',#68521,0.149999999999997) ;
#6095 = CYLINDRICAL_SURFACE('',#68527,0.149999999999997) ;
#6096 = CYLINDRICAL_SURFACE('',#68528,0.149999999999997) ;
#6097 = CYLINDRICAL_SURFACE('',#68537,0.149999999999997) ;
#6098 = CYLINDRICAL_SURFACE('',#68539,0.149999999999997) ;
#6099 = CYLINDRICAL_SURFACE('',#68541,0.149999999999997) ;
#6100 = CYLINDRICAL_SURFACE('',#68544,0.149999999999997) ;
#6101 = CYLINDRICAL_SURFACE('',#68546,0.149999999999997) ;
#6102 = CYLINDRICAL_SURFACE('',#68548,0.149999999999997) ;
#6103 = CYLINDRICAL_SURFACE('',#68559,0.149999999999997) ;
#6104 = CYLINDRICAL_SURFACE('',#68561,0.149999999999997) ;
#6105 = CYLINDRICAL_SURFACE('',#68563,0.149999999999997) ;
#6106 = CYLINDRICAL_SURFACE('',#68565,0.149999999999997) ;
#6107 = CYLINDRICAL_SURFACE('',#68571,0.149999999999997) ;
#6108 = CYLINDRICAL_SURFACE('',#68572,0.149999999999997) ;
#6109 = CYLINDRICAL_SURFACE('',#68581,0.150000000000001) ;
#6110 = CYLINDRICAL_SURFACE('',#68583,0.150000000000001) ;
#6111 = CYLINDRICAL_SURFACE('',#68585,0.149999999999997) ;
#6112 = CYLINDRICAL_SURFACE('',#68588,0.149999999999997) ;
#6113 = CYLINDRICAL_SURFACE('',#68590,0.150000000000001) ;
#6114 = CYLINDRICAL_SURFACE('',#68592,0.149999999999997) ;
#6115 = CYLINDRICAL_SURFACE('',#68603,0.150000000000001) ;
#6116 = CYLINDRICAL_SURFACE('',#68605,0.150000000000001) ;
#6117 = CYLINDRICAL_SURFACE('',#68607,0.150000000000001) ;
#6118 = CYLINDRICAL_SURFACE('',#68609,0.149999999999997) ;
#6119 = CYLINDRICAL_SURFACE('',#68615,0.149999999999997) ;
#6120 = CYLINDRICAL_SURFACE('',#68616,0.149999999999997) ;
#6121 = CYLINDRICAL_SURFACE('',#68625,0.150000000000001) ;
#6122 = CYLINDRICAL_SURFACE('',#68627,0.149999999999997) ;
#6123 = CYLINDRICAL_SURFACE('',#68629,0.149999999999997) ;
#6124 = CYLINDRICAL_SURFACE('',#68632,0.150000000000001) ;
#6125 = CYLINDRICAL_SURFACE('',#68634,0.150000000000001) ;
#6126 = CYLINDRICAL_SURFACE('',#68636,0.149999999999997) ;
#6127 = CYLINDRICAL_SURFACE('',#68647,0.149999999999997) ;
#6128 = CYLINDRICAL_SURFACE('',#68649,0.150000000000001) ;
#6129 = CYLINDRICAL_SURFACE('',#68651,0.150000000000001) ;
#6130 = CYLINDRICAL_SURFACE('',#68653,0.150000000000001) ;
#6131 = CYLINDRICAL_SURFACE('',#68659,0.149999999999997) ;
#6132 = CYLINDRICAL_SURFACE('',#68660,0.149999999999997) ;
#6133 = CYLINDRICAL_SURFACE('',#68669,0.150000000000001) ;
#6134 = CYLINDRICAL_SURFACE('',#68671,0.150000000000001) ;
#6135 = CYLINDRICAL_SURFACE('',#68673,0.149999999999997) ;
#6136 = CYLINDRICAL_SURFACE('',#68676,0.149999999999997) ;
#6137 = CYLINDRICAL_SURFACE('',#68678,0.150000000000001) ;
#6138 = CYLINDRICAL_SURFACE('',#68680,0.149999999999997) ;
#6139 = CYLINDRICAL_SURFACE('',#68691,0.150000000000001) ;
#6140 = CYLINDRICAL_SURFACE('',#68693,0.150000000000001) ;
#6141 = CYLINDRICAL_SURFACE('',#68695,0.150000000000001) ;
#6142 = CYLINDRICAL_SURFACE('',#68697,0.149999999999997) ;
#6143 = CYLINDRICAL_SURFACE('',#68703,0.149999999999997) ;
#6144 = CYLINDRICAL_SURFACE('',#68704,0.149999999999997) ;
#6145 = CYLINDRICAL_SURFACE('',#68713,0.150000000000001) ;
#6146 = CYLINDRICAL_SURFACE('',#68715,0.150000000000001) ;
#6147 = CYLINDRICAL_SURFACE('',#68717,0.149999999999997) ;
#6148 = CYLINDRICAL_SURFACE('',#68720,0.15) ;
#6149 = CYLINDRICAL_SURFACE('',#68722,0.15) ;
#6150 = CYLINDRICAL_SURFACE('',#68724,0.149999999999997) ;
#6151 = CYLINDRICAL_SURFACE('',#68735,0.150000000000001) ;
#6152 = CYLINDRICAL_SURFACE('',#68737,0.150000000000001) ;
#6153 = CYLINDRICAL_SURFACE('',#68739,0.15) ;
#6154 = CYLINDRICAL_SURFACE('',#68741,0.15) ;
#6155 = CYLINDRICAL_SURFACE('',#68747,0.149999999999997) ;
#6156 = CYLINDRICAL_SURFACE('',#68748,0.149999999999997) ;
#6157 = CYLINDRICAL_SURFACE('',#68751,0.149999999999997) ;
#6158 = CYLINDRICAL_SURFACE('',#68754,0.150000000000001) ;
#6159 = CYLINDRICAL_SURFACE('',#68759,0.15) ;
#6160 = CYLINDRICAL_SURFACE('',#68761,0.15) ;
#6161 = CYLINDRICAL_SURFACE('',#68765,0.150000000000001) ;
#6162 = CYLINDRICAL_SURFACE('',#68767,0.149999999999997) ;
#6163 = CYLINDRICAL_SURFACE('',#68769,0.149999999999997) ;
#6164 = CYLINDRICAL_SURFACE('',#68771,0.150000000000001) ;
#6165 = CYLINDRICAL_SURFACE('',#68777,0.150000000000001) ;
#6166 = CYLINDRICAL_SURFACE('',#68794,0.1) ;
#6167 = CYLINDRICAL_SURFACE('',#68798,0.1) ;
#6168 = CYLINDRICAL_SURFACE('',#68806,1.5) ;
#6169 = CYLINDRICAL_SURFACE('',#68807,3.) ;
#6170 = CYLINDRICAL_SURFACE('',#68905,1.75) ;
#6171 = CYLINDRICAL_SURFACE('',#68908,1.75) ;
#6172 = CYLINDRICAL_SURFACE('',#68920,1.75) ;
#6173 = CYLINDRICAL_SURFACE('',#68924,1.75) ;
#6174 = CYLINDRICAL_SURFACE('',#68950,2.) ;
#6175 = CYLINDRICAL_SURFACE('',#68958,1.) ;
#6176 = CYLINDRICAL_SURFACE('',#68973,0.1) ;
#6177 = CYLINDRICAL_SURFACE('',#68978,0.1) ;
#6178 = CYLINDRICAL_SURFACE('',#68980,0.1) ;
#6179 = CYLINDRICAL_SURFACE('',#68989,0.1) ;
#6180 = CYLINDRICAL_SURFACE('',#68991,0.1) ;
#6181 = CYLINDRICAL_SURFACE('',#68994,0.1) ;
#6182 = CYLINDRICAL_SURFACE('',#68998,0.1) ;
#6183 = CYLINDRICAL_SURFACE('',#69000,0.1) ;
#6184 = CYLINDRICAL_SURFACE('',#69002,0.1) ;
#6185 = CYLINDRICAL_SURFACE('',#69014,0.1) ;
#6186 = CYLINDRICAL_SURFACE('',#69019,0.1) ;
#6187 = CYLINDRICAL_SURFACE('',#69021,0.1) ;
#6188 = CYLINDRICAL_SURFACE('',#69029,0.1) ;
#6189 = CYLINDRICAL_SURFACE('',#69031,0.1) ;
#6190 = CYLINDRICAL_SURFACE('',#69033,0.1) ;
#6191 = CYLINDRICAL_SURFACE('',#69035,0.1) ;
#6192 = CYLINDRICAL_SURFACE('',#69041,0.1) ;
#6193 = CYLINDRICAL_SURFACE('',#69046,0.1) ;
#6194 = CYLINDRICAL_SURFACE('',#69048,0.1) ;
#6195 = CYLINDRICAL_SURFACE('',#69050,0.1) ;
#6196 = CYLINDRICAL_SURFACE('',#69052,0.1) ;
#6197 = CYLINDRICAL_SURFACE('',#69055,0.1) ;
#6198 = CYLINDRICAL_SURFACE('',#69061,0.1) ;
#6199 = CYLINDRICAL_SURFACE('',#69066,0.1) ;
#6200 = CYLINDRICAL_SURFACE('',#69069,0.1) ;
#6201 = CYLINDRICAL_SURFACE('',#69072,0.1) ;
#6202 = CYLINDRICAL_SURFACE('',#69074,0.1) ;
#6203 = CYLINDRICAL_SURFACE('',#69079,0.1) ;
#6204 = CYLINDRICAL_SURFACE('',#69086,0.1) ;
#6205 = CYLINDRICAL_SURFACE('',#69088,0.1) ;
#6206 = CYLINDRICAL_SURFACE('',#69093,0.1) ;
#6207 = CYLINDRICAL_SURFACE('',#69095,0.1) ;
#6208 = CYLINDRICAL_SURFACE('',#69101,0.1) ;
#6209 = CYLINDRICAL_SURFACE('',#69108,0.1) ;
#6210 = CYLINDRICAL_SURFACE('',#69110,0.1) ;
#6211 = CYLINDRICAL_SURFACE('',#69112,0.1) ;
#6212 = CYLINDRICAL_SURFACE('',#69115,0.1) ;
#6213 = CYLINDRICAL_SURFACE('',#69116,0.0999999999999998) ;
#6214 = CYLINDRICAL_SURFACE('',#69121,0.0999999999999998) ;
#6215 = CYLINDRICAL_SURFACE('',#69123,0.0999999999999998) ;
#6216 = CYLINDRICAL_SURFACE('',#69127,0.1) ;
#6217 = CYLINDRICAL_SURFACE('',#69129,0.1) ;
#6218 = CYLINDRICAL_SURFACE('',#69141,0.0999999999999998) ;
#6219 = CYLINDRICAL_SURFACE('',#69143,0.1) ;
#6220 = CYLINDRICAL_SURFACE('',#69147,0.1) ;
#6221 = CYLINDRICAL_SURFACE('',#69150,0.1) ;
#6222 = CYLINDRICAL_SURFACE('',#69152,0.0999999999999998) ;
#6223 = CYLINDRICAL_SURFACE('',#69162,0.1) ;
#6224 = CYLINDRICAL_SURFACE('',#69165,0.1) ;
#6225 = CYLINDRICAL_SURFACE('',#69170,0.0999999999999998) ;
#6226 = CYLINDRICAL_SURFACE('',#69172,0.0999999999999998) ;
#6227 = CYLINDRICAL_SURFACE('',#69183,0.0999999999999998) ;
#6228 = CYLINDRICAL_SURFACE('',#69189,0.1) ;
#6229 = CYLINDRICAL_SURFACE('',#69192,0.1) ;
#6230 = CYLINDRICAL_SURFACE('',#69196,0.1) ;
#6231 = CYLINDRICAL_SURFACE('',#69201,0.1) ;
#6232 = CYLINDRICAL_SURFACE('',#69206,0.1) ;
#6233 = CYLINDRICAL_SURFACE('',#69208,0.1) ;
#6234 = CYLINDRICAL_SURFACE('',#69211,0.1) ;
#6235 = CYLINDRICAL_SURFACE('',#69213,0.1) ;
#6236 = CYLINDRICAL_SURFACE('',#69215,0.1) ;
#6237 = CYLINDRICAL_SURFACE('',#69222,0.1) ;
#6238 = CYLINDRICAL_SURFACE('',#69224,0.1) ;
#6239 = CYLINDRICAL_SURFACE('',#69228,0.1) ;
#6240 = CYLINDRICAL_SURFACE('',#69230,0.1) ;
#6241 = CYLINDRICAL_SURFACE('',#69234,0.0999999999999998) ;
#6242 = CYLINDRICAL_SURFACE('',#69236,0.1) ;
#6243 = CYLINDRICAL_SURFACE('',#69238,0.1) ;
#6244 = CYLINDRICAL_SURFACE('',#69241,0.1) ;
#6245 = CYLINDRICAL_SURFACE('',#69244,0.1) ;
#6246 = CYLINDRICAL_SURFACE('',#69249,0.0999999999999998) ;
#6247 = CYLINDRICAL_SURFACE('',#69251,0.1) ;
#6248 = CYLINDRICAL_SURFACE('',#69255,0.0999999999999994) ;
#6249 = CYLINDRICAL_SURFACE('',#69257,0.1) ;
#6250 = CYLINDRICAL_SURFACE('',#69260,0.1) ;
#6251 = CYLINDRICAL_SURFACE('',#69263,0.0999999999999994) ;
#6252 = CYLINDRICAL_SURFACE('',#69269,0.1) ;
#6253 = CYLINDRICAL_SURFACE('',#69270,0.0999999999999994) ;
#6254 = CYLINDRICAL_SURFACE('',#69272,0.1) ;
#6255 = CYLINDRICAL_SURFACE('',#69276,0.0999999999999994) ;
#6256 = CYLINDRICAL_SURFACE('',#69278,0.0999999999999994) ;
#6257 = CYLINDRICAL_SURFACE('',#69282,0.0999999999999998) ;
#6258 = CYLINDRICAL_SURFACE('',#69283,0.1) ;
#6259 = CYLINDRICAL_SURFACE('',#69286,0.0999999999999994) ;
#6260 = CYLINDRICAL_SURFACE('',#69290,0.0999999999999994) ;
#6261 = CYLINDRICAL_SURFACE('',#69292,0.0999999999999994) ;
#6262 = CYLINDRICAL_SURFACE('',#69296,0.0999999999999998) ;
#6263 = CYLINDRICAL_SURFACE('',#69298,0.1) ;
#6264 = CYLINDRICAL_SURFACE('',#69301,0.1) ;
#6265 = CYLINDRICAL_SURFACE('',#69302,0.1) ;
#6266 = CYLINDRICAL_SURFACE('',#69303,0.1) ;
#6267 = CYLINDRICAL_SURFACE('',#69304,0.0999999999999994) ;
#6268 = CYLINDRICAL_SURFACE('',#69305,0.0999999999999994) ;
#6269 = CYLINDRICAL_SURFACE('',#69310,0.0999999999999994) ;
#6270 = CYLINDRICAL_SURFACE('',#69313,0.1) ;
#6271 = CYLINDRICAL_SURFACE('',#69317,0.1) ;
#6272 = CYLINDRICAL_SURFACE('',#69320,0.1) ;
#6273 = CYLINDRICAL_SURFACE('',#69324,0.1) ;
#6274 = CYLINDRICAL_SURFACE('',#69327,0.1) ;
#6275 = CYLINDRICAL_SURFACE('',#69329,0.0999999999999994) ;
#6276 = CYLINDRICAL_SURFACE('',#69332,0.0999999999999994) ;
#6277 = CYLINDRICAL_SURFACE('',#69334,0.0999999999999994) ;
#6278 = CYLINDRICAL_SURFACE('',#69336,0.1) ;
#6279 = CYLINDRICAL_SURFACE('',#69338,0.0999999999999994) ;
#6280 = CYLINDRICAL_SURFACE('',#69347,0.1) ;
#6281 = CYLINDRICAL_SURFACE('',#69349,0.1) ;
#6282 = CYLINDRICAL_SURFACE('',#69355,0.1) ;
#6283 = CYLINDRICAL_SURFACE('',#69357,0.1) ;
#6284 = CYLINDRICAL_SURFACE('',#69363,0.0999999999999994) ;
#6285 = CYLINDRICAL_SURFACE('',#69365,0.0999999999999994) ;
#6286 = CYLINDRICAL_SURFACE('',#69371,0.0999999999999994) ;
#6287 = CYLINDRICAL_SURFACE('',#69373,0.0999999999999994) ;
#6288 = CYLINDRICAL_SURFACE('',#69376,0.0999999999999994) ;
#6289 = CYLINDRICAL_SURFACE('',#69382,0.0999999999999994) ;
#6290 = CYLINDRICAL_SURFACE('',#69385,0.0999999999999994) ;
#6291 = CYLINDRICAL_SURFACE('',#69388,0.0999999999999994) ;
#6292 = CYLINDRICAL_SURFACE('',#69404,0.1) ;
#6293 = CYLINDRICAL_SURFACE('',#69408,0.1) ;
#6294 = CYLINDRICAL_SURFACE('',#69416,1.5) ;
#6295 = CYLINDRICAL_SURFACE('',#69417,3.) ;
#6296 = CYLINDRICAL_SURFACE('',#69515,1.75) ;
#6297 = CYLINDRICAL_SURFACE('',#69518,1.75) ;
#6298 = CYLINDRICAL_SURFACE('',#69530,1.75) ;
#6299 = CYLINDRICAL_SURFACE('',#69534,1.75) ;
#6300 = CYLINDRICAL_SURFACE('',#69560,2.) ;
#6301 = CYLINDRICAL_SURFACE('',#69568,1.) ;
#6302 = CYLINDRICAL_SURFACE('',#69583,0.1) ;
#6303 = CYLINDRICAL_SURFACE('',#69588,0.1) ;
#6304 = CYLINDRICAL_SURFACE('',#69590,0.1) ;
#6305 = CYLINDRICAL_SURFACE('',#69599,0.1) ;
#6306 = CYLINDRICAL_SURFACE('',#69601,0.1) ;
#6307 = CYLINDRICAL_SURFACE('',#69604,0.1) ;
#6308 = CYLINDRICAL_SURFACE('',#69608,0.1) ;
#6309 = CYLINDRICAL_SURFACE('',#69610,0.1) ;
#6310 = CYLINDRICAL_SURFACE('',#69612,0.1) ;
#6311 = CYLINDRICAL_SURFACE('',#69624,0.1) ;
#6312 = CYLINDRICAL_SURFACE('',#69629,0.1) ;
#6313 = CYLINDRICAL_SURFACE('',#69631,0.1) ;
#6314 = CYLINDRICAL_SURFACE('',#69639,0.1) ;
#6315 = CYLINDRICAL_SURFACE('',#69641,0.1) ;
#6316 = CYLINDRICAL_SURFACE('',#69643,0.1) ;
#6317 = CYLINDRICAL_SURFACE('',#69645,0.1) ;
#6318 = CYLINDRICAL_SURFACE('',#69651,0.1) ;
#6319 = CYLINDRICAL_SURFACE('',#69656,0.1) ;
#6320 = CYLINDRICAL_SURFACE('',#69658,0.1) ;
#6321 = CYLINDRICAL_SURFACE('',#69660,0.1) ;
#6322 = CYLINDRICAL_SURFACE('',#69662,0.1) ;
#6323 = CYLINDRICAL_SURFACE('',#69665,0.1) ;
#6324 = CYLINDRICAL_SURFACE('',#69671,0.1) ;
#6325 = CYLINDRICAL_SURFACE('',#69676,0.1) ;
#6326 = CYLINDRICAL_SURFACE('',#69679,0.1) ;
#6327 = CYLINDRICAL_SURFACE('',#69682,0.1) ;
#6328 = CYLINDRICAL_SURFACE('',#69684,0.1) ;
#6329 = CYLINDRICAL_SURFACE('',#69689,0.1) ;
#6330 = CYLINDRICAL_SURFACE('',#69696,0.1) ;
#6331 = CYLINDRICAL_SURFACE('',#69698,0.1) ;
#6332 = CYLINDRICAL_SURFACE('',#69703,0.1) ;
#6333 = CYLINDRICAL_SURFACE('',#69705,0.1) ;
#6334 = CYLINDRICAL_SURFACE('',#69711,0.0999999999999998) ;
#6335 = CYLINDRICAL_SURFACE('',#69718,0.1) ;
#6336 = CYLINDRICAL_SURFACE('',#69720,0.0999999999999998) ;
#6337 = CYLINDRICAL_SURFACE('',#69722,0.0999999999999998) ;
#6338 = CYLINDRICAL_SURFACE('',#69725,0.0999999999999998) ;
#6339 = CYLINDRICAL_SURFACE('',#69726,0.0999999999999998) ;
#6340 = CYLINDRICAL_SURFACE('',#69731,0.0999999999999998) ;
#6341 = CYLINDRICAL_SURFACE('',#69733,0.0999999999999998) ;
#6342 = CYLINDRICAL_SURFACE('',#69737,0.1) ;
#6343 = CYLINDRICAL_SURFACE('',#69739,0.1) ;
#6344 = CYLINDRICAL_SURFACE('',#69751,0.0999999999999998) ;
#6345 = CYLINDRICAL_SURFACE('',#69753,0.1) ;
#6346 = CYLINDRICAL_SURFACE('',#69757,0.1) ;
#6347 = CYLINDRICAL_SURFACE('',#69760,0.1) ;
#6348 = CYLINDRICAL_SURFACE('',#69762,0.0999999999999998) ;
#6349 = CYLINDRICAL_SURFACE('',#69772,0.1) ;
#6350 = CYLINDRICAL_SURFACE('',#69775,0.1) ;
#6351 = CYLINDRICAL_SURFACE('',#69780,0.0999999999999998) ;
#6352 = CYLINDRICAL_SURFACE('',#69782,0.0999999999999998) ;
#6353 = CYLINDRICAL_SURFACE('',#69793,0.0999999999999998) ;
#6354 = CYLINDRICAL_SURFACE('',#69799,0.1) ;
#6355 = CYLINDRICAL_SURFACE('',#69802,0.1) ;
#6356 = CYLINDRICAL_SURFACE('',#69806,0.1) ;
#6357 = CYLINDRICAL_SURFACE('',#69811,0.1) ;
#6358 = CYLINDRICAL_SURFACE('',#69816,0.1) ;
#6359 = CYLINDRICAL_SURFACE('',#69818,0.1) ;
#6360 = CYLINDRICAL_SURFACE('',#69821,0.1) ;
#6361 = CYLINDRICAL_SURFACE('',#69823,0.1) ;
#6362 = CYLINDRICAL_SURFACE('',#69825,0.1) ;
#6363 = CYLINDRICAL_SURFACE('',#69832,0.1) ;
#6364 = CYLINDRICAL_SURFACE('',#69834,0.1) ;
#6365 = CYLINDRICAL_SURFACE('',#69838,0.1) ;
#6366 = CYLINDRICAL_SURFACE('',#69840,0.1) ;
#6367 = CYLINDRICAL_SURFACE('',#69844,0.0999999999999998) ;
#6368 = CYLINDRICAL_SURFACE('',#69846,0.1) ;
#6369 = CYLINDRICAL_SURFACE('',#69848,0.1) ;
#6370 = CYLINDRICAL_SURFACE('',#69851,0.1) ;
#6371 = CYLINDRICAL_SURFACE('',#69854,0.1) ;
#6372 = CYLINDRICAL_SURFACE('',#69859,0.0999999999999998) ;
#6373 = CYLINDRICAL_SURFACE('',#69861,0.1) ;
#6374 = CYLINDRICAL_SURFACE('',#69865,0.0999999999999994) ;
#6375 = CYLINDRICAL_SURFACE('',#69867,0.1) ;
#6376 = CYLINDRICAL_SURFACE('',#69870,0.1) ;
#6377 = CYLINDRICAL_SURFACE('',#69873,0.0999999999999994) ;
#6378 = CYLINDRICAL_SURFACE('',#69879,0.1) ;
#6379 = CYLINDRICAL_SURFACE('',#69880,0.0999999999999994) ;
#6380 = CYLINDRICAL_SURFACE('',#69882,0.1) ;
#6381 = CYLINDRICAL_SURFACE('',#69886,0.0999999999999994) ;
#6382 = CYLINDRICAL_SURFACE('',#69888,0.0999999999999994) ;
#6383 = CYLINDRICAL_SURFACE('',#69892,0.0999999999999998) ;
#6384 = CYLINDRICAL_SURFACE('',#69893,0.1) ;
#6385 = CYLINDRICAL_SURFACE('',#69896,0.0999999999999994) ;
#6386 = CYLINDRICAL_SURFACE('',#69900,0.0999999999999994) ;
#6387 = CYLINDRICAL_SURFACE('',#69902,0.0999999999999994) ;
#6388 = CYLINDRICAL_SURFACE('',#69906,0.0999999999999998) ;
#6389 = CYLINDRICAL_SURFACE('',#69908,0.1) ;
#6390 = CYLINDRICAL_SURFACE('',#69911,0.1) ;
#6391 = CYLINDRICAL_SURFACE('',#69912,0.1) ;
#6392 = CYLINDRICAL_SURFACE('',#69913,0.1) ;
#6393 = CYLINDRICAL_SURFACE('',#69914,0.0999999999999994) ;
#6394 = CYLINDRICAL_SURFACE('',#69915,0.0999999999999994) ;
#6395 = CYLINDRICAL_SURFACE('',#69920,0.0999999999999994) ;
#6396 = CYLINDRICAL_SURFACE('',#69923,0.1) ;
#6397 = CYLINDRICAL_SURFACE('',#69927,0.1) ;
#6398 = CYLINDRICAL_SURFACE('',#69930,0.1) ;
#6399 = CYLINDRICAL_SURFACE('',#69934,0.1) ;
#6400 = CYLINDRICAL_SURFACE('',#69937,0.1) ;
#6401 = CYLINDRICAL_SURFACE('',#69939,0.0999999999999994) ;
#6402 = CYLINDRICAL_SURFACE('',#69942,0.0999999999999994) ;
#6403 = CYLINDRICAL_SURFACE('',#69944,0.0999999999999994) ;
#6404 = CYLINDRICAL_SURFACE('',#69946,0.1) ;
#6405 = CYLINDRICAL_SURFACE('',#69948,0.0999999999999994) ;
#6406 = CYLINDRICAL_SURFACE('',#69957,0.1) ;
#6407 = CYLINDRICAL_SURFACE('',#69959,0.1) ;
#6408 = CYLINDRICAL_SURFACE('',#69965,0.1) ;
#6409 = CYLINDRICAL_SURFACE('',#69967,0.1) ;
#6410 = CYLINDRICAL_SURFACE('',#69973,0.0999999999999994) ;
#6411 = CYLINDRICAL_SURFACE('',#69975,0.0999999999999994) ;
#6412 = CYLINDRICAL_SURFACE('',#69981,0.0999999999999994) ;
#6413 = CYLINDRICAL_SURFACE('',#69983,0.0999999999999994) ;
#6414 = CYLINDRICAL_SURFACE('',#69986,0.0999999999999994) ;
#6415 = CYLINDRICAL_SURFACE('',#69992,0.0999999999999994) ;
#6416 = CYLINDRICAL_SURFACE('',#69995,0.0999999999999994) ;
#6417 = CYLINDRICAL_SURFACE('',#69998,0.0999999999999994) ;
#6418 = CYLINDRICAL_SURFACE('',#70014,0.1) ;
#6419 = CYLINDRICAL_SURFACE('',#70018,0.1) ;
#6420 = CYLINDRICAL_SURFACE('',#70026,1.5) ;
#6421 = CYLINDRICAL_SURFACE('',#70027,3.) ;
#6422 = CYLINDRICAL_SURFACE('',#70125,1.75) ;
#6423 = CYLINDRICAL_SURFACE('',#70128,1.75) ;
#6424 = CYLINDRICAL_SURFACE('',#70140,1.75) ;
#6425 = CYLINDRICAL_SURFACE('',#70144,1.75) ;
#6426 = CYLINDRICAL_SURFACE('',#70170,2.) ;
#6427 = CYLINDRICAL_SURFACE('',#70178,1.) ;
#6428 = CYLINDRICAL_SURFACE('',#70193,0.1) ;
#6429 = CYLINDRICAL_SURFACE('',#70198,0.1) ;
#6430 = CYLINDRICAL_SURFACE('',#70200,0.1) ;
#6431 = CYLINDRICAL_SURFACE('',#70209,0.1) ;
#6432 = CYLINDRICAL_SURFACE('',#70211,0.1) ;
#6433 = CYLINDRICAL_SURFACE('',#70214,0.1) ;
#6434 = CYLINDRICAL_SURFACE('',#70218,0.1) ;
#6435 = CYLINDRICAL_SURFACE('',#70220,0.0999999999999994) ;
#6436 = CYLINDRICAL_SURFACE('',#70222,0.1) ;
#6437 = CYLINDRICAL_SURFACE('',#70234,0.1) ;
#6438 = CYLINDRICAL_SURFACE('',#70239,0.0999999999999994) ;
#6439 = CYLINDRICAL_SURFACE('',#70241,0.0999999999999994) ;
#6440 = CYLINDRICAL_SURFACE('',#70249,0.1) ;
#6441 = CYLINDRICAL_SURFACE('',#70251,0.1) ;
#6442 = CYLINDRICAL_SURFACE('',#70253,0.1) ;
#6443 = CYLINDRICAL_SURFACE('',#70255,0.1) ;
#6444 = CYLINDRICAL_SURFACE('',#70261,0.0999999999999994) ;
#6445 = CYLINDRICAL_SURFACE('',#70266,0.0999999999999994) ;
#6446 = CYLINDRICAL_SURFACE('',#70268,0.0999999999999994) ;
#6447 = CYLINDRICAL_SURFACE('',#70270,0.1) ;
#6448 = CYLINDRICAL_SURFACE('',#70272,0.1) ;
#6449 = CYLINDRICAL_SURFACE('',#70275,0.1) ;
#6450 = CYLINDRICAL_SURFACE('',#70281,0.0999999999999994) ;
#6451 = CYLINDRICAL_SURFACE('',#70286,0.0999999999999994) ;
#6452 = CYLINDRICAL_SURFACE('',#70289,0.1) ;
#6453 = CYLINDRICAL_SURFACE('',#70292,0.0999999999999994) ;
#6454 = CYLINDRICAL_SURFACE('',#70294,0.0999999999999994) ;
#6455 = CYLINDRICAL_SURFACE('',#70299,0.1) ;
#6456 = CYLINDRICAL_SURFACE('',#70306,0.0999999999999994) ;
#6457 = CYLINDRICAL_SURFACE('',#70308,0.1) ;
#6458 = CYLINDRICAL_SURFACE('',#70313,0.1) ;
#6459 = CYLINDRICAL_SURFACE('',#70315,0.1) ;
#6460 = CYLINDRICAL_SURFACE('',#70321,0.0999999999999994) ;
#6461 = CYLINDRICAL_SURFACE('',#70328,0.1) ;
#6462 = CYLINDRICAL_SURFACE('',#70330,0.0999999999999994) ;
#6463 = CYLINDRICAL_SURFACE('',#70332,0.0999999999999994) ;
#6464 = CYLINDRICAL_SURFACE('',#70335,0.0999999999999994) ;
#6465 = CYLINDRICAL_SURFACE('',#70336,0.0999999999999998) ;
#6466 = CYLINDRICAL_SURFACE('',#70341,0.0999999999999998) ;
#6467 = CYLINDRICAL_SURFACE('',#70343,0.0999999999999998) ;
#6468 = CYLINDRICAL_SURFACE('',#70347,0.1) ;
#6469 = CYLINDRICAL_SURFACE('',#70349,0.1) ;
#6470 = CYLINDRICAL_SURFACE('',#70361,0.0999999999999998) ;
#6471 = CYLINDRICAL_SURFACE('',#70363,0.1) ;
#6472 = CYLINDRICAL_SURFACE('',#70367,0.1) ;
#6473 = CYLINDRICAL_SURFACE('',#70370,0.1) ;
#6474 = CYLINDRICAL_SURFACE('',#70372,0.0999999999999998) ;
#6475 = CYLINDRICAL_SURFACE('',#70382,0.1) ;
#6476 = CYLINDRICAL_SURFACE('',#70385,0.0999999999999994) ;
#6477 = CYLINDRICAL_SURFACE('',#70390,0.0999999999999998) ;
#6478 = CYLINDRICAL_SURFACE('',#70392,0.0999999999999998) ;
#6479 = CYLINDRICAL_SURFACE('',#70403,0.0999999999999998) ;
#6480 = CYLINDRICAL_SURFACE('',#70409,0.0999999999999994) ;
#6481 = CYLINDRICAL_SURFACE('',#70412,0.0999999999999994) ;
#6482 = CYLINDRICAL_SURFACE('',#70416,0.1) ;
#6483 = CYLINDRICAL_SURFACE('',#70421,0.0999999999999994) ;
#6484 = CYLINDRICAL_SURFACE('',#70426,0.0999999999999994) ;
#6485 = CYLINDRICAL_SURFACE('',#70428,0.1) ;
#6486 = CYLINDRICAL_SURFACE('',#70431,0.0999999999999994) ;
#6487 = CYLINDRICAL_SURFACE('',#70433,0.1) ;
#6488 = CYLINDRICAL_SURFACE('',#70435,0.1) ;
#6489 = CYLINDRICAL_SURFACE('',#70442,0.1) ;
#6490 = CYLINDRICAL_SURFACE('',#70444,0.0999999999999994) ;
#6491 = CYLINDRICAL_SURFACE('',#70448,0.1) ;
#6492 = CYLINDRICAL_SURFACE('',#70450,0.0999999999999994) ;
#6493 = CYLINDRICAL_SURFACE('',#70454,0.0999999999999998) ;
#6494 = CYLINDRICAL_SURFACE('',#70456,0.1) ;
#6495 = CYLINDRICAL_SURFACE('',#70458,0.1) ;
#6496 = CYLINDRICAL_SURFACE('',#70461,0.1) ;
#6497 = CYLINDRICAL_SURFACE('',#70464,0.0999999999999994) ;
#6498 = CYLINDRICAL_SURFACE('',#70469,0.0999999999999998) ;
#6499 = CYLINDRICAL_SURFACE('',#70471,0.1) ;
#6500 = CYLINDRICAL_SURFACE('',#70475,0.0999999999999994) ;
#6501 = CYLINDRICAL_SURFACE('',#70477,0.1) ;
#6502 = CYLINDRICAL_SURFACE('',#70480,0.1) ;
#6503 = CYLINDRICAL_SURFACE('',#70483,0.0999999999999994) ;
#6504 = CYLINDRICAL_SURFACE('',#70489,0.0999999999999994) ;
#6505 = CYLINDRICAL_SURFACE('',#70490,0.0999999999999994) ;
#6506 = CYLINDRICAL_SURFACE('',#70492,0.0999999999999995) ;
#6507 = CYLINDRICAL_SURFACE('',#70496,0.0999999999999994) ;
#6508 = CYLINDRICAL_SURFACE('',#70498,0.0999999999999994) ;
#6509 = CYLINDRICAL_SURFACE('',#70502,0.0999999999999998) ;
#6510 = CYLINDRICAL_SURFACE('',#70503,0.0999999999999995) ;
#6511 = CYLINDRICAL_SURFACE('',#70506,0.0999999999999994) ;
#6512 = CYLINDRICAL_SURFACE('',#70510,0.0999999999999994) ;
#6513 = CYLINDRICAL_SURFACE('',#70512,0.0999999999999994) ;
#6514 = CYLINDRICAL_SURFACE('',#70516,0.0999999999999998) ;
#6515 = CYLINDRICAL_SURFACE('',#70518,0.1) ;
#6516 = CYLINDRICAL_SURFACE('',#70521,0.1) ;
#6517 = CYLINDRICAL_SURFACE('',#70522,0.1) ;
#6518 = CYLINDRICAL_SURFACE('',#70523,0.1) ;
#6519 = CYLINDRICAL_SURFACE('',#70524,0.0999999999999994) ;
#6520 = CYLINDRICAL_SURFACE('',#70525,0.0999999999999994) ;
#6521 = CYLINDRICAL_SURFACE('',#70530,0.0999999999999994) ;
#6522 = CYLINDRICAL_SURFACE('',#70533,0.0999999999999994) ;
#6523 = CYLINDRICAL_SURFACE('',#70537,0.1) ;
#6524 = CYLINDRICAL_SURFACE('',#70540,0.1) ;
#6525 = CYLINDRICAL_SURFACE('',#70544,0.1) ;
#6526 = CYLINDRICAL_SURFACE('',#70547,0.0999999999999994) ;
#6527 = CYLINDRICAL_SURFACE('',#70549,0.0999999999999994) ;
#6528 = CYLINDRICAL_SURFACE('',#70552,0.0999999999999994) ;
#6529 = CYLINDRICAL_SURFACE('',#70554,0.0999999999999994) ;
#6530 = CYLINDRICAL_SURFACE('',#70556,0.0999999999999994) ;
#6531 = CYLINDRICAL_SURFACE('',#70558,0.0999999999999994) ;
#6532 = CYLINDRICAL_SURFACE('',#70567,0.1) ;
#6533 = CYLINDRICAL_SURFACE('',#70569,0.0999999999999994) ;
#6534 = CYLINDRICAL_SURFACE('',#70575,0.0999999999999994) ;
#6535 = CYLINDRICAL_SURFACE('',#70577,0.1) ;
#6536 = CYLINDRICAL_SURFACE('',#70583,0.0999999999999994) ;
#6537 = CYLINDRICAL_SURFACE('',#70585,0.0999999999999994) ;
#6538 = CYLINDRICAL_SURFACE('',#70591,0.0999999999999994) ;
#6539 = CYLINDRICAL_SURFACE('',#70593,0.0999999999999994) ;
#6540 = CYLINDRICAL_SURFACE('',#70596,0.0999999999999994) ;
#6541 = CYLINDRICAL_SURFACE('',#70602,0.0999999999999994) ;
#6542 = CYLINDRICAL_SURFACE('',#70605,0.0999999999999994) ;
#6543 = CYLINDRICAL_SURFACE('',#70608,0.0999999999999994) ;
#6544 = CYLINDRICAL_SURFACE('',#70624,0.1) ;
#6545 = CYLINDRICAL_SURFACE('',#70628,0.1) ;
#6546 = CYLINDRICAL_SURFACE('',#70636,1.5) ;
#6547 = CYLINDRICAL_SURFACE('',#70637,3.) ;
#6548 = CYLINDRICAL_SURFACE('',#70735,1.75) ;
#6549 = CYLINDRICAL_SURFACE('',#70738,1.75) ;
#6550 = CYLINDRICAL_SURFACE('',#70750,1.75) ;
#6551 = CYLINDRICAL_SURFACE('',#70754,1.75) ;
#6552 = CYLINDRICAL_SURFACE('',#70780,2.) ;
#6553 = CYLINDRICAL_SURFACE('',#70788,1.) ;
#6554 = CYLINDRICAL_SURFACE('',#70803,0.1) ;
#6555 = CYLINDRICAL_SURFACE('',#70808,0.1) ;
#6556 = CYLINDRICAL_SURFACE('',#70810,0.1) ;
#6557 = CYLINDRICAL_SURFACE('',#70819,0.1) ;
#6558 = CYLINDRICAL_SURFACE('',#70821,0.1) ;
#6559 = CYLINDRICAL_SURFACE('',#70824,0.1) ;
#6560 = CYLINDRICAL_SURFACE('',#70828,0.1) ;
#6561 = CYLINDRICAL_SURFACE('',#70830,0.0999999999999994) ;
#6562 = CYLINDRICAL_SURFACE('',#70832,0.1) ;
#6563 = CYLINDRICAL_SURFACE('',#70844,0.1) ;
#6564 = CYLINDRICAL_SURFACE('',#70849,0.0999999999999994) ;
#6565 = CYLINDRICAL_SURFACE('',#70851,0.0999999999999994) ;
#6566 = CYLINDRICAL_SURFACE('',#70859,0.1) ;
#6567 = CYLINDRICAL_SURFACE('',#70861,0.1) ;
#6568 = CYLINDRICAL_SURFACE('',#70863,0.1) ;
#6569 = CYLINDRICAL_SURFACE('',#70865,0.1) ;
#6570 = CYLINDRICAL_SURFACE('',#70871,0.0999999999999994) ;
#6571 = CYLINDRICAL_SURFACE('',#70876,0.0999999999999994) ;
#6572 = CYLINDRICAL_SURFACE('',#70878,0.0999999999999994) ;
#6573 = CYLINDRICAL_SURFACE('',#70880,0.1) ;
#6574 = CYLINDRICAL_SURFACE('',#70882,0.1) ;
#6575 = CYLINDRICAL_SURFACE('',#70885,0.1) ;
#6576 = CYLINDRICAL_SURFACE('',#70891,0.0999999999999994) ;
#6577 = CYLINDRICAL_SURFACE('',#70896,0.0999999999999994) ;
#6578 = CYLINDRICAL_SURFACE('',#70899,0.1) ;
#6579 = CYLINDRICAL_SURFACE('',#70902,0.0999999999999994) ;
#6580 = CYLINDRICAL_SURFACE('',#70904,0.0999999999999994) ;
#6581 = CYLINDRICAL_SURFACE('',#70909,0.1) ;
#6582 = CYLINDRICAL_SURFACE('',#70916,0.0999999999999994) ;
#6583 = CYLINDRICAL_SURFACE('',#70918,0.1) ;
#6584 = CYLINDRICAL_SURFACE('',#70923,0.1) ;
#6585 = CYLINDRICAL_SURFACE('',#70925,0.1) ;
#6586 = CYLINDRICAL_SURFACE('',#70931,0.0999999999999994) ;
#6587 = CYLINDRICAL_SURFACE('',#70938,0.1) ;
#6588 = CYLINDRICAL_SURFACE('',#70940,0.0999999999999994) ;
#6589 = CYLINDRICAL_SURFACE('',#70942,0.0999999999999994) ;
#6590 = CYLINDRICAL_SURFACE('',#70945,0.0999999999999994) ;
#6591 = CYLINDRICAL_SURFACE('',#70946,0.0999999999999998) ;
#6592 = CYLINDRICAL_SURFACE('',#70951,0.0999999999999998) ;
#6593 = CYLINDRICAL_SURFACE('',#70953,0.0999999999999998) ;
#6594 = CYLINDRICAL_SURFACE('',#70957,0.1) ;
#6595 = CYLINDRICAL_SURFACE('',#70959,0.1) ;
#6596 = CYLINDRICAL_SURFACE('',#70971,0.0999999999999998) ;
#6597 = CYLINDRICAL_SURFACE('',#70973,0.1) ;
#6598 = CYLINDRICAL_SURFACE('',#70977,0.1) ;
#6599 = CYLINDRICAL_SURFACE('',#70980,0.1) ;
#6600 = CYLINDRICAL_SURFACE('',#70982,0.0999999999999998) ;
#6601 = CYLINDRICAL_SURFACE('',#70992,0.1) ;
#6602 = CYLINDRICAL_SURFACE('',#70995,0.0999999999999994) ;
#6603 = CYLINDRICAL_SURFACE('',#71000,0.0999999999999998) ;
#6604 = CYLINDRICAL_SURFACE('',#71002,0.0999999999999998) ;
#6605 = CYLINDRICAL_SURFACE('',#71013,0.0999999999999998) ;
#6606 = CYLINDRICAL_SURFACE('',#71019,0.0999999999999994) ;
#6607 = CYLINDRICAL_SURFACE('',#71022,0.0999999999999994) ;
#6608 = CYLINDRICAL_SURFACE('',#71026,0.1) ;
#6609 = CYLINDRICAL_SURFACE('',#71031,0.0999999999999994) ;
#6610 = CYLINDRICAL_SURFACE('',#71036,0.0999999999999994) ;
#6611 = CYLINDRICAL_SURFACE('',#71038,0.1) ;
#6612 = CYLINDRICAL_SURFACE('',#71041,0.0999999999999994) ;
#6613 = CYLINDRICAL_SURFACE('',#71043,0.1) ;
#6614 = CYLINDRICAL_SURFACE('',#71045,0.1) ;
#6615 = CYLINDRICAL_SURFACE('',#71052,0.1) ;
#6616 = CYLINDRICAL_SURFACE('',#71054,0.0999999999999994) ;
#6617 = CYLINDRICAL_SURFACE('',#71058,0.1) ;
#6618 = CYLINDRICAL_SURFACE('',#71060,0.0999999999999994) ;
#6619 = CYLINDRICAL_SURFACE('',#71064,0.0999999999999998) ;
#6620 = CYLINDRICAL_SURFACE('',#71066,0.1) ;
#6621 = CYLINDRICAL_SURFACE('',#71068,0.1) ;
#6622 = CYLINDRICAL_SURFACE('',#71071,0.1) ;
#6623 = CYLINDRICAL_SURFACE('',#71074,0.0999999999999994) ;
#6624 = CYLINDRICAL_SURFACE('',#71079,0.0999999999999998) ;
#6625 = CYLINDRICAL_SURFACE('',#71081,0.1) ;
#6626 = CYLINDRICAL_SURFACE('',#71085,0.0999999999999994) ;
#6627 = CYLINDRICAL_SURFACE('',#71087,0.1) ;
#6628 = CYLINDRICAL_SURFACE('',#71090,0.1) ;
#6629 = CYLINDRICAL_SURFACE('',#71093,0.0999999999999994) ;
#6630 = CYLINDRICAL_SURFACE('',#71099,0.0999999999999994) ;
#6631 = CYLINDRICAL_SURFACE('',#71100,0.0999999999999994) ;
#6632 = CYLINDRICAL_SURFACE('',#71102,0.0999999999999995) ;
#6633 = CYLINDRICAL_SURFACE('',#71106,0.0999999999999994) ;
#6634 = CYLINDRICAL_SURFACE('',#71108,0.0999999999999994) ;
#6635 = CYLINDRICAL_SURFACE('',#71112,0.0999999999999998) ;
#6636 = CYLINDRICAL_SURFACE('',#71113,0.0999999999999995) ;
#6637 = CYLINDRICAL_SURFACE('',#71116,0.0999999999999994) ;
#6638 = CYLINDRICAL_SURFACE('',#71120,0.0999999999999994) ;
#6639 = CYLINDRICAL_SURFACE('',#71122,0.0999999999999994) ;
#6640 = CYLINDRICAL_SURFACE('',#71126,0.0999999999999998) ;
#6641 = CYLINDRICAL_SURFACE('',#71128,0.1) ;
#6642 = CYLINDRICAL_SURFACE('',#71131,0.1) ;
#6643 = CYLINDRICAL_SURFACE('',#71132,0.1) ;
#6644 = CYLINDRICAL_SURFACE('',#71133,0.1) ;
#6645 = CYLINDRICAL_SURFACE('',#71134,0.0999999999999994) ;
#6646 = CYLINDRICAL_SURFACE('',#71135,0.0999999999999994) ;
#6647 = CYLINDRICAL_SURFACE('',#71140,0.0999999999999994) ;
#6648 = CYLINDRICAL_SURFACE('',#71143,0.0999999999999994) ;
#6649 = CYLINDRICAL_SURFACE('',#71147,0.1) ;
#6650 = CYLINDRICAL_SURFACE('',#71150,0.1) ;
#6651 = CYLINDRICAL_SURFACE('',#71154,0.1) ;
#6652 = CYLINDRICAL_SURFACE('',#71157,0.0999999999999994) ;
#6653 = CYLINDRICAL_SURFACE('',#71159,0.0999999999999994) ;
#6654 = CYLINDRICAL_SURFACE('',#71162,0.0999999999999994) ;
#6655 = CYLINDRICAL_SURFACE('',#71164,0.0999999999999994) ;
#6656 = CYLINDRICAL_SURFACE('',#71166,0.0999999999999994) ;
#6657 = CYLINDRICAL_SURFACE('',#71168,0.0999999999999994) ;
#6658 = CYLINDRICAL_SURFACE('',#71177,0.1) ;
#6659 = CYLINDRICAL_SURFACE('',#71179,0.0999999999999994) ;
#6660 = CYLINDRICAL_SURFACE('',#71185,0.0999999999999994) ;
#6661 = CYLINDRICAL_SURFACE('',#71187,0.1) ;
#6662 = CYLINDRICAL_SURFACE('',#71193,0.0999999999999994) ;
#6663 = CYLINDRICAL_SURFACE('',#71195,0.0999999999999994) ;
#6664 = CYLINDRICAL_SURFACE('',#71201,0.0999999999999994) ;
#6665 = CYLINDRICAL_SURFACE('',#71203,0.0999999999999994) ;
#6666 = CYLINDRICAL_SURFACE('',#71206,0.0999999999999994) ;
#6667 = CYLINDRICAL_SURFACE('',#71212,0.0999999999999994) ;
#6668 = CYLINDRICAL_SURFACE('',#71215,0.0999999999999994) ;
#6669 = CYLINDRICAL_SURFACE('',#71218,0.0999999999999994) ;
#6670 = CYLINDRICAL_SURFACE('',#71234,0.1) ;
#6671 = CYLINDRICAL_SURFACE('',#71238,0.1) ;
#6672 = CYLINDRICAL_SURFACE('',#71246,1.5) ;
#6673 = CYLINDRICAL_SURFACE('',#71247,3.) ;
#6674 = CYLINDRICAL_SURFACE('',#71345,1.75) ;
#6675 = CYLINDRICAL_SURFACE('',#71348,1.75) ;
#6676 = CYLINDRICAL_SURFACE('',#71360,1.75) ;
#6677 = CYLINDRICAL_SURFACE('',#71364,1.75) ;
#6678 = CYLINDRICAL_SURFACE('',#71390,2.) ;
#6679 = CYLINDRICAL_SURFACE('',#71398,1.) ;
#6680 = CYLINDRICAL_SURFACE('',#71413,0.1) ;
#6681 = CYLINDRICAL_SURFACE('',#71418,0.1) ;
#6682 = CYLINDRICAL_SURFACE('',#71420,0.1) ;
#6683 = CYLINDRICAL_SURFACE('',#71429,0.1) ;
#6684 = CYLINDRICAL_SURFACE('',#71431,0.1) ;
#6685 = CYLINDRICAL_SURFACE('',#71434,0.1) ;
#6686 = CYLINDRICAL_SURFACE('',#71438,0.1) ;
#6687 = CYLINDRICAL_SURFACE('',#71440,0.0999999999999994) ;
#6688 = CYLINDRICAL_SURFACE('',#71442,0.1) ;
#6689 = CYLINDRICAL_SURFACE('',#71454,0.1) ;
#6690 = CYLINDRICAL_SURFACE('',#71459,0.0999999999999994) ;
#6691 = CYLINDRICAL_SURFACE('',#71461,0.0999999999999994) ;
#6692 = CYLINDRICAL_SURFACE('',#71469,0.1) ;
#6693 = CYLINDRICAL_SURFACE('',#71471,0.1) ;
#6694 = CYLINDRICAL_SURFACE('',#71473,0.1) ;
#6695 = CYLINDRICAL_SURFACE('',#71475,0.1) ;
#6696 = CYLINDRICAL_SURFACE('',#71481,0.0999999999999994) ;
#6697 = CYLINDRICAL_SURFACE('',#71486,0.0999999999999994) ;
#6698 = CYLINDRICAL_SURFACE('',#71488,0.0999999999999994) ;
#6699 = CYLINDRICAL_SURFACE('',#71490,0.1) ;
#6700 = CYLINDRICAL_SURFACE('',#71492,0.1) ;
#6701 = CYLINDRICAL_SURFACE('',#71495,0.1) ;
#6702 = CYLINDRICAL_SURFACE('',#71501,0.0999999999999994) ;
#6703 = CYLINDRICAL_SURFACE('',#71506,0.0999999999999994) ;
#6704 = CYLINDRICAL_SURFACE('',#71509,0.1) ;
#6705 = CYLINDRICAL_SURFACE('',#71512,0.0999999999999994) ;
#6706 = CYLINDRICAL_SURFACE('',#71514,0.0999999999999994) ;
#6707 = CYLINDRICAL_SURFACE('',#71519,0.1) ;
#6708 = CYLINDRICAL_SURFACE('',#71526,0.0999999999999994) ;
#6709 = CYLINDRICAL_SURFACE('',#71528,0.1) ;
#6710 = CYLINDRICAL_SURFACE('',#71533,0.1) ;
#6711 = CYLINDRICAL_SURFACE('',#71535,0.1) ;
#6712 = CYLINDRICAL_SURFACE('',#71541,0.0999999999999994) ;
#6713 = CYLINDRICAL_SURFACE('',#71548,0.1) ;
#6714 = CYLINDRICAL_SURFACE('',#71550,0.0999999999999994) ;
#6715 = CYLINDRICAL_SURFACE('',#71552,0.0999999999999994) ;
#6716 = CYLINDRICAL_SURFACE('',#71555,0.0999999999999994) ;
#6717 = CYLINDRICAL_SURFACE('',#71556,0.0999999999999998) ;
#6718 = CYLINDRICAL_SURFACE('',#71561,0.0999999999999998) ;
#6719 = CYLINDRICAL_SURFACE('',#71563,0.0999999999999998) ;
#6720 = CYLINDRICAL_SURFACE('',#71567,0.1) ;
#6721 = CYLINDRICAL_SURFACE('',#71569,0.1) ;
#6722 = CYLINDRICAL_SURFACE('',#71581,0.0999999999999998) ;
#6723 = CYLINDRICAL_SURFACE('',#71583,0.1) ;
#6724 = CYLINDRICAL_SURFACE('',#71587,0.1) ;
#6725 = CYLINDRICAL_SURFACE('',#71590,0.1) ;
#6726 = CYLINDRICAL_SURFACE('',#71592,0.0999999999999998) ;
#6727 = CYLINDRICAL_SURFACE('',#71602,0.1) ;
#6728 = CYLINDRICAL_SURFACE('',#71605,0.0999999999999994) ;
#6729 = CYLINDRICAL_SURFACE('',#71610,0.0999999999999998) ;
#6730 = CYLINDRICAL_SURFACE('',#71612,0.0999999999999998) ;
#6731 = CYLINDRICAL_SURFACE('',#71623,0.0999999999999998) ;
#6732 = CYLINDRICAL_SURFACE('',#71629,0.0999999999999994) ;
#6733 = CYLINDRICAL_SURFACE('',#71632,0.0999999999999994) ;
#6734 = CYLINDRICAL_SURFACE('',#71636,0.1) ;
#6735 = CYLINDRICAL_SURFACE('',#71641,0.0999999999999994) ;
#6736 = CYLINDRICAL_SURFACE('',#71646,0.0999999999999994) ;
#6737 = CYLINDRICAL_SURFACE('',#71648,0.1) ;
#6738 = CYLINDRICAL_SURFACE('',#71651,0.0999999999999994) ;
#6739 = CYLINDRICAL_SURFACE('',#71653,0.1) ;
#6740 = CYLINDRICAL_SURFACE('',#71655,0.1) ;
#6741 = CYLINDRICAL_SURFACE('',#71662,0.1) ;
#6742 = CYLINDRICAL_SURFACE('',#71664,0.0999999999999994) ;
#6743 = CYLINDRICAL_SURFACE('',#71668,0.1) ;
#6744 = CYLINDRICAL_SURFACE('',#71670,0.0999999999999994) ;
#6745 = CYLINDRICAL_SURFACE('',#71674,0.0999999999999998) ;
#6746 = CYLINDRICAL_SURFACE('',#71676,0.1) ;
#6747 = CYLINDRICAL_SURFACE('',#71678,0.1) ;
#6748 = CYLINDRICAL_SURFACE('',#71681,0.1) ;
#6749 = CYLINDRICAL_SURFACE('',#71684,0.0999999999999994) ;
#6750 = CYLINDRICAL_SURFACE('',#71689,0.0999999999999998) ;
#6751 = CYLINDRICAL_SURFACE('',#71691,0.1) ;
#6752 = CYLINDRICAL_SURFACE('',#71695,0.0999999999999994) ;
#6753 = CYLINDRICAL_SURFACE('',#71697,0.1) ;
#6754 = CYLINDRICAL_SURFACE('',#71700,0.1) ;
#6755 = CYLINDRICAL_SURFACE('',#71703,0.0999999999999994) ;
#6756 = CYLINDRICAL_SURFACE('',#71709,0.0999999999999994) ;
#6757 = CYLINDRICAL_SURFACE('',#71710,0.0999999999999994) ;
#6758 = CYLINDRICAL_SURFACE('',#71712,0.0999999999999995) ;
#6759 = CYLINDRICAL_SURFACE('',#71716,0.0999999999999994) ;
#6760 = CYLINDRICAL_SURFACE('',#71718,0.0999999999999994) ;
#6761 = CYLINDRICAL_SURFACE('',#71722,0.0999999999999998) ;
#6762 = CYLINDRICAL_SURFACE('',#71723,0.0999999999999995) ;
#6763 = CYLINDRICAL_SURFACE('',#71726,0.0999999999999994) ;
#6764 = CYLINDRICAL_SURFACE('',#71730,0.0999999999999994) ;
#6765 = CYLINDRICAL_SURFACE('',#71732,0.0999999999999994) ;
#6766 = CYLINDRICAL_SURFACE('',#71736,0.0999999999999998) ;
#6767 = CYLINDRICAL_SURFACE('',#71738,0.1) ;
#6768 = CYLINDRICAL_SURFACE('',#71741,0.1) ;
#6769 = CYLINDRICAL_SURFACE('',#71742,0.1) ;
#6770 = CYLINDRICAL_SURFACE('',#71743,0.1) ;
#6771 = CYLINDRICAL_SURFACE('',#71744,0.0999999999999994) ;
#6772 = CYLINDRICAL_SURFACE('',#71745,0.0999999999999994) ;
#6773 = CYLINDRICAL_SURFACE('',#71750,0.0999999999999994) ;
#6774 = CYLINDRICAL_SURFACE('',#71753,0.0999999999999994) ;
#6775 = CYLINDRICAL_SURFACE('',#71757,0.1) ;
#6776 = CYLINDRICAL_SURFACE('',#71760,0.1) ;
#6777 = CYLINDRICAL_SURFACE('',#71764,0.1) ;
#6778 = CYLINDRICAL_SURFACE('',#71767,0.0999999999999994) ;
#6779 = CYLINDRICAL_SURFACE('',#71769,0.0999999999999994) ;
#6780 = CYLINDRICAL_SURFACE('',#71772,0.0999999999999994) ;
#6781 = CYLINDRICAL_SURFACE('',#71774,0.0999999999999994) ;
#6782 = CYLINDRICAL_SURFACE('',#71776,0.0999999999999994) ;
#6783 = CYLINDRICAL_SURFACE('',#71778,0.0999999999999994) ;
#6784 = CYLINDRICAL_SURFACE('',#71787,0.1) ;
#6785 = CYLINDRICAL_SURFACE('',#71789,0.0999999999999994) ;
#6786 = CYLINDRICAL_SURFACE('',#71795,0.0999999999999994) ;
#6787 = CYLINDRICAL_SURFACE('',#71797,0.1) ;
#6788 = CYLINDRICAL_SURFACE('',#71803,0.0999999999999994) ;
#6789 = CYLINDRICAL_SURFACE('',#71805,0.0999999999999994) ;
#6790 = CYLINDRICAL_SURFACE('',#71811,0.0999999999999994) ;
#6791 = CYLINDRICAL_SURFACE('',#71813,0.0999999999999994) ;
#6792 = CYLINDRICAL_SURFACE('',#71816,0.0999999999999994) ;
#6793 = CYLINDRICAL_SURFACE('',#71822,0.0999999999999994) ;
#6794 = CYLINDRICAL_SURFACE('',#71825,0.0999999999999994) ;
#6795 = CYLINDRICAL_SURFACE('',#71828,0.0999999999999994) ;
#6796 = CYLINDRICAL_SURFACE('',#71830,1.4986) ;
#6797 = CYLINDRICAL_SURFACE('',#71834,1.9939) ;
#6798 = CYLINDRICAL_SURFACE('',#71855,0.254) ;
#6799 = CYLINDRICAL_SURFACE('',#71856,0.254) ;
#6800 = CYLINDRICAL_SURFACE('',#71857,0.254) ;
#6801 = CYLINDRICAL_SURFACE('',#71858,0.254) ;
#6802 = CYLINDRICAL_SURFACE('',#71880,0.1) ;
#6803 = CYLINDRICAL_SURFACE('',#71897,0.1) ;
#6804 = CYLINDRICAL_SURFACE('',#71914,0.1) ;
#6805 = CYLINDRICAL_SURFACE('',#71931,0.1) ;
#6806 = CYLINDRICAL_SURFACE('',#71948,0.1) ;
#6807 = CYLINDRICAL_SURFACE('',#71965,0.1) ;
#6808 = CYLINDRICAL_SURFACE('',#71982,0.1) ;
#6809 = CYLINDRICAL_SURFACE('',#71999,0.1) ;
#6810 = CYLINDRICAL_SURFACE('',#72061,0.1) ;
#6811 = CYLINDRICAL_SURFACE('',#72065,1.) ;
#6812 = CYLINDRICAL_SURFACE('',#72066,1.) ;
#6813 = CYLINDRICAL_SURFACE('',#72067,1.) ;
#6814 = CYLINDRICAL_SURFACE('',#72068,1.) ;
#6815 = CYLINDRICAL_SURFACE('',#72069,1.) ;
#6816 = CYLINDRICAL_SURFACE('',#72070,0.999999999999999) ;
#6817 = CYLINDRICAL_SURFACE('',#72071,0.999999999999999) ;
#6818 = CYLINDRICAL_SURFACE('',#72072,1.) ;
#6819 = CYLINDRICAL_SURFACE('',#72073,1.) ;
#6820 = CYLINDRICAL_SURFACE('',#72074,0.1) ;
#6821 = CYLINDRICAL_SURFACE('',#72076,0.100000000000001) ;
#6822 = CYLINDRICAL_SURFACE('',#72078,0.100000000000001) ;
#6823 = CYLINDRICAL_SURFACE('',#72080,0.0999999999999994) ;
#6824 = CYLINDRICAL_SURFACE('',#72082,0.0999999999999994) ;
#6825 = CYLINDRICAL_SURFACE('',#72084,0.0999999999999994) ;
#6826 = CYLINDRICAL_SURFACE('',#72086,0.0999999999999994) ;
#6827 = CYLINDRICAL_SURFACE('',#72088,0.100000000000003) ;
#6828 = CYLINDRICAL_SURFACE('',#72090,0.100000000000003) ;
#6829 = CYLINDRICAL_SURFACE('',#72110,0.1) ;
#6830 = CYLINDRICAL_SURFACE('',#72114,1.) ;
#6831 = CYLINDRICAL_SURFACE('',#72115,0.1) ;
#6832 = CYLINDRICAL_SURFACE('',#72198,0.1) ;
#6833 = CYLINDRICAL_SURFACE('',#72201,0.1) ;
#6834 = CYLINDRICAL_SURFACE('',#72204,0.1) ;
#6835 = CYLINDRICAL_SURFACE('',#72207,0.1) ;
#6836 = CYLINDRICAL_SURFACE('',#72210,0.1) ;
#6837 = CYLINDRICAL_SURFACE('',#72213,0.1) ;
#6838 = CYLINDRICAL_SURFACE('',#72216,0.1) ;
#6839 = CYLINDRICAL_SURFACE('',#72219,0.1) ;
#6840 = CYLINDRICAL_SURFACE('',#72222,0.1) ;
#6841 = CYLINDRICAL_SURFACE('',#72234,0.1) ;
#6842 = CYLINDRICAL_SURFACE('',#72237,0.0999999999999994) ;
#6843 = CYLINDRICAL_SURFACE('',#72261,0.1) ;
#6844 = CYLINDRICAL_SURFACE('',#72285,0.1) ;
#6845 = CYLINDRICAL_SURFACE('',#72289,0.1) ;
#6846 = CYLINDRICAL_SURFACE('',#72293,0.1) ;
#6847 = CYLINDRICAL_SURFACE('',#72297,0.100000000000001) ;
#6848 = CYLINDRICAL_SURFACE('',#72301,0.1) ;
#6849 = CYLINDRICAL_SURFACE('',#72305,0.0999999999999994) ;
#6850 = CYLINDRICAL_SURFACE('',#72423,0.1) ;
#6851 = CYLINDRICAL_SURFACE('',#72427,0.1) ;
#6852 = CYLINDRICAL_SURFACE('',#72431,0.0999999999999994) ;
#6853 = CYLINDRICAL_SURFACE('',#72435,0.1) ;
#6854 = CYLINDRICAL_SURFACE('',#72439,0.1) ;
#6855 = CYLINDRICAL_SURFACE('',#72443,0.1) ;
#6856 = CYLINDRICAL_SURFACE('',#72447,0.1) ;
#6857 = CYLINDRICAL_SURFACE('',#72451,0.1) ;
#6858 = CYLINDRICAL_SURFACE('',#72455,0.1) ;
#6859 = CYLINDRICAL_SURFACE('',#72459,0.1) ;
#6860 = CYLINDRICAL_SURFACE('',#72462,1.65625) ;
#6861 = CYLINDRICAL_SURFACE('',#72465,0.1) ;
#6862 = CYLINDRICAL_SURFACE('',#72469,0.1) ;
#6863 = CYLINDRICAL_SURFACE('',#72473,0.1) ;
#6864 = CYLINDRICAL_SURFACE('',#72488,0.1) ;
#6865 = CYLINDRICAL_SURFACE('',#72491,0.1) ;
#6866 = CYLINDRICAL_SURFACE('',#72502,0.1) ;
#6867 = CYLINDRICAL_SURFACE('',#72504,0.1) ;
#6868 = CYLINDRICAL_SURFACE('',#72506,0.1) ;
#6869 = CYLINDRICAL_SURFACE('',#72508,0.1) ;
#6870 = CYLINDRICAL_SURFACE('',#72510,0.1) ;
#6871 = CYLINDRICAL_SURFACE('',#72512,0.1) ;
#6872 = CYLINDRICAL_SURFACE('',#72523,0.1) ;
#6873 = CYLINDRICAL_SURFACE('',#72525,0.0999999999999998) ;
#6874 = CYLINDRICAL_SURFACE('',#72527,0.1) ;
#6875 = CYLINDRICAL_SURFACE('',#72529,0.1) ;
#6876 = CYLINDRICAL_SURFACE('',#72531,0.1) ;
#6877 = CYLINDRICAL_SURFACE('',#72541,0.1) ;
#6878 = CYLINDRICAL_SURFACE('',#72548,0.1) ;
#6879 = CYLINDRICAL_SURFACE('',#72550,0.1) ;
#6880 = CYLINDRICAL_SURFACE('',#72552,0.1) ;
#6881 = CYLINDRICAL_SURFACE('',#72556,0.1) ;
#6882 = CYLINDRICAL_SURFACE('',#72558,0.1) ;
#6883 = CYLINDRICAL_SURFACE('',#72560,0.0999999999999998) ;
#6884 = CYLINDRICAL_SURFACE('',#72567,0.1) ;
#6885 = CYLINDRICAL_SURFACE('',#72574,0.1) ;
#6886 = CYLINDRICAL_SURFACE('',#72576,0.1) ;
#6887 = CYLINDRICAL_SURFACE('',#72580,0.1) ;
#6888 = CYLINDRICAL_SURFACE('',#72583,0.1) ;
#6889 = CYLINDRICAL_SURFACE('',#72585,0.1) ;
#6890 = CYLINDRICAL_SURFACE('',#72591,0.100000000000003) ;
#6891 = CYLINDRICAL_SURFACE('',#72593,0.100000000000003) ;
#6892 = CYLINDRICAL_SURFACE('',#72599,0.1) ;
#6893 = CYLINDRICAL_SURFACE('',#72601,0.1) ;
#6894 = CYLINDRICAL_SURFACE('',#72607,0.1) ;
#6895 = CYLINDRICAL_SURFACE('',#72609,0.1) ;
#6896 = CYLINDRICAL_SURFACE('',#72615,0.100000000000003) ;
#6897 = CYLINDRICAL_SURFACE('',#72617,0.100000000000003) ;
#6898 = CYLINDRICAL_SURFACE('',#72623,0.0999999999999998) ;
#6899 = CYLINDRICAL_SURFACE('',#72625,0.0999999999999998) ;
#6900 = CYLINDRICAL_SURFACE('',#72631,0.1) ;
#6901 = CYLINDRICAL_SURFACE('',#72633,0.1) ;
#6902 = CYLINDRICAL_SURFACE('',#72639,0.1) ;
#6903 = CYLINDRICAL_SURFACE('',#72641,0.1) ;
#6904 = CYLINDRICAL_SURFACE('',#72647,0.0999999999999998) ;
#6905 = CYLINDRICAL_SURFACE('',#72649,0.0999999999999998) ;
#6906 = CYLINDRICAL_SURFACE('',#72652,0.1) ;
#6907 = CYLINDRICAL_SURFACE('',#72659,0.1) ;
#6908 = CYLINDRICAL_SURFACE('',#72661,0.1) ;
#6909 = CYLINDRICAL_SURFACE('',#72667,0.1) ;
#6910 = CYLINDRICAL_SURFACE('',#72669,0.1) ;
#6911 = CYLINDRICAL_SURFACE('',#72675,0.0999999999999999) ;
#6912 = CYLINDRICAL_SURFACE('',#72683,0.1) ;
#6913 = CYLINDRICAL_SURFACE('',#72684,0.1) ;
#6914 = CYLINDRICAL_SURFACE('',#72688,0.1) ;
#6915 = CYLINDRICAL_SURFACE('',#72690,0.1) ;
#6916 = CYLINDRICAL_SURFACE('',#72696,0.0999999999999998) ;
#6917 = CYLINDRICAL_SURFACE('',#72698,0.1) ;
#6918 = CYLINDRICAL_SURFACE('',#72704,0.1) ;
#6919 = CYLINDRICAL_SURFACE('',#72705,0.1) ;
#6920 = CYLINDRICAL_SURFACE('',#72712,0.0999999999999994) ;
#6921 = CYLINDRICAL_SURFACE('',#72714,0.1) ;
#6922 = CYLINDRICAL_SURFACE('',#72720,0.1) ;
#6923 = CYLINDRICAL_SURFACE('',#72721,0.1) ;
#6924 = CYLINDRICAL_SURFACE('',#72725,0.1) ;
#6925 = CYLINDRICAL_SURFACE('',#72727,0.0999999999999994) ;
#6926 = CYLINDRICAL_SURFACE('',#72733,0.1) ;
#6927 = CYLINDRICAL_SURFACE('',#72741,0.0999999999999998) ;
#6928 = CYLINDRICAL_SURFACE('',#72743,0.0999999999999994) ;
#6929 = CYLINDRICAL_SURFACE('',#72749,0.1) ;
#6930 = CYLINDRICAL_SURFACE('',#72751,0.1) ;
#6931 = CYLINDRICAL_SURFACE('',#72757,0.1) ;
#6932 = CYLINDRICAL_SURFACE('',#72769,1.) ;
#6933 = CYLINDRICAL_SURFACE('',#72772,0.2) ;
#6934 = CYLINDRICAL_SURFACE('',#72786,0.1) ;
#6935 = CYLINDRICAL_SURFACE('',#72789,0.1) ;
#6936 = CYLINDRICAL_SURFACE('',#72795,0.1) ;
#6937 = CYLINDRICAL_SURFACE('',#72798,0.1) ;
#6938 = CYLINDRICAL_SURFACE('',#72800,0.1) ;
#6939 = CYLINDRICAL_SURFACE('',#72807,0.1) ;
#6940 = CYLINDRICAL_SURFACE('',#72809,0.1) ;
#6941 = CYLINDRICAL_SURFACE('',#72811,0.1) ;
#6942 = CYLINDRICAL_SURFACE('',#72815,0.1) ;
#6943 = CYLINDRICAL_SURFACE('',#72818,0.1) ;
#6944 = CYLINDRICAL_SURFACE('',#72820,0.1) ;
#6945 = CYLINDRICAL_SURFACE('',#72823,0.1) ;
#6946 = CYLINDRICAL_SURFACE('',#72829,0.1) ;
#6947 = CYLINDRICAL_SURFACE('',#72832,0.1) ;
#6948 = CYLINDRICAL_SURFACE('',#72834,0.1) ;
#6949 = CYLINDRICAL_SURFACE('',#72841,0.1) ;
#6950 = CYLINDRICAL_SURFACE('',#72843,0.1) ;
#6951 = CYLINDRICAL_SURFACE('',#72845,0.1) ;
#6952 = CYLINDRICAL_SURFACE('',#72849,0.1) ;
#6953 = CYLINDRICAL_SURFACE('',#72852,0.1) ;
#6954 = CYLINDRICAL_SURFACE('',#72856,0.1) ;
#6955 = CYLINDRICAL_SURFACE('',#72860,0.1) ;
#6956 = CYLINDRICAL_SURFACE('',#72864,0.1) ;
#6957 = CYLINDRICAL_SURFACE('',#72869,0.1) ;
#6958 = CYLINDRICAL_SURFACE('',#72873,0.1) ;
#6959 = CYLINDRICAL_SURFACE('',#72877,0.1) ;
#6960 = CYLINDRICAL_SURFACE('',#72880,0.1) ;
#6961 = CYLINDRICAL_SURFACE('',#72884,0.1) ;
#6962 = CYLINDRICAL_SURFACE('',#72888,0.1) ;
#6963 = CYLINDRICAL_SURFACE('',#72889,0.1) ;
#6964 = CYLINDRICAL_SURFACE('',#72893,0.1) ;
#6965 = CYLINDRICAL_SURFACE('',#72895,0.1) ;
#6966 = CYLINDRICAL_SURFACE('',#72970,0.100000000000003) ;
#6967 = CYLINDRICAL_SURFACE('',#72974,0.100000000000003) ;
#6968 = CYLINDRICAL_SURFACE('',#72978,0.0999999999999959) ;
#6969 = CYLINDRICAL_SURFACE('',#72982,0.100000000000003) ;
#6970 = CYLINDRICAL_SURFACE('',#72986,0.100000000000003) ;
#6971 = CYLINDRICAL_SURFACE('',#72990,0.100000000000003) ;
#6972 = CYLINDRICAL_SURFACE('',#72994,0.100000000000003) ;
#6973 = CYLINDRICAL_SURFACE('',#72998,0.100000000000003) ;
#6974 = CYLINDRICAL_SURFACE('',#73002,0.100000000000003) ;
#6975 = CYLINDRICAL_SURFACE('',#73006,0.100000000000003) ;
#6976 = CYLINDRICAL_SURFACE('',#73009,1.65625) ;
#6977 = CYLINDRICAL_SURFACE('',#73012,0.100000000000003) ;
#6978 = CYLINDRICAL_SURFACE('',#73016,0.100000000000003) ;
#6979 = CYLINDRICAL_SURFACE('',#73020,0.100000000000003) ;
#6980 = CYLINDRICAL_SURFACE('',#73030,0.0999999999999994) ;
#6981 = CYLINDRICAL_SURFACE('',#73034,0.0999999999999994) ;
#6982 = CYLINDRICAL_SURFACE('',#73038,0.0999999999999994) ;
#6983 = CYLINDRICAL_SURFACE('',#73042,0.0999999999999994) ;
#6984 = CYLINDRICAL_SURFACE('',#73046,0.100000000000003) ;
#6985 = CYLINDRICAL_SURFACE('',#73050,0.0999999999999994) ;
#6986 = CYLINDRICAL_SURFACE('',#73054,0.0999999999999994) ;
#6987 = CYLINDRICAL_SURFACE('',#73058,0.100000000000003) ;
#6988 = CYLINDRICAL_SURFACE('',#73062,0.100000000000003) ;
#6989 = CYLINDRICAL_SURFACE('',#73066,0.100000000000003) ;
#6990 = CYLINDRICAL_SURFACE('',#73069,1.65625) ;
#6991 = CYLINDRICAL_SURFACE('',#73072,0.0999999999999994) ;
#6992 = CYLINDRICAL_SURFACE('',#73076,0.0999999999999994) ;
#6993 = CYLINDRICAL_SURFACE('',#73080,0.0999999999999994) ;
#6994 = CYLINDRICAL_SURFACE('',#73090,0.0999999999999994) ;
#6995 = CYLINDRICAL_SURFACE('',#73094,0.0999999999999994) ;
#6996 = CYLINDRICAL_SURFACE('',#73098,0.0999999999999994) ;
#6997 = CYLINDRICAL_SURFACE('',#73102,0.0999999999999994) ;
#6998 = CYLINDRICAL_SURFACE('',#73106,0.0999999999999994) ;
#6999 = CYLINDRICAL_SURFACE('',#73110,0.0999999999999994) ;
#7000 = CYLINDRICAL_SURFACE('',#73114,0.0999999999999994) ;
#7001 = CYLINDRICAL_SURFACE('',#73118,0.0999999999999994) ;
#7002 = CYLINDRICAL_SURFACE('',#73122,0.0999999999999994) ;
#7003 = CYLINDRICAL_SURFACE('',#73126,0.0999999999999994) ;
#7004 = CYLINDRICAL_SURFACE('',#73129,1.65625) ;
#7005 = CYLINDRICAL_SURFACE('',#73132,0.0999999999999994) ;
#7006 = CYLINDRICAL_SURFACE('',#73136,0.0999999999999994) ;
#7007 = CYLINDRICAL_SURFACE('',#73140,0.0999999999999994) ;
#7008 = CYLINDRICAL_SURFACE('',#73150,0.0999999999999994) ;
#7009 = CYLINDRICAL_SURFACE('',#73154,0.0999999999999994) ;
#7010 = CYLINDRICAL_SURFACE('',#73158,0.0999999999999994) ;
#7011 = CYLINDRICAL_SURFACE('',#73162,0.0999999999999994) ;
#7012 = CYLINDRICAL_SURFACE('',#73166,0.0999999999999994) ;
#7013 = CYLINDRICAL_SURFACE('',#73170,0.0999999999999994) ;
#7014 = CYLINDRICAL_SURFACE('',#73174,0.0999999999999994) ;
#7015 = CYLINDRICAL_SURFACE('',#73178,0.0999999999999994) ;
#7016 = CYLINDRICAL_SURFACE('',#73182,0.0999999999999994) ;
#7017 = CYLINDRICAL_SURFACE('',#73186,0.0999999999999994) ;
#7018 = CYLINDRICAL_SURFACE('',#73189,1.65625) ;
#7019 = CYLINDRICAL_SURFACE('',#73192,0.0999999999999994) ;
#7020 = CYLINDRICAL_SURFACE('',#73196,0.0999999999999994) ;
#7021 = CYLINDRICAL_SURFACE('',#73200,0.0999999999999994) ;
#7022 = CYLINDRICAL_SURFACE('',#73210,0.0999999999999994) ;
#7023 = CYLINDRICAL_SURFACE('',#73214,0.0999999999999994) ;
#7024 = CYLINDRICAL_SURFACE('',#73218,0.0999999999999994) ;
#7025 = CYLINDRICAL_SURFACE('',#73222,0.0999999999999994) ;
#7026 = CYLINDRICAL_SURFACE('',#73226,0.0999999999999994) ;
#7027 = CYLINDRICAL_SURFACE('',#73230,0.0999999999999994) ;
#7028 = CYLINDRICAL_SURFACE('',#73234,0.0999999999999994) ;
#7029 = CYLINDRICAL_SURFACE('',#73238,0.0999999999999994) ;
#7030 = CYLINDRICAL_SURFACE('',#73242,0.0999999999999994) ;
#7031 = CYLINDRICAL_SURFACE('',#73246,0.0999999999999994) ;
#7032 = CYLINDRICAL_SURFACE('',#73249,1.65625) ;
#7033 = CYLINDRICAL_SURFACE('',#73252,0.0999999999999994) ;
#7034 = CYLINDRICAL_SURFACE('',#73256,0.0999999999999994) ;
#7035 = CYLINDRICAL_SURFACE('',#73260,0.0999999999999994) ;
#7036 = CYLINDRICAL_SURFACE('',#73270,0.0999999999999994) ;
#7037 = CYLINDRICAL_SURFACE('',#73274,0.0999999999999994) ;
#7038 = CYLINDRICAL_SURFACE('',#73278,0.0999999999999994) ;
#7039 = CYLINDRICAL_SURFACE('',#73282,0.100000000000001) ;
#7040 = CYLINDRICAL_SURFACE('',#73286,0.0999999999999994) ;
#7041 = CYLINDRICAL_SURFACE('',#73290,0.0999999999999994) ;
#7042 = CYLINDRICAL_SURFACE('',#73294,0.0999999999999994) ;
#7043 = CYLINDRICAL_SURFACE('',#73298,0.0999999999999994) ;
#7044 = CYLINDRICAL_SURFACE('',#73302,0.0999999999999994) ;
#7045 = CYLINDRICAL_SURFACE('',#73306,0.0999999999999994) ;
#7046 = CYLINDRICAL_SURFACE('',#73309,1.65625) ;
#7047 = CYLINDRICAL_SURFACE('',#73312,0.0999999999999994) ;
#7048 = CYLINDRICAL_SURFACE('',#73316,0.0999999999999994) ;
#7049 = CYLINDRICAL_SURFACE('',#73320,0.0999999999999994) ;
#7050 = CYLINDRICAL_SURFACE('',#73330,0.0999999999999994) ;
#7051 = CYLINDRICAL_SURFACE('',#73334,0.0999999999999994) ;
#7052 = CYLINDRICAL_SURFACE('',#73338,0.0999999999999994) ;
#7053 = CYLINDRICAL_SURFACE('',#73342,0.100000000000001) ;
#7054 = CYLINDRICAL_SURFACE('',#73346,0.100000000000001) ;
#7055 = CYLINDRICAL_SURFACE('',#73350,0.0999999999999994) ;
#7056 = CYLINDRICAL_SURFACE('',#73354,0.0999999999999994) ;
#7057 = CYLINDRICAL_SURFACE('',#73358,0.0999999999999994) ;
#7058 = CYLINDRICAL_SURFACE('',#73362,0.0999999999999994) ;
#7059 = CYLINDRICAL_SURFACE('',#73366,0.0999999999999994) ;
#7060 = CYLINDRICAL_SURFACE('',#73369,1.65625) ;
#7061 = CYLINDRICAL_SURFACE('',#73372,0.0999999999999994) ;
#7062 = CYLINDRICAL_SURFACE('',#73376,0.0999999999999994) ;
#7063 = CYLINDRICAL_SURFACE('',#73380,0.0999999999999994) ;
#7064 = CYLINDRICAL_SURFACE('',#73390,0.1) ;
#7065 = CYLINDRICAL_SURFACE('',#73394,0.1) ;
#7066 = CYLINDRICAL_SURFACE('',#73398,0.0999999999999994) ;
#7067 = CYLINDRICAL_SURFACE('',#73402,0.1) ;
#7068 = CYLINDRICAL_SURFACE('',#73406,0.100000000000001) ;
#7069 = CYLINDRICAL_SURFACE('',#73410,0.0999999999999994) ;
#7070 = CYLINDRICAL_SURFACE('',#73414,0.0999999999999994) ;
#7071 = CYLINDRICAL_SURFACE('',#73418,0.0999999999999994) ;
#7072 = CYLINDRICAL_SURFACE('',#73422,0.0999999999999994) ;
#7073 = CYLINDRICAL_SURFACE('',#73426,0.0999999999999994) ;
#7074 = CYLINDRICAL_SURFACE('',#73429,1.65625) ;
#7075 = CYLINDRICAL_SURFACE('',#73432,0.1) ;
#7076 = CYLINDRICAL_SURFACE('',#73436,0.1) ;
#7077 = CYLINDRICAL_SURFACE('',#73440,0.1) ;
#7078 = CYLINDRICAL_SURFACE('',#73450,0.0999999999999998) ;
#7079 = CYLINDRICAL_SURFACE('',#73454,0.0999999999999998) ;
#7080 = CYLINDRICAL_SURFACE('',#73458,0.0999999999999994) ;
#7081 = CYLINDRICAL_SURFACE('',#73462,0.100000000000001) ;
#7082 = CYLINDRICAL_SURFACE('',#73466,0.1) ;
#7083 = CYLINDRICAL_SURFACE('',#73470,0.1) ;
#7084 = CYLINDRICAL_SURFACE('',#73474,0.1) ;
#7085 = CYLINDRICAL_SURFACE('',#73478,0.1) ;
#7086 = CYLINDRICAL_SURFACE('',#73482,0.1) ;
#7087 = CYLINDRICAL_SURFACE('',#73486,0.1) ;
#7088 = CYLINDRICAL_SURFACE('',#73489,1.65625) ;
#7089 = CYLINDRICAL_SURFACE('',#73492,0.0999999999999998) ;
#7090 = CYLINDRICAL_SURFACE('',#73496,0.0999999999999998) ;
#7091 = CYLINDRICAL_SURFACE('',#73500,0.1) ;
#7092 = CYLINDRICAL_SURFACE('',#73555,0.1) ;
#7093 = CYLINDRICAL_SURFACE('',#73558,0.1) ;
#7094 = CYLINDRICAL_SURFACE('',#73569,0.1) ;
#7095 = CYLINDRICAL_SURFACE('',#73571,0.1) ;
#7096 = CYLINDRICAL_SURFACE('',#73573,0.1) ;
#7097 = CYLINDRICAL_SURFACE('',#73575,0.1) ;
#7098 = CYLINDRICAL_SURFACE('',#73577,0.1) ;
#7099 = CYLINDRICAL_SURFACE('',#73579,0.1) ;
#7100 = CYLINDRICAL_SURFACE('',#73590,0.1) ;
#7101 = CYLINDRICAL_SURFACE('',#73592,0.0999999999999998) ;
#7102 = CYLINDRICAL_SURFACE('',#73594,0.1) ;
#7103 = CYLINDRICAL_SURFACE('',#73596,0.1) ;
#7104 = CYLINDRICAL_SURFACE('',#73598,0.1) ;
#7105 = CYLINDRICAL_SURFACE('',#73608,0.1) ;
#7106 = CYLINDRICAL_SURFACE('',#73615,0.1) ;
#7107 = CYLINDRICAL_SURFACE('',#73617,0.1) ;
#7108 = CYLINDRICAL_SURFACE('',#73619,0.0999999999999998) ;
#7109 = CYLINDRICAL_SURFACE('',#73623,0.1) ;
#7110 = CYLINDRICAL_SURFACE('',#73625,0.1) ;
#7111 = CYLINDRICAL_SURFACE('',#73627,0.0999999999999998) ;
#7112 = CYLINDRICAL_SURFACE('',#73634,0.1) ;
#7113 = CYLINDRICAL_SURFACE('',#73641,0.1) ;
#7114 = CYLINDRICAL_SURFACE('',#73643,0.1) ;
#7115 = CYLINDRICAL_SURFACE('',#73647,0.1) ;
#7116 = CYLINDRICAL_SURFACE('',#73650,0.1) ;
#7117 = CYLINDRICAL_SURFACE('',#73652,0.1) ;
#7118 = CYLINDRICAL_SURFACE('',#73655,0.1) ;
#7119 = CYLINDRICAL_SURFACE('',#73662,0.1) ;
#7120 = CYLINDRICAL_SURFACE('',#73664,0.1) ;
#7121 = CYLINDRICAL_SURFACE('',#73670,0.1) ;
#7122 = CYLINDRICAL_SURFACE('',#73672,0.1) ;
#7123 = CYLINDRICAL_SURFACE('',#73678,0.1) ;
#7124 = CYLINDRICAL_SURFACE('',#73686,0.1) ;
#7125 = CYLINDRICAL_SURFACE('',#73687,0.1) ;
#7126 = CYLINDRICAL_SURFACE('',#73691,0.1) ;
#7127 = CYLINDRICAL_SURFACE('',#73693,0.0999999999999998) ;
#7128 = CYLINDRICAL_SURFACE('',#73699,0.0999999999999998) ;
#7129 = CYLINDRICAL_SURFACE('',#73701,0.1) ;
#7130 = CYLINDRICAL_SURFACE('',#73707,0.0999999999999998) ;
#7131 = CYLINDRICAL_SURFACE('',#73708,0.100000000000003) ;
#7132 = CYLINDRICAL_SURFACE('',#73715,0.0999999999999994) ;
#7133 = CYLINDRICAL_SURFACE('',#73717,0.1) ;
#7134 = CYLINDRICAL_SURFACE('',#73723,0.0999999999999989) ;
#7135 = CYLINDRICAL_SURFACE('',#73724,0.100000000000003) ;
#7136 = CYLINDRICAL_SURFACE('',#73728,0.1) ;
#7137 = CYLINDRICAL_SURFACE('',#73730,0.0999999999999994) ;
#7138 = CYLINDRICAL_SURFACE('',#73736,0.0999999999999989) ;
#7139 = CYLINDRICAL_SURFACE('',#73744,0.0999999999999998) ;
#7140 = CYLINDRICAL_SURFACE('',#73746,0.0999999999999994) ;
#7141 = CYLINDRICAL_SURFACE('',#73752,0.100000000000003) ;
#7142 = CYLINDRICAL_SURFACE('',#73754,0.100000000000003) ;
#7143 = CYLINDRICAL_SURFACE('',#73760,0.1) ;
#7144 = CYLINDRICAL_SURFACE('',#73761,0.0999999999999994) ;
#7145 = CYLINDRICAL_SURFACE('',#73768,0.0999999999999994) ;
#7146 = CYLINDRICAL_SURFACE('',#73770,0.1) ;
#7147 = CYLINDRICAL_SURFACE('',#73776,0.0999999999999989) ;
#7148 = CYLINDRICAL_SURFACE('',#73777,0.100000000000003) ;
#7149 = CYLINDRICAL_SURFACE('',#73781,0.1) ;
#7150 = CYLINDRICAL_SURFACE('',#73783,0.0999999999999994) ;
#7151 = CYLINDRICAL_SURFACE('',#73789,0.0999999999999989) ;
#7152 = CYLINDRICAL_SURFACE('',#73797,0.0999999999999998) ;
#7153 = CYLINDRICAL_SURFACE('',#73799,0.0999999999999994) ;
#7154 = CYLINDRICAL_SURFACE('',#73805,0.0999999999999994) ;
#7155 = CYLINDRICAL_SURFACE('',#73807,0.0999999999999994) ;
#7156 = CYLINDRICAL_SURFACE('',#73813,0.1) ;
#7157 = CYLINDRICAL_SURFACE('',#73814,0.0999999999999994) ;
#7158 = CYLINDRICAL_SURFACE('',#73821,0.0999999999999994) ;
#7159 = CYLINDRICAL_SURFACE('',#73823,0.1) ;
#7160 = CYLINDRICAL_SURFACE('',#73829,0.0999999999999989) ;
#7161 = CYLINDRICAL_SURFACE('',#73830,0.0999999999999994) ;
#7162 = CYLINDRICAL_SURFACE('',#73834,0.1) ;
#7163 = CYLINDRICAL_SURFACE('',#73836,0.0999999999999994) ;
#7164 = CYLINDRICAL_SURFACE('',#73842,0.0999999999999989) ;
#7165 = CYLINDRICAL_SURFACE('',#73850,0.0999999999999998) ;
#7166 = CYLINDRICAL_SURFACE('',#73852,0.0999999999999994) ;
#7167 = CYLINDRICAL_SURFACE('',#73858,0.0999999999999994) ;
#7168 = CYLINDRICAL_SURFACE('',#73860,0.0999999999999994) ;
#7169 = CYLINDRICAL_SURFACE('',#73866,0.1) ;
#7170 = CYLINDRICAL_SURFACE('',#73867,0.0999999999999994) ;
#7171 = CYLINDRICAL_SURFACE('',#73874,0.0999999999999994) ;
#7172 = CYLINDRICAL_SURFACE('',#73876,0.1) ;
#7173 = CYLINDRICAL_SURFACE('',#73882,0.0999999999999989) ;
#7174 = CYLINDRICAL_SURFACE('',#73883,0.0999999999999994) ;
#7175 = CYLINDRICAL_SURFACE('',#73887,0.1) ;
#7176 = CYLINDRICAL_SURFACE('',#73889,0.0999999999999994) ;
#7177 = CYLINDRICAL_SURFACE('',#73895,0.0999999999999989) ;
#7178 = CYLINDRICAL_SURFACE('',#73903,0.0999999999999998) ;
#7179 = CYLINDRICAL_SURFACE('',#73905,0.0999999999999994) ;
#7180 = CYLINDRICAL_SURFACE('',#73911,0.0999999999999994) ;
#7181 = CYLINDRICAL_SURFACE('',#73913,0.0999999999999994) ;
#7182 = CYLINDRICAL_SURFACE('',#73919,0.1) ;
#7183 = CYLINDRICAL_SURFACE('',#73920,0.0999999999999994) ;
#7184 = CYLINDRICAL_SURFACE('',#73927,0.0999999999999994) ;
#7185 = CYLINDRICAL_SURFACE('',#73929,0.1) ;
#7186 = CYLINDRICAL_SURFACE('',#73935,0.0999999999999989) ;
#7187 = CYLINDRICAL_SURFACE('',#73936,0.0999999999999994) ;
#7188 = CYLINDRICAL_SURFACE('',#73940,0.1) ;
#7189 = CYLINDRICAL_SURFACE('',#73942,0.0999999999999994) ;
#7190 = CYLINDRICAL_SURFACE('',#73948,0.0999999999999989) ;
#7191 = CYLINDRICAL_SURFACE('',#73956,0.0999999999999998) ;
#7192 = CYLINDRICAL_SURFACE('',#73958,0.0999999999999994) ;
#7193 = CYLINDRICAL_SURFACE('',#73964,0.0999999999999994) ;
#7194 = CYLINDRICAL_SURFACE('',#73966,0.0999999999999994) ;
#7195 = CYLINDRICAL_SURFACE('',#73972,0.1) ;
#7196 = CYLINDRICAL_SURFACE('',#73973,0.0999999999999994) ;
#7197 = CYLINDRICAL_SURFACE('',#73980,0.0999999999999994) ;
#7198 = CYLINDRICAL_SURFACE('',#73982,0.1) ;
#7199 = CYLINDRICAL_SURFACE('',#73988,0.0999999999999989) ;
#7200 = CYLINDRICAL_SURFACE('',#73989,0.0999999999999994) ;
#7201 = CYLINDRICAL_SURFACE('',#73993,0.1) ;
#7202 = CYLINDRICAL_SURFACE('',#73995,0.0999999999999994) ;
#7203 = CYLINDRICAL_SURFACE('',#74001,0.1) ;
#7204 = CYLINDRICAL_SURFACE('',#74009,0.0999999999999998) ;
#7205 = CYLINDRICAL_SURFACE('',#74011,0.0999999999999994) ;
#7206 = CYLINDRICAL_SURFACE('',#74017,0.0999999999999994) ;
#7207 = CYLINDRICAL_SURFACE('',#74019,0.0999999999999994) ;
#7208 = CYLINDRICAL_SURFACE('',#74025,0.1) ;
#7209 = CYLINDRICAL_SURFACE('',#74026,0.0999999999999994) ;
#7210 = CYLINDRICAL_SURFACE('',#74033,0.0999999999999994) ;
#7211 = CYLINDRICAL_SURFACE('',#74035,0.1) ;
#7212 = CYLINDRICAL_SURFACE('',#74041,0.1) ;
#7213 = CYLINDRICAL_SURFACE('',#74042,0.0999999999999994) ;
#7214 = CYLINDRICAL_SURFACE('',#74046,0.1) ;
#7215 = CYLINDRICAL_SURFACE('',#74048,0.0999999999999994) ;
#7216 = CYLINDRICAL_SURFACE('',#74054,0.1) ;
#7217 = CYLINDRICAL_SURFACE('',#74062,0.0999999999999998) ;
#7218 = CYLINDRICAL_SURFACE('',#74064,0.0999999999999994) ;
#7219 = CYLINDRICAL_SURFACE('',#74070,0.0999999999999994) ;
#7220 = CYLINDRICAL_SURFACE('',#74072,0.0999999999999994) ;
#7221 = CYLINDRICAL_SURFACE('',#74078,0.1) ;
#7222 = CYLINDRICAL_SURFACE('',#74079,0.0999999999999994) ;
#7223 = CYLINDRICAL_SURFACE('',#74086,0.0999999999999994) ;
#7224 = CYLINDRICAL_SURFACE('',#74088,0.1) ;
#7225 = CYLINDRICAL_SURFACE('',#74094,0.1) ;
#7226 = CYLINDRICAL_SURFACE('',#74095,0.0999999999999994) ;
#7227 = CYLINDRICAL_SURFACE('',#74099,0.1) ;
#7228 = CYLINDRICAL_SURFACE('',#74101,0.0999999999999994) ;
#7229 = CYLINDRICAL_SURFACE('',#74107,0.1) ;
#7230 = CYLINDRICAL_SURFACE('',#74115,0.0999999999999998) ;
#7231 = CYLINDRICAL_SURFACE('',#74117,0.0999999999999994) ;
#7232 = CYLINDRICAL_SURFACE('',#74123,0.1) ;
#7233 = CYLINDRICAL_SURFACE('',#74125,0.1) ;
#7234 = CYLINDRICAL_SURFACE('',#74131,0.1) ;
#7235 = CYLINDRICAL_SURFACE('',#74132,0.1) ;
#7236 = CYLINDRICAL_SURFACE('',#74139,0.0999999999999994) ;
#7237 = CYLINDRICAL_SURFACE('',#74141,0.1) ;
#7238 = CYLINDRICAL_SURFACE('',#74147,0.1) ;
#7239 = CYLINDRICAL_SURFACE('',#74148,0.1) ;
#7240 = CYLINDRICAL_SURFACE('',#74152,0.1) ;
#7241 = CYLINDRICAL_SURFACE('',#74154,0.0999999999999994) ;
#7242 = CYLINDRICAL_SURFACE('',#74160,0.1) ;
#7243 = CYLINDRICAL_SURFACE('',#74168,0.0999999999999998) ;
#7244 = CYLINDRICAL_SURFACE('',#74170,0.0999999999999994) ;
#7245 = CYLINDRICAL_SURFACE('',#74176,0.0999999999999998) ;
#7246 = CYLINDRICAL_SURFACE('',#74178,0.0999999999999998) ;
#7247 = CYLINDRICAL_SURFACE('',#74184,0.1) ;
#7248 = CYLINDRICAL_SURFACE('',#74185,0.1) ;
#7249 = CYLINDRICAL_SURFACE('',#74188,0.1) ;
#7250 = CYLINDRICAL_SURFACE('',#74199,0.1) ;
#7251 = CYLINDRICAL_SURFACE('',#74201,0.1) ;
#7252 = CYLINDRICAL_SURFACE('',#74203,0.1) ;
#7253 = CYLINDRICAL_SURFACE('',#74205,0.1) ;
#7254 = CYLINDRICAL_SURFACE('',#74207,0.1) ;
#7255 = CYLINDRICAL_SURFACE('',#74209,0.1) ;
#7256 = CYLINDRICAL_SURFACE('',#74220,0.1) ;
#7257 = CYLINDRICAL_SURFACE('',#74222,0.0999999999999998) ;
#7258 = CYLINDRICAL_SURFACE('',#74224,0.1) ;
#7259 = CYLINDRICAL_SURFACE('',#74226,0.1) ;
#7260 = CYLINDRICAL_SURFACE('',#74228,0.1) ;
#7261 = CYLINDRICAL_SURFACE('',#74238,0.1) ;
#7262 = CYLINDRICAL_SURFACE('',#74245,0.1) ;
#7263 = CYLINDRICAL_SURFACE('',#74247,0.1) ;
#7264 = CYLINDRICAL_SURFACE('',#74249,0.1) ;
#7265 = CYLINDRICAL_SURFACE('',#74253,0.1) ;
#7266 = CYLINDRICAL_SURFACE('',#74255,0.1) ;
#7267 = CYLINDRICAL_SURFACE('',#74257,0.0999999999999998) ;
#7268 = CYLINDRICAL_SURFACE('',#74264,0.1) ;
#7269 = CYLINDRICAL_SURFACE('',#74271,0.1) ;
#7270 = CYLINDRICAL_SURFACE('',#74273,0.1) ;
#7271 = CYLINDRICAL_SURFACE('',#74277,0.1) ;
#7272 = CYLINDRICAL_SURFACE('',#74280,0.1) ;
#7273 = CYLINDRICAL_SURFACE('',#74282,0.0999999999999994) ;
#7274 = CYLINDRICAL_SURFACE('',#74285,0.1) ;
#7275 = CYLINDRICAL_SURFACE('',#74292,0.0999999999999994) ;
#7276 = CYLINDRICAL_SURFACE('',#74294,0.0999999999999994) ;
#7277 = CYLINDRICAL_SURFACE('',#74300,0.1) ;
#7278 = CYLINDRICAL_SURFACE('',#74302,0.1) ;
#7279 = CYLINDRICAL_SURFACE('',#74308,0.1) ;
#7280 = CYLINDRICAL_SURFACE('',#74316,0.1) ;
#7281 = CYLINDRICAL_SURFACE('',#74317,0.1) ;
#7282 = CYLINDRICAL_SURFACE('',#74321,0.1) ;
#7283 = CYLINDRICAL_SURFACE('',#74323,0.1) ;
#7284 = CYLINDRICAL_SURFACE('',#74329,0.0999999999999998) ;
#7285 = CYLINDRICAL_SURFACE('',#74331,0.1) ;
#7286 = CYLINDRICAL_SURFACE('',#74337,0.1) ;
#7287 = CYLINDRICAL_SURFACE('',#74338,0.1) ;
#7288 = CYLINDRICAL_SURFACE('',#74341,0.1) ;
#7289 = CYLINDRICAL_SURFACE('',#74352,0.1) ;
#7290 = CYLINDRICAL_SURFACE('',#74354,0.1) ;
#7291 = CYLINDRICAL_SURFACE('',#74356,0.1) ;
#7292 = CYLINDRICAL_SURFACE('',#74358,0.1) ;
#7293 = CYLINDRICAL_SURFACE('',#74360,0.1) ;
#7294 = CYLINDRICAL_SURFACE('',#74362,0.1) ;
#7295 = CYLINDRICAL_SURFACE('',#74373,0.1) ;
#7296 = CYLINDRICAL_SURFACE('',#74375,0.0999999999999998) ;
#7297 = CYLINDRICAL_SURFACE('',#74377,0.1) ;
#7298 = CYLINDRICAL_SURFACE('',#74379,0.1) ;
#7299 = CYLINDRICAL_SURFACE('',#74381,0.1) ;
#7300 = CYLINDRICAL_SURFACE('',#74391,0.1) ;
#7301 = CYLINDRICAL_SURFACE('',#74398,0.1) ;
#7302 = CYLINDRICAL_SURFACE('',#74400,0.1) ;
#7303 = CYLINDRICAL_SURFACE('',#74402,0.0999999999999994) ;
#7304 = CYLINDRICAL_SURFACE('',#74406,0.1) ;
#7305 = CYLINDRICAL_SURFACE('',#74408,0.1) ;
#7306 = CYLINDRICAL_SURFACE('',#74410,0.0999999999999998) ;
#7307 = CYLINDRICAL_SURFACE('',#74417,0.1) ;
#7308 = CYLINDRICAL_SURFACE('',#74424,0.1) ;
#7309 = CYLINDRICAL_SURFACE('',#74426,0.1) ;
#7310 = CYLINDRICAL_SURFACE('',#74430,0.1) ;
#7311 = CYLINDRICAL_SURFACE('',#74433,0.1) ;
#7312 = CYLINDRICAL_SURFACE('',#74435,0.0999999999999994) ;
#7313 = CYLINDRICAL_SURFACE('',#74438,0.1) ;
#7314 = CYLINDRICAL_SURFACE('',#74445,0.0999999999999994) ;
#7315 = CYLINDRICAL_SURFACE('',#74447,0.0999999999999994) ;
#7316 = CYLINDRICAL_SURFACE('',#74453,0.1) ;
#7317 = CYLINDRICAL_SURFACE('',#74455,0.1) ;
#7318 = CYLINDRICAL_SURFACE('',#74461,0.1) ;
#7319 = CYLINDRICAL_SURFACE('',#74469,0.1) ;
#7320 = CYLINDRICAL_SURFACE('',#74470,0.1) ;
#7321 = CYLINDRICAL_SURFACE('',#74474,0.1) ;
#7322 = CYLINDRICAL_SURFACE('',#74476,0.0999999999999994) ;
#7323 = CYLINDRICAL_SURFACE('',#74482,0.0999999999999998) ;
#7324 = CYLINDRICAL_SURFACE('',#74484,0.1) ;
#7325 = CYLINDRICAL_SURFACE('',#74490,0.0999999999999994) ;
#7326 = CYLINDRICAL_SURFACE('',#74491,0.1) ;
#7327 = CYLINDRICAL_SURFACE('',#74494,0.1) ;
#7328 = CYLINDRICAL_SURFACE('',#74505,0.1) ;
#7329 = CYLINDRICAL_SURFACE('',#74507,0.1) ;
#7330 = CYLINDRICAL_SURFACE('',#74509,0.1) ;
#7331 = CYLINDRICAL_SURFACE('',#74511,0.1) ;
#7332 = CYLINDRICAL_SURFACE('',#74513,0.1) ;
#7333 = CYLINDRICAL_SURFACE('',#74515,0.1) ;
#7334 = CYLINDRICAL_SURFACE('',#74526,0.1) ;
#7335 = CYLINDRICAL_SURFACE('',#74528,0.0999999999999998) ;
#7336 = CYLINDRICAL_SURFACE('',#74530,0.1) ;
#7337 = CYLINDRICAL_SURFACE('',#74532,0.1) ;
#7338 = CYLINDRICAL_SURFACE('',#74534,0.1) ;
#7339 = CYLINDRICAL_SURFACE('',#74544,0.1) ;
#7340 = CYLINDRICAL_SURFACE('',#74551,0.1) ;
#7341 = CYLINDRICAL_SURFACE('',#74553,0.1) ;
#7342 = CYLINDRICAL_SURFACE('',#74555,0.0999999999999994) ;
#7343 = CYLINDRICAL_SURFACE('',#74559,0.1) ;
#7344 = CYLINDRICAL_SURFACE('',#74561,0.1) ;
#7345 = CYLINDRICAL_SURFACE('',#74563,0.0999999999999998) ;
#7346 = CYLINDRICAL_SURFACE('',#74570,0.1) ;
#7347 = CYLINDRICAL_SURFACE('',#74577,0.1) ;
#7348 = CYLINDRICAL_SURFACE('',#74579,0.1) ;
#7349 = CYLINDRICAL_SURFACE('',#74583,0.1) ;
#7350 = CYLINDRICAL_SURFACE('',#74586,0.1) ;
#7351 = CYLINDRICAL_SURFACE('',#74588,0.0999999999999994) ;
#7352 = CYLINDRICAL_SURFACE('',#74591,0.1) ;
#7353 = CYLINDRICAL_SURFACE('',#74598,0.0999999999999994) ;
#7354 = CYLINDRICAL_SURFACE('',#74600,0.0999999999999994) ;
#7355 = CYLINDRICAL_SURFACE('',#74606,0.1) ;
#7356 = CYLINDRICAL_SURFACE('',#74608,0.1) ;
#7357 = CYLINDRICAL_SURFACE('',#74614,0.1) ;
#7358 = CYLINDRICAL_SURFACE('',#74622,0.1) ;
#7359 = CYLINDRICAL_SURFACE('',#74623,0.1) ;
#7360 = CYLINDRICAL_SURFACE('',#74627,0.1) ;
#7361 = CYLINDRICAL_SURFACE('',#74629,0.0999999999999994) ;
#7362 = CYLINDRICAL_SURFACE('',#74635,0.0999999999999998) ;
#7363 = CYLINDRICAL_SURFACE('',#74637,0.1) ;
#7364 = CYLINDRICAL_SURFACE('',#74643,0.0999999999999994) ;
#7365 = CYLINDRICAL_SURFACE('',#74644,0.1) ;
#7366 = CYLINDRICAL_SURFACE('',#74647,0.1) ;
#7367 = CYLINDRICAL_SURFACE('',#74658,0.1) ;
#7368 = CYLINDRICAL_SURFACE('',#74660,0.1) ;
#7369 = CYLINDRICAL_SURFACE('',#74662,0.1) ;
#7370 = CYLINDRICAL_SURFACE('',#74664,0.1) ;
#7371 = CYLINDRICAL_SURFACE('',#74666,0.1) ;
#7372 = CYLINDRICAL_SURFACE('',#74668,0.1) ;
#7373 = CYLINDRICAL_SURFACE('',#74679,0.1) ;
#7374 = CYLINDRICAL_SURFACE('',#74681,0.0999999999999998) ;
#7375 = CYLINDRICAL_SURFACE('',#74683,0.1) ;
#7376 = CYLINDRICAL_SURFACE('',#74685,0.1) ;
#7377 = CYLINDRICAL_SURFACE('',#74687,0.1) ;
#7378 = CYLINDRICAL_SURFACE('',#74697,0.1) ;
#7379 = CYLINDRICAL_SURFACE('',#74704,0.1) ;
#7380 = CYLINDRICAL_SURFACE('',#74706,0.1) ;
#7381 = CYLINDRICAL_SURFACE('',#74708,0.0999999999999994) ;
#7382 = CYLINDRICAL_SURFACE('',#74712,0.1) ;
#7383 = CYLINDRICAL_SURFACE('',#74714,0.1) ;
#7384 = CYLINDRICAL_SURFACE('',#74716,0.0999999999999998) ;
#7385 = CYLINDRICAL_SURFACE('',#74723,0.1) ;
#7386 = CYLINDRICAL_SURFACE('',#74730,0.1) ;
#7387 = CYLINDRICAL_SURFACE('',#74732,0.1) ;
#7388 = CYLINDRICAL_SURFACE('',#74736,0.1) ;
#7389 = CYLINDRICAL_SURFACE('',#74739,0.1) ;
#7390 = CYLINDRICAL_SURFACE('',#74741,0.0999999999999994) ;
#7391 = CYLINDRICAL_SURFACE('',#74744,0.1) ;
#7392 = CYLINDRICAL_SURFACE('',#74751,0.0999999999999994) ;
#7393 = CYLINDRICAL_SURFACE('',#74753,0.0999999999999994) ;
#7394 = CYLINDRICAL_SURFACE('',#74759,0.1) ;
#7395 = CYLINDRICAL_SURFACE('',#74761,0.1) ;
#7396 = CYLINDRICAL_SURFACE('',#74767,0.0999999999999988) ;
#7397 = CYLINDRICAL_SURFACE('',#74775,0.1) ;
#7398 = CYLINDRICAL_SURFACE('',#74776,0.1) ;
#7399 = CYLINDRICAL_SURFACE('',#74780,0.0999999999999989) ;
#7400 = CYLINDRICAL_SURFACE('',#74782,0.0999999999999994) ;
#7401 = CYLINDRICAL_SURFACE('',#74788,0.0999999999999998) ;
#7402 = CYLINDRICAL_SURFACE('',#74790,0.1) ;
#7403 = CYLINDRICAL_SURFACE('',#74796,0.0999999999999994) ;
#7404 = CYLINDRICAL_SURFACE('',#74797,0.1) ;
#7405 = CYLINDRICAL_SURFACE('',#74800,0.1) ;
#7406 = CYLINDRICAL_SURFACE('',#74811,0.1) ;
#7407 = CYLINDRICAL_SURFACE('',#74813,0.1) ;
#7408 = CYLINDRICAL_SURFACE('',#74815,0.1) ;
#7409 = CYLINDRICAL_SURFACE('',#74817,0.1) ;
#7410 = CYLINDRICAL_SURFACE('',#74819,0.1) ;
#7411 = CYLINDRICAL_SURFACE('',#74821,0.1) ;
#7412 = CYLINDRICAL_SURFACE('',#74832,0.1) ;
#7413 = CYLINDRICAL_SURFACE('',#74834,0.0999999999999998) ;
#7414 = CYLINDRICAL_SURFACE('',#74836,0.1) ;
#7415 = CYLINDRICAL_SURFACE('',#74838,0.1) ;
#7416 = CYLINDRICAL_SURFACE('',#74840,0.1) ;
#7417 = CYLINDRICAL_SURFACE('',#74850,0.1) ;
#7418 = CYLINDRICAL_SURFACE('',#74857,0.1) ;
#7419 = CYLINDRICAL_SURFACE('',#74859,0.1) ;
#7420 = CYLINDRICAL_SURFACE('',#74861,0.0999999999999994) ;
#7421 = CYLINDRICAL_SURFACE('',#74865,0.1) ;
#7422 = CYLINDRICAL_SURFACE('',#74867,0.1) ;
#7423 = CYLINDRICAL_SURFACE('',#74869,0.0999999999999998) ;
#7424 = CYLINDRICAL_SURFACE('',#74876,0.1) ;
#7425 = CYLINDRICAL_SURFACE('',#74883,0.1) ;
#7426 = CYLINDRICAL_SURFACE('',#74885,0.1) ;
#7427 = CYLINDRICAL_SURFACE('',#74889,0.1) ;
#7428 = CYLINDRICAL_SURFACE('',#74892,0.1) ;
#7429 = CYLINDRICAL_SURFACE('',#74894,0.0999999999999994) ;
#7430 = CYLINDRICAL_SURFACE('',#74897,0.1) ;
#7431 = CYLINDRICAL_SURFACE('',#74904,0.0999999999999994) ;
#7432 = CYLINDRICAL_SURFACE('',#74906,0.0999999999999994) ;
#7433 = CYLINDRICAL_SURFACE('',#74912,0.1) ;
#7434 = CYLINDRICAL_SURFACE('',#74914,0.1) ;
#7435 = CYLINDRICAL_SURFACE('',#74920,0.0999999999999988) ;
#7436 = CYLINDRICAL_SURFACE('',#74928,0.1) ;
#7437 = CYLINDRICAL_SURFACE('',#74929,0.1) ;
#7438 = CYLINDRICAL_SURFACE('',#74933,0.0999999999999989) ;
#7439 = CYLINDRICAL_SURFACE('',#74935,0.0999999999999994) ;
#7440 = CYLINDRICAL_SURFACE('',#74941,0.0999999999999998) ;
#7441 = CYLINDRICAL_SURFACE('',#74943,0.1) ;
#7442 = CYLINDRICAL_SURFACE('',#74949,0.0999999999999994) ;
#7443 = CYLINDRICAL_SURFACE('',#74950,0.1) ;
#7444 = CYLINDRICAL_SURFACE('',#74953,0.1) ;
#7445 = CYLINDRICAL_SURFACE('',#74964,0.1) ;
#7446 = CYLINDRICAL_SURFACE('',#74966,0.1) ;
#7447 = CYLINDRICAL_SURFACE('',#74968,0.1) ;
#7448 = CYLINDRICAL_SURFACE('',#74970,0.1) ;
#7449 = CYLINDRICAL_SURFACE('',#74972,0.1) ;
#7450 = CYLINDRICAL_SURFACE('',#74974,0.1) ;
#7451 = CYLINDRICAL_SURFACE('',#74985,0.1) ;
#7452 = CYLINDRICAL_SURFACE('',#74987,0.0999999999999998) ;
#7453 = CYLINDRICAL_SURFACE('',#74989,0.1) ;
#7454 = CYLINDRICAL_SURFACE('',#74991,0.1) ;
#7455 = CYLINDRICAL_SURFACE('',#74993,0.1) ;
#7456 = CYLINDRICAL_SURFACE('',#75003,0.1) ;
#7457 = CYLINDRICAL_SURFACE('',#75010,0.1) ;
#7458 = CYLINDRICAL_SURFACE('',#75012,0.1) ;
#7459 = CYLINDRICAL_SURFACE('',#75014,0.0999999999999994) ;
#7460 = CYLINDRICAL_SURFACE('',#75018,0.1) ;
#7461 = CYLINDRICAL_SURFACE('',#75020,0.1) ;
#7462 = CYLINDRICAL_SURFACE('',#75022,0.0999999999999998) ;
#7463 = CYLINDRICAL_SURFACE('',#75029,0.1) ;
#7464 = CYLINDRICAL_SURFACE('',#75036,0.1) ;
#7465 = CYLINDRICAL_SURFACE('',#75038,0.1) ;
#7466 = CYLINDRICAL_SURFACE('',#75042,0.1) ;
#7467 = CYLINDRICAL_SURFACE('',#75045,0.1) ;
#7468 = CYLINDRICAL_SURFACE('',#75047,0.0999999999999994) ;
#7469 = CYLINDRICAL_SURFACE('',#75050,0.1) ;
#7470 = CYLINDRICAL_SURFACE('',#75057,0.0999999999999994) ;
#7471 = CYLINDRICAL_SURFACE('',#75059,0.0999999999999994) ;
#7472 = CYLINDRICAL_SURFACE('',#75065,0.1) ;
#7473 = CYLINDRICAL_SURFACE('',#75067,0.1) ;
#7474 = CYLINDRICAL_SURFACE('',#75073,0.0999999999999988) ;
#7475 = CYLINDRICAL_SURFACE('',#75081,0.1) ;
#7476 = CYLINDRICAL_SURFACE('',#75082,0.1) ;
#7477 = CYLINDRICAL_SURFACE('',#75086,0.0999999999999989) ;
#7478 = CYLINDRICAL_SURFACE('',#75088,0.0999999999999994) ;
#7479 = CYLINDRICAL_SURFACE('',#75094,0.0999999999999998) ;
#7480 = CYLINDRICAL_SURFACE('',#75096,0.1) ;
#7481 = CYLINDRICAL_SURFACE('',#75102,0.0999999999999994) ;
#7482 = CYLINDRICAL_SURFACE('',#75103,0.1) ;
#7483 = CYLINDRICAL_SURFACE('',#75106,0.1) ;
#7484 = CYLINDRICAL_SURFACE('',#75117,0.1) ;
#7485 = CYLINDRICAL_SURFACE('',#75119,0.1) ;
#7486 = CYLINDRICAL_SURFACE('',#75121,0.1) ;
#7487 = CYLINDRICAL_SURFACE('',#75123,0.1) ;
#7488 = CYLINDRICAL_SURFACE('',#75125,0.1) ;
#7489 = CYLINDRICAL_SURFACE('',#75127,0.1) ;
#7490 = CYLINDRICAL_SURFACE('',#75138,0.1) ;
#7491 = CYLINDRICAL_SURFACE('',#75140,0.0999999999999998) ;
#7492 = CYLINDRICAL_SURFACE('',#75142,0.1) ;
#7493 = CYLINDRICAL_SURFACE('',#75144,0.1) ;
#7494 = CYLINDRICAL_SURFACE('',#75146,0.1) ;
#7495 = CYLINDRICAL_SURFACE('',#75156,0.1) ;
#7496 = CYLINDRICAL_SURFACE('',#75163,0.1) ;
#7497 = CYLINDRICAL_SURFACE('',#75165,0.1) ;
#7498 = CYLINDRICAL_SURFACE('',#75167,0.0999999999999994) ;
#7499 = CYLINDRICAL_SURFACE('',#75171,0.1) ;
#7500 = CYLINDRICAL_SURFACE('',#75173,0.1) ;
#7501 = CYLINDRICAL_SURFACE('',#75175,0.0999999999999998) ;
#7502 = CYLINDRICAL_SURFACE('',#75182,0.1) ;
#7503 = CYLINDRICAL_SURFACE('',#75189,0.1) ;
#7504 = CYLINDRICAL_SURFACE('',#75191,0.1) ;
#7505 = CYLINDRICAL_SURFACE('',#75195,0.1) ;
#7506 = CYLINDRICAL_SURFACE('',#75198,0.1) ;
#7507 = CYLINDRICAL_SURFACE('',#75200,0.100000000000003) ;
#7508 = CYLINDRICAL_SURFACE('',#75203,0.1) ;
#7509 = CYLINDRICAL_SURFACE('',#75210,0.0999999999999994) ;
#7510 = CYLINDRICAL_SURFACE('',#75212,0.100000000000003) ;
#7511 = CYLINDRICAL_SURFACE('',#75218,0.1) ;
#7512 = CYLINDRICAL_SURFACE('',#75220,0.1) ;
#7513 = CYLINDRICAL_SURFACE('',#75226,0.0999999999999988) ;
#7514 = CYLINDRICAL_SURFACE('',#75234,0.1) ;
#7515 = CYLINDRICAL_SURFACE('',#75235,0.1) ;
#7516 = CYLINDRICAL_SURFACE('',#75239,0.0999999999999989) ;
#7517 = CYLINDRICAL_SURFACE('',#75241,0.0999999999999994) ;
#7518 = CYLINDRICAL_SURFACE('',#75247,0.0999999999999998) ;
#7519 = CYLINDRICAL_SURFACE('',#75249,0.1) ;
#7520 = CYLINDRICAL_SURFACE('',#75255,0.0999999999999994) ;
#7521 = CYLINDRICAL_SURFACE('',#75256,0.1) ;
#7522 = CYLINDRICAL_SURFACE('',#75259,0.1) ;
#7523 = CYLINDRICAL_SURFACE('',#75270,0.1) ;
#7524 = CYLINDRICAL_SURFACE('',#75272,0.1) ;
#7525 = CYLINDRICAL_SURFACE('',#75274,0.1) ;
#7526 = CYLINDRICAL_SURFACE('',#75276,0.1) ;
#7527 = CYLINDRICAL_SURFACE('',#75278,0.1) ;
#7528 = CYLINDRICAL_SURFACE('',#75280,0.1) ;
#7529 = CYLINDRICAL_SURFACE('',#75291,0.1) ;
#7530 = CYLINDRICAL_SURFACE('',#75293,0.0999999999999998) ;
#7531 = CYLINDRICAL_SURFACE('',#75295,0.1) ;
#7532 = CYLINDRICAL_SURFACE('',#75297,0.1) ;
#7533 = CYLINDRICAL_SURFACE('',#75299,0.1) ;
#7534 = CYLINDRICAL_SURFACE('',#75309,0.1) ;
#7535 = CYLINDRICAL_SURFACE('',#75316,0.1) ;
#7536 = CYLINDRICAL_SURFACE('',#75318,0.1) ;
#7537 = CYLINDRICAL_SURFACE('',#75320,0.100000000000003) ;
#7538 = CYLINDRICAL_SURFACE('',#75324,0.1) ;
#7539 = CYLINDRICAL_SURFACE('',#75326,0.1) ;
#7540 = CYLINDRICAL_SURFACE('',#75328,0.0999999999999998) ;
#7541 = CYLINDRICAL_SURFACE('',#75335,0.1) ;
#7542 = CYLINDRICAL_SURFACE('',#75342,0.1) ;
#7543 = CYLINDRICAL_SURFACE('',#75344,0.1) ;
#7544 = CYLINDRICAL_SURFACE('',#75348,0.1) ;
#7545 = CYLINDRICAL_SURFACE('',#75351,0.1) ;
#7546 = CYLINDRICAL_SURFACE('',#75353,0.100000000000003) ;
#7547 = CYLINDRICAL_SURFACE('',#75356,0.1) ;
#7548 = CYLINDRICAL_SURFACE('',#75363,0.100000000000003) ;
#7549 = CYLINDRICAL_SURFACE('',#75365,0.100000000000003) ;
#7550 = CYLINDRICAL_SURFACE('',#75371,0.1) ;
#7551 = CYLINDRICAL_SURFACE('',#75373,0.1) ;
#7552 = CYLINDRICAL_SURFACE('',#75379,0.0999999999999988) ;
#7553 = CYLINDRICAL_SURFACE('',#75387,0.1) ;
#7554 = CYLINDRICAL_SURFACE('',#75388,0.1) ;
#7555 = CYLINDRICAL_SURFACE('',#75392,0.0999999999999989) ;
#7556 = CYLINDRICAL_SURFACE('',#75394,0.100000000000003) ;
#7557 = CYLINDRICAL_SURFACE('',#75400,0.0999999999999998) ;
#7558 = CYLINDRICAL_SURFACE('',#75402,0.1) ;
#7559 = CYLINDRICAL_SURFACE('',#75408,0.100000000000003) ;
#7560 = CYLINDRICAL_SURFACE('',#75420,1.) ;
#7561 = CYLINDRICAL_SURFACE('',#75423,0.2) ;
#7562 = CYLINDRICAL_SURFACE('',#75444,1.) ;
#7563 = CYLINDRICAL_SURFACE('',#75447,0.2) ;
#7564 = CYLINDRICAL_SURFACE('',#75468,1.) ;
#7565 = CYLINDRICAL_SURFACE('',#75471,0.2) ;
#7566 = CYLINDRICAL_SURFACE('',#75492,1.) ;
#7567 = CYLINDRICAL_SURFACE('',#75495,0.2) ;
#7568 = CYLINDRICAL_SURFACE('',#75516,1.) ;
#7569 = CYLINDRICAL_SURFACE('',#75519,0.2) ;
#7570 = CYLINDRICAL_SURFACE('',#75540,1.) ;
#7571 = CYLINDRICAL_SURFACE('',#75543,0.2) ;
#7572 = CYLINDRICAL_SURFACE('',#75564,1.) ;
#7573 = CYLINDRICAL_SURFACE('',#75567,0.2) ;
#7574 = CYLINDRICAL_SURFACE('',#75588,1.) ;
#7575 = CYLINDRICAL_SURFACE('',#75591,0.2) ;
#7576 = CYLINDRICAL_SURFACE('',#75612,1.) ;
#7577 = CYLINDRICAL_SURFACE('',#75615,0.2) ;
#7578 = CYLINDRICAL_SURFACE('',#75661,0.0999999999999999) ;
#7579 = CYLINDRICAL_SURFACE('',#75664,0.1) ;
#7580 = CYLINDRICAL_SURFACE('',#75670,0.0999999999999999) ;
#7581 = CYLINDRICAL_SURFACE('',#75673,0.1) ;
#7582 = CYLINDRICAL_SURFACE('',#75675,0.0999999999999998) ;
#7583 = CYLINDRICAL_SURFACE('',#75682,0.0999999999999998) ;
#7584 = CYLINDRICAL_SURFACE('',#75684,0.1) ;
#7585 = CYLINDRICAL_SURFACE('',#75686,0.1) ;
#7586 = CYLINDRICAL_SURFACE('',#75690,0.1) ;
#7587 = CYLINDRICAL_SURFACE('',#75693,0.0999999999999999) ;
#7588 = CYLINDRICAL_SURFACE('',#75695,0.1) ;
#7589 = CYLINDRICAL_SURFACE('',#75698,0.1) ;
#7590 = CYLINDRICAL_SURFACE('',#75704,0.1) ;
#7591 = CYLINDRICAL_SURFACE('',#75707,0.1) ;
#7592 = CYLINDRICAL_SURFACE('',#75709,0.0999999999999998) ;
#7593 = CYLINDRICAL_SURFACE('',#75716,0.0999999999999998) ;
#7594 = CYLINDRICAL_SURFACE('',#75718,0.1) ;
#7595 = CYLINDRICAL_SURFACE('',#75720,0.1) ;
#7596 = CYLINDRICAL_SURFACE('',#75724,0.1) ;
#7597 = CYLINDRICAL_SURFACE('',#75727,0.1) ;
#7598 = CYLINDRICAL_SURFACE('',#75729,0.1) ;
#7599 = CYLINDRICAL_SURFACE('',#75732,0.1) ;
#7600 = CYLINDRICAL_SURFACE('',#75738,0.1) ;
#7601 = CYLINDRICAL_SURFACE('',#75741,0.1) ;
#7602 = CYLINDRICAL_SURFACE('',#75743,0.1) ;
#7603 = CYLINDRICAL_SURFACE('',#75750,0.1) ;
#7604 = CYLINDRICAL_SURFACE('',#75752,0.1) ;
#7605 = CYLINDRICAL_SURFACE('',#75754,0.1) ;
#7606 = CYLINDRICAL_SURFACE('',#75758,0.1) ;
#7607 = CYLINDRICAL_SURFACE('',#75761,0.1) ;
#7608 = CYLINDRICAL_SURFACE('',#75763,0.1) ;
#7609 = CYLINDRICAL_SURFACE('',#75766,0.1) ;
#7610 = CYLINDRICAL_SURFACE('',#75772,0.1) ;
#7611 = CYLINDRICAL_SURFACE('',#75775,0.1) ;
#7612 = CYLINDRICAL_SURFACE('',#75777,0.1) ;
#7613 = CYLINDRICAL_SURFACE('',#75784,0.1) ;
#7614 = CYLINDRICAL_SURFACE('',#75786,0.1) ;
#7615 = CYLINDRICAL_SURFACE('',#75788,0.1) ;
#7616 = CYLINDRICAL_SURFACE('',#75792,0.1) ;
#7617 = CYLINDRICAL_SURFACE('',#75795,0.1) ;
#7618 = CYLINDRICAL_SURFACE('',#75797,0.1) ;
#7619 = CYLINDRICAL_SURFACE('',#75800,0.1) ;
#7620 = CYLINDRICAL_SURFACE('',#75806,0.1) ;
#7621 = CYLINDRICAL_SURFACE('',#75809,0.1) ;
#7622 = CYLINDRICAL_SURFACE('',#75811,0.0999999999999994) ;
#7623 = CYLINDRICAL_SURFACE('',#75818,0.0999999999999994) ;
#7624 = CYLINDRICAL_SURFACE('',#75820,0.1) ;
#7625 = CYLINDRICAL_SURFACE('',#75822,0.1) ;
#7626 = CYLINDRICAL_SURFACE('',#75826,0.1) ;
#7627 = CYLINDRICAL_SURFACE('',#75829,0.1) ;
#7628 = CYLINDRICAL_SURFACE('',#75831,0.1) ;
#7629 = CYLINDRICAL_SURFACE('',#75834,0.1) ;
#7630 = CYLINDRICAL_SURFACE('',#75840,0.1) ;
#7631 = CYLINDRICAL_SURFACE('',#75843,0.1) ;
#7632 = CYLINDRICAL_SURFACE('',#75845,0.0999999999999994) ;
#7633 = CYLINDRICAL_SURFACE('',#75852,0.0999999999999994) ;
#7634 = CYLINDRICAL_SURFACE('',#75854,0.1) ;
#7635 = CYLINDRICAL_SURFACE('',#75856,0.1) ;
#7636 = CYLINDRICAL_SURFACE('',#75860,0.1) ;
#7637 = CYLINDRICAL_SURFACE('',#75863,0.1) ;
#7638 = CYLINDRICAL_SURFACE('',#75865,0.1) ;
#7639 = CYLINDRICAL_SURFACE('',#75868,0.1) ;
#7640 = CYLINDRICAL_SURFACE('',#75874,0.1) ;
#7641 = CYLINDRICAL_SURFACE('',#75877,0.1) ;
#7642 = CYLINDRICAL_SURFACE('',#75879,0.0999999999999994) ;
#7643 = CYLINDRICAL_SURFACE('',#75886,0.0999999999999994) ;
#7644 = CYLINDRICAL_SURFACE('',#75888,0.1) ;
#7645 = CYLINDRICAL_SURFACE('',#75890,0.1) ;
#7646 = CYLINDRICAL_SURFACE('',#75894,0.1) ;
#7647 = CYLINDRICAL_SURFACE('',#75897,0.1) ;
#7648 = CYLINDRICAL_SURFACE('',#75899,0.1) ;
#7649 = CYLINDRICAL_SURFACE('',#75902,0.1) ;
#7650 = CYLINDRICAL_SURFACE('',#75908,0.1) ;
#7651 = CYLINDRICAL_SURFACE('',#75911,0.1) ;
#7652 = CYLINDRICAL_SURFACE('',#75913,0.0999999999999994) ;
#7653 = CYLINDRICAL_SURFACE('',#75920,0.0999999999999994) ;
#7654 = CYLINDRICAL_SURFACE('',#75922,0.1) ;
#7655 = CYLINDRICAL_SURFACE('',#75924,0.1) ;
#7656 = CYLINDRICAL_SURFACE('',#75928,0.1) ;
#7657 = CYLINDRICAL_SURFACE('',#75931,0.1) ;
#7658 = CYLINDRICAL_SURFACE('',#75933,0.099999999999999) ;
#7659 = CYLINDRICAL_SURFACE('',#75936,0.1) ;
#7660 = CYLINDRICAL_SURFACE('',#75942,0.099999999999999) ;
#7661 = CYLINDRICAL_SURFACE('',#75945,0.1) ;
#7662 = CYLINDRICAL_SURFACE('',#75947,0.0999999999999994) ;
#7663 = CYLINDRICAL_SURFACE('',#75954,0.0999999999999994) ;
#7664 = CYLINDRICAL_SURFACE('',#75956,0.1) ;
#7665 = CYLINDRICAL_SURFACE('',#75958,0.099999999999999) ;
#7666 = CYLINDRICAL_SURFACE('',#75962,0.1) ;
#7667 = CYLINDRICAL_SURFACE('',#75965,0.099999999999999) ;
#7668 = CYLINDRICAL_SURFACE('',#75967,0.0999999999999989) ;
#7669 = CYLINDRICAL_SURFACE('',#75970,0.1) ;
#7670 = CYLINDRICAL_SURFACE('',#75976,0.0999999999999989) ;
#7671 = CYLINDRICAL_SURFACE('',#75979,0.1) ;
#7672 = CYLINDRICAL_SURFACE('',#75981,0.0999999999999994) ;
#7673 = CYLINDRICAL_SURFACE('',#75988,0.0999999999999994) ;
#7674 = CYLINDRICAL_SURFACE('',#75990,0.1) ;
#7675 = CYLINDRICAL_SURFACE('',#75992,0.0999999999999989) ;
#7676 = CYLINDRICAL_SURFACE('',#75996,0.1) ;
#7677 = CYLINDRICAL_SURFACE('',#75999,0.0999999999999989) ;
#7678 = CYLINDRICAL_SURFACE('',#76001,0.099999999999999) ;
#7679 = CYLINDRICAL_SURFACE('',#76004,0.1) ;
#7680 = CYLINDRICAL_SURFACE('',#76010,0.099999999999999) ;
#7681 = CYLINDRICAL_SURFACE('',#76013,0.1) ;
#7682 = CYLINDRICAL_SURFACE('',#76015,0.0999999999999994) ;
#7683 = CYLINDRICAL_SURFACE('',#76022,0.0999999999999994) ;
#7684 = CYLINDRICAL_SURFACE('',#76024,0.1) ;
#7685 = CYLINDRICAL_SURFACE('',#76026,0.099999999999999) ;
#7686 = CYLINDRICAL_SURFACE('',#76030,0.1) ;
#7687 = CYLINDRICAL_SURFACE('',#76033,0.099999999999999) ;
#7688 = CYLINDRICAL_SURFACE('',#76035,0.0999999999999989) ;
#7689 = CYLINDRICAL_SURFACE('',#76038,0.1) ;
#7690 = CYLINDRICAL_SURFACE('',#76044,0.0999999999999989) ;
#7691 = CYLINDRICAL_SURFACE('',#76047,0.1) ;
#7692 = CYLINDRICAL_SURFACE('',#76049,0.0999999999999994) ;
#7693 = CYLINDRICAL_SURFACE('',#76056,0.0999999999999994) ;
#7694 = CYLINDRICAL_SURFACE('',#76058,0.1) ;
#7695 = CYLINDRICAL_SURFACE('',#76060,0.0999999999999989) ;
#7696 = CYLINDRICAL_SURFACE('',#76064,0.1) ;
#7697 = CYLINDRICAL_SURFACE('',#76067,0.0999999999999989) ;
#7698 = CYLINDRICAL_SURFACE('',#76069,0.099999999999999) ;
#7699 = CYLINDRICAL_SURFACE('',#76072,0.1) ;
#7700 = CYLINDRICAL_SURFACE('',#76078,0.099999999999999) ;
#7701 = CYLINDRICAL_SURFACE('',#76081,0.1) ;
#7702 = CYLINDRICAL_SURFACE('',#76083,0.0999999999999994) ;
#7703 = CYLINDRICAL_SURFACE('',#76090,0.0999999999999994) ;
#7704 = CYLINDRICAL_SURFACE('',#76092,0.1) ;
#7705 = CYLINDRICAL_SURFACE('',#76094,0.099999999999999) ;
#7706 = CYLINDRICAL_SURFACE('',#76098,0.1) ;
#7707 = CYLINDRICAL_SURFACE('',#76101,0.099999999999999) ;
#7708 = CYLINDRICAL_SURFACE('',#76103,0.0999999999999989) ;
#7709 = CYLINDRICAL_SURFACE('',#76106,0.1) ;
#7710 = CYLINDRICAL_SURFACE('',#76112,0.0999999999999989) ;
#7711 = CYLINDRICAL_SURFACE('',#76115,0.1) ;
#7712 = CYLINDRICAL_SURFACE('',#76117,0.0999999999999994) ;
#7713 = CYLINDRICAL_SURFACE('',#76124,0.0999999999999994) ;
#7714 = CYLINDRICAL_SURFACE('',#76126,0.1) ;
#7715 = CYLINDRICAL_SURFACE('',#76128,0.0999999999999989) ;
#7716 = CYLINDRICAL_SURFACE('',#76132,0.1) ;
#7717 = CYLINDRICAL_SURFACE('',#76135,0.0999999999999989) ;
#7718 = CYLINDRICAL_SURFACE('',#76137,0.099999999999999) ;
#7719 = CYLINDRICAL_SURFACE('',#76140,0.1) ;
#7720 = CYLINDRICAL_SURFACE('',#76146,0.099999999999999) ;
#7721 = CYLINDRICAL_SURFACE('',#76149,0.1) ;
#7722 = CYLINDRICAL_SURFACE('',#76151,0.0999999999999994) ;
#7723 = CYLINDRICAL_SURFACE('',#76158,0.0999999999999994) ;
#7724 = CYLINDRICAL_SURFACE('',#76160,0.1) ;
#7725 = CYLINDRICAL_SURFACE('',#76162,0.099999999999999) ;
#7726 = CYLINDRICAL_SURFACE('',#76166,0.1) ;
#7727 = CYLINDRICAL_SURFACE('',#76169,0.099999999999999) ;
#7728 = CYLINDRICAL_SURFACE('',#76171,0.0999999999999989) ;
#7729 = CYLINDRICAL_SURFACE('',#76174,0.1) ;
#7730 = CYLINDRICAL_SURFACE('',#76180,0.0999999999999989) ;
#7731 = CYLINDRICAL_SURFACE('',#76183,0.1) ;
#7732 = CYLINDRICAL_SURFACE('',#76185,0.0999999999999994) ;
#7733 = CYLINDRICAL_SURFACE('',#76192,0.0999999999999994) ;
#7734 = CYLINDRICAL_SURFACE('',#76194,0.1) ;
#7735 = CYLINDRICAL_SURFACE('',#76196,0.0999999999999989) ;
#7736 = CYLINDRICAL_SURFACE('',#76200,0.1) ;
#7737 = CYLINDRICAL_SURFACE('',#76203,0.0999999999999989) ;
#7738 = CYLINDRICAL_SURFACE('',#76205,0.099999999999999) ;
#7739 = CYLINDRICAL_SURFACE('',#76208,0.1) ;
#7740 = CYLINDRICAL_SURFACE('',#76214,0.099999999999999) ;
#7741 = CYLINDRICAL_SURFACE('',#76217,0.1) ;
#7742 = CYLINDRICAL_SURFACE('',#76219,0.100000000000003) ;
#7743 = CYLINDRICAL_SURFACE('',#76226,0.100000000000003) ;
#7744 = CYLINDRICAL_SURFACE('',#76228,0.1) ;
#7745 = CYLINDRICAL_SURFACE('',#76230,0.099999999999999) ;
#7746 = CYLINDRICAL_SURFACE('',#76234,0.1) ;
#7747 = CYLINDRICAL_SURFACE('',#76237,0.099999999999999) ;
#7748 = CYLINDRICAL_SURFACE('',#76239,0.0999999999999989) ;
#7749 = CYLINDRICAL_SURFACE('',#76242,0.1) ;
#7750 = CYLINDRICAL_SURFACE('',#76248,0.0999999999999989) ;
#7751 = CYLINDRICAL_SURFACE('',#76251,0.1) ;
#7752 = CYLINDRICAL_SURFACE('',#76253,0.100000000000003) ;
#7753 = CYLINDRICAL_SURFACE('',#76260,0.100000000000003) ;
#7754 = CYLINDRICAL_SURFACE('',#76262,0.1) ;
#7755 = CYLINDRICAL_SURFACE('',#76264,0.0999999999999989) ;
#7756 = CYLINDRICAL_SURFACE('',#76268,0.1) ;
#7757 = CYLINDRICAL_SURFACE('',#76271,0.0999999999999989) ;
#7758 = CYLINDRICAL_SURFACE('',#76275,0.1) ;
#7759 = CYLINDRICAL_SURFACE('',#76279,0.1) ;
#7760 = CYLINDRICAL_SURFACE('',#76283,0.1) ;
#7761 = CYLINDRICAL_SURFACE('',#76288,0.1) ;
#7762 = CYLINDRICAL_SURFACE('',#76292,0.1) ;
#7763 = CYLINDRICAL_SURFACE('',#76296,0.1) ;
#7764 = CYLINDRICAL_SURFACE('',#76299,0.1) ;
#7765 = CYLINDRICAL_SURFACE('',#76303,0.1) ;
#7766 = CYLINDRICAL_SURFACE('',#76307,0.1) ;
#7767 = CYLINDRICAL_SURFACE('',#76308,0.1) ;
#7768 = CYLINDRICAL_SURFACE('',#76312,0.1) ;
#7769 = CYLINDRICAL_SURFACE('',#76314,0.1) ;
#7770 = CYLINDRICAL_SURFACE('',#76319,0.1) ;
#7771 = CYLINDRICAL_SURFACE('',#76323,0.1) ;
#7772 = CYLINDRICAL_SURFACE('',#76327,0.1) ;
#7773 = CYLINDRICAL_SURFACE('',#76332,0.1) ;
#7774 = CYLINDRICAL_SURFACE('',#76336,0.1) ;
#7775 = CYLINDRICAL_SURFACE('',#76340,0.1) ;
#7776 = CYLINDRICAL_SURFACE('',#76343,0.1) ;
#7777 = CYLINDRICAL_SURFACE('',#76347,0.1) ;
#7778 = CYLINDRICAL_SURFACE('',#76351,0.1) ;
#7779 = CYLINDRICAL_SURFACE('',#76352,0.1) ;
#7780 = CYLINDRICAL_SURFACE('',#76356,0.1) ;
#7781 = CYLINDRICAL_SURFACE('',#76358,0.1) ;
#7782 = CYLINDRICAL_SURFACE('',#76363,0.1) ;
#7783 = CYLINDRICAL_SURFACE('',#76367,0.1) ;
#7784 = CYLINDRICAL_SURFACE('',#76371,0.1) ;
#7785 = CYLINDRICAL_SURFACE('',#76376,0.1) ;
#7786 = CYLINDRICAL_SURFACE('',#76380,0.1) ;
#7787 = CYLINDRICAL_SURFACE('',#76384,0.1) ;
#7788 = CYLINDRICAL_SURFACE('',#76387,0.1) ;
#7789 = CYLINDRICAL_SURFACE('',#76391,0.1) ;
#7790 = CYLINDRICAL_SURFACE('',#76395,0.1) ;
#7791 = CYLINDRICAL_SURFACE('',#76396,0.1) ;
#7792 = CYLINDRICAL_SURFACE('',#76400,0.1) ;
#7793 = CYLINDRICAL_SURFACE('',#76402,0.1) ;
#7794 = CYLINDRICAL_SURFACE('',#76407,0.1) ;
#7795 = CYLINDRICAL_SURFACE('',#76411,0.1) ;
#7796 = CYLINDRICAL_SURFACE('',#76415,0.1) ;
#7797 = CYLINDRICAL_SURFACE('',#76420,0.1) ;
#7798 = CYLINDRICAL_SURFACE('',#76424,0.1) ;
#7799 = CYLINDRICAL_SURFACE('',#76428,0.1) ;
#7800 = CYLINDRICAL_SURFACE('',#76431,0.1) ;
#7801 = CYLINDRICAL_SURFACE('',#76435,0.1) ;
#7802 = CYLINDRICAL_SURFACE('',#76439,0.1) ;
#7803 = CYLINDRICAL_SURFACE('',#76440,0.1) ;
#7804 = CYLINDRICAL_SURFACE('',#76444,0.1) ;
#7805 = CYLINDRICAL_SURFACE('',#76446,0.1) ;
#7806 = CYLINDRICAL_SURFACE('',#76451,0.1) ;
#7807 = CYLINDRICAL_SURFACE('',#76455,0.1) ;
#7808 = CYLINDRICAL_SURFACE('',#76459,0.1) ;
#7809 = CYLINDRICAL_SURFACE('',#76464,0.1) ;
#7810 = CYLINDRICAL_SURFACE('',#76468,0.1) ;
#7811 = CYLINDRICAL_SURFACE('',#76472,0.1) ;
#7812 = CYLINDRICAL_SURFACE('',#76475,0.1) ;
#7813 = CYLINDRICAL_SURFACE('',#76479,0.1) ;
#7814 = CYLINDRICAL_SURFACE('',#76483,0.1) ;
#7815 = CYLINDRICAL_SURFACE('',#76484,0.1) ;
#7816 = CYLINDRICAL_SURFACE('',#76488,0.1) ;
#7817 = CYLINDRICAL_SURFACE('',#76490,0.1) ;
#7818 = CYLINDRICAL_SURFACE('',#76495,0.1) ;
#7819 = CYLINDRICAL_SURFACE('',#76499,0.1) ;
#7820 = CYLINDRICAL_SURFACE('',#76503,0.1) ;
#7821 = CYLINDRICAL_SURFACE('',#76508,0.1) ;
#7822 = CYLINDRICAL_SURFACE('',#76512,0.1) ;
#7823 = CYLINDRICAL_SURFACE('',#76516,0.1) ;
#7824 = CYLINDRICAL_SURFACE('',#76519,0.1) ;
#7825 = CYLINDRICAL_SURFACE('',#76523,0.1) ;
#7826 = CYLINDRICAL_SURFACE('',#76527,0.1) ;
#7827 = CYLINDRICAL_SURFACE('',#76528,0.1) ;
#7828 = CYLINDRICAL_SURFACE('',#76532,0.1) ;
#7829 = CYLINDRICAL_SURFACE('',#76534,0.1) ;
#7830 = CYLINDRICAL_SURFACE('',#76539,0.1) ;
#7831 = CYLINDRICAL_SURFACE('',#76543,0.1) ;
#7832 = CYLINDRICAL_SURFACE('',#76547,0.1) ;
#7833 = CYLINDRICAL_SURFACE('',#76552,0.1) ;
#7834 = CYLINDRICAL_SURFACE('',#76556,0.1) ;
#7835 = CYLINDRICAL_SURFACE('',#76560,0.1) ;
#7836 = CYLINDRICAL_SURFACE('',#76563,0.1) ;
#7837 = CYLINDRICAL_SURFACE('',#76567,0.1) ;
#7838 = CYLINDRICAL_SURFACE('',#76571,0.1) ;
#7839 = CYLINDRICAL_SURFACE('',#76572,0.1) ;
#7840 = CYLINDRICAL_SURFACE('',#76576,0.1) ;
#7841 = CYLINDRICAL_SURFACE('',#76578,0.1) ;
#7842 = CYLINDRICAL_SURFACE('',#76583,0.1) ;
#7843 = CYLINDRICAL_SURFACE('',#76587,0.1) ;
#7844 = CYLINDRICAL_SURFACE('',#76591,0.1) ;
#7845 = CYLINDRICAL_SURFACE('',#76596,0.1) ;
#7846 = CYLINDRICAL_SURFACE('',#76600,0.1) ;
#7847 = CYLINDRICAL_SURFACE('',#76604,0.1) ;
#7848 = CYLINDRICAL_SURFACE('',#76607,0.1) ;
#7849 = CYLINDRICAL_SURFACE('',#76611,0.1) ;
#7850 = CYLINDRICAL_SURFACE('',#76615,0.1) ;
#7851 = CYLINDRICAL_SURFACE('',#76616,0.1) ;
#7852 = CYLINDRICAL_SURFACE('',#76620,0.1) ;
#7853 = CYLINDRICAL_SURFACE('',#76622,0.1) ;
#7854 = CYLINDRICAL_SURFACE('',#76627,0.1) ;
#7855 = CYLINDRICAL_SURFACE('',#76631,0.1) ;
#7856 = CYLINDRICAL_SURFACE('',#76635,0.1) ;
#7857 = CYLINDRICAL_SURFACE('',#76640,0.1) ;
#7858 = CYLINDRICAL_SURFACE('',#76644,0.1) ;
#7859 = CYLINDRICAL_SURFACE('',#76648,0.1) ;
#7860 = CYLINDRICAL_SURFACE('',#76651,0.1) ;
#7861 = CYLINDRICAL_SURFACE('',#76655,0.1) ;
#7862 = CYLINDRICAL_SURFACE('',#76659,0.1) ;
#7863 = CYLINDRICAL_SURFACE('',#76660,0.1) ;
#7864 = CYLINDRICAL_SURFACE('',#76664,0.1) ;
#7865 = CYLINDRICAL_SURFACE('',#76666,0.1) ;
#7866 = CYLINDRICAL_SURFACE('',#76670,1.2293670625) ;
#7867 = CYLINDRICAL_SURFACE('',#76671,1.2293670625) ;
#7868 = CYLINDRICAL_SURFACE('',#76672,1.2293670625) ;
#7869 = CYLINDRICAL_SURFACE('',#76673,1.2293670625) ;
#7870 = CYLINDRICAL_SURFACE('',#76674,1.2293670625) ;
#7871 = CYLINDRICAL_SURFACE('',#76675,1.2293670625) ;
#7872 = CYLINDRICAL_SURFACE('',#76676,1.2293670625) ;
#7873 = CYLINDRICAL_SURFACE('',#76677,1.2293670625) ;
#7874 = CYLINDRICAL_SURFACE('',#76678,1.2293670625) ;
#7875 = CYLINDRICAL_SURFACE('',#76679,1.2293670625) ;
#7876 = CYLINDRICAL_SURFACE('',#76680,1.5) ;
#7877 = CYLINDRICAL_SURFACE('',#76682,1.5) ;
#7878 = CYLINDRICAL_SURFACE('',#76683,1.5) ;
#7879 = CYLINDRICAL_SURFACE('',#76684,1.5) ;
#7880 = CYLINDRICAL_SURFACE('',#76685,1.5) ;
#7881 = CYLINDRICAL_SURFACE('',#76686,1.5) ;
#7882 = CYLINDRICAL_SURFACE('',#76687,1.5) ;
#7883 = CYLINDRICAL_SURFACE('',#76688,1.5) ;
#7884 = CYLINDRICAL_SURFACE('',#76689,1.5) ;
#7885 = CYLINDRICAL_SURFACE('',#76693,1.5) ;
#7886 = CYLINDRICAL_SURFACE('',#76694,1.2293670625) ;
#7887 = CYLINDRICAL_SURFACE('',#76699,1.25) ;
#7888 = CYLINDRICAL_SURFACE('',#76707,2.49807621135332) ;
#7889 = CYLINDRICAL_SURFACE('',#76710,2.49807621135332) ;
#7890 = CYLINDRICAL_SURFACE('',#76713,2.49807621135332) ;
#7891 = CYLINDRICAL_SURFACE('',#76716,2.49807621135332) ;
#7892 = CYLINDRICAL_SURFACE('',#76719,2.49807621135332) ;
#7893 = CYLINDRICAL_SURFACE('',#76722,2.49807621135332) ;
#7894 = CYLINDRICAL_SURFACE('',#76791,2.8) ;
#7895 = CYLINDRICAL_SURFACE('',#76793,1.5) ;
#7896 = LINE('',#99198,#12012) ;
#7897 = LINE('',#99201,#12013) ;
#7898 = LINE('',#99204,#12014) ;
#7899 = LINE('',#99207,#12015) ;
#7900 = LINE('',#99209,#12016) ;
#7901 = LINE('',#99213,#12017) ;
#7902 = LINE('',#99215,#12018) ;
#7903 = LINE('',#99217,#12019) ;
#7904 = LINE('',#99219,#12020) ;
#7905 = LINE('',#99221,#12021) ;
#7906 = LINE('',#99222,#12022) ;
#7907 = LINE('',#99227,#12023) ;
#7908 = LINE('',#99231,#12024) ;
#7909 = LINE('',#99235,#12025) ;
#7910 = LINE('',#99238,#12026) ;
#7911 = LINE('',#99242,#12027) ;
#7912 = LINE('',#99244,#12028) ;
#7913 = LINE('',#99246,#12029) ;
#7914 = LINE('',#99248,#12030) ;
#7915 = LINE('',#99250,#12031) ;
#7916 = LINE('',#99251,#12032) ;
#7917 = LINE('',#99256,#12033) ;
#7918 = LINE('',#99260,#12034) ;
#7919 = LINE('',#99264,#12035) ;
#7920 = LINE('',#99267,#12036) ;
#7921 = LINE('',#99273,#12037) ;
#7922 = LINE('',#99275,#12038) ;
#7923 = LINE('',#99277,#12039) ;
#7924 = LINE('',#99279,#12040) ;
#7925 = LINE('',#99281,#12041) ;
#7926 = LINE('',#99283,#12042) ;
#7927 = LINE('',#99287,#12043) ;
#7928 = LINE('',#99289,#12044) ;
#7929 = LINE('',#99290,#12045) ;
#7930 = LINE('',#99295,#12046) ;
#7931 = LINE('',#99299,#12047) ;
#7932 = LINE('',#99303,#12048) ;
#7933 = LINE('',#99306,#12049) ;
#7934 = LINE('',#99311,#12050) ;
#7935 = LINE('',#99315,#12051) ;
#7936 = LINE('',#99319,#12052) ;
#7937 = LINE('',#99322,#12053) ;
#7938 = LINE('',#99327,#12054) ;
#7939 = LINE('',#99331,#12055) ;
#7940 = LINE('',#99335,#12056) ;
#7941 = LINE('',#99338,#12057) ;
#7942 = LINE('',#99343,#12058) ;
#7943 = LINE('',#99347,#12059) ;
#7944 = LINE('',#99351,#12060) ;
#7945 = LINE('',#99354,#12061) ;
#7946 = LINE('',#99358,#12062) ;
#7947 = LINE('',#99360,#12063) ;
#7948 = LINE('',#99364,#12064) ;
#7949 = LINE('',#99366,#12065) ;
#7950 = LINE('',#99368,#12066) ;
#7951 = LINE('',#99372,#12067) ;
#7952 = LINE('',#99374,#12068) ;
#7953 = LINE('',#99376,#12069) ;
#7954 = LINE('',#99377,#12070) ;
#7955 = LINE('',#99382,#12071) ;
#7956 = LINE('',#99386,#12072) ;
#7957 = LINE('',#99390,#12073) ;
#7958 = LINE('',#99393,#12074) ;
#7959 = LINE('',#99398,#12075) ;
#7960 = LINE('',#99402,#12076) ;
#7961 = LINE('',#99406,#12077) ;
#7962 = LINE('',#99409,#12078) ;
#7963 = LINE('',#99414,#12079) ;
#7964 = LINE('',#99418,#12080) ;
#7965 = LINE('',#99422,#12081) ;
#7966 = LINE('',#99425,#12082) ;
#7967 = LINE('',#99430,#12083) ;
#7968 = LINE('',#99434,#12084) ;
#7969 = LINE('',#99438,#12085) ;
#7970 = LINE('',#99441,#12086) ;
#7971 = LINE('',#99445,#12087) ;
#7972 = LINE('',#99447,#12088) ;
#7973 = LINE('',#99451,#12089) ;
#7974 = LINE('',#99453,#12090) ;
#7975 = LINE('',#99455,#12091) ;
#7976 = LINE('',#99459,#12092) ;
#7977 = LINE('',#99461,#12093) ;
#7978 = LINE('',#99463,#12094) ;
#7979 = LINE('',#99464,#12095) ;
#7980 = LINE('',#99469,#12096) ;
#7981 = LINE('',#99473,#12097) ;
#7982 = LINE('',#99477,#12098) ;
#7983 = LINE('',#99480,#12099) ;
#7984 = LINE('',#99485,#12100) ;
#7985 = LINE('',#99489,#12101) ;
#7986 = LINE('',#99493,#12102) ;
#7987 = LINE('',#99496,#12103) ;
#7988 = LINE('',#99501,#12104) ;
#7989 = LINE('',#99505,#12105) ;
#7990 = LINE('',#99509,#12106) ;
#7991 = LINE('',#99512,#12107) ;
#7992 = LINE('',#99517,#12108) ;
#7993 = LINE('',#99521,#12109) ;
#7994 = LINE('',#99525,#12110) ;
#7995 = LINE('',#99528,#12111) ;
#7996 = LINE('',#99533,#12112) ;
#7997 = LINE('',#99537,#12113) ;
#7998 = LINE('',#99541,#12114) ;
#7999 = LINE('',#99544,#12115) ;
#8000 = LINE('',#99549,#12116) ;
#8001 = LINE('',#99553,#12117) ;
#8002 = LINE('',#99557,#12118) ;
#8003 = LINE('',#99560,#12119) ;
#8004 = LINE('',#99565,#12120) ;
#8005 = LINE('',#99569,#12121) ;
#8006 = LINE('',#99573,#12122) ;
#8007 = LINE('',#99576,#12123) ;
#8008 = LINE('',#99582,#12124) ;
#8009 = LINE('',#99584,#12125) ;
#8010 = LINE('',#99586,#12126) ;
#8011 = LINE('',#99588,#12127) ;
#8012 = LINE('',#99590,#12128) ;
#8013 = LINE('',#99592,#12129) ;
#8014 = LINE('',#99596,#12130) ;
#8015 = LINE('',#99598,#12131) ;
#8016 = LINE('',#99599,#12132) ;
#8017 = LINE('',#99604,#12133) ;
#8018 = LINE('',#99608,#12134) ;
#8019 = LINE('',#99612,#12135) ;
#8020 = LINE('',#99615,#12136) ;
#8021 = LINE('',#99620,#12137) ;
#8022 = LINE('',#99624,#12138) ;
#8023 = LINE('',#99628,#12139) ;
#8024 = LINE('',#99631,#12140) ;
#8025 = LINE('',#99636,#12141) ;
#8026 = LINE('',#99640,#12142) ;
#8027 = LINE('',#99644,#12143) ;
#8028 = LINE('',#99647,#12144) ;
#8029 = LINE('',#99652,#12145) ;
#8030 = LINE('',#99656,#12146) ;
#8031 = LINE('',#99660,#12147) ;
#8032 = LINE('',#99663,#12148) ;
#8033 = LINE('',#99668,#12149) ;
#8034 = LINE('',#99672,#12150) ;
#8035 = LINE('',#99676,#12151) ;
#8036 = LINE('',#99679,#12152) ;
#8037 = LINE('',#99684,#12153) ;
#8038 = LINE('',#99688,#12154) ;
#8039 = LINE('',#99692,#12155) ;
#8040 = LINE('',#99695,#12156) ;
#8041 = LINE('',#99700,#12157) ;
#8042 = LINE('',#99704,#12158) ;
#8043 = LINE('',#99708,#12159) ;
#8044 = LINE('',#99711,#12160) ;
#8045 = LINE('',#99717,#12161) ;
#8046 = LINE('',#99719,#12162) ;
#8047 = LINE('',#99721,#12163) ;
#8048 = LINE('',#99723,#12164) ;
#8049 = LINE('',#99725,#12165) ;
#8050 = LINE('',#99729,#12166) ;
#8051 = LINE('',#99731,#12167) ;
#8052 = LINE('',#99732,#12168) ;
#8053 = LINE('',#99736,#12169) ;
#8054 = LINE('',#99738,#12170) ;
#8055 = LINE('',#99742,#12171) ;
#8056 = LINE('',#99744,#12172) ;
#8057 = LINE('',#99746,#12173) ;
#8058 = LINE('',#99750,#12174) ;
#8059 = LINE('',#99752,#12175) ;
#8060 = LINE('',#99753,#12176) ;
#8061 = LINE('',#99757,#12177) ;
#8062 = LINE('',#99759,#12178) ;
#8063 = LINE('',#99761,#12179) ;
#8064 = LINE('',#99762,#12180) ;
#8065 = LINE('',#99766,#12181) ;
#8066 = LINE('',#99768,#12182) ;
#8067 = LINE('',#99770,#12183) ;
#8068 = LINE('',#99771,#12184) ;
#8069 = LINE('',#99775,#12185) ;
#8070 = LINE('',#99777,#12186) ;
#8071 = LINE('',#99779,#12187) ;
#8072 = LINE('',#99780,#12188) ;
#8073 = LINE('',#99784,#12189) ;
#8074 = LINE('',#99786,#12190) ;
#8075 = LINE('',#99788,#12191) ;
#8076 = LINE('',#99789,#12192) ;
#8077 = LINE('',#99793,#12193) ;
#8078 = LINE('',#99795,#12194) ;
#8079 = LINE('',#99797,#12195) ;
#8080 = LINE('',#99798,#12196) ;
#8081 = LINE('',#99803,#12197) ;
#8082 = LINE('',#99807,#12198) ;
#8083 = LINE('',#99809,#12199) ;
#8084 = LINE('',#99817,#12200) ;
#8085 = LINE('',#99819,#12201) ;
#8086 = LINE('',#99821,#12202) ;
#8087 = LINE('',#99822,#12203) ;
#8088 = LINE('',#99826,#12204) ;
#8089 = LINE('',#99828,#12205) ;
#8090 = LINE('',#99830,#12206) ;
#8091 = LINE('',#99831,#12207) ;
#8092 = LINE('',#99835,#12208) ;
#8093 = LINE('',#99837,#12209) ;
#8094 = LINE('',#99839,#12210) ;
#8095 = LINE('',#99840,#12211) ;
#8096 = LINE('',#99844,#12212) ;
#8097 = LINE('',#99846,#12213) ;
#8098 = LINE('',#99848,#12214) ;
#8099 = LINE('',#99849,#12215) ;
#8100 = LINE('',#99853,#12216) ;
#8101 = LINE('',#99855,#12217) ;
#8102 = LINE('',#99857,#12218) ;
#8103 = LINE('',#99858,#12219) ;
#8104 = LINE('',#99862,#12220) ;
#8105 = LINE('',#99864,#12221) ;
#8106 = LINE('',#99866,#12222) ;
#8107 = LINE('',#99867,#12223) ;
#8108 = LINE('',#99870,#12224) ;
#8109 = LINE('',#99872,#12225) ;
#8110 = LINE('',#99873,#12226) ;
#8111 = LINE('',#99875,#12227) ;
#8112 = LINE('',#99879,#12228) ;
#8113 = LINE('',#99881,#12229) ;
#8114 = LINE('',#99883,#12230) ;
#8115 = LINE('',#99884,#12231) ;
#8116 = LINE('',#99888,#12232) ;
#8117 = LINE('',#99890,#12233) ;
#8118 = LINE('',#99892,#12234) ;
#8119 = LINE('',#99893,#12235) ;
#8120 = LINE('',#99897,#12236) ;
#8121 = LINE('',#99899,#12237) ;
#8122 = LINE('',#99901,#12238) ;
#8123 = LINE('',#99902,#12239) ;
#8124 = LINE('',#99904,#12240) ;
#8125 = LINE('',#99905,#12241) ;
#8126 = LINE('',#99907,#12242) ;
#8127 = LINE('',#99908,#12243) ;
#8128 = LINE('',#99911,#12244) ;
#8129 = LINE('',#99921,#12245) ;
#8130 = LINE('',#99926,#12246) ;
#8131 = LINE('',#99935,#12247) ;
#8132 = LINE('',#99937,#12248) ;
#8133 = LINE('',#99939,#12249) ;
#8134 = LINE('',#99940,#12250) ;
#8135 = LINE('',#99944,#12251) ;
#8136 = LINE('',#99946,#12252) ;
#8137 = LINE('',#99948,#12253) ;
#8138 = LINE('',#99949,#12254) ;
#8139 = LINE('',#99953,#12255) ;
#8140 = LINE('',#99955,#12256) ;
#8141 = LINE('',#99957,#12257) ;
#8142 = LINE('',#99958,#12258) ;
#8143 = LINE('',#99962,#12259) ;
#8144 = LINE('',#99964,#12260) ;
#8145 = LINE('',#99966,#12261) ;
#8146 = LINE('',#99967,#12262) ;
#8147 = LINE('',#99971,#12263) ;
#8148 = LINE('',#99973,#12264) ;
#8149 = LINE('',#99975,#12265) ;
#8150 = LINE('',#99976,#12266) ;
#8151 = LINE('',#99980,#12267) ;
#8152 = LINE('',#99982,#12268) ;
#8153 = LINE('',#99984,#12269) ;
#8154 = LINE('',#99985,#12270) ;
#8155 = LINE('',#99987,#12271) ;
#8156 = LINE('',#99991,#12272) ;
#8157 = LINE('',#99992,#12273) ;
#8158 = LINE('',#99993,#12274) ;
#8159 = LINE('',#99997,#12275) ;
#8160 = LINE('',#99999,#12276) ;
#8161 = LINE('',#100001,#12277) ;
#8162 = LINE('',#100002,#12278) ;
#8163 = LINE('',#100006,#12279) ;
#8164 = LINE('',#100008,#12280) ;
#8165 = LINE('',#100010,#12281) ;
#8166 = LINE('',#100011,#12282) ;
#8167 = LINE('',#100015,#12283) ;
#8168 = LINE('',#100017,#12284) ;
#8169 = LINE('',#100019,#12285) ;
#8170 = LINE('',#100020,#12286) ;
#8171 = LINE('',#100024,#12287) ;
#8172 = LINE('',#100026,#12288) ;
#8173 = LINE('',#100028,#12289) ;
#8174 = LINE('',#100029,#12290) ;
#8175 = LINE('',#100033,#12291) ;
#8176 = LINE('',#100035,#12292) ;
#8177 = LINE('',#100037,#12293) ;
#8178 = LINE('',#100038,#12294) ;
#8179 = LINE('',#100042,#12295) ;
#8180 = LINE('',#100044,#12296) ;
#8181 = LINE('',#100046,#12297) ;
#8182 = LINE('',#100047,#12298) ;
#8183 = LINE('',#100051,#12299) ;
#8184 = LINE('',#100053,#12300) ;
#8185 = LINE('',#100055,#12301) ;
#8186 = LINE('',#100056,#12302) ;
#8187 = LINE('',#100060,#12303) ;
#8188 = LINE('',#100062,#12304) ;
#8189 = LINE('',#100064,#12305) ;
#8190 = LINE('',#100065,#12306) ;
#8191 = LINE('',#100069,#12307) ;
#8192 = LINE('',#100071,#12308) ;
#8193 = LINE('',#100073,#12309) ;
#8194 = LINE('',#100074,#12310) ;
#8195 = LINE('',#100078,#12311) ;
#8196 = LINE('',#100080,#12312) ;
#8197 = LINE('',#100082,#12313) ;
#8198 = LINE('',#100083,#12314) ;
#8199 = LINE('',#100087,#12315) ;
#8200 = LINE('',#100089,#12316) ;
#8201 = LINE('',#100091,#12317) ;
#8202 = LINE('',#100092,#12318) ;
#8203 = LINE('',#100096,#12319) ;
#8204 = LINE('',#100098,#12320) ;
#8205 = LINE('',#100100,#12321) ;
#8206 = LINE('',#100101,#12322) ;
#8207 = LINE('',#100105,#12323) ;
#8208 = LINE('',#100107,#12324) ;
#8209 = LINE('',#100109,#12325) ;
#8210 = LINE('',#100110,#12326) ;
#8211 = LINE('',#100114,#12327) ;
#8212 = LINE('',#100116,#12328) ;
#8213 = LINE('',#100118,#12329) ;
#8214 = LINE('',#100119,#12330) ;
#8215 = LINE('',#100123,#12331) ;
#8216 = LINE('',#100125,#12332) ;
#8217 = LINE('',#100127,#12333) ;
#8218 = LINE('',#100128,#12334) ;
#8219 = LINE('',#100132,#12335) ;
#8220 = LINE('',#100134,#12336) ;
#8221 = LINE('',#100136,#12337) ;
#8222 = LINE('',#100137,#12338) ;
#8223 = LINE('',#100141,#12339) ;
#8224 = LINE('',#100143,#12340) ;
#8225 = LINE('',#100145,#12341) ;
#8226 = LINE('',#100146,#12342) ;
#8227 = LINE('',#100150,#12343) ;
#8228 = LINE('',#100152,#12344) ;
#8229 = LINE('',#100154,#12345) ;
#8230 = LINE('',#100155,#12346) ;
#8231 = LINE('',#100159,#12347) ;
#8232 = LINE('',#100161,#12348) ;
#8233 = LINE('',#100163,#12349) ;
#8234 = LINE('',#100164,#12350) ;
#8235 = LINE('',#100168,#12351) ;
#8236 = LINE('',#100170,#12352) ;
#8237 = LINE('',#100172,#12353) ;
#8238 = LINE('',#100173,#12354) ;
#8239 = LINE('',#100177,#12355) ;
#8240 = LINE('',#100179,#12356) ;
#8241 = LINE('',#100181,#12357) ;
#8242 = LINE('',#100182,#12358) ;
#8243 = LINE('',#100186,#12359) ;
#8244 = LINE('',#100188,#12360) ;
#8245 = LINE('',#100190,#12361) ;
#8246 = LINE('',#100191,#12362) ;
#8247 = LINE('',#100195,#12363) ;
#8248 = LINE('',#100197,#12364) ;
#8249 = LINE('',#100199,#12365) ;
#8250 = LINE('',#100200,#12366) ;
#8251 = LINE('',#100204,#12367) ;
#8252 = LINE('',#100206,#12368) ;
#8253 = LINE('',#100208,#12369) ;
#8254 = LINE('',#100209,#12370) ;
#8255 = LINE('',#100213,#12371) ;
#8256 = LINE('',#100215,#12372) ;
#8257 = LINE('',#100217,#12373) ;
#8258 = LINE('',#100218,#12374) ;
#8259 = LINE('',#100222,#12375) ;
#8260 = LINE('',#100224,#12376) ;
#8261 = LINE('',#100226,#12377) ;
#8262 = LINE('',#100227,#12378) ;
#8263 = LINE('',#100231,#12379) ;
#8264 = LINE('',#100233,#12380) ;
#8265 = LINE('',#100235,#12381) ;
#8266 = LINE('',#100236,#12382) ;
#8267 = LINE('',#100240,#12383) ;
#8268 = LINE('',#100242,#12384) ;
#8269 = LINE('',#100244,#12385) ;
#8270 = LINE('',#100245,#12386) ;
#8271 = LINE('',#100249,#12387) ;
#8272 = LINE('',#100251,#12388) ;
#8273 = LINE('',#100253,#12389) ;
#8274 = LINE('',#100254,#12390) ;
#8275 = LINE('',#100258,#12391) ;
#8276 = LINE('',#100260,#12392) ;
#8277 = LINE('',#100262,#12393) ;
#8278 = LINE('',#100263,#12394) ;
#8279 = LINE('',#100267,#12395) ;
#8280 = LINE('',#100269,#12396) ;
#8281 = LINE('',#100271,#12397) ;
#8282 = LINE('',#100272,#12398) ;
#8283 = LINE('',#100276,#12399) ;
#8284 = LINE('',#100278,#12400) ;
#8285 = LINE('',#100280,#12401) ;
#8286 = LINE('',#100281,#12402) ;
#8287 = LINE('',#100285,#12403) ;
#8288 = LINE('',#100287,#12404) ;
#8289 = LINE('',#100289,#12405) ;
#8290 = LINE('',#100290,#12406) ;
#8291 = LINE('',#100294,#12407) ;
#8292 = LINE('',#100296,#12408) ;
#8293 = LINE('',#100298,#12409) ;
#8294 = LINE('',#100299,#12410) ;
#8295 = LINE('',#100303,#12411) ;
#8296 = LINE('',#100305,#12412) ;
#8297 = LINE('',#100307,#12413) ;
#8298 = LINE('',#100308,#12414) ;
#8299 = LINE('',#100312,#12415) ;
#8300 = LINE('',#100314,#12416) ;
#8301 = LINE('',#100316,#12417) ;
#8302 = LINE('',#100317,#12418) ;
#8303 = LINE('',#100321,#12419) ;
#8304 = LINE('',#100323,#12420) ;
#8305 = LINE('',#100325,#12421) ;
#8306 = LINE('',#100326,#12422) ;
#8307 = LINE('',#100330,#12423) ;
#8308 = LINE('',#100332,#12424) ;
#8309 = LINE('',#100334,#12425) ;
#8310 = LINE('',#100335,#12426) ;
#8311 = LINE('',#100339,#12427) ;
#8312 = LINE('',#100341,#12428) ;
#8313 = LINE('',#100343,#12429) ;
#8314 = LINE('',#100344,#12430) ;
#8315 = LINE('',#100348,#12431) ;
#8316 = LINE('',#100350,#12432) ;
#8317 = LINE('',#100352,#12433) ;
#8318 = LINE('',#100353,#12434) ;
#8319 = LINE('',#100357,#12435) ;
#8320 = LINE('',#100359,#12436) ;
#8321 = LINE('',#100361,#12437) ;
#8322 = LINE('',#100362,#12438) ;
#8323 = LINE('',#100366,#12439) ;
#8324 = LINE('',#100368,#12440) ;
#8325 = LINE('',#100370,#12441) ;
#8326 = LINE('',#100371,#12442) ;
#8327 = LINE('',#100375,#12443) ;
#8328 = LINE('',#100377,#12444) ;
#8329 = LINE('',#100379,#12445) ;
#8330 = LINE('',#100380,#12446) ;
#8331 = LINE('',#100384,#12447) ;
#8332 = LINE('',#100386,#12448) ;
#8333 = LINE('',#100388,#12449) ;
#8334 = LINE('',#100389,#12450) ;
#8335 = LINE('',#100393,#12451) ;
#8336 = LINE('',#100395,#12452) ;
#8337 = LINE('',#100397,#12453) ;
#8338 = LINE('',#100398,#12454) ;
#8339 = LINE('',#100402,#12455) ;
#8340 = LINE('',#100404,#12456) ;
#8341 = LINE('',#100406,#12457) ;
#8342 = LINE('',#100407,#12458) ;
#8343 = LINE('',#100411,#12459) ;
#8344 = LINE('',#100413,#12460) ;
#8345 = LINE('',#100415,#12461) ;
#8346 = LINE('',#100416,#12462) ;
#8347 = LINE('',#100420,#12463) ;
#8348 = LINE('',#100422,#12464) ;
#8349 = LINE('',#100424,#12465) ;
#8350 = LINE('',#100425,#12466) ;
#8351 = LINE('',#101276,#12467) ;
#8352 = LINE('',#101281,#12468) ;
#8353 = LINE('',#101287,#12469) ;
#8354 = LINE('',#101290,#12470) ;
#8355 = LINE('',#101301,#12471) ;
#8356 = LINE('',#101304,#12472) ;
#8357 = LINE('',#101323,#12473) ;
#8358 = LINE('',#101327,#12474) ;
#8359 = LINE('',#101329,#12475) ;
#8360 = LINE('',#101338,#12476) ;
#8361 = LINE('',#101341,#12477) ;
#8362 = LINE('',#101345,#12478) ;
#8363 = LINE('',#101347,#12479) ;
#8364 = LINE('',#101389,#12480) ;
#8365 = LINE('',#101390,#12481) ;
#8366 = LINE('',#101394,#12482) ;
#8367 = LINE('',#101396,#12483) ;
#8368 = LINE('',#101398,#12484) ;
#8369 = LINE('',#101399,#12485) ;
#8370 = LINE('',#101403,#12486) ;
#8371 = LINE('',#101426,#12487) ;
#8372 = LINE('',#101428,#12488) ;
#8373 = LINE('',#101429,#12489) ;
#8374 = LINE('',#101433,#12490) ;
#8375 = LINE('',#101435,#12491) ;
#8376 = LINE('',#101437,#12492) ;
#8377 = LINE('',#101438,#12493) ;
#8378 = LINE('',#101442,#12494) ;
#8379 = LINE('',#101444,#12495) ;
#8380 = LINE('',#101446,#12496) ;
#8381 = LINE('',#101447,#12497) ;
#8382 = LINE('',#101451,#12498) ;
#8383 = LINE('',#101453,#12499) ;
#8384 = LINE('',#101455,#12500) ;
#8385 = LINE('',#101457,#12501) ;
#8386 = LINE('',#101460,#12502) ;
#8387 = LINE('',#101464,#12503) ;
#8388 = LINE('',#101471,#12504) ;
#8389 = LINE('',#101475,#12505) ;
#8390 = LINE('',#101479,#12506) ;
#8391 = LINE('',#101483,#12507) ;
#8392 = LINE('',#101487,#12508) ;
#8393 = LINE('',#101491,#12509) ;
#8394 = LINE('',#101496,#12510) ;
#8395 = LINE('',#101501,#12511) ;
#8396 = LINE('',#101503,#12512) ;
#8397 = LINE('',#101507,#12513) ;
#8398 = LINE('',#101511,#12514) ;
#8399 = LINE('',#101516,#12515) ;
#8400 = LINE('',#101520,#12516) ;
#8401 = LINE('',#101524,#12517) ;
#8402 = LINE('',#101528,#12518) ;
#8403 = LINE('',#101532,#12519) ;
#8404 = LINE('',#101534,#12520) ;
#8405 = LINE('',#101539,#12521) ;
#8406 = LINE('',#101544,#12522) ;
#8407 = LINE('',#101548,#12523) ;
#8408 = LINE('',#101552,#12524) ;
#8409 = LINE('',#101556,#12525) ;
#8410 = LINE('',#101560,#12526) ;
#8411 = LINE('',#101564,#12527) ;
#8412 = LINE('',#101568,#12528) ;
#8413 = LINE('',#101572,#12529) ;
#8414 = LINE('',#101575,#12530) ;
#8415 = LINE('',#101576,#12531) ;
#8416 = LINE('',#101578,#12532) ;
#8417 = LINE('',#101579,#12533) ;
#8418 = LINE('',#101623,#12534) ;
#8419 = LINE('',#101624,#12535) ;
#8420 = LINE('',#101626,#12536) ;
#8421 = LINE('',#101668,#12537) ;
#8422 = LINE('',#101681,#12538) ;
#8423 = LINE('',#101683,#12539) ;
#8424 = LINE('',#101684,#12540) ;
#8425 = LINE('',#101688,#12541) ;
#8426 = LINE('',#101689,#12542) ;
#8427 = LINE('',#101690,#12543) ;
#8428 = LINE('',#101708,#12544) ;
#8429 = LINE('',#101709,#12545) ;
#8430 = LINE('',#101710,#12546) ;
#8431 = LINE('',#101713,#12547) ;
#8432 = LINE('',#101750,#12548) ;
#8433 = LINE('',#101804,#12549) ;
#8434 = LINE('',#101806,#12550) ;
#8435 = LINE('',#101808,#12551) ;
#8436 = LINE('',#101812,#12552) ;
#8437 = LINE('',#101816,#12553) ;
#8438 = LINE('',#101817,#12554) ;
#8439 = LINE('',#101822,#12555) ;
#8440 = LINE('',#101824,#12556) ;
#8441 = LINE('',#101832,#12557) ;
#8442 = LINE('',#101834,#12558) ;
#8443 = LINE('',#101836,#12559) ;
#8444 = LINE('',#101843,#12560) ;
#8445 = LINE('',#101845,#12561) ;
#8446 = LINE('',#101853,#12562) ;
#8447 = LINE('',#101857,#12563) ;
#8448 = LINE('',#101866,#12564) ;
#8449 = LINE('',#101867,#12565) ;
#8450 = LINE('',#101868,#12566) ;
#8451 = LINE('',#101870,#12567) ;
#8452 = LINE('',#101872,#12568) ;
#8453 = LINE('',#101875,#12569) ;
#8454 = LINE('',#101880,#12570) ;
#8455 = LINE('',#101881,#12571) ;
#8456 = LINE('',#101883,#12572) ;
#8457 = LINE('',#101886,#12573) ;
#8458 = LINE('',#101890,#12574) ;
#8459 = LINE('',#101892,#12575) ;
#8460 = LINE('',#101899,#12576) ;
#8461 = LINE('',#101900,#12577) ;
#8462 = LINE('',#101904,#12578) ;
#8463 = LINE('',#101906,#12579) ;
#8464 = LINE('',#101908,#12580) ;
#8465 = LINE('',#101910,#12581) ;
#8466 = LINE('',#101912,#12582) ;
#8467 = LINE('',#101914,#12583) ;
#8468 = LINE('',#101916,#12584) ;
#8469 = LINE('',#101917,#12585) ;
#8470 = LINE('',#101921,#12586) ;
#8471 = LINE('',#101923,#12587) ;
#8472 = LINE('',#101925,#12588) ;
#8473 = LINE('',#101926,#12589) ;
#8474 = LINE('',#101930,#12590) ;
#8475 = LINE('',#101932,#12591) ;
#8476 = LINE('',#101934,#12592) ;
#8477 = LINE('',#101935,#12593) ;
#8478 = LINE('',#101939,#12594) ;
#8479 = LINE('',#101941,#12595) ;
#8480 = LINE('',#101943,#12596) ;
#8481 = LINE('',#101944,#12597) ;
#8482 = LINE('',#101957,#12598) ;
#8483 = LINE('',#101959,#12599) ;
#8484 = LINE('',#101961,#12600) ;
#8485 = LINE('',#101971,#12601) ;
#8486 = LINE('',#101975,#12602) ;
#8487 = LINE('',#101977,#12603) ;
#8488 = LINE('',#101979,#12604) ;
#8489 = LINE('',#101981,#12605) ;
#8490 = LINE('',#101983,#12606) ;
#8491 = LINE('',#101985,#12607) ;
#8492 = LINE('',#101987,#12608) ;
#8493 = LINE('',#101988,#12609) ;
#8494 = LINE('',#101992,#12610) ;
#8495 = LINE('',#101996,#12611) ;
#8496 = LINE('',#102000,#12612) ;
#8497 = LINE('',#102004,#12613) ;
#8498 = LINE('',#102010,#12614) ;
#8499 = LINE('',#102012,#12615) ;
#8500 = LINE('',#102016,#12616) ;
#8501 = LINE('',#102020,#12617) ;
#8502 = LINE('',#102022,#12618) ;
#8503 = LINE('',#102023,#12619) ;
#8504 = LINE('',#102027,#12620) ;
#8505 = LINE('',#102028,#12621) ;
#8506 = LINE('',#102029,#12622) ;
#8507 = LINE('',#102035,#12623) ;
#8508 = LINE('',#102038,#12624) ;
#8509 = LINE('',#102044,#12625) ;
#8510 = LINE('',#102047,#12626) ;
#8511 = LINE('',#102050,#12627) ;
#8512 = LINE('',#102052,#12628) ;
#8513 = LINE('',#102053,#12629) ;
#8514 = LINE('',#102057,#12630) ;
#8515 = LINE('',#102058,#12631) ;
#8516 = LINE('',#102059,#12632) ;
#8517 = LINE('',#102064,#12633) ;
#8518 = LINE('',#102066,#12634) ;
#8519 = LINE('',#102071,#12635) ;
#8520 = LINE('',#102076,#12636) ;
#8521 = LINE('',#102078,#12637) ;
#8522 = LINE('',#102079,#12638) ;
#8523 = LINE('',#102083,#12639) ;
#8524 = LINE('',#102084,#12640) ;
#8525 = LINE('',#102085,#12641) ;
#8526 = LINE('',#102091,#12642) ;
#8527 = LINE('',#102094,#12643) ;
#8528 = LINE('',#102098,#12644) ;
#8529 = LINE('',#102100,#12645) ;
#8530 = LINE('',#102102,#12646) ;
#8531 = LINE('',#102103,#12647) ;
#8532 = LINE('',#102109,#12648) ;
#8533 = LINE('',#102112,#12649) ;
#8534 = LINE('',#102115,#12650) ;
#8535 = LINE('',#102117,#12651) ;
#8536 = LINE('',#102118,#12652) ;
#8537 = LINE('',#102122,#12653) ;
#8538 = LINE('',#102124,#12654) ;
#8539 = LINE('',#102126,#12655) ;
#8540 = LINE('',#102127,#12656) ;
#8541 = LINE('',#102131,#12657) ;
#8542 = LINE('',#102132,#12658) ;
#8543 = LINE('',#102134,#12659) ;
#8544 = LINE('',#102139,#12660) ;
#8545 = LINE('',#102141,#12661) ;
#8546 = LINE('',#102143,#12662) ;
#8547 = LINE('',#102144,#12663) ;
#8548 = LINE('',#102149,#12664) ;
#8549 = LINE('',#102151,#12665) ;
#8550 = LINE('',#102155,#12666) ;
#8551 = LINE('',#102158,#12667) ;
#8552 = LINE('',#102162,#12668) ;
#8553 = LINE('',#102163,#12669) ;
#8554 = LINE('',#102165,#12670) ;
#8555 = LINE('',#102166,#12671) ;
#8556 = LINE('',#102170,#12672) ;
#8557 = LINE('',#102172,#12673) ;
#8558 = LINE('',#102174,#12674) ;
#8559 = LINE('',#102175,#12675) ;
#8560 = LINE('',#102179,#12676) ;
#8561 = LINE('',#102181,#12677) ;
#8562 = LINE('',#102183,#12678) ;
#8563 = LINE('',#102184,#12679) ;
#8564 = LINE('',#102188,#12680) ;
#8565 = LINE('',#102190,#12681) ;
#8566 = LINE('',#102192,#12682) ;
#8567 = LINE('',#102193,#12683) ;
#8568 = LINE('',#102196,#12684) ;
#8569 = LINE('',#102198,#12685) ;
#8570 = LINE('',#102199,#12686) ;
#8571 = LINE('',#102202,#12687) ;
#8572 = LINE('',#102204,#12688) ;
#8573 = LINE('',#102205,#12689) ;
#8574 = LINE('',#102208,#12690) ;
#8575 = LINE('',#102210,#12691) ;
#8576 = LINE('',#102211,#12692) ;
#8577 = LINE('',#102214,#12693) ;
#8578 = LINE('',#102216,#12694) ;
#8579 = LINE('',#102217,#12695) ;
#8580 = LINE('',#102221,#12696) ;
#8581 = LINE('',#102223,#12697) ;
#8582 = LINE('',#102225,#12698) ;
#8583 = LINE('',#102229,#12699) ;
#8584 = LINE('',#102234,#12700) ;
#8585 = LINE('',#102236,#12701) ;
#8586 = LINE('',#102238,#12702) ;
#8587 = LINE('',#102242,#12703) ;
#8588 = LINE('',#102247,#12704) ;
#8589 = LINE('',#102252,#12705) ;
#8590 = LINE('',#102254,#12706) ;
#8591 = LINE('',#102255,#12707) ;
#8592 = LINE('',#102259,#12708) ;
#8593 = LINE('',#102261,#12709) ;
#8594 = LINE('',#102263,#12710) ;
#8595 = LINE('',#102264,#12711) ;
#8596 = LINE('',#102268,#12712) ;
#8597 = LINE('',#102270,#12713) ;
#8598 = LINE('',#102272,#12714) ;
#8599 = LINE('',#102273,#12715) ;
#8600 = LINE('',#102277,#12716) ;
#8601 = LINE('',#102279,#12717) ;
#8602 = LINE('',#102281,#12718) ;
#8603 = LINE('',#102282,#12719) ;
#8604 = LINE('',#102286,#12720) ;
#8605 = LINE('',#102288,#12721) ;
#8606 = LINE('',#102290,#12722) ;
#8607 = LINE('',#102291,#12723) ;
#8608 = LINE('',#102298,#12724) ;
#8609 = LINE('',#102300,#12725) ;
#8610 = LINE('',#102302,#12726) ;
#8611 = LINE('',#102303,#12727) ;
#8612 = LINE('',#102307,#12728) ;
#8613 = LINE('',#102309,#12729) ;
#8614 = LINE('',#102311,#12730) ;
#8615 = LINE('',#102312,#12731) ;
#8616 = LINE('',#102316,#12732) ;
#8617 = LINE('',#102318,#12733) ;
#8618 = LINE('',#102320,#12734) ;
#8619 = LINE('',#102321,#12735) ;
#8620 = LINE('',#102325,#12736) ;
#8621 = LINE('',#102327,#12737) ;
#8622 = LINE('',#102329,#12738) ;
#8623 = LINE('',#102330,#12739) ;
#8624 = LINE('',#102333,#12740) ;
#8625 = LINE('',#102336,#12741) ;
#8626 = LINE('',#102345,#12742) ;
#8627 = LINE('',#102348,#12743) ;
#8628 = LINE('',#102529,#12744) ;
#8629 = LINE('',#102574,#12745) ;
#8630 = LINE('',#102582,#12746) ;
#8631 = LINE('',#102603,#12747) ;
#8632 = LINE('',#102609,#12748) ;
#8633 = LINE('',#102622,#12749) ;
#8634 = LINE('',#103788,#12750) ;
#8635 = LINE('',#103793,#12751) ;
#8636 = LINE('',#103799,#12752) ;
#8637 = LINE('',#103802,#12753) ;
#8638 = LINE('',#103813,#12754) ;
#8639 = LINE('',#103816,#12755) ;
#8640 = LINE('',#103835,#12756) ;
#8641 = LINE('',#103839,#12757) ;
#8642 = LINE('',#103841,#12758) ;
#8643 = LINE('',#103850,#12759) ;
#8644 = LINE('',#103853,#12760) ;
#8645 = LINE('',#103857,#12761) ;
#8646 = LINE('',#103859,#12762) ;
#8647 = LINE('',#103901,#12763) ;
#8648 = LINE('',#103902,#12764) ;
#8649 = LINE('',#103906,#12765) ;
#8650 = LINE('',#103908,#12766) ;
#8651 = LINE('',#103910,#12767) ;
#8652 = LINE('',#103911,#12768) ;
#8653 = LINE('',#103915,#12769) ;
#8654 = LINE('',#103938,#12770) ;
#8655 = LINE('',#103940,#12771) ;
#8656 = LINE('',#103941,#12772) ;
#8657 = LINE('',#103945,#12773) ;
#8658 = LINE('',#103947,#12774) ;
#8659 = LINE('',#103949,#12775) ;
#8660 = LINE('',#103950,#12776) ;
#8661 = LINE('',#103954,#12777) ;
#8662 = LINE('',#103956,#12778) ;
#8663 = LINE('',#103958,#12779) ;
#8664 = LINE('',#103959,#12780) ;
#8665 = LINE('',#103963,#12781) ;
#8666 = LINE('',#103965,#12782) ;
#8667 = LINE('',#103967,#12783) ;
#8668 = LINE('',#103969,#12784) ;
#8669 = LINE('',#103972,#12785) ;
#8670 = LINE('',#103976,#12786) ;
#8671 = LINE('',#103983,#12787) ;
#8672 = LINE('',#103987,#12788) ;
#8673 = LINE('',#103991,#12789) ;
#8674 = LINE('',#103995,#12790) ;
#8675 = LINE('',#103999,#12791) ;
#8676 = LINE('',#104003,#12792) ;
#8677 = LINE('',#104008,#12793) ;
#8678 = LINE('',#104013,#12794) ;
#8679 = LINE('',#104015,#12795) ;
#8680 = LINE('',#104019,#12796) ;
#8681 = LINE('',#104023,#12797) ;
#8682 = LINE('',#104028,#12798) ;
#8683 = LINE('',#104032,#12799) ;
#8684 = LINE('',#104036,#12800) ;
#8685 = LINE('',#104040,#12801) ;
#8686 = LINE('',#104044,#12802) ;
#8687 = LINE('',#104046,#12803) ;
#8688 = LINE('',#104051,#12804) ;
#8689 = LINE('',#104056,#12805) ;
#8690 = LINE('',#104060,#12806) ;
#8691 = LINE('',#104064,#12807) ;
#8692 = LINE('',#104068,#12808) ;
#8693 = LINE('',#104072,#12809) ;
#8694 = LINE('',#104076,#12810) ;
#8695 = LINE('',#104080,#12811) ;
#8696 = LINE('',#104084,#12812) ;
#8697 = LINE('',#104087,#12813) ;
#8698 = LINE('',#104088,#12814) ;
#8699 = LINE('',#104090,#12815) ;
#8700 = LINE('',#104091,#12816) ;
#8701 = LINE('',#104135,#12817) ;
#8702 = LINE('',#104136,#12818) ;
#8703 = LINE('',#104138,#12819) ;
#8704 = LINE('',#104180,#12820) ;
#8705 = LINE('',#104193,#12821) ;
#8706 = LINE('',#104195,#12822) ;
#8707 = LINE('',#104196,#12823) ;
#8708 = LINE('',#104200,#12824) ;
#8709 = LINE('',#104201,#12825) ;
#8710 = LINE('',#104202,#12826) ;
#8711 = LINE('',#104220,#12827) ;
#8712 = LINE('',#104221,#12828) ;
#8713 = LINE('',#104222,#12829) ;
#8714 = LINE('',#104225,#12830) ;
#8715 = LINE('',#104262,#12831) ;
#8716 = LINE('',#104316,#12832) ;
#8717 = LINE('',#104318,#12833) ;
#8718 = LINE('',#104320,#12834) ;
#8719 = LINE('',#104324,#12835) ;
#8720 = LINE('',#104328,#12836) ;
#8721 = LINE('',#104329,#12837) ;
#8722 = LINE('',#104334,#12838) ;
#8723 = LINE('',#104336,#12839) ;
#8724 = LINE('',#104344,#12840) ;
#8725 = LINE('',#104346,#12841) ;
#8726 = LINE('',#104348,#12842) ;
#8727 = LINE('',#104355,#12843) ;
#8728 = LINE('',#104357,#12844) ;
#8729 = LINE('',#104365,#12845) ;
#8730 = LINE('',#104369,#12846) ;
#8731 = LINE('',#104378,#12847) ;
#8732 = LINE('',#104379,#12848) ;
#8733 = LINE('',#104380,#12849) ;
#8734 = LINE('',#104382,#12850) ;
#8735 = LINE('',#104384,#12851) ;
#8736 = LINE('',#104387,#12852) ;
#8737 = LINE('',#104392,#12853) ;
#8738 = LINE('',#104393,#12854) ;
#8739 = LINE('',#104395,#12855) ;
#8740 = LINE('',#104398,#12856) ;
#8741 = LINE('',#104402,#12857) ;
#8742 = LINE('',#104404,#12858) ;
#8743 = LINE('',#104411,#12859) ;
#8744 = LINE('',#104412,#12860) ;
#8745 = LINE('',#104416,#12861) ;
#8746 = LINE('',#104418,#12862) ;
#8747 = LINE('',#104420,#12863) ;
#8748 = LINE('',#104422,#12864) ;
#8749 = LINE('',#104424,#12865) ;
#8750 = LINE('',#104426,#12866) ;
#8751 = LINE('',#104428,#12867) ;
#8752 = LINE('',#104429,#12868) ;
#8753 = LINE('',#104433,#12869) ;
#8754 = LINE('',#104435,#12870) ;
#8755 = LINE('',#104437,#12871) ;
#8756 = LINE('',#104438,#12872) ;
#8757 = LINE('',#104442,#12873) ;
#8758 = LINE('',#104444,#12874) ;
#8759 = LINE('',#104446,#12875) ;
#8760 = LINE('',#104447,#12876) ;
#8761 = LINE('',#104451,#12877) ;
#8762 = LINE('',#104453,#12878) ;
#8763 = LINE('',#104455,#12879) ;
#8764 = LINE('',#104456,#12880) ;
#8765 = LINE('',#104469,#12881) ;
#8766 = LINE('',#104471,#12882) ;
#8767 = LINE('',#104473,#12883) ;
#8768 = LINE('',#104483,#12884) ;
#8769 = LINE('',#104487,#12885) ;
#8770 = LINE('',#104489,#12886) ;
#8771 = LINE('',#104491,#12887) ;
#8772 = LINE('',#104493,#12888) ;
#8773 = LINE('',#104495,#12889) ;
#8774 = LINE('',#104497,#12890) ;
#8775 = LINE('',#104499,#12891) ;
#8776 = LINE('',#104500,#12892) ;
#8777 = LINE('',#104504,#12893) ;
#8778 = LINE('',#104508,#12894) ;
#8779 = LINE('',#104512,#12895) ;
#8780 = LINE('',#104516,#12896) ;
#8781 = LINE('',#104522,#12897) ;
#8782 = LINE('',#104524,#12898) ;
#8783 = LINE('',#104528,#12899) ;
#8784 = LINE('',#104532,#12900) ;
#8785 = LINE('',#104534,#12901) ;
#8786 = LINE('',#104535,#12902) ;
#8787 = LINE('',#104539,#12903) ;
#8788 = LINE('',#104540,#12904) ;
#8789 = LINE('',#104541,#12905) ;
#8790 = LINE('',#104547,#12906) ;
#8791 = LINE('',#104550,#12907) ;
#8792 = LINE('',#104556,#12908) ;
#8793 = LINE('',#104559,#12909) ;
#8794 = LINE('',#104562,#12910) ;
#8795 = LINE('',#104564,#12911) ;
#8796 = LINE('',#104565,#12912) ;
#8797 = LINE('',#104569,#12913) ;
#8798 = LINE('',#104570,#12914) ;
#8799 = LINE('',#104571,#12915) ;
#8800 = LINE('',#104576,#12916) ;
#8801 = LINE('',#104578,#12917) ;
#8802 = LINE('',#104583,#12918) ;
#8803 = LINE('',#104588,#12919) ;
#8804 = LINE('',#104590,#12920) ;
#8805 = LINE('',#104591,#12921) ;
#8806 = LINE('',#104595,#12922) ;
#8807 = LINE('',#104596,#12923) ;
#8808 = LINE('',#104597,#12924) ;
#8809 = LINE('',#104603,#12925) ;
#8810 = LINE('',#104606,#12926) ;
#8811 = LINE('',#104610,#12927) ;
#8812 = LINE('',#104612,#12928) ;
#8813 = LINE('',#104614,#12929) ;
#8814 = LINE('',#104615,#12930) ;
#8815 = LINE('',#104621,#12931) ;
#8816 = LINE('',#104624,#12932) ;
#8817 = LINE('',#104627,#12933) ;
#8818 = LINE('',#104629,#12934) ;
#8819 = LINE('',#104630,#12935) ;
#8820 = LINE('',#104634,#12936) ;
#8821 = LINE('',#104636,#12937) ;
#8822 = LINE('',#104638,#12938) ;
#8823 = LINE('',#104639,#12939) ;
#8824 = LINE('',#104643,#12940) ;
#8825 = LINE('',#104644,#12941) ;
#8826 = LINE('',#104646,#12942) ;
#8827 = LINE('',#104651,#12943) ;
#8828 = LINE('',#104653,#12944) ;
#8829 = LINE('',#104655,#12945) ;
#8830 = LINE('',#104656,#12946) ;
#8831 = LINE('',#104661,#12947) ;
#8832 = LINE('',#104663,#12948) ;
#8833 = LINE('',#104667,#12949) ;
#8834 = LINE('',#104670,#12950) ;
#8835 = LINE('',#104674,#12951) ;
#8836 = LINE('',#104675,#12952) ;
#8837 = LINE('',#104677,#12953) ;
#8838 = LINE('',#104678,#12954) ;
#8839 = LINE('',#104682,#12955) ;
#8840 = LINE('',#104684,#12956) ;
#8841 = LINE('',#104686,#12957) ;
#8842 = LINE('',#104687,#12958) ;
#8843 = LINE('',#104691,#12959) ;
#8844 = LINE('',#104693,#12960) ;
#8845 = LINE('',#104695,#12961) ;
#8846 = LINE('',#104696,#12962) ;
#8847 = LINE('',#104700,#12963) ;
#8848 = LINE('',#104702,#12964) ;
#8849 = LINE('',#104704,#12965) ;
#8850 = LINE('',#104705,#12966) ;
#8851 = LINE('',#104708,#12967) ;
#8852 = LINE('',#104710,#12968) ;
#8853 = LINE('',#104711,#12969) ;
#8854 = LINE('',#104714,#12970) ;
#8855 = LINE('',#104716,#12971) ;
#8856 = LINE('',#104717,#12972) ;
#8857 = LINE('',#104720,#12973) ;
#8858 = LINE('',#104722,#12974) ;
#8859 = LINE('',#104723,#12975) ;
#8860 = LINE('',#104726,#12976) ;
#8861 = LINE('',#104728,#12977) ;
#8862 = LINE('',#104729,#12978) ;
#8863 = LINE('',#104733,#12979) ;
#8864 = LINE('',#104735,#12980) ;
#8865 = LINE('',#104737,#12981) ;
#8866 = LINE('',#104741,#12982) ;
#8867 = LINE('',#104746,#12983) ;
#8868 = LINE('',#104748,#12984) ;
#8869 = LINE('',#104750,#12985) ;
#8870 = LINE('',#104754,#12986) ;
#8871 = LINE('',#104759,#12987) ;
#8872 = LINE('',#104764,#12988) ;
#8873 = LINE('',#104766,#12989) ;
#8874 = LINE('',#104767,#12990) ;
#8875 = LINE('',#104771,#12991) ;
#8876 = LINE('',#104773,#12992) ;
#8877 = LINE('',#104775,#12993) ;
#8878 = LINE('',#104776,#12994) ;
#8879 = LINE('',#104780,#12995) ;
#8880 = LINE('',#104782,#12996) ;
#8881 = LINE('',#104784,#12997) ;
#8882 = LINE('',#104785,#12998) ;
#8883 = LINE('',#104789,#12999) ;
#8884 = LINE('',#104791,#13000) ;
#8885 = LINE('',#104793,#13001) ;
#8886 = LINE('',#104794,#13002) ;
#8887 = LINE('',#104798,#13003) ;
#8888 = LINE('',#104800,#13004) ;
#8889 = LINE('',#104802,#13005) ;
#8890 = LINE('',#104803,#13006) ;
#8891 = LINE('',#104810,#13007) ;
#8892 = LINE('',#104812,#13008) ;
#8893 = LINE('',#104814,#13009) ;
#8894 = LINE('',#104815,#13010) ;
#8895 = LINE('',#104819,#13011) ;
#8896 = LINE('',#104821,#13012) ;
#8897 = LINE('',#104823,#13013) ;
#8898 = LINE('',#104824,#13014) ;
#8899 = LINE('',#104828,#13015) ;
#8900 = LINE('',#104830,#13016) ;
#8901 = LINE('',#104832,#13017) ;
#8902 = LINE('',#104833,#13018) ;
#8903 = LINE('',#104837,#13019) ;
#8904 = LINE('',#104839,#13020) ;
#8905 = LINE('',#104841,#13021) ;
#8906 = LINE('',#104842,#13022) ;
#8907 = LINE('',#104845,#13023) ;
#8908 = LINE('',#104848,#13024) ;
#8909 = LINE('',#104857,#13025) ;
#8910 = LINE('',#104860,#13026) ;
#8911 = LINE('',#105041,#13027) ;
#8912 = LINE('',#105086,#13028) ;
#8913 = LINE('',#105094,#13029) ;
#8914 = LINE('',#105115,#13030) ;
#8915 = LINE('',#105121,#13031) ;
#8916 = LINE('',#105134,#13032) ;
#8917 = LINE('',#106300,#13033) ;
#8918 = LINE('',#106305,#13034) ;
#8919 = LINE('',#106311,#13035) ;
#8920 = LINE('',#106314,#13036) ;
#8921 = LINE('',#106325,#13037) ;
#8922 = LINE('',#106328,#13038) ;
#8923 = LINE('',#106347,#13039) ;
#8924 = LINE('',#106351,#13040) ;
#8925 = LINE('',#106353,#13041) ;
#8926 = LINE('',#106362,#13042) ;
#8927 = LINE('',#106365,#13043) ;
#8928 = LINE('',#106369,#13044) ;
#8929 = LINE('',#106371,#13045) ;
#8930 = LINE('',#106413,#13046) ;
#8931 = LINE('',#106414,#13047) ;
#8932 = LINE('',#106418,#13048) ;
#8933 = LINE('',#106420,#13049) ;
#8934 = LINE('',#106422,#13050) ;
#8935 = LINE('',#106423,#13051) ;
#8936 = LINE('',#106427,#13052) ;
#8937 = LINE('',#106450,#13053) ;
#8938 = LINE('',#106452,#13054) ;
#8939 = LINE('',#106453,#13055) ;
#8940 = LINE('',#106457,#13056) ;
#8941 = LINE('',#106459,#13057) ;
#8942 = LINE('',#106461,#13058) ;
#8943 = LINE('',#106462,#13059) ;
#8944 = LINE('',#106466,#13060) ;
#8945 = LINE('',#106468,#13061) ;
#8946 = LINE('',#106470,#13062) ;
#8947 = LINE('',#106471,#13063) ;
#8948 = LINE('',#106475,#13064) ;
#8949 = LINE('',#106477,#13065) ;
#8950 = LINE('',#106479,#13066) ;
#8951 = LINE('',#106481,#13067) ;
#8952 = LINE('',#106484,#13068) ;
#8953 = LINE('',#106488,#13069) ;
#8954 = LINE('',#106495,#13070) ;
#8955 = LINE('',#106499,#13071) ;
#8956 = LINE('',#106503,#13072) ;
#8957 = LINE('',#106507,#13073) ;
#8958 = LINE('',#106511,#13074) ;
#8959 = LINE('',#106515,#13075) ;
#8960 = LINE('',#106520,#13076) ;
#8961 = LINE('',#106525,#13077) ;
#8962 = LINE('',#106527,#13078) ;
#8963 = LINE('',#106531,#13079) ;
#8964 = LINE('',#106535,#13080) ;
#8965 = LINE('',#106540,#13081) ;
#8966 = LINE('',#106544,#13082) ;
#8967 = LINE('',#106548,#13083) ;
#8968 = LINE('',#106552,#13084) ;
#8969 = LINE('',#106556,#13085) ;
#8970 = LINE('',#106558,#13086) ;
#8971 = LINE('',#106563,#13087) ;
#8972 = LINE('',#106568,#13088) ;
#8973 = LINE('',#106572,#13089) ;
#8974 = LINE('',#106576,#13090) ;
#8975 = LINE('',#106580,#13091) ;
#8976 = LINE('',#106584,#13092) ;
#8977 = LINE('',#106588,#13093) ;
#8978 = LINE('',#106592,#13094) ;
#8979 = LINE('',#106596,#13095) ;
#8980 = LINE('',#106599,#13096) ;
#8981 = LINE('',#106600,#13097) ;
#8982 = LINE('',#106602,#13098) ;
#8983 = LINE('',#106603,#13099) ;
#8984 = LINE('',#106647,#13100) ;
#8985 = LINE('',#106648,#13101) ;
#8986 = LINE('',#106650,#13102) ;
#8987 = LINE('',#106692,#13103) ;
#8988 = LINE('',#106705,#13104) ;
#8989 = LINE('',#106707,#13105) ;
#8990 = LINE('',#106708,#13106) ;
#8991 = LINE('',#106712,#13107) ;
#8992 = LINE('',#106713,#13108) ;
#8993 = LINE('',#106714,#13109) ;
#8994 = LINE('',#106732,#13110) ;
#8995 = LINE('',#106733,#13111) ;
#8996 = LINE('',#106734,#13112) ;
#8997 = LINE('',#106737,#13113) ;
#8998 = LINE('',#106774,#13114) ;
#8999 = LINE('',#106828,#13115) ;
#9000 = LINE('',#106830,#13116) ;
#9001 = LINE('',#106832,#13117) ;
#9002 = LINE('',#106836,#13118) ;
#9003 = LINE('',#106840,#13119) ;
#9004 = LINE('',#106841,#13120) ;
#9005 = LINE('',#106846,#13121) ;
#9006 = LINE('',#106848,#13122) ;
#9007 = LINE('',#106856,#13123) ;
#9008 = LINE('',#106858,#13124) ;
#9009 = LINE('',#106860,#13125) ;
#9010 = LINE('',#106867,#13126) ;
#9011 = LINE('',#106869,#13127) ;
#9012 = LINE('',#106877,#13128) ;
#9013 = LINE('',#106881,#13129) ;
#9014 = LINE('',#106890,#13130) ;
#9015 = LINE('',#106891,#13131) ;
#9016 = LINE('',#106892,#13132) ;
#9017 = LINE('',#106894,#13133) ;
#9018 = LINE('',#106896,#13134) ;
#9019 = LINE('',#106899,#13135) ;
#9020 = LINE('',#106904,#13136) ;
#9021 = LINE('',#106905,#13137) ;
#9022 = LINE('',#106907,#13138) ;
#9023 = LINE('',#106910,#13139) ;
#9024 = LINE('',#106914,#13140) ;
#9025 = LINE('',#106916,#13141) ;
#9026 = LINE('',#106923,#13142) ;
#9027 = LINE('',#106924,#13143) ;
#9028 = LINE('',#106928,#13144) ;
#9029 = LINE('',#106930,#13145) ;
#9030 = LINE('',#106932,#13146) ;
#9031 = LINE('',#106934,#13147) ;
#9032 = LINE('',#106936,#13148) ;
#9033 = LINE('',#106938,#13149) ;
#9034 = LINE('',#106940,#13150) ;
#9035 = LINE('',#106941,#13151) ;
#9036 = LINE('',#106945,#13152) ;
#9037 = LINE('',#106947,#13153) ;
#9038 = LINE('',#106949,#13154) ;
#9039 = LINE('',#106950,#13155) ;
#9040 = LINE('',#106954,#13156) ;
#9041 = LINE('',#106956,#13157) ;
#9042 = LINE('',#106958,#13158) ;
#9043 = LINE('',#106959,#13159) ;
#9044 = LINE('',#106963,#13160) ;
#9045 = LINE('',#106965,#13161) ;
#9046 = LINE('',#106967,#13162) ;
#9047 = LINE('',#106968,#13163) ;
#9048 = LINE('',#106981,#13164) ;
#9049 = LINE('',#106983,#13165) ;
#9050 = LINE('',#106985,#13166) ;
#9051 = LINE('',#106995,#13167) ;
#9052 = LINE('',#106999,#13168) ;
#9053 = LINE('',#107001,#13169) ;
#9054 = LINE('',#107003,#13170) ;
#9055 = LINE('',#107005,#13171) ;
#9056 = LINE('',#107007,#13172) ;
#9057 = LINE('',#107009,#13173) ;
#9058 = LINE('',#107011,#13174) ;
#9059 = LINE('',#107012,#13175) ;
#9060 = LINE('',#107016,#13176) ;
#9061 = LINE('',#107020,#13177) ;
#9062 = LINE('',#107024,#13178) ;
#9063 = LINE('',#107028,#13179) ;
#9064 = LINE('',#107034,#13180) ;
#9065 = LINE('',#107036,#13181) ;
#9066 = LINE('',#107040,#13182) ;
#9067 = LINE('',#107044,#13183) ;
#9068 = LINE('',#107046,#13184) ;
#9069 = LINE('',#107047,#13185) ;
#9070 = LINE('',#107051,#13186) ;
#9071 = LINE('',#107052,#13187) ;
#9072 = LINE('',#107053,#13188) ;
#9073 = LINE('',#107059,#13189) ;
#9074 = LINE('',#107062,#13190) ;
#9075 = LINE('',#107068,#13191) ;
#9076 = LINE('',#107071,#13192) ;
#9077 = LINE('',#107074,#13193) ;
#9078 = LINE('',#107076,#13194) ;
#9079 = LINE('',#107077,#13195) ;
#9080 = LINE('',#107081,#13196) ;
#9081 = LINE('',#107082,#13197) ;
#9082 = LINE('',#107083,#13198) ;
#9083 = LINE('',#107088,#13199) ;
#9084 = LINE('',#107090,#13200) ;
#9085 = LINE('',#107095,#13201) ;
#9086 = LINE('',#107100,#13202) ;
#9087 = LINE('',#107102,#13203) ;
#9088 = LINE('',#107103,#13204) ;
#9089 = LINE('',#107107,#13205) ;
#9090 = LINE('',#107108,#13206) ;
#9091 = LINE('',#107109,#13207) ;
#9092 = LINE('',#107115,#13208) ;
#9093 = LINE('',#107118,#13209) ;
#9094 = LINE('',#107122,#13210) ;
#9095 = LINE('',#107124,#13211) ;
#9096 = LINE('',#107126,#13212) ;
#9097 = LINE('',#107127,#13213) ;
#9098 = LINE('',#107133,#13214) ;
#9099 = LINE('',#107136,#13215) ;
#9100 = LINE('',#107139,#13216) ;
#9101 = LINE('',#107141,#13217) ;
#9102 = LINE('',#107142,#13218) ;
#9103 = LINE('',#107146,#13219) ;
#9104 = LINE('',#107148,#13220) ;
#9105 = LINE('',#107150,#13221) ;
#9106 = LINE('',#107151,#13222) ;
#9107 = LINE('',#107155,#13223) ;
#9108 = LINE('',#107156,#13224) ;
#9109 = LINE('',#107158,#13225) ;
#9110 = LINE('',#107163,#13226) ;
#9111 = LINE('',#107165,#13227) ;
#9112 = LINE('',#107167,#13228) ;
#9113 = LINE('',#107168,#13229) ;
#9114 = LINE('',#107173,#13230) ;
#9115 = LINE('',#107175,#13231) ;
#9116 = LINE('',#107179,#13232) ;
#9117 = LINE('',#107182,#13233) ;
#9118 = LINE('',#107186,#13234) ;
#9119 = LINE('',#107187,#13235) ;
#9120 = LINE('',#107189,#13236) ;
#9121 = LINE('',#107190,#13237) ;
#9122 = LINE('',#107194,#13238) ;
#9123 = LINE('',#107196,#13239) ;
#9124 = LINE('',#107198,#13240) ;
#9125 = LINE('',#107199,#13241) ;
#9126 = LINE('',#107203,#13242) ;
#9127 = LINE('',#107205,#13243) ;
#9128 = LINE('',#107207,#13244) ;
#9129 = LINE('',#107208,#13245) ;
#9130 = LINE('',#107212,#13246) ;
#9131 = LINE('',#107214,#13247) ;
#9132 = LINE('',#107216,#13248) ;
#9133 = LINE('',#107217,#13249) ;
#9134 = LINE('',#107220,#13250) ;
#9135 = LINE('',#107222,#13251) ;
#9136 = LINE('',#107223,#13252) ;
#9137 = LINE('',#107226,#13253) ;
#9138 = LINE('',#107228,#13254) ;
#9139 = LINE('',#107229,#13255) ;
#9140 = LINE('',#107232,#13256) ;
#9141 = LINE('',#107234,#13257) ;
#9142 = LINE('',#107235,#13258) ;
#9143 = LINE('',#107238,#13259) ;
#9144 = LINE('',#107240,#13260) ;
#9145 = LINE('',#107241,#13261) ;
#9146 = LINE('',#107245,#13262) ;
#9147 = LINE('',#107247,#13263) ;
#9148 = LINE('',#107249,#13264) ;
#9149 = LINE('',#107253,#13265) ;
#9150 = LINE('',#107258,#13266) ;
#9151 = LINE('',#107260,#13267) ;
#9152 = LINE('',#107262,#13268) ;
#9153 = LINE('',#107266,#13269) ;
#9154 = LINE('',#107271,#13270) ;
#9155 = LINE('',#107276,#13271) ;
#9156 = LINE('',#107278,#13272) ;
#9157 = LINE('',#107279,#13273) ;
#9158 = LINE('',#107283,#13274) ;
#9159 = LINE('',#107285,#13275) ;
#9160 = LINE('',#107287,#13276) ;
#9161 = LINE('',#107288,#13277) ;
#9162 = LINE('',#107292,#13278) ;
#9163 = LINE('',#107294,#13279) ;
#9164 = LINE('',#107296,#13280) ;
#9165 = LINE('',#107297,#13281) ;
#9166 = LINE('',#107301,#13282) ;
#9167 = LINE('',#107303,#13283) ;
#9168 = LINE('',#107305,#13284) ;
#9169 = LINE('',#107306,#13285) ;
#9170 = LINE('',#107310,#13286) ;
#9171 = LINE('',#107312,#13287) ;
#9172 = LINE('',#107314,#13288) ;
#9173 = LINE('',#107315,#13289) ;
#9174 = LINE('',#107322,#13290) ;
#9175 = LINE('',#107324,#13291) ;
#9176 = LINE('',#107326,#13292) ;
#9177 = LINE('',#107327,#13293) ;
#9178 = LINE('',#107331,#13294) ;
#9179 = LINE('',#107333,#13295) ;
#9180 = LINE('',#107335,#13296) ;
#9181 = LINE('',#107336,#13297) ;
#9182 = LINE('',#107340,#13298) ;
#9183 = LINE('',#107342,#13299) ;
#9184 = LINE('',#107344,#13300) ;
#9185 = LINE('',#107345,#13301) ;
#9186 = LINE('',#107349,#13302) ;
#9187 = LINE('',#107351,#13303) ;
#9188 = LINE('',#107353,#13304) ;
#9189 = LINE('',#107354,#13305) ;
#9190 = LINE('',#107357,#13306) ;
#9191 = LINE('',#107360,#13307) ;
#9192 = LINE('',#107369,#13308) ;
#9193 = LINE('',#107372,#13309) ;
#9194 = LINE('',#107553,#13310) ;
#9195 = LINE('',#107598,#13311) ;
#9196 = LINE('',#107606,#13312) ;
#9197 = LINE('',#107627,#13313) ;
#9198 = LINE('',#107633,#13314) ;
#9199 = LINE('',#107646,#13315) ;
#9200 = LINE('',#108812,#13316) ;
#9201 = LINE('',#108817,#13317) ;
#9202 = LINE('',#108823,#13318) ;
#9203 = LINE('',#108826,#13319) ;
#9204 = LINE('',#108837,#13320) ;
#9205 = LINE('',#108840,#13321) ;
#9206 = LINE('',#108859,#13322) ;
#9207 = LINE('',#108863,#13323) ;
#9208 = LINE('',#108865,#13324) ;
#9209 = LINE('',#108874,#13325) ;
#9210 = LINE('',#108877,#13326) ;
#9211 = LINE('',#108881,#13327) ;
#9212 = LINE('',#108883,#13328) ;
#9213 = LINE('',#108925,#13329) ;
#9214 = LINE('',#108926,#13330) ;
#9215 = LINE('',#108930,#13331) ;
#9216 = LINE('',#108932,#13332) ;
#9217 = LINE('',#108934,#13333) ;
#9218 = LINE('',#108935,#13334) ;
#9219 = LINE('',#108939,#13335) ;
#9220 = LINE('',#108962,#13336) ;
#9221 = LINE('',#108964,#13337) ;
#9222 = LINE('',#108965,#13338) ;
#9223 = LINE('',#108969,#13339) ;
#9224 = LINE('',#108971,#13340) ;
#9225 = LINE('',#108973,#13341) ;
#9226 = LINE('',#108974,#13342) ;
#9227 = LINE('',#108978,#13343) ;
#9228 = LINE('',#108980,#13344) ;
#9229 = LINE('',#108982,#13345) ;
#9230 = LINE('',#108983,#13346) ;
#9231 = LINE('',#108987,#13347) ;
#9232 = LINE('',#108989,#13348) ;
#9233 = LINE('',#108991,#13349) ;
#9234 = LINE('',#108993,#13350) ;
#9235 = LINE('',#108996,#13351) ;
#9236 = LINE('',#109000,#13352) ;
#9237 = LINE('',#109007,#13353) ;
#9238 = LINE('',#109011,#13354) ;
#9239 = LINE('',#109015,#13355) ;
#9240 = LINE('',#109019,#13356) ;
#9241 = LINE('',#109023,#13357) ;
#9242 = LINE('',#109027,#13358) ;
#9243 = LINE('',#109032,#13359) ;
#9244 = LINE('',#109037,#13360) ;
#9245 = LINE('',#109039,#13361) ;
#9246 = LINE('',#109043,#13362) ;
#9247 = LINE('',#109047,#13363) ;
#9248 = LINE('',#109052,#13364) ;
#9249 = LINE('',#109056,#13365) ;
#9250 = LINE('',#109060,#13366) ;
#9251 = LINE('',#109064,#13367) ;
#9252 = LINE('',#109068,#13368) ;
#9253 = LINE('',#109070,#13369) ;
#9254 = LINE('',#109075,#13370) ;
#9255 = LINE('',#109080,#13371) ;
#9256 = LINE('',#109084,#13372) ;
#9257 = LINE('',#109088,#13373) ;
#9258 = LINE('',#109092,#13374) ;
#9259 = LINE('',#109096,#13375) ;
#9260 = LINE('',#109100,#13376) ;
#9261 = LINE('',#109104,#13377) ;
#9262 = LINE('',#109108,#13378) ;
#9263 = LINE('',#109111,#13379) ;
#9264 = LINE('',#109112,#13380) ;
#9265 = LINE('',#109114,#13381) ;
#9266 = LINE('',#109115,#13382) ;
#9267 = LINE('',#109159,#13383) ;
#9268 = LINE('',#109160,#13384) ;
#9269 = LINE('',#109162,#13385) ;
#9270 = LINE('',#109204,#13386) ;
#9271 = LINE('',#109217,#13387) ;
#9272 = LINE('',#109219,#13388) ;
#9273 = LINE('',#109220,#13389) ;
#9274 = LINE('',#109224,#13390) ;
#9275 = LINE('',#109225,#13391) ;
#9276 = LINE('',#109226,#13392) ;
#9277 = LINE('',#109244,#13393) ;
#9278 = LINE('',#109245,#13394) ;
#9279 = LINE('',#109246,#13395) ;
#9280 = LINE('',#109249,#13396) ;
#9281 = LINE('',#109286,#13397) ;
#9282 = LINE('',#109340,#13398) ;
#9283 = LINE('',#109342,#13399) ;
#9284 = LINE('',#109344,#13400) ;
#9285 = LINE('',#109348,#13401) ;
#9286 = LINE('',#109352,#13402) ;
#9287 = LINE('',#109353,#13403) ;
#9288 = LINE('',#109358,#13404) ;
#9289 = LINE('',#109360,#13405) ;
#9290 = LINE('',#109368,#13406) ;
#9291 = LINE('',#109370,#13407) ;
#9292 = LINE('',#109372,#13408) ;
#9293 = LINE('',#109379,#13409) ;
#9294 = LINE('',#109381,#13410) ;
#9295 = LINE('',#109389,#13411) ;
#9296 = LINE('',#109393,#13412) ;
#9297 = LINE('',#109402,#13413) ;
#9298 = LINE('',#109403,#13414) ;
#9299 = LINE('',#109404,#13415) ;
#9300 = LINE('',#109406,#13416) ;
#9301 = LINE('',#109408,#13417) ;
#9302 = LINE('',#109411,#13418) ;
#9303 = LINE('',#109416,#13419) ;
#9304 = LINE('',#109417,#13420) ;
#9305 = LINE('',#109419,#13421) ;
#9306 = LINE('',#109422,#13422) ;
#9307 = LINE('',#109426,#13423) ;
#9308 = LINE('',#109428,#13424) ;
#9309 = LINE('',#109435,#13425) ;
#9310 = LINE('',#109436,#13426) ;
#9311 = LINE('',#109440,#13427) ;
#9312 = LINE('',#109442,#13428) ;
#9313 = LINE('',#109444,#13429) ;
#9314 = LINE('',#109446,#13430) ;
#9315 = LINE('',#109448,#13431) ;
#9316 = LINE('',#109450,#13432) ;
#9317 = LINE('',#109452,#13433) ;
#9318 = LINE('',#109453,#13434) ;
#9319 = LINE('',#109457,#13435) ;
#9320 = LINE('',#109459,#13436) ;
#9321 = LINE('',#109461,#13437) ;
#9322 = LINE('',#109462,#13438) ;
#9323 = LINE('',#109466,#13439) ;
#9324 = LINE('',#109468,#13440) ;
#9325 = LINE('',#109470,#13441) ;
#9326 = LINE('',#109471,#13442) ;
#9327 = LINE('',#109475,#13443) ;
#9328 = LINE('',#109477,#13444) ;
#9329 = LINE('',#109479,#13445) ;
#9330 = LINE('',#109480,#13446) ;
#9331 = LINE('',#109493,#13447) ;
#9332 = LINE('',#109495,#13448) ;
#9333 = LINE('',#109497,#13449) ;
#9334 = LINE('',#109507,#13450) ;
#9335 = LINE('',#109511,#13451) ;
#9336 = LINE('',#109513,#13452) ;
#9337 = LINE('',#109515,#13453) ;
#9338 = LINE('',#109517,#13454) ;
#9339 = LINE('',#109519,#13455) ;
#9340 = LINE('',#109521,#13456) ;
#9341 = LINE('',#109523,#13457) ;
#9342 = LINE('',#109524,#13458) ;
#9343 = LINE('',#109528,#13459) ;
#9344 = LINE('',#109532,#13460) ;
#9345 = LINE('',#109536,#13461) ;
#9346 = LINE('',#109540,#13462) ;
#9347 = LINE('',#109546,#13463) ;
#9348 = LINE('',#109548,#13464) ;
#9349 = LINE('',#109552,#13465) ;
#9350 = LINE('',#109556,#13466) ;
#9351 = LINE('',#109558,#13467) ;
#9352 = LINE('',#109559,#13468) ;
#9353 = LINE('',#109563,#13469) ;
#9354 = LINE('',#109564,#13470) ;
#9355 = LINE('',#109565,#13471) ;
#9356 = LINE('',#109571,#13472) ;
#9357 = LINE('',#109574,#13473) ;
#9358 = LINE('',#109580,#13474) ;
#9359 = LINE('',#109583,#13475) ;
#9360 = LINE('',#109586,#13476) ;
#9361 = LINE('',#109588,#13477) ;
#9362 = LINE('',#109589,#13478) ;
#9363 = LINE('',#109593,#13479) ;
#9364 = LINE('',#109594,#13480) ;
#9365 = LINE('',#109595,#13481) ;
#9366 = LINE('',#109600,#13482) ;
#9367 = LINE('',#109602,#13483) ;
#9368 = LINE('',#109607,#13484) ;
#9369 = LINE('',#109612,#13485) ;
#9370 = LINE('',#109614,#13486) ;
#9371 = LINE('',#109615,#13487) ;
#9372 = LINE('',#109619,#13488) ;
#9373 = LINE('',#109620,#13489) ;
#9374 = LINE('',#109621,#13490) ;
#9375 = LINE('',#109627,#13491) ;
#9376 = LINE('',#109630,#13492) ;
#9377 = LINE('',#109634,#13493) ;
#9378 = LINE('',#109636,#13494) ;
#9379 = LINE('',#109638,#13495) ;
#9380 = LINE('',#109639,#13496) ;
#9381 = LINE('',#109645,#13497) ;
#9382 = LINE('',#109648,#13498) ;
#9383 = LINE('',#109651,#13499) ;
#9384 = LINE('',#109653,#13500) ;
#9385 = LINE('',#109654,#13501) ;
#9386 = LINE('',#109658,#13502) ;
#9387 = LINE('',#109660,#13503) ;
#9388 = LINE('',#109662,#13504) ;
#9389 = LINE('',#109663,#13505) ;
#9390 = LINE('',#109667,#13506) ;
#9391 = LINE('',#109668,#13507) ;
#9392 = LINE('',#109670,#13508) ;
#9393 = LINE('',#109675,#13509) ;
#9394 = LINE('',#109677,#13510) ;
#9395 = LINE('',#109679,#13511) ;
#9396 = LINE('',#109680,#13512) ;
#9397 = LINE('',#109685,#13513) ;
#9398 = LINE('',#109687,#13514) ;
#9399 = LINE('',#109691,#13515) ;
#9400 = LINE('',#109694,#13516) ;
#9401 = LINE('',#109698,#13517) ;
#9402 = LINE('',#109699,#13518) ;
#9403 = LINE('',#109701,#13519) ;
#9404 = LINE('',#109702,#13520) ;
#9405 = LINE('',#109706,#13521) ;
#9406 = LINE('',#109708,#13522) ;
#9407 = LINE('',#109710,#13523) ;
#9408 = LINE('',#109711,#13524) ;
#9409 = LINE('',#109715,#13525) ;
#9410 = LINE('',#109717,#13526) ;
#9411 = LINE('',#109719,#13527) ;
#9412 = LINE('',#109720,#13528) ;
#9413 = LINE('',#109724,#13529) ;
#9414 = LINE('',#109726,#13530) ;
#9415 = LINE('',#109728,#13531) ;
#9416 = LINE('',#109729,#13532) ;
#9417 = LINE('',#109732,#13533) ;
#9418 = LINE('',#109734,#13534) ;
#9419 = LINE('',#109735,#13535) ;
#9420 = LINE('',#109738,#13536) ;
#9421 = LINE('',#109740,#13537) ;
#9422 = LINE('',#109741,#13538) ;
#9423 = LINE('',#109744,#13539) ;
#9424 = LINE('',#109746,#13540) ;
#9425 = LINE('',#109747,#13541) ;
#9426 = LINE('',#109750,#13542) ;
#9427 = LINE('',#109752,#13543) ;
#9428 = LINE('',#109753,#13544) ;
#9429 = LINE('',#109757,#13545) ;
#9430 = LINE('',#109759,#13546) ;
#9431 = LINE('',#109761,#13547) ;
#9432 = LINE('',#109765,#13548) ;
#9433 = LINE('',#109770,#13549) ;
#9434 = LINE('',#109772,#13550) ;
#9435 = LINE('',#109774,#13551) ;
#9436 = LINE('',#109778,#13552) ;
#9437 = LINE('',#109783,#13553) ;
#9438 = LINE('',#109788,#13554) ;
#9439 = LINE('',#109790,#13555) ;
#9440 = LINE('',#109791,#13556) ;
#9441 = LINE('',#109795,#13557) ;
#9442 = LINE('',#109797,#13558) ;
#9443 = LINE('',#109799,#13559) ;
#9444 = LINE('',#109800,#13560) ;
#9445 = LINE('',#109804,#13561) ;
#9446 = LINE('',#109806,#13562) ;
#9447 = LINE('',#109808,#13563) ;
#9448 = LINE('',#109809,#13564) ;
#9449 = LINE('',#109813,#13565) ;
#9450 = LINE('',#109815,#13566) ;
#9451 = LINE('',#109817,#13567) ;
#9452 = LINE('',#109818,#13568) ;
#9453 = LINE('',#109822,#13569) ;
#9454 = LINE('',#109824,#13570) ;
#9455 = LINE('',#109826,#13571) ;
#9456 = LINE('',#109827,#13572) ;
#9457 = LINE('',#109834,#13573) ;
#9458 = LINE('',#109836,#13574) ;
#9459 = LINE('',#109838,#13575) ;
#9460 = LINE('',#109839,#13576) ;
#9461 = LINE('',#109843,#13577) ;
#9462 = LINE('',#109845,#13578) ;
#9463 = LINE('',#109847,#13579) ;
#9464 = LINE('',#109848,#13580) ;
#9465 = LINE('',#109852,#13581) ;
#9466 = LINE('',#109854,#13582) ;
#9467 = LINE('',#109856,#13583) ;
#9468 = LINE('',#109857,#13584) ;
#9469 = LINE('',#109861,#13585) ;
#9470 = LINE('',#109863,#13586) ;
#9471 = LINE('',#109865,#13587) ;
#9472 = LINE('',#109866,#13588) ;
#9473 = LINE('',#109869,#13589) ;
#9474 = LINE('',#109872,#13590) ;
#9475 = LINE('',#109881,#13591) ;
#9476 = LINE('',#109884,#13592) ;
#9477 = LINE('',#110065,#13593) ;
#9478 = LINE('',#110110,#13594) ;
#9479 = LINE('',#110118,#13595) ;
#9480 = LINE('',#110139,#13596) ;
#9481 = LINE('',#110145,#13597) ;
#9482 = LINE('',#110158,#13598) ;
#9483 = LINE('',#111324,#13599) ;
#9484 = LINE('',#111329,#13600) ;
#9485 = LINE('',#111335,#13601) ;
#9486 = LINE('',#111338,#13602) ;
#9487 = LINE('',#111349,#13603) ;
#9488 = LINE('',#111352,#13604) ;
#9489 = LINE('',#111371,#13605) ;
#9490 = LINE('',#111375,#13606) ;
#9491 = LINE('',#111377,#13607) ;
#9492 = LINE('',#111386,#13608) ;
#9493 = LINE('',#111389,#13609) ;
#9494 = LINE('',#111393,#13610) ;
#9495 = LINE('',#111395,#13611) ;
#9496 = LINE('',#111437,#13612) ;
#9497 = LINE('',#111438,#13613) ;
#9498 = LINE('',#111442,#13614) ;
#9499 = LINE('',#111444,#13615) ;
#9500 = LINE('',#111446,#13616) ;
#9501 = LINE('',#111447,#13617) ;
#9502 = LINE('',#111451,#13618) ;
#9503 = LINE('',#111474,#13619) ;
#9504 = LINE('',#111476,#13620) ;
#9505 = LINE('',#111477,#13621) ;
#9506 = LINE('',#111481,#13622) ;
#9507 = LINE('',#111483,#13623) ;
#9508 = LINE('',#111485,#13624) ;
#9509 = LINE('',#111486,#13625) ;
#9510 = LINE('',#111490,#13626) ;
#9511 = LINE('',#111492,#13627) ;
#9512 = LINE('',#111494,#13628) ;
#9513 = LINE('',#111495,#13629) ;
#9514 = LINE('',#111499,#13630) ;
#9515 = LINE('',#111501,#13631) ;
#9516 = LINE('',#111503,#13632) ;
#9517 = LINE('',#111505,#13633) ;
#9518 = LINE('',#111508,#13634) ;
#9519 = LINE('',#111512,#13635) ;
#9520 = LINE('',#111519,#13636) ;
#9521 = LINE('',#111523,#13637) ;
#9522 = LINE('',#111527,#13638) ;
#9523 = LINE('',#111531,#13639) ;
#9524 = LINE('',#111535,#13640) ;
#9525 = LINE('',#111539,#13641) ;
#9526 = LINE('',#111544,#13642) ;
#9527 = LINE('',#111549,#13643) ;
#9528 = LINE('',#111551,#13644) ;
#9529 = LINE('',#111555,#13645) ;
#9530 = LINE('',#111559,#13646) ;
#9531 = LINE('',#111564,#13647) ;
#9532 = LINE('',#111568,#13648) ;
#9533 = LINE('',#111572,#13649) ;
#9534 = LINE('',#111576,#13650) ;
#9535 = LINE('',#111580,#13651) ;
#9536 = LINE('',#111582,#13652) ;
#9537 = LINE('',#111587,#13653) ;
#9538 = LINE('',#111592,#13654) ;
#9539 = LINE('',#111596,#13655) ;
#9540 = LINE('',#111600,#13656) ;
#9541 = LINE('',#111604,#13657) ;
#9542 = LINE('',#111608,#13658) ;
#9543 = LINE('',#111612,#13659) ;
#9544 = LINE('',#111616,#13660) ;
#9545 = LINE('',#111620,#13661) ;
#9546 = LINE('',#111623,#13662) ;
#9547 = LINE('',#111624,#13663) ;
#9548 = LINE('',#111626,#13664) ;
#9549 = LINE('',#111627,#13665) ;
#9550 = LINE('',#111671,#13666) ;
#9551 = LINE('',#111672,#13667) ;
#9552 = LINE('',#111674,#13668) ;
#9553 = LINE('',#111716,#13669) ;
#9554 = LINE('',#111729,#13670) ;
#9555 = LINE('',#111731,#13671) ;
#9556 = LINE('',#111732,#13672) ;
#9557 = LINE('',#111736,#13673) ;
#9558 = LINE('',#111737,#13674) ;
#9559 = LINE('',#111738,#13675) ;
#9560 = LINE('',#111756,#13676) ;
#9561 = LINE('',#111757,#13677) ;
#9562 = LINE('',#111758,#13678) ;
#9563 = LINE('',#111761,#13679) ;
#9564 = LINE('',#111798,#13680) ;
#9565 = LINE('',#111852,#13681) ;
#9566 = LINE('',#111854,#13682) ;
#9567 = LINE('',#111856,#13683) ;
#9568 = LINE('',#111860,#13684) ;
#9569 = LINE('',#111864,#13685) ;
#9570 = LINE('',#111865,#13686) ;
#9571 = LINE('',#111870,#13687) ;
#9572 = LINE('',#111872,#13688) ;
#9573 = LINE('',#111880,#13689) ;
#9574 = LINE('',#111882,#13690) ;
#9575 = LINE('',#111884,#13691) ;
#9576 = LINE('',#111891,#13692) ;
#9577 = LINE('',#111893,#13693) ;
#9578 = LINE('',#111901,#13694) ;
#9579 = LINE('',#111905,#13695) ;
#9580 = LINE('',#111914,#13696) ;
#9581 = LINE('',#111915,#13697) ;
#9582 = LINE('',#111916,#13698) ;
#9583 = LINE('',#111918,#13699) ;
#9584 = LINE('',#111920,#13700) ;
#9585 = LINE('',#111923,#13701) ;
#9586 = LINE('',#111928,#13702) ;
#9587 = LINE('',#111929,#13703) ;
#9588 = LINE('',#111931,#13704) ;
#9589 = LINE('',#111934,#13705) ;
#9590 = LINE('',#111938,#13706) ;
#9591 = LINE('',#111940,#13707) ;
#9592 = LINE('',#111947,#13708) ;
#9593 = LINE('',#111948,#13709) ;
#9594 = LINE('',#111952,#13710) ;
#9595 = LINE('',#111954,#13711) ;
#9596 = LINE('',#111956,#13712) ;
#9597 = LINE('',#111958,#13713) ;
#9598 = LINE('',#111960,#13714) ;
#9599 = LINE('',#111962,#13715) ;
#9600 = LINE('',#111964,#13716) ;
#9601 = LINE('',#111965,#13717) ;
#9602 = LINE('',#111969,#13718) ;
#9603 = LINE('',#111971,#13719) ;
#9604 = LINE('',#111973,#13720) ;
#9605 = LINE('',#111974,#13721) ;
#9606 = LINE('',#111978,#13722) ;
#9607 = LINE('',#111980,#13723) ;
#9608 = LINE('',#111982,#13724) ;
#9609 = LINE('',#111983,#13725) ;
#9610 = LINE('',#111987,#13726) ;
#9611 = LINE('',#111989,#13727) ;
#9612 = LINE('',#111991,#13728) ;
#9613 = LINE('',#111992,#13729) ;
#9614 = LINE('',#112005,#13730) ;
#9615 = LINE('',#112007,#13731) ;
#9616 = LINE('',#112009,#13732) ;
#9617 = LINE('',#112019,#13733) ;
#9618 = LINE('',#112023,#13734) ;
#9619 = LINE('',#112025,#13735) ;
#9620 = LINE('',#112027,#13736) ;
#9621 = LINE('',#112029,#13737) ;
#9622 = LINE('',#112031,#13738) ;
#9623 = LINE('',#112033,#13739) ;
#9624 = LINE('',#112035,#13740) ;
#9625 = LINE('',#112036,#13741) ;
#9626 = LINE('',#112040,#13742) ;
#9627 = LINE('',#112044,#13743) ;
#9628 = LINE('',#112048,#13744) ;
#9629 = LINE('',#112052,#13745) ;
#9630 = LINE('',#112058,#13746) ;
#9631 = LINE('',#112060,#13747) ;
#9632 = LINE('',#112064,#13748) ;
#9633 = LINE('',#112068,#13749) ;
#9634 = LINE('',#112070,#13750) ;
#9635 = LINE('',#112071,#13751) ;
#9636 = LINE('',#112075,#13752) ;
#9637 = LINE('',#112076,#13753) ;
#9638 = LINE('',#112077,#13754) ;
#9639 = LINE('',#112083,#13755) ;
#9640 = LINE('',#112086,#13756) ;
#9641 = LINE('',#112092,#13757) ;
#9642 = LINE('',#112095,#13758) ;
#9643 = LINE('',#112098,#13759) ;
#9644 = LINE('',#112100,#13760) ;
#9645 = LINE('',#112101,#13761) ;
#9646 = LINE('',#112105,#13762) ;
#9647 = LINE('',#112106,#13763) ;
#9648 = LINE('',#112107,#13764) ;
#9649 = LINE('',#112112,#13765) ;
#9650 = LINE('',#112114,#13766) ;
#9651 = LINE('',#112119,#13767) ;
#9652 = LINE('',#112124,#13768) ;
#9653 = LINE('',#112126,#13769) ;
#9654 = LINE('',#112127,#13770) ;
#9655 = LINE('',#112131,#13771) ;
#9656 = LINE('',#112132,#13772) ;
#9657 = LINE('',#112133,#13773) ;
#9658 = LINE('',#112139,#13774) ;
#9659 = LINE('',#112142,#13775) ;
#9660 = LINE('',#112146,#13776) ;
#9661 = LINE('',#112148,#13777) ;
#9662 = LINE('',#112150,#13778) ;
#9663 = LINE('',#112151,#13779) ;
#9664 = LINE('',#112157,#13780) ;
#9665 = LINE('',#112160,#13781) ;
#9666 = LINE('',#112163,#13782) ;
#9667 = LINE('',#112165,#13783) ;
#9668 = LINE('',#112166,#13784) ;
#9669 = LINE('',#112170,#13785) ;
#9670 = LINE('',#112172,#13786) ;
#9671 = LINE('',#112174,#13787) ;
#9672 = LINE('',#112175,#13788) ;
#9673 = LINE('',#112179,#13789) ;
#9674 = LINE('',#112180,#13790) ;
#9675 = LINE('',#112182,#13791) ;
#9676 = LINE('',#112187,#13792) ;
#9677 = LINE('',#112189,#13793) ;
#9678 = LINE('',#112191,#13794) ;
#9679 = LINE('',#112192,#13795) ;
#9680 = LINE('',#112197,#13796) ;
#9681 = LINE('',#112199,#13797) ;
#9682 = LINE('',#112203,#13798) ;
#9683 = LINE('',#112206,#13799) ;
#9684 = LINE('',#112210,#13800) ;
#9685 = LINE('',#112211,#13801) ;
#9686 = LINE('',#112213,#13802) ;
#9687 = LINE('',#112214,#13803) ;
#9688 = LINE('',#112218,#13804) ;
#9689 = LINE('',#112220,#13805) ;
#9690 = LINE('',#112222,#13806) ;
#9691 = LINE('',#112223,#13807) ;
#9692 = LINE('',#112227,#13808) ;
#9693 = LINE('',#112229,#13809) ;
#9694 = LINE('',#112231,#13810) ;
#9695 = LINE('',#112232,#13811) ;
#9696 = LINE('',#112236,#13812) ;
#9697 = LINE('',#112238,#13813) ;
#9698 = LINE('',#112240,#13814) ;
#9699 = LINE('',#112241,#13815) ;
#9700 = LINE('',#112244,#13816) ;
#9701 = LINE('',#112246,#13817) ;
#9702 = LINE('',#112247,#13818) ;
#9703 = LINE('',#112250,#13819) ;
#9704 = LINE('',#112252,#13820) ;
#9705 = LINE('',#112253,#13821) ;
#9706 = LINE('',#112256,#13822) ;
#9707 = LINE('',#112258,#13823) ;
#9708 = LINE('',#112259,#13824) ;
#9709 = LINE('',#112262,#13825) ;
#9710 = LINE('',#112264,#13826) ;
#9711 = LINE('',#112265,#13827) ;
#9712 = LINE('',#112269,#13828) ;
#9713 = LINE('',#112271,#13829) ;
#9714 = LINE('',#112273,#13830) ;
#9715 = LINE('',#112277,#13831) ;
#9716 = LINE('',#112282,#13832) ;
#9717 = LINE('',#112284,#13833) ;
#9718 = LINE('',#112286,#13834) ;
#9719 = LINE('',#112290,#13835) ;
#9720 = LINE('',#112295,#13836) ;
#9721 = LINE('',#112300,#13837) ;
#9722 = LINE('',#112302,#13838) ;
#9723 = LINE('',#112303,#13839) ;
#9724 = LINE('',#112307,#13840) ;
#9725 = LINE('',#112309,#13841) ;
#9726 = LINE('',#112311,#13842) ;
#9727 = LINE('',#112312,#13843) ;
#9728 = LINE('',#112316,#13844) ;
#9729 = LINE('',#112318,#13845) ;
#9730 = LINE('',#112320,#13846) ;
#9731 = LINE('',#112321,#13847) ;
#9732 = LINE('',#112325,#13848) ;
#9733 = LINE('',#112327,#13849) ;
#9734 = LINE('',#112329,#13850) ;
#9735 = LINE('',#112330,#13851) ;
#9736 = LINE('',#112334,#13852) ;
#9737 = LINE('',#112336,#13853) ;
#9738 = LINE('',#112338,#13854) ;
#9739 = LINE('',#112339,#13855) ;
#9740 = LINE('',#112346,#13856) ;
#9741 = LINE('',#112348,#13857) ;
#9742 = LINE('',#112350,#13858) ;
#9743 = LINE('',#112351,#13859) ;
#9744 = LINE('',#112355,#13860) ;
#9745 = LINE('',#112357,#13861) ;
#9746 = LINE('',#112359,#13862) ;
#9747 = LINE('',#112360,#13863) ;
#9748 = LINE('',#112364,#13864) ;
#9749 = LINE('',#112366,#13865) ;
#9750 = LINE('',#112368,#13866) ;
#9751 = LINE('',#112369,#13867) ;
#9752 = LINE('',#112373,#13868) ;
#9753 = LINE('',#112375,#13869) ;
#9754 = LINE('',#112377,#13870) ;
#9755 = LINE('',#112378,#13871) ;
#9756 = LINE('',#112381,#13872) ;
#9757 = LINE('',#112384,#13873) ;
#9758 = LINE('',#112393,#13874) ;
#9759 = LINE('',#112396,#13875) ;
#9760 = LINE('',#112577,#13876) ;
#9761 = LINE('',#112622,#13877) ;
#9762 = LINE('',#112630,#13878) ;
#9763 = LINE('',#112651,#13879) ;
#9764 = LINE('',#112657,#13880) ;
#9765 = LINE('',#112670,#13881) ;
#9766 = LINE('',#113750,#13882) ;
#9767 = LINE('',#113759,#13883) ;
#9768 = LINE('',#113762,#13884) ;
#9769 = LINE('',#113768,#13885) ;
#9770 = LINE('',#113770,#13886) ;
#9771 = LINE('',#113774,#13887) ;
#9772 = LINE('',#113776,#13888) ;
#9773 = LINE('',#113777,#13889) ;
#9774 = LINE('',#113781,#13890) ;
#9775 = LINE('',#113783,#13891) ;
#9776 = LINE('',#113787,#13892) ;
#9777 = LINE('',#113789,#13893) ;
#9778 = LINE('',#113791,#13894) ;
#9779 = LINE('',#113794,#13895) ;
#9780 = LINE('',#113795,#13896) ;
#9781 = LINE('',#113799,#13897) ;
#9782 = LINE('',#113801,#13898) ;
#9783 = LINE('',#113805,#13899) ;
#9784 = LINE('',#113807,#13900) ;
#9785 = LINE('',#113809,#13901) ;
#9786 = LINE('',#113814,#13902) ;
#9787 = LINE('',#113815,#13903) ;
#9788 = LINE('',#113816,#13904) ;
#9789 = LINE('',#113822,#13905) ;
#9790 = LINE('',#113824,#13906) ;
#9791 = LINE('',#113827,#13907) ;
#9792 = LINE('',#113828,#13908) ;
#9793 = LINE('',#113830,#13909) ;
#9794 = LINE('',#113831,#13910) ;
#9795 = LINE('',#113834,#13911) ;
#9796 = LINE('',#113835,#13912) ;
#9797 = LINE('',#113838,#13913) ;
#9798 = LINE('',#113840,#13914) ;
#9799 = LINE('',#113842,#13915) ;
#9800 = LINE('',#113844,#13916) ;
#9801 = LINE('',#113846,#13917) ;
#9802 = LINE('',#113847,#13918) ;
#9803 = LINE('',#113848,#13919) ;
#9804 = LINE('',#113850,#13920) ;
#9805 = LINE('',#113851,#13921) ;
#9806 = LINE('',#113887,#13922) ;
#9807 = LINE('',#113891,#13923) ;
#9808 = LINE('',#113893,#13924) ;
#9809 = LINE('',#113930,#13925) ;
#9810 = LINE('',#113934,#13926) ;
#9811 = LINE('',#113936,#13927) ;
#9812 = LINE('',#113973,#13928) ;
#9813 = LINE('',#113977,#13929) ;
#9814 = LINE('',#113979,#13930) ;
#9815 = LINE('',#114016,#13931) ;
#9816 = LINE('',#114020,#13932) ;
#9817 = LINE('',#114022,#13933) ;
#9818 = LINE('',#114059,#13934) ;
#9819 = LINE('',#114063,#13935) ;
#9820 = LINE('',#114065,#13936) ;
#9821 = LINE('',#114102,#13937) ;
#9822 = LINE('',#114106,#13938) ;
#9823 = LINE('',#114108,#13939) ;
#9824 = LINE('',#114145,#13940) ;
#9825 = LINE('',#114149,#13941) ;
#9826 = LINE('',#114151,#13942) ;
#9827 = LINE('',#114188,#13943) ;
#9828 = LINE('',#114192,#13944) ;
#9829 = LINE('',#114194,#13945) ;
#9830 = LINE('',#114312,#13946) ;
#9831 = LINE('',#114316,#13947) ;
#9832 = LINE('',#114318,#13948) ;
#9833 = LINE('',#114328,#13949) ;
#9834 = LINE('',#114330,#13950) ;
#9835 = LINE('',#114332,#13951) ;
#9836 = LINE('',#114334,#13952) ;
#9837 = LINE('',#114336,#13953) ;
#9838 = LINE('',#114338,#13954) ;
#9839 = LINE('',#114340,#13955) ;
#9840 = LINE('',#114342,#13956) ;
#9841 = LINE('',#114344,#13957) ;
#9842 = LINE('',#114349,#13958) ;
#9843 = LINE('',#114350,#13959) ;
#9844 = LINE('',#114355,#13960) ;
#9845 = LINE('',#114356,#13961) ;
#9846 = LINE('',#114361,#13962) ;
#9847 = LINE('',#114362,#13963) ;
#9848 = LINE('',#114367,#13964) ;
#9849 = LINE('',#114368,#13965) ;
#9850 = LINE('',#114373,#13966) ;
#9851 = LINE('',#114374,#13967) ;
#9852 = LINE('',#114379,#13968) ;
#9853 = LINE('',#114380,#13969) ;
#9854 = LINE('',#114385,#13970) ;
#9855 = LINE('',#114386,#13971) ;
#9856 = LINE('',#114391,#13972) ;
#9857 = LINE('',#114392,#13973) ;
#9858 = LINE('',#114397,#13974) ;
#9859 = LINE('',#114398,#13975) ;
#9860 = LINE('',#114436,#13976) ;
#9861 = LINE('',#114440,#13977) ;
#9862 = LINE('',#114442,#13978) ;
#9863 = LINE('',#114452,#13979) ;
#9864 = LINE('',#114457,#13980) ;
#9865 = LINE('',#114458,#13981) ;
#9866 = LINE('',#114462,#13982) ;
#9867 = LINE('',#114466,#13983) ;
#9868 = LINE('',#114471,#13984) ;
#9869 = LINE('',#114473,#13985) ;
#9870 = LINE('',#114475,#13986) ;
#9871 = LINE('',#114477,#13987) ;
#9872 = LINE('',#114479,#13988) ;
#9873 = LINE('',#114484,#13989) ;
#9874 = LINE('',#114488,#13990) ;
#9875 = LINE('',#114493,#13991) ;
#9876 = LINE('',#114495,#13992) ;
#9877 = LINE('',#114497,#13993) ;
#9878 = LINE('',#114499,#13994) ;
#9879 = LINE('',#114501,#13995) ;
#9880 = LINE('',#114506,#13996) ;
#9881 = LINE('',#114510,#13997) ;
#9882 = LINE('',#114515,#13998) ;
#9883 = LINE('',#114517,#13999) ;
#9884 = LINE('',#114519,#14000) ;
#9885 = LINE('',#114521,#14001) ;
#9886 = LINE('',#114523,#14002) ;
#9887 = LINE('',#114528,#14003) ;
#9888 = LINE('',#114532,#14004) ;
#9889 = LINE('',#114537,#14005) ;
#9890 = LINE('',#114539,#14006) ;
#9891 = LINE('',#114541,#14007) ;
#9892 = LINE('',#114543,#14008) ;
#9893 = LINE('',#114545,#14009) ;
#9894 = LINE('',#114550,#14010) ;
#9895 = LINE('',#114554,#14011) ;
#9896 = LINE('',#114559,#14012) ;
#9897 = LINE('',#114561,#14013) ;
#9898 = LINE('',#114563,#14014) ;
#9899 = LINE('',#114565,#14015) ;
#9900 = LINE('',#114567,#14016) ;
#9901 = LINE('',#114572,#14017) ;
#9902 = LINE('',#114576,#14018) ;
#9903 = LINE('',#114581,#14019) ;
#9904 = LINE('',#114583,#14020) ;
#9905 = LINE('',#114585,#14021) ;
#9906 = LINE('',#114587,#14022) ;
#9907 = LINE('',#114589,#14023) ;
#9908 = LINE('',#114594,#14024) ;
#9909 = LINE('',#114598,#14025) ;
#9910 = LINE('',#114603,#14026) ;
#9911 = LINE('',#114605,#14027) ;
#9912 = LINE('',#114607,#14028) ;
#9913 = LINE('',#114609,#14029) ;
#9914 = LINE('',#114611,#14030) ;
#9915 = LINE('',#114616,#14031) ;
#9916 = LINE('',#114620,#14032) ;
#9917 = LINE('',#114625,#14033) ;
#9918 = LINE('',#114627,#14034) ;
#9919 = LINE('',#114629,#14035) ;
#9920 = LINE('',#114631,#14036) ;
#9921 = LINE('',#114633,#14037) ;
#9922 = LINE('',#114638,#14038) ;
#9923 = LINE('',#114642,#14039) ;
#9924 = LINE('',#114647,#14040) ;
#9925 = LINE('',#114649,#14041) ;
#9926 = LINE('',#114651,#14042) ;
#9927 = LINE('',#114653,#14043) ;
#9928 = LINE('',#114655,#14044) ;
#9929 = LINE('',#114662,#14045) ;
#9930 = LINE('',#114664,#14046) ;
#9931 = LINE('',#114666,#14047) ;
#9932 = LINE('',#114667,#14048) ;
#9933 = LINE('',#114673,#14049) ;
#9934 = LINE('',#114675,#14050) ;
#9935 = LINE('',#114677,#14051) ;
#9936 = LINE('',#114678,#14052) ;
#9937 = LINE('',#114684,#14053) ;
#9938 = LINE('',#114686,#14054) ;
#9939 = LINE('',#114688,#14055) ;
#9940 = LINE('',#114689,#14056) ;
#9941 = LINE('',#114695,#14057) ;
#9942 = LINE('',#114697,#14058) ;
#9943 = LINE('',#114699,#14059) ;
#9944 = LINE('',#114700,#14060) ;
#9945 = LINE('',#114706,#14061) ;
#9946 = LINE('',#114708,#14062) ;
#9947 = LINE('',#114710,#14063) ;
#9948 = LINE('',#114711,#14064) ;
#9949 = LINE('',#114717,#14065) ;
#9950 = LINE('',#114719,#14066) ;
#9951 = LINE('',#114721,#14067) ;
#9952 = LINE('',#114722,#14068) ;
#9953 = LINE('',#114728,#14069) ;
#9954 = LINE('',#114730,#14070) ;
#9955 = LINE('',#114732,#14071) ;
#9956 = LINE('',#114733,#14072) ;
#9957 = LINE('',#114739,#14073) ;
#9958 = LINE('',#114741,#14074) ;
#9959 = LINE('',#114743,#14075) ;
#9960 = LINE('',#114744,#14076) ;
#9961 = LINE('',#114750,#14077) ;
#9962 = LINE('',#114752,#14078) ;
#9963 = LINE('',#114754,#14079) ;
#9964 = LINE('',#114755,#14080) ;
#9965 = LINE('',#114761,#14081) ;
#9966 = LINE('',#114763,#14082) ;
#9967 = LINE('',#114765,#14083) ;
#9968 = LINE('',#114766,#14084) ;
#9969 = LINE('',#114772,#14085) ;
#9970 = LINE('',#114774,#14086) ;
#9971 = LINE('',#114776,#14087) ;
#9972 = LINE('',#114777,#14088) ;
#9973 = LINE('',#114783,#14089) ;
#9974 = LINE('',#114785,#14090) ;
#9975 = LINE('',#114787,#14091) ;
#9976 = LINE('',#114788,#14092) ;
#9977 = LINE('',#114794,#14093) ;
#9978 = LINE('',#114796,#14094) ;
#9979 = LINE('',#114798,#14095) ;
#9980 = LINE('',#114799,#14096) ;
#9981 = LINE('',#114805,#14097) ;
#9982 = LINE('',#114807,#14098) ;
#9983 = LINE('',#114809,#14099) ;
#9984 = LINE('',#114810,#14100) ;
#9985 = LINE('',#114816,#14101) ;
#9986 = LINE('',#114818,#14102) ;
#9987 = LINE('',#114820,#14103) ;
#9988 = LINE('',#114821,#14104) ;
#9989 = LINE('',#114827,#14105) ;
#9990 = LINE('',#114829,#14106) ;
#9991 = LINE('',#114831,#14107) ;
#9992 = LINE('',#114832,#14108) ;
#9993 = LINE('',#114838,#14109) ;
#9994 = LINE('',#114840,#14110) ;
#9995 = LINE('',#114842,#14111) ;
#9996 = LINE('',#114843,#14112) ;
#9997 = LINE('',#114849,#14113) ;
#9998 = LINE('',#114851,#14114) ;
#9999 = LINE('',#114853,#14115) ;
#10000 = LINE('',#114854,#14116) ;
#10001 = LINE('',#114858,#14117) ;
#10002 = LINE('',#114862,#14118) ;
#10003 = LINE('',#114867,#14119) ;
#10004 = LINE('',#114871,#14120) ;
#10005 = LINE('',#114876,#14121) ;
#10006 = LINE('',#114880,#14122) ;
#10007 = LINE('',#114885,#14123) ;
#10008 = LINE('',#114889,#14124) ;
#10009 = LINE('',#114894,#14125) ;
#10010 = LINE('',#114898,#14126) ;
#10011 = LINE('',#114903,#14127) ;
#10012 = LINE('',#114907,#14128) ;
#10013 = LINE('',#114912,#14129) ;
#10014 = LINE('',#114916,#14130) ;
#10015 = LINE('',#114921,#14131) ;
#10016 = LINE('',#114925,#14132) ;
#10017 = LINE('',#114930,#14133) ;
#10018 = LINE('',#114934,#14134) ;
#10019 = LINE('',#114939,#14135) ;
#10020 = LINE('',#114943,#14136) ;
#10021 = LINE('',#114948,#14137) ;
#10022 = LINE('',#114950,#14138) ;
#10023 = LINE('',#114952,#14139) ;
#10024 = LINE('',#114954,#14140) ;
#10025 = LINE('',#114956,#14141) ;
#10026 = LINE('',#114963,#14142) ;
#10027 = LINE('',#114965,#14143) ;
#10028 = LINE('',#114967,#14144) ;
#10029 = LINE('',#114968,#14145) ;
#10030 = LINE('',#114974,#14146) ;
#10031 = LINE('',#114976,#14147) ;
#10032 = LINE('',#114978,#14148) ;
#10033 = LINE('',#114979,#14149) ;
#10034 = LINE('',#114983,#14150) ;
#10035 = LINE('',#114987,#14151) ;
#10036 = LINE('',#114992,#14152) ;
#10037 = LINE('',#114996,#14153) ;
#10038 = LINE('',#115003,#14154) ;
#10039 = LINE('',#115005,#14155) ;
#10040 = LINE('',#115006,#14156) ;
#10041 = LINE('',#115007,#14157) ;
#10042 = LINE('',#115009,#14158) ;
#10043 = LINE('',#115013,#14159) ;
#10044 = LINE('',#115016,#14160) ;
#10045 = LINE('',#115018,#14161) ;
#10046 = LINE('',#115022,#14162) ;
#10047 = LINE('',#115025,#14163) ;
#10048 = LINE('',#115027,#14164) ;
#10049 = LINE('',#115031,#14165) ;
#10050 = LINE('',#115034,#14166) ;
#10051 = LINE('',#115036,#14167) ;
#10052 = LINE('',#115040,#14168) ;
#10053 = LINE('',#115043,#14169) ;
#10054 = LINE('',#115045,#14170) ;
#10055 = LINE('',#115049,#14171) ;
#10056 = LINE('',#115052,#14172) ;
#10057 = LINE('',#115054,#14173) ;
#10058 = LINE('',#115058,#14174) ;
#10059 = LINE('',#115061,#14175) ;
#10060 = LINE('',#115063,#14176) ;
#10061 = LINE('',#115067,#14177) ;
#10062 = LINE('',#115070,#14178) ;
#10063 = LINE('',#115072,#14179) ;
#10064 = LINE('',#115076,#14180) ;
#10065 = LINE('',#115079,#14181) ;
#10066 = LINE('',#115081,#14182) ;
#10067 = LINE('',#115085,#14183) ;
#10068 = LINE('',#115088,#14184) ;
#10069 = LINE('',#115090,#14185) ;
#10070 = LINE('',#115093,#14186) ;
#10071 = LINE('',#115098,#14187) ;
#10072 = LINE('',#115104,#14188) ;
#10073 = LINE('',#115106,#14189) ;
#10074 = LINE('',#115110,#14190) ;
#10075 = LINE('',#115113,#14191) ;
#10076 = LINE('',#115115,#14192) ;
#10077 = LINE('',#115119,#14193) ;
#10078 = LINE('',#115122,#14194) ;
#10079 = LINE('',#115124,#14195) ;
#10080 = LINE('',#115128,#14196) ;
#10081 = LINE('',#115131,#14197) ;
#10082 = LINE('',#115133,#14198) ;
#10083 = LINE('',#115137,#14199) ;
#10084 = LINE('',#115140,#14200) ;
#10085 = LINE('',#115142,#14201) ;
#10086 = LINE('',#115146,#14202) ;
#10087 = LINE('',#115149,#14203) ;
#10088 = LINE('',#115151,#14204) ;
#10089 = LINE('',#115155,#14205) ;
#10090 = LINE('',#115158,#14206) ;
#10091 = LINE('',#115160,#14207) ;
#10092 = LINE('',#115164,#14208) ;
#10093 = LINE('',#115167,#14209) ;
#10094 = LINE('',#115169,#14210) ;
#10095 = LINE('',#115173,#14211) ;
#10096 = LINE('',#115176,#14212) ;
#10097 = LINE('',#115178,#14213) ;
#10098 = LINE('',#115182,#14214) ;
#10099 = LINE('',#115185,#14215) ;
#10100 = LINE('',#115187,#14216) ;
#10101 = LINE('',#115189,#14217) ;
#10102 = LINE('',#115190,#14218) ;
#10103 = LINE('',#115192,#14219) ;
#10104 = LINE('',#115195,#14220) ;
#10105 = LINE('',#115199,#14221) ;
#10106 = LINE('',#115205,#14222) ;
#10107 = LINE('',#115206,#14223) ;
#10108 = LINE('',#115207,#14224) ;
#10109 = LINE('',#115211,#14225) ;
#10110 = LINE('',#115217,#14226) ;
#10111 = LINE('',#115218,#14227) ;
#10112 = LINE('',#115219,#14228) ;
#10113 = LINE('',#115223,#14229) ;
#10114 = LINE('',#115229,#14230) ;
#10115 = LINE('',#115230,#14231) ;
#10116 = LINE('',#115231,#14232) ;
#10117 = LINE('',#115235,#14233) ;
#10118 = LINE('',#115241,#14234) ;
#10119 = LINE('',#115242,#14235) ;
#10120 = LINE('',#115243,#14236) ;
#10121 = LINE('',#115247,#14237) ;
#10122 = LINE('',#115253,#14238) ;
#10123 = LINE('',#115254,#14239) ;
#10124 = LINE('',#115255,#14240) ;
#10125 = LINE('',#115259,#14241) ;
#10126 = LINE('',#115263,#14242) ;
#10127 = LINE('',#115264,#14243) ;
#10128 = LINE('',#115269,#14244) ;
#10129 = LINE('',#115271,#14245) ;
#10130 = LINE('',#115273,#14246) ;
#10131 = LINE('',#115277,#14247) ;
#10132 = LINE('',#115280,#14248) ;
#10133 = LINE('',#115282,#14249) ;
#10134 = LINE('',#115286,#14250) ;
#10135 = LINE('',#115288,#14251) ;
#10136 = LINE('',#115290,#14252) ;
#10137 = LINE('',#115294,#14253) ;
#10138 = LINE('',#115298,#14254) ;
#10139 = LINE('',#115306,#14255) ;
#10140 = LINE('',#115309,#14256) ;
#10141 = LINE('',#115314,#14257) ;
#10142 = LINE('',#115316,#14258) ;
#10143 = LINE('',#115318,#14259) ;
#10144 = LINE('',#115322,#14260) ;
#10145 = LINE('',#115325,#14261) ;
#10146 = LINE('',#115327,#14262) ;
#10147 = LINE('',#115331,#14263) ;
#10148 = LINE('',#115333,#14264) ;
#10149 = LINE('',#115335,#14265) ;
#10150 = LINE('',#115339,#14266) ;
#10151 = LINE('',#115343,#14267) ;
#10152 = LINE('',#115351,#14268) ;
#10153 = LINE('',#115354,#14269) ;
#10154 = LINE('',#115359,#14270) ;
#10155 = LINE('',#115361,#14271) ;
#10156 = LINE('',#115363,#14272) ;
#10157 = LINE('',#115367,#14273) ;
#10158 = LINE('',#115370,#14274) ;
#10159 = LINE('',#115372,#14275) ;
#10160 = LINE('',#115376,#14276) ;
#10161 = LINE('',#115378,#14277) ;
#10162 = LINE('',#115380,#14278) ;
#10163 = LINE('',#115384,#14279) ;
#10164 = LINE('',#115388,#14280) ;
#10165 = LINE('',#115396,#14281) ;
#10166 = LINE('',#115399,#14282) ;
#10167 = LINE('',#115404,#14283) ;
#10168 = LINE('',#115406,#14284) ;
#10169 = LINE('',#115408,#14285) ;
#10170 = LINE('',#115412,#14286) ;
#10171 = LINE('',#115415,#14287) ;
#10172 = LINE('',#115417,#14288) ;
#10173 = LINE('',#115421,#14289) ;
#10174 = LINE('',#115423,#14290) ;
#10175 = LINE('',#115425,#14291) ;
#10176 = LINE('',#115429,#14292) ;
#10177 = LINE('',#115433,#14293) ;
#10178 = LINE('',#115441,#14294) ;
#10179 = LINE('',#115444,#14295) ;
#10180 = LINE('',#115449,#14296) ;
#10181 = LINE('',#115451,#14297) ;
#10182 = LINE('',#115453,#14298) ;
#10183 = LINE('',#115457,#14299) ;
#10184 = LINE('',#115460,#14300) ;
#10185 = LINE('',#115462,#14301) ;
#10186 = LINE('',#115466,#14302) ;
#10187 = LINE('',#115468,#14303) ;
#10188 = LINE('',#115470,#14304) ;
#10189 = LINE('',#115474,#14305) ;
#10190 = LINE('',#115478,#14306) ;
#10191 = LINE('',#115486,#14307) ;
#10192 = LINE('',#115489,#14308) ;
#10193 = LINE('',#115494,#14309) ;
#10194 = LINE('',#115496,#14310) ;
#10195 = LINE('',#115498,#14311) ;
#10196 = LINE('',#115502,#14312) ;
#10197 = LINE('',#115505,#14313) ;
#10198 = LINE('',#115507,#14314) ;
#10199 = LINE('',#115511,#14315) ;
#10200 = LINE('',#115513,#14316) ;
#10201 = LINE('',#115515,#14317) ;
#10202 = LINE('',#115519,#14318) ;
#10203 = LINE('',#115523,#14319) ;
#10204 = LINE('',#115531,#14320) ;
#10205 = LINE('',#115534,#14321) ;
#10206 = LINE('',#115539,#14322) ;
#10207 = LINE('',#115541,#14323) ;
#10208 = LINE('',#115543,#14324) ;
#10209 = LINE('',#115547,#14325) ;
#10210 = LINE('',#115550,#14326) ;
#10211 = LINE('',#115552,#14327) ;
#10212 = LINE('',#115556,#14328) ;
#10213 = LINE('',#115558,#14329) ;
#10214 = LINE('',#115560,#14330) ;
#10215 = LINE('',#115564,#14331) ;
#10216 = LINE('',#115568,#14332) ;
#10217 = LINE('',#115576,#14333) ;
#10218 = LINE('',#115579,#14334) ;
#10219 = LINE('',#115584,#14335) ;
#10220 = LINE('',#115586,#14336) ;
#10221 = LINE('',#115588,#14337) ;
#10222 = LINE('',#115592,#14338) ;
#10223 = LINE('',#115595,#14339) ;
#10224 = LINE('',#115597,#14340) ;
#10225 = LINE('',#115601,#14341) ;
#10226 = LINE('',#115603,#14342) ;
#10227 = LINE('',#115605,#14343) ;
#10228 = LINE('',#115609,#14344) ;
#10229 = LINE('',#115613,#14345) ;
#10230 = LINE('',#115621,#14346) ;
#10231 = LINE('',#115624,#14347) ;
#10232 = LINE('',#115629,#14348) ;
#10233 = LINE('',#115631,#14349) ;
#10234 = LINE('',#115633,#14350) ;
#10235 = LINE('',#115637,#14351) ;
#10236 = LINE('',#115640,#14352) ;
#10237 = LINE('',#115642,#14353) ;
#10238 = LINE('',#115646,#14354) ;
#10239 = LINE('',#115648,#14355) ;
#10240 = LINE('',#115650,#14356) ;
#10241 = LINE('',#115654,#14357) ;
#10242 = LINE('',#115658,#14358) ;
#10243 = LINE('',#115666,#14359) ;
#10244 = LINE('',#115669,#14360) ;
#10245 = LINE('',#115674,#14361) ;
#10246 = LINE('',#115676,#14362) ;
#10247 = LINE('',#115678,#14363) ;
#10248 = LINE('',#115682,#14364) ;
#10249 = LINE('',#115685,#14365) ;
#10250 = LINE('',#115687,#14366) ;
#10251 = LINE('',#115691,#14367) ;
#10252 = LINE('',#115693,#14368) ;
#10253 = LINE('',#115695,#14369) ;
#10254 = LINE('',#115699,#14370) ;
#10255 = LINE('',#115703,#14371) ;
#10256 = LINE('',#115711,#14372) ;
#10257 = LINE('',#115714,#14373) ;
#10258 = LINE('',#115718,#14374) ;
#10259 = LINE('',#115720,#14375) ;
#10260 = LINE('',#115722,#14376) ;
#10261 = LINE('',#115724,#14377) ;
#10262 = LINE('',#115728,#14378) ;
#10263 = LINE('',#115730,#14379) ;
#10264 = LINE('',#115732,#14380) ;
#10265 = LINE('',#115735,#14381) ;
#10266 = LINE('',#115739,#14382) ;
#10267 = LINE('',#115741,#14383) ;
#10268 = LINE('',#115743,#14384) ;
#10269 = LINE('',#115745,#14385) ;
#10270 = LINE('',#115749,#14386) ;
#10271 = LINE('',#115751,#14387) ;
#10272 = LINE('',#115753,#14388) ;
#10273 = LINE('',#115756,#14389) ;
#10274 = LINE('',#115760,#14390) ;
#10275 = LINE('',#115762,#14391) ;
#10276 = LINE('',#115764,#14392) ;
#10277 = LINE('',#115766,#14393) ;
#10278 = LINE('',#115768,#14394) ;
#10279 = LINE('',#115770,#14395) ;
#10280 = LINE('',#115774,#14396) ;
#10281 = LINE('',#115777,#14397) ;
#10282 = LINE('',#115781,#14398) ;
#10283 = LINE('',#115783,#14399) ;
#10284 = LINE('',#115785,#14400) ;
#10285 = LINE('',#115786,#14401) ;
#10286 = LINE('',#115789,#14402) ;
#10287 = LINE('',#115791,#14403) ;
#10288 = LINE('',#115792,#14404) ;
#10289 = LINE('',#115796,#14405) ;
#10290 = LINE('',#115798,#14406) ;
#10291 = LINE('',#115800,#14407) ;
#10292 = LINE('',#115801,#14408) ;
#10293 = LINE('',#115805,#14409) ;
#10294 = LINE('',#115807,#14410) ;
#10295 = LINE('',#115809,#14411) ;
#10296 = LINE('',#115810,#14412) ;
#10297 = LINE('',#115814,#14413) ;
#10298 = LINE('',#115816,#14414) ;
#10299 = LINE('',#115818,#14415) ;
#10300 = LINE('',#115819,#14416) ;
#10301 = LINE('',#115823,#14417) ;
#10302 = LINE('',#115827,#14418) ;
#10303 = LINE('',#115831,#14419) ;
#10304 = LINE('',#115833,#14420) ;
#10305 = LINE('',#115834,#14421) ;
#10306 = LINE('',#115839,#14422) ;
#10307 = LINE('',#115843,#14423) ;
#10308 = LINE('',#115845,#14424) ;
#10309 = LINE('',#115846,#14425) ;
#10310 = LINE('',#115851,#14426) ;
#10311 = LINE('',#115854,#14427) ;
#10312 = LINE('',#115856,#14428) ;
#10313 = LINE('',#115857,#14429) ;
#10314 = LINE('',#115860,#14430) ;
#10315 = LINE('',#115863,#14431) ;
#10316 = LINE('',#115864,#14432) ;
#10317 = LINE('',#115867,#14433) ;
#10318 = LINE('',#115869,#14434) ;
#10319 = LINE('',#115870,#14435) ;
#10320 = LINE('',#115875,#14436) ;
#10321 = LINE('',#115879,#14437) ;
#10322 = LINE('',#115881,#14438) ;
#10323 = LINE('',#115882,#14439) ;
#10324 = LINE('',#115887,#14440) ;
#10325 = LINE('',#115891,#14441) ;
#10326 = LINE('',#115893,#14442) ;
#10327 = LINE('',#115894,#14443) ;
#10328 = LINE('',#115899,#14444) ;
#10329 = LINE('',#115903,#14445) ;
#10330 = LINE('',#115905,#14446) ;
#10331 = LINE('',#115906,#14447) ;
#10332 = LINE('',#115911,#14448) ;
#10333 = LINE('',#115915,#14449) ;
#10334 = LINE('',#115917,#14450) ;
#10335 = LINE('',#115918,#14451) ;
#10336 = LINE('',#115923,#14452) ;
#10337 = LINE('',#115927,#14453) ;
#10338 = LINE('',#115929,#14454) ;
#10339 = LINE('',#115930,#14455) ;
#10340 = LINE('',#115935,#14456) ;
#10341 = LINE('',#115941,#14457) ;
#10342 = LINE('',#115947,#14458) ;
#10343 = LINE('',#115951,#14459) ;
#10344 = LINE('',#115953,#14460) ;
#10345 = LINE('',#115954,#14461) ;
#10346 = LINE('',#115959,#14462) ;
#10347 = LINE('',#115963,#14463) ;
#10348 = LINE('',#115965,#14464) ;
#10349 = LINE('',#115966,#14465) ;
#10350 = LINE('',#115971,#14466) ;
#10351 = LINE('',#115974,#14467) ;
#10352 = LINE('',#115975,#14468) ;
#10353 = LINE('',#115981,#14469) ;
#10354 = LINE('',#115985,#14470) ;
#10355 = LINE('',#115987,#14471) ;
#10356 = LINE('',#115989,#14472) ;
#10357 = LINE('',#115993,#14473) ;
#10358 = LINE('',#115995,#14474) ;
#10359 = LINE('',#115997,#14475) ;
#10360 = LINE('',#116001,#14476) ;
#10361 = LINE('',#116005,#14477) ;
#10362 = LINE('',#116007,#14478) ;
#10363 = LINE('',#116008,#14479) ;
#10364 = LINE('',#116010,#14480) ;
#10365 = LINE('',#116011,#14481) ;
#10366 = LINE('',#116015,#14482) ;
#10367 = LINE('',#116019,#14483) ;
#10368 = LINE('',#116023,#14484) ;
#10369 = LINE('',#116027,#14485) ;
#10370 = LINE('',#116055,#14486) ;
#10371 = LINE('',#116112,#14487) ;
#10372 = LINE('',#116137,#14488) ;
#10373 = LINE('',#116169,#14489) ;
#10374 = LINE('',#116195,#14490) ;
#10375 = LINE('',#116376,#14491) ;
#10376 = LINE('',#116378,#14492) ;
#10377 = LINE('',#116380,#14493) ;
#10378 = LINE('',#116381,#14494) ;
#10379 = LINE('',#116385,#14495) ;
#10380 = LINE('',#116387,#14496) ;
#10381 = LINE('',#116389,#14497) ;
#10382 = LINE('',#116390,#14498) ;
#10383 = LINE('',#116394,#14499) ;
#10384 = LINE('',#116396,#14500) ;
#10385 = LINE('',#116398,#14501) ;
#10386 = LINE('',#116399,#14502) ;
#10387 = LINE('',#116403,#14503) ;
#10388 = LINE('',#116405,#14504) ;
#10389 = LINE('',#116407,#14505) ;
#10390 = LINE('',#116408,#14506) ;
#10391 = LINE('',#116412,#14507) ;
#10392 = LINE('',#116414,#14508) ;
#10393 = LINE('',#116416,#14509) ;
#10394 = LINE('',#116417,#14510) ;
#10395 = LINE('',#116421,#14511) ;
#10396 = LINE('',#116426,#14512) ;
#10397 = LINE('',#116427,#14513) ;
#10398 = LINE('',#116431,#14514) ;
#10399 = LINE('',#116436,#14515) ;
#10400 = LINE('',#116437,#14516) ;
#10401 = LINE('',#116447,#14517) ;
#10402 = LINE('',#116449,#14518) ;
#10403 = LINE('',#116451,#14519) ;
#10404 = LINE('',#116452,#14520) ;
#10405 = LINE('',#116456,#14521) ;
#10406 = LINE('',#116457,#14522) ;
#10407 = LINE('',#116458,#14523) ;
#10408 = LINE('',#116461,#14524) ;
#10409 = LINE('',#116463,#14525) ;
#10410 = LINE('',#116464,#14526) ;
#10411 = LINE('',#116468,#14527) ;
#10412 = LINE('',#116470,#14528) ;
#10413 = LINE('',#116472,#14529) ;
#10414 = LINE('',#116473,#14530) ;
#10415 = LINE('',#116477,#14531) ;
#10416 = LINE('',#116479,#14532) ;
#10417 = LINE('',#116481,#14533) ;
#10418 = LINE('',#116482,#14534) ;
#10419 = LINE('',#116486,#14535) ;
#10420 = LINE('',#116487,#14536) ;
#10421 = LINE('',#116488,#14537) ;
#10422 = LINE('',#116491,#14538) ;
#10423 = LINE('',#116493,#14539) ;
#10424 = LINE('',#116494,#14540) ;
#10425 = LINE('',#116498,#14541) ;
#10426 = LINE('',#116500,#14542) ;
#10427 = LINE('',#116502,#14543) ;
#10428 = LINE('',#116503,#14544) ;
#10429 = LINE('',#116507,#14545) ;
#10430 = LINE('',#116509,#14546) ;
#10431 = LINE('',#116511,#14547) ;
#10432 = LINE('',#116512,#14548) ;
#10433 = LINE('',#116516,#14549) ;
#10434 = LINE('',#116518,#14550) ;
#10435 = LINE('',#116520,#14551) ;
#10436 = LINE('',#116521,#14552) ;
#10437 = LINE('',#116525,#14553) ;
#10438 = LINE('',#116527,#14554) ;
#10439 = LINE('',#116529,#14555) ;
#10440 = LINE('',#116530,#14556) ;
#10441 = LINE('',#116646,#14557) ;
#10442 = LINE('',#116648,#14558) ;
#10443 = LINE('',#116650,#14559) ;
#10444 = LINE('',#116652,#14560) ;
#10445 = LINE('',#116654,#14561) ;
#10446 = LINE('',#116656,#14562) ;
#10447 = LINE('',#116660,#14563) ;
#10448 = LINE('',#116663,#14564) ;
#10449 = LINE('',#116667,#14565) ;
#10450 = LINE('',#116669,#14566) ;
#10451 = LINE('',#116671,#14567) ;
#10452 = LINE('',#116673,#14568) ;
#10453 = LINE('',#116675,#14569) ;
#10454 = LINE('',#116677,#14570) ;
#10455 = LINE('',#116681,#14571) ;
#10456 = LINE('',#116684,#14572) ;
#10457 = LINE('',#116688,#14573) ;
#10458 = LINE('',#116690,#14574) ;
#10459 = LINE('',#116692,#14575) ;
#10460 = LINE('',#116694,#14576) ;
#10461 = LINE('',#116696,#14577) ;
#10462 = LINE('',#116698,#14578) ;
#10463 = LINE('',#116702,#14579) ;
#10464 = LINE('',#116705,#14580) ;
#10465 = LINE('',#116709,#14581) ;
#10466 = LINE('',#116711,#14582) ;
#10467 = LINE('',#116713,#14583) ;
#10468 = LINE('',#116715,#14584) ;
#10469 = LINE('',#116717,#14585) ;
#10470 = LINE('',#116719,#14586) ;
#10471 = LINE('',#116723,#14587) ;
#10472 = LINE('',#116726,#14588) ;
#10473 = LINE('',#116730,#14589) ;
#10474 = LINE('',#116732,#14590) ;
#10475 = LINE('',#116734,#14591) ;
#10476 = LINE('',#116736,#14592) ;
#10477 = LINE('',#116738,#14593) ;
#10478 = LINE('',#116740,#14594) ;
#10479 = LINE('',#116744,#14595) ;
#10480 = LINE('',#116747,#14596) ;
#10481 = LINE('',#116751,#14597) ;
#10482 = LINE('',#116753,#14598) ;
#10483 = LINE('',#116755,#14599) ;
#10484 = LINE('',#116757,#14600) ;
#10485 = LINE('',#116759,#14601) ;
#10486 = LINE('',#116761,#14602) ;
#10487 = LINE('',#116765,#14603) ;
#10488 = LINE('',#116768,#14604) ;
#10489 = LINE('',#116772,#14605) ;
#10490 = LINE('',#116774,#14606) ;
#10491 = LINE('',#116776,#14607) ;
#10492 = LINE('',#116778,#14608) ;
#10493 = LINE('',#116780,#14609) ;
#10494 = LINE('',#116782,#14610) ;
#10495 = LINE('',#116786,#14611) ;
#10496 = LINE('',#116789,#14612) ;
#10497 = LINE('',#116793,#14613) ;
#10498 = LINE('',#116795,#14614) ;
#10499 = LINE('',#116797,#14615) ;
#10500 = LINE('',#116799,#14616) ;
#10501 = LINE('',#116801,#14617) ;
#10502 = LINE('',#116803,#14618) ;
#10503 = LINE('',#116807,#14619) ;
#10504 = LINE('',#116810,#14620) ;
#10505 = LINE('',#116814,#14621) ;
#10506 = LINE('',#116816,#14622) ;
#10507 = LINE('',#116818,#14623) ;
#10508 = LINE('',#116820,#14624) ;
#10509 = LINE('',#116822,#14625) ;
#10510 = LINE('',#116824,#14626) ;
#10511 = LINE('',#116828,#14627) ;
#10512 = LINE('',#116831,#14628) ;
#10513 = LINE('',#116835,#14629) ;
#10514 = LINE('',#116837,#14630) ;
#10515 = LINE('',#116839,#14631) ;
#10516 = LINE('',#116840,#14632) ;
#10517 = LINE('',#116843,#14633) ;
#10518 = LINE('',#116845,#14634) ;
#10519 = LINE('',#116846,#14635) ;
#10520 = LINE('',#116850,#14636) ;
#10521 = LINE('',#116852,#14637) ;
#10522 = LINE('',#116854,#14638) ;
#10523 = LINE('',#116855,#14639) ;
#10524 = LINE('',#116859,#14640) ;
#10525 = LINE('',#116861,#14641) ;
#10526 = LINE('',#116863,#14642) ;
#10527 = LINE('',#116864,#14643) ;
#10528 = LINE('',#116868,#14644) ;
#10529 = LINE('',#116870,#14645) ;
#10530 = LINE('',#116872,#14646) ;
#10531 = LINE('',#116873,#14647) ;
#10532 = LINE('',#116877,#14648) ;
#10533 = LINE('',#116879,#14649) ;
#10534 = LINE('',#116881,#14650) ;
#10535 = LINE('',#116882,#14651) ;
#10536 = LINE('',#116885,#14652) ;
#10537 = LINE('',#116887,#14653) ;
#10538 = LINE('',#116888,#14654) ;
#10539 = LINE('',#116892,#14655) ;
#10540 = LINE('',#116894,#14656) ;
#10541 = LINE('',#116896,#14657) ;
#10542 = LINE('',#116897,#14658) ;
#10543 = LINE('',#116901,#14659) ;
#10544 = LINE('',#116903,#14660) ;
#10545 = LINE('',#116905,#14661) ;
#10546 = LINE('',#116906,#14662) ;
#10547 = LINE('',#116910,#14663) ;
#10548 = LINE('',#116912,#14664) ;
#10549 = LINE('',#116914,#14665) ;
#10550 = LINE('',#116915,#14666) ;
#10551 = LINE('',#116919,#14667) ;
#10552 = LINE('',#116921,#14668) ;
#10553 = LINE('',#116923,#14669) ;
#10554 = LINE('',#116924,#14670) ;
#10555 = LINE('',#116927,#14671) ;
#10556 = LINE('',#116929,#14672) ;
#10557 = LINE('',#116930,#14673) ;
#10558 = LINE('',#116934,#14674) ;
#10559 = LINE('',#116936,#14675) ;
#10560 = LINE('',#116938,#14676) ;
#10561 = LINE('',#116939,#14677) ;
#10562 = LINE('',#116943,#14678) ;
#10563 = LINE('',#116945,#14679) ;
#10564 = LINE('',#116947,#14680) ;
#10565 = LINE('',#116948,#14681) ;
#10566 = LINE('',#116952,#14682) ;
#10567 = LINE('',#116954,#14683) ;
#10568 = LINE('',#116956,#14684) ;
#10569 = LINE('',#116957,#14685) ;
#10570 = LINE('',#116961,#14686) ;
#10571 = LINE('',#116963,#14687) ;
#10572 = LINE('',#116965,#14688) ;
#10573 = LINE('',#116966,#14689) ;
#10574 = LINE('',#116969,#14690) ;
#10575 = LINE('',#116971,#14691) ;
#10576 = LINE('',#116972,#14692) ;
#10577 = LINE('',#116976,#14693) ;
#10578 = LINE('',#116978,#14694) ;
#10579 = LINE('',#116980,#14695) ;
#10580 = LINE('',#116981,#14696) ;
#10581 = LINE('',#116985,#14697) ;
#10582 = LINE('',#116987,#14698) ;
#10583 = LINE('',#116989,#14699) ;
#10584 = LINE('',#116990,#14700) ;
#10585 = LINE('',#116994,#14701) ;
#10586 = LINE('',#116996,#14702) ;
#10587 = LINE('',#116998,#14703) ;
#10588 = LINE('',#116999,#14704) ;
#10589 = LINE('',#117003,#14705) ;
#10590 = LINE('',#117005,#14706) ;
#10591 = LINE('',#117007,#14707) ;
#10592 = LINE('',#117008,#14708) ;
#10593 = LINE('',#117011,#14709) ;
#10594 = LINE('',#117013,#14710) ;
#10595 = LINE('',#117014,#14711) ;
#10596 = LINE('',#117018,#14712) ;
#10597 = LINE('',#117020,#14713) ;
#10598 = LINE('',#117022,#14714) ;
#10599 = LINE('',#117023,#14715) ;
#10600 = LINE('',#117027,#14716) ;
#10601 = LINE('',#117029,#14717) ;
#10602 = LINE('',#117031,#14718) ;
#10603 = LINE('',#117032,#14719) ;
#10604 = LINE('',#117036,#14720) ;
#10605 = LINE('',#117038,#14721) ;
#10606 = LINE('',#117040,#14722) ;
#10607 = LINE('',#117041,#14723) ;
#10608 = LINE('',#117045,#14724) ;
#10609 = LINE('',#117047,#14725) ;
#10610 = LINE('',#117049,#14726) ;
#10611 = LINE('',#117050,#14727) ;
#10612 = LINE('',#117053,#14728) ;
#10613 = LINE('',#117055,#14729) ;
#10614 = LINE('',#117056,#14730) ;
#10615 = LINE('',#117060,#14731) ;
#10616 = LINE('',#117062,#14732) ;
#10617 = LINE('',#117064,#14733) ;
#10618 = LINE('',#117065,#14734) ;
#10619 = LINE('',#117069,#14735) ;
#10620 = LINE('',#117071,#14736) ;
#10621 = LINE('',#117073,#14737) ;
#10622 = LINE('',#117074,#14738) ;
#10623 = LINE('',#117078,#14739) ;
#10624 = LINE('',#117080,#14740) ;
#10625 = LINE('',#117082,#14741) ;
#10626 = LINE('',#117083,#14742) ;
#10627 = LINE('',#117087,#14743) ;
#10628 = LINE('',#117089,#14744) ;
#10629 = LINE('',#117091,#14745) ;
#10630 = LINE('',#117092,#14746) ;
#10631 = LINE('',#117095,#14747) ;
#10632 = LINE('',#117097,#14748) ;
#10633 = LINE('',#117098,#14749) ;
#10634 = LINE('',#117102,#14750) ;
#10635 = LINE('',#117104,#14751) ;
#10636 = LINE('',#117106,#14752) ;
#10637 = LINE('',#117107,#14753) ;
#10638 = LINE('',#117111,#14754) ;
#10639 = LINE('',#117113,#14755) ;
#10640 = LINE('',#117115,#14756) ;
#10641 = LINE('',#117116,#14757) ;
#10642 = LINE('',#117120,#14758) ;
#10643 = LINE('',#117122,#14759) ;
#10644 = LINE('',#117124,#14760) ;
#10645 = LINE('',#117125,#14761) ;
#10646 = LINE('',#117129,#14762) ;
#10647 = LINE('',#117131,#14763) ;
#10648 = LINE('',#117133,#14764) ;
#10649 = LINE('',#117134,#14765) ;
#10650 = LINE('',#117137,#14766) ;
#10651 = LINE('',#117139,#14767) ;
#10652 = LINE('',#117140,#14768) ;
#10653 = LINE('',#117144,#14769) ;
#10654 = LINE('',#117146,#14770) ;
#10655 = LINE('',#117148,#14771) ;
#10656 = LINE('',#117149,#14772) ;
#10657 = LINE('',#117153,#14773) ;
#10658 = LINE('',#117155,#14774) ;
#10659 = LINE('',#117157,#14775) ;
#10660 = LINE('',#117158,#14776) ;
#10661 = LINE('',#117162,#14777) ;
#10662 = LINE('',#117164,#14778) ;
#10663 = LINE('',#117166,#14779) ;
#10664 = LINE('',#117167,#14780) ;
#10665 = LINE('',#117171,#14781) ;
#10666 = LINE('',#117173,#14782) ;
#10667 = LINE('',#117175,#14783) ;
#10668 = LINE('',#117176,#14784) ;
#10669 = LINE('',#117179,#14785) ;
#10670 = LINE('',#117181,#14786) ;
#10671 = LINE('',#117182,#14787) ;
#10672 = LINE('',#117186,#14788) ;
#10673 = LINE('',#117188,#14789) ;
#10674 = LINE('',#117190,#14790) ;
#10675 = LINE('',#117191,#14791) ;
#10676 = LINE('',#117195,#14792) ;
#10677 = LINE('',#117197,#14793) ;
#10678 = LINE('',#117199,#14794) ;
#10679 = LINE('',#117200,#14795) ;
#10680 = LINE('',#117204,#14796) ;
#10681 = LINE('',#117206,#14797) ;
#10682 = LINE('',#117208,#14798) ;
#10683 = LINE('',#117209,#14799) ;
#10684 = LINE('',#117213,#14800) ;
#10685 = LINE('',#117217,#14801) ;
#10686 = LINE('',#117221,#14802) ;
#10687 = LINE('',#117223,#14803) ;
#10688 = LINE('',#117224,#14804) ;
#10689 = LINE('',#117229,#14805) ;
#10690 = LINE('',#117233,#14806) ;
#10691 = LINE('',#117235,#14807) ;
#10692 = LINE('',#117236,#14808) ;
#10693 = LINE('',#117241,#14809) ;
#10694 = LINE('',#117244,#14810) ;
#10695 = LINE('',#117246,#14811) ;
#10696 = LINE('',#117247,#14812) ;
#10697 = LINE('',#117250,#14813) ;
#10698 = LINE('',#117253,#14814) ;
#10699 = LINE('',#117254,#14815) ;
#10700 = LINE('',#117257,#14816) ;
#10701 = LINE('',#117259,#14817) ;
#10702 = LINE('',#117260,#14818) ;
#10703 = LINE('',#117265,#14819) ;
#10704 = LINE('',#117269,#14820) ;
#10705 = LINE('',#117271,#14821) ;
#10706 = LINE('',#117272,#14822) ;
#10707 = LINE('',#117277,#14823) ;
#10708 = LINE('',#117281,#14824) ;
#10709 = LINE('',#117283,#14825) ;
#10710 = LINE('',#117284,#14826) ;
#10711 = LINE('',#117289,#14827) ;
#10712 = LINE('',#117293,#14828) ;
#10713 = LINE('',#117295,#14829) ;
#10714 = LINE('',#117296,#14830) ;
#10715 = LINE('',#117301,#14831) ;
#10716 = LINE('',#117305,#14832) ;
#10717 = LINE('',#117307,#14833) ;
#10718 = LINE('',#117308,#14834) ;
#10719 = LINE('',#117313,#14835) ;
#10720 = LINE('',#117317,#14836) ;
#10721 = LINE('',#117319,#14837) ;
#10722 = LINE('',#117320,#14838) ;
#10723 = LINE('',#117325,#14839) ;
#10724 = LINE('',#117331,#14840) ;
#10725 = LINE('',#117337,#14841) ;
#10726 = LINE('',#117341,#14842) ;
#10727 = LINE('',#117343,#14843) ;
#10728 = LINE('',#117344,#14844) ;
#10729 = LINE('',#117349,#14845) ;
#10730 = LINE('',#117353,#14846) ;
#10731 = LINE('',#117355,#14847) ;
#10732 = LINE('',#117356,#14848) ;
#10733 = LINE('',#117361,#14849) ;
#10734 = LINE('',#117364,#14850) ;
#10735 = LINE('',#117365,#14851) ;
#10736 = LINE('',#117371,#14852) ;
#10737 = LINE('',#117375,#14853) ;
#10738 = LINE('',#117377,#14854) ;
#10739 = LINE('',#117379,#14855) ;
#10740 = LINE('',#117383,#14856) ;
#10741 = LINE('',#117385,#14857) ;
#10742 = LINE('',#117387,#14858) ;
#10743 = LINE('',#117391,#14859) ;
#10744 = LINE('',#117395,#14860) ;
#10745 = LINE('',#117397,#14861) ;
#10746 = LINE('',#117398,#14862) ;
#10747 = LINE('',#117400,#14863) ;
#10748 = LINE('',#117401,#14864) ;
#10749 = LINE('',#117405,#14865) ;
#10750 = LINE('',#117409,#14866) ;
#10751 = LINE('',#117413,#14867) ;
#10752 = LINE('',#117415,#14868) ;
#10753 = LINE('',#117416,#14869) ;
#10754 = LINE('',#117421,#14870) ;
#10755 = LINE('',#117425,#14871) ;
#10756 = LINE('',#117427,#14872) ;
#10757 = LINE('',#117428,#14873) ;
#10758 = LINE('',#117433,#14874) ;
#10759 = LINE('',#117436,#14875) ;
#10760 = LINE('',#117438,#14876) ;
#10761 = LINE('',#117439,#14877) ;
#10762 = LINE('',#117442,#14878) ;
#10763 = LINE('',#117445,#14879) ;
#10764 = LINE('',#117446,#14880) ;
#10765 = LINE('',#117449,#14881) ;
#10766 = LINE('',#117451,#14882) ;
#10767 = LINE('',#117452,#14883) ;
#10768 = LINE('',#117457,#14884) ;
#10769 = LINE('',#117461,#14885) ;
#10770 = LINE('',#117463,#14886) ;
#10771 = LINE('',#117464,#14887) ;
#10772 = LINE('',#117469,#14888) ;
#10773 = LINE('',#117473,#14889) ;
#10774 = LINE('',#117475,#14890) ;
#10775 = LINE('',#117476,#14891) ;
#10776 = LINE('',#117481,#14892) ;
#10777 = LINE('',#117485,#14893) ;
#10778 = LINE('',#117487,#14894) ;
#10779 = LINE('',#117488,#14895) ;
#10780 = LINE('',#117493,#14896) ;
#10781 = LINE('',#117497,#14897) ;
#10782 = LINE('',#117499,#14898) ;
#10783 = LINE('',#117500,#14899) ;
#10784 = LINE('',#117505,#14900) ;
#10785 = LINE('',#117509,#14901) ;
#10786 = LINE('',#117511,#14902) ;
#10787 = LINE('',#117512,#14903) ;
#10788 = LINE('',#117517,#14904) ;
#10789 = LINE('',#117523,#14905) ;
#10790 = LINE('',#117529,#14906) ;
#10791 = LINE('',#117533,#14907) ;
#10792 = LINE('',#117535,#14908) ;
#10793 = LINE('',#117536,#14909) ;
#10794 = LINE('',#117541,#14910) ;
#10795 = LINE('',#117545,#14911) ;
#10796 = LINE('',#117547,#14912) ;
#10797 = LINE('',#117548,#14913) ;
#10798 = LINE('',#117553,#14914) ;
#10799 = LINE('',#117556,#14915) ;
#10800 = LINE('',#117557,#14916) ;
#10801 = LINE('',#117563,#14917) ;
#10802 = LINE('',#117567,#14918) ;
#10803 = LINE('',#117569,#14919) ;
#10804 = LINE('',#117571,#14920) ;
#10805 = LINE('',#117575,#14921) ;
#10806 = LINE('',#117577,#14922) ;
#10807 = LINE('',#117579,#14923) ;
#10808 = LINE('',#117583,#14924) ;
#10809 = LINE('',#117587,#14925) ;
#10810 = LINE('',#117589,#14926) ;
#10811 = LINE('',#117590,#14927) ;
#10812 = LINE('',#117592,#14928) ;
#10813 = LINE('',#117593,#14929) ;
#10814 = LINE('',#117597,#14930) ;
#10815 = LINE('',#117601,#14931) ;
#10816 = LINE('',#117605,#14932) ;
#10817 = LINE('',#117607,#14933) ;
#10818 = LINE('',#117608,#14934) ;
#10819 = LINE('',#117613,#14935) ;
#10820 = LINE('',#117617,#14936) ;
#10821 = LINE('',#117619,#14937) ;
#10822 = LINE('',#117620,#14938) ;
#10823 = LINE('',#117625,#14939) ;
#10824 = LINE('',#117628,#14940) ;
#10825 = LINE('',#117630,#14941) ;
#10826 = LINE('',#117631,#14942) ;
#10827 = LINE('',#117634,#14943) ;
#10828 = LINE('',#117637,#14944) ;
#10829 = LINE('',#117638,#14945) ;
#10830 = LINE('',#117641,#14946) ;
#10831 = LINE('',#117643,#14947) ;
#10832 = LINE('',#117644,#14948) ;
#10833 = LINE('',#117649,#14949) ;
#10834 = LINE('',#117653,#14950) ;
#10835 = LINE('',#117655,#14951) ;
#10836 = LINE('',#117656,#14952) ;
#10837 = LINE('',#117661,#14953) ;
#10838 = LINE('',#117665,#14954) ;
#10839 = LINE('',#117667,#14955) ;
#10840 = LINE('',#117668,#14956) ;
#10841 = LINE('',#117673,#14957) ;
#10842 = LINE('',#117677,#14958) ;
#10843 = LINE('',#117679,#14959) ;
#10844 = LINE('',#117680,#14960) ;
#10845 = LINE('',#117685,#14961) ;
#10846 = LINE('',#117689,#14962) ;
#10847 = LINE('',#117691,#14963) ;
#10848 = LINE('',#117692,#14964) ;
#10849 = LINE('',#117697,#14965) ;
#10850 = LINE('',#117701,#14966) ;
#10851 = LINE('',#117703,#14967) ;
#10852 = LINE('',#117704,#14968) ;
#10853 = LINE('',#117709,#14969) ;
#10854 = LINE('',#117715,#14970) ;
#10855 = LINE('',#117721,#14971) ;
#10856 = LINE('',#117725,#14972) ;
#10857 = LINE('',#117727,#14973) ;
#10858 = LINE('',#117728,#14974) ;
#10859 = LINE('',#117733,#14975) ;
#10860 = LINE('',#117737,#14976) ;
#10861 = LINE('',#117739,#14977) ;
#10862 = LINE('',#117740,#14978) ;
#10863 = LINE('',#117745,#14979) ;
#10864 = LINE('',#117748,#14980) ;
#10865 = LINE('',#117749,#14981) ;
#10866 = LINE('',#117755,#14982) ;
#10867 = LINE('',#117759,#14983) ;
#10868 = LINE('',#117761,#14984) ;
#10869 = LINE('',#117763,#14985) ;
#10870 = LINE('',#117767,#14986) ;
#10871 = LINE('',#117769,#14987) ;
#10872 = LINE('',#117771,#14988) ;
#10873 = LINE('',#117775,#14989) ;
#10874 = LINE('',#117779,#14990) ;
#10875 = LINE('',#117781,#14991) ;
#10876 = LINE('',#117782,#14992) ;
#10877 = LINE('',#117784,#14993) ;
#10878 = LINE('',#117785,#14994) ;
#10879 = LINE('',#117789,#14995) ;
#10880 = LINE('',#117793,#14996) ;
#10881 = LINE('',#117797,#14997) ;
#10882 = LINE('',#117799,#14998) ;
#10883 = LINE('',#117800,#14999) ;
#10884 = LINE('',#117805,#15000) ;
#10885 = LINE('',#117809,#15001) ;
#10886 = LINE('',#117811,#15002) ;
#10887 = LINE('',#117812,#15003) ;
#10888 = LINE('',#117817,#15004) ;
#10889 = LINE('',#117820,#15005) ;
#10890 = LINE('',#117822,#15006) ;
#10891 = LINE('',#117823,#15007) ;
#10892 = LINE('',#117826,#15008) ;
#10893 = LINE('',#117829,#15009) ;
#10894 = LINE('',#117830,#15010) ;
#10895 = LINE('',#117833,#15011) ;
#10896 = LINE('',#117835,#15012) ;
#10897 = LINE('',#117836,#15013) ;
#10898 = LINE('',#117841,#15014) ;
#10899 = LINE('',#117845,#15015) ;
#10900 = LINE('',#117847,#15016) ;
#10901 = LINE('',#117848,#15017) ;
#10902 = LINE('',#117853,#15018) ;
#10903 = LINE('',#117857,#15019) ;
#10904 = LINE('',#117859,#15020) ;
#10905 = LINE('',#117860,#15021) ;
#10906 = LINE('',#117865,#15022) ;
#10907 = LINE('',#117869,#15023) ;
#10908 = LINE('',#117871,#15024) ;
#10909 = LINE('',#117872,#15025) ;
#10910 = LINE('',#117877,#15026) ;
#10911 = LINE('',#117881,#15027) ;
#10912 = LINE('',#117883,#15028) ;
#10913 = LINE('',#117884,#15029) ;
#10914 = LINE('',#117889,#15030) ;
#10915 = LINE('',#117893,#15031) ;
#10916 = LINE('',#117895,#15032) ;
#10917 = LINE('',#117896,#15033) ;
#10918 = LINE('',#117901,#15034) ;
#10919 = LINE('',#117907,#15035) ;
#10920 = LINE('',#117913,#15036) ;
#10921 = LINE('',#117917,#15037) ;
#10922 = LINE('',#117919,#15038) ;
#10923 = LINE('',#117920,#15039) ;
#10924 = LINE('',#117925,#15040) ;
#10925 = LINE('',#117929,#15041) ;
#10926 = LINE('',#117931,#15042) ;
#10927 = LINE('',#117932,#15043) ;
#10928 = LINE('',#117937,#15044) ;
#10929 = LINE('',#117940,#15045) ;
#10930 = LINE('',#117941,#15046) ;
#10931 = LINE('',#117947,#15047) ;
#10932 = LINE('',#117951,#15048) ;
#10933 = LINE('',#117953,#15049) ;
#10934 = LINE('',#117955,#15050) ;
#10935 = LINE('',#117959,#15051) ;
#10936 = LINE('',#117961,#15052) ;
#10937 = LINE('',#117963,#15053) ;
#10938 = LINE('',#117967,#15054) ;
#10939 = LINE('',#117971,#15055) ;
#10940 = LINE('',#117973,#15056) ;
#10941 = LINE('',#117974,#15057) ;
#10942 = LINE('',#117976,#15058) ;
#10943 = LINE('',#117977,#15059) ;
#10944 = LINE('',#117981,#15060) ;
#10945 = LINE('',#117985,#15061) ;
#10946 = LINE('',#117989,#15062) ;
#10947 = LINE('',#117991,#15063) ;
#10948 = LINE('',#117992,#15064) ;
#10949 = LINE('',#117997,#15065) ;
#10950 = LINE('',#118001,#15066) ;
#10951 = LINE('',#118003,#15067) ;
#10952 = LINE('',#118004,#15068) ;
#10953 = LINE('',#118009,#15069) ;
#10954 = LINE('',#118012,#15070) ;
#10955 = LINE('',#118014,#15071) ;
#10956 = LINE('',#118015,#15072) ;
#10957 = LINE('',#118018,#15073) ;
#10958 = LINE('',#118021,#15074) ;
#10959 = LINE('',#118022,#15075) ;
#10960 = LINE('',#118025,#15076) ;
#10961 = LINE('',#118027,#15077) ;
#10962 = LINE('',#118028,#15078) ;
#10963 = LINE('',#118033,#15079) ;
#10964 = LINE('',#118037,#15080) ;
#10965 = LINE('',#118039,#15081) ;
#10966 = LINE('',#118040,#15082) ;
#10967 = LINE('',#118045,#15083) ;
#10968 = LINE('',#118049,#15084) ;
#10969 = LINE('',#118051,#15085) ;
#10970 = LINE('',#118052,#15086) ;
#10971 = LINE('',#118057,#15087) ;
#10972 = LINE('',#118061,#15088) ;
#10973 = LINE('',#118063,#15089) ;
#10974 = LINE('',#118064,#15090) ;
#10975 = LINE('',#118069,#15091) ;
#10976 = LINE('',#118073,#15092) ;
#10977 = LINE('',#118075,#15093) ;
#10978 = LINE('',#118076,#15094) ;
#10979 = LINE('',#118081,#15095) ;
#10980 = LINE('',#118085,#15096) ;
#10981 = LINE('',#118087,#15097) ;
#10982 = LINE('',#118088,#15098) ;
#10983 = LINE('',#118093,#15099) ;
#10984 = LINE('',#118099,#15100) ;
#10985 = LINE('',#118105,#15101) ;
#10986 = LINE('',#118109,#15102) ;
#10987 = LINE('',#118111,#15103) ;
#10988 = LINE('',#118112,#15104) ;
#10989 = LINE('',#118117,#15105) ;
#10990 = LINE('',#118121,#15106) ;
#10991 = LINE('',#118123,#15107) ;
#10992 = LINE('',#118124,#15108) ;
#10993 = LINE('',#118129,#15109) ;
#10994 = LINE('',#118132,#15110) ;
#10995 = LINE('',#118133,#15111) ;
#10996 = LINE('',#118139,#15112) ;
#10997 = LINE('',#118143,#15113) ;
#10998 = LINE('',#118145,#15114) ;
#10999 = LINE('',#118147,#15115) ;
#11000 = LINE('',#118151,#15116) ;
#11001 = LINE('',#118153,#15117) ;
#11002 = LINE('',#118155,#15118) ;
#11003 = LINE('',#118159,#15119) ;
#11004 = LINE('',#118163,#15120) ;
#11005 = LINE('',#118165,#15121) ;
#11006 = LINE('',#118166,#15122) ;
#11007 = LINE('',#118168,#15123) ;
#11008 = LINE('',#118169,#15124) ;
#11009 = LINE('',#118173,#15125) ;
#11010 = LINE('',#118177,#15126) ;
#11011 = LINE('',#118181,#15127) ;
#11012 = LINE('',#118183,#15128) ;
#11013 = LINE('',#118184,#15129) ;
#11014 = LINE('',#118189,#15130) ;
#11015 = LINE('',#118193,#15131) ;
#11016 = LINE('',#118195,#15132) ;
#11017 = LINE('',#118196,#15133) ;
#11018 = LINE('',#118201,#15134) ;
#11019 = LINE('',#118204,#15135) ;
#11020 = LINE('',#118206,#15136) ;
#11021 = LINE('',#118207,#15137) ;
#11022 = LINE('',#118210,#15138) ;
#11023 = LINE('',#118213,#15139) ;
#11024 = LINE('',#118214,#15140) ;
#11025 = LINE('',#118217,#15141) ;
#11026 = LINE('',#118219,#15142) ;
#11027 = LINE('',#118220,#15143) ;
#11028 = LINE('',#118225,#15144) ;
#11029 = LINE('',#118229,#15145) ;
#11030 = LINE('',#118231,#15146) ;
#11031 = LINE('',#118232,#15147) ;
#11032 = LINE('',#118237,#15148) ;
#11033 = LINE('',#118241,#15149) ;
#11034 = LINE('',#118243,#15150) ;
#11035 = LINE('',#118244,#15151) ;
#11036 = LINE('',#118249,#15152) ;
#11037 = LINE('',#118253,#15153) ;
#11038 = LINE('',#118255,#15154) ;
#11039 = LINE('',#118256,#15155) ;
#11040 = LINE('',#118261,#15156) ;
#11041 = LINE('',#118265,#15157) ;
#11042 = LINE('',#118267,#15158) ;
#11043 = LINE('',#118268,#15159) ;
#11044 = LINE('',#118273,#15160) ;
#11045 = LINE('',#118277,#15161) ;
#11046 = LINE('',#118279,#15162) ;
#11047 = LINE('',#118280,#15163) ;
#11048 = LINE('',#118285,#15164) ;
#11049 = LINE('',#118291,#15165) ;
#11050 = LINE('',#118297,#15166) ;
#11051 = LINE('',#118301,#15167) ;
#11052 = LINE('',#118303,#15168) ;
#11053 = LINE('',#118304,#15169) ;
#11054 = LINE('',#118309,#15170) ;
#11055 = LINE('',#118313,#15171) ;
#11056 = LINE('',#118315,#15172) ;
#11057 = LINE('',#118316,#15173) ;
#11058 = LINE('',#118321,#15174) ;
#11059 = LINE('',#118324,#15175) ;
#11060 = LINE('',#118325,#15176) ;
#11061 = LINE('',#118331,#15177) ;
#11062 = LINE('',#118335,#15178) ;
#11063 = LINE('',#118337,#15179) ;
#11064 = LINE('',#118339,#15180) ;
#11065 = LINE('',#118343,#15181) ;
#11066 = LINE('',#118345,#15182) ;
#11067 = LINE('',#118347,#15183) ;
#11068 = LINE('',#118351,#15184) ;
#11069 = LINE('',#118355,#15185) ;
#11070 = LINE('',#118357,#15186) ;
#11071 = LINE('',#118358,#15187) ;
#11072 = LINE('',#118360,#15188) ;
#11073 = LINE('',#118361,#15189) ;
#11074 = LINE('',#118365,#15190) ;
#11075 = LINE('',#118369,#15191) ;
#11076 = LINE('',#118373,#15192) ;
#11077 = LINE('',#118375,#15193) ;
#11078 = LINE('',#118376,#15194) ;
#11079 = LINE('',#118381,#15195) ;
#11080 = LINE('',#118385,#15196) ;
#11081 = LINE('',#118387,#15197) ;
#11082 = LINE('',#118388,#15198) ;
#11083 = LINE('',#118393,#15199) ;
#11084 = LINE('',#118396,#15200) ;
#11085 = LINE('',#118398,#15201) ;
#11086 = LINE('',#118399,#15202) ;
#11087 = LINE('',#118402,#15203) ;
#11088 = LINE('',#118405,#15204) ;
#11089 = LINE('',#118406,#15205) ;
#11090 = LINE('',#118409,#15206) ;
#11091 = LINE('',#118411,#15207) ;
#11092 = LINE('',#118412,#15208) ;
#11093 = LINE('',#118417,#15209) ;
#11094 = LINE('',#118421,#15210) ;
#11095 = LINE('',#118423,#15211) ;
#11096 = LINE('',#118424,#15212) ;
#11097 = LINE('',#118429,#15213) ;
#11098 = LINE('',#118433,#15214) ;
#11099 = LINE('',#118435,#15215) ;
#11100 = LINE('',#118436,#15216) ;
#11101 = LINE('',#118441,#15217) ;
#11102 = LINE('',#118445,#15218) ;
#11103 = LINE('',#118447,#15219) ;
#11104 = LINE('',#118448,#15220) ;
#11105 = LINE('',#118453,#15221) ;
#11106 = LINE('',#118457,#15222) ;
#11107 = LINE('',#118459,#15223) ;
#11108 = LINE('',#118460,#15224) ;
#11109 = LINE('',#118465,#15225) ;
#11110 = LINE('',#118469,#15226) ;
#11111 = LINE('',#118471,#15227) ;
#11112 = LINE('',#118472,#15228) ;
#11113 = LINE('',#118477,#15229) ;
#11114 = LINE('',#118483,#15230) ;
#11115 = LINE('',#118489,#15231) ;
#11116 = LINE('',#118493,#15232) ;
#11117 = LINE('',#118495,#15233) ;
#11118 = LINE('',#118496,#15234) ;
#11119 = LINE('',#118501,#15235) ;
#11120 = LINE('',#118505,#15236) ;
#11121 = LINE('',#118507,#15237) ;
#11122 = LINE('',#118508,#15238) ;
#11123 = LINE('',#118513,#15239) ;
#11124 = LINE('',#118516,#15240) ;
#11125 = LINE('',#118517,#15241) ;
#11126 = LINE('',#118523,#15242) ;
#11127 = LINE('',#118527,#15243) ;
#11128 = LINE('',#118529,#15244) ;
#11129 = LINE('',#118531,#15245) ;
#11130 = LINE('',#118535,#15246) ;
#11131 = LINE('',#118537,#15247) ;
#11132 = LINE('',#118539,#15248) ;
#11133 = LINE('',#118543,#15249) ;
#11134 = LINE('',#118547,#15250) ;
#11135 = LINE('',#118549,#15251) ;
#11136 = LINE('',#118550,#15252) ;
#11137 = LINE('',#118552,#15253) ;
#11138 = LINE('',#118553,#15254) ;
#11139 = LINE('',#118557,#15255) ;
#11140 = LINE('',#118561,#15256) ;
#11141 = LINE('',#118565,#15257) ;
#11142 = LINE('',#118567,#15258) ;
#11143 = LINE('',#118568,#15259) ;
#11144 = LINE('',#118573,#15260) ;
#11145 = LINE('',#118577,#15261) ;
#11146 = LINE('',#118579,#15262) ;
#11147 = LINE('',#118580,#15263) ;
#11148 = LINE('',#118585,#15264) ;
#11149 = LINE('',#118588,#15265) ;
#11150 = LINE('',#118590,#15266) ;
#11151 = LINE('',#118591,#15267) ;
#11152 = LINE('',#118594,#15268) ;
#11153 = LINE('',#118597,#15269) ;
#11154 = LINE('',#118598,#15270) ;
#11155 = LINE('',#118601,#15271) ;
#11156 = LINE('',#118603,#15272) ;
#11157 = LINE('',#118604,#15273) ;
#11158 = LINE('',#118609,#15274) ;
#11159 = LINE('',#118613,#15275) ;
#11160 = LINE('',#118615,#15276) ;
#11161 = LINE('',#118616,#15277) ;
#11162 = LINE('',#118621,#15278) ;
#11163 = LINE('',#118625,#15279) ;
#11164 = LINE('',#118627,#15280) ;
#11165 = LINE('',#118628,#15281) ;
#11166 = LINE('',#118633,#15282) ;
#11167 = LINE('',#118637,#15283) ;
#11168 = LINE('',#118639,#15284) ;
#11169 = LINE('',#118640,#15285) ;
#11170 = LINE('',#118645,#15286) ;
#11171 = LINE('',#118649,#15287) ;
#11172 = LINE('',#118651,#15288) ;
#11173 = LINE('',#118652,#15289) ;
#11174 = LINE('',#118657,#15290) ;
#11175 = LINE('',#118661,#15291) ;
#11176 = LINE('',#118663,#15292) ;
#11177 = LINE('',#118664,#15293) ;
#11178 = LINE('',#118669,#15294) ;
#11179 = LINE('',#118675,#15295) ;
#11180 = LINE('',#118681,#15296) ;
#11181 = LINE('',#118685,#15297) ;
#11182 = LINE('',#118687,#15298) ;
#11183 = LINE('',#118688,#15299) ;
#11184 = LINE('',#118693,#15300) ;
#11185 = LINE('',#118697,#15301) ;
#11186 = LINE('',#118699,#15302) ;
#11187 = LINE('',#118700,#15303) ;
#11188 = LINE('',#118705,#15304) ;
#11189 = LINE('',#118708,#15305) ;
#11190 = LINE('',#118709,#15306) ;
#11191 = LINE('',#118715,#15307) ;
#11192 = LINE('',#118719,#15308) ;
#11193 = LINE('',#118721,#15309) ;
#11194 = LINE('',#118723,#15310) ;
#11195 = LINE('',#118727,#15311) ;
#11196 = LINE('',#118729,#15312) ;
#11197 = LINE('',#118731,#15313) ;
#11198 = LINE('',#118735,#15314) ;
#11199 = LINE('',#118739,#15315) ;
#11200 = LINE('',#118741,#15316) ;
#11201 = LINE('',#118742,#15317) ;
#11202 = LINE('',#118744,#15318) ;
#11203 = LINE('',#118745,#15319) ;
#11204 = LINE('',#118749,#15320) ;
#11205 = LINE('',#118753,#15321) ;
#11206 = LINE('',#118757,#15322) ;
#11207 = LINE('',#118759,#15323) ;
#11208 = LINE('',#118760,#15324) ;
#11209 = LINE('',#118765,#15325) ;
#11210 = LINE('',#118769,#15326) ;
#11211 = LINE('',#118771,#15327) ;
#11212 = LINE('',#118772,#15328) ;
#11213 = LINE('',#118777,#15329) ;
#11214 = LINE('',#118780,#15330) ;
#11215 = LINE('',#118782,#15331) ;
#11216 = LINE('',#118783,#15332) ;
#11217 = LINE('',#118786,#15333) ;
#11218 = LINE('',#118789,#15334) ;
#11219 = LINE('',#118790,#15335) ;
#11220 = LINE('',#118793,#15336) ;
#11221 = LINE('',#118795,#15337) ;
#11222 = LINE('',#118796,#15338) ;
#11223 = LINE('',#118801,#15339) ;
#11224 = LINE('',#118805,#15340) ;
#11225 = LINE('',#118807,#15341) ;
#11226 = LINE('',#118808,#15342) ;
#11227 = LINE('',#118813,#15343) ;
#11228 = LINE('',#118817,#15344) ;
#11229 = LINE('',#118819,#15345) ;
#11230 = LINE('',#118820,#15346) ;
#11231 = LINE('',#118825,#15347) ;
#11232 = LINE('',#118829,#15348) ;
#11233 = LINE('',#118831,#15349) ;
#11234 = LINE('',#118832,#15350) ;
#11235 = LINE('',#118837,#15351) ;
#11236 = LINE('',#118841,#15352) ;
#11237 = LINE('',#118843,#15353) ;
#11238 = LINE('',#118844,#15354) ;
#11239 = LINE('',#118849,#15355) ;
#11240 = LINE('',#118853,#15356) ;
#11241 = LINE('',#118855,#15357) ;
#11242 = LINE('',#118856,#15358) ;
#11243 = LINE('',#118861,#15359) ;
#11244 = LINE('',#118867,#15360) ;
#11245 = LINE('',#118873,#15361) ;
#11246 = LINE('',#118877,#15362) ;
#11247 = LINE('',#118879,#15363) ;
#11248 = LINE('',#118880,#15364) ;
#11249 = LINE('',#118885,#15365) ;
#11250 = LINE('',#118889,#15366) ;
#11251 = LINE('',#118891,#15367) ;
#11252 = LINE('',#118892,#15368) ;
#11253 = LINE('',#118897,#15369) ;
#11254 = LINE('',#118900,#15370) ;
#11255 = LINE('',#118901,#15371) ;
#11256 = LINE('',#118907,#15372) ;
#11257 = LINE('',#118911,#15373) ;
#11258 = LINE('',#118913,#15374) ;
#11259 = LINE('',#118915,#15375) ;
#11260 = LINE('',#118919,#15376) ;
#11261 = LINE('',#118921,#15377) ;
#11262 = LINE('',#118923,#15378) ;
#11263 = LINE('',#118927,#15379) ;
#11264 = LINE('',#118931,#15380) ;
#11265 = LINE('',#118933,#15381) ;
#11266 = LINE('',#118934,#15382) ;
#11267 = LINE('',#118936,#15383) ;
#11268 = LINE('',#118937,#15384) ;
#11269 = LINE('',#118941,#15385) ;
#11270 = LINE('',#118945,#15386) ;
#11271 = LINE('',#118949,#15387) ;
#11272 = LINE('',#118953,#15388) ;
#11273 = LINE('',#118958,#15389) ;
#11274 = LINE('',#118962,#15390) ;
#11275 = LINE('',#118966,#15391) ;
#11276 = LINE('',#118970,#15392) ;
#11277 = LINE('',#118975,#15393) ;
#11278 = LINE('',#118979,#15394) ;
#11279 = LINE('',#118983,#15395) ;
#11280 = LINE('',#118987,#15396) ;
#11281 = LINE('',#118992,#15397) ;
#11282 = LINE('',#118996,#15398) ;
#11283 = LINE('',#119000,#15399) ;
#11284 = LINE('',#119004,#15400) ;
#11285 = LINE('',#119009,#15401) ;
#11286 = LINE('',#119013,#15402) ;
#11287 = LINE('',#119017,#15403) ;
#11288 = LINE('',#119021,#15404) ;
#11289 = LINE('',#119026,#15405) ;
#11290 = LINE('',#119030,#15406) ;
#11291 = LINE('',#119034,#15407) ;
#11292 = LINE('',#119038,#15408) ;
#11293 = LINE('',#119043,#15409) ;
#11294 = LINE('',#119047,#15410) ;
#11295 = LINE('',#119051,#15411) ;
#11296 = LINE('',#119055,#15412) ;
#11297 = LINE('',#119060,#15413) ;
#11298 = LINE('',#119064,#15414) ;
#11299 = LINE('',#119068,#15415) ;
#11300 = LINE('',#119072,#15416) ;
#11301 = LINE('',#119077,#15417) ;
#11302 = LINE('',#119081,#15418) ;
#11303 = LINE('',#119085,#15419) ;
#11304 = LINE('',#119089,#15420) ;
#11305 = LINE('',#119117,#15421) ;
#11306 = LINE('',#119174,#15422) ;
#11307 = LINE('',#119199,#15423) ;
#11308 = LINE('',#119231,#15424) ;
#11309 = LINE('',#119257,#15425) ;
#11310 = LINE('',#119821,#15426) ;
#11311 = LINE('',#119878,#15427) ;
#11312 = LINE('',#119903,#15428) ;
#11313 = LINE('',#119935,#15429) ;
#11314 = LINE('',#119961,#15430) ;
#11315 = LINE('',#120048,#15431) ;
#11316 = LINE('',#120105,#15432) ;
#11317 = LINE('',#120130,#15433) ;
#11318 = LINE('',#120162,#15434) ;
#11319 = LINE('',#120188,#15435) ;
#11320 = LINE('',#120275,#15436) ;
#11321 = LINE('',#120332,#15437) ;
#11322 = LINE('',#120357,#15438) ;
#11323 = LINE('',#120389,#15439) ;
#11324 = LINE('',#120415,#15440) ;
#11325 = LINE('',#120502,#15441) ;
#11326 = LINE('',#120559,#15442) ;
#11327 = LINE('',#120584,#15443) ;
#11328 = LINE('',#120616,#15444) ;
#11329 = LINE('',#120642,#15445) ;
#11330 = LINE('',#120729,#15446) ;
#11331 = LINE('',#120786,#15447) ;
#11332 = LINE('',#120811,#15448) ;
#11333 = LINE('',#120843,#15449) ;
#11334 = LINE('',#120869,#15450) ;
#11335 = LINE('',#120956,#15451) ;
#11336 = LINE('',#121013,#15452) ;
#11337 = LINE('',#121038,#15453) ;
#11338 = LINE('',#121070,#15454) ;
#11339 = LINE('',#121096,#15455) ;
#11340 = LINE('',#121183,#15456) ;
#11341 = LINE('',#121240,#15457) ;
#11342 = LINE('',#121265,#15458) ;
#11343 = LINE('',#121297,#15459) ;
#11344 = LINE('',#121323,#15460) ;
#11345 = LINE('',#121410,#15461) ;
#11346 = LINE('',#121467,#15462) ;
#11347 = LINE('',#121492,#15463) ;
#11348 = LINE('',#121524,#15464) ;
#11349 = LINE('',#121550,#15465) ;
#11350 = LINE('',#121614,#15466) ;
#11351 = LINE('',#121616,#15467) ;
#11352 = LINE('',#121618,#15468) ;
#11353 = LINE('',#121619,#15469) ;
#11354 = LINE('',#121623,#15470) ;
#11355 = LINE('',#121625,#15471) ;
#11356 = LINE('',#121627,#15472) ;
#11357 = LINE('',#121628,#15473) ;
#11358 = LINE('',#121632,#15474) ;
#11359 = LINE('',#121634,#15475) ;
#11360 = LINE('',#121636,#15476) ;
#11361 = LINE('',#121637,#15477) ;
#11362 = LINE('',#121641,#15478) ;
#11363 = LINE('',#121643,#15479) ;
#11364 = LINE('',#121645,#15480) ;
#11365 = LINE('',#121646,#15481) ;
#11366 = LINE('',#121650,#15482) ;
#11367 = LINE('',#121652,#15483) ;
#11368 = LINE('',#121654,#15484) ;
#11369 = LINE('',#121655,#15485) ;
#11370 = LINE('',#121659,#15486) ;
#11371 = LINE('',#121664,#15487) ;
#11372 = LINE('',#121665,#15488) ;
#11373 = LINE('',#121669,#15489) ;
#11374 = LINE('',#121674,#15490) ;
#11375 = LINE('',#121675,#15491) ;
#11376 = LINE('',#121685,#15492) ;
#11377 = LINE('',#121687,#15493) ;
#11378 = LINE('',#121689,#15494) ;
#11379 = LINE('',#121690,#15495) ;
#11380 = LINE('',#121694,#15496) ;
#11381 = LINE('',#121695,#15497) ;
#11382 = LINE('',#121696,#15498) ;
#11383 = LINE('',#121699,#15499) ;
#11384 = LINE('',#121701,#15500) ;
#11385 = LINE('',#121702,#15501) ;
#11386 = LINE('',#121706,#15502) ;
#11387 = LINE('',#121708,#15503) ;
#11388 = LINE('',#121710,#15504) ;
#11389 = LINE('',#121711,#15505) ;
#11390 = LINE('',#121715,#15506) ;
#11391 = LINE('',#121717,#15507) ;
#11392 = LINE('',#121719,#15508) ;
#11393 = LINE('',#121720,#15509) ;
#11394 = LINE('',#121724,#15510) ;
#11395 = LINE('',#121725,#15511) ;
#11396 = LINE('',#121726,#15512) ;
#11397 = LINE('',#121729,#15513) ;
#11398 = LINE('',#121731,#15514) ;
#11399 = LINE('',#121732,#15515) ;
#11400 = LINE('',#121736,#15516) ;
#11401 = LINE('',#121738,#15517) ;
#11402 = LINE('',#121740,#15518) ;
#11403 = LINE('',#121741,#15519) ;
#11404 = LINE('',#121745,#15520) ;
#11405 = LINE('',#121747,#15521) ;
#11406 = LINE('',#121749,#15522) ;
#11407 = LINE('',#121750,#15523) ;
#11408 = LINE('',#121754,#15524) ;
#11409 = LINE('',#121756,#15525) ;
#11410 = LINE('',#121758,#15526) ;
#11411 = LINE('',#121759,#15527) ;
#11412 = LINE('',#121763,#15528) ;
#11413 = LINE('',#121765,#15529) ;
#11414 = LINE('',#121767,#15530) ;
#11415 = LINE('',#121768,#15531) ;
#11416 = LINE('',#121772,#15532) ;
#11417 = LINE('',#121774,#15533) ;
#11418 = LINE('',#121776,#15534) ;
#11419 = LINE('',#121777,#15535) ;
#11420 = LINE('',#121781,#15536) ;
#11421 = LINE('',#121786,#15537) ;
#11422 = LINE('',#121787,#15538) ;
#11423 = LINE('',#121791,#15539) ;
#11424 = LINE('',#121796,#15540) ;
#11425 = LINE('',#121797,#15541) ;
#11426 = LINE('',#121807,#15542) ;
#11427 = LINE('',#121809,#15543) ;
#11428 = LINE('',#121811,#15544) ;
#11429 = LINE('',#121812,#15545) ;
#11430 = LINE('',#121816,#15546) ;
#11431 = LINE('',#121817,#15547) ;
#11432 = LINE('',#121818,#15548) ;
#11433 = LINE('',#121821,#15549) ;
#11434 = LINE('',#121823,#15550) ;
#11435 = LINE('',#121824,#15551) ;
#11436 = LINE('',#121828,#15552) ;
#11437 = LINE('',#121830,#15553) ;
#11438 = LINE('',#121832,#15554) ;
#11439 = LINE('',#121833,#15555) ;
#11440 = LINE('',#121837,#15556) ;
#11441 = LINE('',#121839,#15557) ;
#11442 = LINE('',#121841,#15558) ;
#11443 = LINE('',#121842,#15559) ;
#11444 = LINE('',#121846,#15560) ;
#11445 = LINE('',#121847,#15561) ;
#11446 = LINE('',#121848,#15562) ;
#11447 = LINE('',#121851,#15563) ;
#11448 = LINE('',#121853,#15564) ;
#11449 = LINE('',#121854,#15565) ;
#11450 = LINE('',#121858,#15566) ;
#11451 = LINE('',#121860,#15567) ;
#11452 = LINE('',#121862,#15568) ;
#11453 = LINE('',#121863,#15569) ;
#11454 = LINE('',#121867,#15570) ;
#11455 = LINE('',#121869,#15571) ;
#11456 = LINE('',#121871,#15572) ;
#11457 = LINE('',#121872,#15573) ;
#11458 = LINE('',#121876,#15574) ;
#11459 = LINE('',#121878,#15575) ;
#11460 = LINE('',#121880,#15576) ;
#11461 = LINE('',#121881,#15577) ;
#11462 = LINE('',#121885,#15578) ;
#11463 = LINE('',#121887,#15579) ;
#11464 = LINE('',#121889,#15580) ;
#11465 = LINE('',#121890,#15581) ;
#11466 = LINE('',#121894,#15582) ;
#11467 = LINE('',#121896,#15583) ;
#11468 = LINE('',#121898,#15584) ;
#11469 = LINE('',#121899,#15585) ;
#11470 = LINE('',#121903,#15586) ;
#11471 = LINE('',#121908,#15587) ;
#11472 = LINE('',#121909,#15588) ;
#11473 = LINE('',#121913,#15589) ;
#11474 = LINE('',#121918,#15590) ;
#11475 = LINE('',#121919,#15591) ;
#11476 = LINE('',#121929,#15592) ;
#11477 = LINE('',#121931,#15593) ;
#11478 = LINE('',#121933,#15594) ;
#11479 = LINE('',#121934,#15595) ;
#11480 = LINE('',#121938,#15596) ;
#11481 = LINE('',#121939,#15597) ;
#11482 = LINE('',#121940,#15598) ;
#11483 = LINE('',#121943,#15599) ;
#11484 = LINE('',#121945,#15600) ;
#11485 = LINE('',#121946,#15601) ;
#11486 = LINE('',#121950,#15602) ;
#11487 = LINE('',#121952,#15603) ;
#11488 = LINE('',#121954,#15604) ;
#11489 = LINE('',#121955,#15605) ;
#11490 = LINE('',#121959,#15606) ;
#11491 = LINE('',#121961,#15607) ;
#11492 = LINE('',#121963,#15608) ;
#11493 = LINE('',#121964,#15609) ;
#11494 = LINE('',#121968,#15610) ;
#11495 = LINE('',#121969,#15611) ;
#11496 = LINE('',#121970,#15612) ;
#11497 = LINE('',#121973,#15613) ;
#11498 = LINE('',#121975,#15614) ;
#11499 = LINE('',#121976,#15615) ;
#11500 = LINE('',#121980,#15616) ;
#11501 = LINE('',#121982,#15617) ;
#11502 = LINE('',#121984,#15618) ;
#11503 = LINE('',#121985,#15619) ;
#11504 = LINE('',#121989,#15620) ;
#11505 = LINE('',#121991,#15621) ;
#11506 = LINE('',#121993,#15622) ;
#11507 = LINE('',#121994,#15623) ;
#11508 = LINE('',#121998,#15624) ;
#11509 = LINE('',#122000,#15625) ;
#11510 = LINE('',#122002,#15626) ;
#11511 = LINE('',#122003,#15627) ;
#11512 = LINE('',#122007,#15628) ;
#11513 = LINE('',#122009,#15629) ;
#11514 = LINE('',#122011,#15630) ;
#11515 = LINE('',#122012,#15631) ;
#11516 = LINE('',#122016,#15632) ;
#11517 = LINE('',#122018,#15633) ;
#11518 = LINE('',#122020,#15634) ;
#11519 = LINE('',#122021,#15635) ;
#11520 = LINE('',#122025,#15636) ;
#11521 = LINE('',#122030,#15637) ;
#11522 = LINE('',#122031,#15638) ;
#11523 = LINE('',#122035,#15639) ;
#11524 = LINE('',#122040,#15640) ;
#11525 = LINE('',#122041,#15641) ;
#11526 = LINE('',#122051,#15642) ;
#11527 = LINE('',#122053,#15643) ;
#11528 = LINE('',#122055,#15644) ;
#11529 = LINE('',#122056,#15645) ;
#11530 = LINE('',#122060,#15646) ;
#11531 = LINE('',#122061,#15647) ;
#11532 = LINE('',#122062,#15648) ;
#11533 = LINE('',#122065,#15649) ;
#11534 = LINE('',#122067,#15650) ;
#11535 = LINE('',#122068,#15651) ;
#11536 = LINE('',#122072,#15652) ;
#11537 = LINE('',#122074,#15653) ;
#11538 = LINE('',#122076,#15654) ;
#11539 = LINE('',#122077,#15655) ;
#11540 = LINE('',#122081,#15656) ;
#11541 = LINE('',#122083,#15657) ;
#11542 = LINE('',#122085,#15658) ;
#11543 = LINE('',#122086,#15659) ;
#11544 = LINE('',#122090,#15660) ;
#11545 = LINE('',#122091,#15661) ;
#11546 = LINE('',#122092,#15662) ;
#11547 = LINE('',#122095,#15663) ;
#11548 = LINE('',#122097,#15664) ;
#11549 = LINE('',#122098,#15665) ;
#11550 = LINE('',#122102,#15666) ;
#11551 = LINE('',#122104,#15667) ;
#11552 = LINE('',#122106,#15668) ;
#11553 = LINE('',#122107,#15669) ;
#11554 = LINE('',#122111,#15670) ;
#11555 = LINE('',#122113,#15671) ;
#11556 = LINE('',#122115,#15672) ;
#11557 = LINE('',#122116,#15673) ;
#11558 = LINE('',#122120,#15674) ;
#11559 = LINE('',#122122,#15675) ;
#11560 = LINE('',#122124,#15676) ;
#11561 = LINE('',#122125,#15677) ;
#11562 = LINE('',#122129,#15678) ;
#11563 = LINE('',#122131,#15679) ;
#11564 = LINE('',#122133,#15680) ;
#11565 = LINE('',#122134,#15681) ;
#11566 = LINE('',#122138,#15682) ;
#11567 = LINE('',#122140,#15683) ;
#11568 = LINE('',#122142,#15684) ;
#11569 = LINE('',#122143,#15685) ;
#11570 = LINE('',#122147,#15686) ;
#11571 = LINE('',#122152,#15687) ;
#11572 = LINE('',#122153,#15688) ;
#11573 = LINE('',#122157,#15689) ;
#11574 = LINE('',#122162,#15690) ;
#11575 = LINE('',#122163,#15691) ;
#11576 = LINE('',#122173,#15692) ;
#11577 = LINE('',#122175,#15693) ;
#11578 = LINE('',#122177,#15694) ;
#11579 = LINE('',#122178,#15695) ;
#11580 = LINE('',#122182,#15696) ;
#11581 = LINE('',#122183,#15697) ;
#11582 = LINE('',#122184,#15698) ;
#11583 = LINE('',#122187,#15699) ;
#11584 = LINE('',#122189,#15700) ;
#11585 = LINE('',#122190,#15701) ;
#11586 = LINE('',#122194,#15702) ;
#11587 = LINE('',#122196,#15703) ;
#11588 = LINE('',#122198,#15704) ;
#11589 = LINE('',#122199,#15705) ;
#11590 = LINE('',#122203,#15706) ;
#11591 = LINE('',#122205,#15707) ;
#11592 = LINE('',#122207,#15708) ;
#11593 = LINE('',#122208,#15709) ;
#11594 = LINE('',#122212,#15710) ;
#11595 = LINE('',#122213,#15711) ;
#11596 = LINE('',#122214,#15712) ;
#11597 = LINE('',#122217,#15713) ;
#11598 = LINE('',#122219,#15714) ;
#11599 = LINE('',#122220,#15715) ;
#11600 = LINE('',#122224,#15716) ;
#11601 = LINE('',#122226,#15717) ;
#11602 = LINE('',#122228,#15718) ;
#11603 = LINE('',#122229,#15719) ;
#11604 = LINE('',#122233,#15720) ;
#11605 = LINE('',#122235,#15721) ;
#11606 = LINE('',#122237,#15722) ;
#11607 = LINE('',#122238,#15723) ;
#11608 = LINE('',#122242,#15724) ;
#11609 = LINE('',#122244,#15725) ;
#11610 = LINE('',#122246,#15726) ;
#11611 = LINE('',#122247,#15727) ;
#11612 = LINE('',#122251,#15728) ;
#11613 = LINE('',#122253,#15729) ;
#11614 = LINE('',#122255,#15730) ;
#11615 = LINE('',#122256,#15731) ;
#11616 = LINE('',#122260,#15732) ;
#11617 = LINE('',#122262,#15733) ;
#11618 = LINE('',#122264,#15734) ;
#11619 = LINE('',#122265,#15735) ;
#11620 = LINE('',#122269,#15736) ;
#11621 = LINE('',#122274,#15737) ;
#11622 = LINE('',#122275,#15738) ;
#11623 = LINE('',#122279,#15739) ;
#11624 = LINE('',#122284,#15740) ;
#11625 = LINE('',#122285,#15741) ;
#11626 = LINE('',#122295,#15742) ;
#11627 = LINE('',#122297,#15743) ;
#11628 = LINE('',#122299,#15744) ;
#11629 = LINE('',#122300,#15745) ;
#11630 = LINE('',#122304,#15746) ;
#11631 = LINE('',#122305,#15747) ;
#11632 = LINE('',#122306,#15748) ;
#11633 = LINE('',#122309,#15749) ;
#11634 = LINE('',#122311,#15750) ;
#11635 = LINE('',#122312,#15751) ;
#11636 = LINE('',#122316,#15752) ;
#11637 = LINE('',#122318,#15753) ;
#11638 = LINE('',#122320,#15754) ;
#11639 = LINE('',#122321,#15755) ;
#11640 = LINE('',#122325,#15756) ;
#11641 = LINE('',#122327,#15757) ;
#11642 = LINE('',#122329,#15758) ;
#11643 = LINE('',#122330,#15759) ;
#11644 = LINE('',#122334,#15760) ;
#11645 = LINE('',#122335,#15761) ;
#11646 = LINE('',#122336,#15762) ;
#11647 = LINE('',#122339,#15763) ;
#11648 = LINE('',#122341,#15764) ;
#11649 = LINE('',#122342,#15765) ;
#11650 = LINE('',#122346,#15766) ;
#11651 = LINE('',#122348,#15767) ;
#11652 = LINE('',#122350,#15768) ;
#11653 = LINE('',#122351,#15769) ;
#11654 = LINE('',#122355,#15770) ;
#11655 = LINE('',#122357,#15771) ;
#11656 = LINE('',#122359,#15772) ;
#11657 = LINE('',#122360,#15773) ;
#11658 = LINE('',#122364,#15774) ;
#11659 = LINE('',#122366,#15775) ;
#11660 = LINE('',#122368,#15776) ;
#11661 = LINE('',#122369,#15777) ;
#11662 = LINE('',#122373,#15778) ;
#11663 = LINE('',#122375,#15779) ;
#11664 = LINE('',#122377,#15780) ;
#11665 = LINE('',#122378,#15781) ;
#11666 = LINE('',#122382,#15782) ;
#11667 = LINE('',#122384,#15783) ;
#11668 = LINE('',#122386,#15784) ;
#11669 = LINE('',#122387,#15785) ;
#11670 = LINE('',#122391,#15786) ;
#11671 = LINE('',#122396,#15787) ;
#11672 = LINE('',#122397,#15788) ;
#11673 = LINE('',#122401,#15789) ;
#11674 = LINE('',#122406,#15790) ;
#11675 = LINE('',#122407,#15791) ;
#11676 = LINE('',#122417,#15792) ;
#11677 = LINE('',#122419,#15793) ;
#11678 = LINE('',#122421,#15794) ;
#11679 = LINE('',#122422,#15795) ;
#11680 = LINE('',#122426,#15796) ;
#11681 = LINE('',#122427,#15797) ;
#11682 = LINE('',#122428,#15798) ;
#11683 = LINE('',#122431,#15799) ;
#11684 = LINE('',#122433,#15800) ;
#11685 = LINE('',#122434,#15801) ;
#11686 = LINE('',#122438,#15802) ;
#11687 = LINE('',#122440,#15803) ;
#11688 = LINE('',#122442,#15804) ;
#11689 = LINE('',#122443,#15805) ;
#11690 = LINE('',#122447,#15806) ;
#11691 = LINE('',#122449,#15807) ;
#11692 = LINE('',#122451,#15808) ;
#11693 = LINE('',#122452,#15809) ;
#11694 = LINE('',#122456,#15810) ;
#11695 = LINE('',#122457,#15811) ;
#11696 = LINE('',#122458,#15812) ;
#11697 = LINE('',#122461,#15813) ;
#11698 = LINE('',#122463,#15814) ;
#11699 = LINE('',#122464,#15815) ;
#11700 = LINE('',#122468,#15816) ;
#11701 = LINE('',#122470,#15817) ;
#11702 = LINE('',#122472,#15818) ;
#11703 = LINE('',#122473,#15819) ;
#11704 = LINE('',#122477,#15820) ;
#11705 = LINE('',#122479,#15821) ;
#11706 = LINE('',#122481,#15822) ;
#11707 = LINE('',#122482,#15823) ;
#11708 = LINE('',#122486,#15824) ;
#11709 = LINE('',#122488,#15825) ;
#11710 = LINE('',#122490,#15826) ;
#11711 = LINE('',#122491,#15827) ;
#11712 = LINE('',#122495,#15828) ;
#11713 = LINE('',#122497,#15829) ;
#11714 = LINE('',#122499,#15830) ;
#11715 = LINE('',#122500,#15831) ;
#11716 = LINE('',#122504,#15832) ;
#11717 = LINE('',#122506,#15833) ;
#11718 = LINE('',#122508,#15834) ;
#11719 = LINE('',#122509,#15835) ;
#11720 = LINE('',#122513,#15836) ;
#11721 = LINE('',#122518,#15837) ;
#11722 = LINE('',#122519,#15838) ;
#11723 = LINE('',#122523,#15839) ;
#11724 = LINE('',#122528,#15840) ;
#11725 = LINE('',#122529,#15841) ;
#11726 = LINE('',#122539,#15842) ;
#11727 = LINE('',#122541,#15843) ;
#11728 = LINE('',#122543,#15844) ;
#11729 = LINE('',#122544,#15845) ;
#11730 = LINE('',#122548,#15846) ;
#11731 = LINE('',#122549,#15847) ;
#11732 = LINE('',#122550,#15848) ;
#11733 = LINE('',#122553,#15849) ;
#11734 = LINE('',#122555,#15850) ;
#11735 = LINE('',#122556,#15851) ;
#11736 = LINE('',#122560,#15852) ;
#11737 = LINE('',#122562,#15853) ;
#11738 = LINE('',#122564,#15854) ;
#11739 = LINE('',#122565,#15855) ;
#11740 = LINE('',#122569,#15856) ;
#11741 = LINE('',#122571,#15857) ;
#11742 = LINE('',#122573,#15858) ;
#11743 = LINE('',#122574,#15859) ;
#11744 = LINE('',#122578,#15860) ;
#11745 = LINE('',#122579,#15861) ;
#11746 = LINE('',#122580,#15862) ;
#11747 = LINE('',#122583,#15863) ;
#11748 = LINE('',#122585,#15864) ;
#11749 = LINE('',#122586,#15865) ;
#11750 = LINE('',#122590,#15866) ;
#11751 = LINE('',#122592,#15867) ;
#11752 = LINE('',#122594,#15868) ;
#11753 = LINE('',#122595,#15869) ;
#11754 = LINE('',#122599,#15870) ;
#11755 = LINE('',#122601,#15871) ;
#11756 = LINE('',#122603,#15872) ;
#11757 = LINE('',#122604,#15873) ;
#11758 = LINE('',#122608,#15874) ;
#11759 = LINE('',#122610,#15875) ;
#11760 = LINE('',#122612,#15876) ;
#11761 = LINE('',#122613,#15877) ;
#11762 = LINE('',#122617,#15878) ;
#11763 = LINE('',#122619,#15879) ;
#11764 = LINE('',#122621,#15880) ;
#11765 = LINE('',#122622,#15881) ;
#11766 = LINE('',#122626,#15882) ;
#11767 = LINE('',#122628,#15883) ;
#11768 = LINE('',#122630,#15884) ;
#11769 = LINE('',#122631,#15885) ;
#11770 = LINE('',#122635,#15886) ;
#11771 = LINE('',#122640,#15887) ;
#11772 = LINE('',#122641,#15888) ;
#11773 = LINE('',#122645,#15889) ;
#11774 = LINE('',#122650,#15890) ;
#11775 = LINE('',#122651,#15891) ;
#11776 = LINE('',#122661,#15892) ;
#11777 = LINE('',#122663,#15893) ;
#11778 = LINE('',#122665,#15894) ;
#11779 = LINE('',#122666,#15895) ;
#11780 = LINE('',#122670,#15896) ;
#11781 = LINE('',#122671,#15897) ;
#11782 = LINE('',#122672,#15898) ;
#11783 = LINE('',#122675,#15899) ;
#11784 = LINE('',#122677,#15900) ;
#11785 = LINE('',#122678,#15901) ;
#11786 = LINE('',#122682,#15902) ;
#11787 = LINE('',#122684,#15903) ;
#11788 = LINE('',#122686,#15904) ;
#11789 = LINE('',#122687,#15905) ;
#11790 = LINE('',#122691,#15906) ;
#11791 = LINE('',#122693,#15907) ;
#11792 = LINE('',#122695,#15908) ;
#11793 = LINE('',#122696,#15909) ;
#11794 = LINE('',#122700,#15910) ;
#11795 = LINE('',#122701,#15911) ;
#11796 = LINE('',#122702,#15912) ;
#11797 = LINE('',#122705,#15913) ;
#11798 = LINE('',#122707,#15914) ;
#11799 = LINE('',#122708,#15915) ;
#11800 = LINE('',#122712,#15916) ;
#11801 = LINE('',#122714,#15917) ;
#11802 = LINE('',#122716,#15918) ;
#11803 = LINE('',#122717,#15919) ;
#11804 = LINE('',#122721,#15920) ;
#11805 = LINE('',#122723,#15921) ;
#11806 = LINE('',#122725,#15922) ;
#11807 = LINE('',#122726,#15923) ;
#11808 = LINE('',#122730,#15924) ;
#11809 = LINE('',#122732,#15925) ;
#11810 = LINE('',#122734,#15926) ;
#11811 = LINE('',#122735,#15927) ;
#11812 = LINE('',#122739,#15928) ;
#11813 = LINE('',#122741,#15929) ;
#11814 = LINE('',#122743,#15930) ;
#11815 = LINE('',#122744,#15931) ;
#11816 = LINE('',#122748,#15932) ;
#11817 = LINE('',#122750,#15933) ;
#11818 = LINE('',#122752,#15934) ;
#11819 = LINE('',#122753,#15935) ;
#11820 = LINE('',#122757,#15936) ;
#11821 = LINE('',#122759,#15937) ;
#11822 = LINE('',#122761,#15938) ;
#11823 = LINE('',#122762,#15939) ;
#11824 = LINE('',#122766,#15940) ;
#11825 = LINE('',#122768,#15941) ;
#11826 = LINE('',#122770,#15942) ;
#11827 = LINE('',#122771,#15943) ;
#11828 = LINE('',#122775,#15944) ;
#11829 = LINE('',#122777,#15945) ;
#11830 = LINE('',#122779,#15946) ;
#11831 = LINE('',#122780,#15947) ;
#11832 = LINE('',#122784,#15948) ;
#11833 = LINE('',#122786,#15949) ;
#11834 = LINE('',#122788,#15950) ;
#11835 = LINE('',#122789,#15951) ;
#11836 = LINE('',#122793,#15952) ;
#11837 = LINE('',#122795,#15953) ;
#11838 = LINE('',#122797,#15954) ;
#11839 = LINE('',#122798,#15955) ;
#11840 = LINE('',#122802,#15956) ;
#11841 = LINE('',#122804,#15957) ;
#11842 = LINE('',#122806,#15958) ;
#11843 = LINE('',#122807,#15959) ;
#11844 = LINE('',#122811,#15960) ;
#11845 = LINE('',#122813,#15961) ;
#11846 = LINE('',#122815,#15962) ;
#11847 = LINE('',#122816,#15963) ;
#11848 = LINE('',#122820,#15964) ;
#11849 = LINE('',#122822,#15965) ;
#11850 = LINE('',#122824,#15966) ;
#11851 = LINE('',#122825,#15967) ;
#11852 = LINE('',#122829,#15968) ;
#11853 = LINE('',#122831,#15969) ;
#11854 = LINE('',#122833,#15970) ;
#11855 = LINE('',#122834,#15971) ;
#11856 = LINE('',#122838,#15972) ;
#11857 = LINE('',#122840,#15973) ;
#11858 = LINE('',#122842,#15974) ;
#11859 = LINE('',#122843,#15975) ;
#11860 = LINE('',#122847,#15976) ;
#11861 = LINE('',#122849,#15977) ;
#11862 = LINE('',#122851,#15978) ;
#11863 = LINE('',#122852,#15979) ;
#11864 = LINE('',#122856,#15980) ;
#11865 = LINE('',#122858,#15981) ;
#11866 = LINE('',#122860,#15982) ;
#11867 = LINE('',#122861,#15983) ;
#11868 = LINE('',#122865,#15984) ;
#11869 = LINE('',#122867,#15985) ;
#11870 = LINE('',#122869,#15986) ;
#11871 = LINE('',#122870,#15987) ;
#11872 = LINE('',#122874,#15988) ;
#11873 = LINE('',#122876,#15989) ;
#11874 = LINE('',#122878,#15990) ;
#11875 = LINE('',#122879,#15991) ;
#11876 = LINE('',#122883,#15992) ;
#11877 = LINE('',#122885,#15993) ;
#11878 = LINE('',#122887,#15994) ;
#11879 = LINE('',#122888,#15995) ;
#11880 = LINE('',#122892,#15996) ;
#11881 = LINE('',#122894,#15997) ;
#11882 = LINE('',#122896,#15998) ;
#11883 = LINE('',#122897,#15999) ;
#11884 = LINE('',#122901,#16000) ;
#11885 = LINE('',#122903,#16001) ;
#11886 = LINE('',#122905,#16002) ;
#11887 = LINE('',#122906,#16003) ;
#11888 = LINE('',#122910,#16004) ;
#11889 = LINE('',#122912,#16005) ;
#11890 = LINE('',#122914,#16006) ;
#11891 = LINE('',#122915,#16007) ;
#11892 = LINE('',#122919,#16008) ;
#11893 = LINE('',#122921,#16009) ;
#11894 = LINE('',#122923,#16010) ;
#11895 = LINE('',#122924,#16011) ;
#11896 = LINE('',#122928,#16012) ;
#11897 = LINE('',#122930,#16013) ;
#11898 = LINE('',#122932,#16014) ;
#11899 = LINE('',#122933,#16015) ;
#11900 = LINE('',#122937,#16016) ;
#11901 = LINE('',#122939,#16017) ;
#11902 = LINE('',#122941,#16018) ;
#11903 = LINE('',#122942,#16019) ;
#11904 = LINE('',#122946,#16020) ;
#11905 = LINE('',#122948,#16021) ;
#11906 = LINE('',#122950,#16022) ;
#11907 = LINE('',#122951,#16023) ;
#11908 = LINE('',#122955,#16024) ;
#11909 = LINE('',#122957,#16025) ;
#11910 = LINE('',#122959,#16026) ;
#11911 = LINE('',#122960,#16027) ;
#11912 = LINE('',#122964,#16028) ;
#11913 = LINE('',#122966,#16029) ;
#11914 = LINE('',#122968,#16030) ;
#11915 = LINE('',#122969,#16031) ;
#11916 = LINE('',#122973,#16032) ;
#11917 = LINE('',#122975,#16033) ;
#11918 = LINE('',#122977,#16034) ;
#11919 = LINE('',#122978,#16035) ;
#11920 = LINE('',#122982,#16036) ;
#11921 = LINE('',#122984,#16037) ;
#11922 = LINE('',#122986,#16038) ;
#11923 = LINE('',#122987,#16039) ;
#11924 = LINE('',#122991,#16040) ;
#11925 = LINE('',#122993,#16041) ;
#11926 = LINE('',#122995,#16042) ;
#11927 = LINE('',#122996,#16043) ;
#11928 = LINE('',#123000,#16044) ;
#11929 = LINE('',#123002,#16045) ;
#11930 = LINE('',#123004,#16046) ;
#11931 = LINE('',#123005,#16047) ;
#11932 = LINE('',#123009,#16048) ;
#11933 = LINE('',#123011,#16049) ;
#11934 = LINE('',#123013,#16050) ;
#11935 = LINE('',#123014,#16051) ;
#11936 = LINE('',#123018,#16052) ;
#11937 = LINE('',#123020,#16053) ;
#11938 = LINE('',#123022,#16054) ;
#11939 = LINE('',#123023,#16055) ;
#11940 = LINE('',#123027,#16056) ;
#11941 = LINE('',#123029,#16057) ;
#11942 = LINE('',#123031,#16058) ;
#11943 = LINE('',#123032,#16059) ;
#11944 = LINE('',#124045,#16060) ;
#11945 = LINE('',#124068,#16061) ;
#11946 = LINE('',#124092,#16062) ;
#11947 = LINE('',#124172,#16063) ;
#11948 = LINE('',#124248,#16064) ;
#11949 = LINE('',#124324,#16065) ;
#11950 = LINE('',#124400,#16066) ;
#11951 = LINE('',#124476,#16067) ;
#11952 = LINE('',#124552,#16068) ;
#11953 = LINE('',#124628,#16069) ;
#11954 = LINE('',#124708,#16070) ;
#11955 = LINE('',#124784,#16071) ;
#11956 = LINE('',#124811,#16072) ;
#11957 = LINE('',#124887,#16073) ;
#11958 = LINE('',#124963,#16074) ;
#11959 = LINE('',#125039,#16075) ;
#11960 = LINE('',#125115,#16076) ;
#11961 = LINE('',#125191,#16077) ;
#11962 = LINE('',#125269,#16078) ;
#11963 = LINE('',#125348,#16079) ;
#11964 = LINE('',#125381,#16080) ;
#11965 = LINE('',#125416,#16081) ;
#11966 = LINE('',#125570,#16082) ;
#11967 = LINE('',#125575,#16083) ;
#11968 = LINE('',#125578,#16084) ;
#11969 = LINE('',#125616,#16085) ;
#11970 = LINE('',#125641,#16086) ;
#11971 = LINE('',#125645,#16087) ;
#11972 = LINE('',#125650,#16088) ;
#11973 = LINE('',#125654,#16089) ;
#11974 = LINE('',#125659,#16090) ;
#11975 = LINE('',#125663,#16091) ;
#11976 = LINE('',#125668,#16092) ;
#11977 = LINE('',#125672,#16093) ;
#11978 = LINE('',#125677,#16094) ;
#11979 = LINE('',#125681,#16095) ;
#11980 = LINE('',#125686,#16096) ;
#11981 = LINE('',#125690,#16097) ;
#11982 = LINE('',#126079,#16098) ;
#11983 = LINE('',#126363,#16099) ;
#11984 = LINE('',#126365,#16100) ;
#11985 = LINE('',#126371,#16101) ;
#11986 = LINE('',#126421,#16102) ;
#11987 = LINE('',#126425,#16103) ;
#11988 = LINE('',#126465,#16104) ;
#11989 = LINE('',#126466,#16105) ;
#11990 = LINE('',#126469,#16106) ;
#11991 = LINE('',#126473,#16107) ;
#11992 = LINE('',#126476,#16108) ;
#11993 = LINE('',#126480,#16109) ;
#11994 = LINE('',#126486,#16110) ;
#11995 = LINE('',#126487,#16111) ;
#11996 = LINE('',#126490,#16112) ;
#11997 = LINE('',#126491,#16113) ;
#11998 = LINE('',#126494,#16114) ;
#11999 = LINE('',#126495,#16115) ;
#12000 = LINE('',#126498,#16116) ;
#12001 = LINE('',#126499,#16117) ;
#12002 = LINE('',#126504,#16118) ;
#12003 = LINE('',#126505,#16119) ;
#12004 = LINE('',#126508,#16120) ;
#12005 = LINE('',#126509,#16121) ;
#12006 = LINE('',#126517,#16122) ;
#12007 = LINE('',#126518,#16123) ;
#12008 = LINE('',#126523,#16124) ;
#12009 = LINE('',#126525,#16125) ;
#12010 = LINE('',#126528,#16126) ;
#12011 = LINE('',#126529,#16127) ;
#12012 = VECTOR('',#76918,1.6) ;
#12013 = VECTOR('',#76923,1.49999999999999) ;
#12014 = VECTOR('',#76926,1.6) ;
#12015 = VECTOR('',#76931,1.49999999999999) ;
#12016 = VECTOR('',#76934,1.6) ;
#12017 = VECTOR('',#76937,1000.) ;
#12018 = VECTOR('',#76938,1000.) ;
#12019 = VECTOR('',#76939,1000.) ;
#12020 = VECTOR('',#76940,1000.) ;
#12021 = VECTOR('',#76941,1000.) ;
#12022 = VECTOR('',#76942,1000.) ;
#12023 = VECTOR('',#76945,1000.) ;
#12024 = VECTOR('',#76948,1000.) ;
#12025 = VECTOR('',#76951,1000.) ;
#12026 = VECTOR('',#76954,1000.) ;
#12027 = VECTOR('',#76957,1000.) ;
#12028 = VECTOR('',#76958,1000.) ;
#12029 = VECTOR('',#76959,1000.) ;
#12030 = VECTOR('',#76960,1000.) ;
#12031 = VECTOR('',#76961,1000.) ;
#12032 = VECTOR('',#76962,1000.) ;
#12033 = VECTOR('',#76965,1000.) ;
#12034 = VECTOR('',#76968,1000.) ;
#12035 = VECTOR('',#76971,1000.) ;
#12036 = VECTOR('',#76974,1000.) ;
#12037 = VECTOR('',#76979,1000.) ;
#12038 = VECTOR('',#76980,1000.) ;
#12039 = VECTOR('',#76981,1000.) ;
#12040 = VECTOR('',#76982,1000.) ;
#12041 = VECTOR('',#76983,1000.) ;
#12042 = VECTOR('',#76984,1000.) ;
#12043 = VECTOR('',#76987,1000.) ;
#12044 = VECTOR('',#76988,1000.) ;
#12045 = VECTOR('',#76989,1000.) ;
#12046 = VECTOR('',#76992,1000.) ;
#12047 = VECTOR('',#76995,1000.) ;
#12048 = VECTOR('',#76998,1000.) ;
#12049 = VECTOR('',#77001,1000.) ;
#12050 = VECTOR('',#77004,1000.) ;
#12051 = VECTOR('',#77007,1000.) ;
#12052 = VECTOR('',#77010,1000.) ;
#12053 = VECTOR('',#77013,1000.) ;
#12054 = VECTOR('',#77016,1000.) ;
#12055 = VECTOR('',#77019,1000.) ;
#12056 = VECTOR('',#77022,1000.) ;
#12057 = VECTOR('',#77025,1000.) ;
#12058 = VECTOR('',#77028,1000.) ;
#12059 = VECTOR('',#77031,1000.) ;
#12060 = VECTOR('',#77034,1000.) ;
#12061 = VECTOR('',#77037,1000.) ;
#12062 = VECTOR('',#77040,1000.) ;
#12063 = VECTOR('',#77041,1000.) ;
#12064 = VECTOR('',#77044,1000.) ;
#12065 = VECTOR('',#77045,1000.) ;
#12066 = VECTOR('',#77046,1000.) ;
#12067 = VECTOR('',#77049,1000.) ;
#12068 = VECTOR('',#77050,1000.) ;
#12069 = VECTOR('',#77051,1000.) ;
#12070 = VECTOR('',#77052,1000.) ;
#12071 = VECTOR('',#77055,1000.) ;
#12072 = VECTOR('',#77058,1000.) ;
#12073 = VECTOR('',#77061,1000.) ;
#12074 = VECTOR('',#77064,1000.) ;
#12075 = VECTOR('',#77067,1000.) ;
#12076 = VECTOR('',#77070,1000.) ;
#12077 = VECTOR('',#77073,1000.) ;
#12078 = VECTOR('',#77076,1000.) ;
#12079 = VECTOR('',#77079,1000.) ;
#12080 = VECTOR('',#77082,1000.) ;
#12081 = VECTOR('',#77085,1000.) ;
#12082 = VECTOR('',#77088,1000.) ;
#12083 = VECTOR('',#77091,1000.) ;
#12084 = VECTOR('',#77094,1000.) ;
#12085 = VECTOR('',#77097,1000.) ;
#12086 = VECTOR('',#77100,1000.) ;
#12087 = VECTOR('',#77103,1000.) ;
#12088 = VECTOR('',#77104,1000.) ;
#12089 = VECTOR('',#77107,1000.) ;
#12090 = VECTOR('',#77108,1000.) ;
#12091 = VECTOR('',#77109,1000.) ;
#12092 = VECTOR('',#77112,1000.) ;
#12093 = VECTOR('',#77113,1000.) ;
#12094 = VECTOR('',#77114,1000.) ;
#12095 = VECTOR('',#77115,1000.) ;
#12096 = VECTOR('',#77118,1000.) ;
#12097 = VECTOR('',#77121,1000.) ;
#12098 = VECTOR('',#77124,1000.) ;
#12099 = VECTOR('',#77127,1000.) ;
#12100 = VECTOR('',#77130,1000.) ;
#12101 = VECTOR('',#77133,1000.) ;
#12102 = VECTOR('',#77136,1000.) ;
#12103 = VECTOR('',#77139,1000.) ;
#12104 = VECTOR('',#77142,1000.) ;
#12105 = VECTOR('',#77145,1000.) ;
#12106 = VECTOR('',#77148,1000.) ;
#12107 = VECTOR('',#77151,1000.) ;
#12108 = VECTOR('',#77154,1000.) ;
#12109 = VECTOR('',#77157,1000.) ;
#12110 = VECTOR('',#77160,1000.) ;
#12111 = VECTOR('',#77163,1000.) ;
#12112 = VECTOR('',#77166,1000.) ;
#12113 = VECTOR('',#77169,1000.) ;
#12114 = VECTOR('',#77172,1000.) ;
#12115 = VECTOR('',#77175,1000.) ;
#12116 = VECTOR('',#77178,1000.) ;
#12117 = VECTOR('',#77181,1000.) ;
#12118 = VECTOR('',#77184,1000.) ;
#12119 = VECTOR('',#77187,1000.) ;
#12120 = VECTOR('',#77190,1000.) ;
#12121 = VECTOR('',#77193,1000.) ;
#12122 = VECTOR('',#77196,1000.) ;
#12123 = VECTOR('',#77199,1000.) ;
#12124 = VECTOR('',#77204,1000.) ;
#12125 = VECTOR('',#77205,1000.) ;
#12126 = VECTOR('',#77206,1000.) ;
#12127 = VECTOR('',#77207,1000.) ;
#12128 = VECTOR('',#77208,1000.) ;
#12129 = VECTOR('',#77209,1000.) ;
#12130 = VECTOR('',#77212,1000.) ;
#12131 = VECTOR('',#77213,1000.) ;
#12132 = VECTOR('',#77214,1000.) ;
#12133 = VECTOR('',#77217,1000.) ;
#12134 = VECTOR('',#77220,1000.) ;
#12135 = VECTOR('',#77223,1000.) ;
#12136 = VECTOR('',#77226,1000.) ;
#12137 = VECTOR('',#77229,1000.) ;
#12138 = VECTOR('',#77232,1000.) ;
#12139 = VECTOR('',#77235,1000.) ;
#12140 = VECTOR('',#77238,1000.) ;
#12141 = VECTOR('',#77241,1000.) ;
#12142 = VECTOR('',#77244,1000.) ;
#12143 = VECTOR('',#77247,1000.) ;
#12144 = VECTOR('',#77250,1000.) ;
#12145 = VECTOR('',#77253,1000.) ;
#12146 = VECTOR('',#77256,1000.) ;
#12147 = VECTOR('',#77259,1000.) ;
#12148 = VECTOR('',#77262,1000.) ;
#12149 = VECTOR('',#77265,1000.) ;
#12150 = VECTOR('',#77268,1000.) ;
#12151 = VECTOR('',#77271,1000.) ;
#12152 = VECTOR('',#77274,1000.) ;
#12153 = VECTOR('',#77277,1000.) ;
#12154 = VECTOR('',#77280,1000.) ;
#12155 = VECTOR('',#77283,1000.) ;
#12156 = VECTOR('',#77286,1000.) ;
#12157 = VECTOR('',#77289,1000.) ;
#12158 = VECTOR('',#77292,1000.) ;
#12159 = VECTOR('',#77295,1000.) ;
#12160 = VECTOR('',#77298,1000.) ;
#12161 = VECTOR('',#77303,1000.) ;
#12162 = VECTOR('',#77304,1000.) ;
#12163 = VECTOR('',#77305,1000.) ;
#12164 = VECTOR('',#77306,1000.) ;
#12165 = VECTOR('',#77307,1000.) ;
#12166 = VECTOR('',#77310,1000.) ;
#12167 = VECTOR('',#77311,1000.) ;
#12168 = VECTOR('',#77312,1000.) ;
#12169 = VECTOR('',#77315,1000.) ;
#12170 = VECTOR('',#77316,1000.) ;
#12171 = VECTOR('',#77319,1000.) ;
#12172 = VECTOR('',#77320,1000.) ;
#12173 = VECTOR('',#77321,1000.) ;
#12174 = VECTOR('',#77324,1000.) ;
#12175 = VECTOR('',#77325,1000.) ;
#12176 = VECTOR('',#77326,1000.) ;
#12177 = VECTOR('',#77329,1000.) ;
#12178 = VECTOR('',#77330,1000.) ;
#12179 = VECTOR('',#77331,1000.) ;
#12180 = VECTOR('',#77332,1000.) ;
#12181 = VECTOR('',#77335,1000.) ;
#12182 = VECTOR('',#77336,1000.) ;
#12183 = VECTOR('',#77337,1000.) ;
#12184 = VECTOR('',#77338,1000.) ;
#12185 = VECTOR('',#77341,1000.) ;
#12186 = VECTOR('',#77342,1000.) ;
#12187 = VECTOR('',#77343,1000.) ;
#12188 = VECTOR('',#77344,1000.) ;
#12189 = VECTOR('',#77347,1000.) ;
#12190 = VECTOR('',#77348,1000.) ;
#12191 = VECTOR('',#77349,1000.) ;
#12192 = VECTOR('',#77350,1000.) ;
#12193 = VECTOR('',#77353,1000.) ;
#12194 = VECTOR('',#77354,1000.) ;
#12195 = VECTOR('',#77355,1000.) ;
#12196 = VECTOR('',#77356,1000.) ;
#12197 = VECTOR('',#77361,1000.) ;
#12198 = VECTOR('',#77368,1000.) ;
#12199 = VECTOR('',#77371,1000.) ;
#12200 = VECTOR('',#77382,1000.) ;
#12201 = VECTOR('',#77383,1000.) ;
#12202 = VECTOR('',#77384,1000.) ;
#12203 = VECTOR('',#77385,1000.) ;
#12204 = VECTOR('',#77388,1000.) ;
#12205 = VECTOR('',#77389,1000.) ;
#12206 = VECTOR('',#77390,1000.) ;
#12207 = VECTOR('',#77391,1000.) ;
#12208 = VECTOR('',#77394,1000.) ;
#12209 = VECTOR('',#77395,1000.) ;
#12210 = VECTOR('',#77396,1000.) ;
#12211 = VECTOR('',#77397,1000.) ;
#12212 = VECTOR('',#77400,1000.) ;
#12213 = VECTOR('',#77401,1000.) ;
#12214 = VECTOR('',#77402,1000.) ;
#12215 = VECTOR('',#77403,1000.) ;
#12216 = VECTOR('',#77406,1000.) ;
#12217 = VECTOR('',#77407,1000.) ;
#12218 = VECTOR('',#77408,1000.) ;
#12219 = VECTOR('',#77409,1000.) ;
#12220 = VECTOR('',#77412,1000.) ;
#12221 = VECTOR('',#77413,1000.) ;
#12222 = VECTOR('',#77414,1000.) ;
#12223 = VECTOR('',#77415,1000.) ;
#12224 = VECTOR('',#77418,1000.) ;
#12225 = VECTOR('',#77419,1000.) ;
#12226 = VECTOR('',#77420,1000.) ;
#12227 = VECTOR('',#77423,1000.) ;
#12228 = VECTOR('',#77426,1000.) ;
#12229 = VECTOR('',#77427,1000.) ;
#12230 = VECTOR('',#77428,1000.) ;
#12231 = VECTOR('',#77429,1000.) ;
#12232 = VECTOR('',#77432,1000.) ;
#12233 = VECTOR('',#77433,1000.) ;
#12234 = VECTOR('',#77434,1000.) ;
#12235 = VECTOR('',#77435,1000.) ;
#12236 = VECTOR('',#77438,1000.) ;
#12237 = VECTOR('',#77439,1000.) ;
#12238 = VECTOR('',#77440,1000.) ;
#12239 = VECTOR('',#77441,1000.) ;
#12240 = VECTOR('',#77444,1000.) ;
#12241 = VECTOR('',#77445,1000.) ;
#12242 = VECTOR('',#77448,1000.) ;
#12243 = VECTOR('',#77449,1000.) ;
#12244 = VECTOR('',#77454,1000.) ;
#12245 = VECTOR('',#77469,1000.) ;
#12246 = VECTOR('',#77478,1000.) ;
#12247 = VECTOR('',#77491,1000.) ;
#12248 = VECTOR('',#77492,1000.) ;
#12249 = VECTOR('',#77493,1000.) ;
#12250 = VECTOR('',#77494,1000.) ;
#12251 = VECTOR('',#77497,1000.) ;
#12252 = VECTOR('',#77498,1000.) ;
#12253 = VECTOR('',#77499,1000.) ;
#12254 = VECTOR('',#77500,1000.) ;
#12255 = VECTOR('',#77503,1000.) ;
#12256 = VECTOR('',#77504,1000.) ;
#12257 = VECTOR('',#77505,1000.) ;
#12258 = VECTOR('',#77506,1000.) ;
#12259 = VECTOR('',#77509,1000.) ;
#12260 = VECTOR('',#77510,1000.) ;
#12261 = VECTOR('',#77511,1000.) ;
#12262 = VECTOR('',#77512,1000.) ;
#12263 = VECTOR('',#77515,1000.) ;
#12264 = VECTOR('',#77516,1000.) ;
#12265 = VECTOR('',#77517,1000.) ;
#12266 = VECTOR('',#77518,1000.) ;
#12267 = VECTOR('',#77521,1000.) ;
#12268 = VECTOR('',#77522,1000.) ;
#12269 = VECTOR('',#77523,1000.) ;
#12270 = VECTOR('',#77524,1000.) ;
#12271 = VECTOR('',#77527,1000.) ;
#12272 = VECTOR('',#77530,1000.) ;
#12273 = VECTOR('',#77531,1000.) ;
#12274 = VECTOR('',#77532,1000.) ;
#12275 = VECTOR('',#77535,1000.) ;
#12276 = VECTOR('',#77536,1000.) ;
#12277 = VECTOR('',#77537,1000.) ;
#12278 = VECTOR('',#77538,1000.) ;
#12279 = VECTOR('',#77541,1000.) ;
#12280 = VECTOR('',#77542,1000.) ;
#12281 = VECTOR('',#77543,1000.) ;
#12282 = VECTOR('',#77544,1000.) ;
#12283 = VECTOR('',#77547,1000.) ;
#12284 = VECTOR('',#77548,1000.) ;
#12285 = VECTOR('',#77549,1000.) ;
#12286 = VECTOR('',#77550,1000.) ;
#12287 = VECTOR('',#77553,1000.) ;
#12288 = VECTOR('',#77554,1000.) ;
#12289 = VECTOR('',#77555,1000.) ;
#12290 = VECTOR('',#77556,1000.) ;
#12291 = VECTOR('',#77559,1000.) ;
#12292 = VECTOR('',#77560,1000.) ;
#12293 = VECTOR('',#77561,1000.) ;
#12294 = VECTOR('',#77562,1000.) ;
#12295 = VECTOR('',#77565,1000.) ;
#12296 = VECTOR('',#77566,1000.) ;
#12297 = VECTOR('',#77567,1000.) ;
#12298 = VECTOR('',#77568,1000.) ;
#12299 = VECTOR('',#77571,1000.) ;
#12300 = VECTOR('',#77572,1000.) ;
#12301 = VECTOR('',#77573,1000.) ;
#12302 = VECTOR('',#77574,1000.) ;
#12303 = VECTOR('',#77577,1000.) ;
#12304 = VECTOR('',#77578,1000.) ;
#12305 = VECTOR('',#77579,1000.) ;
#12306 = VECTOR('',#77580,1000.) ;
#12307 = VECTOR('',#77583,1000.) ;
#12308 = VECTOR('',#77584,1000.) ;
#12309 = VECTOR('',#77585,1000.) ;
#12310 = VECTOR('',#77586,1000.) ;
#12311 = VECTOR('',#77589,1000.) ;
#12312 = VECTOR('',#77590,1000.) ;
#12313 = VECTOR('',#77591,1000.) ;
#12314 = VECTOR('',#77592,1000.) ;
#12315 = VECTOR('',#77595,1000.) ;
#12316 = VECTOR('',#77596,1000.) ;
#12317 = VECTOR('',#77597,1000.) ;
#12318 = VECTOR('',#77598,1000.) ;
#12319 = VECTOR('',#77601,1000.) ;
#12320 = VECTOR('',#77602,1000.) ;
#12321 = VECTOR('',#77603,1000.) ;
#12322 = VECTOR('',#77604,1000.) ;
#12323 = VECTOR('',#77607,1000.) ;
#12324 = VECTOR('',#77608,1000.) ;
#12325 = VECTOR('',#77609,1000.) ;
#12326 = VECTOR('',#77610,1000.) ;
#12327 = VECTOR('',#77613,1000.) ;
#12328 = VECTOR('',#77614,1000.) ;
#12329 = VECTOR('',#77615,1000.) ;
#12330 = VECTOR('',#77616,1000.) ;
#12331 = VECTOR('',#77619,1000.) ;
#12332 = VECTOR('',#77620,1000.) ;
#12333 = VECTOR('',#77621,1000.) ;
#12334 = VECTOR('',#77622,1000.) ;
#12335 = VECTOR('',#77625,1000.) ;
#12336 = VECTOR('',#77626,1000.) ;
#12337 = VECTOR('',#77627,1000.) ;
#12338 = VECTOR('',#77628,1000.) ;
#12339 = VECTOR('',#77631,1000.) ;
#12340 = VECTOR('',#77632,1000.) ;
#12341 = VECTOR('',#77633,1000.) ;
#12342 = VECTOR('',#77634,1000.) ;
#12343 = VECTOR('',#77637,1000.) ;
#12344 = VECTOR('',#77638,1000.) ;
#12345 = VECTOR('',#77639,1000.) ;
#12346 = VECTOR('',#77640,1000.) ;
#12347 = VECTOR('',#77643,1000.) ;
#12348 = VECTOR('',#77644,1000.) ;
#12349 = VECTOR('',#77645,1000.) ;
#12350 = VECTOR('',#77646,1000.) ;
#12351 = VECTOR('',#77649,1000.) ;
#12352 = VECTOR('',#77650,1000.) ;
#12353 = VECTOR('',#77651,1000.) ;
#12354 = VECTOR('',#77652,1000.) ;
#12355 = VECTOR('',#77655,1000.) ;
#12356 = VECTOR('',#77656,1000.) ;
#12357 = VECTOR('',#77657,1000.) ;
#12358 = VECTOR('',#77658,1000.) ;
#12359 = VECTOR('',#77661,1000.) ;
#12360 = VECTOR('',#77662,1000.) ;
#12361 = VECTOR('',#77663,1000.) ;
#12362 = VECTOR('',#77664,1000.) ;
#12363 = VECTOR('',#77667,1000.) ;
#12364 = VECTOR('',#77668,1000.) ;
#12365 = VECTOR('',#77669,1000.) ;
#12366 = VECTOR('',#77670,1000.) ;
#12367 = VECTOR('',#77673,1000.) ;
#12368 = VECTOR('',#77674,1000.) ;
#12369 = VECTOR('',#77675,1000.) ;
#12370 = VECTOR('',#77676,1000.) ;
#12371 = VECTOR('',#77679,1000.) ;
#12372 = VECTOR('',#77680,1000.) ;
#12373 = VECTOR('',#77681,1000.) ;
#12374 = VECTOR('',#77682,1000.) ;
#12375 = VECTOR('',#77685,1000.) ;
#12376 = VECTOR('',#77686,1000.) ;
#12377 = VECTOR('',#77687,1000.) ;
#12378 = VECTOR('',#77688,1000.) ;
#12379 = VECTOR('',#77691,1000.) ;
#12380 = VECTOR('',#77692,1000.) ;
#12381 = VECTOR('',#77693,1000.) ;
#12382 = VECTOR('',#77694,1000.) ;
#12383 = VECTOR('',#77697,1000.) ;
#12384 = VECTOR('',#77698,1000.) ;
#12385 = VECTOR('',#77699,1000.) ;
#12386 = VECTOR('',#77700,1000.) ;
#12387 = VECTOR('',#77703,1000.) ;
#12388 = VECTOR('',#77704,1000.) ;
#12389 = VECTOR('',#77705,1000.) ;
#12390 = VECTOR('',#77706,1000.) ;
#12391 = VECTOR('',#77709,1000.) ;
#12392 = VECTOR('',#77710,1000.) ;
#12393 = VECTOR('',#77711,1000.) ;
#12394 = VECTOR('',#77712,1000.) ;
#12395 = VECTOR('',#77715,1000.) ;
#12396 = VECTOR('',#77716,1000.) ;
#12397 = VECTOR('',#77717,1000.) ;
#12398 = VECTOR('',#77718,1000.) ;
#12399 = VECTOR('',#77721,1000.) ;
#12400 = VECTOR('',#77722,1000.) ;
#12401 = VECTOR('',#77723,1000.) ;
#12402 = VECTOR('',#77724,1000.) ;
#12403 = VECTOR('',#77727,1000.) ;
#12404 = VECTOR('',#77728,1000.) ;
#12405 = VECTOR('',#77729,1000.) ;
#12406 = VECTOR('',#77730,1000.) ;
#12407 = VECTOR('',#77733,1000.) ;
#12408 = VECTOR('',#77734,1000.) ;
#12409 = VECTOR('',#77735,1000.) ;
#12410 = VECTOR('',#77736,1000.) ;
#12411 = VECTOR('',#77739,1000.) ;
#12412 = VECTOR('',#77740,1000.) ;
#12413 = VECTOR('',#77741,1000.) ;
#12414 = VECTOR('',#77742,1000.) ;
#12415 = VECTOR('',#77745,1000.) ;
#12416 = VECTOR('',#77746,1000.) ;
#12417 = VECTOR('',#77747,1000.) ;
#12418 = VECTOR('',#77748,1000.) ;
#12419 = VECTOR('',#77751,1000.) ;
#12420 = VECTOR('',#77752,1000.) ;
#12421 = VECTOR('',#77753,1000.) ;
#12422 = VECTOR('',#77754,1000.) ;
#12423 = VECTOR('',#77757,1000.) ;
#12424 = VECTOR('',#77758,1000.) ;
#12425 = VECTOR('',#77759,1000.) ;
#12426 = VECTOR('',#77760,1000.) ;
#12427 = VECTOR('',#77763,1000.) ;
#12428 = VECTOR('',#77764,1000.) ;
#12429 = VECTOR('',#77765,1000.) ;
#12430 = VECTOR('',#77766,1000.) ;
#12431 = VECTOR('',#77769,1000.) ;
#12432 = VECTOR('',#77770,1000.) ;
#12433 = VECTOR('',#77771,1000.) ;
#12434 = VECTOR('',#77772,1000.) ;
#12435 = VECTOR('',#77775,1000.) ;
#12436 = VECTOR('',#77776,1000.) ;
#12437 = VECTOR('',#77777,1000.) ;
#12438 = VECTOR('',#77778,1000.) ;
#12439 = VECTOR('',#77781,1000.) ;
#12440 = VECTOR('',#77782,1000.) ;
#12441 = VECTOR('',#77783,1000.) ;
#12442 = VECTOR('',#77784,1000.) ;
#12443 = VECTOR('',#77787,1000.) ;
#12444 = VECTOR('',#77788,1000.) ;
#12445 = VECTOR('',#77789,1000.) ;
#12446 = VECTOR('',#77790,1000.) ;
#12447 = VECTOR('',#77793,1000.) ;
#12448 = VECTOR('',#77794,1000.) ;
#12449 = VECTOR('',#77795,1000.) ;
#12450 = VECTOR('',#77796,1000.) ;
#12451 = VECTOR('',#77799,1000.) ;
#12452 = VECTOR('',#77800,1000.) ;
#12453 = VECTOR('',#77801,1000.) ;
#12454 = VECTOR('',#77802,1000.) ;
#12455 = VECTOR('',#77805,1000.) ;
#12456 = VECTOR('',#77806,1000.) ;
#12457 = VECTOR('',#77807,1000.) ;
#12458 = VECTOR('',#77808,1000.) ;
#12459 = VECTOR('',#77811,1000.) ;
#12460 = VECTOR('',#77812,1000.) ;
#12461 = VECTOR('',#77813,1000.) ;
#12462 = VECTOR('',#77814,1000.) ;
#12463 = VECTOR('',#77817,1000.) ;
#12464 = VECTOR('',#77818,1000.) ;
#12465 = VECTOR('',#77819,1000.) ;
#12466 = VECTOR('',#77820,1000.) ;
#12467 = VECTOR('',#79373,1000.) ;
#12468 = VECTOR('',#79378,1000.) ;
#12469 = VECTOR('',#79383,1000.) ;
#12470 = VECTOR('',#79386,1000.) ;
#12471 = VECTOR('',#79399,1.5) ;
#12472 = VECTOR('',#79402,1000.) ;
#12473 = VECTOR('',#79409,1000.) ;
#12474 = VECTOR('',#79412,1000.) ;
#12475 = VECTOR('',#79413,1000.) ;
#12476 = VECTOR('',#79414,1000.) ;
#12477 = VECTOR('',#79417,1000.) ;
#12478 = VECTOR('',#79420,1000.) ;
#12479 = VECTOR('',#79421,1000.) ;
#12480 = VECTOR('',#79422,999.999999999999) ;
#12481 = VECTOR('',#79423,1000.) ;
#12482 = VECTOR('',#79426,1000.) ;
#12483 = VECTOR('',#79427,1000.) ;
#12484 = VECTOR('',#79428,1000.) ;
#12485 = VECTOR('',#79429,1000.) ;
#12486 = VECTOR('',#79432,1000.) ;
#12487 = VECTOR('',#79433,1000.) ;
#12488 = VECTOR('',#79434,1000.) ;
#12489 = VECTOR('',#79435,1000.) ;
#12490 = VECTOR('',#79438,1000.) ;
#12491 = VECTOR('',#79439,1000.) ;
#12492 = VECTOR('',#79440,1000.) ;
#12493 = VECTOR('',#79441,1000.) ;
#12494 = VECTOR('',#79444,1000.) ;
#12495 = VECTOR('',#79445,1000.) ;
#12496 = VECTOR('',#79446,1000.) ;
#12497 = VECTOR('',#79447,1000.) ;
#12498 = VECTOR('',#79450,1000.) ;
#12499 = VECTOR('',#79451,1000.) ;
#12500 = VECTOR('',#79452,1000.) ;
#12501 = VECTOR('',#79453,1000.) ;
#12502 = VECTOR('',#79456,1000.) ;
#12503 = VECTOR('',#79459,1000.) ;
#12504 = VECTOR('',#79468,1000.) ;
#12505 = VECTOR('',#79471,1000.) ;
#12506 = VECTOR('',#79474,1000.) ;
#12507 = VECTOR('',#79477,1000.) ;
#12508 = VECTOR('',#79480,1000.) ;
#12509 = VECTOR('',#79483,1000.) ;
#12510 = VECTOR('',#79488,1000.) ;
#12511 = VECTOR('',#79493,1000.) ;
#12512 = VECTOR('',#79494,1000.) ;
#12513 = VECTOR('',#79497,1000.) ;
#12514 = VECTOR('',#79500,1000.) ;
#12515 = VECTOR('',#79505,1000.) ;
#12516 = VECTOR('',#79508,1000.) ;
#12517 = VECTOR('',#79511,1000.) ;
#12518 = VECTOR('',#79514,1000.) ;
#12519 = VECTOR('',#79517,1000.) ;
#12520 = VECTOR('',#79518,1000.) ;
#12521 = VECTOR('',#79523,1000.) ;
#12522 = VECTOR('',#79528,1000.) ;
#12523 = VECTOR('',#79531,1000.) ;
#12524 = VECTOR('',#79534,1000.) ;
#12525 = VECTOR('',#79537,1000.) ;
#12526 = VECTOR('',#79540,1000.) ;
#12527 = VECTOR('',#79543,1000.) ;
#12528 = VECTOR('',#79546,1000.) ;
#12529 = VECTOR('',#79549,1000.) ;
#12530 = VECTOR('',#79554,1000.) ;
#12531 = VECTOR('',#79555,1000.) ;
#12532 = VECTOR('',#79558,1000.) ;
#12533 = VECTOR('',#79559,1000.) ;
#12534 = VECTOR('',#79562,1000.) ;
#12535 = VECTOR('',#79563,1000.) ;
#12536 = VECTOR('',#79564,1000.) ;
#12537 = VECTOR('',#79565,1000.) ;
#12538 = VECTOR('',#79570,1000.) ;
#12539 = VECTOR('',#79571,1000.) ;
#12540 = VECTOR('',#79572,999.999999999999) ;
#12541 = VECTOR('',#79575,1000.) ;
#12542 = VECTOR('',#79576,1000.) ;
#12543 = VECTOR('',#79577,1000.) ;
#12544 = VECTOR('',#79580,1000.) ;
#12545 = VECTOR('',#79581,1000.) ;
#12546 = VECTOR('',#79582,1000.) ;
#12547 = VECTOR('',#79585,1000.) ;
#12548 = VECTOR('',#79586,1000.) ;
#12549 = VECTOR('',#79587,1000.) ;
#12550 = VECTOR('',#79588,1000.) ;
#12551 = VECTOR('',#79589,1000.) ;
#12552 = VECTOR('',#79592,1000.) ;
#12553 = VECTOR('',#79595,1000.) ;
#12554 = VECTOR('',#79596,1000.) ;
#12555 = VECTOR('',#79601,1000.) ;
#12556 = VECTOR('',#79602,1000.) ;
#12557 = VECTOR('',#79609,1000.) ;
#12558 = VECTOR('',#79610,1000.) ;
#12559 = VECTOR('',#79611,1000.) ;
#12560 = VECTOR('',#79618,1000.) ;
#12561 = VECTOR('',#79619,1000.) ;
#12562 = VECTOR('',#79626,1000.) ;
#12563 = VECTOR('',#79629,1000.) ;
#12564 = VECTOR('',#79638,1000.) ;
#12565 = VECTOR('',#79639,1000.) ;
#12566 = VECTOR('',#79640,1000.) ;
#12567 = VECTOR('',#79641,1000.) ;
#12568 = VECTOR('',#79642,1000.) ;
#12569 = VECTOR('',#79645,1000.) ;
#12570 = VECTOR('',#79650,1000.) ;
#12571 = VECTOR('',#79651,1000.) ;
#12572 = VECTOR('',#79652,1000.) ;
#12573 = VECTOR('',#79655,1000.) ;
#12574 = VECTOR('',#79658,1000.) ;
#12575 = VECTOR('',#79659,1000.) ;
#12576 = VECTOR('',#79666,1000.) ;
#12577 = VECTOR('',#79667,1000.) ;
#12578 = VECTOR('',#79670,1000.) ;
#12579 = VECTOR('',#79671,1000.) ;
#12580 = VECTOR('',#79672,1000.) ;
#12581 = VECTOR('',#79673,1000.) ;
#12582 = VECTOR('',#79674,1000.) ;
#12583 = VECTOR('',#79675,1000.) ;
#12584 = VECTOR('',#79676,1000.) ;
#12585 = VECTOR('',#79677,1000.) ;
#12586 = VECTOR('',#79680,1000.) ;
#12587 = VECTOR('',#79681,1000.) ;
#12588 = VECTOR('',#79682,1000.) ;
#12589 = VECTOR('',#79683,1000.) ;
#12590 = VECTOR('',#79686,1000.) ;
#12591 = VECTOR('',#79687,1000.) ;
#12592 = VECTOR('',#79688,1000.) ;
#12593 = VECTOR('',#79689,1000.) ;
#12594 = VECTOR('',#79692,1000.) ;
#12595 = VECTOR('',#79693,1000.) ;
#12596 = VECTOR('',#79694,1000.) ;
#12597 = VECTOR('',#79695,1000.) ;
#12598 = VECTOR('',#79698,1000.) ;
#12599 = VECTOR('',#79699,1000.) ;
#12600 = VECTOR('',#79700,1000.) ;
#12601 = VECTOR('',#79701,1000.) ;
#12602 = VECTOR('',#79704,1000.) ;
#12603 = VECTOR('',#79705,1000.) ;
#12604 = VECTOR('',#79706,1000.) ;
#12605 = VECTOR('',#79707,1000.) ;
#12606 = VECTOR('',#79708,1000.) ;
#12607 = VECTOR('',#79709,1000.) ;
#12608 = VECTOR('',#79710,1000.) ;
#12609 = VECTOR('',#79711,1000.) ;
#12610 = VECTOR('',#79714,1000.) ;
#12611 = VECTOR('',#79717,1000.) ;
#12612 = VECTOR('',#79720,1000.) ;
#12613 = VECTOR('',#79723,1000.) ;
#12614 = VECTOR('',#79730,1000.) ;
#12615 = VECTOR('',#79731,1000.) ;
#12616 = VECTOR('',#79734,1000.) ;
#12617 = VECTOR('',#79739,1000.) ;
#12618 = VECTOR('',#79740,1000.) ;
#12619 = VECTOR('',#79741,1000.) ;
#12620 = VECTOR('',#79744,1000.) ;
#12621 = VECTOR('',#79745,1000.) ;
#12622 = VECTOR('',#79746,1000.) ;
#12623 = VECTOR('',#79751,1000.) ;
#12624 = VECTOR('',#79754,1000.) ;
#12625 = VECTOR('',#79759,1000.) ;
#12626 = VECTOR('',#79762,1000.) ;
#12627 = VECTOR('',#79765,1000.) ;
#12628 = VECTOR('',#79766,1000.) ;
#12629 = VECTOR('',#79767,1000.) ;
#12630 = VECTOR('',#79770,1000.) ;
#12631 = VECTOR('',#79771,1000.) ;
#12632 = VECTOR('',#79772,1000.) ;
#12633 = VECTOR('',#79777,1000.) ;
#12634 = VECTOR('',#79778,1000.) ;
#12635 = VECTOR('',#79783,1000.) ;
#12636 = VECTOR('',#79788,1000.) ;
#12637 = VECTOR('',#79789,1000.) ;
#12638 = VECTOR('',#79790,1000.) ;
#12639 = VECTOR('',#79793,1000.) ;
#12640 = VECTOR('',#79794,1000.) ;
#12641 = VECTOR('',#79795,1000.) ;
#12642 = VECTOR('',#79800,1000.) ;
#12643 = VECTOR('',#79803,1000.) ;
#12644 = VECTOR('',#79806,1000.) ;
#12645 = VECTOR('',#79807,1000.) ;
#12646 = VECTOR('',#79808,1000.) ;
#12647 = VECTOR('',#79809,1000.) ;
#12648 = VECTOR('',#79814,1000.) ;
#12649 = VECTOR('',#79817,1000.) ;
#12650 = VECTOR('',#79820,1000.) ;
#12651 = VECTOR('',#79821,1000.) ;
#12652 = VECTOR('',#79822,1000.) ;
#12653 = VECTOR('',#79825,1000.) ;
#12654 = VECTOR('',#79826,1000.) ;
#12655 = VECTOR('',#79827,1000.) ;
#12656 = VECTOR('',#79828,1000.) ;
#12657 = VECTOR('',#79831,1000.) ;
#12658 = VECTOR('',#79832,1000.) ;
#12659 = VECTOR('',#79833,1000.) ;
#12660 = VECTOR('',#79838,1000.) ;
#12661 = VECTOR('',#79839,1000.) ;
#12662 = VECTOR('',#79840,1000.) ;
#12663 = VECTOR('',#79841,1000.) ;
#12664 = VECTOR('',#79846,1000.) ;
#12665 = VECTOR('',#79847,1000.) ;
#12666 = VECTOR('',#79850,1000.) ;
#12667 = VECTOR('',#79853,1000.) ;
#12668 = VECTOR('',#79856,1000.) ;
#12669 = VECTOR('',#79857,1000.) ;
#12670 = VECTOR('',#79858,1000.) ;
#12671 = VECTOR('',#79859,1000.) ;
#12672 = VECTOR('',#79862,1000.) ;
#12673 = VECTOR('',#79863,1000.) ;
#12674 = VECTOR('',#79864,1000.) ;
#12675 = VECTOR('',#79865,1000.) ;
#12676 = VECTOR('',#79868,1000.) ;
#12677 = VECTOR('',#79869,1000.) ;
#12678 = VECTOR('',#79870,1000.) ;
#12679 = VECTOR('',#79871,1000.) ;
#12680 = VECTOR('',#79874,1000.) ;
#12681 = VECTOR('',#79875,1000.) ;
#12682 = VECTOR('',#79876,1000.) ;
#12683 = VECTOR('',#79877,1000.) ;
#12684 = VECTOR('',#79880,1000.) ;
#12685 = VECTOR('',#79881,1000.) ;
#12686 = VECTOR('',#79882,1000.) ;
#12687 = VECTOR('',#79885,1000.) ;
#12688 = VECTOR('',#79886,1000.) ;
#12689 = VECTOR('',#79887,1000.) ;
#12690 = VECTOR('',#79890,1000.) ;
#12691 = VECTOR('',#79891,1000.) ;
#12692 = VECTOR('',#79892,1000.) ;
#12693 = VECTOR('',#79895,1000.) ;
#12694 = VECTOR('',#79896,1000.) ;
#12695 = VECTOR('',#79897,1000.) ;
#12696 = VECTOR('',#79900,1000.) ;
#12697 = VECTOR('',#79901,1000.) ;
#12698 = VECTOR('',#79902,1000.) ;
#12699 = VECTOR('',#79905,1000.) ;
#12700 = VECTOR('',#79910,1000.) ;
#12701 = VECTOR('',#79911,1000.) ;
#12702 = VECTOR('',#79912,1000.) ;
#12703 = VECTOR('',#79915,1000.) ;
#12704 = VECTOR('',#79920,1000.) ;
#12705 = VECTOR('',#79927,1000.) ;
#12706 = VECTOR('',#79928,1000.) ;
#12707 = VECTOR('',#79929,1000.) ;
#12708 = VECTOR('',#79932,1000.) ;
#12709 = VECTOR('',#79933,1000.) ;
#12710 = VECTOR('',#79934,1000.) ;
#12711 = VECTOR('',#79935,1000.) ;
#12712 = VECTOR('',#79938,1000.) ;
#12713 = VECTOR('',#79939,1000.) ;
#12714 = VECTOR('',#79940,1000.) ;
#12715 = VECTOR('',#79941,1000.) ;
#12716 = VECTOR('',#79944,1000.) ;
#12717 = VECTOR('',#79945,1000.) ;
#12718 = VECTOR('',#79946,1000.) ;
#12719 = VECTOR('',#79947,1000.) ;
#12720 = VECTOR('',#79950,1000.) ;
#12721 = VECTOR('',#79951,1000.) ;
#12722 = VECTOR('',#79952,1000.) ;
#12723 = VECTOR('',#79953,1000.) ;
#12724 = VECTOR('',#79962,1000.) ;
#12725 = VECTOR('',#79963,1000.) ;
#12726 = VECTOR('',#79964,1000.) ;
#12727 = VECTOR('',#79965,1000.) ;
#12728 = VECTOR('',#79968,1000.) ;
#12729 = VECTOR('',#79969,1000.) ;
#12730 = VECTOR('',#79970,1000.) ;
#12731 = VECTOR('',#79971,1000.) ;
#12732 = VECTOR('',#79974,1000.) ;
#12733 = VECTOR('',#79975,1000.) ;
#12734 = VECTOR('',#79976,1000.) ;
#12735 = VECTOR('',#79977,1000.) ;
#12736 = VECTOR('',#79980,1000.) ;
#12737 = VECTOR('',#79981,1000.) ;
#12738 = VECTOR('',#79982,1000.) ;
#12739 = VECTOR('',#79983,1000.) ;
#12740 = VECTOR('',#79986,1000.) ;
#12741 = VECTOR('',#79989,1000.) ;
#12742 = VECTOR('',#80000,1000.) ;
#12743 = VECTOR('',#80003,1000.) ;
#12744 = VECTOR('',#80182,1000.) ;
#12745 = VECTOR('',#80207,1000.) ;
#12746 = VECTOR('',#80220,1000.) ;
#12747 = VECTOR('',#80255,1000.) ;
#12748 = VECTOR('',#80266,1000.) ;
#12749 = VECTOR('',#80289,1000.) ;
#12750 = VECTOR('',#80876,1000.) ;
#12751 = VECTOR('',#80881,1000.) ;
#12752 = VECTOR('',#80886,1000.) ;
#12753 = VECTOR('',#80889,1000.) ;
#12754 = VECTOR('',#80902,1.5) ;
#12755 = VECTOR('',#80905,1000.) ;
#12756 = VECTOR('',#80912,1000.) ;
#12757 = VECTOR('',#80915,1000.) ;
#12758 = VECTOR('',#80916,1000.) ;
#12759 = VECTOR('',#80917,1000.) ;
#12760 = VECTOR('',#80920,1000.) ;
#12761 = VECTOR('',#80923,1000.) ;
#12762 = VECTOR('',#80924,1000.) ;
#12763 = VECTOR('',#80925,1000.) ;
#12764 = VECTOR('',#80926,1000.) ;
#12765 = VECTOR('',#80929,1000.) ;
#12766 = VECTOR('',#80930,1000.) ;
#12767 = VECTOR('',#80931,1000.) ;
#12768 = VECTOR('',#80932,1000.) ;
#12769 = VECTOR('',#80935,1000.) ;
#12770 = VECTOR('',#80936,1000.) ;
#12771 = VECTOR('',#80937,1000.) ;
#12772 = VECTOR('',#80938,1000.) ;
#12773 = VECTOR('',#80941,1000.) ;
#12774 = VECTOR('',#80942,1000.) ;
#12775 = VECTOR('',#80943,1000.) ;
#12776 = VECTOR('',#80944,1000.) ;
#12777 = VECTOR('',#80947,1000.) ;
#12778 = VECTOR('',#80948,1000.) ;
#12779 = VECTOR('',#80949,1000.) ;
#12780 = VECTOR('',#80950,1000.) ;
#12781 = VECTOR('',#80953,1000.) ;
#12782 = VECTOR('',#80954,1000.) ;
#12783 = VECTOR('',#80955,1000.) ;
#12784 = VECTOR('',#80956,1000.) ;
#12785 = VECTOR('',#80959,1000.) ;
#12786 = VECTOR('',#80962,1000.) ;
#12787 = VECTOR('',#80971,1000.) ;
#12788 = VECTOR('',#80974,1000.) ;
#12789 = VECTOR('',#80977,1000.) ;
#12790 = VECTOR('',#80980,1000.) ;
#12791 = VECTOR('',#80983,1000.) ;
#12792 = VECTOR('',#80986,1000.) ;
#12793 = VECTOR('',#80991,1000.) ;
#12794 = VECTOR('',#80996,1000.) ;
#12795 = VECTOR('',#80997,1000.) ;
#12796 = VECTOR('',#81000,1000.) ;
#12797 = VECTOR('',#81003,1000.) ;
#12798 = VECTOR('',#81008,1000.) ;
#12799 = VECTOR('',#81011,1000.) ;
#12800 = VECTOR('',#81014,1000.) ;
#12801 = VECTOR('',#81017,1000.) ;
#12802 = VECTOR('',#81020,1000.) ;
#12803 = VECTOR('',#81021,1000.) ;
#12804 = VECTOR('',#81026,1000.) ;
#12805 = VECTOR('',#81031,1000.) ;
#12806 = VECTOR('',#81034,1000.) ;
#12807 = VECTOR('',#81037,1000.) ;
#12808 = VECTOR('',#81040,1000.) ;
#12809 = VECTOR('',#81043,1000.) ;
#12810 = VECTOR('',#81046,1000.) ;
#12811 = VECTOR('',#81049,1000.) ;
#12812 = VECTOR('',#81052,1000.) ;
#12813 = VECTOR('',#81057,1000.) ;
#12814 = VECTOR('',#81058,1000.) ;
#12815 = VECTOR('',#81061,1000.) ;
#12816 = VECTOR('',#81062,1000.) ;
#12817 = VECTOR('',#81065,1000.) ;
#12818 = VECTOR('',#81066,1000.) ;
#12819 = VECTOR('',#81067,1000.) ;
#12820 = VECTOR('',#81068,1000.) ;
#12821 = VECTOR('',#81073,1000.) ;
#12822 = VECTOR('',#81074,1000.) ;
#12823 = VECTOR('',#81075,1000.) ;
#12824 = VECTOR('',#81078,1000.) ;
#12825 = VECTOR('',#81079,1000.) ;
#12826 = VECTOR('',#81080,1000.) ;
#12827 = VECTOR('',#81083,1000.) ;
#12828 = VECTOR('',#81084,1000.) ;
#12829 = VECTOR('',#81085,1000.) ;
#12830 = VECTOR('',#81088,1000.) ;
#12831 = VECTOR('',#81089,1000.) ;
#12832 = VECTOR('',#81090,1000.) ;
#12833 = VECTOR('',#81091,1000.) ;
#12834 = VECTOR('',#81092,1000.) ;
#12835 = VECTOR('',#81095,1000.) ;
#12836 = VECTOR('',#81098,1000.) ;
#12837 = VECTOR('',#81099,1000.) ;
#12838 = VECTOR('',#81104,1000.) ;
#12839 = VECTOR('',#81105,1000.) ;
#12840 = VECTOR('',#81112,1000.) ;
#12841 = VECTOR('',#81113,1000.) ;
#12842 = VECTOR('',#81114,1000.) ;
#12843 = VECTOR('',#81121,1000.) ;
#12844 = VECTOR('',#81122,1000.) ;
#12845 = VECTOR('',#81129,1000.) ;
#12846 = VECTOR('',#81132,1000.) ;
#12847 = VECTOR('',#81141,1000.) ;
#12848 = VECTOR('',#81142,1000.) ;
#12849 = VECTOR('',#81143,1000.) ;
#12850 = VECTOR('',#81144,1000.) ;
#12851 = VECTOR('',#81145,1000.) ;
#12852 = VECTOR('',#81148,1000.) ;
#12853 = VECTOR('',#81153,1000.) ;
#12854 = VECTOR('',#81154,1000.) ;
#12855 = VECTOR('',#81155,1000.) ;
#12856 = VECTOR('',#81158,1000.) ;
#12857 = VECTOR('',#81161,1000.) ;
#12858 = VECTOR('',#81162,1000.) ;
#12859 = VECTOR('',#81169,1000.) ;
#12860 = VECTOR('',#81170,1000.) ;
#12861 = VECTOR('',#81173,1000.) ;
#12862 = VECTOR('',#81174,1000.) ;
#12863 = VECTOR('',#81175,1000.) ;
#12864 = VECTOR('',#81176,1000.) ;
#12865 = VECTOR('',#81177,1000.) ;
#12866 = VECTOR('',#81178,1000.) ;
#12867 = VECTOR('',#81179,1000.) ;
#12868 = VECTOR('',#81180,1000.) ;
#12869 = VECTOR('',#81183,1000.) ;
#12870 = VECTOR('',#81184,1000.) ;
#12871 = VECTOR('',#81185,1000.) ;
#12872 = VECTOR('',#81186,1000.) ;
#12873 = VECTOR('',#81189,1000.) ;
#12874 = VECTOR('',#81190,1000.) ;
#12875 = VECTOR('',#81191,1000.) ;
#12876 = VECTOR('',#81192,1000.) ;
#12877 = VECTOR('',#81195,1000.) ;
#12878 = VECTOR('',#81196,1000.) ;
#12879 = VECTOR('',#81197,1000.) ;
#12880 = VECTOR('',#81198,1000.) ;
#12881 = VECTOR('',#81201,1000.) ;
#12882 = VECTOR('',#81202,1000.) ;
#12883 = VECTOR('',#81203,1000.) ;
#12884 = VECTOR('',#81204,1000.) ;
#12885 = VECTOR('',#81207,1000.) ;
#12886 = VECTOR('',#81208,1000.) ;
#12887 = VECTOR('',#81209,1000.) ;
#12888 = VECTOR('',#81210,1000.) ;
#12889 = VECTOR('',#81211,1000.) ;
#12890 = VECTOR('',#81212,1000.) ;
#12891 = VECTOR('',#81213,1000.) ;
#12892 = VECTOR('',#81214,1000.) ;
#12893 = VECTOR('',#81217,1000.) ;
#12894 = VECTOR('',#81220,1000.) ;
#12895 = VECTOR('',#81223,1000.) ;
#12896 = VECTOR('',#81226,1000.) ;
#12897 = VECTOR('',#81233,1000.) ;
#12898 = VECTOR('',#81234,1000.) ;
#12899 = VECTOR('',#81237,1000.) ;
#12900 = VECTOR('',#81242,1000.) ;
#12901 = VECTOR('',#81243,1000.) ;
#12902 = VECTOR('',#81244,1000.) ;
#12903 = VECTOR('',#81247,1000.) ;
#12904 = VECTOR('',#81248,1000.) ;
#12905 = VECTOR('',#81249,1000.) ;
#12906 = VECTOR('',#81254,1000.) ;
#12907 = VECTOR('',#81257,1000.) ;
#12908 = VECTOR('',#81262,1000.) ;
#12909 = VECTOR('',#81265,1000.) ;
#12910 = VECTOR('',#81268,1000.) ;
#12911 = VECTOR('',#81269,1000.) ;
#12912 = VECTOR('',#81270,1000.) ;
#12913 = VECTOR('',#81273,1000.) ;
#12914 = VECTOR('',#81274,1000.) ;
#12915 = VECTOR('',#81275,1000.) ;
#12916 = VECTOR('',#81280,1000.) ;
#12917 = VECTOR('',#81281,1000.) ;
#12918 = VECTOR('',#81286,1000.) ;
#12919 = VECTOR('',#81291,1000.) ;
#12920 = VECTOR('',#81292,1000.) ;
#12921 = VECTOR('',#81293,1000.) ;
#12922 = VECTOR('',#81296,1000.) ;
#12923 = VECTOR('',#81297,1000.) ;
#12924 = VECTOR('',#81298,1000.) ;
#12925 = VECTOR('',#81303,1000.) ;
#12926 = VECTOR('',#81306,1000.) ;
#12927 = VECTOR('',#81309,1000.) ;
#12928 = VECTOR('',#81310,1000.) ;
#12929 = VECTOR('',#81311,1000.) ;
#12930 = VECTOR('',#81312,1000.) ;
#12931 = VECTOR('',#81317,1000.) ;
#12932 = VECTOR('',#81320,1000.) ;
#12933 = VECTOR('',#81323,1000.) ;
#12934 = VECTOR('',#81324,1000.) ;
#12935 = VECTOR('',#81325,1000.) ;
#12936 = VECTOR('',#81328,1000.) ;
#12937 = VECTOR('',#81329,1000.) ;
#12938 = VECTOR('',#81330,1000.) ;
#12939 = VECTOR('',#81331,1000.) ;
#12940 = VECTOR('',#81334,1000.) ;
#12941 = VECTOR('',#81335,1000.) ;
#12942 = VECTOR('',#81336,1000.) ;
#12943 = VECTOR('',#81341,1000.) ;
#12944 = VECTOR('',#81342,1000.) ;
#12945 = VECTOR('',#81343,1000.) ;
#12946 = VECTOR('',#81344,1000.) ;
#12947 = VECTOR('',#81349,1000.) ;
#12948 = VECTOR('',#81350,1000.) ;
#12949 = VECTOR('',#81353,1000.) ;
#12950 = VECTOR('',#81356,1000.) ;
#12951 = VECTOR('',#81359,1000.) ;
#12952 = VECTOR('',#81360,1000.) ;
#12953 = VECTOR('',#81361,1000.) ;
#12954 = VECTOR('',#81362,1000.) ;
#12955 = VECTOR('',#81365,1000.) ;
#12956 = VECTOR('',#81366,1000.) ;
#12957 = VECTOR('',#81367,1000.) ;
#12958 = VECTOR('',#81368,1000.) ;
#12959 = VECTOR('',#81371,1000.) ;
#12960 = VECTOR('',#81372,1000.) ;
#12961 = VECTOR('',#81373,1000.) ;
#12962 = VECTOR('',#81374,1000.) ;
#12963 = VECTOR('',#81377,1000.) ;
#12964 = VECTOR('',#81378,1000.) ;
#12965 = VECTOR('',#81379,1000.) ;
#12966 = VECTOR('',#81380,1000.) ;
#12967 = VECTOR('',#81383,1000.) ;
#12968 = VECTOR('',#81384,1000.) ;
#12969 = VECTOR('',#81385,1000.) ;
#12970 = VECTOR('',#81388,1000.) ;
#12971 = VECTOR('',#81389,1000.) ;
#12972 = VECTOR('',#81390,1000.) ;
#12973 = VECTOR('',#81393,1000.) ;
#12974 = VECTOR('',#81394,1000.) ;
#12975 = VECTOR('',#81395,1000.) ;
#12976 = VECTOR('',#81398,1000.) ;
#12977 = VECTOR('',#81399,1000.) ;
#12978 = VECTOR('',#81400,1000.) ;
#12979 = VECTOR('',#81403,1000.) ;
#12980 = VECTOR('',#81404,1000.) ;
#12981 = VECTOR('',#81405,1000.) ;
#12982 = VECTOR('',#81408,1000.) ;
#12983 = VECTOR('',#81413,1000.) ;
#12984 = VECTOR('',#81414,1000.) ;
#12985 = VECTOR('',#81415,1000.) ;
#12986 = VECTOR('',#81418,1000.) ;
#12987 = VECTOR('',#81423,1000.) ;
#12988 = VECTOR('',#81430,1000.) ;
#12989 = VECTOR('',#81431,1000.) ;
#12990 = VECTOR('',#81432,1000.) ;
#12991 = VECTOR('',#81435,1000.) ;
#12992 = VECTOR('',#81436,1000.) ;
#12993 = VECTOR('',#81437,1000.) ;
#12994 = VECTOR('',#81438,1000.) ;
#12995 = VECTOR('',#81441,1000.) ;
#12996 = VECTOR('',#81442,1000.) ;
#12997 = VECTOR('',#81443,1000.) ;
#12998 = VECTOR('',#81444,1000.) ;
#12999 = VECTOR('',#81447,1000.) ;
#13000 = VECTOR('',#81448,1000.) ;
#13001 = VECTOR('',#81449,1000.) ;
#13002 = VECTOR('',#81450,1000.) ;
#13003 = VECTOR('',#81453,1000.) ;
#13004 = VECTOR('',#81454,1000.) ;
#13005 = VECTOR('',#81455,1000.) ;
#13006 = VECTOR('',#81456,1000.) ;
#13007 = VECTOR('',#81465,1000.) ;
#13008 = VECTOR('',#81466,1000.) ;
#13009 = VECTOR('',#81467,1000.) ;
#13010 = VECTOR('',#81468,1000.) ;
#13011 = VECTOR('',#81471,1000.) ;
#13012 = VECTOR('',#81472,1000.) ;
#13013 = VECTOR('',#81473,1000.) ;
#13014 = VECTOR('',#81474,1000.) ;
#13015 = VECTOR('',#81477,1000.) ;
#13016 = VECTOR('',#81478,1000.) ;
#13017 = VECTOR('',#81479,1000.) ;
#13018 = VECTOR('',#81480,1000.) ;
#13019 = VECTOR('',#81483,1000.) ;
#13020 = VECTOR('',#81484,1000.) ;
#13021 = VECTOR('',#81485,1000.) ;
#13022 = VECTOR('',#81486,1000.) ;
#13023 = VECTOR('',#81489,1000.) ;
#13024 = VECTOR('',#81492,1000.) ;
#13025 = VECTOR('',#81503,1000.) ;
#13026 = VECTOR('',#81506,1000.) ;
#13027 = VECTOR('',#81685,1000.) ;
#13028 = VECTOR('',#81710,1000.) ;
#13029 = VECTOR('',#81723,1000.) ;
#13030 = VECTOR('',#81758,1000.) ;
#13031 = VECTOR('',#81769,1000.) ;
#13032 = VECTOR('',#81792,1000.) ;
#13033 = VECTOR('',#82379,1000.) ;
#13034 = VECTOR('',#82384,1000.) ;
#13035 = VECTOR('',#82389,1000.) ;
#13036 = VECTOR('',#82392,1000.) ;
#13037 = VECTOR('',#82405,1.5) ;
#13038 = VECTOR('',#82408,1000.) ;
#13039 = VECTOR('',#82415,1000.) ;
#13040 = VECTOR('',#82418,1000.) ;
#13041 = VECTOR('',#82419,1000.) ;
#13042 = VECTOR('',#82420,1000.) ;
#13043 = VECTOR('',#82423,1000.) ;
#13044 = VECTOR('',#82426,1000.) ;
#13045 = VECTOR('',#82427,1000.) ;
#13046 = VECTOR('',#82428,1000.) ;
#13047 = VECTOR('',#82429,1000.) ;
#13048 = VECTOR('',#82432,1000.) ;
#13049 = VECTOR('',#82433,1000.) ;
#13050 = VECTOR('',#82434,1000.) ;
#13051 = VECTOR('',#82435,1000.) ;
#13052 = VECTOR('',#82438,1000.) ;
#13053 = VECTOR('',#82439,1000.) ;
#13054 = VECTOR('',#82440,1000.) ;
#13055 = VECTOR('',#82441,1000.) ;
#13056 = VECTOR('',#82444,1000.) ;
#13057 = VECTOR('',#82445,1000.) ;
#13058 = VECTOR('',#82446,1000.) ;
#13059 = VECTOR('',#82447,1000.) ;
#13060 = VECTOR('',#82450,1000.) ;
#13061 = VECTOR('',#82451,1000.) ;
#13062 = VECTOR('',#82452,1000.) ;
#13063 = VECTOR('',#82453,1000.) ;
#13064 = VECTOR('',#82456,1000.) ;
#13065 = VECTOR('',#82457,1000.) ;
#13066 = VECTOR('',#82458,1000.) ;
#13067 = VECTOR('',#82459,1000.) ;
#13068 = VECTOR('',#82462,1000.) ;
#13069 = VECTOR('',#82465,1000.) ;
#13070 = VECTOR('',#82474,1000.) ;
#13071 = VECTOR('',#82477,1000.) ;
#13072 = VECTOR('',#82480,1000.) ;
#13073 = VECTOR('',#82483,1000.) ;
#13074 = VECTOR('',#82486,1000.) ;
#13075 = VECTOR('',#82489,1000.) ;
#13076 = VECTOR('',#82494,1000.) ;
#13077 = VECTOR('',#82499,1000.) ;
#13078 = VECTOR('',#82500,1000.) ;
#13079 = VECTOR('',#82503,1000.) ;
#13080 = VECTOR('',#82506,1000.) ;
#13081 = VECTOR('',#82511,1000.) ;
#13082 = VECTOR('',#82514,1000.) ;
#13083 = VECTOR('',#82517,1000.) ;
#13084 = VECTOR('',#82520,1000.) ;
#13085 = VECTOR('',#82523,1000.) ;
#13086 = VECTOR('',#82524,1000.) ;
#13087 = VECTOR('',#82529,1000.) ;
#13088 = VECTOR('',#82534,1000.) ;
#13089 = VECTOR('',#82537,1000.) ;
#13090 = VECTOR('',#82540,1000.) ;
#13091 = VECTOR('',#82543,1000.) ;
#13092 = VECTOR('',#82546,1000.) ;
#13093 = VECTOR('',#82549,1000.) ;
#13094 = VECTOR('',#82552,1000.) ;
#13095 = VECTOR('',#82555,1000.) ;
#13096 = VECTOR('',#82560,1000.) ;
#13097 = VECTOR('',#82561,1000.) ;
#13098 = VECTOR('',#82564,1000.) ;
#13099 = VECTOR('',#82565,1000.) ;
#13100 = VECTOR('',#82568,1000.) ;
#13101 = VECTOR('',#82569,1000.) ;
#13102 = VECTOR('',#82570,1000.) ;
#13103 = VECTOR('',#82571,1000.) ;
#13104 = VECTOR('',#82576,1000.) ;
#13105 = VECTOR('',#82577,1000.) ;
#13106 = VECTOR('',#82578,1000.) ;
#13107 = VECTOR('',#82581,1000.) ;
#13108 = VECTOR('',#82582,1000.) ;
#13109 = VECTOR('',#82583,1000.) ;
#13110 = VECTOR('',#82586,1000.) ;
#13111 = VECTOR('',#82587,1000.) ;
#13112 = VECTOR('',#82588,1000.) ;
#13113 = VECTOR('',#82591,1000.) ;
#13114 = VECTOR('',#82592,1000.) ;
#13115 = VECTOR('',#82593,1000.) ;
#13116 = VECTOR('',#82594,1000.) ;
#13117 = VECTOR('',#82595,1000.) ;
#13118 = VECTOR('',#82598,1000.) ;
#13119 = VECTOR('',#82601,1000.) ;
#13120 = VECTOR('',#82602,1000.) ;
#13121 = VECTOR('',#82607,1000.) ;
#13122 = VECTOR('',#82608,1000.) ;
#13123 = VECTOR('',#82615,1000.) ;
#13124 = VECTOR('',#82616,1000.) ;
#13125 = VECTOR('',#82617,1000.) ;
#13126 = VECTOR('',#82624,1000.) ;
#13127 = VECTOR('',#82625,1000.) ;
#13128 = VECTOR('',#82632,1000.) ;
#13129 = VECTOR('',#82635,1000.) ;
#13130 = VECTOR('',#82644,1000.) ;
#13131 = VECTOR('',#82645,1000.) ;
#13132 = VECTOR('',#82646,1000.) ;
#13133 = VECTOR('',#82647,1000.) ;
#13134 = VECTOR('',#82648,1000.) ;
#13135 = VECTOR('',#82651,1000.) ;
#13136 = VECTOR('',#82656,1000.) ;
#13137 = VECTOR('',#82657,1000.) ;
#13138 = VECTOR('',#82658,1000.) ;
#13139 = VECTOR('',#82661,1000.) ;
#13140 = VECTOR('',#82664,1000.) ;
#13141 = VECTOR('',#82665,1000.) ;
#13142 = VECTOR('',#82672,1000.) ;
#13143 = VECTOR('',#82673,1000.) ;
#13144 = VECTOR('',#82676,1000.) ;
#13145 = VECTOR('',#82677,1000.) ;
#13146 = VECTOR('',#82678,1000.) ;
#13147 = VECTOR('',#82679,1000.) ;
#13148 = VECTOR('',#82680,1000.) ;
#13149 = VECTOR('',#82681,1000.) ;
#13150 = VECTOR('',#82682,1000.) ;
#13151 = VECTOR('',#82683,1000.) ;
#13152 = VECTOR('',#82686,1000.) ;
#13153 = VECTOR('',#82687,1000.) ;
#13154 = VECTOR('',#82688,1000.) ;
#13155 = VECTOR('',#82689,1000.) ;
#13156 = VECTOR('',#82692,1000.) ;
#13157 = VECTOR('',#82693,1000.) ;
#13158 = VECTOR('',#82694,1000.) ;
#13159 = VECTOR('',#82695,1000.) ;
#13160 = VECTOR('',#82698,1000.) ;
#13161 = VECTOR('',#82699,1000.) ;
#13162 = VECTOR('',#82700,1000.) ;
#13163 = VECTOR('',#82701,1000.) ;
#13164 = VECTOR('',#82704,1000.) ;
#13165 = VECTOR('',#82705,1000.) ;
#13166 = VECTOR('',#82706,1000.) ;
#13167 = VECTOR('',#82707,1000.) ;
#13168 = VECTOR('',#82710,1000.) ;
#13169 = VECTOR('',#82711,1000.) ;
#13170 = VECTOR('',#82712,1000.) ;
#13171 = VECTOR('',#82713,1000.) ;
#13172 = VECTOR('',#82714,1000.) ;
#13173 = VECTOR('',#82715,1000.) ;
#13174 = VECTOR('',#82716,1000.) ;
#13175 = VECTOR('',#82717,1000.) ;
#13176 = VECTOR('',#82720,1000.) ;
#13177 = VECTOR('',#82723,1000.) ;
#13178 = VECTOR('',#82726,1000.) ;
#13179 = VECTOR('',#82729,1000.) ;
#13180 = VECTOR('',#82736,1000.) ;
#13181 = VECTOR('',#82737,1000.) ;
#13182 = VECTOR('',#82740,1000.) ;
#13183 = VECTOR('',#82745,1000.) ;
#13184 = VECTOR('',#82746,1000.) ;
#13185 = VECTOR('',#82747,1000.) ;
#13186 = VECTOR('',#82750,1000.) ;
#13187 = VECTOR('',#82751,1000.) ;
#13188 = VECTOR('',#82752,1000.) ;
#13189 = VECTOR('',#82757,1000.) ;
#13190 = VECTOR('',#82760,1000.) ;
#13191 = VECTOR('',#82765,1000.) ;
#13192 = VECTOR('',#82768,1000.) ;
#13193 = VECTOR('',#82771,1000.) ;
#13194 = VECTOR('',#82772,1000.) ;
#13195 = VECTOR('',#82773,1000.) ;
#13196 = VECTOR('',#82776,1000.) ;
#13197 = VECTOR('',#82777,1000.) ;
#13198 = VECTOR('',#82778,1000.) ;
#13199 = VECTOR('',#82783,1000.) ;
#13200 = VECTOR('',#82784,1000.) ;
#13201 = VECTOR('',#82789,1000.) ;
#13202 = VECTOR('',#82794,1000.) ;
#13203 = VECTOR('',#82795,1000.) ;
#13204 = VECTOR('',#82796,1000.) ;
#13205 = VECTOR('',#82799,1000.) ;
#13206 = VECTOR('',#82800,1000.) ;
#13207 = VECTOR('',#82801,1000.) ;
#13208 = VECTOR('',#82806,1000.) ;
#13209 = VECTOR('',#82809,1000.) ;
#13210 = VECTOR('',#82812,1000.) ;
#13211 = VECTOR('',#82813,1000.) ;
#13212 = VECTOR('',#82814,1000.) ;
#13213 = VECTOR('',#82815,1000.) ;
#13214 = VECTOR('',#82820,1000.) ;
#13215 = VECTOR('',#82823,1000.) ;
#13216 = VECTOR('',#82826,1000.) ;
#13217 = VECTOR('',#82827,1000.) ;
#13218 = VECTOR('',#82828,1000.) ;
#13219 = VECTOR('',#82831,1000.) ;
#13220 = VECTOR('',#82832,1000.) ;
#13221 = VECTOR('',#82833,1000.) ;
#13222 = VECTOR('',#82834,1000.) ;
#13223 = VECTOR('',#82837,1000.) ;
#13224 = VECTOR('',#82838,1000.) ;
#13225 = VECTOR('',#82839,1000.) ;
#13226 = VECTOR('',#82844,1000.) ;
#13227 = VECTOR('',#82845,1000.) ;
#13228 = VECTOR('',#82846,1000.) ;
#13229 = VECTOR('',#82847,1000.) ;
#13230 = VECTOR('',#82852,1000.) ;
#13231 = VECTOR('',#82853,1000.) ;
#13232 = VECTOR('',#82856,1000.) ;
#13233 = VECTOR('',#82859,1000.) ;
#13234 = VECTOR('',#82862,1000.) ;
#13235 = VECTOR('',#82863,1000.) ;
#13236 = VECTOR('',#82864,1000.) ;
#13237 = VECTOR('',#82865,1000.) ;
#13238 = VECTOR('',#82868,1000.) ;
#13239 = VECTOR('',#82869,1000.) ;
#13240 = VECTOR('',#82870,1000.) ;
#13241 = VECTOR('',#82871,1000.) ;
#13242 = VECTOR('',#82874,1000.) ;
#13243 = VECTOR('',#82875,1000.) ;
#13244 = VECTOR('',#82876,1000.) ;
#13245 = VECTOR('',#82877,1000.) ;
#13246 = VECTOR('',#82880,1000.) ;
#13247 = VECTOR('',#82881,1000.) ;
#13248 = VECTOR('',#82882,1000.) ;
#13249 = VECTOR('',#82883,1000.) ;
#13250 = VECTOR('',#82886,1000.) ;
#13251 = VECTOR('',#82887,1000.) ;
#13252 = VECTOR('',#82888,1000.) ;
#13253 = VECTOR('',#82891,1000.) ;
#13254 = VECTOR('',#82892,1000.) ;
#13255 = VECTOR('',#82893,1000.) ;
#13256 = VECTOR('',#82896,1000.) ;
#13257 = VECTOR('',#82897,1000.) ;
#13258 = VECTOR('',#82898,1000.) ;
#13259 = VECTOR('',#82901,1000.) ;
#13260 = VECTOR('',#82902,1000.) ;
#13261 = VECTOR('',#82903,1000.) ;
#13262 = VECTOR('',#82906,1000.) ;
#13263 = VECTOR('',#82907,1000.) ;
#13264 = VECTOR('',#82908,1000.) ;
#13265 = VECTOR('',#82911,1000.) ;
#13266 = VECTOR('',#82916,1000.) ;
#13267 = VECTOR('',#82917,1000.) ;
#13268 = VECTOR('',#82918,1000.) ;
#13269 = VECTOR('',#82921,1000.) ;
#13270 = VECTOR('',#82926,1000.) ;
#13271 = VECTOR('',#82933,1000.) ;
#13272 = VECTOR('',#82934,1000.) ;
#13273 = VECTOR('',#82935,1000.) ;
#13274 = VECTOR('',#82938,1000.) ;
#13275 = VECTOR('',#82939,1000.) ;
#13276 = VECTOR('',#82940,1000.) ;
#13277 = VECTOR('',#82941,1000.) ;
#13278 = VECTOR('',#82944,1000.) ;
#13279 = VECTOR('',#82945,1000.) ;
#13280 = VECTOR('',#82946,1000.) ;
#13281 = VECTOR('',#82947,1000.) ;
#13282 = VECTOR('',#82950,1000.) ;
#13283 = VECTOR('',#82951,1000.) ;
#13284 = VECTOR('',#82952,1000.) ;
#13285 = VECTOR('',#82953,1000.) ;
#13286 = VECTOR('',#82956,1000.) ;
#13287 = VECTOR('',#82957,1000.) ;
#13288 = VECTOR('',#82958,1000.) ;
#13289 = VECTOR('',#82959,1000.) ;
#13290 = VECTOR('',#82968,1000.) ;
#13291 = VECTOR('',#82969,1000.) ;
#13292 = VECTOR('',#82970,1000.) ;
#13293 = VECTOR('',#82971,1000.) ;
#13294 = VECTOR('',#82974,1000.) ;
#13295 = VECTOR('',#82975,1000.) ;
#13296 = VECTOR('',#82976,1000.) ;
#13297 = VECTOR('',#82977,1000.) ;
#13298 = VECTOR('',#82980,1000.) ;
#13299 = VECTOR('',#82981,1000.) ;
#13300 = VECTOR('',#82982,1000.) ;
#13301 = VECTOR('',#82983,1000.) ;
#13302 = VECTOR('',#82986,1000.) ;
#13303 = VECTOR('',#82987,1000.) ;
#13304 = VECTOR('',#82988,1000.) ;
#13305 = VECTOR('',#82989,1000.) ;
#13306 = VECTOR('',#82992,1000.) ;
#13307 = VECTOR('',#82995,1000.) ;
#13308 = VECTOR('',#83006,1000.) ;
#13309 = VECTOR('',#83009,1000.) ;
#13310 = VECTOR('',#83188,1000.) ;
#13311 = VECTOR('',#83213,1000.) ;
#13312 = VECTOR('',#83226,1000.) ;
#13313 = VECTOR('',#83261,1000.) ;
#13314 = VECTOR('',#83272,1000.) ;
#13315 = VECTOR('',#83295,1000.) ;
#13316 = VECTOR('',#83882,1000.) ;
#13317 = VECTOR('',#83887,1000.) ;
#13318 = VECTOR('',#83892,1000.) ;
#13319 = VECTOR('',#83895,1000.) ;
#13320 = VECTOR('',#83908,1.5) ;
#13321 = VECTOR('',#83911,1000.) ;
#13322 = VECTOR('',#83918,1000.) ;
#13323 = VECTOR('',#83921,1000.) ;
#13324 = VECTOR('',#83922,1000.) ;
#13325 = VECTOR('',#83923,1000.) ;
#13326 = VECTOR('',#83926,1000.) ;
#13327 = VECTOR('',#83929,1000.) ;
#13328 = VECTOR('',#83930,1000.) ;
#13329 = VECTOR('',#83931,999.999999999999) ;
#13330 = VECTOR('',#83932,1000.) ;
#13331 = VECTOR('',#83935,1000.) ;
#13332 = VECTOR('',#83936,1000.) ;
#13333 = VECTOR('',#83937,1000.) ;
#13334 = VECTOR('',#83938,1000.) ;
#13335 = VECTOR('',#83941,1000.) ;
#13336 = VECTOR('',#83942,1000.) ;
#13337 = VECTOR('',#83943,1000.) ;
#13338 = VECTOR('',#83944,1000.) ;
#13339 = VECTOR('',#83947,1000.) ;
#13340 = VECTOR('',#83948,1000.) ;
#13341 = VECTOR('',#83949,1000.) ;
#13342 = VECTOR('',#83950,1000.) ;
#13343 = VECTOR('',#83953,1000.) ;
#13344 = VECTOR('',#83954,1000.) ;
#13345 = VECTOR('',#83955,1000.) ;
#13346 = VECTOR('',#83956,1000.) ;
#13347 = VECTOR('',#83959,1000.) ;
#13348 = VECTOR('',#83960,1000.) ;
#13349 = VECTOR('',#83961,1000.) ;
#13350 = VECTOR('',#83962,1000.) ;
#13351 = VECTOR('',#83965,1000.) ;
#13352 = VECTOR('',#83968,1000.) ;
#13353 = VECTOR('',#83977,1000.) ;
#13354 = VECTOR('',#83980,1000.) ;
#13355 = VECTOR('',#83983,1000.) ;
#13356 = VECTOR('',#83986,1000.) ;
#13357 = VECTOR('',#83989,1000.) ;
#13358 = VECTOR('',#83992,1000.) ;
#13359 = VECTOR('',#83997,1000.) ;
#13360 = VECTOR('',#84002,1000.) ;
#13361 = VECTOR('',#84003,1000.) ;
#13362 = VECTOR('',#84006,1000.) ;
#13363 = VECTOR('',#84009,1000.) ;
#13364 = VECTOR('',#84014,1000.) ;
#13365 = VECTOR('',#84017,1000.) ;
#13366 = VECTOR('',#84020,1000.) ;
#13367 = VECTOR('',#84023,1000.) ;
#13368 = VECTOR('',#84026,1000.) ;
#13369 = VECTOR('',#84027,1000.) ;
#13370 = VECTOR('',#84032,1000.) ;
#13371 = VECTOR('',#84037,1000.) ;
#13372 = VECTOR('',#84040,1000.) ;
#13373 = VECTOR('',#84043,1000.) ;
#13374 = VECTOR('',#84046,1000.) ;
#13375 = VECTOR('',#84049,1000.) ;
#13376 = VECTOR('',#84052,1000.) ;
#13377 = VECTOR('',#84055,1000.) ;
#13378 = VECTOR('',#84058,1000.) ;
#13379 = VECTOR('',#84063,1000.) ;
#13380 = VECTOR('',#84064,1000.) ;
#13381 = VECTOR('',#84067,1000.) ;
#13382 = VECTOR('',#84068,1000.) ;
#13383 = VECTOR('',#84071,1000.) ;
#13384 = VECTOR('',#84072,1000.) ;
#13385 = VECTOR('',#84073,1000.) ;
#13386 = VECTOR('',#84074,1000.) ;
#13387 = VECTOR('',#84079,1000.) ;
#13388 = VECTOR('',#84080,1000.) ;
#13389 = VECTOR('',#84081,999.999999999999) ;
#13390 = VECTOR('',#84084,1000.) ;
#13391 = VECTOR('',#84085,1000.) ;
#13392 = VECTOR('',#84086,1000.) ;
#13393 = VECTOR('',#84089,1000.) ;
#13394 = VECTOR('',#84090,1000.) ;
#13395 = VECTOR('',#84091,1000.) ;
#13396 = VECTOR('',#84094,1000.) ;
#13397 = VECTOR('',#84095,1000.) ;
#13398 = VECTOR('',#84096,1000.) ;
#13399 = VECTOR('',#84097,1000.) ;
#13400 = VECTOR('',#84098,1000.) ;
#13401 = VECTOR('',#84101,1000.) ;
#13402 = VECTOR('',#84104,1000.) ;
#13403 = VECTOR('',#84105,1000.) ;
#13404 = VECTOR('',#84110,1000.) ;
#13405 = VECTOR('',#84111,1000.) ;
#13406 = VECTOR('',#84118,1000.) ;
#13407 = VECTOR('',#84119,1000.) ;
#13408 = VECTOR('',#84120,1000.) ;
#13409 = VECTOR('',#84127,1000.) ;
#13410 = VECTOR('',#84128,1000.) ;
#13411 = VECTOR('',#84135,1000.) ;
#13412 = VECTOR('',#84138,1000.) ;
#13413 = VECTOR('',#84147,1000.) ;
#13414 = VECTOR('',#84148,1000.) ;
#13415 = VECTOR('',#84149,1000.) ;
#13416 = VECTOR('',#84150,1000.) ;
#13417 = VECTOR('',#84151,1000.) ;
#13418 = VECTOR('',#84154,1000.) ;
#13419 = VECTOR('',#84159,1000.) ;
#13420 = VECTOR('',#84160,1000.) ;
#13421 = VECTOR('',#84161,1000.) ;
#13422 = VECTOR('',#84164,1000.) ;
#13423 = VECTOR('',#84167,1000.) ;
#13424 = VECTOR('',#84168,1000.) ;
#13425 = VECTOR('',#84175,1000.) ;
#13426 = VECTOR('',#84176,1000.) ;
#13427 = VECTOR('',#84179,1000.) ;
#13428 = VECTOR('',#84180,1000.) ;
#13429 = VECTOR('',#84181,1000.) ;
#13430 = VECTOR('',#84182,1000.) ;
#13431 = VECTOR('',#84183,1000.) ;
#13432 = VECTOR('',#84184,1000.) ;
#13433 = VECTOR('',#84185,1000.) ;
#13434 = VECTOR('',#84186,1000.) ;
#13435 = VECTOR('',#84189,1000.) ;
#13436 = VECTOR('',#84190,1000.) ;
#13437 = VECTOR('',#84191,1000.) ;
#13438 = VECTOR('',#84192,1000.) ;
#13439 = VECTOR('',#84195,1000.) ;
#13440 = VECTOR('',#84196,1000.) ;
#13441 = VECTOR('',#84197,1000.) ;
#13442 = VECTOR('',#84198,1000.) ;
#13443 = VECTOR('',#84201,1000.) ;
#13444 = VECTOR('',#84202,1000.) ;
#13445 = VECTOR('',#84203,1000.) ;
#13446 = VECTOR('',#84204,1000.) ;
#13447 = VECTOR('',#84207,1000.) ;
#13448 = VECTOR('',#84208,1000.) ;
#13449 = VECTOR('',#84209,1000.) ;
#13450 = VECTOR('',#84210,1000.) ;
#13451 = VECTOR('',#84213,1000.) ;
#13452 = VECTOR('',#84214,1000.) ;
#13453 = VECTOR('',#84215,1000.) ;
#13454 = VECTOR('',#84216,1000.) ;
#13455 = VECTOR('',#84217,1000.) ;
#13456 = VECTOR('',#84218,1000.) ;
#13457 = VECTOR('',#84219,1000.) ;
#13458 = VECTOR('',#84220,1000.) ;
#13459 = VECTOR('',#84223,1000.) ;
#13460 = VECTOR('',#84226,1000.) ;
#13461 = VECTOR('',#84229,1000.) ;
#13462 = VECTOR('',#84232,1000.) ;
#13463 = VECTOR('',#84239,1000.) ;
#13464 = VECTOR('',#84240,1000.) ;
#13465 = VECTOR('',#84243,1000.) ;
#13466 = VECTOR('',#84248,1000.) ;
#13467 = VECTOR('',#84249,1000.) ;
#13468 = VECTOR('',#84250,1000.) ;
#13469 = VECTOR('',#84253,1000.) ;
#13470 = VECTOR('',#84254,1000.) ;
#13471 = VECTOR('',#84255,1000.) ;
#13472 = VECTOR('',#84260,1000.) ;
#13473 = VECTOR('',#84263,1000.) ;
#13474 = VECTOR('',#84268,1000.) ;
#13475 = VECTOR('',#84271,1000.) ;
#13476 = VECTOR('',#84274,1000.) ;
#13477 = VECTOR('',#84275,1000.) ;
#13478 = VECTOR('',#84276,1000.) ;
#13479 = VECTOR('',#84279,1000.) ;
#13480 = VECTOR('',#84280,1000.) ;
#13481 = VECTOR('',#84281,1000.) ;
#13482 = VECTOR('',#84286,1000.) ;
#13483 = VECTOR('',#84287,1000.) ;
#13484 = VECTOR('',#84292,1000.) ;
#13485 = VECTOR('',#84297,1000.) ;
#13486 = VECTOR('',#84298,1000.) ;
#13487 = VECTOR('',#84299,1000.) ;
#13488 = VECTOR('',#84302,1000.) ;
#13489 = VECTOR('',#84303,1000.) ;
#13490 = VECTOR('',#84304,1000.) ;
#13491 = VECTOR('',#84309,1000.) ;
#13492 = VECTOR('',#84312,1000.) ;
#13493 = VECTOR('',#84315,1000.) ;
#13494 = VECTOR('',#84316,1000.) ;
#13495 = VECTOR('',#84317,1000.) ;
#13496 = VECTOR('',#84318,1000.) ;
#13497 = VECTOR('',#84323,1000.) ;
#13498 = VECTOR('',#84326,1000.) ;
#13499 = VECTOR('',#84329,1000.) ;
#13500 = VECTOR('',#84330,1000.) ;
#13501 = VECTOR('',#84331,1000.) ;
#13502 = VECTOR('',#84334,1000.) ;
#13503 = VECTOR('',#84335,1000.) ;
#13504 = VECTOR('',#84336,1000.) ;
#13505 = VECTOR('',#84337,1000.) ;
#13506 = VECTOR('',#84340,1000.) ;
#13507 = VECTOR('',#84341,1000.) ;
#13508 = VECTOR('',#84342,1000.) ;
#13509 = VECTOR('',#84347,1000.) ;
#13510 = VECTOR('',#84348,1000.) ;
#13511 = VECTOR('',#84349,1000.) ;
#13512 = VECTOR('',#84350,1000.) ;
#13513 = VECTOR('',#84355,1000.) ;
#13514 = VECTOR('',#84356,1000.) ;
#13515 = VECTOR('',#84359,1000.) ;
#13516 = VECTOR('',#84362,1000.) ;
#13517 = VECTOR('',#84365,1000.) ;
#13518 = VECTOR('',#84366,1000.) ;
#13519 = VECTOR('',#84367,1000.) ;
#13520 = VECTOR('',#84368,1000.) ;
#13521 = VECTOR('',#84371,1000.) ;
#13522 = VECTOR('',#84372,1000.) ;
#13523 = VECTOR('',#84373,1000.) ;
#13524 = VECTOR('',#84374,1000.) ;
#13525 = VECTOR('',#84377,1000.) ;
#13526 = VECTOR('',#84378,1000.) ;
#13527 = VECTOR('',#84379,1000.) ;
#13528 = VECTOR('',#84380,1000.) ;
#13529 = VECTOR('',#84383,1000.) ;
#13530 = VECTOR('',#84384,1000.) ;
#13531 = VECTOR('',#84385,1000.) ;
#13532 = VECTOR('',#84386,1000.) ;
#13533 = VECTOR('',#84389,1000.) ;
#13534 = VECTOR('',#84390,1000.) ;
#13535 = VECTOR('',#84391,1000.) ;
#13536 = VECTOR('',#84394,1000.) ;
#13537 = VECTOR('',#84395,1000.) ;
#13538 = VECTOR('',#84396,1000.) ;
#13539 = VECTOR('',#84399,1000.) ;
#13540 = VECTOR('',#84400,1000.) ;
#13541 = VECTOR('',#84401,1000.) ;
#13542 = VECTOR('',#84404,1000.) ;
#13543 = VECTOR('',#84405,1000.) ;
#13544 = VECTOR('',#84406,1000.) ;
#13545 = VECTOR('',#84409,1000.) ;
#13546 = VECTOR('',#84410,1000.) ;
#13547 = VECTOR('',#84411,1000.) ;
#13548 = VECTOR('',#84414,1000.) ;
#13549 = VECTOR('',#84419,1000.) ;
#13550 = VECTOR('',#84420,1000.) ;
#13551 = VECTOR('',#84421,1000.) ;
#13552 = VECTOR('',#84424,1000.) ;
#13553 = VECTOR('',#84429,1000.) ;
#13554 = VECTOR('',#84436,1000.) ;
#13555 = VECTOR('',#84437,1000.) ;
#13556 = VECTOR('',#84438,1000.) ;
#13557 = VECTOR('',#84441,1000.) ;
#13558 = VECTOR('',#84442,1000.) ;
#13559 = VECTOR('',#84443,1000.) ;
#13560 = VECTOR('',#84444,1000.) ;
#13561 = VECTOR('',#84447,1000.) ;
#13562 = VECTOR('',#84448,1000.) ;
#13563 = VECTOR('',#84449,1000.) ;
#13564 = VECTOR('',#84450,1000.) ;
#13565 = VECTOR('',#84453,1000.) ;
#13566 = VECTOR('',#84454,1000.) ;
#13567 = VECTOR('',#84455,1000.) ;
#13568 = VECTOR('',#84456,1000.) ;
#13569 = VECTOR('',#84459,1000.) ;
#13570 = VECTOR('',#84460,1000.) ;
#13571 = VECTOR('',#84461,1000.) ;
#13572 = VECTOR('',#84462,1000.) ;
#13573 = VECTOR('',#84471,1000.) ;
#13574 = VECTOR('',#84472,1000.) ;
#13575 = VECTOR('',#84473,1000.) ;
#13576 = VECTOR('',#84474,1000.) ;
#13577 = VECTOR('',#84477,1000.) ;
#13578 = VECTOR('',#84478,1000.) ;
#13579 = VECTOR('',#84479,1000.) ;
#13580 = VECTOR('',#84480,1000.) ;
#13581 = VECTOR('',#84483,1000.) ;
#13582 = VECTOR('',#84484,1000.) ;
#13583 = VECTOR('',#84485,1000.) ;
#13584 = VECTOR('',#84486,1000.) ;
#13585 = VECTOR('',#84489,1000.) ;
#13586 = VECTOR('',#84490,1000.) ;
#13587 = VECTOR('',#84491,1000.) ;
#13588 = VECTOR('',#84492,1000.) ;
#13589 = VECTOR('',#84495,1000.) ;
#13590 = VECTOR('',#84498,1000.) ;
#13591 = VECTOR('',#84509,1000.) ;
#13592 = VECTOR('',#84512,1000.) ;
#13593 = VECTOR('',#84691,1000.) ;
#13594 = VECTOR('',#84716,1000.) ;
#13595 = VECTOR('',#84729,1000.) ;
#13596 = VECTOR('',#84764,1000.) ;
#13597 = VECTOR('',#84775,1000.) ;
#13598 = VECTOR('',#84798,1000.) ;
#13599 = VECTOR('',#85385,1000.) ;
#13600 = VECTOR('',#85390,1000.) ;
#13601 = VECTOR('',#85395,1000.) ;
#13602 = VECTOR('',#85398,1000.) ;
#13603 = VECTOR('',#85411,1.5) ;
#13604 = VECTOR('',#85414,1000.) ;
#13605 = VECTOR('',#85421,1000.) ;
#13606 = VECTOR('',#85424,1000.) ;
#13607 = VECTOR('',#85425,1000.) ;
#13608 = VECTOR('',#85426,1000.) ;
#13609 = VECTOR('',#85429,1000.) ;
#13610 = VECTOR('',#85432,1000.) ;
#13611 = VECTOR('',#85433,1000.) ;
#13612 = VECTOR('',#85434,1000.) ;
#13613 = VECTOR('',#85435,1000.) ;
#13614 = VECTOR('',#85438,1000.) ;
#13615 = VECTOR('',#85439,1000.) ;
#13616 = VECTOR('',#85440,1000.) ;
#13617 = VECTOR('',#85441,1000.) ;
#13618 = VECTOR('',#85444,1000.) ;
#13619 = VECTOR('',#85445,1000.) ;
#13620 = VECTOR('',#85446,1000.) ;
#13621 = VECTOR('',#85447,1000.) ;
#13622 = VECTOR('',#85450,1000.) ;
#13623 = VECTOR('',#85451,1000.) ;
#13624 = VECTOR('',#85452,1000.) ;
#13625 = VECTOR('',#85453,1000.) ;
#13626 = VECTOR('',#85456,1000.) ;
#13627 = VECTOR('',#85457,1000.) ;
#13628 = VECTOR('',#85458,1000.) ;
#13629 = VECTOR('',#85459,1000.) ;
#13630 = VECTOR('',#85462,1000.) ;
#13631 = VECTOR('',#85463,1000.) ;
#13632 = VECTOR('',#85464,1000.) ;
#13633 = VECTOR('',#85465,1000.) ;
#13634 = VECTOR('',#85468,1000.) ;
#13635 = VECTOR('',#85471,1000.) ;
#13636 = VECTOR('',#85480,1000.) ;
#13637 = VECTOR('',#85483,1000.) ;
#13638 = VECTOR('',#85486,1000.) ;
#13639 = VECTOR('',#85489,1000.) ;
#13640 = VECTOR('',#85492,1000.) ;
#13641 = VECTOR('',#85495,1000.) ;
#13642 = VECTOR('',#85500,1000.) ;
#13643 = VECTOR('',#85505,1000.) ;
#13644 = VECTOR('',#85506,1000.) ;
#13645 = VECTOR('',#85509,1000.) ;
#13646 = VECTOR('',#85512,1000.) ;
#13647 = VECTOR('',#85517,1000.) ;
#13648 = VECTOR('',#85520,1000.) ;
#13649 = VECTOR('',#85523,1000.) ;
#13650 = VECTOR('',#85526,1000.) ;
#13651 = VECTOR('',#85529,1000.) ;
#13652 = VECTOR('',#85530,1000.) ;
#13653 = VECTOR('',#85535,1000.) ;
#13654 = VECTOR('',#85540,1000.) ;
#13655 = VECTOR('',#85543,1000.) ;
#13656 = VECTOR('',#85546,1000.) ;
#13657 = VECTOR('',#85549,1000.) ;
#13658 = VECTOR('',#85552,1000.) ;
#13659 = VECTOR('',#85555,1000.) ;
#13660 = VECTOR('',#85558,1000.) ;
#13661 = VECTOR('',#85561,1000.) ;
#13662 = VECTOR('',#85566,1000.) ;
#13663 = VECTOR('',#85567,1000.) ;
#13664 = VECTOR('',#85570,1000.) ;
#13665 = VECTOR('',#85571,1000.) ;
#13666 = VECTOR('',#85574,1000.) ;
#13667 = VECTOR('',#85575,1000.) ;
#13668 = VECTOR('',#85576,1000.) ;
#13669 = VECTOR('',#85577,1000.) ;
#13670 = VECTOR('',#85582,1000.) ;
#13671 = VECTOR('',#85583,1000.) ;
#13672 = VECTOR('',#85584,999.999999999999) ;
#13673 = VECTOR('',#85587,1000.) ;
#13674 = VECTOR('',#85588,1000.) ;
#13675 = VECTOR('',#85589,1000.) ;
#13676 = VECTOR('',#85592,1000.) ;
#13677 = VECTOR('',#85593,1000.) ;
#13678 = VECTOR('',#85594,1000.) ;
#13679 = VECTOR('',#85597,1000.) ;
#13680 = VECTOR('',#85598,1000.) ;
#13681 = VECTOR('',#85599,1000.) ;
#13682 = VECTOR('',#85600,1000.) ;
#13683 = VECTOR('',#85601,1000.) ;
#13684 = VECTOR('',#85604,1000.) ;
#13685 = VECTOR('',#85607,1000.) ;
#13686 = VECTOR('',#85608,1000.) ;
#13687 = VECTOR('',#85613,1000.) ;
#13688 = VECTOR('',#85614,1000.) ;
#13689 = VECTOR('',#85621,1000.) ;
#13690 = VECTOR('',#85622,1000.) ;
#13691 = VECTOR('',#85623,1000.) ;
#13692 = VECTOR('',#85630,1000.) ;
#13693 = VECTOR('',#85631,1000.) ;
#13694 = VECTOR('',#85638,1000.) ;
#13695 = VECTOR('',#85641,1000.) ;
#13696 = VECTOR('',#85650,1000.) ;
#13697 = VECTOR('',#85651,1000.) ;
#13698 = VECTOR('',#85652,1000.) ;
#13699 = VECTOR('',#85653,1000.) ;
#13700 = VECTOR('',#85654,1000.) ;
#13701 = VECTOR('',#85657,1000.) ;
#13702 = VECTOR('',#85662,1000.) ;
#13703 = VECTOR('',#85663,1000.) ;
#13704 = VECTOR('',#85664,1000.) ;
#13705 = VECTOR('',#85667,1000.) ;
#13706 = VECTOR('',#85670,1000.) ;
#13707 = VECTOR('',#85671,1000.) ;
#13708 = VECTOR('',#85678,1000.) ;
#13709 = VECTOR('',#85679,1000.) ;
#13710 = VECTOR('',#85682,1000.) ;
#13711 = VECTOR('',#85683,1000.) ;
#13712 = VECTOR('',#85684,1000.) ;
#13713 = VECTOR('',#85685,1000.) ;
#13714 = VECTOR('',#85686,1000.) ;
#13715 = VECTOR('',#85687,1000.) ;
#13716 = VECTOR('',#85688,1000.) ;
#13717 = VECTOR('',#85689,1000.) ;
#13718 = VECTOR('',#85692,1000.) ;
#13719 = VECTOR('',#85693,1000.) ;
#13720 = VECTOR('',#85694,1000.) ;
#13721 = VECTOR('',#85695,1000.) ;
#13722 = VECTOR('',#85698,1000.) ;
#13723 = VECTOR('',#85699,1000.) ;
#13724 = VECTOR('',#85700,1000.) ;
#13725 = VECTOR('',#85701,1000.) ;
#13726 = VECTOR('',#85704,1000.) ;
#13727 = VECTOR('',#85705,1000.) ;
#13728 = VECTOR('',#85706,1000.) ;
#13729 = VECTOR('',#85707,1000.) ;
#13730 = VECTOR('',#85710,1000.) ;
#13731 = VECTOR('',#85711,1000.) ;
#13732 = VECTOR('',#85712,1000.) ;
#13733 = VECTOR('',#85713,1000.) ;
#13734 = VECTOR('',#85716,1000.) ;
#13735 = VECTOR('',#85717,1000.) ;
#13736 = VECTOR('',#85718,1000.) ;
#13737 = VECTOR('',#85719,1000.) ;
#13738 = VECTOR('',#85720,1000.) ;
#13739 = VECTOR('',#85721,1000.) ;
#13740 = VECTOR('',#85722,1000.) ;
#13741 = VECTOR('',#85723,1000.) ;
#13742 = VECTOR('',#85726,1000.) ;
#13743 = VECTOR('',#85729,1000.) ;
#13744 = VECTOR('',#85732,1000.) ;
#13745 = VECTOR('',#85735,1000.) ;
#13746 = VECTOR('',#85742,1000.) ;
#13747 = VECTOR('',#85743,1000.) ;
#13748 = VECTOR('',#85746,1000.) ;
#13749 = VECTOR('',#85751,1000.) ;
#13750 = VECTOR('',#85752,1000.) ;
#13751 = VECTOR('',#85753,1000.) ;
#13752 = VECTOR('',#85756,1000.) ;
#13753 = VECTOR('',#85757,1000.) ;
#13754 = VECTOR('',#85758,1000.) ;
#13755 = VECTOR('',#85763,1000.) ;
#13756 = VECTOR('',#85766,1000.) ;
#13757 = VECTOR('',#85771,1000.) ;
#13758 = VECTOR('',#85774,1000.) ;
#13759 = VECTOR('',#85777,1000.) ;
#13760 = VECTOR('',#85778,1000.) ;
#13761 = VECTOR('',#85779,1000.) ;
#13762 = VECTOR('',#85782,1000.) ;
#13763 = VECTOR('',#85783,1000.) ;
#13764 = VECTOR('',#85784,1000.) ;
#13765 = VECTOR('',#85789,1000.) ;
#13766 = VECTOR('',#85790,1000.) ;
#13767 = VECTOR('',#85795,1000.) ;
#13768 = VECTOR('',#85800,1000.) ;
#13769 = VECTOR('',#85801,1000.) ;
#13770 = VECTOR('',#85802,1000.) ;
#13771 = VECTOR('',#85805,1000.) ;
#13772 = VECTOR('',#85806,1000.) ;
#13773 = VECTOR('',#85807,1000.) ;
#13774 = VECTOR('',#85812,1000.) ;
#13775 = VECTOR('',#85815,1000.) ;
#13776 = VECTOR('',#85818,1000.) ;
#13777 = VECTOR('',#85819,1000.) ;
#13778 = VECTOR('',#85820,1000.) ;
#13779 = VECTOR('',#85821,1000.) ;
#13780 = VECTOR('',#85826,1000.) ;
#13781 = VECTOR('',#85829,1000.) ;
#13782 = VECTOR('',#85832,1000.) ;
#13783 = VECTOR('',#85833,1000.) ;
#13784 = VECTOR('',#85834,1000.) ;
#13785 = VECTOR('',#85837,1000.) ;
#13786 = VECTOR('',#85838,1000.) ;
#13787 = VECTOR('',#85839,1000.) ;
#13788 = VECTOR('',#85840,1000.) ;
#13789 = VECTOR('',#85843,1000.) ;
#13790 = VECTOR('',#85844,1000.) ;
#13791 = VECTOR('',#85845,1000.) ;
#13792 = VECTOR('',#85850,1000.) ;
#13793 = VECTOR('',#85851,1000.) ;
#13794 = VECTOR('',#85852,1000.) ;
#13795 = VECTOR('',#85853,1000.) ;
#13796 = VECTOR('',#85858,1000.) ;
#13797 = VECTOR('',#85859,1000.) ;
#13798 = VECTOR('',#85862,1000.) ;
#13799 = VECTOR('',#85865,1000.) ;
#13800 = VECTOR('',#85868,1000.) ;
#13801 = VECTOR('',#85869,1000.) ;
#13802 = VECTOR('',#85870,1000.) ;
#13803 = VECTOR('',#85871,1000.) ;
#13804 = VECTOR('',#85874,1000.) ;
#13805 = VECTOR('',#85875,1000.) ;
#13806 = VECTOR('',#85876,1000.) ;
#13807 = VECTOR('',#85877,1000.) ;
#13808 = VECTOR('',#85880,1000.) ;
#13809 = VECTOR('',#85881,1000.) ;
#13810 = VECTOR('',#85882,1000.) ;
#13811 = VECTOR('',#85883,1000.) ;
#13812 = VECTOR('',#85886,1000.) ;
#13813 = VECTOR('',#85887,1000.) ;
#13814 = VECTOR('',#85888,1000.) ;
#13815 = VECTOR('',#85889,1000.) ;
#13816 = VECTOR('',#85892,1000.) ;
#13817 = VECTOR('',#85893,1000.) ;
#13818 = VECTOR('',#85894,1000.) ;
#13819 = VECTOR('',#85897,1000.) ;
#13820 = VECTOR('',#85898,1000.) ;
#13821 = VECTOR('',#85899,1000.) ;
#13822 = VECTOR('',#85902,1000.) ;
#13823 = VECTOR('',#85903,1000.) ;
#13824 = VECTOR('',#85904,1000.) ;
#13825 = VECTOR('',#85907,1000.) ;
#13826 = VECTOR('',#85908,1000.) ;
#13827 = VECTOR('',#85909,1000.) ;
#13828 = VECTOR('',#85912,1000.) ;
#13829 = VECTOR('',#85913,1000.) ;
#13830 = VECTOR('',#85914,1000.) ;
#13831 = VECTOR('',#85917,1000.) ;
#13832 = VECTOR('',#85922,1000.) ;
#13833 = VECTOR('',#85923,1000.) ;
#13834 = VECTOR('',#85924,1000.) ;
#13835 = VECTOR('',#85927,1000.) ;
#13836 = VECTOR('',#85932,1000.) ;
#13837 = VECTOR('',#85939,1000.) ;
#13838 = VECTOR('',#85940,1000.) ;
#13839 = VECTOR('',#85941,1000.) ;
#13840 = VECTOR('',#85944,1000.) ;
#13841 = VECTOR('',#85945,1000.) ;
#13842 = VECTOR('',#85946,1000.) ;
#13843 = VECTOR('',#85947,1000.) ;
#13844 = VECTOR('',#85950,1000.) ;
#13845 = VECTOR('',#85951,1000.) ;
#13846 = VECTOR('',#85952,1000.) ;
#13847 = VECTOR('',#85953,1000.) ;
#13848 = VECTOR('',#85956,1000.) ;
#13849 = VECTOR('',#85957,1000.) ;
#13850 = VECTOR('',#85958,1000.) ;
#13851 = VECTOR('',#85959,1000.) ;
#13852 = VECTOR('',#85962,1000.) ;
#13853 = VECTOR('',#85963,1000.) ;
#13854 = VECTOR('',#85964,1000.) ;
#13855 = VECTOR('',#85965,1000.) ;
#13856 = VECTOR('',#85974,1000.) ;
#13857 = VECTOR('',#85975,1000.) ;
#13858 = VECTOR('',#85976,1000.) ;
#13859 = VECTOR('',#85977,1000.) ;
#13860 = VECTOR('',#85980,1000.) ;
#13861 = VECTOR('',#85981,1000.) ;
#13862 = VECTOR('',#85982,1000.) ;
#13863 = VECTOR('',#85983,1000.) ;
#13864 = VECTOR('',#85986,1000.) ;
#13865 = VECTOR('',#85987,1000.) ;
#13866 = VECTOR('',#85988,1000.) ;
#13867 = VECTOR('',#85989,1000.) ;
#13868 = VECTOR('',#85992,1000.) ;
#13869 = VECTOR('',#85993,1000.) ;
#13870 = VECTOR('',#85994,1000.) ;
#13871 = VECTOR('',#85995,1000.) ;
#13872 = VECTOR('',#85998,1000.) ;
#13873 = VECTOR('',#86001,1000.) ;
#13874 = VECTOR('',#86012,1000.) ;
#13875 = VECTOR('',#86015,1000.) ;
#13876 = VECTOR('',#86194,1000.) ;
#13877 = VECTOR('',#86219,1000.) ;
#13878 = VECTOR('',#86232,1000.) ;
#13879 = VECTOR('',#86267,1000.) ;
#13880 = VECTOR('',#86278,1000.) ;
#13881 = VECTOR('',#86301,1000.) ;
#13882 = VECTOR('',#86860,1.4986) ;
#13883 = VECTOR('',#86869,1000.) ;
#13884 = VECTOR('',#86872,1000.) ;
#13885 = VECTOR('',#86877,1000.) ;
#13886 = VECTOR('',#86878,1000.) ;
#13887 = VECTOR('',#86881,1000.) ;
#13888 = VECTOR('',#86882,1000.) ;
#13889 = VECTOR('',#86883,1000.) ;
#13890 = VECTOR('',#86886,1000.) ;
#13891 = VECTOR('',#86887,1000.) ;
#13892 = VECTOR('',#86890,1000.) ;
#13893 = VECTOR('',#86891,1000.) ;
#13894 = VECTOR('',#86892,1000.) ;
#13895 = VECTOR('',#86897,1000.) ;
#13896 = VECTOR('',#86898,1000.) ;
#13897 = VECTOR('',#86901,1000.) ;
#13898 = VECTOR('',#86902,1000.) ;
#13899 = VECTOR('',#86905,1000.) ;
#13900 = VECTOR('',#86906,1000.) ;
#13901 = VECTOR('',#86907,1000.) ;
#13902 = VECTOR('',#86912,1000.) ;
#13903 = VECTOR('',#86913,1000.) ;
#13904 = VECTOR('',#86914,1000.) ;
#13905 = VECTOR('',#86919,1000.) ;
#13906 = VECTOR('',#86920,1000.) ;
#13907 = VECTOR('',#86923,1000.) ;
#13908 = VECTOR('',#86924,1000.) ;
#13909 = VECTOR('',#86927,1000.) ;
#13910 = VECTOR('',#86928,1000.) ;
#13911 = VECTOR('',#86933,1000.) ;
#13912 = VECTOR('',#86934,1000.) ;
#13913 = VECTOR('',#86939,1000.) ;
#13914 = VECTOR('',#86942,1000.) ;
#13915 = VECTOR('',#86945,1000.) ;
#13916 = VECTOR('',#86948,1000.) ;
#13917 = VECTOR('',#86951,1000.) ;
#13918 = VECTOR('',#86952,1000.) ;
#13919 = VECTOR('',#86953,1000.) ;
#13920 = VECTOR('',#86956,1000.) ;
#13921 = VECTOR('',#86957,1000.) ;
#13922 = VECTOR('',#87002,1000.) ;
#13923 = VECTOR('',#87005,1000.) ;
#13924 = VECTOR('',#87006,1000.) ;
#13925 = VECTOR('',#87039,1000.) ;
#13926 = VECTOR('',#87042,1000.) ;
#13927 = VECTOR('',#87043,1000.) ;
#13928 = VECTOR('',#87076,1000.) ;
#13929 = VECTOR('',#87079,1000.) ;
#13930 = VECTOR('',#87080,1000.) ;
#13931 = VECTOR('',#87113,1000.) ;
#13932 = VECTOR('',#87116,1000.) ;
#13933 = VECTOR('',#87117,1000.) ;
#13934 = VECTOR('',#87150,1000.) ;
#13935 = VECTOR('',#87153,1000.) ;
#13936 = VECTOR('',#87154,1000.) ;
#13937 = VECTOR('',#87187,1000.) ;
#13938 = VECTOR('',#87190,1000.) ;
#13939 = VECTOR('',#87191,1000.) ;
#13940 = VECTOR('',#87224,1000.) ;
#13941 = VECTOR('',#87227,1000.) ;
#13942 = VECTOR('',#87228,1000.) ;
#13943 = VECTOR('',#87261,1000.) ;
#13944 = VECTOR('',#87264,1000.) ;
#13945 = VECTOR('',#87265,1000.) ;
#13946 = VECTOR('',#87388,1000.) ;
#13947 = VECTOR('',#87391,1000.) ;
#13948 = VECTOR('',#87392,1000.) ;
#13949 = VECTOR('',#87395,1.) ;
#13950 = VECTOR('',#87398,1.) ;
#13951 = VECTOR('',#87401,1.) ;
#13952 = VECTOR('',#87404,1.) ;
#13953 = VECTOR('',#87407,1.) ;
#13954 = VECTOR('',#87410,0.999999999999999) ;
#13955 = VECTOR('',#87413,0.999999999999999) ;
#13956 = VECTOR('',#87416,1.) ;
#13957 = VECTOR('',#87419,1.) ;
#13958 = VECTOR('',#87424,1000.) ;
#13959 = VECTOR('',#87425,1000.) ;
#13960 = VECTOR('',#87430,1000.) ;
#13961 = VECTOR('',#87431,1000.) ;
#13962 = VECTOR('',#87436,1000.) ;
#13963 = VECTOR('',#87437,1000.) ;
#13964 = VECTOR('',#87442,1000.) ;
#13965 = VECTOR('',#87443,1000.) ;
#13966 = VECTOR('',#87448,1000.) ;
#13967 = VECTOR('',#87449,1000.) ;
#13968 = VECTOR('',#87454,1000.) ;
#13969 = VECTOR('',#87455,1000.) ;
#13970 = VECTOR('',#87460,1000.) ;
#13971 = VECTOR('',#87461,1000.) ;
#13972 = VECTOR('',#87466,1000.) ;
#13973 = VECTOR('',#87467,1000.) ;
#13974 = VECTOR('',#87472,1000.) ;
#13975 = VECTOR('',#87473,1000.) ;
#13976 = VECTOR('',#87516,1000.) ;
#13977 = VECTOR('',#87519,1000.) ;
#13978 = VECTOR('',#87520,1000.) ;
#13979 = VECTOR('',#87523,1.) ;
#13980 = VECTOR('',#87528,1000.) ;
#13981 = VECTOR('',#87529,1000.) ;
#13982 = VECTOR('',#87532,1000.) ;
#13983 = VECTOR('',#87535,1000.) ;
#13984 = VECTOR('',#87540,1000.) ;
#13985 = VECTOR('',#87541,1000.) ;
#13986 = VECTOR('',#87542,1000.) ;
#13987 = VECTOR('',#87543,1000.) ;
#13988 = VECTOR('',#87544,1000.) ;
#13989 = VECTOR('',#87549,1000.) ;
#13990 = VECTOR('',#87552,1000.) ;
#13991 = VECTOR('',#87557,1000.) ;
#13992 = VECTOR('',#87558,1000.) ;
#13993 = VECTOR('',#87559,1000.) ;
#13994 = VECTOR('',#87560,1000.) ;
#13995 = VECTOR('',#87561,1000.) ;
#13996 = VECTOR('',#87566,1000.) ;
#13997 = VECTOR('',#87569,1000.) ;
#13998 = VECTOR('',#87574,1000.) ;
#13999 = VECTOR('',#87575,1000.) ;
#14000 = VECTOR('',#87576,1000.) ;
#14001 = VECTOR('',#87577,1000.) ;
#14002 = VECTOR('',#87578,1000.) ;
#14003 = VECTOR('',#87583,1000.) ;
#14004 = VECTOR('',#87586,1000.) ;
#14005 = VECTOR('',#87591,1000.) ;
#14006 = VECTOR('',#87592,1000.) ;
#14007 = VECTOR('',#87593,1000.) ;
#14008 = VECTOR('',#87594,1000.) ;
#14009 = VECTOR('',#87595,1000.) ;
#14010 = VECTOR('',#87600,1000.) ;
#14011 = VECTOR('',#87603,1000.) ;
#14012 = VECTOR('',#87608,1000.) ;
#14013 = VECTOR('',#87609,1000.) ;
#14014 = VECTOR('',#87610,1000.) ;
#14015 = VECTOR('',#87611,1000.) ;
#14016 = VECTOR('',#87612,1000.) ;
#14017 = VECTOR('',#87617,1000.) ;
#14018 = VECTOR('',#87620,1000.) ;
#14019 = VECTOR('',#87625,1000.) ;
#14020 = VECTOR('',#87626,1000.) ;
#14021 = VECTOR('',#87627,1000.) ;
#14022 = VECTOR('',#87628,1000.) ;
#14023 = VECTOR('',#87629,1000.) ;
#14024 = VECTOR('',#87634,1000.) ;
#14025 = VECTOR('',#87637,1000.) ;
#14026 = VECTOR('',#87642,1000.) ;
#14027 = VECTOR('',#87643,1000.) ;
#14028 = VECTOR('',#87644,1000.) ;
#14029 = VECTOR('',#87645,1000.) ;
#14030 = VECTOR('',#87646,1000.) ;
#14031 = VECTOR('',#87651,1000.) ;
#14032 = VECTOR('',#87654,1000.) ;
#14033 = VECTOR('',#87659,1000.) ;
#14034 = VECTOR('',#87660,1000.) ;
#14035 = VECTOR('',#87661,1000.) ;
#14036 = VECTOR('',#87662,1000.) ;
#14037 = VECTOR('',#87663,1000.) ;
#14038 = VECTOR('',#87668,1000.) ;
#14039 = VECTOR('',#87671,1000.) ;
#14040 = VECTOR('',#87676,1000.) ;
#14041 = VECTOR('',#87677,1000.) ;
#14042 = VECTOR('',#87678,1000.) ;
#14043 = VECTOR('',#87679,1000.) ;
#14044 = VECTOR('',#87680,1000.) ;
#14045 = VECTOR('',#87687,1000.) ;
#14046 = VECTOR('',#87688,1000.) ;
#14047 = VECTOR('',#87689,1000.) ;
#14048 = VECTOR('',#87690,1000.) ;
#14049 = VECTOR('',#87695,1000.) ;
#14050 = VECTOR('',#87696,1000.) ;
#14051 = VECTOR('',#87697,1000.) ;
#14052 = VECTOR('',#87698,1000.) ;
#14053 = VECTOR('',#87703,1000.) ;
#14054 = VECTOR('',#87704,1000.) ;
#14055 = VECTOR('',#87705,1000.) ;
#14056 = VECTOR('',#87706,1000.) ;
#14057 = VECTOR('',#87711,1000.) ;
#14058 = VECTOR('',#87712,1000.) ;
#14059 = VECTOR('',#87713,1000.) ;
#14060 = VECTOR('',#87714,1000.) ;
#14061 = VECTOR('',#87719,1000.) ;
#14062 = VECTOR('',#87720,1000.) ;
#14063 = VECTOR('',#87721,1000.) ;
#14064 = VECTOR('',#87722,1000.) ;
#14065 = VECTOR('',#87727,1000.) ;
#14066 = VECTOR('',#87728,1000.) ;
#14067 = VECTOR('',#87729,1000.) ;
#14068 = VECTOR('',#87730,1000.) ;
#14069 = VECTOR('',#87735,1000.) ;
#14070 = VECTOR('',#87736,1000.) ;
#14071 = VECTOR('',#87737,1000.) ;
#14072 = VECTOR('',#87738,1000.) ;
#14073 = VECTOR('',#87743,1000.) ;
#14074 = VECTOR('',#87744,1000.) ;
#14075 = VECTOR('',#87745,1000.) ;
#14076 = VECTOR('',#87746,1000.) ;
#14077 = VECTOR('',#87751,1000.) ;
#14078 = VECTOR('',#87752,1000.) ;
#14079 = VECTOR('',#87753,1000.) ;
#14080 = VECTOR('',#87754,1000.) ;
#14081 = VECTOR('',#87759,1000.) ;
#14082 = VECTOR('',#87760,1000.) ;
#14083 = VECTOR('',#87761,1000.) ;
#14084 = VECTOR('',#87762,1000.) ;
#14085 = VECTOR('',#87767,1000.) ;
#14086 = VECTOR('',#87768,1000.) ;
#14087 = VECTOR('',#87769,1000.) ;
#14088 = VECTOR('',#87770,1000.) ;
#14089 = VECTOR('',#87775,1000.) ;
#14090 = VECTOR('',#87776,1000.) ;
#14091 = VECTOR('',#87777,1000.) ;
#14092 = VECTOR('',#87778,1000.) ;
#14093 = VECTOR('',#87783,1000.) ;
#14094 = VECTOR('',#87784,1000.) ;
#14095 = VECTOR('',#87785,1000.) ;
#14096 = VECTOR('',#87786,1000.) ;
#14097 = VECTOR('',#87791,1000.) ;
#14098 = VECTOR('',#87792,1000.) ;
#14099 = VECTOR('',#87793,1000.) ;
#14100 = VECTOR('',#87794,1000.) ;
#14101 = VECTOR('',#87799,1000.) ;
#14102 = VECTOR('',#87800,1000.) ;
#14103 = VECTOR('',#87801,1000.) ;
#14104 = VECTOR('',#87802,1000.) ;
#14105 = VECTOR('',#87807,1000.) ;
#14106 = VECTOR('',#87808,1000.) ;
#14107 = VECTOR('',#87809,1000.) ;
#14108 = VECTOR('',#87810,1000.) ;
#14109 = VECTOR('',#87815,1000.) ;
#14110 = VECTOR('',#87816,1000.) ;
#14111 = VECTOR('',#87817,1000.) ;
#14112 = VECTOR('',#87818,1000.) ;
#14113 = VECTOR('',#87823,1000.) ;
#14114 = VECTOR('',#87824,1000.) ;
#14115 = VECTOR('',#87825,1000.) ;
#14116 = VECTOR('',#87826,1000.) ;
#14117 = VECTOR('',#87829,1000.) ;
#14118 = VECTOR('',#87832,1000.) ;
#14119 = VECTOR('',#87837,1000.) ;
#14120 = VECTOR('',#87840,1000.) ;
#14121 = VECTOR('',#87845,1000.) ;
#14122 = VECTOR('',#87848,1000.) ;
#14123 = VECTOR('',#87853,1000.) ;
#14124 = VECTOR('',#87856,1000.) ;
#14125 = VECTOR('',#87861,1000.) ;
#14126 = VECTOR('',#87864,1000.) ;
#14127 = VECTOR('',#87869,1000.) ;
#14128 = VECTOR('',#87872,1000.) ;
#14129 = VECTOR('',#87877,1000.) ;
#14130 = VECTOR('',#87880,1000.) ;
#14131 = VECTOR('',#87885,1000.) ;
#14132 = VECTOR('',#87888,1000.) ;
#14133 = VECTOR('',#87893,1000.) ;
#14134 = VECTOR('',#87896,1000.) ;
#14135 = VECTOR('',#87901,1000.) ;
#14136 = VECTOR('',#87904,1000.) ;
#14137 = VECTOR('',#87909,1000.) ;
#14138 = VECTOR('',#87910,1000.) ;
#14139 = VECTOR('',#87911,1000.) ;
#14140 = VECTOR('',#87912,1000.) ;
#14141 = VECTOR('',#87913,1000.) ;
#14142 = VECTOR('',#87920,1000.) ;
#14143 = VECTOR('',#87921,1000.) ;
#14144 = VECTOR('',#87922,1000.) ;
#14145 = VECTOR('',#87923,1000.) ;
#14146 = VECTOR('',#87928,1000.) ;
#14147 = VECTOR('',#87929,1000.) ;
#14148 = VECTOR('',#87930,1000.) ;
#14149 = VECTOR('',#87931,1000.) ;
#14150 = VECTOR('',#87934,1000.) ;
#14151 = VECTOR('',#87937,1000.) ;
#14152 = VECTOR('',#87942,1000.) ;
#14153 = VECTOR('',#87945,1000.) ;
#14154 = VECTOR('',#87952,1000.) ;
#14155 = VECTOR('',#87953,1000.) ;
#14156 = VECTOR('',#87954,1000.) ;
#14157 = VECTOR('',#87955,1000.) ;
#14158 = VECTOR('',#87956,1000.) ;
#14159 = VECTOR('',#87959,1000.) ;
#14160 = VECTOR('',#87962,1000.) ;
#14161 = VECTOR('',#87963,1000.) ;
#14162 = VECTOR('',#87966,1000.) ;
#14163 = VECTOR('',#87969,1000.) ;
#14164 = VECTOR('',#87970,1000.) ;
#14165 = VECTOR('',#87973,1000.) ;
#14166 = VECTOR('',#87976,1000.) ;
#14167 = VECTOR('',#87977,1000.) ;
#14168 = VECTOR('',#87980,1000.) ;
#14169 = VECTOR('',#87983,1000.) ;
#14170 = VECTOR('',#87984,1000.) ;
#14171 = VECTOR('',#87987,1000.) ;
#14172 = VECTOR('',#87990,1000.) ;
#14173 = VECTOR('',#87991,1000.) ;
#14174 = VECTOR('',#87994,1000.) ;
#14175 = VECTOR('',#87997,1000.) ;
#14176 = VECTOR('',#87998,1000.) ;
#14177 = VECTOR('',#88001,1000.) ;
#14178 = VECTOR('',#88004,1000.) ;
#14179 = VECTOR('',#88005,1000.) ;
#14180 = VECTOR('',#88008,1000.) ;
#14181 = VECTOR('',#88011,1000.) ;
#14182 = VECTOR('',#88012,1000.) ;
#14183 = VECTOR('',#88015,1000.) ;
#14184 = VECTOR('',#88018,1000.) ;
#14185 = VECTOR('',#88019,1000.) ;
#14186 = VECTOR('',#88022,1000.) ;
#14187 = VECTOR('',#88027,1000.) ;
#14188 = VECTOR('',#88034,1000.) ;
#14189 = VECTOR('',#88035,1000.) ;
#14190 = VECTOR('',#88038,1000.) ;
#14191 = VECTOR('',#88041,1000.) ;
#14192 = VECTOR('',#88042,1000.) ;
#14193 = VECTOR('',#88045,1000.) ;
#14194 = VECTOR('',#88048,1000.) ;
#14195 = VECTOR('',#88049,1000.) ;
#14196 = VECTOR('',#88052,1000.) ;
#14197 = VECTOR('',#88055,1000.) ;
#14198 = VECTOR('',#88056,1000.) ;
#14199 = VECTOR('',#88059,1000.) ;
#14200 = VECTOR('',#88062,1000.) ;
#14201 = VECTOR('',#88063,1000.) ;
#14202 = VECTOR('',#88066,1000.) ;
#14203 = VECTOR('',#88069,1000.) ;
#14204 = VECTOR('',#88070,1000.) ;
#14205 = VECTOR('',#88073,1000.) ;
#14206 = VECTOR('',#88076,1000.) ;
#14207 = VECTOR('',#88077,1000.) ;
#14208 = VECTOR('',#88080,1000.) ;
#14209 = VECTOR('',#88083,1000.) ;
#14210 = VECTOR('',#88084,1000.) ;
#14211 = VECTOR('',#88087,1000.) ;
#14212 = VECTOR('',#88090,1000.) ;
#14213 = VECTOR('',#88091,1000.) ;
#14214 = VECTOR('',#88094,1000.) ;
#14215 = VECTOR('',#88097,1000.) ;
#14216 = VECTOR('',#88098,1000.) ;
#14217 = VECTOR('',#88099,1000.) ;
#14218 = VECTOR('',#88100,1000.) ;
#14219 = VECTOR('',#88101,1000.) ;
#14220 = VECTOR('',#88104,1000.) ;
#14221 = VECTOR('',#88107,1000.) ;
#14222 = VECTOR('',#88114,1000.) ;
#14223 = VECTOR('',#88115,1000.) ;
#14224 = VECTOR('',#88116,1000.) ;
#14225 = VECTOR('',#88119,1000.) ;
#14226 = VECTOR('',#88126,1000.) ;
#14227 = VECTOR('',#88127,1000.) ;
#14228 = VECTOR('',#88128,1000.) ;
#14229 = VECTOR('',#88131,1000.) ;
#14230 = VECTOR('',#88138,1000.) ;
#14231 = VECTOR('',#88139,1000.) ;
#14232 = VECTOR('',#88140,1000.) ;
#14233 = VECTOR('',#88143,1000.) ;
#14234 = VECTOR('',#88150,1000.) ;
#14235 = VECTOR('',#88151,1000.) ;
#14236 = VECTOR('',#88152,1000.) ;
#14237 = VECTOR('',#88155,1000.) ;
#14238 = VECTOR('',#88162,1000.) ;
#14239 = VECTOR('',#88163,1000.) ;
#14240 = VECTOR('',#88164,1000.) ;
#14241 = VECTOR('',#88167,1000.) ;
#14242 = VECTOR('',#88174,1000.) ;
#14243 = VECTOR('',#88175,1000.) ;
#14244 = VECTOR('',#88178,1000.) ;
#14245 = VECTOR('',#88179,1000.) ;
#14246 = VECTOR('',#88180,1000.) ;
#14247 = VECTOR('',#88183,1000.) ;
#14248 = VECTOR('',#88186,1000.) ;
#14249 = VECTOR('',#88187,1000.) ;
#14250 = VECTOR('',#88190,1000.) ;
#14251 = VECTOR('',#88191,1000.) ;
#14252 = VECTOR('',#88192,1000.) ;
#14253 = VECTOR('',#88195,1000.) ;
#14254 = VECTOR('',#88198,1000.) ;
#14255 = VECTOR('',#88205,1000.) ;
#14256 = VECTOR('',#88208,1000.) ;
#14257 = VECTOR('',#88211,1000.) ;
#14258 = VECTOR('',#88212,1000.) ;
#14259 = VECTOR('',#88213,1000.) ;
#14260 = VECTOR('',#88216,1000.) ;
#14261 = VECTOR('',#88219,1000.) ;
#14262 = VECTOR('',#88220,1000.) ;
#14263 = VECTOR('',#88223,1000.) ;
#14264 = VECTOR('',#88224,1000.) ;
#14265 = VECTOR('',#88225,1000.) ;
#14266 = VECTOR('',#88228,1000.) ;
#14267 = VECTOR('',#88231,1000.) ;
#14268 = VECTOR('',#88238,1000.) ;
#14269 = VECTOR('',#88241,1000.) ;
#14270 = VECTOR('',#88244,1000.) ;
#14271 = VECTOR('',#88245,1000.) ;
#14272 = VECTOR('',#88246,1000.) ;
#14273 = VECTOR('',#88249,1000.) ;
#14274 = VECTOR('',#88252,1000.) ;
#14275 = VECTOR('',#88253,1000.) ;
#14276 = VECTOR('',#88256,1000.) ;
#14277 = VECTOR('',#88257,1000.) ;
#14278 = VECTOR('',#88258,1000.) ;
#14279 = VECTOR('',#88261,1000.) ;
#14280 = VECTOR('',#88264,1000.) ;
#14281 = VECTOR('',#88271,1000.) ;
#14282 = VECTOR('',#88274,1000.) ;
#14283 = VECTOR('',#88277,1000.) ;
#14284 = VECTOR('',#88278,1000.) ;
#14285 = VECTOR('',#88279,1000.) ;
#14286 = VECTOR('',#88282,1000.) ;
#14287 = VECTOR('',#88285,1000.) ;
#14288 = VECTOR('',#88286,1000.) ;
#14289 = VECTOR('',#88289,1000.) ;
#14290 = VECTOR('',#88290,1000.) ;
#14291 = VECTOR('',#88291,1000.) ;
#14292 = VECTOR('',#88294,1000.) ;
#14293 = VECTOR('',#88297,1000.) ;
#14294 = VECTOR('',#88304,1000.) ;
#14295 = VECTOR('',#88307,1000.) ;
#14296 = VECTOR('',#88310,1000.) ;
#14297 = VECTOR('',#88311,1000.) ;
#14298 = VECTOR('',#88312,1000.) ;
#14299 = VECTOR('',#88315,1000.) ;
#14300 = VECTOR('',#88318,1000.) ;
#14301 = VECTOR('',#88319,1000.) ;
#14302 = VECTOR('',#88322,1000.) ;
#14303 = VECTOR('',#88323,1000.) ;
#14304 = VECTOR('',#88324,1000.) ;
#14305 = VECTOR('',#88327,1000.) ;
#14306 = VECTOR('',#88330,1000.) ;
#14307 = VECTOR('',#88337,1000.) ;
#14308 = VECTOR('',#88340,1000.) ;
#14309 = VECTOR('',#88343,1000.) ;
#14310 = VECTOR('',#88344,1000.) ;
#14311 = VECTOR('',#88345,1000.) ;
#14312 = VECTOR('',#88348,1000.) ;
#14313 = VECTOR('',#88351,1000.) ;
#14314 = VECTOR('',#88352,1000.) ;
#14315 = VECTOR('',#88355,1000.) ;
#14316 = VECTOR('',#88356,1000.) ;
#14317 = VECTOR('',#88357,1000.) ;
#14318 = VECTOR('',#88360,1000.) ;
#14319 = VECTOR('',#88363,1000.) ;
#14320 = VECTOR('',#88370,1000.) ;
#14321 = VECTOR('',#88373,1000.) ;
#14322 = VECTOR('',#88376,1000.) ;
#14323 = VECTOR('',#88377,1000.) ;
#14324 = VECTOR('',#88378,1000.) ;
#14325 = VECTOR('',#88381,1000.) ;
#14326 = VECTOR('',#88384,1000.) ;
#14327 = VECTOR('',#88385,1000.) ;
#14328 = VECTOR('',#88388,1000.) ;
#14329 = VECTOR('',#88389,1000.) ;
#14330 = VECTOR('',#88390,1000.) ;
#14331 = VECTOR('',#88393,1000.) ;
#14332 = VECTOR('',#88396,1000.) ;
#14333 = VECTOR('',#88403,1000.) ;
#14334 = VECTOR('',#88406,1000.) ;
#14335 = VECTOR('',#88409,1000.) ;
#14336 = VECTOR('',#88410,1000.) ;
#14337 = VECTOR('',#88411,1000.) ;
#14338 = VECTOR('',#88414,1000.) ;
#14339 = VECTOR('',#88417,1000.) ;
#14340 = VECTOR('',#88418,1000.) ;
#14341 = VECTOR('',#88421,1000.) ;
#14342 = VECTOR('',#88422,1000.) ;
#14343 = VECTOR('',#88423,1000.) ;
#14344 = VECTOR('',#88426,1000.) ;
#14345 = VECTOR('',#88429,1000.) ;
#14346 = VECTOR('',#88436,1000.) ;
#14347 = VECTOR('',#88439,1000.) ;
#14348 = VECTOR('',#88442,1000.) ;
#14349 = VECTOR('',#88443,1000.) ;
#14350 = VECTOR('',#88444,1000.) ;
#14351 = VECTOR('',#88447,1000.) ;
#14352 = VECTOR('',#88450,1000.) ;
#14353 = VECTOR('',#88451,1000.) ;
#14354 = VECTOR('',#88454,1000.) ;
#14355 = VECTOR('',#88455,1000.) ;
#14356 = VECTOR('',#88456,1000.) ;
#14357 = VECTOR('',#88459,1000.) ;
#14358 = VECTOR('',#88462,1000.) ;
#14359 = VECTOR('',#88469,1000.) ;
#14360 = VECTOR('',#88472,1000.) ;
#14361 = VECTOR('',#88475,1000.) ;
#14362 = VECTOR('',#88476,1000.) ;
#14363 = VECTOR('',#88477,1000.) ;
#14364 = VECTOR('',#88480,1000.) ;
#14365 = VECTOR('',#88483,1000.) ;
#14366 = VECTOR('',#88484,1000.) ;
#14367 = VECTOR('',#88487,1000.) ;
#14368 = VECTOR('',#88488,1000.) ;
#14369 = VECTOR('',#88489,1000.) ;
#14370 = VECTOR('',#88492,1000.) ;
#14371 = VECTOR('',#88495,1000.) ;
#14372 = VECTOR('',#88502,1000.) ;
#14373 = VECTOR('',#88505,1000.) ;
#14374 = VECTOR('',#88508,1000.) ;
#14375 = VECTOR('',#88509,1000.) ;
#14376 = VECTOR('',#88510,1000.) ;
#14377 = VECTOR('',#88511,1000.) ;
#14378 = VECTOR('',#88514,1000.) ;
#14379 = VECTOR('',#88515,1000.) ;
#14380 = VECTOR('',#88516,1000.) ;
#14381 = VECTOR('',#88519,1000.) ;
#14382 = VECTOR('',#88522,1000.) ;
#14383 = VECTOR('',#88523,1000.) ;
#14384 = VECTOR('',#88524,1000.) ;
#14385 = VECTOR('',#88525,1000.) ;
#14386 = VECTOR('',#88528,1000.) ;
#14387 = VECTOR('',#88529,1000.) ;
#14388 = VECTOR('',#88530,1000.) ;
#14389 = VECTOR('',#88533,1000.) ;
#14390 = VECTOR('',#88536,1000.) ;
#14391 = VECTOR('',#88537,1000.) ;
#14392 = VECTOR('',#88538,1000.) ;
#14393 = VECTOR('',#88539,1000.) ;
#14394 = VECTOR('',#88540,1000.) ;
#14395 = VECTOR('',#88541,1000.) ;
#14396 = VECTOR('',#88544,1000.) ;
#14397 = VECTOR('',#88547,1000.) ;
#14398 = VECTOR('',#88550,1000.) ;
#14399 = VECTOR('',#88551,1000.) ;
#14400 = VECTOR('',#88552,1000.) ;
#14401 = VECTOR('',#88553,1000.) ;
#14402 = VECTOR('',#88556,1000.) ;
#14403 = VECTOR('',#88557,1000.) ;
#14404 = VECTOR('',#88558,1000.) ;
#14405 = VECTOR('',#88561,1000.) ;
#14406 = VECTOR('',#88562,1000.) ;
#14407 = VECTOR('',#88563,1000.) ;
#14408 = VECTOR('',#88564,1000.) ;
#14409 = VECTOR('',#88567,1000.) ;
#14410 = VECTOR('',#88568,1000.) ;
#14411 = VECTOR('',#88569,1000.) ;
#14412 = VECTOR('',#88570,1000.) ;
#14413 = VECTOR('',#88573,1000.) ;
#14414 = VECTOR('',#88574,1000.) ;
#14415 = VECTOR('',#88575,1000.) ;
#14416 = VECTOR('',#88576,1000.) ;
#14417 = VECTOR('',#88579,1000.) ;
#14418 = VECTOR('',#88582,1000.) ;
#14419 = VECTOR('',#88587,1000.) ;
#14420 = VECTOR('',#88588,1000.) ;
#14421 = VECTOR('',#88589,1000.) ;
#14422 = VECTOR('',#88594,1000.) ;
#14423 = VECTOR('',#88599,1000.) ;
#14424 = VECTOR('',#88600,1000.) ;
#14425 = VECTOR('',#88601,1000.) ;
#14426 = VECTOR('',#88606,1000.) ;
#14427 = VECTOR('',#88611,1000.) ;
#14428 = VECTOR('',#88612,1000.) ;
#14429 = VECTOR('',#88613,1000.) ;
#14430 = VECTOR('',#88616,1000.) ;
#14431 = VECTOR('',#88621,1000.) ;
#14432 = VECTOR('',#88622,1000.) ;
#14433 = VECTOR('',#88625,1000.) ;
#14434 = VECTOR('',#88626,1000.) ;
#14435 = VECTOR('',#88627,1000.) ;
#14436 = VECTOR('',#88632,1000.) ;
#14437 = VECTOR('',#88637,1000.) ;
#14438 = VECTOR('',#88638,1000.) ;
#14439 = VECTOR('',#88639,1000.) ;
#14440 = VECTOR('',#88644,1000.) ;
#14441 = VECTOR('',#88649,1000.) ;
#14442 = VECTOR('',#88650,1000.) ;
#14443 = VECTOR('',#88651,1000.) ;
#14444 = VECTOR('',#88656,1000.) ;
#14445 = VECTOR('',#88661,1000.) ;
#14446 = VECTOR('',#88662,1000.) ;
#14447 = VECTOR('',#88663,1000.) ;
#14448 = VECTOR('',#88668,1000.) ;
#14449 = VECTOR('',#88673,1000.) ;
#14450 = VECTOR('',#88674,1000.) ;
#14451 = VECTOR('',#88675,1000.) ;
#14452 = VECTOR('',#88680,1000.) ;
#14453 = VECTOR('',#88685,1000.) ;
#14454 = VECTOR('',#88686,1000.) ;
#14455 = VECTOR('',#88687,1000.) ;
#14456 = VECTOR('',#88692,1000.) ;
#14457 = VECTOR('',#88699,1000.) ;
#14458 = VECTOR('',#88706,1000.) ;
#14459 = VECTOR('',#88711,1000.) ;
#14460 = VECTOR('',#88712,1000.) ;
#14461 = VECTOR('',#88713,1000.) ;
#14462 = VECTOR('',#88718,1000.) ;
#14463 = VECTOR('',#88723,1000.) ;
#14464 = VECTOR('',#88724,1000.) ;
#14465 = VECTOR('',#88725,1000.) ;
#14466 = VECTOR('',#88730,1000.) ;
#14467 = VECTOR('',#88735,1000.) ;
#14468 = VECTOR('',#88736,1000.) ;
#14469 = VECTOR('',#88741,1000.) ;
#14470 = VECTOR('',#88744,1000.) ;
#14471 = VECTOR('',#88745,1000.) ;
#14472 = VECTOR('',#88746,1000.) ;
#14473 = VECTOR('',#88749,1000.) ;
#14474 = VECTOR('',#88750,1000.) ;
#14475 = VECTOR('',#88751,1000.) ;
#14476 = VECTOR('',#88754,1000.) ;
#14477 = VECTOR('',#88757,1000.) ;
#14478 = VECTOR('',#88758,1000.) ;
#14479 = VECTOR('',#88759,1000.) ;
#14480 = VECTOR('',#88760,1000.) ;
#14481 = VECTOR('',#88761,1000.) ;
#14482 = VECTOR('',#88764,1000.) ;
#14483 = VECTOR('',#88767,1000.) ;
#14484 = VECTOR('',#88770,1000.) ;
#14485 = VECTOR('',#88773,1000.) ;
#14486 = VECTOR('',#88808,1000.) ;
#14487 = VECTOR('',#88811,1000.) ;
#14488 = VECTOR('',#88858,1000.) ;
#14489 = VECTOR('',#88917,1000.) ;
#14490 = VECTOR('',#88966,1000.) ;
#14491 = VECTOR('',#89323,1000.) ;
#14492 = VECTOR('',#89324,1000.) ;
#14493 = VECTOR('',#89325,1000.) ;
#14494 = VECTOR('',#89326,1000.) ;
#14495 = VECTOR('',#89329,1000.) ;
#14496 = VECTOR('',#89330,1000.) ;
#14497 = VECTOR('',#89331,1000.) ;
#14498 = VECTOR('',#89332,1000.) ;
#14499 = VECTOR('',#89335,1000.) ;
#14500 = VECTOR('',#89336,1000.) ;
#14501 = VECTOR('',#89337,1000.) ;
#14502 = VECTOR('',#89338,1000.) ;
#14503 = VECTOR('',#89341,1000.) ;
#14504 = VECTOR('',#89342,1000.) ;
#14505 = VECTOR('',#89343,1000.) ;
#14506 = VECTOR('',#89344,1000.) ;
#14507 = VECTOR('',#89347,1000.) ;
#14508 = VECTOR('',#89348,1000.) ;
#14509 = VECTOR('',#89349,1000.) ;
#14510 = VECTOR('',#89350,1000.) ;
#14511 = VECTOR('',#89353,1000.) ;
#14512 = VECTOR('',#89358,1000.) ;
#14513 = VECTOR('',#89359,1000.) ;
#14514 = VECTOR('',#89362,1000.) ;
#14515 = VECTOR('',#89367,1000.) ;
#14516 = VECTOR('',#89368,1000.) ;
#14517 = VECTOR('',#89383,1000.) ;
#14518 = VECTOR('',#89384,1000.) ;
#14519 = VECTOR('',#89385,1000.) ;
#14520 = VECTOR('',#89386,1000.) ;
#14521 = VECTOR('',#89389,1000.) ;
#14522 = VECTOR('',#89390,1000.) ;
#14523 = VECTOR('',#89391,1000.) ;
#14524 = VECTOR('',#89394,1000.) ;
#14525 = VECTOR('',#89395,1000.) ;
#14526 = VECTOR('',#89396,1000.) ;
#14527 = VECTOR('',#89399,1000.) ;
#14528 = VECTOR('',#89400,1000.) ;
#14529 = VECTOR('',#89401,1000.) ;
#14530 = VECTOR('',#89402,1000.) ;
#14531 = VECTOR('',#89405,1000.) ;
#14532 = VECTOR('',#89406,1000.) ;
#14533 = VECTOR('',#89407,1000.) ;
#14534 = VECTOR('',#89408,1000.) ;
#14535 = VECTOR('',#89411,1000.) ;
#14536 = VECTOR('',#89412,1000.) ;
#14537 = VECTOR('',#89413,1000.) ;
#14538 = VECTOR('',#89416,1000.) ;
#14539 = VECTOR('',#89417,1000.) ;
#14540 = VECTOR('',#89418,1000.) ;
#14541 = VECTOR('',#89421,1000.) ;
#14542 = VECTOR('',#89422,1000.) ;
#14543 = VECTOR('',#89423,1000.) ;
#14544 = VECTOR('',#89424,1000.) ;
#14545 = VECTOR('',#89427,1000.) ;
#14546 = VECTOR('',#89428,1000.) ;
#14547 = VECTOR('',#89429,1000.) ;
#14548 = VECTOR('',#89430,1000.) ;
#14549 = VECTOR('',#89433,1000.) ;
#14550 = VECTOR('',#89434,1000.) ;
#14551 = VECTOR('',#89435,1000.) ;
#14552 = VECTOR('',#89436,1000.) ;
#14553 = VECTOR('',#89439,1000.) ;
#14554 = VECTOR('',#89440,1000.) ;
#14555 = VECTOR('',#89441,1000.) ;
#14556 = VECTOR('',#89442,1000.) ;
#14557 = VECTOR('',#89669,1000.) ;
#14558 = VECTOR('',#89670,1000.) ;
#14559 = VECTOR('',#89671,1000.) ;
#14560 = VECTOR('',#89672,1000.) ;
#14561 = VECTOR('',#89673,1000.) ;
#14562 = VECTOR('',#89674,1000.) ;
#14563 = VECTOR('',#89677,1000.) ;
#14564 = VECTOR('',#89680,1000.) ;
#14565 = VECTOR('',#89683,1000.) ;
#14566 = VECTOR('',#89684,1000.) ;
#14567 = VECTOR('',#89685,1000.) ;
#14568 = VECTOR('',#89686,1000.) ;
#14569 = VECTOR('',#89687,1000.) ;
#14570 = VECTOR('',#89688,1000.) ;
#14571 = VECTOR('',#89691,1000.) ;
#14572 = VECTOR('',#89694,1000.) ;
#14573 = VECTOR('',#89697,1000.) ;
#14574 = VECTOR('',#89698,1000.) ;
#14575 = VECTOR('',#89699,1000.) ;
#14576 = VECTOR('',#89700,1000.) ;
#14577 = VECTOR('',#89701,1000.) ;
#14578 = VECTOR('',#89702,1000.) ;
#14579 = VECTOR('',#89705,1000.) ;
#14580 = VECTOR('',#89708,1000.) ;
#14581 = VECTOR('',#89711,1000.) ;
#14582 = VECTOR('',#89712,1000.) ;
#14583 = VECTOR('',#89713,1000.) ;
#14584 = VECTOR('',#89714,1000.) ;
#14585 = VECTOR('',#89715,1000.) ;
#14586 = VECTOR('',#89716,1000.) ;
#14587 = VECTOR('',#89719,1000.) ;
#14588 = VECTOR('',#89722,1000.) ;
#14589 = VECTOR('',#89725,1000.) ;
#14590 = VECTOR('',#89726,1000.) ;
#14591 = VECTOR('',#89727,1000.) ;
#14592 = VECTOR('',#89728,1000.) ;
#14593 = VECTOR('',#89729,1000.) ;
#14594 = VECTOR('',#89730,1000.) ;
#14595 = VECTOR('',#89733,1000.) ;
#14596 = VECTOR('',#89736,1000.) ;
#14597 = VECTOR('',#89739,1000.) ;
#14598 = VECTOR('',#89740,1000.) ;
#14599 = VECTOR('',#89741,1000.) ;
#14600 = VECTOR('',#89742,1000.) ;
#14601 = VECTOR('',#89743,1000.) ;
#14602 = VECTOR('',#89744,1000.) ;
#14603 = VECTOR('',#89747,1000.) ;
#14604 = VECTOR('',#89750,1000.) ;
#14605 = VECTOR('',#89753,1000.) ;
#14606 = VECTOR('',#89754,1000.) ;
#14607 = VECTOR('',#89755,1000.) ;
#14608 = VECTOR('',#89756,1000.) ;
#14609 = VECTOR('',#89757,1000.) ;
#14610 = VECTOR('',#89758,1000.) ;
#14611 = VECTOR('',#89761,1000.) ;
#14612 = VECTOR('',#89764,1000.) ;
#14613 = VECTOR('',#89767,1000.) ;
#14614 = VECTOR('',#89768,1000.) ;
#14615 = VECTOR('',#89769,1000.) ;
#14616 = VECTOR('',#89770,1000.) ;
#14617 = VECTOR('',#89771,1000.) ;
#14618 = VECTOR('',#89772,1000.) ;
#14619 = VECTOR('',#89775,1000.) ;
#14620 = VECTOR('',#89778,1000.) ;
#14621 = VECTOR('',#89781,1000.) ;
#14622 = VECTOR('',#89782,1000.) ;
#14623 = VECTOR('',#89783,1000.) ;
#14624 = VECTOR('',#89784,1000.) ;
#14625 = VECTOR('',#89785,1000.) ;
#14626 = VECTOR('',#89786,1000.) ;
#14627 = VECTOR('',#89789,1000.) ;
#14628 = VECTOR('',#89792,1000.) ;
#14629 = VECTOR('',#89795,1000.) ;
#14630 = VECTOR('',#89796,1000.) ;
#14631 = VECTOR('',#89797,1000.) ;
#14632 = VECTOR('',#89798,1000.) ;
#14633 = VECTOR('',#89801,1000.) ;
#14634 = VECTOR('',#89802,1000.) ;
#14635 = VECTOR('',#89803,1000.) ;
#14636 = VECTOR('',#89806,1000.) ;
#14637 = VECTOR('',#89807,1000.) ;
#14638 = VECTOR('',#89808,1000.) ;
#14639 = VECTOR('',#89809,1000.) ;
#14640 = VECTOR('',#89812,1000.) ;
#14641 = VECTOR('',#89813,1000.) ;
#14642 = VECTOR('',#89814,1000.) ;
#14643 = VECTOR('',#89815,1000.) ;
#14644 = VECTOR('',#89818,1000.) ;
#14645 = VECTOR('',#89819,1000.) ;
#14646 = VECTOR('',#89820,1000.) ;
#14647 = VECTOR('',#89821,1000.) ;
#14648 = VECTOR('',#89824,1000.) ;
#14649 = VECTOR('',#89825,1000.) ;
#14650 = VECTOR('',#89826,1000.) ;
#14651 = VECTOR('',#89827,1000.) ;
#14652 = VECTOR('',#89830,1000.) ;
#14653 = VECTOR('',#89831,1000.) ;
#14654 = VECTOR('',#89832,1000.) ;
#14655 = VECTOR('',#89835,1000.) ;
#14656 = VECTOR('',#89836,1000.) ;
#14657 = VECTOR('',#89837,1000.) ;
#14658 = VECTOR('',#89838,1000.) ;
#14659 = VECTOR('',#89841,1000.) ;
#14660 = VECTOR('',#89842,1000.) ;
#14661 = VECTOR('',#89843,1000.) ;
#14662 = VECTOR('',#89844,1000.) ;
#14663 = VECTOR('',#89847,1000.) ;
#14664 = VECTOR('',#89848,1000.) ;
#14665 = VECTOR('',#89849,1000.) ;
#14666 = VECTOR('',#89850,1000.) ;
#14667 = VECTOR('',#89853,1000.) ;
#14668 = VECTOR('',#89854,1000.) ;
#14669 = VECTOR('',#89855,1000.) ;
#14670 = VECTOR('',#89856,1000.) ;
#14671 = VECTOR('',#89859,1000.) ;
#14672 = VECTOR('',#89860,1000.) ;
#14673 = VECTOR('',#89861,1000.) ;
#14674 = VECTOR('',#89864,1000.) ;
#14675 = VECTOR('',#89865,1000.) ;
#14676 = VECTOR('',#89866,1000.) ;
#14677 = VECTOR('',#89867,1000.) ;
#14678 = VECTOR('',#89870,1000.) ;
#14679 = VECTOR('',#89871,1000.) ;
#14680 = VECTOR('',#89872,1000.) ;
#14681 = VECTOR('',#89873,1000.) ;
#14682 = VECTOR('',#89876,1000.) ;
#14683 = VECTOR('',#89877,1000.) ;
#14684 = VECTOR('',#89878,1000.) ;
#14685 = VECTOR('',#89879,1000.) ;
#14686 = VECTOR('',#89882,1000.) ;
#14687 = VECTOR('',#89883,1000.) ;
#14688 = VECTOR('',#89884,1000.) ;
#14689 = VECTOR('',#89885,1000.) ;
#14690 = VECTOR('',#89888,1000.) ;
#14691 = VECTOR('',#89889,1000.) ;
#14692 = VECTOR('',#89890,1000.) ;
#14693 = VECTOR('',#89893,1000.) ;
#14694 = VECTOR('',#89894,1000.) ;
#14695 = VECTOR('',#89895,1000.) ;
#14696 = VECTOR('',#89896,1000.) ;
#14697 = VECTOR('',#89899,1000.) ;
#14698 = VECTOR('',#89900,1000.) ;
#14699 = VECTOR('',#89901,1000.) ;
#14700 = VECTOR('',#89902,1000.) ;
#14701 = VECTOR('',#89905,1000.) ;
#14702 = VECTOR('',#89906,1000.) ;
#14703 = VECTOR('',#89907,1000.) ;
#14704 = VECTOR('',#89908,1000.) ;
#14705 = VECTOR('',#89911,1000.) ;
#14706 = VECTOR('',#89912,1000.) ;
#14707 = VECTOR('',#89913,1000.) ;
#14708 = VECTOR('',#89914,1000.) ;
#14709 = VECTOR('',#89917,1000.) ;
#14710 = VECTOR('',#89918,1000.) ;
#14711 = VECTOR('',#89919,1000.) ;
#14712 = VECTOR('',#89922,1000.) ;
#14713 = VECTOR('',#89923,1000.) ;
#14714 = VECTOR('',#89924,1000.) ;
#14715 = VECTOR('',#89925,1000.) ;
#14716 = VECTOR('',#89928,1000.) ;
#14717 = VECTOR('',#89929,1000.) ;
#14718 = VECTOR('',#89930,1000.) ;
#14719 = VECTOR('',#89931,1000.) ;
#14720 = VECTOR('',#89934,1000.) ;
#14721 = VECTOR('',#89935,1000.) ;
#14722 = VECTOR('',#89936,1000.) ;
#14723 = VECTOR('',#89937,1000.) ;
#14724 = VECTOR('',#89940,1000.) ;
#14725 = VECTOR('',#89941,1000.) ;
#14726 = VECTOR('',#89942,1000.) ;
#14727 = VECTOR('',#89943,1000.) ;
#14728 = VECTOR('',#89946,1000.) ;
#14729 = VECTOR('',#89947,1000.) ;
#14730 = VECTOR('',#89948,1000.) ;
#14731 = VECTOR('',#89951,1000.) ;
#14732 = VECTOR('',#89952,1000.) ;
#14733 = VECTOR('',#89953,1000.) ;
#14734 = VECTOR('',#89954,1000.) ;
#14735 = VECTOR('',#89957,1000.) ;
#14736 = VECTOR('',#89958,1000.) ;
#14737 = VECTOR('',#89959,1000.) ;
#14738 = VECTOR('',#89960,1000.) ;
#14739 = VECTOR('',#89963,1000.) ;
#14740 = VECTOR('',#89964,1000.) ;
#14741 = VECTOR('',#89965,1000.) ;
#14742 = VECTOR('',#89966,1000.) ;
#14743 = VECTOR('',#89969,1000.) ;
#14744 = VECTOR('',#89970,1000.) ;
#14745 = VECTOR('',#89971,1000.) ;
#14746 = VECTOR('',#89972,1000.) ;
#14747 = VECTOR('',#89975,1000.) ;
#14748 = VECTOR('',#89976,1000.) ;
#14749 = VECTOR('',#89977,1000.) ;
#14750 = VECTOR('',#89980,1000.) ;
#14751 = VECTOR('',#89981,1000.) ;
#14752 = VECTOR('',#89982,1000.) ;
#14753 = VECTOR('',#89983,1000.) ;
#14754 = VECTOR('',#89986,1000.) ;
#14755 = VECTOR('',#89987,1000.) ;
#14756 = VECTOR('',#89988,1000.) ;
#14757 = VECTOR('',#89989,1000.) ;
#14758 = VECTOR('',#89992,1000.) ;
#14759 = VECTOR('',#89993,1000.) ;
#14760 = VECTOR('',#89994,1000.) ;
#14761 = VECTOR('',#89995,1000.) ;
#14762 = VECTOR('',#89998,1000.) ;
#14763 = VECTOR('',#89999,1000.) ;
#14764 = VECTOR('',#90000,1000.) ;
#14765 = VECTOR('',#90001,1000.) ;
#14766 = VECTOR('',#90004,1000.) ;
#14767 = VECTOR('',#90005,1000.) ;
#14768 = VECTOR('',#90006,1000.) ;
#14769 = VECTOR('',#90009,1000.) ;
#14770 = VECTOR('',#90010,1000.) ;
#14771 = VECTOR('',#90011,1000.) ;
#14772 = VECTOR('',#90012,1000.) ;
#14773 = VECTOR('',#90015,1000.) ;
#14774 = VECTOR('',#90016,1000.) ;
#14775 = VECTOR('',#90017,1000.) ;
#14776 = VECTOR('',#90018,1000.) ;
#14777 = VECTOR('',#90021,1000.) ;
#14778 = VECTOR('',#90022,1000.) ;
#14779 = VECTOR('',#90023,1000.) ;
#14780 = VECTOR('',#90024,1000.) ;
#14781 = VECTOR('',#90027,1000.) ;
#14782 = VECTOR('',#90028,1000.) ;
#14783 = VECTOR('',#90029,1000.) ;
#14784 = VECTOR('',#90030,1000.) ;
#14785 = VECTOR('',#90033,1000.) ;
#14786 = VECTOR('',#90034,1000.) ;
#14787 = VECTOR('',#90035,1000.) ;
#14788 = VECTOR('',#90038,1000.) ;
#14789 = VECTOR('',#90039,1000.) ;
#14790 = VECTOR('',#90040,1000.) ;
#14791 = VECTOR('',#90041,1000.) ;
#14792 = VECTOR('',#90044,1000.) ;
#14793 = VECTOR('',#90045,1000.) ;
#14794 = VECTOR('',#90046,1000.) ;
#14795 = VECTOR('',#90047,1000.) ;
#14796 = VECTOR('',#90050,1000.) ;
#14797 = VECTOR('',#90051,1000.) ;
#14798 = VECTOR('',#90052,1000.) ;
#14799 = VECTOR('',#90053,1000.) ;
#14800 = VECTOR('',#90056,1000.) ;
#14801 = VECTOR('',#90059,1000.) ;
#14802 = VECTOR('',#90064,1000.) ;
#14803 = VECTOR('',#90065,1000.) ;
#14804 = VECTOR('',#90066,1000.) ;
#14805 = VECTOR('',#90071,1000.) ;
#14806 = VECTOR('',#90076,1000.) ;
#14807 = VECTOR('',#90077,1000.) ;
#14808 = VECTOR('',#90078,1000.) ;
#14809 = VECTOR('',#90083,1000.) ;
#14810 = VECTOR('',#90088,1000.) ;
#14811 = VECTOR('',#90089,1000.) ;
#14812 = VECTOR('',#90090,1000.) ;
#14813 = VECTOR('',#90093,1000.) ;
#14814 = VECTOR('',#90098,1000.) ;
#14815 = VECTOR('',#90099,1000.) ;
#14816 = VECTOR('',#90102,1000.) ;
#14817 = VECTOR('',#90103,1000.) ;
#14818 = VECTOR('',#90104,1000.) ;
#14819 = VECTOR('',#90109,1000.) ;
#14820 = VECTOR('',#90114,1000.) ;
#14821 = VECTOR('',#90115,1000.) ;
#14822 = VECTOR('',#90116,1000.) ;
#14823 = VECTOR('',#90121,1000.) ;
#14824 = VECTOR('',#90126,1000.) ;
#14825 = VECTOR('',#90127,1000.) ;
#14826 = VECTOR('',#90128,1000.) ;
#14827 = VECTOR('',#90133,1000.) ;
#14828 = VECTOR('',#90138,1000.) ;
#14829 = VECTOR('',#90139,1000.) ;
#14830 = VECTOR('',#90140,1000.) ;
#14831 = VECTOR('',#90145,1000.) ;
#14832 = VECTOR('',#90150,1000.) ;
#14833 = VECTOR('',#90151,1000.) ;
#14834 = VECTOR('',#90152,1000.) ;
#14835 = VECTOR('',#90157,1000.) ;
#14836 = VECTOR('',#90162,1000.) ;
#14837 = VECTOR('',#90163,1000.) ;
#14838 = VECTOR('',#90164,1000.) ;
#14839 = VECTOR('',#90169,1000.) ;
#14840 = VECTOR('',#90176,1000.) ;
#14841 = VECTOR('',#90183,1000.) ;
#14842 = VECTOR('',#90188,1000.) ;
#14843 = VECTOR('',#90189,1000.) ;
#14844 = VECTOR('',#90190,1000.) ;
#14845 = VECTOR('',#90195,1000.) ;
#14846 = VECTOR('',#90200,1000.) ;
#14847 = VECTOR('',#90201,1000.) ;
#14848 = VECTOR('',#90202,1000.) ;
#14849 = VECTOR('',#90207,1000.) ;
#14850 = VECTOR('',#90212,1000.) ;
#14851 = VECTOR('',#90213,1000.) ;
#14852 = VECTOR('',#90218,1000.) ;
#14853 = VECTOR('',#90221,1000.) ;
#14854 = VECTOR('',#90222,1000.) ;
#14855 = VECTOR('',#90223,1000.) ;
#14856 = VECTOR('',#90226,1000.) ;
#14857 = VECTOR('',#90227,1000.) ;
#14858 = VECTOR('',#90228,1000.) ;
#14859 = VECTOR('',#90231,1000.) ;
#14860 = VECTOR('',#90234,1000.) ;
#14861 = VECTOR('',#90235,1000.) ;
#14862 = VECTOR('',#90236,1000.) ;
#14863 = VECTOR('',#90237,1000.) ;
#14864 = VECTOR('',#90238,1000.) ;
#14865 = VECTOR('',#90241,1000.) ;
#14866 = VECTOR('',#90244,1000.) ;
#14867 = VECTOR('',#90249,1000.) ;
#14868 = VECTOR('',#90250,1000.) ;
#14869 = VECTOR('',#90251,1000.) ;
#14870 = VECTOR('',#90256,1000.) ;
#14871 = VECTOR('',#90261,1000.) ;
#14872 = VECTOR('',#90262,1000.) ;
#14873 = VECTOR('',#90263,1000.) ;
#14874 = VECTOR('',#90268,1000.) ;
#14875 = VECTOR('',#90273,1000.) ;
#14876 = VECTOR('',#90274,1000.) ;
#14877 = VECTOR('',#90275,1000.) ;
#14878 = VECTOR('',#90278,1000.) ;
#14879 = VECTOR('',#90283,1000.) ;
#14880 = VECTOR('',#90284,1000.) ;
#14881 = VECTOR('',#90287,1000.) ;
#14882 = VECTOR('',#90288,1000.) ;
#14883 = VECTOR('',#90289,1000.) ;
#14884 = VECTOR('',#90294,1000.) ;
#14885 = VECTOR('',#90299,1000.) ;
#14886 = VECTOR('',#90300,1000.) ;
#14887 = VECTOR('',#90301,1000.) ;
#14888 = VECTOR('',#90306,1000.) ;
#14889 = VECTOR('',#90311,1000.) ;
#14890 = VECTOR('',#90312,1000.) ;
#14891 = VECTOR('',#90313,1000.) ;
#14892 = VECTOR('',#90318,1000.) ;
#14893 = VECTOR('',#90323,1000.) ;
#14894 = VECTOR('',#90324,1000.) ;
#14895 = VECTOR('',#90325,1000.) ;
#14896 = VECTOR('',#90330,1000.) ;
#14897 = VECTOR('',#90335,1000.) ;
#14898 = VECTOR('',#90336,1000.) ;
#14899 = VECTOR('',#90337,1000.) ;
#14900 = VECTOR('',#90342,1000.) ;
#14901 = VECTOR('',#90347,1000.) ;
#14902 = VECTOR('',#90348,1000.) ;
#14903 = VECTOR('',#90349,1000.) ;
#14904 = VECTOR('',#90354,1000.) ;
#14905 = VECTOR('',#90361,1000.) ;
#14906 = VECTOR('',#90368,1000.) ;
#14907 = VECTOR('',#90373,1000.) ;
#14908 = VECTOR('',#90374,1000.) ;
#14909 = VECTOR('',#90375,1000.) ;
#14910 = VECTOR('',#90380,1000.) ;
#14911 = VECTOR('',#90385,1000.) ;
#14912 = VECTOR('',#90386,1000.) ;
#14913 = VECTOR('',#90387,1000.) ;
#14914 = VECTOR('',#90392,1000.) ;
#14915 = VECTOR('',#90397,1000.) ;
#14916 = VECTOR('',#90398,1000.) ;
#14917 = VECTOR('',#90403,1000.) ;
#14918 = VECTOR('',#90406,1000.) ;
#14919 = VECTOR('',#90407,1000.) ;
#14920 = VECTOR('',#90408,1000.) ;
#14921 = VECTOR('',#90411,1000.) ;
#14922 = VECTOR('',#90412,1000.) ;
#14923 = VECTOR('',#90413,1000.) ;
#14924 = VECTOR('',#90416,1000.) ;
#14925 = VECTOR('',#90419,1000.) ;
#14926 = VECTOR('',#90420,1000.) ;
#14927 = VECTOR('',#90421,1000.) ;
#14928 = VECTOR('',#90422,1000.) ;
#14929 = VECTOR('',#90423,1000.) ;
#14930 = VECTOR('',#90426,1000.) ;
#14931 = VECTOR('',#90429,1000.) ;
#14932 = VECTOR('',#90434,1000.) ;
#14933 = VECTOR('',#90435,1000.) ;
#14934 = VECTOR('',#90436,1000.) ;
#14935 = VECTOR('',#90441,1000.) ;
#14936 = VECTOR('',#90446,1000.) ;
#14937 = VECTOR('',#90447,1000.) ;
#14938 = VECTOR('',#90448,1000.) ;
#14939 = VECTOR('',#90453,1000.) ;
#14940 = VECTOR('',#90458,1000.) ;
#14941 = VECTOR('',#90459,1000.) ;
#14942 = VECTOR('',#90460,1000.) ;
#14943 = VECTOR('',#90463,1000.) ;
#14944 = VECTOR('',#90468,1000.) ;
#14945 = VECTOR('',#90469,1000.) ;
#14946 = VECTOR('',#90472,1000.) ;
#14947 = VECTOR('',#90473,1000.) ;
#14948 = VECTOR('',#90474,1000.) ;
#14949 = VECTOR('',#90479,1000.) ;
#14950 = VECTOR('',#90484,1000.) ;
#14951 = VECTOR('',#90485,1000.) ;
#14952 = VECTOR('',#90486,1000.) ;
#14953 = VECTOR('',#90491,1000.) ;
#14954 = VECTOR('',#90496,1000.) ;
#14955 = VECTOR('',#90497,1000.) ;
#14956 = VECTOR('',#90498,1000.) ;
#14957 = VECTOR('',#90503,1000.) ;
#14958 = VECTOR('',#90508,1000.) ;
#14959 = VECTOR('',#90509,1000.) ;
#14960 = VECTOR('',#90510,1000.) ;
#14961 = VECTOR('',#90515,1000.) ;
#14962 = VECTOR('',#90520,1000.) ;
#14963 = VECTOR('',#90521,1000.) ;
#14964 = VECTOR('',#90522,1000.) ;
#14965 = VECTOR('',#90527,1000.) ;
#14966 = VECTOR('',#90532,1000.) ;
#14967 = VECTOR('',#90533,1000.) ;
#14968 = VECTOR('',#90534,1000.) ;
#14969 = VECTOR('',#90539,1000.) ;
#14970 = VECTOR('',#90546,1000.) ;
#14971 = VECTOR('',#90553,1000.) ;
#14972 = VECTOR('',#90558,1000.) ;
#14973 = VECTOR('',#90559,1000.) ;
#14974 = VECTOR('',#90560,1000.) ;
#14975 = VECTOR('',#90565,1000.) ;
#14976 = VECTOR('',#90570,1000.) ;
#14977 = VECTOR('',#90571,1000.) ;
#14978 = VECTOR('',#90572,1000.) ;
#14979 = VECTOR('',#90577,1000.) ;
#14980 = VECTOR('',#90582,1000.) ;
#14981 = VECTOR('',#90583,1000.) ;
#14982 = VECTOR('',#90588,1000.) ;
#14983 = VECTOR('',#90591,1000.) ;
#14984 = VECTOR('',#90592,1000.) ;
#14985 = VECTOR('',#90593,1000.) ;
#14986 = VECTOR('',#90596,1000.) ;
#14987 = VECTOR('',#90597,1000.) ;
#14988 = VECTOR('',#90598,1000.) ;
#14989 = VECTOR('',#90601,1000.) ;
#14990 = VECTOR('',#90604,1000.) ;
#14991 = VECTOR('',#90605,1000.) ;
#14992 = VECTOR('',#90606,1000.) ;
#14993 = VECTOR('',#90607,1000.) ;
#14994 = VECTOR('',#90608,1000.) ;
#14995 = VECTOR('',#90611,1000.) ;
#14996 = VECTOR('',#90614,1000.) ;
#14997 = VECTOR('',#90619,1000.) ;
#14998 = VECTOR('',#90620,1000.) ;
#14999 = VECTOR('',#90621,1000.) ;
#15000 = VECTOR('',#90626,1000.) ;
#15001 = VECTOR('',#90631,1000.) ;
#15002 = VECTOR('',#90632,1000.) ;
#15003 = VECTOR('',#90633,1000.) ;
#15004 = VECTOR('',#90638,1000.) ;
#15005 = VECTOR('',#90643,1000.) ;
#15006 = VECTOR('',#90644,1000.) ;
#15007 = VECTOR('',#90645,1000.) ;
#15008 = VECTOR('',#90648,1000.) ;
#15009 = VECTOR('',#90653,1000.) ;
#15010 = VECTOR('',#90654,1000.) ;
#15011 = VECTOR('',#90657,1000.) ;
#15012 = VECTOR('',#90658,1000.) ;
#15013 = VECTOR('',#90659,1000.) ;
#15014 = VECTOR('',#90664,1000.) ;
#15015 = VECTOR('',#90669,1000.) ;
#15016 = VECTOR('',#90670,1000.) ;
#15017 = VECTOR('',#90671,1000.) ;
#15018 = VECTOR('',#90676,1000.) ;
#15019 = VECTOR('',#90681,1000.) ;
#15020 = VECTOR('',#90682,1000.) ;
#15021 = VECTOR('',#90683,1000.) ;
#15022 = VECTOR('',#90688,1000.) ;
#15023 = VECTOR('',#90693,1000.) ;
#15024 = VECTOR('',#90694,1000.) ;
#15025 = VECTOR('',#90695,1000.) ;
#15026 = VECTOR('',#90700,1000.) ;
#15027 = VECTOR('',#90705,1000.) ;
#15028 = VECTOR('',#90706,1000.) ;
#15029 = VECTOR('',#90707,1000.) ;
#15030 = VECTOR('',#90712,1000.) ;
#15031 = VECTOR('',#90717,1000.) ;
#15032 = VECTOR('',#90718,1000.) ;
#15033 = VECTOR('',#90719,1000.) ;
#15034 = VECTOR('',#90724,1000.) ;
#15035 = VECTOR('',#90731,1000.) ;
#15036 = VECTOR('',#90738,1000.) ;
#15037 = VECTOR('',#90743,1000.) ;
#15038 = VECTOR('',#90744,1000.) ;
#15039 = VECTOR('',#90745,1000.) ;
#15040 = VECTOR('',#90750,1000.) ;
#15041 = VECTOR('',#90755,1000.) ;
#15042 = VECTOR('',#90756,1000.) ;
#15043 = VECTOR('',#90757,1000.) ;
#15044 = VECTOR('',#90762,1000.) ;
#15045 = VECTOR('',#90767,1000.) ;
#15046 = VECTOR('',#90768,1000.) ;
#15047 = VECTOR('',#90773,1000.) ;
#15048 = VECTOR('',#90776,1000.) ;
#15049 = VECTOR('',#90777,1000.) ;
#15050 = VECTOR('',#90778,1000.) ;
#15051 = VECTOR('',#90781,1000.) ;
#15052 = VECTOR('',#90782,1000.) ;
#15053 = VECTOR('',#90783,1000.) ;
#15054 = VECTOR('',#90786,1000.) ;
#15055 = VECTOR('',#90789,1000.) ;
#15056 = VECTOR('',#90790,1000.) ;
#15057 = VECTOR('',#90791,1000.) ;
#15058 = VECTOR('',#90792,1000.) ;
#15059 = VECTOR('',#90793,1000.) ;
#15060 = VECTOR('',#90796,1000.) ;
#15061 = VECTOR('',#90799,1000.) ;
#15062 = VECTOR('',#90804,1000.) ;
#15063 = VECTOR('',#90805,1000.) ;
#15064 = VECTOR('',#90806,1000.) ;
#15065 = VECTOR('',#90811,1000.) ;
#15066 = VECTOR('',#90816,1000.) ;
#15067 = VECTOR('',#90817,1000.) ;
#15068 = VECTOR('',#90818,1000.) ;
#15069 = VECTOR('',#90823,1000.) ;
#15070 = VECTOR('',#90828,1000.) ;
#15071 = VECTOR('',#90829,1000.) ;
#15072 = VECTOR('',#90830,1000.) ;
#15073 = VECTOR('',#90833,1000.) ;
#15074 = VECTOR('',#90838,1000.) ;
#15075 = VECTOR('',#90839,1000.) ;
#15076 = VECTOR('',#90842,1000.) ;
#15077 = VECTOR('',#90843,1000.) ;
#15078 = VECTOR('',#90844,1000.) ;
#15079 = VECTOR('',#90849,1000.) ;
#15080 = VECTOR('',#90854,1000.) ;
#15081 = VECTOR('',#90855,1000.) ;
#15082 = VECTOR('',#90856,1000.) ;
#15083 = VECTOR('',#90861,1000.) ;
#15084 = VECTOR('',#90866,1000.) ;
#15085 = VECTOR('',#90867,1000.) ;
#15086 = VECTOR('',#90868,1000.) ;
#15087 = VECTOR('',#90873,1000.) ;
#15088 = VECTOR('',#90878,1000.) ;
#15089 = VECTOR('',#90879,1000.) ;
#15090 = VECTOR('',#90880,1000.) ;
#15091 = VECTOR('',#90885,1000.) ;
#15092 = VECTOR('',#90890,1000.) ;
#15093 = VECTOR('',#90891,1000.) ;
#15094 = VECTOR('',#90892,1000.) ;
#15095 = VECTOR('',#90897,1000.) ;
#15096 = VECTOR('',#90902,1000.) ;
#15097 = VECTOR('',#90903,1000.) ;
#15098 = VECTOR('',#90904,1000.) ;
#15099 = VECTOR('',#90909,1000.) ;
#15100 = VECTOR('',#90916,1000.) ;
#15101 = VECTOR('',#90923,1000.) ;
#15102 = VECTOR('',#90928,1000.) ;
#15103 = VECTOR('',#90929,1000.) ;
#15104 = VECTOR('',#90930,1000.) ;
#15105 = VECTOR('',#90935,1000.) ;
#15106 = VECTOR('',#90940,1000.) ;
#15107 = VECTOR('',#90941,1000.) ;
#15108 = VECTOR('',#90942,1000.) ;
#15109 = VECTOR('',#90947,1000.) ;
#15110 = VECTOR('',#90952,1000.) ;
#15111 = VECTOR('',#90953,1000.) ;
#15112 = VECTOR('',#90958,1000.) ;
#15113 = VECTOR('',#90961,1000.) ;
#15114 = VECTOR('',#90962,1000.) ;
#15115 = VECTOR('',#90963,1000.) ;
#15116 = VECTOR('',#90966,1000.) ;
#15117 = VECTOR('',#90967,1000.) ;
#15118 = VECTOR('',#90968,1000.) ;
#15119 = VECTOR('',#90971,1000.) ;
#15120 = VECTOR('',#90974,1000.) ;
#15121 = VECTOR('',#90975,1000.) ;
#15122 = VECTOR('',#90976,1000.) ;
#15123 = VECTOR('',#90977,1000.) ;
#15124 = VECTOR('',#90978,1000.) ;
#15125 = VECTOR('',#90981,1000.) ;
#15126 = VECTOR('',#90984,1000.) ;
#15127 = VECTOR('',#90989,1000.) ;
#15128 = VECTOR('',#90990,1000.) ;
#15129 = VECTOR('',#90991,1000.) ;
#15130 = VECTOR('',#90996,1000.) ;
#15131 = VECTOR('',#91001,1000.) ;
#15132 = VECTOR('',#91002,1000.) ;
#15133 = VECTOR('',#91003,1000.) ;
#15134 = VECTOR('',#91008,1000.) ;
#15135 = VECTOR('',#91013,1000.) ;
#15136 = VECTOR('',#91014,1000.) ;
#15137 = VECTOR('',#91015,1000.) ;
#15138 = VECTOR('',#91018,1000.) ;
#15139 = VECTOR('',#91023,1000.) ;
#15140 = VECTOR('',#91024,1000.) ;
#15141 = VECTOR('',#91027,1000.) ;
#15142 = VECTOR('',#91028,1000.) ;
#15143 = VECTOR('',#91029,1000.) ;
#15144 = VECTOR('',#91034,1000.) ;
#15145 = VECTOR('',#91039,1000.) ;
#15146 = VECTOR('',#91040,1000.) ;
#15147 = VECTOR('',#91041,1000.) ;
#15148 = VECTOR('',#91046,1000.) ;
#15149 = VECTOR('',#91051,1000.) ;
#15150 = VECTOR('',#91052,1000.) ;
#15151 = VECTOR('',#91053,1000.) ;
#15152 = VECTOR('',#91058,1000.) ;
#15153 = VECTOR('',#91063,1000.) ;
#15154 = VECTOR('',#91064,1000.) ;
#15155 = VECTOR('',#91065,1000.) ;
#15156 = VECTOR('',#91070,1000.) ;
#15157 = VECTOR('',#91075,1000.) ;
#15158 = VECTOR('',#91076,1000.) ;
#15159 = VECTOR('',#91077,1000.) ;
#15160 = VECTOR('',#91082,1000.) ;
#15161 = VECTOR('',#91087,1000.) ;
#15162 = VECTOR('',#91088,1000.) ;
#15163 = VECTOR('',#91089,1000.) ;
#15164 = VECTOR('',#91094,1000.) ;
#15165 = VECTOR('',#91101,1000.) ;
#15166 = VECTOR('',#91108,1000.) ;
#15167 = VECTOR('',#91113,1000.) ;
#15168 = VECTOR('',#91114,1000.) ;
#15169 = VECTOR('',#91115,1000.) ;
#15170 = VECTOR('',#91120,1000.) ;
#15171 = VECTOR('',#91125,1000.) ;
#15172 = VECTOR('',#91126,1000.) ;
#15173 = VECTOR('',#91127,1000.) ;
#15174 = VECTOR('',#91132,1000.) ;
#15175 = VECTOR('',#91137,1000.) ;
#15176 = VECTOR('',#91138,1000.) ;
#15177 = VECTOR('',#91143,1000.) ;
#15178 = VECTOR('',#91146,1000.) ;
#15179 = VECTOR('',#91147,1000.) ;
#15180 = VECTOR('',#91148,1000.) ;
#15181 = VECTOR('',#91151,1000.) ;
#15182 = VECTOR('',#91152,1000.) ;
#15183 = VECTOR('',#91153,1000.) ;
#15184 = VECTOR('',#91156,1000.) ;
#15185 = VECTOR('',#91159,1000.) ;
#15186 = VECTOR('',#91160,1000.) ;
#15187 = VECTOR('',#91161,1000.) ;
#15188 = VECTOR('',#91162,1000.) ;
#15189 = VECTOR('',#91163,1000.) ;
#15190 = VECTOR('',#91166,1000.) ;
#15191 = VECTOR('',#91169,1000.) ;
#15192 = VECTOR('',#91174,1000.) ;
#15193 = VECTOR('',#91175,1000.) ;
#15194 = VECTOR('',#91176,1000.) ;
#15195 = VECTOR('',#91181,1000.) ;
#15196 = VECTOR('',#91186,1000.) ;
#15197 = VECTOR('',#91187,1000.) ;
#15198 = VECTOR('',#91188,1000.) ;
#15199 = VECTOR('',#91193,1000.) ;
#15200 = VECTOR('',#91198,1000.) ;
#15201 = VECTOR('',#91199,1000.) ;
#15202 = VECTOR('',#91200,1000.) ;
#15203 = VECTOR('',#91203,1000.) ;
#15204 = VECTOR('',#91208,1000.) ;
#15205 = VECTOR('',#91209,1000.) ;
#15206 = VECTOR('',#91212,1000.) ;
#15207 = VECTOR('',#91213,1000.) ;
#15208 = VECTOR('',#91214,1000.) ;
#15209 = VECTOR('',#91219,1000.) ;
#15210 = VECTOR('',#91224,1000.) ;
#15211 = VECTOR('',#91225,1000.) ;
#15212 = VECTOR('',#91226,1000.) ;
#15213 = VECTOR('',#91231,1000.) ;
#15214 = VECTOR('',#91236,1000.) ;
#15215 = VECTOR('',#91237,1000.) ;
#15216 = VECTOR('',#91238,1000.) ;
#15217 = VECTOR('',#91243,1000.) ;
#15218 = VECTOR('',#91248,1000.) ;
#15219 = VECTOR('',#91249,1000.) ;
#15220 = VECTOR('',#91250,1000.) ;
#15221 = VECTOR('',#91255,1000.) ;
#15222 = VECTOR('',#91260,1000.) ;
#15223 = VECTOR('',#91261,1000.) ;
#15224 = VECTOR('',#91262,1000.) ;
#15225 = VECTOR('',#91267,1000.) ;
#15226 = VECTOR('',#91272,1000.) ;
#15227 = VECTOR('',#91273,1000.) ;
#15228 = VECTOR('',#91274,1000.) ;
#15229 = VECTOR('',#91279,1000.) ;
#15230 = VECTOR('',#91286,1000.) ;
#15231 = VECTOR('',#91293,1000.) ;
#15232 = VECTOR('',#91298,1000.) ;
#15233 = VECTOR('',#91299,1000.) ;
#15234 = VECTOR('',#91300,1000.) ;
#15235 = VECTOR('',#91305,1000.) ;
#15236 = VECTOR('',#91310,1000.) ;
#15237 = VECTOR('',#91311,1000.) ;
#15238 = VECTOR('',#91312,1000.) ;
#15239 = VECTOR('',#91317,1000.) ;
#15240 = VECTOR('',#91322,1000.) ;
#15241 = VECTOR('',#91323,1000.) ;
#15242 = VECTOR('',#91328,1000.) ;
#15243 = VECTOR('',#91331,1000.) ;
#15244 = VECTOR('',#91332,1000.) ;
#15245 = VECTOR('',#91333,1000.) ;
#15246 = VECTOR('',#91336,1000.) ;
#15247 = VECTOR('',#91337,1000.) ;
#15248 = VECTOR('',#91338,1000.) ;
#15249 = VECTOR('',#91341,1000.) ;
#15250 = VECTOR('',#91344,1000.) ;
#15251 = VECTOR('',#91345,1000.) ;
#15252 = VECTOR('',#91346,1000.) ;
#15253 = VECTOR('',#91347,1000.) ;
#15254 = VECTOR('',#91348,1000.) ;
#15255 = VECTOR('',#91351,1000.) ;
#15256 = VECTOR('',#91354,1000.) ;
#15257 = VECTOR('',#91359,1000.) ;
#15258 = VECTOR('',#91360,1000.) ;
#15259 = VECTOR('',#91361,1000.) ;
#15260 = VECTOR('',#91366,1000.) ;
#15261 = VECTOR('',#91371,1000.) ;
#15262 = VECTOR('',#91372,1000.) ;
#15263 = VECTOR('',#91373,1000.) ;
#15264 = VECTOR('',#91378,1000.) ;
#15265 = VECTOR('',#91383,1000.) ;
#15266 = VECTOR('',#91384,1000.) ;
#15267 = VECTOR('',#91385,1000.) ;
#15268 = VECTOR('',#91388,1000.) ;
#15269 = VECTOR('',#91393,1000.) ;
#15270 = VECTOR('',#91394,1000.) ;
#15271 = VECTOR('',#91397,1000.) ;
#15272 = VECTOR('',#91398,1000.) ;
#15273 = VECTOR('',#91399,1000.) ;
#15274 = VECTOR('',#91404,1000.) ;
#15275 = VECTOR('',#91409,1000.) ;
#15276 = VECTOR('',#91410,1000.) ;
#15277 = VECTOR('',#91411,1000.) ;
#15278 = VECTOR('',#91416,1000.) ;
#15279 = VECTOR('',#91421,1000.) ;
#15280 = VECTOR('',#91422,1000.) ;
#15281 = VECTOR('',#91423,1000.) ;
#15282 = VECTOR('',#91428,1000.) ;
#15283 = VECTOR('',#91433,1000.) ;
#15284 = VECTOR('',#91434,1000.) ;
#15285 = VECTOR('',#91435,1000.) ;
#15286 = VECTOR('',#91440,1000.) ;
#15287 = VECTOR('',#91445,1000.) ;
#15288 = VECTOR('',#91446,1000.) ;
#15289 = VECTOR('',#91447,1000.) ;
#15290 = VECTOR('',#91452,1000.) ;
#15291 = VECTOR('',#91457,1000.) ;
#15292 = VECTOR('',#91458,1000.) ;
#15293 = VECTOR('',#91459,1000.) ;
#15294 = VECTOR('',#91464,1000.) ;
#15295 = VECTOR('',#91471,1000.) ;
#15296 = VECTOR('',#91478,1000.) ;
#15297 = VECTOR('',#91483,1000.) ;
#15298 = VECTOR('',#91484,1000.) ;
#15299 = VECTOR('',#91485,1000.) ;
#15300 = VECTOR('',#91490,1000.) ;
#15301 = VECTOR('',#91495,1000.) ;
#15302 = VECTOR('',#91496,1000.) ;
#15303 = VECTOR('',#91497,1000.) ;
#15304 = VECTOR('',#91502,1000.) ;
#15305 = VECTOR('',#91507,1000.) ;
#15306 = VECTOR('',#91508,1000.) ;
#15307 = VECTOR('',#91513,1000.) ;
#15308 = VECTOR('',#91516,1000.) ;
#15309 = VECTOR('',#91517,1000.) ;
#15310 = VECTOR('',#91518,1000.) ;
#15311 = VECTOR('',#91521,1000.) ;
#15312 = VECTOR('',#91522,1000.) ;
#15313 = VECTOR('',#91523,1000.) ;
#15314 = VECTOR('',#91526,1000.) ;
#15315 = VECTOR('',#91529,1000.) ;
#15316 = VECTOR('',#91530,1000.) ;
#15317 = VECTOR('',#91531,1000.) ;
#15318 = VECTOR('',#91532,1000.) ;
#15319 = VECTOR('',#91533,1000.) ;
#15320 = VECTOR('',#91536,1000.) ;
#15321 = VECTOR('',#91539,1000.) ;
#15322 = VECTOR('',#91544,1000.) ;
#15323 = VECTOR('',#91545,1000.) ;
#15324 = VECTOR('',#91546,1000.) ;
#15325 = VECTOR('',#91551,1000.) ;
#15326 = VECTOR('',#91556,1000.) ;
#15327 = VECTOR('',#91557,1000.) ;
#15328 = VECTOR('',#91558,1000.) ;
#15329 = VECTOR('',#91563,1000.) ;
#15330 = VECTOR('',#91568,1000.) ;
#15331 = VECTOR('',#91569,1000.) ;
#15332 = VECTOR('',#91570,1000.) ;
#15333 = VECTOR('',#91573,1000.) ;
#15334 = VECTOR('',#91578,1000.) ;
#15335 = VECTOR('',#91579,1000.) ;
#15336 = VECTOR('',#91582,1000.) ;
#15337 = VECTOR('',#91583,1000.) ;
#15338 = VECTOR('',#91584,1000.) ;
#15339 = VECTOR('',#91589,1000.) ;
#15340 = VECTOR('',#91594,1000.) ;
#15341 = VECTOR('',#91595,1000.) ;
#15342 = VECTOR('',#91596,1000.) ;
#15343 = VECTOR('',#91601,1000.) ;
#15344 = VECTOR('',#91606,1000.) ;
#15345 = VECTOR('',#91607,1000.) ;
#15346 = VECTOR('',#91608,1000.) ;
#15347 = VECTOR('',#91613,1000.) ;
#15348 = VECTOR('',#91618,1000.) ;
#15349 = VECTOR('',#91619,1000.) ;
#15350 = VECTOR('',#91620,1000.) ;
#15351 = VECTOR('',#91625,1000.) ;
#15352 = VECTOR('',#91630,1000.) ;
#15353 = VECTOR('',#91631,1000.) ;
#15354 = VECTOR('',#91632,1000.) ;
#15355 = VECTOR('',#91637,1000.) ;
#15356 = VECTOR('',#91642,1000.) ;
#15357 = VECTOR('',#91643,1000.) ;
#15358 = VECTOR('',#91644,1000.) ;
#15359 = VECTOR('',#91649,1000.) ;
#15360 = VECTOR('',#91656,1000.) ;
#15361 = VECTOR('',#91663,1000.) ;
#15362 = VECTOR('',#91668,1000.) ;
#15363 = VECTOR('',#91669,1000.) ;
#15364 = VECTOR('',#91670,1000.) ;
#15365 = VECTOR('',#91675,1000.) ;
#15366 = VECTOR('',#91680,1000.) ;
#15367 = VECTOR('',#91681,1000.) ;
#15368 = VECTOR('',#91682,1000.) ;
#15369 = VECTOR('',#91687,1000.) ;
#15370 = VECTOR('',#91692,1000.) ;
#15371 = VECTOR('',#91693,1000.) ;
#15372 = VECTOR('',#91698,1000.) ;
#15373 = VECTOR('',#91701,1000.) ;
#15374 = VECTOR('',#91702,1000.) ;
#15375 = VECTOR('',#91703,1000.) ;
#15376 = VECTOR('',#91706,1000.) ;
#15377 = VECTOR('',#91707,1000.) ;
#15378 = VECTOR('',#91708,1000.) ;
#15379 = VECTOR('',#91711,1000.) ;
#15380 = VECTOR('',#91714,1000.) ;
#15381 = VECTOR('',#91715,1000.) ;
#15382 = VECTOR('',#91716,1000.) ;
#15383 = VECTOR('',#91717,1000.) ;
#15384 = VECTOR('',#91718,1000.) ;
#15385 = VECTOR('',#91721,1000.) ;
#15386 = VECTOR('',#91724,1000.) ;
#15387 = VECTOR('',#91727,1000.) ;
#15388 = VECTOR('',#91730,1000.) ;
#15389 = VECTOR('',#91735,1000.) ;
#15390 = VECTOR('',#91738,1000.) ;
#15391 = VECTOR('',#91741,1000.) ;
#15392 = VECTOR('',#91744,1000.) ;
#15393 = VECTOR('',#91749,1000.) ;
#15394 = VECTOR('',#91752,1000.) ;
#15395 = VECTOR('',#91755,1000.) ;
#15396 = VECTOR('',#91758,1000.) ;
#15397 = VECTOR('',#91763,1000.) ;
#15398 = VECTOR('',#91766,1000.) ;
#15399 = VECTOR('',#91769,1000.) ;
#15400 = VECTOR('',#91772,1000.) ;
#15401 = VECTOR('',#91777,1000.) ;
#15402 = VECTOR('',#91780,1000.) ;
#15403 = VECTOR('',#91783,1000.) ;
#15404 = VECTOR('',#91786,1000.) ;
#15405 = VECTOR('',#91791,1000.) ;
#15406 = VECTOR('',#91794,1000.) ;
#15407 = VECTOR('',#91797,1000.) ;
#15408 = VECTOR('',#91800,1000.) ;
#15409 = VECTOR('',#91805,1000.) ;
#15410 = VECTOR('',#91808,1000.) ;
#15411 = VECTOR('',#91811,1000.) ;
#15412 = VECTOR('',#91814,1000.) ;
#15413 = VECTOR('',#91819,1000.) ;
#15414 = VECTOR('',#91822,1000.) ;
#15415 = VECTOR('',#91825,1000.) ;
#15416 = VECTOR('',#91828,1000.) ;
#15417 = VECTOR('',#91833,1000.) ;
#15418 = VECTOR('',#91836,1000.) ;
#15419 = VECTOR('',#91839,1000.) ;
#15420 = VECTOR('',#91842,1000.) ;
#15421 = VECTOR('',#91877,1000.) ;
#15422 = VECTOR('',#91880,1000.) ;
#15423 = VECTOR('',#91927,1000.) ;
#15424 = VECTOR('',#91986,1000.) ;
#15425 = VECTOR('',#92035,1000.) ;
#15426 = VECTOR('',#93142,1000.) ;
#15427 = VECTOR('',#93145,1000.) ;
#15428 = VECTOR('',#93192,1000.) ;
#15429 = VECTOR('',#93251,1000.) ;
#15430 = VECTOR('',#93300,1000.) ;
#15431 = VECTOR('',#93453,1000.) ;
#15432 = VECTOR('',#93456,1000.) ;
#15433 = VECTOR('',#93503,1000.) ;
#15434 = VECTOR('',#93562,1000.) ;
#15435 = VECTOR('',#93611,1000.) ;
#15436 = VECTOR('',#93764,1000.) ;
#15437 = VECTOR('',#93767,1000.) ;
#15438 = VECTOR('',#93814,1000.) ;
#15439 = VECTOR('',#93873,1000.) ;
#15440 = VECTOR('',#93922,1000.) ;
#15441 = VECTOR('',#94075,1000.) ;
#15442 = VECTOR('',#94078,1000.) ;
#15443 = VECTOR('',#94125,1000.) ;
#15444 = VECTOR('',#94184,1000.) ;
#15445 = VECTOR('',#94233,1000.) ;
#15446 = VECTOR('',#94386,1000.) ;
#15447 = VECTOR('',#94389,1000.) ;
#15448 = VECTOR('',#94436,1000.) ;
#15449 = VECTOR('',#94495,1000.) ;
#15450 = VECTOR('',#94544,1000.) ;
#15451 = VECTOR('',#94697,1000.) ;
#15452 = VECTOR('',#94700,1000.) ;
#15453 = VECTOR('',#94747,1000.) ;
#15454 = VECTOR('',#94806,1000.) ;
#15455 = VECTOR('',#94855,1000.) ;
#15456 = VECTOR('',#95008,1000.) ;
#15457 = VECTOR('',#95011,1000.) ;
#15458 = VECTOR('',#95058,1000.) ;
#15459 = VECTOR('',#95117,1000.) ;
#15460 = VECTOR('',#95166,1000.) ;
#15461 = VECTOR('',#95319,1000.) ;
#15462 = VECTOR('',#95322,1000.) ;
#15463 = VECTOR('',#95369,1000.) ;
#15464 = VECTOR('',#95428,1000.) ;
#15465 = VECTOR('',#95477,1000.) ;
#15466 = VECTOR('',#95600,1000.) ;
#15467 = VECTOR('',#95601,1000.) ;
#15468 = VECTOR('',#95602,1000.) ;
#15469 = VECTOR('',#95603,1000.) ;
#15470 = VECTOR('',#95606,1000.) ;
#15471 = VECTOR('',#95607,1000.) ;
#15472 = VECTOR('',#95608,1000.) ;
#15473 = VECTOR('',#95609,1000.) ;
#15474 = VECTOR('',#95612,1000.) ;
#15475 = VECTOR('',#95613,1000.) ;
#15476 = VECTOR('',#95614,1000.) ;
#15477 = VECTOR('',#95615,1000.) ;
#15478 = VECTOR('',#95618,1000.) ;
#15479 = VECTOR('',#95619,1000.) ;
#15480 = VECTOR('',#95620,1000.) ;
#15481 = VECTOR('',#95621,1000.) ;
#15482 = VECTOR('',#95624,1000.) ;
#15483 = VECTOR('',#95625,1000.) ;
#15484 = VECTOR('',#95626,1000.) ;
#15485 = VECTOR('',#95627,1000.) ;
#15486 = VECTOR('',#95630,1000.) ;
#15487 = VECTOR('',#95635,1000.) ;
#15488 = VECTOR('',#95636,1000.) ;
#15489 = VECTOR('',#95639,1000.) ;
#15490 = VECTOR('',#95644,1000.) ;
#15491 = VECTOR('',#95645,1000.) ;
#15492 = VECTOR('',#95660,1000.) ;
#15493 = VECTOR('',#95661,1000.) ;
#15494 = VECTOR('',#95662,1000.) ;
#15495 = VECTOR('',#95663,1000.) ;
#15496 = VECTOR('',#95666,1000.) ;
#15497 = VECTOR('',#95667,1000.) ;
#15498 = VECTOR('',#95668,1000.) ;
#15499 = VECTOR('',#95671,1000.) ;
#15500 = VECTOR('',#95672,1000.) ;
#15501 = VECTOR('',#95673,1000.) ;
#15502 = VECTOR('',#95676,1000.) ;
#15503 = VECTOR('',#95677,1000.) ;
#15504 = VECTOR('',#95678,1000.) ;
#15505 = VECTOR('',#95679,1000.) ;
#15506 = VECTOR('',#95682,1000.) ;
#15507 = VECTOR('',#95683,1000.) ;
#15508 = VECTOR('',#95684,1000.) ;
#15509 = VECTOR('',#95685,1000.) ;
#15510 = VECTOR('',#95688,1000.) ;
#15511 = VECTOR('',#95689,1000.) ;
#15512 = VECTOR('',#95690,1000.) ;
#15513 = VECTOR('',#95693,1000.) ;
#15514 = VECTOR('',#95694,1000.) ;
#15515 = VECTOR('',#95695,1000.) ;
#15516 = VECTOR('',#95698,1000.) ;
#15517 = VECTOR('',#95699,1000.) ;
#15518 = VECTOR('',#95700,1000.) ;
#15519 = VECTOR('',#95701,1000.) ;
#15520 = VECTOR('',#95704,1000.) ;
#15521 = VECTOR('',#95705,1000.) ;
#15522 = VECTOR('',#95706,1000.) ;
#15523 = VECTOR('',#95707,1000.) ;
#15524 = VECTOR('',#95710,1000.) ;
#15525 = VECTOR('',#95711,1000.) ;
#15526 = VECTOR('',#95712,1000.) ;
#15527 = VECTOR('',#95713,1000.) ;
#15528 = VECTOR('',#95716,1000.) ;
#15529 = VECTOR('',#95717,1000.) ;
#15530 = VECTOR('',#95718,1000.) ;
#15531 = VECTOR('',#95719,1000.) ;
#15532 = VECTOR('',#95722,1000.) ;
#15533 = VECTOR('',#95723,1000.) ;
#15534 = VECTOR('',#95724,1000.) ;
#15535 = VECTOR('',#95725,1000.) ;
#15536 = VECTOR('',#95728,1000.) ;
#15537 = VECTOR('',#95733,1000.) ;
#15538 = VECTOR('',#95734,1000.) ;
#15539 = VECTOR('',#95737,1000.) ;
#15540 = VECTOR('',#95742,1000.) ;
#15541 = VECTOR('',#95743,1000.) ;
#15542 = VECTOR('',#95758,1000.) ;
#15543 = VECTOR('',#95759,1000.) ;
#15544 = VECTOR('',#95760,1000.) ;
#15545 = VECTOR('',#95761,1000.) ;
#15546 = VECTOR('',#95764,1000.) ;
#15547 = VECTOR('',#95765,1000.) ;
#15548 = VECTOR('',#95766,1000.) ;
#15549 = VECTOR('',#95769,1000.) ;
#15550 = VECTOR('',#95770,1000.) ;
#15551 = VECTOR('',#95771,1000.) ;
#15552 = VECTOR('',#95774,1000.) ;
#15553 = VECTOR('',#95775,1000.) ;
#15554 = VECTOR('',#95776,1000.) ;
#15555 = VECTOR('',#95777,1000.) ;
#15556 = VECTOR('',#95780,1000.) ;
#15557 = VECTOR('',#95781,1000.) ;
#15558 = VECTOR('',#95782,1000.) ;
#15559 = VECTOR('',#95783,1000.) ;
#15560 = VECTOR('',#95786,1000.) ;
#15561 = VECTOR('',#95787,1000.) ;
#15562 = VECTOR('',#95788,1000.) ;
#15563 = VECTOR('',#95791,1000.) ;
#15564 = VECTOR('',#95792,1000.) ;
#15565 = VECTOR('',#95793,1000.) ;
#15566 = VECTOR('',#95796,1000.) ;
#15567 = VECTOR('',#95797,1000.) ;
#15568 = VECTOR('',#95798,1000.) ;
#15569 = VECTOR('',#95799,1000.) ;
#15570 = VECTOR('',#95802,1000.) ;
#15571 = VECTOR('',#95803,1000.) ;
#15572 = VECTOR('',#95804,1000.) ;
#15573 = VECTOR('',#95805,1000.) ;
#15574 = VECTOR('',#95808,1000.) ;
#15575 = VECTOR('',#95809,1000.) ;
#15576 = VECTOR('',#95810,1000.) ;
#15577 = VECTOR('',#95811,1000.) ;
#15578 = VECTOR('',#95814,1000.) ;
#15579 = VECTOR('',#95815,1000.) ;
#15580 = VECTOR('',#95816,1000.) ;
#15581 = VECTOR('',#95817,1000.) ;
#15582 = VECTOR('',#95820,1000.) ;
#15583 = VECTOR('',#95821,1000.) ;
#15584 = VECTOR('',#95822,1000.) ;
#15585 = VECTOR('',#95823,1000.) ;
#15586 = VECTOR('',#95826,1000.) ;
#15587 = VECTOR('',#95831,1000.) ;
#15588 = VECTOR('',#95832,1000.) ;
#15589 = VECTOR('',#95835,1000.) ;
#15590 = VECTOR('',#95840,1000.) ;
#15591 = VECTOR('',#95841,1000.) ;
#15592 = VECTOR('',#95856,1000.) ;
#15593 = VECTOR('',#95857,1000.) ;
#15594 = VECTOR('',#95858,1000.) ;
#15595 = VECTOR('',#95859,1000.) ;
#15596 = VECTOR('',#95862,1000.) ;
#15597 = VECTOR('',#95863,1000.) ;
#15598 = VECTOR('',#95864,1000.) ;
#15599 = VECTOR('',#95867,1000.) ;
#15600 = VECTOR('',#95868,1000.) ;
#15601 = VECTOR('',#95869,1000.) ;
#15602 = VECTOR('',#95872,1000.) ;
#15603 = VECTOR('',#95873,1000.) ;
#15604 = VECTOR('',#95874,1000.) ;
#15605 = VECTOR('',#95875,1000.) ;
#15606 = VECTOR('',#95878,1000.) ;
#15607 = VECTOR('',#95879,1000.) ;
#15608 = VECTOR('',#95880,1000.) ;
#15609 = VECTOR('',#95881,1000.) ;
#15610 = VECTOR('',#95884,1000.) ;
#15611 = VECTOR('',#95885,1000.) ;
#15612 = VECTOR('',#95886,1000.) ;
#15613 = VECTOR('',#95889,1000.) ;
#15614 = VECTOR('',#95890,1000.) ;
#15615 = VECTOR('',#95891,1000.) ;
#15616 = VECTOR('',#95894,1000.) ;
#15617 = VECTOR('',#95895,1000.) ;
#15618 = VECTOR('',#95896,1000.) ;
#15619 = VECTOR('',#95897,1000.) ;
#15620 = VECTOR('',#95900,1000.) ;
#15621 = VECTOR('',#95901,1000.) ;
#15622 = VECTOR('',#95902,1000.) ;
#15623 = VECTOR('',#95903,1000.) ;
#15624 = VECTOR('',#95906,1000.) ;
#15625 = VECTOR('',#95907,1000.) ;
#15626 = VECTOR('',#95908,1000.) ;
#15627 = VECTOR('',#95909,1000.) ;
#15628 = VECTOR('',#95912,1000.) ;
#15629 = VECTOR('',#95913,1000.) ;
#15630 = VECTOR('',#95914,1000.) ;
#15631 = VECTOR('',#95915,1000.) ;
#15632 = VECTOR('',#95918,1000.) ;
#15633 = VECTOR('',#95919,1000.) ;
#15634 = VECTOR('',#95920,1000.) ;
#15635 = VECTOR('',#95921,1000.) ;
#15636 = VECTOR('',#95924,1000.) ;
#15637 = VECTOR('',#95929,1000.) ;
#15638 = VECTOR('',#95930,1000.) ;
#15639 = VECTOR('',#95933,1000.) ;
#15640 = VECTOR('',#95938,1000.) ;
#15641 = VECTOR('',#95939,1000.) ;
#15642 = VECTOR('',#95954,1000.) ;
#15643 = VECTOR('',#95955,1000.) ;
#15644 = VECTOR('',#95956,1000.) ;
#15645 = VECTOR('',#95957,1000.) ;
#15646 = VECTOR('',#95960,1000.) ;
#15647 = VECTOR('',#95961,1000.) ;
#15648 = VECTOR('',#95962,1000.) ;
#15649 = VECTOR('',#95965,1000.) ;
#15650 = VECTOR('',#95966,1000.) ;
#15651 = VECTOR('',#95967,1000.) ;
#15652 = VECTOR('',#95970,1000.) ;
#15653 = VECTOR('',#95971,1000.) ;
#15654 = VECTOR('',#95972,1000.) ;
#15655 = VECTOR('',#95973,1000.) ;
#15656 = VECTOR('',#95976,1000.) ;
#15657 = VECTOR('',#95977,1000.) ;
#15658 = VECTOR('',#95978,1000.) ;
#15659 = VECTOR('',#95979,1000.) ;
#15660 = VECTOR('',#95982,1000.) ;
#15661 = VECTOR('',#95983,1000.) ;
#15662 = VECTOR('',#95984,1000.) ;
#15663 = VECTOR('',#95987,1000.) ;
#15664 = VECTOR('',#95988,1000.) ;
#15665 = VECTOR('',#95989,1000.) ;
#15666 = VECTOR('',#95992,1000.) ;
#15667 = VECTOR('',#95993,1000.) ;
#15668 = VECTOR('',#95994,1000.) ;
#15669 = VECTOR('',#95995,1000.) ;
#15670 = VECTOR('',#95998,1000.) ;
#15671 = VECTOR('',#95999,1000.) ;
#15672 = VECTOR('',#96000,1000.) ;
#15673 = VECTOR('',#96001,1000.) ;
#15674 = VECTOR('',#96004,1000.) ;
#15675 = VECTOR('',#96005,1000.) ;
#15676 = VECTOR('',#96006,1000.) ;
#15677 = VECTOR('',#96007,1000.) ;
#15678 = VECTOR('',#96010,1000.) ;
#15679 = VECTOR('',#96011,1000.) ;
#15680 = VECTOR('',#96012,1000.) ;
#15681 = VECTOR('',#96013,1000.) ;
#15682 = VECTOR('',#96016,1000.) ;
#15683 = VECTOR('',#96017,1000.) ;
#15684 = VECTOR('',#96018,1000.) ;
#15685 = VECTOR('',#96019,1000.) ;
#15686 = VECTOR('',#96022,1000.) ;
#15687 = VECTOR('',#96027,1000.) ;
#15688 = VECTOR('',#96028,1000.) ;
#15689 = VECTOR('',#96031,1000.) ;
#15690 = VECTOR('',#96036,1000.) ;
#15691 = VECTOR('',#96037,1000.) ;
#15692 = VECTOR('',#96052,1000.) ;
#15693 = VECTOR('',#96053,1000.) ;
#15694 = VECTOR('',#96054,1000.) ;
#15695 = VECTOR('',#96055,1000.) ;
#15696 = VECTOR('',#96058,1000.) ;
#15697 = VECTOR('',#96059,1000.) ;
#15698 = VECTOR('',#96060,1000.) ;
#15699 = VECTOR('',#96063,1000.) ;
#15700 = VECTOR('',#96064,1000.) ;
#15701 = VECTOR('',#96065,1000.) ;
#15702 = VECTOR('',#96068,1000.) ;
#15703 = VECTOR('',#96069,1000.) ;
#15704 = VECTOR('',#96070,1000.) ;
#15705 = VECTOR('',#96071,1000.) ;
#15706 = VECTOR('',#96074,1000.) ;
#15707 = VECTOR('',#96075,1000.) ;
#15708 = VECTOR('',#96076,1000.) ;
#15709 = VECTOR('',#96077,1000.) ;
#15710 = VECTOR('',#96080,1000.) ;
#15711 = VECTOR('',#96081,1000.) ;
#15712 = VECTOR('',#96082,1000.) ;
#15713 = VECTOR('',#96085,1000.) ;
#15714 = VECTOR('',#96086,1000.) ;
#15715 = VECTOR('',#96087,1000.) ;
#15716 = VECTOR('',#96090,1000.) ;
#15717 = VECTOR('',#96091,1000.) ;
#15718 = VECTOR('',#96092,1000.) ;
#15719 = VECTOR('',#96093,1000.) ;
#15720 = VECTOR('',#96096,1000.) ;
#15721 = VECTOR('',#96097,1000.) ;
#15722 = VECTOR('',#96098,1000.) ;
#15723 = VECTOR('',#96099,1000.) ;
#15724 = VECTOR('',#96102,1000.) ;
#15725 = VECTOR('',#96103,1000.) ;
#15726 = VECTOR('',#96104,1000.) ;
#15727 = VECTOR('',#96105,1000.) ;
#15728 = VECTOR('',#96108,1000.) ;
#15729 = VECTOR('',#96109,1000.) ;
#15730 = VECTOR('',#96110,1000.) ;
#15731 = VECTOR('',#96111,1000.) ;
#15732 = VECTOR('',#96114,1000.) ;
#15733 = VECTOR('',#96115,1000.) ;
#15734 = VECTOR('',#96116,1000.) ;
#15735 = VECTOR('',#96117,1000.) ;
#15736 = VECTOR('',#96120,1000.) ;
#15737 = VECTOR('',#96125,1000.) ;
#15738 = VECTOR('',#96126,1000.) ;
#15739 = VECTOR('',#96129,1000.) ;
#15740 = VECTOR('',#96134,1000.) ;
#15741 = VECTOR('',#96135,1000.) ;
#15742 = VECTOR('',#96150,1000.) ;
#15743 = VECTOR('',#96151,1000.) ;
#15744 = VECTOR('',#96152,1000.) ;
#15745 = VECTOR('',#96153,1000.) ;
#15746 = VECTOR('',#96156,1000.) ;
#15747 = VECTOR('',#96157,1000.) ;
#15748 = VECTOR('',#96158,1000.) ;
#15749 = VECTOR('',#96161,1000.) ;
#15750 = VECTOR('',#96162,1000.) ;
#15751 = VECTOR('',#96163,1000.) ;
#15752 = VECTOR('',#96166,1000.) ;
#15753 = VECTOR('',#96167,1000.) ;
#15754 = VECTOR('',#96168,1000.) ;
#15755 = VECTOR('',#96169,1000.) ;
#15756 = VECTOR('',#96172,1000.) ;
#15757 = VECTOR('',#96173,1000.) ;
#15758 = VECTOR('',#96174,1000.) ;
#15759 = VECTOR('',#96175,1000.) ;
#15760 = VECTOR('',#96178,1000.) ;
#15761 = VECTOR('',#96179,1000.) ;
#15762 = VECTOR('',#96180,1000.) ;
#15763 = VECTOR('',#96183,1000.) ;
#15764 = VECTOR('',#96184,1000.) ;
#15765 = VECTOR('',#96185,1000.) ;
#15766 = VECTOR('',#96188,1000.) ;
#15767 = VECTOR('',#96189,1000.) ;
#15768 = VECTOR('',#96190,1000.) ;
#15769 = VECTOR('',#96191,1000.) ;
#15770 = VECTOR('',#96194,1000.) ;
#15771 = VECTOR('',#96195,1000.) ;
#15772 = VECTOR('',#96196,1000.) ;
#15773 = VECTOR('',#96197,1000.) ;
#15774 = VECTOR('',#96200,1000.) ;
#15775 = VECTOR('',#96201,1000.) ;
#15776 = VECTOR('',#96202,1000.) ;
#15777 = VECTOR('',#96203,1000.) ;
#15778 = VECTOR('',#96206,1000.) ;
#15779 = VECTOR('',#96207,1000.) ;
#15780 = VECTOR('',#96208,1000.) ;
#15781 = VECTOR('',#96209,1000.) ;
#15782 = VECTOR('',#96212,1000.) ;
#15783 = VECTOR('',#96213,1000.) ;
#15784 = VECTOR('',#96214,1000.) ;
#15785 = VECTOR('',#96215,1000.) ;
#15786 = VECTOR('',#96218,1000.) ;
#15787 = VECTOR('',#96223,1000.) ;
#15788 = VECTOR('',#96224,1000.) ;
#15789 = VECTOR('',#96227,1000.) ;
#15790 = VECTOR('',#96232,1000.) ;
#15791 = VECTOR('',#96233,1000.) ;
#15792 = VECTOR('',#96248,1000.) ;
#15793 = VECTOR('',#96249,1000.) ;
#15794 = VECTOR('',#96250,1000.) ;
#15795 = VECTOR('',#96251,1000.) ;
#15796 = VECTOR('',#96254,1000.) ;
#15797 = VECTOR('',#96255,1000.) ;
#15798 = VECTOR('',#96256,1000.) ;
#15799 = VECTOR('',#96259,1000.) ;
#15800 = VECTOR('',#96260,1000.) ;
#15801 = VECTOR('',#96261,1000.) ;
#15802 = VECTOR('',#96264,1000.) ;
#15803 = VECTOR('',#96265,1000.) ;
#15804 = VECTOR('',#96266,1000.) ;
#15805 = VECTOR('',#96267,1000.) ;
#15806 = VECTOR('',#96270,1000.) ;
#15807 = VECTOR('',#96271,1000.) ;
#15808 = VECTOR('',#96272,1000.) ;
#15809 = VECTOR('',#96273,1000.) ;
#15810 = VECTOR('',#96276,1000.) ;
#15811 = VECTOR('',#96277,1000.) ;
#15812 = VECTOR('',#96278,1000.) ;
#15813 = VECTOR('',#96281,1000.) ;
#15814 = VECTOR('',#96282,1000.) ;
#15815 = VECTOR('',#96283,1000.) ;
#15816 = VECTOR('',#96286,1000.) ;
#15817 = VECTOR('',#96287,1000.) ;
#15818 = VECTOR('',#96288,1000.) ;
#15819 = VECTOR('',#96289,1000.) ;
#15820 = VECTOR('',#96292,1000.) ;
#15821 = VECTOR('',#96293,1000.) ;
#15822 = VECTOR('',#96294,1000.) ;
#15823 = VECTOR('',#96295,1000.) ;
#15824 = VECTOR('',#96298,1000.) ;
#15825 = VECTOR('',#96299,1000.) ;
#15826 = VECTOR('',#96300,1000.) ;
#15827 = VECTOR('',#96301,1000.) ;
#15828 = VECTOR('',#96304,1000.) ;
#15829 = VECTOR('',#96305,1000.) ;
#15830 = VECTOR('',#96306,1000.) ;
#15831 = VECTOR('',#96307,1000.) ;
#15832 = VECTOR('',#96310,1000.) ;
#15833 = VECTOR('',#96311,1000.) ;
#15834 = VECTOR('',#96312,1000.) ;
#15835 = VECTOR('',#96313,1000.) ;
#15836 = VECTOR('',#96316,1000.) ;
#15837 = VECTOR('',#96321,1000.) ;
#15838 = VECTOR('',#96322,1000.) ;
#15839 = VECTOR('',#96325,1000.) ;
#15840 = VECTOR('',#96330,1000.) ;
#15841 = VECTOR('',#96331,1000.) ;
#15842 = VECTOR('',#96346,1000.) ;
#15843 = VECTOR('',#96347,1000.) ;
#15844 = VECTOR('',#96348,1000.) ;
#15845 = VECTOR('',#96349,1000.) ;
#15846 = VECTOR('',#96352,1000.) ;
#15847 = VECTOR('',#96353,1000.) ;
#15848 = VECTOR('',#96354,1000.) ;
#15849 = VECTOR('',#96357,1000.) ;
#15850 = VECTOR('',#96358,1000.) ;
#15851 = VECTOR('',#96359,1000.) ;
#15852 = VECTOR('',#96362,1000.) ;
#15853 = VECTOR('',#96363,1000.) ;
#15854 = VECTOR('',#96364,1000.) ;
#15855 = VECTOR('',#96365,1000.) ;
#15856 = VECTOR('',#96368,1000.) ;
#15857 = VECTOR('',#96369,1000.) ;
#15858 = VECTOR('',#96370,1000.) ;
#15859 = VECTOR('',#96371,1000.) ;
#15860 = VECTOR('',#96374,1000.) ;
#15861 = VECTOR('',#96375,1000.) ;
#15862 = VECTOR('',#96376,1000.) ;
#15863 = VECTOR('',#96379,1000.) ;
#15864 = VECTOR('',#96380,1000.) ;
#15865 = VECTOR('',#96381,1000.) ;
#15866 = VECTOR('',#96384,1000.) ;
#15867 = VECTOR('',#96385,1000.) ;
#15868 = VECTOR('',#96386,1000.) ;
#15869 = VECTOR('',#96387,1000.) ;
#15870 = VECTOR('',#96390,1000.) ;
#15871 = VECTOR('',#96391,1000.) ;
#15872 = VECTOR('',#96392,1000.) ;
#15873 = VECTOR('',#96393,1000.) ;
#15874 = VECTOR('',#96396,1000.) ;
#15875 = VECTOR('',#96397,1000.) ;
#15876 = VECTOR('',#96398,1000.) ;
#15877 = VECTOR('',#96399,1000.) ;
#15878 = VECTOR('',#96402,1000.) ;
#15879 = VECTOR('',#96403,1000.) ;
#15880 = VECTOR('',#96404,1000.) ;
#15881 = VECTOR('',#96405,1000.) ;
#15882 = VECTOR('',#96408,1000.) ;
#15883 = VECTOR('',#96409,1000.) ;
#15884 = VECTOR('',#96410,1000.) ;
#15885 = VECTOR('',#96411,1000.) ;
#15886 = VECTOR('',#96414,1000.) ;
#15887 = VECTOR('',#96419,1000.) ;
#15888 = VECTOR('',#96420,1000.) ;
#15889 = VECTOR('',#96423,1000.) ;
#15890 = VECTOR('',#96428,1000.) ;
#15891 = VECTOR('',#96429,1000.) ;
#15892 = VECTOR('',#96444,1000.) ;
#15893 = VECTOR('',#96445,1000.) ;
#15894 = VECTOR('',#96446,1000.) ;
#15895 = VECTOR('',#96447,1000.) ;
#15896 = VECTOR('',#96450,1000.) ;
#15897 = VECTOR('',#96451,1000.) ;
#15898 = VECTOR('',#96452,1000.) ;
#15899 = VECTOR('',#96455,1000.) ;
#15900 = VECTOR('',#96456,1000.) ;
#15901 = VECTOR('',#96457,1000.) ;
#15902 = VECTOR('',#96460,1000.) ;
#15903 = VECTOR('',#96461,1000.) ;
#15904 = VECTOR('',#96462,1000.) ;
#15905 = VECTOR('',#96463,1000.) ;
#15906 = VECTOR('',#96466,1000.) ;
#15907 = VECTOR('',#96467,1000.) ;
#15908 = VECTOR('',#96468,1000.) ;
#15909 = VECTOR('',#96469,1000.) ;
#15910 = VECTOR('',#96472,1000.) ;
#15911 = VECTOR('',#96473,1000.) ;
#15912 = VECTOR('',#96474,1000.) ;
#15913 = VECTOR('',#96477,1000.) ;
#15914 = VECTOR('',#96478,1000.) ;
#15915 = VECTOR('',#96479,1000.) ;
#15916 = VECTOR('',#96482,1000.) ;
#15917 = VECTOR('',#96483,1000.) ;
#15918 = VECTOR('',#96484,1000.) ;
#15919 = VECTOR('',#96485,1000.) ;
#15920 = VECTOR('',#96488,1000.) ;
#15921 = VECTOR('',#96489,1000.) ;
#15922 = VECTOR('',#96490,1000.) ;
#15923 = VECTOR('',#96491,1000.) ;
#15924 = VECTOR('',#96494,1000.) ;
#15925 = VECTOR('',#96495,1000.) ;
#15926 = VECTOR('',#96496,1000.) ;
#15927 = VECTOR('',#96497,1000.) ;
#15928 = VECTOR('',#96500,1000.) ;
#15929 = VECTOR('',#96501,1000.) ;
#15930 = VECTOR('',#96502,1000.) ;
#15931 = VECTOR('',#96503,1000.) ;
#15932 = VECTOR('',#96506,1000.) ;
#15933 = VECTOR('',#96507,1000.) ;
#15934 = VECTOR('',#96508,1000.) ;
#15935 = VECTOR('',#96509,1000.) ;
#15936 = VECTOR('',#96512,1000.) ;
#15937 = VECTOR('',#96513,1000.) ;
#15938 = VECTOR('',#96514,1000.) ;
#15939 = VECTOR('',#96515,1000.) ;
#15940 = VECTOR('',#96518,1000.) ;
#15941 = VECTOR('',#96519,1000.) ;
#15942 = VECTOR('',#96520,1000.) ;
#15943 = VECTOR('',#96521,1000.) ;
#15944 = VECTOR('',#96524,1000.) ;
#15945 = VECTOR('',#96525,1000.) ;
#15946 = VECTOR('',#96526,1000.) ;
#15947 = VECTOR('',#96527,1000.) ;
#15948 = VECTOR('',#96530,1000.) ;
#15949 = VECTOR('',#96531,1000.) ;
#15950 = VECTOR('',#96532,1000.) ;
#15951 = VECTOR('',#96533,1000.) ;
#15952 = VECTOR('',#96536,1000.) ;
#15953 = VECTOR('',#96537,1000.) ;
#15954 = VECTOR('',#96538,1000.) ;
#15955 = VECTOR('',#96539,1000.) ;
#15956 = VECTOR('',#96542,1000.) ;
#15957 = VECTOR('',#96543,1000.) ;
#15958 = VECTOR('',#96544,1000.) ;
#15959 = VECTOR('',#96545,1000.) ;
#15960 = VECTOR('',#96548,1000.) ;
#15961 = VECTOR('',#96549,1000.) ;
#15962 = VECTOR('',#96550,1000.) ;
#15963 = VECTOR('',#96551,1000.) ;
#15964 = VECTOR('',#96554,1000.) ;
#15965 = VECTOR('',#96555,1000.) ;
#15966 = VECTOR('',#96556,1000.) ;
#15967 = VECTOR('',#96557,1000.) ;
#15968 = VECTOR('',#96560,1000.) ;
#15969 = VECTOR('',#96561,1000.) ;
#15970 = VECTOR('',#96562,1000.) ;
#15971 = VECTOR('',#96563,1000.) ;
#15972 = VECTOR('',#96566,1000.) ;
#15973 = VECTOR('',#96567,1000.) ;
#15974 = VECTOR('',#96568,1000.) ;
#15975 = VECTOR('',#96569,1000.) ;
#15976 = VECTOR('',#96572,1000.) ;
#15977 = VECTOR('',#96573,1000.) ;
#15978 = VECTOR('',#96574,1000.) ;
#15979 = VECTOR('',#96575,1000.) ;
#15980 = VECTOR('',#96578,1000.) ;
#15981 = VECTOR('',#96579,1000.) ;
#15982 = VECTOR('',#96580,1000.) ;
#15983 = VECTOR('',#96581,1000.) ;
#15984 = VECTOR('',#96584,1000.) ;
#15985 = VECTOR('',#96585,1000.) ;
#15986 = VECTOR('',#96586,1000.) ;
#15987 = VECTOR('',#96587,1000.) ;
#15988 = VECTOR('',#96590,1000.) ;
#15989 = VECTOR('',#96591,1000.) ;
#15990 = VECTOR('',#96592,1000.) ;
#15991 = VECTOR('',#96593,1000.) ;
#15992 = VECTOR('',#96596,1000.) ;
#15993 = VECTOR('',#96597,1000.) ;
#15994 = VECTOR('',#96598,1000.) ;
#15995 = VECTOR('',#96599,1000.) ;
#15996 = VECTOR('',#96602,1000.) ;
#15997 = VECTOR('',#96603,1000.) ;
#15998 = VECTOR('',#96604,1000.) ;
#15999 = VECTOR('',#96605,1000.) ;
#16000 = VECTOR('',#96608,1000.) ;
#16001 = VECTOR('',#96609,1000.) ;
#16002 = VECTOR('',#96610,1000.) ;
#16003 = VECTOR('',#96611,1000.) ;
#16004 = VECTOR('',#96614,1000.) ;
#16005 = VECTOR('',#96615,1000.) ;
#16006 = VECTOR('',#96616,1000.) ;
#16007 = VECTOR('',#96617,1000.) ;
#16008 = VECTOR('',#96620,1000.) ;
#16009 = VECTOR('',#96621,1000.) ;
#16010 = VECTOR('',#96622,1000.) ;
#16011 = VECTOR('',#96623,1000.) ;
#16012 = VECTOR('',#96626,1000.) ;
#16013 = VECTOR('',#96627,1000.) ;
#16014 = VECTOR('',#96628,1000.) ;
#16015 = VECTOR('',#96629,1000.) ;
#16016 = VECTOR('',#96632,1000.) ;
#16017 = VECTOR('',#96633,1000.) ;
#16018 = VECTOR('',#96634,1000.) ;
#16019 = VECTOR('',#96635,1000.) ;
#16020 = VECTOR('',#96638,1000.) ;
#16021 = VECTOR('',#96639,1000.) ;
#16022 = VECTOR('',#96640,1000.) ;
#16023 = VECTOR('',#96641,1000.) ;
#16024 = VECTOR('',#96644,1000.) ;
#16025 = VECTOR('',#96645,1000.) ;
#16026 = VECTOR('',#96646,1000.) ;
#16027 = VECTOR('',#96647,1000.) ;
#16028 = VECTOR('',#96650,1000.) ;
#16029 = VECTOR('',#96651,1000.) ;
#16030 = VECTOR('',#96652,1000.) ;
#16031 = VECTOR('',#96653,1000.) ;
#16032 = VECTOR('',#96656,1000.) ;
#16033 = VECTOR('',#96657,1000.) ;
#16034 = VECTOR('',#96658,1000.) ;
#16035 = VECTOR('',#96659,1000.) ;
#16036 = VECTOR('',#96662,1000.) ;
#16037 = VECTOR('',#96663,1000.) ;
#16038 = VECTOR('',#96664,1000.) ;
#16039 = VECTOR('',#96665,1000.) ;
#16040 = VECTOR('',#96668,1000.) ;
#16041 = VECTOR('',#96669,1000.) ;
#16042 = VECTOR('',#96670,1000.) ;
#16043 = VECTOR('',#96671,1000.) ;
#16044 = VECTOR('',#96674,1000.) ;
#16045 = VECTOR('',#96675,1000.) ;
#16046 = VECTOR('',#96676,1000.) ;
#16047 = VECTOR('',#96677,1000.) ;
#16048 = VECTOR('',#96680,1000.) ;
#16049 = VECTOR('',#96681,1000.) ;
#16050 = VECTOR('',#96682,1000.) ;
#16051 = VECTOR('',#96683,1000.) ;
#16052 = VECTOR('',#96686,1000.) ;
#16053 = VECTOR('',#96687,1000.) ;
#16054 = VECTOR('',#96688,1000.) ;
#16055 = VECTOR('',#96689,1000.) ;
#16056 = VECTOR('',#96692,1000.) ;
#16057 = VECTOR('',#96693,1000.) ;
#16058 = VECTOR('',#96694,1000.) ;
#16059 = VECTOR('',#96695,1000.) ;
#16060 = VECTOR('',#98716,1.2293670625) ;
#16061 = VECTOR('',#98717,10.) ;
#16062 = VECTOR('',#98720,1.2293670625) ;
#16063 = VECTOR('',#98723,1.2293670625) ;
#16064 = VECTOR('',#98726,1.2293670625) ;
#16065 = VECTOR('',#98729,1.2293670625) ;
#16066 = VECTOR('',#98732,1.2293670625) ;
#16067 = VECTOR('',#98735,1.2293670625) ;
#16068 = VECTOR('',#98738,1.2293670625) ;
#16069 = VECTOR('',#98741,1.2293670625) ;
#16070 = VECTOR('',#98744,1.2293670625) ;
#16071 = VECTOR('',#98747,1.5) ;
#16072 = VECTOR('',#98752,1.5) ;
#16073 = VECTOR('',#98755,1.5) ;
#16074 = VECTOR('',#98758,1.5) ;
#16075 = VECTOR('',#98761,1.5) ;
#16076 = VECTOR('',#98764,1.5) ;
#16077 = VECTOR('',#98767,1.5) ;
#16078 = VECTOR('',#98770,1.5) ;
#16079 = VECTOR('',#98775,1.5) ;
#16080 = VECTOR('',#98778,10.) ;
#16081 = VECTOR('',#98781,1.5) ;
#16082 = VECTOR('',#98792,1.6) ;
#16083 = VECTOR('',#98799,1.25) ;
#16084 = VECTOR('',#98802,1.25) ;
#16085 = VECTOR('',#98811,0.999999999999998) ;
#16086 = VECTOR('',#98816,1000.) ;
#16087 = VECTOR('',#98819,1000.) ;
#16088 = VECTOR('',#98824,1000.) ;
#16089 = VECTOR('',#98827,1000.) ;
#16090 = VECTOR('',#98832,1000.) ;
#16091 = VECTOR('',#98835,1000.) ;
#16092 = VECTOR('',#98840,1000.) ;
#16093 = VECTOR('',#98843,1000.) ;
#16094 = VECTOR('',#98848,1000.) ;
#16095 = VECTOR('',#98851,1000.) ;
#16096 = VECTOR('',#98856,1000.) ;
#16097 = VECTOR('',#98859,1000.) ;
#16098 = VECTOR('',#98928,10.) ;
#16099 = VECTOR('',#98933,1000.) ;
#16100 = VECTOR('',#98936,1000.) ;
#16101 = VECTOR('',#98943,3077.68353717531) ;
#16102 = VECTOR('',#99000,2.8) ;
#16103 = VECTOR('',#99005,1.5) ;
#16104 = VECTOR('',#99044,1000.) ;
#16105 = VECTOR('',#99045,1000.) ;
#16106 = VECTOR('',#99048,1000.) ;
#16107 = VECTOR('',#99049,1000.) ;
#16108 = VECTOR('',#99052,1000.) ;
#16109 = VECTOR('',#99053,1000.) ;
#16110 = VECTOR('',#99056,1000.) ;
#16111 = VECTOR('',#99057,1000.) ;
#16112 = VECTOR('',#99062,1000.) ;
#16113 = VECTOR('',#99063,1000.) ;
#16114 = VECTOR('',#99068,1000.) ;
#16115 = VECTOR('',#99069,1000.) ;
#16116 = VECTOR('',#99072,1000.) ;
#16117 = VECTOR('',#99073,1000.) ;
#16118 = VECTOR('',#99080,1000.) ;
#16119 = VECTOR('',#99081,1000.) ;
#16120 = VECTOR('',#99084,1000.) ;
#16121 = VECTOR('',#99085,1000.) ;
#16122 = VECTOR('',#99092,1000.) ;
#16123 = VECTOR('',#99093,1000.) ;
#16124 = VECTOR('',#99096,1000.) ;
#16125 = VECTOR('',#99099,1000.) ;
#16126 = VECTOR('',#99104,1000.) ;
#16127 = VECTOR('',#99105,1000.) ;
#16128 = CONICAL_SURFACE('',#67795,1.6,0.785398163397431) ;
#16129 = CONICAL_SURFACE('',#67798,1.6,0.785398163397431) ;
#16130 = CONICAL_SURFACE('',#68967,3.,0.165148677414624) ;
#16131 = CONICAL_SURFACE('',#69577,3.,0.165148677414624) ;
#16132 = CONICAL_SURFACE('',#70187,3.,0.165148677414624) ;
#16133 = CONICAL_SURFACE('',#70797,3.,0.165148677414624) ;
#16134 = CONICAL_SURFACE('',#71407,3.,0.165148677414624) ;
#16135 = CONICAL_SURFACE('',#76696,1.6,0.785398163397445) ;
#16136 = CONICAL_SURFACE('',#76701,1.25,1.02974425867665) ;
#16137 = CONICAL_SURFACE('',#76705,0.999999999999998,0.785398163397446) ;
#16138 = CONICAL_SURFACE('',#76725,2.49807621135332,0.785398163397447) ;
#16139 = CONICAL_SURFACE('',#76727,2.49807621135332,0.785398163397447) ;
#16140 = CONICAL_SURFACE('',#76729,2.49807621135332,0.785398163397447) ;
#16141 = CONICAL_SURFACE('',#76731,2.49807621135332,0.785398163397447) ;
#16142 = CONICAL_SURFACE('',#76733,2.49807621135332,0.785398163397447) ;
#16143 = CONICAL_SURFACE('',#76735,2.49807621135332,0.785398163397447) ;
#16144 = CONICAL_SURFACE('',#76737,2.25,0.785398163397443) ;
#16145 = CONICAL_SURFACE('',#76739,2.25,0.785398163397443) ;
#16146 = CONICAL_SURFACE('',#76741,2.25,0.785398163397443) ;
#16147 = CONICAL_SURFACE('',#76743,2.25,0.785398163397443) ;
#16148 = CONICAL_SURFACE('',#76745,2.25,0.785398163397443) ;
#16149 = CONICAL_SURFACE('',#76747,2.25,0.785398163397443) ;
#16150 = CONICAL_SURFACE('',#76763,3077.68353717531,1.25663706143592) ;
#16151 = CONICAL_SURFACE('',#76781,0.556,0.0698131700797659) ;
#16152 = CONICAL_SURFACE('',#76837,0.556,0.0698131700797659) ;
#16153 = CONICAL_SURFACE('',#76838,0.556,0.0698131700797659) ;
#16154 = CONICAL_SURFACE('',#76839,0.556,0.0698131700797659) ;
#16155 = CONICAL_SURFACE('',#76840,0.556,0.0698131700797659) ;
#16156 = CONICAL_SURFACE('',#76841,0.556,0.0698131700797659) ;
#16157 = CONICAL_SURFACE('',#76842,0.556,0.0698131700797659) ;
#16158 = CONICAL_SURFACE('',#76843,0.556,0.0698131700797659) ;
#16159 = FACE_OUTER_BOUND('',#20401,.T.) ;
#16160 = FACE_OUTER_BOUND('',#20402,.T.) ;
#16161 = FACE_OUTER_BOUND('',#20403,.T.) ;
#16162 = FACE_OUTER_BOUND('',#20404,.T.) ;
#16163 = FACE_OUTER_BOUND('',#20405,.T.) ;
#16164 = FACE_OUTER_BOUND('',#20406,.T.) ;
#16165 = FACE_OUTER_BOUND('',#20407,.T.) ;
#16166 = FACE_OUTER_BOUND('',#20408,.T.) ;
#16167 = FACE_OUTER_BOUND('',#20409,.T.) ;
#16168 = FACE_OUTER_BOUND('',#20410,.T.) ;
#16169 = FACE_OUTER_BOUND('',#20411,.T.) ;
#16170 = FACE_OUTER_BOUND('',#20412,.T.) ;
#16171 = FACE_OUTER_BOUND('',#20415,.T.) ;
#16172 = FACE_OUTER_BOUND('',#20418,.T.) ;
#16173 = FACE_OUTER_BOUND('',#20423,.T.) ;
#16174 = FACE_OUTER_BOUND('',#20428,.T.) ;
#16175 = FACE_OUTER_BOUND('',#20436,.T.) ;
#16176 = FACE_OUTER_BOUND('',#20444,.T.) ;
#16177 = FACE_OUTER_BOUND('',#20447,.T.) ;
#16178 = FACE_OUTER_BOUND('',#20450,.T.) ;
#16179 = FACE_OUTER_BOUND('',#20451,.T.) ;
#16180 = FACE_OUTER_BOUND('',#20452,.T.) ;
#16181 = FACE_OUTER_BOUND('',#20453,.T.) ;
#16182 = FACE_OUTER_BOUND('',#20454,.T.) ;
#16183 = FACE_OUTER_BOUND('',#20455,.T.) ;
#16184 = FACE_OUTER_BOUND('',#20456,.T.) ;
#16185 = FACE_OUTER_BOUND('',#20457,.T.) ;
#16186 = FACE_OUTER_BOUND('',#20458,.T.) ;
#16187 = FACE_OUTER_BOUND('',#20459,.T.) ;
#16188 = FACE_OUTER_BOUND('',#20460,.T.) ;
#16189 = FACE_OUTER_BOUND('',#20461,.T.) ;
#16190 = FACE_OUTER_BOUND('',#20462,.T.) ;
#16191 = FACE_OUTER_BOUND('',#20463,.T.) ;
#16192 = FACE_OUTER_BOUND('',#20464,.T.) ;
#16193 = FACE_OUTER_BOUND('',#20465,.T.) ;
#16194 = FACE_OUTER_BOUND('',#20466,.T.) ;
#16195 = FACE_OUTER_BOUND('',#20467,.T.) ;
#16196 = FACE_OUTER_BOUND('',#20468,.T.) ;
#16197 = FACE_OUTER_BOUND('',#20469,.T.) ;
#16198 = FACE_OUTER_BOUND('',#20470,.T.) ;
#16199 = FACE_OUTER_BOUND('',#20471,.T.) ;
#16200 = FACE_OUTER_BOUND('',#20472,.T.) ;
#16201 = FACE_OUTER_BOUND('',#20473,.T.) ;
#16202 = FACE_OUTER_BOUND('',#20474,.T.) ;
#16203 = FACE_OUTER_BOUND('',#20475,.T.) ;
#16204 = FACE_OUTER_BOUND('',#20476,.T.) ;
#16205 = FACE_OUTER_BOUND('',#20477,.T.) ;
#16206 = FACE_OUTER_BOUND('',#20478,.T.) ;
#16207 = FACE_OUTER_BOUND('',#20479,.T.) ;
#16208 = FACE_OUTER_BOUND('',#20480,.T.) ;
#16209 = FACE_OUTER_BOUND('',#20481,.T.) ;
#16210 = FACE_OUTER_BOUND('',#20482,.T.) ;
#16211 = FACE_OUTER_BOUND('',#20483,.T.) ;
#16212 = FACE_OUTER_BOUND('',#20484,.T.) ;
#16213 = FACE_OUTER_BOUND('',#20485,.T.) ;
#16214 = FACE_OUTER_BOUND('',#20486,.T.) ;
#16215 = FACE_OUTER_BOUND('',#20487,.T.) ;
#16216 = FACE_OUTER_BOUND('',#20488,.T.) ;
#16217 = FACE_OUTER_BOUND('',#20489,.T.) ;
#16218 = FACE_OUTER_BOUND('',#20490,.T.) ;
#16219 = FACE_OUTER_BOUND('',#20491,.T.) ;
#16220 = FACE_OUTER_BOUND('',#20492,.T.) ;
#16221 = FACE_OUTER_BOUND('',#20493,.T.) ;
#16222 = FACE_OUTER_BOUND('',#20494,.T.) ;
#16223 = FACE_OUTER_BOUND('',#20495,.T.) ;
#16224 = FACE_OUTER_BOUND('',#20496,.T.) ;
#16225 = FACE_OUTER_BOUND('',#20497,.T.) ;
#16226 = FACE_OUTER_BOUND('',#20498,.T.) ;
#16227 = FACE_OUTER_BOUND('',#20499,.T.) ;
#16228 = FACE_OUTER_BOUND('',#20500,.T.) ;
#16229 = FACE_OUTER_BOUND('',#20501,.T.) ;
#16230 = FACE_OUTER_BOUND('',#20502,.T.) ;
#16231 = FACE_OUTER_BOUND('',#20503,.T.) ;
#16232 = FACE_OUTER_BOUND('',#20504,.T.) ;
#16233 = FACE_OUTER_BOUND('',#20505,.T.) ;
#16234 = FACE_OUTER_BOUND('',#20506,.T.) ;
#16235 = FACE_OUTER_BOUND('',#20507,.T.) ;
#16236 = FACE_OUTER_BOUND('',#20508,.T.) ;
#16237 = FACE_OUTER_BOUND('',#20509,.T.) ;
#16238 = FACE_OUTER_BOUND('',#20510,.T.) ;
#16239 = FACE_OUTER_BOUND('',#20511,.T.) ;
#16240 = FACE_OUTER_BOUND('',#20512,.T.) ;
#16241 = FACE_OUTER_BOUND('',#20513,.T.) ;
#16242 = FACE_OUTER_BOUND('',#20514,.T.) ;
#16243 = FACE_OUTER_BOUND('',#20515,.T.) ;
#16244 = FACE_OUTER_BOUND('',#20516,.T.) ;
#16245 = FACE_OUTER_BOUND('',#20517,.T.) ;
#16246 = FACE_OUTER_BOUND('',#20518,.T.) ;
#16247 = FACE_OUTER_BOUND('',#20519,.T.) ;
#16248 = FACE_OUTER_BOUND('',#20520,.T.) ;
#16249 = FACE_OUTER_BOUND('',#20521,.T.) ;
#16250 = FACE_OUTER_BOUND('',#20522,.T.) ;
#16251 = FACE_OUTER_BOUND('',#20523,.T.) ;
#16252 = FACE_OUTER_BOUND('',#20524,.T.) ;
#16253 = FACE_OUTER_BOUND('',#20525,.T.) ;
#16254 = FACE_OUTER_BOUND('',#20526,.T.) ;
#16255 = FACE_OUTER_BOUND('',#20527,.T.) ;
#16256 = FACE_OUTER_BOUND('',#20528,.T.) ;
#16257 = FACE_OUTER_BOUND('',#20529,.T.) ;
#16258 = FACE_OUTER_BOUND('',#20530,.T.) ;
#16259 = FACE_OUTER_BOUND('',#20531,.T.) ;
#16260 = FACE_OUTER_BOUND('',#20532,.T.) ;
#16261 = FACE_OUTER_BOUND('',#20533,.T.) ;
#16262 = FACE_OUTER_BOUND('',#20534,.T.) ;
#16263 = FACE_OUTER_BOUND('',#20535,.T.) ;
#16264 = FACE_OUTER_BOUND('',#20536,.T.) ;
#16265 = FACE_OUTER_BOUND('',#20537,.T.) ;
#16266 = FACE_OUTER_BOUND('',#20538,.T.) ;
#16267 = FACE_OUTER_BOUND('',#20539,.T.) ;
#16268 = FACE_OUTER_BOUND('',#20540,.T.) ;
#16269 = FACE_OUTER_BOUND('',#20541,.T.) ;
#16270 = FACE_OUTER_BOUND('',#20542,.T.) ;
#16271 = FACE_OUTER_BOUND('',#20543,.T.) ;
#16272 = FACE_OUTER_BOUND('',#20544,.T.) ;
#16273 = FACE_OUTER_BOUND('',#20545,.T.) ;
#16274 = FACE_OUTER_BOUND('',#20546,.T.) ;
#16275 = FACE_OUTER_BOUND('',#20547,.T.) ;
#16276 = FACE_OUTER_BOUND('',#20548,.T.) ;
#16277 = FACE_OUTER_BOUND('',#20549,.T.) ;
#16278 = FACE_OUTER_BOUND('',#20550,.T.) ;
#16279 = FACE_OUTER_BOUND('',#20551,.T.) ;
#16280 = FACE_OUTER_BOUND('',#20552,.T.) ;
#16281 = FACE_OUTER_BOUND('',#20553,.T.) ;
#16282 = FACE_OUTER_BOUND('',#20554,.T.) ;
#16283 = FACE_OUTER_BOUND('',#20555,.T.) ;
#16284 = FACE_OUTER_BOUND('',#20556,.T.) ;
#16285 = FACE_OUTER_BOUND('',#20557,.T.) ;
#16286 = FACE_OUTER_BOUND('',#20558,.T.) ;
#16287 = FACE_OUTER_BOUND('',#20559,.T.) ;
#16288 = FACE_OUTER_BOUND('',#20560,.T.) ;
#16289 = FACE_OUTER_BOUND('',#20561,.T.) ;
#16290 = FACE_OUTER_BOUND('',#20562,.T.) ;
#16291 = FACE_OUTER_BOUND('',#20563,.T.) ;
#16292 = FACE_OUTER_BOUND('',#20564,.T.) ;
#16293 = FACE_OUTER_BOUND('',#20565,.T.) ;
#16294 = FACE_OUTER_BOUND('',#20566,.T.) ;
#16295 = FACE_OUTER_BOUND('',#20567,.T.) ;
#16296 = FACE_OUTER_BOUND('',#20568,.T.) ;
#16297 = FACE_OUTER_BOUND('',#20569,.T.) ;
#16298 = FACE_OUTER_BOUND('',#20570,.T.) ;
#16299 = FACE_OUTER_BOUND('',#20571,.T.) ;
#16300 = FACE_OUTER_BOUND('',#20572,.T.) ;
#16301 = FACE_OUTER_BOUND('',#20573,.T.) ;
#16302 = FACE_OUTER_BOUND('',#20574,.T.) ;
#16303 = FACE_OUTER_BOUND('',#20575,.T.) ;
#16304 = FACE_OUTER_BOUND('',#20576,.T.) ;
#16305 = FACE_OUTER_BOUND('',#20577,.T.) ;
#16306 = FACE_OUTER_BOUND('',#20578,.T.) ;
#16307 = FACE_OUTER_BOUND('',#20579,.T.) ;
#16308 = FACE_OUTER_BOUND('',#20580,.T.) ;
#16309 = FACE_OUTER_BOUND('',#20581,.T.) ;
#16310 = FACE_OUTER_BOUND('',#20582,.T.) ;
#16311 = FACE_OUTER_BOUND('',#20583,.T.) ;
#16312 = FACE_OUTER_BOUND('',#20584,.T.) ;
#16313 = FACE_OUTER_BOUND('',#20585,.T.) ;
#16314 = FACE_OUTER_BOUND('',#20586,.T.) ;
#16315 = FACE_OUTER_BOUND('',#20587,.T.) ;
#16316 = FACE_OUTER_BOUND('',#20588,.T.) ;
#16317 = FACE_OUTER_BOUND('',#20589,.T.) ;
#16318 = FACE_OUTER_BOUND('',#20590,.T.) ;
#16319 = FACE_OUTER_BOUND('',#20591,.T.) ;
#16320 = FACE_OUTER_BOUND('',#20592,.T.) ;
#16321 = FACE_OUTER_BOUND('',#20593,.T.) ;
#16322 = FACE_OUTER_BOUND('',#20594,.T.) ;
#16323 = FACE_OUTER_BOUND('',#20595,.T.) ;
#16324 = FACE_OUTER_BOUND('',#20596,.T.) ;
#16325 = FACE_OUTER_BOUND('',#20597,.T.) ;
#16326 = FACE_OUTER_BOUND('',#20598,.T.) ;
#16327 = FACE_OUTER_BOUND('',#20599,.T.) ;
#16328 = FACE_OUTER_BOUND('',#20600,.T.) ;
#16329 = FACE_OUTER_BOUND('',#20601,.T.) ;
#16330 = FACE_OUTER_BOUND('',#20602,.T.) ;
#16331 = FACE_OUTER_BOUND('',#20603,.T.) ;
#16332 = FACE_OUTER_BOUND('',#20604,.T.) ;
#16333 = FACE_OUTER_BOUND('',#20605,.T.) ;
#16334 = FACE_OUTER_BOUND('',#20606,.T.) ;
#16335 = FACE_OUTER_BOUND('',#20607,.T.) ;
#16336 = FACE_OUTER_BOUND('',#20608,.T.) ;
#16337 = FACE_OUTER_BOUND('',#20609,.T.) ;
#16338 = FACE_OUTER_BOUND('',#20610,.T.) ;
#16339 = FACE_OUTER_BOUND('',#20611,.T.) ;
#16340 = FACE_OUTER_BOUND('',#20612,.T.) ;
#16341 = FACE_OUTER_BOUND('',#20613,.T.) ;
#16342 = FACE_OUTER_BOUND('',#20614,.T.) ;
#16343 = FACE_OUTER_BOUND('',#20615,.T.) ;
#16344 = FACE_OUTER_BOUND('',#20616,.T.) ;
#16345 = FACE_OUTER_BOUND('',#20617,.T.) ;
#16346 = FACE_OUTER_BOUND('',#20618,.T.) ;
#16347 = FACE_OUTER_BOUND('',#20619,.T.) ;
#16348 = FACE_OUTER_BOUND('',#20620,.T.) ;
#16349 = FACE_OUTER_BOUND('',#20621,.T.) ;
#16350 = FACE_OUTER_BOUND('',#20622,.T.) ;
#16351 = FACE_OUTER_BOUND('',#20623,.T.) ;
#16352 = FACE_OUTER_BOUND('',#20624,.T.) ;
#16353 = FACE_OUTER_BOUND('',#20625,.T.) ;
#16354 = FACE_OUTER_BOUND('',#20626,.T.) ;
#16355 = FACE_OUTER_BOUND('',#20627,.T.) ;
#16356 = FACE_OUTER_BOUND('',#20628,.T.) ;
#16357 = FACE_OUTER_BOUND('',#20629,.T.) ;
#16358 = FACE_OUTER_BOUND('',#20630,.T.) ;
#16359 = FACE_OUTER_BOUND('',#20631,.T.) ;
#16360 = FACE_OUTER_BOUND('',#20632,.T.) ;
#16361 = FACE_OUTER_BOUND('',#20633,.T.) ;
#16362 = FACE_OUTER_BOUND('',#20634,.T.) ;
#16363 = FACE_OUTER_BOUND('',#20635,.T.) ;
#16364 = FACE_OUTER_BOUND('',#20636,.T.) ;
#16365 = FACE_OUTER_BOUND('',#20637,.T.) ;
#16366 = FACE_OUTER_BOUND('',#20638,.T.) ;
#16367 = FACE_OUTER_BOUND('',#20639,.T.) ;
#16368 = FACE_OUTER_BOUND('',#20640,.T.) ;
#16369 = FACE_OUTER_BOUND('',#20641,.T.) ;
#16370 = FACE_OUTER_BOUND('',#20642,.T.) ;
#16371 = FACE_OUTER_BOUND('',#20643,.T.) ;
#16372 = FACE_OUTER_BOUND('',#20644,.T.) ;
#16373 = FACE_OUTER_BOUND('',#20645,.T.) ;
#16374 = FACE_OUTER_BOUND('',#20646,.T.) ;
#16375 = FACE_OUTER_BOUND('',#20647,.T.) ;
#16376 = FACE_OUTER_BOUND('',#20648,.T.) ;
#16377 = FACE_OUTER_BOUND('',#20649,.T.) ;
#16378 = FACE_OUTER_BOUND('',#20650,.T.) ;
#16379 = FACE_OUTER_BOUND('',#20651,.T.) ;
#16380 = FACE_OUTER_BOUND('',#20652,.T.) ;
#16381 = FACE_OUTER_BOUND('',#20653,.T.) ;
#16382 = FACE_OUTER_BOUND('',#20654,.T.) ;
#16383 = FACE_OUTER_BOUND('',#20655,.T.) ;
#16384 = FACE_OUTER_BOUND('',#20656,.T.) ;
#16385 = FACE_OUTER_BOUND('',#20657,.T.) ;
#16386 = FACE_OUTER_BOUND('',#20658,.T.) ;
#16387 = FACE_OUTER_BOUND('',#20659,.T.) ;
#16388 = FACE_OUTER_BOUND('',#20660,.T.) ;
#16389 = FACE_OUTER_BOUND('',#20661,.T.) ;
#16390 = FACE_OUTER_BOUND('',#20662,.T.) ;
#16391 = FACE_OUTER_BOUND('',#20663,.T.) ;
#16392 = FACE_OUTER_BOUND('',#20664,.T.) ;
#16393 = FACE_OUTER_BOUND('',#20665,.T.) ;
#16394 = FACE_OUTER_BOUND('',#20666,.T.) ;
#16395 = FACE_OUTER_BOUND('',#20667,.T.) ;
#16396 = FACE_OUTER_BOUND('',#20668,.T.) ;
#16397 = FACE_OUTER_BOUND('',#20669,.T.) ;
#16398 = FACE_OUTER_BOUND('',#20670,.T.) ;
#16399 = FACE_OUTER_BOUND('',#20671,.T.) ;
#16400 = FACE_OUTER_BOUND('',#20672,.T.) ;
#16401 = FACE_OUTER_BOUND('',#20673,.T.) ;
#16402 = FACE_OUTER_BOUND('',#20674,.T.) ;
#16403 = FACE_OUTER_BOUND('',#20675,.T.) ;
#16404 = FACE_OUTER_BOUND('',#20676,.T.) ;
#16405 = FACE_OUTER_BOUND('',#20677,.T.) ;
#16406 = FACE_OUTER_BOUND('',#20678,.T.) ;
#16407 = FACE_OUTER_BOUND('',#20679,.T.) ;
#16408 = FACE_OUTER_BOUND('',#20680,.T.) ;
#16409 = FACE_OUTER_BOUND('',#20681,.T.) ;
#16410 = FACE_OUTER_BOUND('',#20682,.T.) ;
#16411 = FACE_OUTER_BOUND('',#20683,.T.) ;
#16412 = FACE_OUTER_BOUND('',#20684,.T.) ;
#16413 = FACE_OUTER_BOUND('',#20685,.T.) ;
#16414 = FACE_OUTER_BOUND('',#20686,.T.) ;
#16415 = FACE_OUTER_BOUND('',#20687,.T.) ;
#16416 = FACE_OUTER_BOUND('',#20688,.T.) ;
#16417 = FACE_OUTER_BOUND('',#20689,.T.) ;
#16418 = FACE_OUTER_BOUND('',#20690,.T.) ;
#16419 = FACE_OUTER_BOUND('',#20691,.T.) ;
#16420 = FACE_OUTER_BOUND('',#20692,.T.) ;
#16421 = FACE_OUTER_BOUND('',#20693,.T.) ;
#16422 = FACE_OUTER_BOUND('',#20694,.T.) ;
#16423 = FACE_OUTER_BOUND('',#20695,.T.) ;
#16424 = FACE_OUTER_BOUND('',#20696,.T.) ;
#16425 = FACE_OUTER_BOUND('',#20697,.T.) ;
#16426 = FACE_OUTER_BOUND('',#20698,.T.) ;
#16427 = FACE_OUTER_BOUND('',#20699,.T.) ;
#16428 = FACE_OUTER_BOUND('',#20700,.T.) ;
#16429 = FACE_OUTER_BOUND('',#20701,.T.) ;
#16430 = FACE_OUTER_BOUND('',#20702,.T.) ;
#16431 = FACE_OUTER_BOUND('',#20703,.T.) ;
#16432 = FACE_OUTER_BOUND('',#20704,.T.) ;
#16433 = FACE_OUTER_BOUND('',#20705,.T.) ;
#16434 = FACE_OUTER_BOUND('',#20706,.T.) ;
#16435 = FACE_OUTER_BOUND('',#20707,.T.) ;
#16436 = FACE_OUTER_BOUND('',#20708,.T.) ;
#16437 = FACE_OUTER_BOUND('',#20709,.T.) ;
#16438 = FACE_OUTER_BOUND('',#20710,.T.) ;
#16439 = FACE_OUTER_BOUND('',#20711,.T.) ;
#16440 = FACE_OUTER_BOUND('',#20712,.T.) ;
#16441 = FACE_OUTER_BOUND('',#20713,.T.) ;
#16442 = FACE_OUTER_BOUND('',#20714,.T.) ;
#16443 = FACE_OUTER_BOUND('',#20715,.T.) ;
#16444 = FACE_OUTER_BOUND('',#20716,.T.) ;
#16445 = FACE_OUTER_BOUND('',#20717,.T.) ;
#16446 = FACE_OUTER_BOUND('',#20718,.T.) ;
#16447 = FACE_OUTER_BOUND('',#20719,.T.) ;
#16448 = FACE_OUTER_BOUND('',#20720,.T.) ;
#16449 = FACE_OUTER_BOUND('',#20721,.T.) ;
#16450 = FACE_OUTER_BOUND('',#20722,.T.) ;
#16451 = FACE_OUTER_BOUND('',#20723,.T.) ;
#16452 = FACE_OUTER_BOUND('',#20724,.T.) ;
#16453 = FACE_OUTER_BOUND('',#20725,.T.) ;
#16454 = FACE_OUTER_BOUND('',#20726,.T.) ;
#16455 = FACE_OUTER_BOUND('',#20727,.T.) ;
#16456 = FACE_OUTER_BOUND('',#20728,.T.) ;
#16457 = FACE_OUTER_BOUND('',#20729,.T.) ;
#16458 = FACE_OUTER_BOUND('',#20730,.T.) ;
#16459 = FACE_OUTER_BOUND('',#20731,.T.) ;
#16460 = FACE_OUTER_BOUND('',#20732,.T.) ;
#16461 = FACE_OUTER_BOUND('',#20733,.T.) ;
#16462 = FACE_OUTER_BOUND('',#20734,.T.) ;
#16463 = FACE_OUTER_BOUND('',#20735,.T.) ;
#16464 = FACE_OUTER_BOUND('',#20736,.T.) ;
#16465 = FACE_OUTER_BOUND('',#20737,.T.) ;
#16466 = FACE_OUTER_BOUND('',#20738,.T.) ;
#16467 = FACE_OUTER_BOUND('',#20739,.T.) ;
#16468 = FACE_OUTER_BOUND('',#20740,.T.) ;
#16469 = FACE_OUTER_BOUND('',#20741,.T.) ;
#16470 = FACE_OUTER_BOUND('',#20742,.T.) ;
#16471 = FACE_OUTER_BOUND('',#20743,.T.) ;
#16472 = FACE_OUTER_BOUND('',#20744,.T.) ;
#16473 = FACE_OUTER_BOUND('',#20745,.T.) ;
#16474 = FACE_OUTER_BOUND('',#20746,.T.) ;
#16475 = FACE_OUTER_BOUND('',#20747,.T.) ;
#16476 = FACE_OUTER_BOUND('',#20748,.T.) ;
#16477 = FACE_OUTER_BOUND('',#20749,.T.) ;
#16478 = FACE_OUTER_BOUND('',#20750,.T.) ;
#16479 = FACE_OUTER_BOUND('',#20751,.T.) ;
#16480 = FACE_OUTER_BOUND('',#20752,.T.) ;
#16481 = FACE_OUTER_BOUND('',#20753,.T.) ;
#16482 = FACE_OUTER_BOUND('',#20754,.T.) ;
#16483 = FACE_OUTER_BOUND('',#20755,.T.) ;
#16484 = FACE_OUTER_BOUND('',#20756,.T.) ;
#16485 = FACE_OUTER_BOUND('',#20757,.T.) ;
#16486 = FACE_OUTER_BOUND('',#20758,.T.) ;
#16487 = FACE_OUTER_BOUND('',#20759,.T.) ;
#16488 = FACE_OUTER_BOUND('',#20760,.T.) ;
#16489 = FACE_OUTER_BOUND('',#20761,.T.) ;
#16490 = FACE_OUTER_BOUND('',#20762,.T.) ;
#16491 = FACE_OUTER_BOUND('',#20763,.T.) ;
#16492 = FACE_OUTER_BOUND('',#20764,.T.) ;
#16493 = FACE_OUTER_BOUND('',#20765,.T.) ;
#16494 = FACE_OUTER_BOUND('',#20766,.T.) ;
#16495 = FACE_OUTER_BOUND('',#20767,.T.) ;
#16496 = FACE_OUTER_BOUND('',#20768,.T.) ;
#16497 = FACE_OUTER_BOUND('',#20769,.T.) ;
#16498 = FACE_OUTER_BOUND('',#20770,.T.) ;
#16499 = FACE_OUTER_BOUND('',#20771,.T.) ;
#16500 = FACE_OUTER_BOUND('',#20772,.T.) ;
#16501 = FACE_OUTER_BOUND('',#20773,.T.) ;
#16502 = FACE_OUTER_BOUND('',#20774,.T.) ;
#16503 = FACE_OUTER_BOUND('',#20775,.T.) ;
#16504 = FACE_OUTER_BOUND('',#20776,.T.) ;
#16505 = FACE_OUTER_BOUND('',#20777,.T.) ;
#16506 = FACE_OUTER_BOUND('',#20778,.T.) ;
#16507 = FACE_OUTER_BOUND('',#20779,.T.) ;
#16508 = FACE_OUTER_BOUND('',#20780,.T.) ;
#16509 = FACE_OUTER_BOUND('',#20781,.T.) ;
#16510 = FACE_OUTER_BOUND('',#20782,.T.) ;
#16511 = FACE_OUTER_BOUND('',#20783,.T.) ;
#16512 = FACE_OUTER_BOUND('',#20784,.T.) ;
#16513 = FACE_OUTER_BOUND('',#20785,.T.) ;
#16514 = FACE_OUTER_BOUND('',#20786,.T.) ;
#16515 = FACE_OUTER_BOUND('',#20787,.T.) ;
#16516 = FACE_OUTER_BOUND('',#20788,.T.) ;
#16517 = FACE_OUTER_BOUND('',#20789,.T.) ;
#16518 = FACE_OUTER_BOUND('',#20790,.T.) ;
#16519 = FACE_OUTER_BOUND('',#20791,.T.) ;
#16520 = FACE_OUTER_BOUND('',#20792,.T.) ;
#16521 = FACE_OUTER_BOUND('',#20793,.T.) ;
#16522 = FACE_OUTER_BOUND('',#20794,.T.) ;
#16523 = FACE_OUTER_BOUND('',#20795,.T.) ;
#16524 = FACE_OUTER_BOUND('',#20796,.T.) ;
#16525 = FACE_OUTER_BOUND('',#20797,.T.) ;
#16526 = FACE_OUTER_BOUND('',#20798,.T.) ;
#16527 = FACE_OUTER_BOUND('',#20799,.T.) ;
#16528 = FACE_OUTER_BOUND('',#20800,.T.) ;
#16529 = FACE_OUTER_BOUND('',#20801,.T.) ;
#16530 = FACE_OUTER_BOUND('',#20802,.T.) ;
#16531 = FACE_OUTER_BOUND('',#20803,.T.) ;
#16532 = FACE_OUTER_BOUND('',#20804,.T.) ;
#16533 = FACE_OUTER_BOUND('',#20805,.T.) ;
#16534 = FACE_OUTER_BOUND('',#20806,.T.) ;
#16535 = FACE_OUTER_BOUND('',#20807,.T.) ;
#16536 = FACE_OUTER_BOUND('',#20808,.T.) ;
#16537 = FACE_OUTER_BOUND('',#20809,.T.) ;
#16538 = FACE_OUTER_BOUND('',#20810,.T.) ;
#16539 = FACE_OUTER_BOUND('',#20811,.T.) ;
#16540 = FACE_OUTER_BOUND('',#20812,.T.) ;
#16541 = FACE_OUTER_BOUND('',#20813,.T.) ;
#16542 = FACE_OUTER_BOUND('',#20814,.T.) ;
#16543 = FACE_OUTER_BOUND('',#20815,.T.) ;
#16544 = FACE_OUTER_BOUND('',#20816,.T.) ;
#16545 = FACE_OUTER_BOUND('',#20817,.T.) ;
#16546 = FACE_OUTER_BOUND('',#20818,.T.) ;
#16547 = FACE_OUTER_BOUND('',#20819,.T.) ;
#16548 = FACE_OUTER_BOUND('',#20820,.T.) ;
#16549 = FACE_OUTER_BOUND('',#20821,.T.) ;
#16550 = FACE_OUTER_BOUND('',#20822,.T.) ;
#16551 = FACE_OUTER_BOUND('',#20823,.T.) ;
#16552 = FACE_OUTER_BOUND('',#20824,.T.) ;
#16553 = FACE_OUTER_BOUND('',#20825,.T.) ;
#16554 = FACE_OUTER_BOUND('',#20826,.T.) ;
#16555 = FACE_OUTER_BOUND('',#20827,.T.) ;
#16556 = FACE_OUTER_BOUND('',#20828,.T.) ;
#16557 = FACE_OUTER_BOUND('',#20829,.T.) ;
#16558 = FACE_OUTER_BOUND('',#20830,.T.) ;
#16559 = FACE_OUTER_BOUND('',#20831,.T.) ;
#16560 = FACE_OUTER_BOUND('',#20832,.T.) ;
#16561 = FACE_OUTER_BOUND('',#20833,.T.) ;
#16562 = FACE_OUTER_BOUND('',#20834,.T.) ;
#16563 = FACE_OUTER_BOUND('',#20835,.T.) ;
#16564 = FACE_OUTER_BOUND('',#20836,.T.) ;
#16565 = FACE_OUTER_BOUND('',#20837,.T.) ;
#16566 = FACE_OUTER_BOUND('',#20838,.T.) ;
#16567 = FACE_OUTER_BOUND('',#20839,.T.) ;
#16568 = FACE_OUTER_BOUND('',#20840,.T.) ;
#16569 = FACE_OUTER_BOUND('',#20841,.T.) ;
#16570 = FACE_OUTER_BOUND('',#20842,.T.) ;
#16571 = FACE_OUTER_BOUND('',#20843,.T.) ;
#16572 = FACE_OUTER_BOUND('',#20844,.T.) ;
#16573 = FACE_OUTER_BOUND('',#20845,.T.) ;
#16574 = FACE_OUTER_BOUND('',#20846,.T.) ;
#16575 = FACE_OUTER_BOUND('',#20847,.T.) ;
#16576 = FACE_OUTER_BOUND('',#20848,.T.) ;
#16577 = FACE_OUTER_BOUND('',#20849,.T.) ;
#16578 = FACE_OUTER_BOUND('',#20850,.T.) ;
#16579 = FACE_OUTER_BOUND('',#20851,.T.) ;
#16580 = FACE_OUTER_BOUND('',#20852,.T.) ;
#16581 = FACE_OUTER_BOUND('',#20853,.T.) ;
#16582 = FACE_OUTER_BOUND('',#20854,.T.) ;
#16583 = FACE_OUTER_BOUND('',#20855,.T.) ;
#16584 = FACE_OUTER_BOUND('',#20856,.T.) ;
#16585 = FACE_OUTER_BOUND('',#20857,.T.) ;
#16586 = FACE_OUTER_BOUND('',#20858,.T.) ;
#16587 = FACE_OUTER_BOUND('',#20859,.T.) ;
#16588 = FACE_OUTER_BOUND('',#20860,.T.) ;
#16589 = FACE_OUTER_BOUND('',#20861,.T.) ;
#16590 = FACE_OUTER_BOUND('',#20862,.T.) ;
#16591 = FACE_OUTER_BOUND('',#20863,.T.) ;
#16592 = FACE_OUTER_BOUND('',#20864,.T.) ;
#16593 = FACE_OUTER_BOUND('',#20865,.T.) ;
#16594 = FACE_OUTER_BOUND('',#20866,.T.) ;
#16595 = FACE_OUTER_BOUND('',#20867,.T.) ;
#16596 = FACE_OUTER_BOUND('',#20868,.T.) ;
#16597 = FACE_OUTER_BOUND('',#20869,.T.) ;
#16598 = FACE_OUTER_BOUND('',#20870,.T.) ;
#16599 = FACE_OUTER_BOUND('',#20871,.T.) ;
#16600 = FACE_OUTER_BOUND('',#20872,.T.) ;
#16601 = FACE_OUTER_BOUND('',#20873,.T.) ;
#16602 = FACE_OUTER_BOUND('',#20874,.T.) ;
#16603 = FACE_OUTER_BOUND('',#20875,.T.) ;
#16604 = FACE_OUTER_BOUND('',#20876,.T.) ;
#16605 = FACE_OUTER_BOUND('',#20877,.T.) ;
#16606 = FACE_OUTER_BOUND('',#20878,.T.) ;
#16607 = FACE_OUTER_BOUND('',#20879,.T.) ;
#16608 = FACE_OUTER_BOUND('',#20880,.T.) ;
#16609 = FACE_OUTER_BOUND('',#20881,.T.) ;
#16610 = FACE_OUTER_BOUND('',#20882,.T.) ;
#16611 = FACE_OUTER_BOUND('',#20883,.T.) ;
#16612 = FACE_OUTER_BOUND('',#20884,.T.) ;
#16613 = FACE_OUTER_BOUND('',#20885,.T.) ;
#16614 = FACE_OUTER_BOUND('',#20886,.T.) ;
#16615 = FACE_OUTER_BOUND('',#20887,.T.) ;
#16616 = FACE_OUTER_BOUND('',#20888,.T.) ;
#16617 = FACE_OUTER_BOUND('',#20889,.T.) ;
#16618 = FACE_OUTER_BOUND('',#20890,.T.) ;
#16619 = FACE_OUTER_BOUND('',#20891,.T.) ;
#16620 = FACE_OUTER_BOUND('',#20892,.T.) ;
#16621 = FACE_OUTER_BOUND('',#20893,.T.) ;
#16622 = FACE_OUTER_BOUND('',#20894,.T.) ;
#16623 = FACE_OUTER_BOUND('',#20895,.T.) ;
#16624 = FACE_OUTER_BOUND('',#20896,.T.) ;
#16625 = FACE_OUTER_BOUND('',#20897,.T.) ;
#16626 = FACE_OUTER_BOUND('',#20898,.T.) ;
#16627 = FACE_OUTER_BOUND('',#20899,.T.) ;
#16628 = FACE_OUTER_BOUND('',#20900,.T.) ;
#16629 = FACE_OUTER_BOUND('',#20901,.T.) ;
#16630 = FACE_OUTER_BOUND('',#20902,.T.) ;
#16631 = FACE_OUTER_BOUND('',#20903,.T.) ;
#16632 = FACE_OUTER_BOUND('',#20904,.T.) ;
#16633 = FACE_OUTER_BOUND('',#20905,.T.) ;
#16634 = FACE_OUTER_BOUND('',#20906,.T.) ;
#16635 = FACE_OUTER_BOUND('',#20907,.T.) ;
#16636 = FACE_OUTER_BOUND('',#20909,.T.) ;
#16637 = FACE_OUTER_BOUND('',#20910,.T.) ;
#16638 = FACE_OUTER_BOUND('',#20911,.T.) ;
#16639 = FACE_OUTER_BOUND('',#20912,.T.) ;
#16640 = FACE_OUTER_BOUND('',#20913,.T.) ;
#16641 = FACE_OUTER_BOUND('',#20914,.T.) ;
#16642 = FACE_OUTER_BOUND('',#20915,.T.) ;
#16643 = FACE_OUTER_BOUND('',#20916,.T.) ;
#16644 = FACE_OUTER_BOUND('',#20917,.T.) ;
#16645 = FACE_OUTER_BOUND('',#20918,.T.) ;
#16646 = FACE_OUTER_BOUND('',#20919,.T.) ;
#16647 = FACE_OUTER_BOUND('',#20921,.T.) ;
#16648 = FACE_OUTER_BOUND('',#20922,.T.) ;
#16649 = FACE_OUTER_BOUND('',#20923,.T.) ;
#16650 = FACE_OUTER_BOUND('',#20924,.T.) ;
#16651 = FACE_OUTER_BOUND('',#20925,.T.) ;
#16652 = FACE_OUTER_BOUND('',#20926,.T.) ;
#16653 = FACE_OUTER_BOUND('',#20927,.T.) ;
#16654 = FACE_OUTER_BOUND('',#20928,.T.) ;
#16655 = FACE_OUTER_BOUND('',#20929,.T.) ;
#16656 = FACE_OUTER_BOUND('',#20930,.T.) ;
#16657 = FACE_OUTER_BOUND('',#20931,.T.) ;
#16658 = FACE_OUTER_BOUND('',#20932,.T.) ;
#16659 = FACE_OUTER_BOUND('',#20933,.T.) ;
#16660 = FACE_OUTER_BOUND('',#20934,.T.) ;
#16661 = FACE_OUTER_BOUND('',#20935,.T.) ;
#16662 = FACE_OUTER_BOUND('',#20936,.T.) ;
#16663 = FACE_OUTER_BOUND('',#20937,.T.) ;
#16664 = FACE_OUTER_BOUND('',#20938,.T.) ;
#16665 = FACE_OUTER_BOUND('',#20939,.T.) ;
#16666 = FACE_OUTER_BOUND('',#20940,.T.) ;
#16667 = FACE_OUTER_BOUND('',#20941,.T.) ;
#16668 = FACE_OUTER_BOUND('',#20942,.T.) ;
#16669 = FACE_OUTER_BOUND('',#20943,.T.) ;
#16670 = FACE_OUTER_BOUND('',#20944,.T.) ;
#16671 = FACE_OUTER_BOUND('',#20945,.T.) ;
#16672 = FACE_OUTER_BOUND('',#20946,.T.) ;
#16673 = FACE_OUTER_BOUND('',#20947,.T.) ;
#16674 = FACE_OUTER_BOUND('',#20948,.T.) ;
#16675 = FACE_OUTER_BOUND('',#20949,.T.) ;
#16676 = FACE_OUTER_BOUND('',#20950,.T.) ;
#16677 = FACE_OUTER_BOUND('',#20951,.T.) ;
#16678 = FACE_OUTER_BOUND('',#20952,.T.) ;
#16679 = FACE_OUTER_BOUND('',#20953,.T.) ;
#16680 = FACE_OUTER_BOUND('',#20954,.T.) ;
#16681 = FACE_OUTER_BOUND('',#20955,.T.) ;
#16682 = FACE_OUTER_BOUND('',#20956,.T.) ;
#16683 = FACE_OUTER_BOUND('',#20957,.T.) ;
#16684 = FACE_OUTER_BOUND('',#20958,.T.) ;
#16685 = FACE_OUTER_BOUND('',#20959,.T.) ;
#16686 = FACE_OUTER_BOUND('',#20960,.T.) ;
#16687 = FACE_OUTER_BOUND('',#20961,.T.) ;
#16688 = FACE_OUTER_BOUND('',#20962,.T.) ;
#16689 = FACE_OUTER_BOUND('',#20963,.T.) ;
#16690 = FACE_OUTER_BOUND('',#20964,.T.) ;
#16691 = FACE_OUTER_BOUND('',#20965,.T.) ;
#16692 = FACE_OUTER_BOUND('',#20966,.T.) ;
#16693 = FACE_OUTER_BOUND('',#20967,.T.) ;
#16694 = FACE_OUTER_BOUND('',#20968,.T.) ;
#16695 = FACE_OUTER_BOUND('',#20969,.T.) ;
#16696 = FACE_OUTER_BOUND('',#20970,.T.) ;
#16697 = FACE_OUTER_BOUND('',#20971,.T.) ;
#16698 = FACE_OUTER_BOUND('',#20972,.T.) ;
#16699 = FACE_OUTER_BOUND('',#20973,.T.) ;
#16700 = FACE_OUTER_BOUND('',#20974,.T.) ;
#16701 = FACE_OUTER_BOUND('',#20975,.T.) ;
#16702 = FACE_OUTER_BOUND('',#20976,.T.) ;
#16703 = FACE_OUTER_BOUND('',#20977,.T.) ;
#16704 = FACE_OUTER_BOUND('',#20978,.T.) ;
#16705 = FACE_OUTER_BOUND('',#20979,.T.) ;
#16706 = FACE_OUTER_BOUND('',#20980,.T.) ;
#16707 = FACE_OUTER_BOUND('',#20981,.T.) ;
#16708 = FACE_OUTER_BOUND('',#20982,.T.) ;
#16709 = FACE_OUTER_BOUND('',#20983,.T.) ;
#16710 = FACE_OUTER_BOUND('',#20984,.T.) ;
#16711 = FACE_OUTER_BOUND('',#20985,.T.) ;
#16712 = FACE_OUTER_BOUND('',#20986,.T.) ;
#16713 = FACE_OUTER_BOUND('',#20987,.T.) ;
#16714 = FACE_OUTER_BOUND('',#20988,.T.) ;
#16715 = FACE_OUTER_BOUND('',#20989,.T.) ;
#16716 = FACE_OUTER_BOUND('',#20990,.T.) ;
#16717 = FACE_OUTER_BOUND('',#20991,.T.) ;
#16718 = FACE_OUTER_BOUND('',#20992,.T.) ;
#16719 = FACE_OUTER_BOUND('',#20993,.T.) ;
#16720 = FACE_OUTER_BOUND('',#20994,.T.) ;
#16721 = FACE_OUTER_BOUND('',#20995,.T.) ;
#16722 = FACE_OUTER_BOUND('',#20996,.T.) ;
#16723 = FACE_OUTER_BOUND('',#20997,.T.) ;
#16724 = FACE_OUTER_BOUND('',#20998,.T.) ;
#16725 = FACE_OUTER_BOUND('',#20999,.T.) ;
#16726 = FACE_OUTER_BOUND('',#21000,.T.) ;
#16727 = FACE_OUTER_BOUND('',#21001,.T.) ;
#16728 = FACE_OUTER_BOUND('',#21002,.T.) ;
#16729 = FACE_OUTER_BOUND('',#21003,.T.) ;
#16730 = FACE_OUTER_BOUND('',#21004,.T.) ;
#16731 = FACE_OUTER_BOUND('',#21005,.T.) ;
#16732 = FACE_OUTER_BOUND('',#21006,.T.) ;
#16733 = FACE_OUTER_BOUND('',#21007,.T.) ;
#16734 = FACE_OUTER_BOUND('',#21008,.T.) ;
#16735 = FACE_OUTER_BOUND('',#21009,.T.) ;
#16736 = FACE_OUTER_BOUND('',#21010,.T.) ;
#16737 = FACE_OUTER_BOUND('',#21011,.T.) ;
#16738 = FACE_OUTER_BOUND('',#21012,.T.) ;
#16739 = FACE_OUTER_BOUND('',#21013,.T.) ;
#16740 = FACE_OUTER_BOUND('',#21014,.T.) ;
#16741 = FACE_OUTER_BOUND('',#21015,.T.) ;
#16742 = FACE_OUTER_BOUND('',#21016,.T.) ;
#16743 = FACE_OUTER_BOUND('',#21017,.T.) ;
#16744 = FACE_OUTER_BOUND('',#21018,.T.) ;
#16745 = FACE_OUTER_BOUND('',#21019,.T.) ;
#16746 = FACE_OUTER_BOUND('',#21020,.T.) ;
#16747 = FACE_OUTER_BOUND('',#21021,.T.) ;
#16748 = FACE_OUTER_BOUND('',#21022,.T.) ;
#16749 = FACE_OUTER_BOUND('',#21023,.T.) ;
#16750 = FACE_OUTER_BOUND('',#21024,.T.) ;
#16751 = FACE_OUTER_BOUND('',#21025,.T.) ;
#16752 = FACE_OUTER_BOUND('',#21026,.T.) ;
#16753 = FACE_OUTER_BOUND('',#21027,.T.) ;
#16754 = FACE_OUTER_BOUND('',#21028,.T.) ;
#16755 = FACE_OUTER_BOUND('',#21029,.T.) ;
#16756 = FACE_OUTER_BOUND('',#21030,.T.) ;
#16757 = FACE_OUTER_BOUND('',#21031,.T.) ;
#16758 = FACE_OUTER_BOUND('',#21032,.T.) ;
#16759 = FACE_OUTER_BOUND('',#21033,.T.) ;
#16760 = FACE_OUTER_BOUND('',#21034,.T.) ;
#16761 = FACE_OUTER_BOUND('',#21035,.T.) ;
#16762 = FACE_OUTER_BOUND('',#21036,.T.) ;
#16763 = FACE_OUTER_BOUND('',#21037,.T.) ;
#16764 = FACE_OUTER_BOUND('',#21038,.T.) ;
#16765 = FACE_OUTER_BOUND('',#21039,.T.) ;
#16766 = FACE_OUTER_BOUND('',#21040,.T.) ;
#16767 = FACE_OUTER_BOUND('',#21041,.T.) ;
#16768 = FACE_OUTER_BOUND('',#21042,.T.) ;
#16769 = FACE_OUTER_BOUND('',#21043,.T.) ;
#16770 = FACE_OUTER_BOUND('',#21044,.T.) ;
#16771 = FACE_OUTER_BOUND('',#21045,.T.) ;
#16772 = FACE_OUTER_BOUND('',#21046,.T.) ;
#16773 = FACE_OUTER_BOUND('',#21047,.T.) ;
#16774 = FACE_OUTER_BOUND('',#21048,.T.) ;
#16775 = FACE_OUTER_BOUND('',#21049,.T.) ;
#16776 = FACE_OUTER_BOUND('',#21050,.T.) ;
#16777 = FACE_OUTER_BOUND('',#21051,.T.) ;
#16778 = FACE_OUTER_BOUND('',#21052,.T.) ;
#16779 = FACE_OUTER_BOUND('',#21053,.T.) ;
#16780 = FACE_OUTER_BOUND('',#21054,.T.) ;
#16781 = FACE_OUTER_BOUND('',#21055,.T.) ;
#16782 = FACE_OUTER_BOUND('',#21056,.T.) ;
#16783 = FACE_OUTER_BOUND('',#21057,.T.) ;
#16784 = FACE_OUTER_BOUND('',#21058,.T.) ;
#16785 = FACE_OUTER_BOUND('',#21059,.T.) ;
#16786 = FACE_OUTER_BOUND('',#21060,.T.) ;
#16787 = FACE_OUTER_BOUND('',#21061,.T.) ;
#16788 = FACE_OUTER_BOUND('',#21062,.T.) ;
#16789 = FACE_OUTER_BOUND('',#21063,.T.) ;
#16790 = FACE_OUTER_BOUND('',#21064,.T.) ;
#16791 = FACE_OUTER_BOUND('',#21065,.T.) ;
#16792 = FACE_OUTER_BOUND('',#21066,.T.) ;
#16793 = FACE_OUTER_BOUND('',#21067,.T.) ;
#16794 = FACE_OUTER_BOUND('',#21068,.T.) ;
#16795 = FACE_OUTER_BOUND('',#21069,.T.) ;
#16796 = FACE_OUTER_BOUND('',#21070,.T.) ;
#16797 = FACE_OUTER_BOUND('',#21071,.T.) ;
#16798 = FACE_OUTER_BOUND('',#21072,.T.) ;
#16799 = FACE_OUTER_BOUND('',#21073,.T.) ;
#16800 = FACE_OUTER_BOUND('',#21074,.T.) ;
#16801 = FACE_OUTER_BOUND('',#21075,.T.) ;
#16802 = FACE_OUTER_BOUND('',#21076,.T.) ;
#16803 = FACE_OUTER_BOUND('',#21077,.T.) ;
#16804 = FACE_OUTER_BOUND('',#21078,.T.) ;
#16805 = FACE_OUTER_BOUND('',#21079,.T.) ;
#16806 = FACE_OUTER_BOUND('',#21080,.T.) ;
#16807 = FACE_OUTER_BOUND('',#21081,.T.) ;
#16808 = FACE_OUTER_BOUND('',#21082,.T.) ;
#16809 = FACE_OUTER_BOUND('',#21083,.T.) ;
#16810 = FACE_OUTER_BOUND('',#21084,.T.) ;
#16811 = FACE_OUTER_BOUND('',#21085,.T.) ;
#16812 = FACE_OUTER_BOUND('',#21086,.T.) ;
#16813 = FACE_OUTER_BOUND('',#21087,.T.) ;
#16814 = FACE_OUTER_BOUND('',#21088,.T.) ;
#16815 = FACE_OUTER_BOUND('',#21089,.T.) ;
#16816 = FACE_OUTER_BOUND('',#21090,.T.) ;
#16817 = FACE_OUTER_BOUND('',#21091,.T.) ;
#16818 = FACE_OUTER_BOUND('',#21092,.T.) ;
#16819 = FACE_OUTER_BOUND('',#21093,.T.) ;
#16820 = FACE_OUTER_BOUND('',#21094,.T.) ;
#16821 = FACE_OUTER_BOUND('',#21095,.T.) ;
#16822 = FACE_OUTER_BOUND('',#21096,.T.) ;
#16823 = FACE_OUTER_BOUND('',#21097,.T.) ;
#16824 = FACE_OUTER_BOUND('',#21098,.T.) ;
#16825 = FACE_OUTER_BOUND('',#21099,.T.) ;
#16826 = FACE_OUTER_BOUND('',#21100,.T.) ;
#16827 = FACE_OUTER_BOUND('',#21101,.T.) ;
#16828 = FACE_OUTER_BOUND('',#21102,.T.) ;
#16829 = FACE_OUTER_BOUND('',#21103,.T.) ;
#16830 = FACE_OUTER_BOUND('',#21104,.T.) ;
#16831 = FACE_OUTER_BOUND('',#21105,.T.) ;
#16832 = FACE_OUTER_BOUND('',#21106,.T.) ;
#16833 = FACE_OUTER_BOUND('',#21107,.T.) ;
#16834 = FACE_OUTER_BOUND('',#21108,.T.) ;
#16835 = FACE_OUTER_BOUND('',#21109,.T.) ;
#16836 = FACE_OUTER_BOUND('',#21110,.T.) ;
#16837 = FACE_OUTER_BOUND('',#21111,.T.) ;
#16838 = FACE_OUTER_BOUND('',#21112,.T.) ;
#16839 = FACE_OUTER_BOUND('',#21113,.T.) ;
#16840 = FACE_OUTER_BOUND('',#21114,.T.) ;
#16841 = FACE_OUTER_BOUND('',#21115,.T.) ;
#16842 = FACE_OUTER_BOUND('',#21116,.T.) ;
#16843 = FACE_OUTER_BOUND('',#21117,.T.) ;
#16844 = FACE_OUTER_BOUND('',#21118,.T.) ;
#16845 = FACE_OUTER_BOUND('',#21119,.T.) ;
#16846 = FACE_OUTER_BOUND('',#21120,.T.) ;
#16847 = FACE_OUTER_BOUND('',#21121,.T.) ;
#16848 = FACE_OUTER_BOUND('',#21122,.T.) ;
#16849 = FACE_OUTER_BOUND('',#21123,.T.) ;
#16850 = FACE_OUTER_BOUND('',#21124,.T.) ;
#16851 = FACE_OUTER_BOUND('',#21125,.T.) ;
#16852 = FACE_OUTER_BOUND('',#21126,.T.) ;
#16853 = FACE_OUTER_BOUND('',#21127,.T.) ;
#16854 = FACE_OUTER_BOUND('',#21128,.T.) ;
#16855 = FACE_OUTER_BOUND('',#21129,.T.) ;
#16856 = FACE_OUTER_BOUND('',#21130,.T.) ;
#16857 = FACE_OUTER_BOUND('',#21131,.T.) ;
#16858 = FACE_OUTER_BOUND('',#21132,.T.) ;
#16859 = FACE_OUTER_BOUND('',#21133,.T.) ;
#16860 = FACE_OUTER_BOUND('',#21134,.T.) ;
#16861 = FACE_OUTER_BOUND('',#21135,.T.) ;
#16862 = FACE_OUTER_BOUND('',#21136,.T.) ;
#16863 = FACE_OUTER_BOUND('',#21137,.T.) ;
#16864 = FACE_OUTER_BOUND('',#21138,.T.) ;
#16865 = FACE_OUTER_BOUND('',#21139,.T.) ;
#16866 = FACE_OUTER_BOUND('',#21140,.T.) ;
#16867 = FACE_OUTER_BOUND('',#21141,.T.) ;
#16868 = FACE_OUTER_BOUND('',#21142,.T.) ;
#16869 = FACE_OUTER_BOUND('',#21143,.T.) ;
#16870 = FACE_OUTER_BOUND('',#21144,.T.) ;
#16871 = FACE_OUTER_BOUND('',#21145,.T.) ;
#16872 = FACE_OUTER_BOUND('',#21146,.T.) ;
#16873 = FACE_OUTER_BOUND('',#21147,.T.) ;
#16874 = FACE_OUTER_BOUND('',#21148,.T.) ;
#16875 = FACE_OUTER_BOUND('',#21149,.T.) ;
#16876 = FACE_OUTER_BOUND('',#21150,.T.) ;
#16877 = FACE_OUTER_BOUND('',#21151,.T.) ;
#16878 = FACE_OUTER_BOUND('',#21152,.T.) ;
#16879 = FACE_OUTER_BOUND('',#21153,.T.) ;
#16880 = FACE_OUTER_BOUND('',#21154,.T.) ;
#16881 = FACE_OUTER_BOUND('',#21155,.T.) ;
#16882 = FACE_OUTER_BOUND('',#21156,.T.) ;
#16883 = FACE_OUTER_BOUND('',#21157,.T.) ;
#16884 = FACE_OUTER_BOUND('',#21158,.T.) ;
#16885 = FACE_OUTER_BOUND('',#21159,.T.) ;
#16886 = FACE_OUTER_BOUND('',#21160,.T.) ;
#16887 = FACE_OUTER_BOUND('',#21161,.T.) ;
#16888 = FACE_OUTER_BOUND('',#21162,.T.) ;
#16889 = FACE_OUTER_BOUND('',#21163,.T.) ;
#16890 = FACE_OUTER_BOUND('',#21164,.T.) ;
#16891 = FACE_OUTER_BOUND('',#21165,.T.) ;
#16892 = FACE_OUTER_BOUND('',#21166,.T.) ;
#16893 = FACE_OUTER_BOUND('',#21167,.T.) ;
#16894 = FACE_OUTER_BOUND('',#21168,.T.) ;
#16895 = FACE_OUTER_BOUND('',#21169,.T.) ;
#16896 = FACE_OUTER_BOUND('',#21170,.T.) ;
#16897 = FACE_OUTER_BOUND('',#21171,.T.) ;
#16898 = FACE_OUTER_BOUND('',#21172,.T.) ;
#16899 = FACE_OUTER_BOUND('',#21173,.T.) ;
#16900 = FACE_OUTER_BOUND('',#21174,.T.) ;
#16901 = FACE_OUTER_BOUND('',#21175,.T.) ;
#16902 = FACE_OUTER_BOUND('',#21176,.T.) ;
#16903 = FACE_OUTER_BOUND('',#21177,.T.) ;
#16904 = FACE_OUTER_BOUND('',#21178,.T.) ;
#16905 = FACE_OUTER_BOUND('',#21179,.T.) ;
#16906 = FACE_OUTER_BOUND('',#21180,.T.) ;
#16907 = FACE_OUTER_BOUND('',#21181,.T.) ;
#16908 = FACE_OUTER_BOUND('',#21182,.T.) ;
#16909 = FACE_OUTER_BOUND('',#21183,.T.) ;
#16910 = FACE_OUTER_BOUND('',#21184,.T.) ;
#16911 = FACE_OUTER_BOUND('',#21185,.T.) ;
#16912 = FACE_OUTER_BOUND('',#21186,.T.) ;
#16913 = FACE_OUTER_BOUND('',#21187,.T.) ;
#16914 = FACE_OUTER_BOUND('',#21188,.T.) ;
#16915 = FACE_OUTER_BOUND('',#21189,.T.) ;
#16916 = FACE_OUTER_BOUND('',#21190,.T.) ;
#16917 = FACE_OUTER_BOUND('',#21191,.T.) ;
#16918 = FACE_OUTER_BOUND('',#21192,.T.) ;
#16919 = FACE_OUTER_BOUND('',#21193,.T.) ;
#16920 = FACE_OUTER_BOUND('',#21194,.T.) ;
#16921 = FACE_OUTER_BOUND('',#21195,.T.) ;
#16922 = FACE_OUTER_BOUND('',#21196,.T.) ;
#16923 = FACE_OUTER_BOUND('',#21197,.T.) ;
#16924 = FACE_OUTER_BOUND('',#21198,.T.) ;
#16925 = FACE_OUTER_BOUND('',#21200,.T.) ;
#16926 = FACE_OUTER_BOUND('',#21201,.T.) ;
#16927 = FACE_OUTER_BOUND('',#21202,.T.) ;
#16928 = FACE_OUTER_BOUND('',#21203,.T.) ;
#16929 = FACE_OUTER_BOUND('',#21204,.T.) ;
#16930 = FACE_OUTER_BOUND('',#21205,.T.) ;
#16931 = FACE_OUTER_BOUND('',#21206,.T.) ;
#16932 = FACE_OUTER_BOUND('',#21207,.T.) ;
#16933 = FACE_OUTER_BOUND('',#21208,.T.) ;
#16934 = FACE_OUTER_BOUND('',#21209,.T.) ;
#16935 = FACE_OUTER_BOUND('',#21210,.T.) ;
#16936 = FACE_OUTER_BOUND('',#21212,.T.) ;
#16937 = FACE_OUTER_BOUND('',#21213,.T.) ;
#16938 = FACE_OUTER_BOUND('',#21214,.T.) ;
#16939 = FACE_OUTER_BOUND('',#21215,.T.) ;
#16940 = FACE_OUTER_BOUND('',#21216,.T.) ;
#16941 = FACE_OUTER_BOUND('',#21217,.T.) ;
#16942 = FACE_OUTER_BOUND('',#21218,.T.) ;
#16943 = FACE_OUTER_BOUND('',#21219,.T.) ;
#16944 = FACE_OUTER_BOUND('',#21220,.T.) ;
#16945 = FACE_OUTER_BOUND('',#21221,.T.) ;
#16946 = FACE_OUTER_BOUND('',#21222,.T.) ;
#16947 = FACE_OUTER_BOUND('',#21223,.T.) ;
#16948 = FACE_OUTER_BOUND('',#21224,.T.) ;
#16949 = FACE_OUTER_BOUND('',#21225,.T.) ;
#16950 = FACE_OUTER_BOUND('',#21226,.T.) ;
#16951 = FACE_OUTER_BOUND('',#21227,.T.) ;
#16952 = FACE_OUTER_BOUND('',#21228,.T.) ;
#16953 = FACE_OUTER_BOUND('',#21229,.T.) ;
#16954 = FACE_OUTER_BOUND('',#21230,.T.) ;
#16955 = FACE_OUTER_BOUND('',#21231,.T.) ;
#16956 = FACE_OUTER_BOUND('',#21232,.T.) ;
#16957 = FACE_OUTER_BOUND('',#21233,.T.) ;
#16958 = FACE_OUTER_BOUND('',#21234,.T.) ;
#16959 = FACE_OUTER_BOUND('',#21235,.T.) ;
#16960 = FACE_OUTER_BOUND('',#21236,.T.) ;
#16961 = FACE_OUTER_BOUND('',#21237,.T.) ;
#16962 = FACE_OUTER_BOUND('',#21238,.T.) ;
#16963 = FACE_OUTER_BOUND('',#21239,.T.) ;
#16964 = FACE_OUTER_BOUND('',#21240,.T.) ;
#16965 = FACE_OUTER_BOUND('',#21241,.T.) ;
#16966 = FACE_OUTER_BOUND('',#21242,.T.) ;
#16967 = FACE_OUTER_BOUND('',#21243,.T.) ;
#16968 = FACE_OUTER_BOUND('',#21244,.T.) ;
#16969 = FACE_OUTER_BOUND('',#21245,.T.) ;
#16970 = FACE_OUTER_BOUND('',#21246,.T.) ;
#16971 = FACE_OUTER_BOUND('',#21247,.T.) ;
#16972 = FACE_OUTER_BOUND('',#21248,.T.) ;
#16973 = FACE_OUTER_BOUND('',#21249,.T.) ;
#16974 = FACE_OUTER_BOUND('',#21250,.T.) ;
#16975 = FACE_OUTER_BOUND('',#21251,.T.) ;
#16976 = FACE_OUTER_BOUND('',#21252,.T.) ;
#16977 = FACE_OUTER_BOUND('',#21253,.T.) ;
#16978 = FACE_OUTER_BOUND('',#21254,.T.) ;
#16979 = FACE_OUTER_BOUND('',#21255,.T.) ;
#16980 = FACE_OUTER_BOUND('',#21256,.T.) ;
#16981 = FACE_OUTER_BOUND('',#21257,.T.) ;
#16982 = FACE_OUTER_BOUND('',#21258,.T.) ;
#16983 = FACE_OUTER_BOUND('',#21259,.T.) ;
#16984 = FACE_OUTER_BOUND('',#21260,.T.) ;
#16985 = FACE_OUTER_BOUND('',#21261,.T.) ;
#16986 = FACE_OUTER_BOUND('',#21262,.T.) ;
#16987 = FACE_OUTER_BOUND('',#21263,.T.) ;
#16988 = FACE_OUTER_BOUND('',#21264,.T.) ;
#16989 = FACE_OUTER_BOUND('',#21265,.T.) ;
#16990 = FACE_OUTER_BOUND('',#21266,.T.) ;
#16991 = FACE_OUTER_BOUND('',#21267,.T.) ;
#16992 = FACE_OUTER_BOUND('',#21268,.T.) ;
#16993 = FACE_OUTER_BOUND('',#21269,.T.) ;
#16994 = FACE_OUTER_BOUND('',#21270,.T.) ;
#16995 = FACE_OUTER_BOUND('',#21271,.T.) ;
#16996 = FACE_OUTER_BOUND('',#21272,.T.) ;
#16997 = FACE_OUTER_BOUND('',#21273,.T.) ;
#16998 = FACE_OUTER_BOUND('',#21274,.T.) ;
#16999 = FACE_OUTER_BOUND('',#21275,.T.) ;
#17000 = FACE_OUTER_BOUND('',#21276,.T.) ;
#17001 = FACE_OUTER_BOUND('',#21277,.T.) ;
#17002 = FACE_OUTER_BOUND('',#21278,.T.) ;
#17003 = FACE_OUTER_BOUND('',#21279,.T.) ;
#17004 = FACE_OUTER_BOUND('',#21280,.T.) ;
#17005 = FACE_OUTER_BOUND('',#21281,.T.) ;
#17006 = FACE_OUTER_BOUND('',#21282,.T.) ;
#17007 = FACE_OUTER_BOUND('',#21283,.T.) ;
#17008 = FACE_OUTER_BOUND('',#21284,.T.) ;
#17009 = FACE_OUTER_BOUND('',#21285,.T.) ;
#17010 = FACE_OUTER_BOUND('',#21286,.T.) ;
#17011 = FACE_OUTER_BOUND('',#21287,.T.) ;
#17012 = FACE_OUTER_BOUND('',#21288,.T.) ;
#17013 = FACE_OUTER_BOUND('',#21289,.T.) ;
#17014 = FACE_OUTER_BOUND('',#21290,.T.) ;
#17015 = FACE_OUTER_BOUND('',#21291,.T.) ;
#17016 = FACE_OUTER_BOUND('',#21292,.T.) ;
#17017 = FACE_OUTER_BOUND('',#21293,.T.) ;
#17018 = FACE_OUTER_BOUND('',#21294,.T.) ;
#17019 = FACE_OUTER_BOUND('',#21295,.T.) ;
#17020 = FACE_OUTER_BOUND('',#21296,.T.) ;
#17021 = FACE_OUTER_BOUND('',#21297,.T.) ;
#17022 = FACE_OUTER_BOUND('',#21298,.T.) ;
#17023 = FACE_OUTER_BOUND('',#21299,.T.) ;
#17024 = FACE_OUTER_BOUND('',#21300,.T.) ;
#17025 = FACE_OUTER_BOUND('',#21301,.T.) ;
#17026 = FACE_OUTER_BOUND('',#21302,.T.) ;
#17027 = FACE_OUTER_BOUND('',#21303,.T.) ;
#17028 = FACE_OUTER_BOUND('',#21304,.T.) ;
#17029 = FACE_OUTER_BOUND('',#21305,.T.) ;
#17030 = FACE_OUTER_BOUND('',#21306,.T.) ;
#17031 = FACE_OUTER_BOUND('',#21307,.T.) ;
#17032 = FACE_OUTER_BOUND('',#21308,.T.) ;
#17033 = FACE_OUTER_BOUND('',#21309,.T.) ;
#17034 = FACE_OUTER_BOUND('',#21310,.T.) ;
#17035 = FACE_OUTER_BOUND('',#21311,.T.) ;
#17036 = FACE_OUTER_BOUND('',#21312,.T.) ;
#17037 = FACE_OUTER_BOUND('',#21313,.T.) ;
#17038 = FACE_OUTER_BOUND('',#21314,.T.) ;
#17039 = FACE_OUTER_BOUND('',#21315,.T.) ;
#17040 = FACE_OUTER_BOUND('',#21316,.T.) ;
#17041 = FACE_OUTER_BOUND('',#21317,.T.) ;
#17042 = FACE_OUTER_BOUND('',#21318,.T.) ;
#17043 = FACE_OUTER_BOUND('',#21319,.T.) ;
#17044 = FACE_OUTER_BOUND('',#21320,.T.) ;
#17045 = FACE_OUTER_BOUND('',#21321,.T.) ;
#17046 = FACE_OUTER_BOUND('',#21322,.T.) ;
#17047 = FACE_OUTER_BOUND('',#21323,.T.) ;
#17048 = FACE_OUTER_BOUND('',#21324,.T.) ;
#17049 = FACE_OUTER_BOUND('',#21325,.T.) ;
#17050 = FACE_OUTER_BOUND('',#21326,.T.) ;
#17051 = FACE_OUTER_BOUND('',#21327,.T.) ;
#17052 = FACE_OUTER_BOUND('',#21328,.T.) ;
#17053 = FACE_OUTER_BOUND('',#21329,.T.) ;
#17054 = FACE_OUTER_BOUND('',#21330,.T.) ;
#17055 = FACE_OUTER_BOUND('',#21331,.T.) ;
#17056 = FACE_OUTER_BOUND('',#21332,.T.) ;
#17057 = FACE_OUTER_BOUND('',#21333,.T.) ;
#17058 = FACE_OUTER_BOUND('',#21334,.T.) ;
#17059 = FACE_OUTER_BOUND('',#21335,.T.) ;
#17060 = FACE_OUTER_BOUND('',#21336,.T.) ;
#17061 = FACE_OUTER_BOUND('',#21337,.T.) ;
#17062 = FACE_OUTER_BOUND('',#21338,.T.) ;
#17063 = FACE_OUTER_BOUND('',#21339,.T.) ;
#17064 = FACE_OUTER_BOUND('',#21340,.T.) ;
#17065 = FACE_OUTER_BOUND('',#21341,.T.) ;
#17066 = FACE_OUTER_BOUND('',#21342,.T.) ;
#17067 = FACE_OUTER_BOUND('',#21343,.T.) ;
#17068 = FACE_OUTER_BOUND('',#21344,.T.) ;
#17069 = FACE_OUTER_BOUND('',#21345,.T.) ;
#17070 = FACE_OUTER_BOUND('',#21346,.T.) ;
#17071 = FACE_OUTER_BOUND('',#21347,.T.) ;
#17072 = FACE_OUTER_BOUND('',#21348,.T.) ;
#17073 = FACE_OUTER_BOUND('',#21349,.T.) ;
#17074 = FACE_OUTER_BOUND('',#21350,.T.) ;
#17075 = FACE_OUTER_BOUND('',#21351,.T.) ;
#17076 = FACE_OUTER_BOUND('',#21352,.T.) ;
#17077 = FACE_OUTER_BOUND('',#21353,.T.) ;
#17078 = FACE_OUTER_BOUND('',#21354,.T.) ;
#17079 = FACE_OUTER_BOUND('',#21355,.T.) ;
#17080 = FACE_OUTER_BOUND('',#21356,.T.) ;
#17081 = FACE_OUTER_BOUND('',#21357,.T.) ;
#17082 = FACE_OUTER_BOUND('',#21358,.T.) ;
#17083 = FACE_OUTER_BOUND('',#21359,.T.) ;
#17084 = FACE_OUTER_BOUND('',#21360,.T.) ;
#17085 = FACE_OUTER_BOUND('',#21361,.T.) ;
#17086 = FACE_OUTER_BOUND('',#21362,.T.) ;
#17087 = FACE_OUTER_BOUND('',#21363,.T.) ;
#17088 = FACE_OUTER_BOUND('',#21364,.T.) ;
#17089 = FACE_OUTER_BOUND('',#21365,.T.) ;
#17090 = FACE_OUTER_BOUND('',#21366,.T.) ;
#17091 = FACE_OUTER_BOUND('',#21367,.T.) ;
#17092 = FACE_OUTER_BOUND('',#21368,.T.) ;
#17093 = FACE_OUTER_BOUND('',#21369,.T.) ;
#17094 = FACE_OUTER_BOUND('',#21370,.T.) ;
#17095 = FACE_OUTER_BOUND('',#21371,.T.) ;
#17096 = FACE_OUTER_BOUND('',#21372,.T.) ;
#17097 = FACE_OUTER_BOUND('',#21373,.T.) ;
#17098 = FACE_OUTER_BOUND('',#21374,.T.) ;
#17099 = FACE_OUTER_BOUND('',#21375,.T.) ;
#17100 = FACE_OUTER_BOUND('',#21376,.T.) ;
#17101 = FACE_OUTER_BOUND('',#21377,.T.) ;
#17102 = FACE_OUTER_BOUND('',#21378,.T.) ;
#17103 = FACE_OUTER_BOUND('',#21379,.T.) ;
#17104 = FACE_OUTER_BOUND('',#21380,.T.) ;
#17105 = FACE_OUTER_BOUND('',#21381,.T.) ;
#17106 = FACE_OUTER_BOUND('',#21382,.T.) ;
#17107 = FACE_OUTER_BOUND('',#21383,.T.) ;
#17108 = FACE_OUTER_BOUND('',#21384,.T.) ;
#17109 = FACE_OUTER_BOUND('',#21385,.T.) ;
#17110 = FACE_OUTER_BOUND('',#21386,.T.) ;
#17111 = FACE_OUTER_BOUND('',#21387,.T.) ;
#17112 = FACE_OUTER_BOUND('',#21388,.T.) ;
#17113 = FACE_OUTER_BOUND('',#21389,.T.) ;
#17114 = FACE_OUTER_BOUND('',#21390,.T.) ;
#17115 = FACE_OUTER_BOUND('',#21391,.T.) ;
#17116 = FACE_OUTER_BOUND('',#21392,.T.) ;
#17117 = FACE_OUTER_BOUND('',#21393,.T.) ;
#17118 = FACE_OUTER_BOUND('',#21394,.T.) ;
#17119 = FACE_OUTER_BOUND('',#21395,.T.) ;
#17120 = FACE_OUTER_BOUND('',#21396,.T.) ;
#17121 = FACE_OUTER_BOUND('',#21397,.T.) ;
#17122 = FACE_OUTER_BOUND('',#21398,.T.) ;
#17123 = FACE_OUTER_BOUND('',#21399,.T.) ;
#17124 = FACE_OUTER_BOUND('',#21400,.T.) ;
#17125 = FACE_OUTER_BOUND('',#21401,.T.) ;
#17126 = FACE_OUTER_BOUND('',#21402,.T.) ;
#17127 = FACE_OUTER_BOUND('',#21403,.T.) ;
#17128 = FACE_OUTER_BOUND('',#21404,.T.) ;
#17129 = FACE_OUTER_BOUND('',#21405,.T.) ;
#17130 = FACE_OUTER_BOUND('',#21406,.T.) ;
#17131 = FACE_OUTER_BOUND('',#21407,.T.) ;
#17132 = FACE_OUTER_BOUND('',#21408,.T.) ;
#17133 = FACE_OUTER_BOUND('',#21409,.T.) ;
#17134 = FACE_OUTER_BOUND('',#21410,.T.) ;
#17135 = FACE_OUTER_BOUND('',#21411,.T.) ;
#17136 = FACE_OUTER_BOUND('',#21412,.T.) ;
#17137 = FACE_OUTER_BOUND('',#21413,.T.) ;
#17138 = FACE_OUTER_BOUND('',#21414,.T.) ;
#17139 = FACE_OUTER_BOUND('',#21415,.T.) ;
#17140 = FACE_OUTER_BOUND('',#21416,.T.) ;
#17141 = FACE_OUTER_BOUND('',#21417,.T.) ;
#17142 = FACE_OUTER_BOUND('',#21418,.T.) ;
#17143 = FACE_OUTER_BOUND('',#21419,.T.) ;
#17144 = FACE_OUTER_BOUND('',#21420,.T.) ;
#17145 = FACE_OUTER_BOUND('',#21421,.T.) ;
#17146 = FACE_OUTER_BOUND('',#21422,.T.) ;
#17147 = FACE_OUTER_BOUND('',#21423,.T.) ;
#17148 = FACE_OUTER_BOUND('',#21424,.T.) ;
#17149 = FACE_OUTER_BOUND('',#21425,.T.) ;
#17150 = FACE_OUTER_BOUND('',#21426,.T.) ;
#17151 = FACE_OUTER_BOUND('',#21427,.T.) ;
#17152 = FACE_OUTER_BOUND('',#21428,.T.) ;
#17153 = FACE_OUTER_BOUND('',#21429,.T.) ;
#17154 = FACE_OUTER_BOUND('',#21430,.T.) ;
#17155 = FACE_OUTER_BOUND('',#21431,.T.) ;
#17156 = FACE_OUTER_BOUND('',#21432,.T.) ;
#17157 = FACE_OUTER_BOUND('',#21433,.T.) ;
#17158 = FACE_OUTER_BOUND('',#21434,.T.) ;
#17159 = FACE_OUTER_BOUND('',#21435,.T.) ;
#17160 = FACE_OUTER_BOUND('',#21436,.T.) ;
#17161 = FACE_OUTER_BOUND('',#21437,.T.) ;
#17162 = FACE_OUTER_BOUND('',#21438,.T.) ;
#17163 = FACE_OUTER_BOUND('',#21439,.T.) ;
#17164 = FACE_OUTER_BOUND('',#21440,.T.) ;
#17165 = FACE_OUTER_BOUND('',#21441,.T.) ;
#17166 = FACE_OUTER_BOUND('',#21442,.T.) ;
#17167 = FACE_OUTER_BOUND('',#21443,.T.) ;
#17168 = FACE_OUTER_BOUND('',#21444,.T.) ;
#17169 = FACE_OUTER_BOUND('',#21445,.T.) ;
#17170 = FACE_OUTER_BOUND('',#21446,.T.) ;
#17171 = FACE_OUTER_BOUND('',#21447,.T.) ;
#17172 = FACE_OUTER_BOUND('',#21448,.T.) ;
#17173 = FACE_OUTER_BOUND('',#21449,.T.) ;
#17174 = FACE_OUTER_BOUND('',#21450,.T.) ;
#17175 = FACE_OUTER_BOUND('',#21451,.T.) ;
#17176 = FACE_OUTER_BOUND('',#21452,.T.) ;
#17177 = FACE_OUTER_BOUND('',#21453,.T.) ;
#17178 = FACE_OUTER_BOUND('',#21454,.T.) ;
#17179 = FACE_OUTER_BOUND('',#21455,.T.) ;
#17180 = FACE_OUTER_BOUND('',#21456,.T.) ;
#17181 = FACE_OUTER_BOUND('',#21457,.T.) ;
#17182 = FACE_OUTER_BOUND('',#21458,.T.) ;
#17183 = FACE_OUTER_BOUND('',#21459,.T.) ;
#17184 = FACE_OUTER_BOUND('',#21460,.T.) ;
#17185 = FACE_OUTER_BOUND('',#21461,.T.) ;
#17186 = FACE_OUTER_BOUND('',#21462,.T.) ;
#17187 = FACE_OUTER_BOUND('',#21463,.T.) ;
#17188 = FACE_OUTER_BOUND('',#21464,.T.) ;
#17189 = FACE_OUTER_BOUND('',#21465,.T.) ;
#17190 = FACE_OUTER_BOUND('',#21466,.T.) ;
#17191 = FACE_OUTER_BOUND('',#21467,.T.) ;
#17192 = FACE_OUTER_BOUND('',#21468,.T.) ;
#17193 = FACE_OUTER_BOUND('',#21469,.T.) ;
#17194 = FACE_OUTER_BOUND('',#21470,.T.) ;
#17195 = FACE_OUTER_BOUND('',#21471,.T.) ;
#17196 = FACE_OUTER_BOUND('',#21472,.T.) ;
#17197 = FACE_OUTER_BOUND('',#21473,.T.) ;
#17198 = FACE_OUTER_BOUND('',#21474,.T.) ;
#17199 = FACE_OUTER_BOUND('',#21475,.T.) ;
#17200 = FACE_OUTER_BOUND('',#21476,.T.) ;
#17201 = FACE_OUTER_BOUND('',#21477,.T.) ;
#17202 = FACE_OUTER_BOUND('',#21478,.T.) ;
#17203 = FACE_OUTER_BOUND('',#21479,.T.) ;
#17204 = FACE_OUTER_BOUND('',#21480,.T.) ;
#17205 = FACE_OUTER_BOUND('',#21481,.T.) ;
#17206 = FACE_OUTER_BOUND('',#21482,.T.) ;
#17207 = FACE_OUTER_BOUND('',#21483,.T.) ;
#17208 = FACE_OUTER_BOUND('',#21484,.T.) ;
#17209 = FACE_OUTER_BOUND('',#21485,.T.) ;
#17210 = FACE_OUTER_BOUND('',#21486,.T.) ;
#17211 = FACE_OUTER_BOUND('',#21487,.T.) ;
#17212 = FACE_OUTER_BOUND('',#21488,.T.) ;
#17213 = FACE_OUTER_BOUND('',#21489,.T.) ;
#17214 = FACE_OUTER_BOUND('',#21491,.T.) ;
#17215 = FACE_OUTER_BOUND('',#21492,.T.) ;
#17216 = FACE_OUTER_BOUND('',#21493,.T.) ;
#17217 = FACE_OUTER_BOUND('',#21494,.T.) ;
#17218 = FACE_OUTER_BOUND('',#21495,.T.) ;
#17219 = FACE_OUTER_BOUND('',#21496,.T.) ;
#17220 = FACE_OUTER_BOUND('',#21497,.T.) ;
#17221 = FACE_OUTER_BOUND('',#21498,.T.) ;
#17222 = FACE_OUTER_BOUND('',#21499,.T.) ;
#17223 = FACE_OUTER_BOUND('',#21500,.T.) ;
#17224 = FACE_OUTER_BOUND('',#21501,.T.) ;
#17225 = FACE_OUTER_BOUND('',#21503,.T.) ;
#17226 = FACE_OUTER_BOUND('',#21504,.T.) ;
#17227 = FACE_OUTER_BOUND('',#21505,.T.) ;
#17228 = FACE_OUTER_BOUND('',#21506,.T.) ;
#17229 = FACE_OUTER_BOUND('',#21507,.T.) ;
#17230 = FACE_OUTER_BOUND('',#21508,.T.) ;
#17231 = FACE_OUTER_BOUND('',#21509,.T.) ;
#17232 = FACE_OUTER_BOUND('',#21510,.T.) ;
#17233 = FACE_OUTER_BOUND('',#21511,.T.) ;
#17234 = FACE_OUTER_BOUND('',#21512,.T.) ;
#17235 = FACE_OUTER_BOUND('',#21513,.T.) ;
#17236 = FACE_OUTER_BOUND('',#21514,.T.) ;
#17237 = FACE_OUTER_BOUND('',#21515,.T.) ;
#17238 = FACE_OUTER_BOUND('',#21516,.T.) ;
#17239 = FACE_OUTER_BOUND('',#21517,.T.) ;
#17240 = FACE_OUTER_BOUND('',#21518,.T.) ;
#17241 = FACE_OUTER_BOUND('',#21519,.T.) ;
#17242 = FACE_OUTER_BOUND('',#21520,.T.) ;
#17243 = FACE_OUTER_BOUND('',#21521,.T.) ;
#17244 = FACE_OUTER_BOUND('',#21522,.T.) ;
#17245 = FACE_OUTER_BOUND('',#21523,.T.) ;
#17246 = FACE_OUTER_BOUND('',#21524,.T.) ;
#17247 = FACE_OUTER_BOUND('',#21525,.T.) ;
#17248 = FACE_OUTER_BOUND('',#21526,.T.) ;
#17249 = FACE_OUTER_BOUND('',#21527,.T.) ;
#17250 = FACE_OUTER_BOUND('',#21528,.T.) ;
#17251 = FACE_OUTER_BOUND('',#21529,.T.) ;
#17252 = FACE_OUTER_BOUND('',#21530,.T.) ;
#17253 = FACE_OUTER_BOUND('',#21531,.T.) ;
#17254 = FACE_OUTER_BOUND('',#21532,.T.) ;
#17255 = FACE_OUTER_BOUND('',#21533,.T.) ;
#17256 = FACE_OUTER_BOUND('',#21534,.T.) ;
#17257 = FACE_OUTER_BOUND('',#21535,.T.) ;
#17258 = FACE_OUTER_BOUND('',#21536,.T.) ;
#17259 = FACE_OUTER_BOUND('',#21537,.T.) ;
#17260 = FACE_OUTER_BOUND('',#21538,.T.) ;
#17261 = FACE_OUTER_BOUND('',#21539,.T.) ;
#17262 = FACE_OUTER_BOUND('',#21540,.T.) ;
#17263 = FACE_OUTER_BOUND('',#21541,.T.) ;
#17264 = FACE_OUTER_BOUND('',#21542,.T.) ;
#17265 = FACE_OUTER_BOUND('',#21543,.T.) ;
#17266 = FACE_OUTER_BOUND('',#21544,.T.) ;
#17267 = FACE_OUTER_BOUND('',#21545,.T.) ;
#17268 = FACE_OUTER_BOUND('',#21546,.T.) ;
#17269 = FACE_OUTER_BOUND('',#21547,.T.) ;
#17270 = FACE_OUTER_BOUND('',#21548,.T.) ;
#17271 = FACE_OUTER_BOUND('',#21549,.T.) ;
#17272 = FACE_OUTER_BOUND('',#21550,.T.) ;
#17273 = FACE_OUTER_BOUND('',#21551,.T.) ;
#17274 = FACE_OUTER_BOUND('',#21552,.T.) ;
#17275 = FACE_OUTER_BOUND('',#21553,.T.) ;
#17276 = FACE_OUTER_BOUND('',#21554,.T.) ;
#17277 = FACE_OUTER_BOUND('',#21555,.T.) ;
#17278 = FACE_OUTER_BOUND('',#21556,.T.) ;
#17279 = FACE_OUTER_BOUND('',#21557,.T.) ;
#17280 = FACE_OUTER_BOUND('',#21558,.T.) ;
#17281 = FACE_OUTER_BOUND('',#21559,.T.) ;
#17282 = FACE_OUTER_BOUND('',#21560,.T.) ;
#17283 = FACE_OUTER_BOUND('',#21561,.T.) ;
#17284 = FACE_OUTER_BOUND('',#21562,.T.) ;
#17285 = FACE_OUTER_BOUND('',#21563,.T.) ;
#17286 = FACE_OUTER_BOUND('',#21564,.T.) ;
#17287 = FACE_OUTER_BOUND('',#21565,.T.) ;
#17288 = FACE_OUTER_BOUND('',#21566,.T.) ;
#17289 = FACE_OUTER_BOUND('',#21567,.T.) ;
#17290 = FACE_OUTER_BOUND('',#21568,.T.) ;
#17291 = FACE_OUTER_BOUND('',#21569,.T.) ;
#17292 = FACE_OUTER_BOUND('',#21570,.T.) ;
#17293 = FACE_OUTER_BOUND('',#21571,.T.) ;
#17294 = FACE_OUTER_BOUND('',#21572,.T.) ;
#17295 = FACE_OUTER_BOUND('',#21573,.T.) ;
#17296 = FACE_OUTER_BOUND('',#21574,.T.) ;
#17297 = FACE_OUTER_BOUND('',#21575,.T.) ;
#17298 = FACE_OUTER_BOUND('',#21576,.T.) ;
#17299 = FACE_OUTER_BOUND('',#21577,.T.) ;
#17300 = FACE_OUTER_BOUND('',#21578,.T.) ;
#17301 = FACE_OUTER_BOUND('',#21579,.T.) ;
#17302 = FACE_OUTER_BOUND('',#21580,.T.) ;
#17303 = FACE_OUTER_BOUND('',#21581,.T.) ;
#17304 = FACE_OUTER_BOUND('',#21582,.T.) ;
#17305 = FACE_OUTER_BOUND('',#21583,.T.) ;
#17306 = FACE_OUTER_BOUND('',#21584,.T.) ;
#17307 = FACE_OUTER_BOUND('',#21585,.T.) ;
#17308 = FACE_OUTER_BOUND('',#21586,.T.) ;
#17309 = FACE_OUTER_BOUND('',#21587,.T.) ;
#17310 = FACE_OUTER_BOUND('',#21588,.T.) ;
#17311 = FACE_OUTER_BOUND('',#21589,.T.) ;
#17312 = FACE_OUTER_BOUND('',#21590,.T.) ;
#17313 = FACE_OUTER_BOUND('',#21591,.T.) ;
#17314 = FACE_OUTER_BOUND('',#21592,.T.) ;
#17315 = FACE_OUTER_BOUND('',#21593,.T.) ;
#17316 = FACE_OUTER_BOUND('',#21594,.T.) ;
#17317 = FACE_OUTER_BOUND('',#21595,.T.) ;
#17318 = FACE_OUTER_BOUND('',#21596,.T.) ;
#17319 = FACE_OUTER_BOUND('',#21597,.T.) ;
#17320 = FACE_OUTER_BOUND('',#21598,.T.) ;
#17321 = FACE_OUTER_BOUND('',#21599,.T.) ;
#17322 = FACE_OUTER_BOUND('',#21600,.T.) ;
#17323 = FACE_OUTER_BOUND('',#21601,.T.) ;
#17324 = FACE_OUTER_BOUND('',#21602,.T.) ;
#17325 = FACE_OUTER_BOUND('',#21603,.T.) ;
#17326 = FACE_OUTER_BOUND('',#21604,.T.) ;
#17327 = FACE_OUTER_BOUND('',#21605,.T.) ;
#17328 = FACE_OUTER_BOUND('',#21606,.T.) ;
#17329 = FACE_OUTER_BOUND('',#21607,.T.) ;
#17330 = FACE_OUTER_BOUND('',#21608,.T.) ;
#17331 = FACE_OUTER_BOUND('',#21609,.T.) ;
#17332 = FACE_OUTER_BOUND('',#21610,.T.) ;
#17333 = FACE_OUTER_BOUND('',#21611,.T.) ;
#17334 = FACE_OUTER_BOUND('',#21612,.T.) ;
#17335 = FACE_OUTER_BOUND('',#21613,.T.) ;
#17336 = FACE_OUTER_BOUND('',#21614,.T.) ;
#17337 = FACE_OUTER_BOUND('',#21615,.T.) ;
#17338 = FACE_OUTER_BOUND('',#21616,.T.) ;
#17339 = FACE_OUTER_BOUND('',#21617,.T.) ;
#17340 = FACE_OUTER_BOUND('',#21618,.T.) ;
#17341 = FACE_OUTER_BOUND('',#21619,.T.) ;
#17342 = FACE_OUTER_BOUND('',#21620,.T.) ;
#17343 = FACE_OUTER_BOUND('',#21621,.T.) ;
#17344 = FACE_OUTER_BOUND('',#21622,.T.) ;
#17345 = FACE_OUTER_BOUND('',#21623,.T.) ;
#17346 = FACE_OUTER_BOUND('',#21624,.T.) ;
#17347 = FACE_OUTER_BOUND('',#21625,.T.) ;
#17348 = FACE_OUTER_BOUND('',#21626,.T.) ;
#17349 = FACE_OUTER_BOUND('',#21627,.T.) ;
#17350 = FACE_OUTER_BOUND('',#21628,.T.) ;
#17351 = FACE_OUTER_BOUND('',#21629,.T.) ;
#17352 = FACE_OUTER_BOUND('',#21630,.T.) ;
#17353 = FACE_OUTER_BOUND('',#21631,.T.) ;
#17354 = FACE_OUTER_BOUND('',#21632,.T.) ;
#17355 = FACE_OUTER_BOUND('',#21633,.T.) ;
#17356 = FACE_OUTER_BOUND('',#21634,.T.) ;
#17357 = FACE_OUTER_BOUND('',#21635,.T.) ;
#17358 = FACE_OUTER_BOUND('',#21636,.T.) ;
#17359 = FACE_OUTER_BOUND('',#21637,.T.) ;
#17360 = FACE_OUTER_BOUND('',#21638,.T.) ;
#17361 = FACE_OUTER_BOUND('',#21639,.T.) ;
#17362 = FACE_OUTER_BOUND('',#21640,.T.) ;
#17363 = FACE_OUTER_BOUND('',#21641,.T.) ;
#17364 = FACE_OUTER_BOUND('',#21642,.T.) ;
#17365 = FACE_OUTER_BOUND('',#21643,.T.) ;
#17366 = FACE_OUTER_BOUND('',#21644,.T.) ;
#17367 = FACE_OUTER_BOUND('',#21645,.T.) ;
#17368 = FACE_OUTER_BOUND('',#21646,.T.) ;
#17369 = FACE_OUTER_BOUND('',#21647,.T.) ;
#17370 = FACE_OUTER_BOUND('',#21648,.T.) ;
#17371 = FACE_OUTER_BOUND('',#21649,.T.) ;
#17372 = FACE_OUTER_BOUND('',#21650,.T.) ;
#17373 = FACE_OUTER_BOUND('',#21651,.T.) ;
#17374 = FACE_OUTER_BOUND('',#21652,.T.) ;
#17375 = FACE_OUTER_BOUND('',#21653,.T.) ;
#17376 = FACE_OUTER_BOUND('',#21654,.T.) ;
#17377 = FACE_OUTER_BOUND('',#21655,.T.) ;
#17378 = FACE_OUTER_BOUND('',#21656,.T.) ;
#17379 = FACE_OUTER_BOUND('',#21657,.T.) ;
#17380 = FACE_OUTER_BOUND('',#21658,.T.) ;
#17381 = FACE_OUTER_BOUND('',#21659,.T.) ;
#17382 = FACE_OUTER_BOUND('',#21660,.T.) ;
#17383 = FACE_OUTER_BOUND('',#21661,.T.) ;
#17384 = FACE_OUTER_BOUND('',#21662,.T.) ;
#17385 = FACE_OUTER_BOUND('',#21663,.T.) ;
#17386 = FACE_OUTER_BOUND('',#21664,.T.) ;
#17387 = FACE_OUTER_BOUND('',#21665,.T.) ;
#17388 = FACE_OUTER_BOUND('',#21666,.T.) ;
#17389 = FACE_OUTER_BOUND('',#21667,.T.) ;
#17390 = FACE_OUTER_BOUND('',#21668,.T.) ;
#17391 = FACE_OUTER_BOUND('',#21669,.T.) ;
#17392 = FACE_OUTER_BOUND('',#21670,.T.) ;
#17393 = FACE_OUTER_BOUND('',#21671,.T.) ;
#17394 = FACE_OUTER_BOUND('',#21672,.T.) ;
#17395 = FACE_OUTER_BOUND('',#21673,.T.) ;
#17396 = FACE_OUTER_BOUND('',#21674,.T.) ;
#17397 = FACE_OUTER_BOUND('',#21675,.T.) ;
#17398 = FACE_OUTER_BOUND('',#21676,.T.) ;
#17399 = FACE_OUTER_BOUND('',#21677,.T.) ;
#17400 = FACE_OUTER_BOUND('',#21678,.T.) ;
#17401 = FACE_OUTER_BOUND('',#21679,.T.) ;
#17402 = FACE_OUTER_BOUND('',#21680,.T.) ;
#17403 = FACE_OUTER_BOUND('',#21681,.T.) ;
#17404 = FACE_OUTER_BOUND('',#21682,.T.) ;
#17405 = FACE_OUTER_BOUND('',#21683,.T.) ;
#17406 = FACE_OUTER_BOUND('',#21684,.T.) ;
#17407 = FACE_OUTER_BOUND('',#21685,.T.) ;
#17408 = FACE_OUTER_BOUND('',#21686,.T.) ;
#17409 = FACE_OUTER_BOUND('',#21687,.T.) ;
#17410 = FACE_OUTER_BOUND('',#21688,.T.) ;
#17411 = FACE_OUTER_BOUND('',#21689,.T.) ;
#17412 = FACE_OUTER_BOUND('',#21690,.T.) ;
#17413 = FACE_OUTER_BOUND('',#21691,.T.) ;
#17414 = FACE_OUTER_BOUND('',#21692,.T.) ;
#17415 = FACE_OUTER_BOUND('',#21693,.T.) ;
#17416 = FACE_OUTER_BOUND('',#21694,.T.) ;
#17417 = FACE_OUTER_BOUND('',#21695,.T.) ;
#17418 = FACE_OUTER_BOUND('',#21696,.T.) ;
#17419 = FACE_OUTER_BOUND('',#21697,.T.) ;
#17420 = FACE_OUTER_BOUND('',#21698,.T.) ;
#17421 = FACE_OUTER_BOUND('',#21699,.T.) ;
#17422 = FACE_OUTER_BOUND('',#21700,.T.) ;
#17423 = FACE_OUTER_BOUND('',#21701,.T.) ;
#17424 = FACE_OUTER_BOUND('',#21702,.T.) ;
#17425 = FACE_OUTER_BOUND('',#21703,.T.) ;
#17426 = FACE_OUTER_BOUND('',#21704,.T.) ;
#17427 = FACE_OUTER_BOUND('',#21705,.T.) ;
#17428 = FACE_OUTER_BOUND('',#21706,.T.) ;
#17429 = FACE_OUTER_BOUND('',#21707,.T.) ;
#17430 = FACE_OUTER_BOUND('',#21708,.T.) ;
#17431 = FACE_OUTER_BOUND('',#21709,.T.) ;
#17432 = FACE_OUTER_BOUND('',#21710,.T.) ;
#17433 = FACE_OUTER_BOUND('',#21711,.T.) ;
#17434 = FACE_OUTER_BOUND('',#21712,.T.) ;
#17435 = FACE_OUTER_BOUND('',#21713,.T.) ;
#17436 = FACE_OUTER_BOUND('',#21714,.T.) ;
#17437 = FACE_OUTER_BOUND('',#21715,.T.) ;
#17438 = FACE_OUTER_BOUND('',#21716,.T.) ;
#17439 = FACE_OUTER_BOUND('',#21717,.T.) ;
#17440 = FACE_OUTER_BOUND('',#21718,.T.) ;
#17441 = FACE_OUTER_BOUND('',#21719,.T.) ;
#17442 = FACE_OUTER_BOUND('',#21720,.T.) ;
#17443 = FACE_OUTER_BOUND('',#21721,.T.) ;
#17444 = FACE_OUTER_BOUND('',#21722,.T.) ;
#17445 = FACE_OUTER_BOUND('',#21723,.T.) ;
#17446 = FACE_OUTER_BOUND('',#21724,.T.) ;
#17447 = FACE_OUTER_BOUND('',#21725,.T.) ;
#17448 = FACE_OUTER_BOUND('',#21726,.T.) ;
#17449 = FACE_OUTER_BOUND('',#21727,.T.) ;
#17450 = FACE_OUTER_BOUND('',#21728,.T.) ;
#17451 = FACE_OUTER_BOUND('',#21729,.T.) ;
#17452 = FACE_OUTER_BOUND('',#21730,.T.) ;
#17453 = FACE_OUTER_BOUND('',#21731,.T.) ;
#17454 = FACE_OUTER_BOUND('',#21732,.T.) ;
#17455 = FACE_OUTER_BOUND('',#21733,.T.) ;
#17456 = FACE_OUTER_BOUND('',#21734,.T.) ;
#17457 = FACE_OUTER_BOUND('',#21735,.T.) ;
#17458 = FACE_OUTER_BOUND('',#21736,.T.) ;
#17459 = FACE_OUTER_BOUND('',#21737,.T.) ;
#17460 = FACE_OUTER_BOUND('',#21738,.T.) ;
#17461 = FACE_OUTER_BOUND('',#21739,.T.) ;
#17462 = FACE_OUTER_BOUND('',#21740,.T.) ;
#17463 = FACE_OUTER_BOUND('',#21741,.T.) ;
#17464 = FACE_OUTER_BOUND('',#21742,.T.) ;
#17465 = FACE_OUTER_BOUND('',#21743,.T.) ;
#17466 = FACE_OUTER_BOUND('',#21744,.T.) ;
#17467 = FACE_OUTER_BOUND('',#21745,.T.) ;
#17468 = FACE_OUTER_BOUND('',#21746,.T.) ;
#17469 = FACE_OUTER_BOUND('',#21747,.T.) ;
#17470 = FACE_OUTER_BOUND('',#21748,.T.) ;
#17471 = FACE_OUTER_BOUND('',#21749,.T.) ;
#17472 = FACE_OUTER_BOUND('',#21750,.T.) ;
#17473 = FACE_OUTER_BOUND('',#21751,.T.) ;
#17474 = FACE_OUTER_BOUND('',#21752,.T.) ;
#17475 = FACE_OUTER_BOUND('',#21753,.T.) ;
#17476 = FACE_OUTER_BOUND('',#21754,.T.) ;
#17477 = FACE_OUTER_BOUND('',#21755,.T.) ;
#17478 = FACE_OUTER_BOUND('',#21756,.T.) ;
#17479 = FACE_OUTER_BOUND('',#21757,.T.) ;
#17480 = FACE_OUTER_BOUND('',#21758,.T.) ;
#17481 = FACE_OUTER_BOUND('',#21759,.T.) ;
#17482 = FACE_OUTER_BOUND('',#21760,.T.) ;
#17483 = FACE_OUTER_BOUND('',#21761,.T.) ;
#17484 = FACE_OUTER_BOUND('',#21762,.T.) ;
#17485 = FACE_OUTER_BOUND('',#21763,.T.) ;
#17486 = FACE_OUTER_BOUND('',#21764,.T.) ;
#17487 = FACE_OUTER_BOUND('',#21765,.T.) ;
#17488 = FACE_OUTER_BOUND('',#21766,.T.) ;
#17489 = FACE_OUTER_BOUND('',#21767,.T.) ;
#17490 = FACE_OUTER_BOUND('',#21768,.T.) ;
#17491 = FACE_OUTER_BOUND('',#21769,.T.) ;
#17492 = FACE_OUTER_BOUND('',#21770,.T.) ;
#17493 = FACE_OUTER_BOUND('',#21771,.T.) ;
#17494 = FACE_OUTER_BOUND('',#21772,.T.) ;
#17495 = FACE_OUTER_BOUND('',#21773,.T.) ;
#17496 = FACE_OUTER_BOUND('',#21774,.T.) ;
#17497 = FACE_OUTER_BOUND('',#21775,.T.) ;
#17498 = FACE_OUTER_BOUND('',#21776,.T.) ;
#17499 = FACE_OUTER_BOUND('',#21777,.T.) ;
#17500 = FACE_OUTER_BOUND('',#21778,.T.) ;
#17501 = FACE_OUTER_BOUND('',#21779,.T.) ;
#17502 = FACE_OUTER_BOUND('',#21780,.T.) ;
#17503 = FACE_OUTER_BOUND('',#21782,.T.) ;
#17504 = FACE_OUTER_BOUND('',#21783,.T.) ;
#17505 = FACE_OUTER_BOUND('',#21784,.T.) ;
#17506 = FACE_OUTER_BOUND('',#21785,.T.) ;
#17507 = FACE_OUTER_BOUND('',#21786,.T.) ;
#17508 = FACE_OUTER_BOUND('',#21787,.T.) ;
#17509 = FACE_OUTER_BOUND('',#21788,.T.) ;
#17510 = FACE_OUTER_BOUND('',#21789,.T.) ;
#17511 = FACE_OUTER_BOUND('',#21790,.T.) ;
#17512 = FACE_OUTER_BOUND('',#21791,.T.) ;
#17513 = FACE_OUTER_BOUND('',#21792,.T.) ;
#17514 = FACE_OUTER_BOUND('',#21794,.T.) ;
#17515 = FACE_OUTER_BOUND('',#21795,.T.) ;
#17516 = FACE_OUTER_BOUND('',#21796,.T.) ;
#17517 = FACE_OUTER_BOUND('',#21797,.T.) ;
#17518 = FACE_OUTER_BOUND('',#21798,.T.) ;
#17519 = FACE_OUTER_BOUND('',#21799,.T.) ;
#17520 = FACE_OUTER_BOUND('',#21800,.T.) ;
#17521 = FACE_OUTER_BOUND('',#21801,.T.) ;
#17522 = FACE_OUTER_BOUND('',#21802,.T.) ;
#17523 = FACE_OUTER_BOUND('',#21803,.T.) ;
#17524 = FACE_OUTER_BOUND('',#21804,.T.) ;
#17525 = FACE_OUTER_BOUND('',#21805,.T.) ;
#17526 = FACE_OUTER_BOUND('',#21806,.T.) ;
#17527 = FACE_OUTER_BOUND('',#21807,.T.) ;
#17528 = FACE_OUTER_BOUND('',#21808,.T.) ;
#17529 = FACE_OUTER_BOUND('',#21809,.T.) ;
#17530 = FACE_OUTER_BOUND('',#21810,.T.) ;
#17531 = FACE_OUTER_BOUND('',#21811,.T.) ;
#17532 = FACE_OUTER_BOUND('',#21812,.T.) ;
#17533 = FACE_OUTER_BOUND('',#21813,.T.) ;
#17534 = FACE_OUTER_BOUND('',#21814,.T.) ;
#17535 = FACE_OUTER_BOUND('',#21815,.T.) ;
#17536 = FACE_OUTER_BOUND('',#21816,.T.) ;
#17537 = FACE_OUTER_BOUND('',#21817,.T.) ;
#17538 = FACE_OUTER_BOUND('',#21818,.T.) ;
#17539 = FACE_OUTER_BOUND('',#21819,.T.) ;
#17540 = FACE_OUTER_BOUND('',#21820,.T.) ;
#17541 = FACE_OUTER_BOUND('',#21821,.T.) ;
#17542 = FACE_OUTER_BOUND('',#21822,.T.) ;
#17543 = FACE_OUTER_BOUND('',#21823,.T.) ;
#17544 = FACE_OUTER_BOUND('',#21824,.T.) ;
#17545 = FACE_OUTER_BOUND('',#21825,.T.) ;
#17546 = FACE_OUTER_BOUND('',#21826,.T.) ;
#17547 = FACE_OUTER_BOUND('',#21827,.T.) ;
#17548 = FACE_OUTER_BOUND('',#21828,.T.) ;
#17549 = FACE_OUTER_BOUND('',#21829,.T.) ;
#17550 = FACE_OUTER_BOUND('',#21830,.T.) ;
#17551 = FACE_OUTER_BOUND('',#21831,.T.) ;
#17552 = FACE_OUTER_BOUND('',#21832,.T.) ;
#17553 = FACE_OUTER_BOUND('',#21833,.T.) ;
#17554 = FACE_OUTER_BOUND('',#21834,.T.) ;
#17555 = FACE_OUTER_BOUND('',#21835,.T.) ;
#17556 = FACE_OUTER_BOUND('',#21836,.T.) ;
#17557 = FACE_OUTER_BOUND('',#21837,.T.) ;
#17558 = FACE_OUTER_BOUND('',#21838,.T.) ;
#17559 = FACE_OUTER_BOUND('',#21839,.T.) ;
#17560 = FACE_OUTER_BOUND('',#21840,.T.) ;
#17561 = FACE_OUTER_BOUND('',#21841,.T.) ;
#17562 = FACE_OUTER_BOUND('',#21842,.T.) ;
#17563 = FACE_OUTER_BOUND('',#21843,.T.) ;
#17564 = FACE_OUTER_BOUND('',#21844,.T.) ;
#17565 = FACE_OUTER_BOUND('',#21845,.T.) ;
#17566 = FACE_OUTER_BOUND('',#21846,.T.) ;
#17567 = FACE_OUTER_BOUND('',#21847,.T.) ;
#17568 = FACE_OUTER_BOUND('',#21848,.T.) ;
#17569 = FACE_OUTER_BOUND('',#21849,.T.) ;
#17570 = FACE_OUTER_BOUND('',#21850,.T.) ;
#17571 = FACE_OUTER_BOUND('',#21851,.T.) ;
#17572 = FACE_OUTER_BOUND('',#21852,.T.) ;
#17573 = FACE_OUTER_BOUND('',#21853,.T.) ;
#17574 = FACE_OUTER_BOUND('',#21854,.T.) ;
#17575 = FACE_OUTER_BOUND('',#21855,.T.) ;
#17576 = FACE_OUTER_BOUND('',#21856,.T.) ;
#17577 = FACE_OUTER_BOUND('',#21857,.T.) ;
#17578 = FACE_OUTER_BOUND('',#21858,.T.) ;
#17579 = FACE_OUTER_BOUND('',#21859,.T.) ;
#17580 = FACE_OUTER_BOUND('',#21860,.T.) ;
#17581 = FACE_OUTER_BOUND('',#21861,.T.) ;
#17582 = FACE_OUTER_BOUND('',#21862,.T.) ;
#17583 = FACE_OUTER_BOUND('',#21863,.T.) ;
#17584 = FACE_OUTER_BOUND('',#21864,.T.) ;
#17585 = FACE_OUTER_BOUND('',#21865,.T.) ;
#17586 = FACE_OUTER_BOUND('',#21866,.T.) ;
#17587 = FACE_OUTER_BOUND('',#21867,.T.) ;
#17588 = FACE_OUTER_BOUND('',#21868,.T.) ;
#17589 = FACE_OUTER_BOUND('',#21869,.T.) ;
#17590 = FACE_OUTER_BOUND('',#21870,.T.) ;
#17591 = FACE_OUTER_BOUND('',#21871,.T.) ;
#17592 = FACE_OUTER_BOUND('',#21872,.T.) ;
#17593 = FACE_OUTER_BOUND('',#21873,.T.) ;
#17594 = FACE_OUTER_BOUND('',#21874,.T.) ;
#17595 = FACE_OUTER_BOUND('',#21875,.T.) ;
#17596 = FACE_OUTER_BOUND('',#21876,.T.) ;
#17597 = FACE_OUTER_BOUND('',#21877,.T.) ;
#17598 = FACE_OUTER_BOUND('',#21878,.T.) ;
#17599 = FACE_OUTER_BOUND('',#21879,.T.) ;
#17600 = FACE_OUTER_BOUND('',#21880,.T.) ;
#17601 = FACE_OUTER_BOUND('',#21881,.T.) ;
#17602 = FACE_OUTER_BOUND('',#21882,.T.) ;
#17603 = FACE_OUTER_BOUND('',#21883,.T.) ;
#17604 = FACE_OUTER_BOUND('',#21884,.T.) ;
#17605 = FACE_OUTER_BOUND('',#21885,.T.) ;
#17606 = FACE_OUTER_BOUND('',#21886,.T.) ;
#17607 = FACE_OUTER_BOUND('',#21887,.T.) ;
#17608 = FACE_OUTER_BOUND('',#21888,.T.) ;
#17609 = FACE_OUTER_BOUND('',#21889,.T.) ;
#17610 = FACE_OUTER_BOUND('',#21890,.T.) ;
#17611 = FACE_OUTER_BOUND('',#21891,.T.) ;
#17612 = FACE_OUTER_BOUND('',#21892,.T.) ;
#17613 = FACE_OUTER_BOUND('',#21893,.T.) ;
#17614 = FACE_OUTER_BOUND('',#21894,.T.) ;
#17615 = FACE_OUTER_BOUND('',#21895,.T.) ;
#17616 = FACE_OUTER_BOUND('',#21896,.T.) ;
#17617 = FACE_OUTER_BOUND('',#21897,.T.) ;
#17618 = FACE_OUTER_BOUND('',#21898,.T.) ;
#17619 = FACE_OUTER_BOUND('',#21899,.T.) ;
#17620 = FACE_OUTER_BOUND('',#21900,.T.) ;
#17621 = FACE_OUTER_BOUND('',#21901,.T.) ;
#17622 = FACE_OUTER_BOUND('',#21902,.T.) ;
#17623 = FACE_OUTER_BOUND('',#21903,.T.) ;
#17624 = FACE_OUTER_BOUND('',#21904,.T.) ;
#17625 = FACE_OUTER_BOUND('',#21905,.T.) ;
#17626 = FACE_OUTER_BOUND('',#21906,.T.) ;
#17627 = FACE_OUTER_BOUND('',#21907,.T.) ;
#17628 = FACE_OUTER_BOUND('',#21908,.T.) ;
#17629 = FACE_OUTER_BOUND('',#21909,.T.) ;
#17630 = FACE_OUTER_BOUND('',#21910,.T.) ;
#17631 = FACE_OUTER_BOUND('',#21911,.T.) ;
#17632 = FACE_OUTER_BOUND('',#21912,.T.) ;
#17633 = FACE_OUTER_BOUND('',#21913,.T.) ;
#17634 = FACE_OUTER_BOUND('',#21914,.T.) ;
#17635 = FACE_OUTER_BOUND('',#21915,.T.) ;
#17636 = FACE_OUTER_BOUND('',#21916,.T.) ;
#17637 = FACE_OUTER_BOUND('',#21917,.T.) ;
#17638 = FACE_OUTER_BOUND('',#21918,.T.) ;
#17639 = FACE_OUTER_BOUND('',#21919,.T.) ;
#17640 = FACE_OUTER_BOUND('',#21920,.T.) ;
#17641 = FACE_OUTER_BOUND('',#21921,.T.) ;
#17642 = FACE_OUTER_BOUND('',#21922,.T.) ;
#17643 = FACE_OUTER_BOUND('',#21923,.T.) ;
#17644 = FACE_OUTER_BOUND('',#21924,.T.) ;
#17645 = FACE_OUTER_BOUND('',#21925,.T.) ;
#17646 = FACE_OUTER_BOUND('',#21926,.T.) ;
#17647 = FACE_OUTER_BOUND('',#21927,.T.) ;
#17648 = FACE_OUTER_BOUND('',#21928,.T.) ;
#17649 = FACE_OUTER_BOUND('',#21929,.T.) ;
#17650 = FACE_OUTER_BOUND('',#21930,.T.) ;
#17651 = FACE_OUTER_BOUND('',#21931,.T.) ;
#17652 = FACE_OUTER_BOUND('',#21932,.T.) ;
#17653 = FACE_OUTER_BOUND('',#21933,.T.) ;
#17654 = FACE_OUTER_BOUND('',#21934,.T.) ;
#17655 = FACE_OUTER_BOUND('',#21935,.T.) ;
#17656 = FACE_OUTER_BOUND('',#21936,.T.) ;
#17657 = FACE_OUTER_BOUND('',#21937,.T.) ;
#17658 = FACE_OUTER_BOUND('',#21938,.T.) ;
#17659 = FACE_OUTER_BOUND('',#21939,.T.) ;
#17660 = FACE_OUTER_BOUND('',#21940,.T.) ;
#17661 = FACE_OUTER_BOUND('',#21941,.T.) ;
#17662 = FACE_OUTER_BOUND('',#21942,.T.) ;
#17663 = FACE_OUTER_BOUND('',#21943,.T.) ;
#17664 = FACE_OUTER_BOUND('',#21944,.T.) ;
#17665 = FACE_OUTER_BOUND('',#21945,.T.) ;
#17666 = FACE_OUTER_BOUND('',#21946,.T.) ;
#17667 = FACE_OUTER_BOUND('',#21947,.T.) ;
#17668 = FACE_OUTER_BOUND('',#21948,.T.) ;
#17669 = FACE_OUTER_BOUND('',#21949,.T.) ;
#17670 = FACE_OUTER_BOUND('',#21950,.T.) ;
#17671 = FACE_OUTER_BOUND('',#21951,.T.) ;
#17672 = FACE_OUTER_BOUND('',#21952,.T.) ;
#17673 = FACE_OUTER_BOUND('',#21953,.T.) ;
#17674 = FACE_OUTER_BOUND('',#21954,.T.) ;
#17675 = FACE_OUTER_BOUND('',#21955,.T.) ;
#17676 = FACE_OUTER_BOUND('',#21956,.T.) ;
#17677 = FACE_OUTER_BOUND('',#21957,.T.) ;
#17678 = FACE_OUTER_BOUND('',#21958,.T.) ;
#17679 = FACE_OUTER_BOUND('',#21959,.T.) ;
#17680 = FACE_OUTER_BOUND('',#21960,.T.) ;
#17681 = FACE_OUTER_BOUND('',#21961,.T.) ;
#17682 = FACE_OUTER_BOUND('',#21962,.T.) ;
#17683 = FACE_OUTER_BOUND('',#21963,.T.) ;
#17684 = FACE_OUTER_BOUND('',#21964,.T.) ;
#17685 = FACE_OUTER_BOUND('',#21965,.T.) ;
#17686 = FACE_OUTER_BOUND('',#21966,.T.) ;
#17687 = FACE_OUTER_BOUND('',#21967,.T.) ;
#17688 = FACE_OUTER_BOUND('',#21968,.T.) ;
#17689 = FACE_OUTER_BOUND('',#21969,.T.) ;
#17690 = FACE_OUTER_BOUND('',#21970,.T.) ;
#17691 = FACE_OUTER_BOUND('',#21971,.T.) ;
#17692 = FACE_OUTER_BOUND('',#21972,.T.) ;
#17693 = FACE_OUTER_BOUND('',#21973,.T.) ;
#17694 = FACE_OUTER_BOUND('',#21974,.T.) ;
#17695 = FACE_OUTER_BOUND('',#21975,.T.) ;
#17696 = FACE_OUTER_BOUND('',#21976,.T.) ;
#17697 = FACE_OUTER_BOUND('',#21977,.T.) ;
#17698 = FACE_OUTER_BOUND('',#21978,.T.) ;
#17699 = FACE_OUTER_BOUND('',#21979,.T.) ;
#17700 = FACE_OUTER_BOUND('',#21980,.T.) ;
#17701 = FACE_OUTER_BOUND('',#21981,.T.) ;
#17702 = FACE_OUTER_BOUND('',#21982,.T.) ;
#17703 = FACE_OUTER_BOUND('',#21983,.T.) ;
#17704 = FACE_OUTER_BOUND('',#21984,.T.) ;
#17705 = FACE_OUTER_BOUND('',#21985,.T.) ;
#17706 = FACE_OUTER_BOUND('',#21986,.T.) ;
#17707 = FACE_OUTER_BOUND('',#21987,.T.) ;
#17708 = FACE_OUTER_BOUND('',#21988,.T.) ;
#17709 = FACE_OUTER_BOUND('',#21989,.T.) ;
#17710 = FACE_OUTER_BOUND('',#21990,.T.) ;
#17711 = FACE_OUTER_BOUND('',#21991,.T.) ;
#17712 = FACE_OUTER_BOUND('',#21992,.T.) ;
#17713 = FACE_OUTER_BOUND('',#21993,.T.) ;
#17714 = FACE_OUTER_BOUND('',#21994,.T.) ;
#17715 = FACE_OUTER_BOUND('',#21995,.T.) ;
#17716 = FACE_OUTER_BOUND('',#21996,.T.) ;
#17717 = FACE_OUTER_BOUND('',#21997,.T.) ;
#17718 = FACE_OUTER_BOUND('',#21998,.T.) ;
#17719 = FACE_OUTER_BOUND('',#21999,.T.) ;
#17720 = FACE_OUTER_BOUND('',#22000,.T.) ;
#17721 = FACE_OUTER_BOUND('',#22001,.T.) ;
#17722 = FACE_OUTER_BOUND('',#22002,.T.) ;
#17723 = FACE_OUTER_BOUND('',#22003,.T.) ;
#17724 = FACE_OUTER_BOUND('',#22004,.T.) ;
#17725 = FACE_OUTER_BOUND('',#22005,.T.) ;
#17726 = FACE_OUTER_BOUND('',#22006,.T.) ;
#17727 = FACE_OUTER_BOUND('',#22007,.T.) ;
#17728 = FACE_OUTER_BOUND('',#22008,.T.) ;
#17729 = FACE_OUTER_BOUND('',#22009,.T.) ;
#17730 = FACE_OUTER_BOUND('',#22010,.T.) ;
#17731 = FACE_OUTER_BOUND('',#22011,.T.) ;
#17732 = FACE_OUTER_BOUND('',#22012,.T.) ;
#17733 = FACE_OUTER_BOUND('',#22013,.T.) ;
#17734 = FACE_OUTER_BOUND('',#22014,.T.) ;
#17735 = FACE_OUTER_BOUND('',#22015,.T.) ;
#17736 = FACE_OUTER_BOUND('',#22016,.T.) ;
#17737 = FACE_OUTER_BOUND('',#22017,.T.) ;
#17738 = FACE_OUTER_BOUND('',#22018,.T.) ;
#17739 = FACE_OUTER_BOUND('',#22019,.T.) ;
#17740 = FACE_OUTER_BOUND('',#22020,.T.) ;
#17741 = FACE_OUTER_BOUND('',#22021,.T.) ;
#17742 = FACE_OUTER_BOUND('',#22022,.T.) ;
#17743 = FACE_OUTER_BOUND('',#22023,.T.) ;
#17744 = FACE_OUTER_BOUND('',#22024,.T.) ;
#17745 = FACE_OUTER_BOUND('',#22025,.T.) ;
#17746 = FACE_OUTER_BOUND('',#22026,.T.) ;
#17747 = FACE_OUTER_BOUND('',#22027,.T.) ;
#17748 = FACE_OUTER_BOUND('',#22028,.T.) ;
#17749 = FACE_OUTER_BOUND('',#22029,.T.) ;
#17750 = FACE_OUTER_BOUND('',#22030,.T.) ;
#17751 = FACE_OUTER_BOUND('',#22031,.T.) ;
#17752 = FACE_OUTER_BOUND('',#22032,.T.) ;
#17753 = FACE_OUTER_BOUND('',#22033,.T.) ;
#17754 = FACE_OUTER_BOUND('',#22034,.T.) ;
#17755 = FACE_OUTER_BOUND('',#22035,.T.) ;
#17756 = FACE_OUTER_BOUND('',#22036,.T.) ;
#17757 = FACE_OUTER_BOUND('',#22037,.T.) ;
#17758 = FACE_OUTER_BOUND('',#22038,.T.) ;
#17759 = FACE_OUTER_BOUND('',#22039,.T.) ;
#17760 = FACE_OUTER_BOUND('',#22040,.T.) ;
#17761 = FACE_OUTER_BOUND('',#22041,.T.) ;
#17762 = FACE_OUTER_BOUND('',#22042,.T.) ;
#17763 = FACE_OUTER_BOUND('',#22043,.T.) ;
#17764 = FACE_OUTER_BOUND('',#22044,.T.) ;
#17765 = FACE_OUTER_BOUND('',#22045,.T.) ;
#17766 = FACE_OUTER_BOUND('',#22046,.T.) ;
#17767 = FACE_OUTER_BOUND('',#22047,.T.) ;
#17768 = FACE_OUTER_BOUND('',#22048,.T.) ;
#17769 = FACE_OUTER_BOUND('',#22049,.T.) ;
#17770 = FACE_OUTER_BOUND('',#22050,.T.) ;
#17771 = FACE_OUTER_BOUND('',#22051,.T.) ;
#17772 = FACE_OUTER_BOUND('',#22052,.T.) ;
#17773 = FACE_OUTER_BOUND('',#22053,.T.) ;
#17774 = FACE_OUTER_BOUND('',#22054,.T.) ;
#17775 = FACE_OUTER_BOUND('',#22055,.T.) ;
#17776 = FACE_OUTER_BOUND('',#22056,.T.) ;
#17777 = FACE_OUTER_BOUND('',#22057,.T.) ;
#17778 = FACE_OUTER_BOUND('',#22058,.T.) ;
#17779 = FACE_OUTER_BOUND('',#22059,.T.) ;
#17780 = FACE_OUTER_BOUND('',#22060,.T.) ;
#17781 = FACE_OUTER_BOUND('',#22061,.T.) ;
#17782 = FACE_OUTER_BOUND('',#22062,.T.) ;
#17783 = FACE_OUTER_BOUND('',#22063,.T.) ;
#17784 = FACE_OUTER_BOUND('',#22064,.T.) ;
#17785 = FACE_OUTER_BOUND('',#22065,.T.) ;
#17786 = FACE_OUTER_BOUND('',#22066,.T.) ;
#17787 = FACE_OUTER_BOUND('',#22067,.T.) ;
#17788 = FACE_OUTER_BOUND('',#22068,.T.) ;
#17789 = FACE_OUTER_BOUND('',#22069,.T.) ;
#17790 = FACE_OUTER_BOUND('',#22070,.T.) ;
#17791 = FACE_OUTER_BOUND('',#22071,.T.) ;
#17792 = FACE_OUTER_BOUND('',#22073,.T.) ;
#17793 = FACE_OUTER_BOUND('',#22074,.T.) ;
#17794 = FACE_OUTER_BOUND('',#22075,.T.) ;
#17795 = FACE_OUTER_BOUND('',#22076,.T.) ;
#17796 = FACE_OUTER_BOUND('',#22077,.T.) ;
#17797 = FACE_OUTER_BOUND('',#22078,.T.) ;
#17798 = FACE_OUTER_BOUND('',#22079,.T.) ;
#17799 = FACE_OUTER_BOUND('',#22080,.T.) ;
#17800 = FACE_OUTER_BOUND('',#22081,.T.) ;
#17801 = FACE_OUTER_BOUND('',#22082,.T.) ;
#17802 = FACE_OUTER_BOUND('',#22083,.T.) ;
#17803 = FACE_OUTER_BOUND('',#22085,.T.) ;
#17804 = FACE_OUTER_BOUND('',#22086,.T.) ;
#17805 = FACE_OUTER_BOUND('',#22087,.T.) ;
#17806 = FACE_OUTER_BOUND('',#22088,.T.) ;
#17807 = FACE_OUTER_BOUND('',#22089,.T.) ;
#17808 = FACE_OUTER_BOUND('',#22090,.T.) ;
#17809 = FACE_OUTER_BOUND('',#22091,.T.) ;
#17810 = FACE_OUTER_BOUND('',#22092,.T.) ;
#17811 = FACE_OUTER_BOUND('',#22093,.T.) ;
#17812 = FACE_OUTER_BOUND('',#22094,.T.) ;
#17813 = FACE_OUTER_BOUND('',#22095,.T.) ;
#17814 = FACE_OUTER_BOUND('',#22096,.T.) ;
#17815 = FACE_OUTER_BOUND('',#22097,.T.) ;
#17816 = FACE_OUTER_BOUND('',#22098,.T.) ;
#17817 = FACE_OUTER_BOUND('',#22099,.T.) ;
#17818 = FACE_OUTER_BOUND('',#22100,.T.) ;
#17819 = FACE_OUTER_BOUND('',#22101,.T.) ;
#17820 = FACE_OUTER_BOUND('',#22102,.T.) ;
#17821 = FACE_OUTER_BOUND('',#22103,.T.) ;
#17822 = FACE_OUTER_BOUND('',#22104,.T.) ;
#17823 = FACE_OUTER_BOUND('',#22105,.T.) ;
#17824 = FACE_OUTER_BOUND('',#22106,.T.) ;
#17825 = FACE_OUTER_BOUND('',#22107,.T.) ;
#17826 = FACE_OUTER_BOUND('',#22108,.T.) ;
#17827 = FACE_OUTER_BOUND('',#22109,.T.) ;
#17828 = FACE_OUTER_BOUND('',#22110,.T.) ;
#17829 = FACE_OUTER_BOUND('',#22111,.T.) ;
#17830 = FACE_OUTER_BOUND('',#22112,.T.) ;
#17831 = FACE_OUTER_BOUND('',#22113,.T.) ;
#17832 = FACE_OUTER_BOUND('',#22114,.T.) ;
#17833 = FACE_OUTER_BOUND('',#22115,.T.) ;
#17834 = FACE_OUTER_BOUND('',#22116,.T.) ;
#17835 = FACE_OUTER_BOUND('',#22117,.T.) ;
#17836 = FACE_OUTER_BOUND('',#22118,.T.) ;
#17837 = FACE_OUTER_BOUND('',#22119,.T.) ;
#17838 = FACE_OUTER_BOUND('',#22120,.T.) ;
#17839 = FACE_OUTER_BOUND('',#22121,.T.) ;
#17840 = FACE_OUTER_BOUND('',#22122,.T.) ;
#17841 = FACE_OUTER_BOUND('',#22123,.T.) ;
#17842 = FACE_OUTER_BOUND('',#22124,.T.) ;
#17843 = FACE_OUTER_BOUND('',#22125,.T.) ;
#17844 = FACE_OUTER_BOUND('',#22126,.T.) ;
#17845 = FACE_OUTER_BOUND('',#22127,.T.) ;
#17846 = FACE_OUTER_BOUND('',#22128,.T.) ;
#17847 = FACE_OUTER_BOUND('',#22129,.T.) ;
#17848 = FACE_OUTER_BOUND('',#22130,.T.) ;
#17849 = FACE_OUTER_BOUND('',#22131,.T.) ;
#17850 = FACE_OUTER_BOUND('',#22132,.T.) ;
#17851 = FACE_OUTER_BOUND('',#22133,.T.) ;
#17852 = FACE_OUTER_BOUND('',#22134,.T.) ;
#17853 = FACE_OUTER_BOUND('',#22135,.T.) ;
#17854 = FACE_OUTER_BOUND('',#22136,.T.) ;
#17855 = FACE_OUTER_BOUND('',#22137,.T.) ;
#17856 = FACE_OUTER_BOUND('',#22138,.T.) ;
#17857 = FACE_OUTER_BOUND('',#22139,.T.) ;
#17858 = FACE_OUTER_BOUND('',#22140,.T.) ;
#17859 = FACE_OUTER_BOUND('',#22141,.T.) ;
#17860 = FACE_OUTER_BOUND('',#22142,.T.) ;
#17861 = FACE_OUTER_BOUND('',#22143,.T.) ;
#17862 = FACE_OUTER_BOUND('',#22144,.T.) ;
#17863 = FACE_OUTER_BOUND('',#22145,.T.) ;
#17864 = FACE_OUTER_BOUND('',#22146,.T.) ;
#17865 = FACE_OUTER_BOUND('',#22147,.T.) ;
#17866 = FACE_OUTER_BOUND('',#22148,.T.) ;
#17867 = FACE_OUTER_BOUND('',#22149,.T.) ;
#17868 = FACE_OUTER_BOUND('',#22150,.T.) ;
#17869 = FACE_OUTER_BOUND('',#22151,.T.) ;
#17870 = FACE_OUTER_BOUND('',#22152,.T.) ;
#17871 = FACE_OUTER_BOUND('',#22153,.T.) ;
#17872 = FACE_OUTER_BOUND('',#22154,.T.) ;
#17873 = FACE_OUTER_BOUND('',#22155,.T.) ;
#17874 = FACE_OUTER_BOUND('',#22156,.T.) ;
#17875 = FACE_OUTER_BOUND('',#22157,.T.) ;
#17876 = FACE_OUTER_BOUND('',#22158,.T.) ;
#17877 = FACE_OUTER_BOUND('',#22159,.T.) ;
#17878 = FACE_OUTER_BOUND('',#22160,.T.) ;
#17879 = FACE_OUTER_BOUND('',#22161,.T.) ;
#17880 = FACE_OUTER_BOUND('',#22162,.T.) ;
#17881 = FACE_OUTER_BOUND('',#22163,.T.) ;
#17882 = FACE_OUTER_BOUND('',#22164,.T.) ;
#17883 = FACE_OUTER_BOUND('',#22165,.T.) ;
#17884 = FACE_OUTER_BOUND('',#22166,.T.) ;
#17885 = FACE_OUTER_BOUND('',#22167,.T.) ;
#17886 = FACE_OUTER_BOUND('',#22168,.T.) ;
#17887 = FACE_OUTER_BOUND('',#22169,.T.) ;
#17888 = FACE_OUTER_BOUND('',#22170,.T.) ;
#17889 = FACE_OUTER_BOUND('',#22171,.T.) ;
#17890 = FACE_OUTER_BOUND('',#22172,.T.) ;
#17891 = FACE_OUTER_BOUND('',#22173,.T.) ;
#17892 = FACE_OUTER_BOUND('',#22174,.T.) ;
#17893 = FACE_OUTER_BOUND('',#22175,.T.) ;
#17894 = FACE_OUTER_BOUND('',#22176,.T.) ;
#17895 = FACE_OUTER_BOUND('',#22177,.T.) ;
#17896 = FACE_OUTER_BOUND('',#22178,.T.) ;
#17897 = FACE_OUTER_BOUND('',#22179,.T.) ;
#17898 = FACE_OUTER_BOUND('',#22180,.T.) ;
#17899 = FACE_OUTER_BOUND('',#22181,.T.) ;
#17900 = FACE_OUTER_BOUND('',#22182,.T.) ;
#17901 = FACE_OUTER_BOUND('',#22183,.T.) ;
#17902 = FACE_OUTER_BOUND('',#22184,.T.) ;
#17903 = FACE_OUTER_BOUND('',#22185,.T.) ;
#17904 = FACE_OUTER_BOUND('',#22186,.T.) ;
#17905 = FACE_OUTER_BOUND('',#22187,.T.) ;
#17906 = FACE_OUTER_BOUND('',#22188,.T.) ;
#17907 = FACE_OUTER_BOUND('',#22189,.T.) ;
#17908 = FACE_OUTER_BOUND('',#22190,.T.) ;
#17909 = FACE_OUTER_BOUND('',#22191,.T.) ;
#17910 = FACE_OUTER_BOUND('',#22192,.T.) ;
#17911 = FACE_OUTER_BOUND('',#22193,.T.) ;
#17912 = FACE_OUTER_BOUND('',#22194,.T.) ;
#17913 = FACE_OUTER_BOUND('',#22195,.T.) ;
#17914 = FACE_OUTER_BOUND('',#22196,.T.) ;
#17915 = FACE_OUTER_BOUND('',#22197,.T.) ;
#17916 = FACE_OUTER_BOUND('',#22198,.T.) ;
#17917 = FACE_OUTER_BOUND('',#22199,.T.) ;
#17918 = FACE_OUTER_BOUND('',#22200,.T.) ;
#17919 = FACE_OUTER_BOUND('',#22201,.T.) ;
#17920 = FACE_OUTER_BOUND('',#22202,.T.) ;
#17921 = FACE_OUTER_BOUND('',#22203,.T.) ;
#17922 = FACE_OUTER_BOUND('',#22204,.T.) ;
#17923 = FACE_OUTER_BOUND('',#22205,.T.) ;
#17924 = FACE_OUTER_BOUND('',#22206,.T.) ;
#17925 = FACE_OUTER_BOUND('',#22207,.T.) ;
#17926 = FACE_OUTER_BOUND('',#22208,.T.) ;
#17927 = FACE_OUTER_BOUND('',#22209,.T.) ;
#17928 = FACE_OUTER_BOUND('',#22210,.T.) ;
#17929 = FACE_OUTER_BOUND('',#22211,.T.) ;
#17930 = FACE_OUTER_BOUND('',#22212,.T.) ;
#17931 = FACE_OUTER_BOUND('',#22213,.T.) ;
#17932 = FACE_OUTER_BOUND('',#22214,.T.) ;
#17933 = FACE_OUTER_BOUND('',#22215,.T.) ;
#17934 = FACE_OUTER_BOUND('',#22216,.T.) ;
#17935 = FACE_OUTER_BOUND('',#22217,.T.) ;
#17936 = FACE_OUTER_BOUND('',#22218,.T.) ;
#17937 = FACE_OUTER_BOUND('',#22219,.T.) ;
#17938 = FACE_OUTER_BOUND('',#22220,.T.) ;
#17939 = FACE_OUTER_BOUND('',#22221,.T.) ;
#17940 = FACE_OUTER_BOUND('',#22222,.T.) ;
#17941 = FACE_OUTER_BOUND('',#22223,.T.) ;
#17942 = FACE_OUTER_BOUND('',#22224,.T.) ;
#17943 = FACE_OUTER_BOUND('',#22225,.T.) ;
#17944 = FACE_OUTER_BOUND('',#22226,.T.) ;
#17945 = FACE_OUTER_BOUND('',#22227,.T.) ;
#17946 = FACE_OUTER_BOUND('',#22228,.T.) ;
#17947 = FACE_OUTER_BOUND('',#22229,.T.) ;
#17948 = FACE_OUTER_BOUND('',#22230,.T.) ;
#17949 = FACE_OUTER_BOUND('',#22231,.T.) ;
#17950 = FACE_OUTER_BOUND('',#22232,.T.) ;
#17951 = FACE_OUTER_BOUND('',#22233,.T.) ;
#17952 = FACE_OUTER_BOUND('',#22234,.T.) ;
#17953 = FACE_OUTER_BOUND('',#22235,.T.) ;
#17954 = FACE_OUTER_BOUND('',#22236,.T.) ;
#17955 = FACE_OUTER_BOUND('',#22237,.T.) ;
#17956 = FACE_OUTER_BOUND('',#22238,.T.) ;
#17957 = FACE_OUTER_BOUND('',#22239,.T.) ;
#17958 = FACE_OUTER_BOUND('',#22240,.T.) ;
#17959 = FACE_OUTER_BOUND('',#22241,.T.) ;
#17960 = FACE_OUTER_BOUND('',#22242,.T.) ;
#17961 = FACE_OUTER_BOUND('',#22243,.T.) ;
#17962 = FACE_OUTER_BOUND('',#22244,.T.) ;
#17963 = FACE_OUTER_BOUND('',#22245,.T.) ;
#17964 = FACE_OUTER_BOUND('',#22246,.T.) ;
#17965 = FACE_OUTER_BOUND('',#22247,.T.) ;
#17966 = FACE_OUTER_BOUND('',#22248,.T.) ;
#17967 = FACE_OUTER_BOUND('',#22249,.T.) ;
#17968 = FACE_OUTER_BOUND('',#22250,.T.) ;
#17969 = FACE_OUTER_BOUND('',#22251,.T.) ;
#17970 = FACE_OUTER_BOUND('',#22252,.T.) ;
#17971 = FACE_OUTER_BOUND('',#22253,.T.) ;
#17972 = FACE_OUTER_BOUND('',#22254,.T.) ;
#17973 = FACE_OUTER_BOUND('',#22255,.T.) ;
#17974 = FACE_OUTER_BOUND('',#22256,.T.) ;
#17975 = FACE_OUTER_BOUND('',#22257,.T.) ;
#17976 = FACE_OUTER_BOUND('',#22258,.T.) ;
#17977 = FACE_OUTER_BOUND('',#22259,.T.) ;
#17978 = FACE_OUTER_BOUND('',#22260,.T.) ;
#17979 = FACE_OUTER_BOUND('',#22261,.T.) ;
#17980 = FACE_OUTER_BOUND('',#22262,.T.) ;
#17981 = FACE_OUTER_BOUND('',#22263,.T.) ;
#17982 = FACE_OUTER_BOUND('',#22264,.T.) ;
#17983 = FACE_OUTER_BOUND('',#22265,.T.) ;
#17984 = FACE_OUTER_BOUND('',#22266,.T.) ;
#17985 = FACE_OUTER_BOUND('',#22267,.T.) ;
#17986 = FACE_OUTER_BOUND('',#22268,.T.) ;
#17987 = FACE_OUTER_BOUND('',#22269,.T.) ;
#17988 = FACE_OUTER_BOUND('',#22270,.T.) ;
#17989 = FACE_OUTER_BOUND('',#22271,.T.) ;
#17990 = FACE_OUTER_BOUND('',#22272,.T.) ;
#17991 = FACE_OUTER_BOUND('',#22273,.T.) ;
#17992 = FACE_OUTER_BOUND('',#22274,.T.) ;
#17993 = FACE_OUTER_BOUND('',#22275,.T.) ;
#17994 = FACE_OUTER_BOUND('',#22276,.T.) ;
#17995 = FACE_OUTER_BOUND('',#22277,.T.) ;
#17996 = FACE_OUTER_BOUND('',#22278,.T.) ;
#17997 = FACE_OUTER_BOUND('',#22279,.T.) ;
#17998 = FACE_OUTER_BOUND('',#22280,.T.) ;
#17999 = FACE_OUTER_BOUND('',#22281,.T.) ;
#18000 = FACE_OUTER_BOUND('',#22282,.T.) ;
#18001 = FACE_OUTER_BOUND('',#22283,.T.) ;
#18002 = FACE_OUTER_BOUND('',#22284,.T.) ;
#18003 = FACE_OUTER_BOUND('',#22285,.T.) ;
#18004 = FACE_OUTER_BOUND('',#22286,.T.) ;
#18005 = FACE_OUTER_BOUND('',#22287,.T.) ;
#18006 = FACE_OUTER_BOUND('',#22288,.T.) ;
#18007 = FACE_OUTER_BOUND('',#22289,.T.) ;
#18008 = FACE_OUTER_BOUND('',#22290,.T.) ;
#18009 = FACE_OUTER_BOUND('',#22291,.T.) ;
#18010 = FACE_OUTER_BOUND('',#22292,.T.) ;
#18011 = FACE_OUTER_BOUND('',#22293,.T.) ;
#18012 = FACE_OUTER_BOUND('',#22294,.T.) ;
#18013 = FACE_OUTER_BOUND('',#22295,.T.) ;
#18014 = FACE_OUTER_BOUND('',#22296,.T.) ;
#18015 = FACE_OUTER_BOUND('',#22297,.T.) ;
#18016 = FACE_OUTER_BOUND('',#22298,.T.) ;
#18017 = FACE_OUTER_BOUND('',#22299,.T.) ;
#18018 = FACE_OUTER_BOUND('',#22300,.T.) ;
#18019 = FACE_OUTER_BOUND('',#22301,.T.) ;
#18020 = FACE_OUTER_BOUND('',#22302,.T.) ;
#18021 = FACE_OUTER_BOUND('',#22303,.T.) ;
#18022 = FACE_OUTER_BOUND('',#22304,.T.) ;
#18023 = FACE_OUTER_BOUND('',#22305,.T.) ;
#18024 = FACE_OUTER_BOUND('',#22306,.T.) ;
#18025 = FACE_OUTER_BOUND('',#22307,.T.) ;
#18026 = FACE_OUTER_BOUND('',#22308,.T.) ;
#18027 = FACE_OUTER_BOUND('',#22309,.T.) ;
#18028 = FACE_OUTER_BOUND('',#22310,.T.) ;
#18029 = FACE_OUTER_BOUND('',#22311,.T.) ;
#18030 = FACE_OUTER_BOUND('',#22312,.T.) ;
#18031 = FACE_OUTER_BOUND('',#22313,.T.) ;
#18032 = FACE_OUTER_BOUND('',#22314,.T.) ;
#18033 = FACE_OUTER_BOUND('',#22315,.T.) ;
#18034 = FACE_OUTER_BOUND('',#22316,.T.) ;
#18035 = FACE_OUTER_BOUND('',#22317,.T.) ;
#18036 = FACE_OUTER_BOUND('',#22318,.T.) ;
#18037 = FACE_OUTER_BOUND('',#22319,.T.) ;
#18038 = FACE_OUTER_BOUND('',#22320,.T.) ;
#18039 = FACE_OUTER_BOUND('',#22321,.T.) ;
#18040 = FACE_OUTER_BOUND('',#22322,.T.) ;
#18041 = FACE_OUTER_BOUND('',#22323,.T.) ;
#18042 = FACE_OUTER_BOUND('',#22324,.T.) ;
#18043 = FACE_OUTER_BOUND('',#22325,.T.) ;
#18044 = FACE_OUTER_BOUND('',#22326,.T.) ;
#18045 = FACE_OUTER_BOUND('',#22327,.T.) ;
#18046 = FACE_OUTER_BOUND('',#22328,.T.) ;
#18047 = FACE_OUTER_BOUND('',#22329,.T.) ;
#18048 = FACE_OUTER_BOUND('',#22330,.T.) ;
#18049 = FACE_OUTER_BOUND('',#22331,.T.) ;
#18050 = FACE_OUTER_BOUND('',#22332,.T.) ;
#18051 = FACE_OUTER_BOUND('',#22333,.T.) ;
#18052 = FACE_OUTER_BOUND('',#22334,.T.) ;
#18053 = FACE_OUTER_BOUND('',#22335,.T.) ;
#18054 = FACE_OUTER_BOUND('',#22336,.T.) ;
#18055 = FACE_OUTER_BOUND('',#22337,.T.) ;
#18056 = FACE_OUTER_BOUND('',#22338,.T.) ;
#18057 = FACE_OUTER_BOUND('',#22339,.T.) ;
#18058 = FACE_OUTER_BOUND('',#22340,.T.) ;
#18059 = FACE_OUTER_BOUND('',#22341,.T.) ;
#18060 = FACE_OUTER_BOUND('',#22342,.T.) ;
#18061 = FACE_OUTER_BOUND('',#22343,.T.) ;
#18062 = FACE_OUTER_BOUND('',#22344,.T.) ;
#18063 = FACE_OUTER_BOUND('',#22345,.T.) ;
#18064 = FACE_OUTER_BOUND('',#22346,.T.) ;
#18065 = FACE_OUTER_BOUND('',#22347,.T.) ;
#18066 = FACE_OUTER_BOUND('',#22348,.T.) ;
#18067 = FACE_OUTER_BOUND('',#22349,.T.) ;
#18068 = FACE_OUTER_BOUND('',#22350,.T.) ;
#18069 = FACE_OUTER_BOUND('',#22351,.T.) ;
#18070 = FACE_OUTER_BOUND('',#22352,.T.) ;
#18071 = FACE_OUTER_BOUND('',#22353,.T.) ;
#18072 = FACE_OUTER_BOUND('',#22356,.T.) ;
#18073 = FACE_OUTER_BOUND('',#22357,.T.) ;
#18074 = FACE_OUTER_BOUND('',#22358,.T.) ;
#18075 = FACE_OUTER_BOUND('',#22359,.T.) ;
#18076 = FACE_OUTER_BOUND('',#22360,.T.) ;
#18077 = FACE_OUTER_BOUND('',#22361,.T.) ;
#18078 = FACE_OUTER_BOUND('',#22362,.T.) ;
#18079 = FACE_OUTER_BOUND('',#22363,.T.) ;
#18080 = FACE_OUTER_BOUND('',#22364,.T.) ;
#18081 = FACE_OUTER_BOUND('',#22365,.T.) ;
#18082 = FACE_OUTER_BOUND('',#22366,.T.) ;
#18083 = FACE_OUTER_BOUND('',#22367,.T.) ;
#18084 = FACE_OUTER_BOUND('',#22368,.T.) ;
#18085 = FACE_OUTER_BOUND('',#22369,.T.) ;
#18086 = FACE_OUTER_BOUND('',#22370,.T.) ;
#18087 = FACE_OUTER_BOUND('',#22371,.T.) ;
#18088 = FACE_OUTER_BOUND('',#22372,.T.) ;
#18089 = FACE_OUTER_BOUND('',#22373,.T.) ;
#18090 = FACE_OUTER_BOUND('',#22374,.T.) ;
#18091 = FACE_OUTER_BOUND('',#22375,.T.) ;
#18092 = FACE_OUTER_BOUND('',#22376,.T.) ;
#18093 = FACE_OUTER_BOUND('',#22377,.T.) ;
#18094 = FACE_OUTER_BOUND('',#22378,.T.) ;
#18095 = FACE_OUTER_BOUND('',#22379,.T.) ;
#18096 = FACE_OUTER_BOUND('',#22380,.T.) ;
#18097 = FACE_OUTER_BOUND('',#22381,.T.) ;
#18098 = FACE_OUTER_BOUND('',#22382,.T.) ;
#18099 = FACE_OUTER_BOUND('',#22383,.T.) ;
#18100 = FACE_OUTER_BOUND('',#22384,.T.) ;
#18101 = FACE_OUTER_BOUND('',#22385,.T.) ;
#18102 = FACE_OUTER_BOUND('',#22386,.T.) ;
#18103 = FACE_OUTER_BOUND('',#22387,.T.) ;
#18104 = FACE_OUTER_BOUND('',#22388,.T.) ;
#18105 = FACE_OUTER_BOUND('',#22389,.T.) ;
#18106 = FACE_OUTER_BOUND('',#22390,.T.) ;
#18107 = FACE_OUTER_BOUND('',#22391,.T.) ;
#18108 = FACE_OUTER_BOUND('',#22392,.T.) ;
#18109 = FACE_OUTER_BOUND('',#22393,.T.) ;
#18110 = FACE_OUTER_BOUND('',#22394,.T.) ;
#18111 = FACE_OUTER_BOUND('',#22395,.T.) ;
#18112 = FACE_OUTER_BOUND('',#22396,.T.) ;
#18113 = FACE_OUTER_BOUND('',#22397,.T.) ;
#18114 = FACE_OUTER_BOUND('',#22398,.T.) ;
#18115 = FACE_OUTER_BOUND('',#22399,.T.) ;
#18116 = FACE_OUTER_BOUND('',#22400,.T.) ;
#18117 = FACE_OUTER_BOUND('',#22401,.T.) ;
#18118 = FACE_OUTER_BOUND('',#22402,.T.) ;
#18119 = FACE_OUTER_BOUND('',#22403,.T.) ;
#18120 = FACE_OUTER_BOUND('',#22404,.T.) ;
#18121 = FACE_OUTER_BOUND('',#22405,.T.) ;
#18122 = FACE_OUTER_BOUND('',#22406,.T.) ;
#18123 = FACE_OUTER_BOUND('',#22407,.T.) ;
#18124 = FACE_OUTER_BOUND('',#22408,.T.) ;
#18125 = FACE_OUTER_BOUND('',#22409,.T.) ;
#18126 = FACE_OUTER_BOUND('',#22410,.T.) ;
#18127 = FACE_OUTER_BOUND('',#22411,.T.) ;
#18128 = FACE_OUTER_BOUND('',#22412,.T.) ;
#18129 = FACE_OUTER_BOUND('',#22413,.T.) ;
#18130 = FACE_OUTER_BOUND('',#22414,.T.) ;
#18131 = FACE_OUTER_BOUND('',#22415,.T.) ;
#18132 = FACE_OUTER_BOUND('',#22416,.T.) ;
#18133 = FACE_OUTER_BOUND('',#22417,.T.) ;
#18134 = FACE_OUTER_BOUND('',#22418,.T.) ;
#18135 = FACE_OUTER_BOUND('',#22419,.T.) ;
#18136 = FACE_OUTER_BOUND('',#22420,.T.) ;
#18137 = FACE_OUTER_BOUND('',#22421,.T.) ;
#18138 = FACE_OUTER_BOUND('',#22422,.T.) ;
#18139 = FACE_OUTER_BOUND('',#22423,.T.) ;
#18140 = FACE_OUTER_BOUND('',#22424,.T.) ;
#18141 = FACE_OUTER_BOUND('',#22425,.T.) ;
#18142 = FACE_OUTER_BOUND('',#22426,.T.) ;
#18143 = FACE_OUTER_BOUND('',#22427,.T.) ;
#18144 = FACE_OUTER_BOUND('',#22428,.T.) ;
#18145 = FACE_OUTER_BOUND('',#22429,.T.) ;
#18146 = FACE_OUTER_BOUND('',#22430,.T.) ;
#18147 = FACE_OUTER_BOUND('',#22431,.T.) ;
#18148 = FACE_OUTER_BOUND('',#22432,.T.) ;
#18149 = FACE_OUTER_BOUND('',#22433,.T.) ;
#18150 = FACE_OUTER_BOUND('',#22434,.T.) ;
#18151 = FACE_OUTER_BOUND('',#22435,.T.) ;
#18152 = FACE_OUTER_BOUND('',#22436,.T.) ;
#18153 = FACE_OUTER_BOUND('',#22437,.T.) ;
#18154 = FACE_OUTER_BOUND('',#22438,.T.) ;
#18155 = FACE_OUTER_BOUND('',#22439,.T.) ;
#18156 = FACE_OUTER_BOUND('',#22440,.T.) ;
#18157 = FACE_OUTER_BOUND('',#22441,.T.) ;
#18158 = FACE_OUTER_BOUND('',#22442,.T.) ;
#18159 = FACE_OUTER_BOUND('',#22443,.T.) ;
#18160 = FACE_OUTER_BOUND('',#22444,.T.) ;
#18161 = FACE_OUTER_BOUND('',#22445,.T.) ;
#18162 = FACE_OUTER_BOUND('',#22446,.T.) ;
#18163 = FACE_OUTER_BOUND('',#22447,.T.) ;
#18164 = FACE_OUTER_BOUND('',#22448,.T.) ;
#18165 = FACE_OUTER_BOUND('',#22449,.T.) ;
#18166 = FACE_OUTER_BOUND('',#22450,.T.) ;
#18167 = FACE_OUTER_BOUND('',#22451,.T.) ;
#18168 = FACE_OUTER_BOUND('',#22452,.T.) ;
#18169 = FACE_OUTER_BOUND('',#22453,.T.) ;
#18170 = FACE_OUTER_BOUND('',#22454,.T.) ;
#18171 = FACE_OUTER_BOUND('',#22455,.T.) ;
#18172 = FACE_OUTER_BOUND('',#22456,.T.) ;
#18173 = FACE_OUTER_BOUND('',#22457,.T.) ;
#18174 = FACE_OUTER_BOUND('',#22458,.T.) ;
#18175 = FACE_OUTER_BOUND('',#22459,.T.) ;
#18176 = FACE_OUTER_BOUND('',#22460,.T.) ;
#18177 = FACE_OUTER_BOUND('',#22461,.T.) ;
#18178 = FACE_OUTER_BOUND('',#22462,.T.) ;
#18179 = FACE_OUTER_BOUND('',#22463,.T.) ;
#18180 = FACE_OUTER_BOUND('',#22464,.T.) ;
#18181 = FACE_OUTER_BOUND('',#22465,.T.) ;
#18182 = FACE_OUTER_BOUND('',#22466,.T.) ;
#18183 = FACE_OUTER_BOUND('',#22467,.T.) ;
#18184 = FACE_OUTER_BOUND('',#22468,.T.) ;
#18185 = FACE_OUTER_BOUND('',#22469,.T.) ;
#18186 = FACE_OUTER_BOUND('',#22470,.T.) ;
#18187 = FACE_OUTER_BOUND('',#22471,.T.) ;
#18188 = FACE_OUTER_BOUND('',#22472,.T.) ;
#18189 = FACE_OUTER_BOUND('',#22473,.T.) ;
#18190 = FACE_OUTER_BOUND('',#22474,.T.) ;
#18191 = FACE_OUTER_BOUND('',#22475,.T.) ;
#18192 = FACE_OUTER_BOUND('',#22476,.T.) ;
#18193 = FACE_OUTER_BOUND('',#22477,.T.) ;
#18194 = FACE_OUTER_BOUND('',#22478,.T.) ;
#18195 = FACE_OUTER_BOUND('',#22479,.T.) ;
#18196 = FACE_OUTER_BOUND('',#22480,.T.) ;
#18197 = FACE_OUTER_BOUND('',#22481,.T.) ;
#18198 = FACE_OUTER_BOUND('',#22482,.T.) ;
#18199 = FACE_OUTER_BOUND('',#22483,.T.) ;
#18200 = FACE_OUTER_BOUND('',#22484,.T.) ;
#18201 = FACE_OUTER_BOUND('',#22485,.T.) ;
#18202 = FACE_OUTER_BOUND('',#22486,.T.) ;
#18203 = FACE_OUTER_BOUND('',#22497,.T.) ;
#18204 = FACE_OUTER_BOUND('',#22498,.T.) ;
#18205 = FACE_OUTER_BOUND('',#22499,.T.) ;
#18206 = FACE_OUTER_BOUND('',#22500,.T.) ;
#18207 = FACE_OUTER_BOUND('',#22501,.T.) ;
#18208 = FACE_OUTER_BOUND('',#22502,.T.) ;
#18209 = FACE_OUTER_BOUND('',#22503,.T.) ;
#18210 = FACE_OUTER_BOUND('',#22504,.T.) ;
#18211 = FACE_OUTER_BOUND('',#22505,.T.) ;
#18212 = FACE_OUTER_BOUND('',#22506,.T.) ;
#18213 = FACE_OUTER_BOUND('',#22507,.T.) ;
#18214 = FACE_OUTER_BOUND('',#22508,.T.) ;
#18215 = FACE_OUTER_BOUND('',#22509,.T.) ;
#18216 = FACE_OUTER_BOUND('',#22510,.T.) ;
#18217 = FACE_OUTER_BOUND('',#22511,.T.) ;
#18218 = FACE_OUTER_BOUND('',#22512,.T.) ;
#18219 = FACE_OUTER_BOUND('',#22513,.T.) ;
#18220 = FACE_OUTER_BOUND('',#22514,.T.) ;
#18221 = FACE_OUTER_BOUND('',#22515,.T.) ;
#18222 = FACE_OUTER_BOUND('',#22516,.T.) ;
#18223 = FACE_OUTER_BOUND('',#22517,.T.) ;
#18224 = FACE_OUTER_BOUND('',#22518,.T.) ;
#18225 = FACE_OUTER_BOUND('',#22519,.T.) ;
#18226 = FACE_OUTER_BOUND('',#22520,.T.) ;
#18227 = FACE_OUTER_BOUND('',#22521,.T.) ;
#18228 = FACE_OUTER_BOUND('',#22522,.T.) ;
#18229 = FACE_OUTER_BOUND('',#22523,.T.) ;
#18230 = FACE_OUTER_BOUND('',#22524,.T.) ;
#18231 = FACE_OUTER_BOUND('',#22525,.T.) ;
#18232 = FACE_OUTER_BOUND('',#22526,.T.) ;
#18233 = FACE_OUTER_BOUND('',#22527,.T.) ;
#18234 = FACE_OUTER_BOUND('',#22528,.T.) ;
#18235 = FACE_OUTER_BOUND('',#22529,.T.) ;
#18236 = FACE_OUTER_BOUND('',#22530,.T.) ;
#18237 = FACE_OUTER_BOUND('',#22531,.T.) ;
#18238 = FACE_OUTER_BOUND('',#22532,.T.) ;
#18239 = FACE_OUTER_BOUND('',#22534,.T.) ;
#18240 = FACE_OUTER_BOUND('',#22536,.T.) ;
#18241 = FACE_OUTER_BOUND('',#22537,.T.) ;
#18242 = FACE_OUTER_BOUND('',#22538,.T.) ;
#18243 = FACE_OUTER_BOUND('',#22539,.T.) ;
#18244 = FACE_OUTER_BOUND('',#22540,.T.) ;
#18245 = FACE_OUTER_BOUND('',#22541,.T.) ;
#18246 = FACE_OUTER_BOUND('',#22542,.T.) ;
#18247 = FACE_OUTER_BOUND('',#22543,.T.) ;
#18248 = FACE_OUTER_BOUND('',#22544,.T.) ;
#18249 = FACE_OUTER_BOUND('',#22545,.T.) ;
#18250 = FACE_OUTER_BOUND('',#22546,.T.) ;
#18251 = FACE_OUTER_BOUND('',#22547,.T.) ;
#18252 = FACE_OUTER_BOUND('',#22548,.T.) ;
#18253 = FACE_OUTER_BOUND('',#22549,.T.) ;
#18254 = FACE_OUTER_BOUND('',#22550,.T.) ;
#18255 = FACE_OUTER_BOUND('',#22551,.T.) ;
#18256 = FACE_OUTER_BOUND('',#22552,.T.) ;
#18257 = FACE_OUTER_BOUND('',#22553,.T.) ;
#18258 = FACE_OUTER_BOUND('',#22554,.T.) ;
#18259 = FACE_OUTER_BOUND('',#22555,.T.) ;
#18260 = FACE_OUTER_BOUND('',#22556,.T.) ;
#18261 = FACE_OUTER_BOUND('',#22557,.T.) ;
#18262 = FACE_OUTER_BOUND('',#22558,.T.) ;
#18263 = FACE_OUTER_BOUND('',#22559,.T.) ;
#18264 = FACE_OUTER_BOUND('',#22560,.T.) ;
#18265 = FACE_OUTER_BOUND('',#22561,.T.) ;
#18266 = FACE_OUTER_BOUND('',#22562,.T.) ;
#18267 = FACE_OUTER_BOUND('',#22563,.T.) ;
#18268 = FACE_OUTER_BOUND('',#22564,.T.) ;
#18269 = FACE_OUTER_BOUND('',#22565,.T.) ;
#18270 = FACE_OUTER_BOUND('',#22566,.T.) ;
#18271 = FACE_OUTER_BOUND('',#22567,.T.) ;
#18272 = FACE_OUTER_BOUND('',#22568,.T.) ;
#18273 = FACE_OUTER_BOUND('',#22569,.T.) ;
#18274 = FACE_OUTER_BOUND('',#22570,.T.) ;
#18275 = FACE_OUTER_BOUND('',#22571,.T.) ;
#18276 = FACE_OUTER_BOUND('',#22572,.T.) ;
#18277 = FACE_OUTER_BOUND('',#22573,.T.) ;
#18278 = FACE_OUTER_BOUND('',#22574,.T.) ;
#18279 = FACE_OUTER_BOUND('',#22575,.T.) ;
#18280 = FACE_OUTER_BOUND('',#22576,.T.) ;
#18281 = FACE_OUTER_BOUND('',#22577,.T.) ;
#18282 = FACE_OUTER_BOUND('',#22578,.T.) ;
#18283 = FACE_OUTER_BOUND('',#22579,.T.) ;
#18284 = FACE_OUTER_BOUND('',#22580,.T.) ;
#18285 = FACE_OUTER_BOUND('',#22581,.T.) ;
#18286 = FACE_OUTER_BOUND('',#22582,.T.) ;
#18287 = FACE_OUTER_BOUND('',#22583,.T.) ;
#18288 = FACE_OUTER_BOUND('',#22584,.T.) ;
#18289 = FACE_OUTER_BOUND('',#22585,.T.) ;
#18290 = FACE_OUTER_BOUND('',#22586,.T.) ;
#18291 = FACE_OUTER_BOUND('',#22587,.T.) ;
#18292 = FACE_OUTER_BOUND('',#22588,.T.) ;
#18293 = FACE_OUTER_BOUND('',#22589,.T.) ;
#18294 = FACE_OUTER_BOUND('',#22590,.T.) ;
#18295 = FACE_OUTER_BOUND('',#22591,.T.) ;
#18296 = FACE_OUTER_BOUND('',#22592,.T.) ;
#18297 = FACE_OUTER_BOUND('',#22593,.T.) ;
#18298 = FACE_OUTER_BOUND('',#22594,.T.) ;
#18299 = FACE_OUTER_BOUND('',#22595,.T.) ;
#18300 = FACE_OUTER_BOUND('',#22596,.T.) ;
#18301 = FACE_OUTER_BOUND('',#22597,.T.) ;
#18302 = FACE_OUTER_BOUND('',#22598,.T.) ;
#18303 = FACE_OUTER_BOUND('',#22599,.T.) ;
#18304 = FACE_OUTER_BOUND('',#22600,.T.) ;
#18305 = FACE_OUTER_BOUND('',#22601,.T.) ;
#18306 = FACE_OUTER_BOUND('',#22602,.T.) ;
#18307 = FACE_OUTER_BOUND('',#22603,.T.) ;
#18308 = FACE_OUTER_BOUND('',#22604,.T.) ;
#18309 = FACE_OUTER_BOUND('',#22605,.T.) ;
#18310 = FACE_OUTER_BOUND('',#22606,.T.) ;
#18311 = FACE_OUTER_BOUND('',#22607,.T.) ;
#18312 = FACE_OUTER_BOUND('',#22608,.T.) ;
#18313 = FACE_OUTER_BOUND('',#22609,.T.) ;
#18314 = FACE_OUTER_BOUND('',#22610,.T.) ;
#18315 = FACE_OUTER_BOUND('',#22611,.T.) ;
#18316 = FACE_OUTER_BOUND('',#22612,.T.) ;
#18317 = FACE_OUTER_BOUND('',#22613,.T.) ;
#18318 = FACE_OUTER_BOUND('',#22614,.T.) ;
#18319 = FACE_OUTER_BOUND('',#22615,.T.) ;
#18320 = FACE_OUTER_BOUND('',#22616,.T.) ;
#18321 = FACE_OUTER_BOUND('',#22617,.T.) ;
#18322 = FACE_OUTER_BOUND('',#22618,.T.) ;
#18323 = FACE_OUTER_BOUND('',#22619,.T.) ;
#18324 = FACE_OUTER_BOUND('',#22620,.T.) ;
#18325 = FACE_OUTER_BOUND('',#22621,.T.) ;
#18326 = FACE_OUTER_BOUND('',#22622,.T.) ;
#18327 = FACE_OUTER_BOUND('',#22623,.T.) ;
#18328 = FACE_OUTER_BOUND('',#22624,.T.) ;
#18329 = FACE_OUTER_BOUND('',#22625,.T.) ;
#18330 = FACE_OUTER_BOUND('',#22626,.T.) ;
#18331 = FACE_OUTER_BOUND('',#22627,.T.) ;
#18332 = FACE_OUTER_BOUND('',#22628,.T.) ;
#18333 = FACE_OUTER_BOUND('',#22629,.T.) ;
#18334 = FACE_OUTER_BOUND('',#22630,.T.) ;
#18335 = FACE_OUTER_BOUND('',#22631,.T.) ;
#18336 = FACE_OUTER_BOUND('',#22632,.T.) ;
#18337 = FACE_OUTER_BOUND('',#22633,.T.) ;
#18338 = FACE_OUTER_BOUND('',#22634,.T.) ;
#18339 = FACE_OUTER_BOUND('',#22635,.T.) ;
#18340 = FACE_OUTER_BOUND('',#22636,.T.) ;
#18341 = FACE_OUTER_BOUND('',#22637,.T.) ;
#18342 = FACE_OUTER_BOUND('',#22638,.T.) ;
#18343 = FACE_OUTER_BOUND('',#22639,.T.) ;
#18344 = FACE_OUTER_BOUND('',#22640,.T.) ;
#18345 = FACE_OUTER_BOUND('',#22641,.T.) ;
#18346 = FACE_OUTER_BOUND('',#22642,.T.) ;
#18347 = FACE_OUTER_BOUND('',#22643,.T.) ;
#18348 = FACE_OUTER_BOUND('',#22644,.T.) ;
#18349 = FACE_OUTER_BOUND('',#22645,.T.) ;
#18350 = FACE_OUTER_BOUND('',#22646,.T.) ;
#18351 = FACE_OUTER_BOUND('',#22647,.T.) ;
#18352 = FACE_OUTER_BOUND('',#22648,.T.) ;
#18353 = FACE_OUTER_BOUND('',#22649,.T.) ;
#18354 = FACE_OUTER_BOUND('',#22650,.T.) ;
#18355 = FACE_OUTER_BOUND('',#22651,.T.) ;
#18356 = FACE_OUTER_BOUND('',#22652,.T.) ;
#18357 = FACE_OUTER_BOUND('',#22653,.T.) ;
#18358 = FACE_OUTER_BOUND('',#22654,.T.) ;
#18359 = FACE_OUTER_BOUND('',#22655,.T.) ;
#18360 = FACE_OUTER_BOUND('',#22656,.T.) ;
#18361 = FACE_OUTER_BOUND('',#22657,.T.) ;
#18362 = FACE_OUTER_BOUND('',#22658,.T.) ;
#18363 = FACE_OUTER_BOUND('',#22659,.T.) ;
#18364 = FACE_OUTER_BOUND('',#22660,.T.) ;
#18365 = FACE_OUTER_BOUND('',#22661,.T.) ;
#18366 = FACE_OUTER_BOUND('',#22662,.T.) ;
#18367 = FACE_OUTER_BOUND('',#22663,.T.) ;
#18368 = FACE_OUTER_BOUND('',#22664,.T.) ;
#18369 = FACE_OUTER_BOUND('',#22665,.T.) ;
#18370 = FACE_OUTER_BOUND('',#22666,.T.) ;
#18371 = FACE_OUTER_BOUND('',#22667,.T.) ;
#18372 = FACE_OUTER_BOUND('',#22668,.T.) ;
#18373 = FACE_OUTER_BOUND('',#22669,.T.) ;
#18374 = FACE_OUTER_BOUND('',#22670,.T.) ;
#18375 = FACE_OUTER_BOUND('',#22671,.T.) ;
#18376 = FACE_OUTER_BOUND('',#22672,.T.) ;
#18377 = FACE_OUTER_BOUND('',#22673,.T.) ;
#18378 = FACE_OUTER_BOUND('',#22674,.T.) ;
#18379 = FACE_OUTER_BOUND('',#22675,.T.) ;
#18380 = FACE_OUTER_BOUND('',#22676,.T.) ;
#18381 = FACE_OUTER_BOUND('',#22677,.T.) ;
#18382 = FACE_OUTER_BOUND('',#22678,.T.) ;
#18383 = FACE_OUTER_BOUND('',#22679,.T.) ;
#18384 = FACE_OUTER_BOUND('',#22680,.T.) ;
#18385 = FACE_OUTER_BOUND('',#22681,.T.) ;
#18386 = FACE_OUTER_BOUND('',#22682,.T.) ;
#18387 = FACE_OUTER_BOUND('',#22683,.T.) ;
#18388 = FACE_OUTER_BOUND('',#22684,.T.) ;
#18389 = FACE_OUTER_BOUND('',#22685,.T.) ;
#18390 = FACE_OUTER_BOUND('',#22686,.T.) ;
#18391 = FACE_OUTER_BOUND('',#22687,.T.) ;
#18392 = FACE_OUTER_BOUND('',#22688,.T.) ;
#18393 = FACE_OUTER_BOUND('',#22689,.T.) ;
#18394 = FACE_OUTER_BOUND('',#22690,.T.) ;
#18395 = FACE_OUTER_BOUND('',#22691,.T.) ;
#18396 = FACE_OUTER_BOUND('',#22692,.T.) ;
#18397 = FACE_OUTER_BOUND('',#22693,.T.) ;
#18398 = FACE_OUTER_BOUND('',#22694,.T.) ;
#18399 = FACE_OUTER_BOUND('',#22695,.T.) ;
#18400 = FACE_OUTER_BOUND('',#22696,.T.) ;
#18401 = FACE_OUTER_BOUND('',#22697,.T.) ;
#18402 = FACE_OUTER_BOUND('',#22698,.T.) ;
#18403 = FACE_OUTER_BOUND('',#22699,.T.) ;
#18404 = FACE_OUTER_BOUND('',#22700,.T.) ;
#18405 = FACE_OUTER_BOUND('',#22701,.T.) ;
#18406 = FACE_OUTER_BOUND('',#22702,.T.) ;
#18407 = FACE_OUTER_BOUND('',#22703,.T.) ;
#18408 = FACE_OUTER_BOUND('',#22704,.T.) ;
#18409 = FACE_OUTER_BOUND('',#22705,.T.) ;
#18410 = FACE_OUTER_BOUND('',#22706,.T.) ;
#18411 = FACE_OUTER_BOUND('',#22707,.T.) ;
#18412 = FACE_OUTER_BOUND('',#22708,.T.) ;
#18413 = FACE_OUTER_BOUND('',#22709,.T.) ;
#18414 = FACE_OUTER_BOUND('',#22710,.T.) ;
#18415 = FACE_OUTER_BOUND('',#22711,.T.) ;
#18416 = FACE_OUTER_BOUND('',#22712,.T.) ;
#18417 = FACE_OUTER_BOUND('',#22713,.T.) ;
#18418 = FACE_OUTER_BOUND('',#22714,.T.) ;
#18419 = FACE_OUTER_BOUND('',#22715,.T.) ;
#18420 = FACE_OUTER_BOUND('',#22716,.T.) ;
#18421 = FACE_OUTER_BOUND('',#22717,.T.) ;
#18422 = FACE_OUTER_BOUND('',#22718,.T.) ;
#18423 = FACE_OUTER_BOUND('',#22719,.T.) ;
#18424 = FACE_OUTER_BOUND('',#22720,.T.) ;
#18425 = FACE_OUTER_BOUND('',#22721,.T.) ;
#18426 = FACE_OUTER_BOUND('',#22722,.T.) ;
#18427 = FACE_OUTER_BOUND('',#22723,.T.) ;
#18428 = FACE_OUTER_BOUND('',#22724,.T.) ;
#18429 = FACE_OUTER_BOUND('',#22725,.T.) ;
#18430 = FACE_OUTER_BOUND('',#22726,.T.) ;
#18431 = FACE_OUTER_BOUND('',#22727,.T.) ;
#18432 = FACE_OUTER_BOUND('',#22728,.T.) ;
#18433 = FACE_OUTER_BOUND('',#22729,.T.) ;
#18434 = FACE_OUTER_BOUND('',#22730,.T.) ;
#18435 = FACE_OUTER_BOUND('',#22731,.T.) ;
#18436 = FACE_OUTER_BOUND('',#22732,.T.) ;
#18437 = FACE_OUTER_BOUND('',#22733,.T.) ;
#18438 = FACE_OUTER_BOUND('',#22734,.T.) ;
#18439 = FACE_OUTER_BOUND('',#22735,.T.) ;
#18440 = FACE_OUTER_BOUND('',#22736,.T.) ;
#18441 = FACE_OUTER_BOUND('',#22737,.T.) ;
#18442 = FACE_OUTER_BOUND('',#22738,.T.) ;
#18443 = FACE_OUTER_BOUND('',#22739,.T.) ;
#18444 = FACE_OUTER_BOUND('',#22740,.T.) ;
#18445 = FACE_OUTER_BOUND('',#22741,.T.) ;
#18446 = FACE_OUTER_BOUND('',#22742,.T.) ;
#18447 = FACE_OUTER_BOUND('',#22743,.T.) ;
#18448 = FACE_OUTER_BOUND('',#22744,.T.) ;
#18449 = FACE_OUTER_BOUND('',#22745,.T.) ;
#18450 = FACE_OUTER_BOUND('',#22746,.T.) ;
#18451 = FACE_OUTER_BOUND('',#22747,.T.) ;
#18452 = FACE_OUTER_BOUND('',#22748,.T.) ;
#18453 = FACE_OUTER_BOUND('',#22749,.T.) ;
#18454 = FACE_OUTER_BOUND('',#22750,.T.) ;
#18455 = FACE_OUTER_BOUND('',#22751,.T.) ;
#18456 = FACE_OUTER_BOUND('',#22752,.T.) ;
#18457 = FACE_OUTER_BOUND('',#22753,.T.) ;
#18458 = FACE_OUTER_BOUND('',#22754,.T.) ;
#18459 = FACE_OUTER_BOUND('',#22755,.T.) ;
#18460 = FACE_OUTER_BOUND('',#22756,.T.) ;
#18461 = FACE_OUTER_BOUND('',#22757,.T.) ;
#18462 = FACE_OUTER_BOUND('',#22758,.T.) ;
#18463 = FACE_OUTER_BOUND('',#22759,.T.) ;
#18464 = FACE_OUTER_BOUND('',#22760,.T.) ;
#18465 = FACE_OUTER_BOUND('',#22761,.T.) ;
#18466 = FACE_OUTER_BOUND('',#22762,.T.) ;
#18467 = FACE_OUTER_BOUND('',#22763,.T.) ;
#18468 = FACE_OUTER_BOUND('',#22764,.T.) ;
#18469 = FACE_OUTER_BOUND('',#22765,.T.) ;
#18470 = FACE_OUTER_BOUND('',#22766,.T.) ;
#18471 = FACE_OUTER_BOUND('',#22767,.T.) ;
#18472 = FACE_OUTER_BOUND('',#22768,.T.) ;
#18473 = FACE_OUTER_BOUND('',#22769,.T.) ;
#18474 = FACE_OUTER_BOUND('',#22770,.T.) ;
#18475 = FACE_OUTER_BOUND('',#22771,.T.) ;
#18476 = FACE_OUTER_BOUND('',#22772,.T.) ;
#18477 = FACE_OUTER_BOUND('',#22773,.T.) ;
#18478 = FACE_OUTER_BOUND('',#22774,.T.) ;
#18479 = FACE_OUTER_BOUND('',#22775,.T.) ;
#18480 = FACE_OUTER_BOUND('',#22776,.T.) ;
#18481 = FACE_OUTER_BOUND('',#22777,.T.) ;
#18482 = FACE_OUTER_BOUND('',#22778,.T.) ;
#18483 = FACE_OUTER_BOUND('',#22779,.T.) ;
#18484 = FACE_OUTER_BOUND('',#22780,.T.) ;
#18485 = FACE_OUTER_BOUND('',#22781,.T.) ;
#18486 = FACE_OUTER_BOUND('',#22782,.T.) ;
#18487 = FACE_OUTER_BOUND('',#22783,.T.) ;
#18488 = FACE_OUTER_BOUND('',#22784,.T.) ;
#18489 = FACE_OUTER_BOUND('',#22785,.T.) ;
#18490 = FACE_OUTER_BOUND('',#22786,.T.) ;
#18491 = FACE_OUTER_BOUND('',#22787,.T.) ;
#18492 = FACE_OUTER_BOUND('',#22788,.T.) ;
#18493 = FACE_OUTER_BOUND('',#22789,.T.) ;
#18494 = FACE_OUTER_BOUND('',#22790,.T.) ;
#18495 = FACE_OUTER_BOUND('',#22791,.T.) ;
#18496 = FACE_OUTER_BOUND('',#22792,.T.) ;
#18497 = FACE_OUTER_BOUND('',#22793,.T.) ;
#18498 = FACE_OUTER_BOUND('',#22794,.T.) ;
#18499 = FACE_OUTER_BOUND('',#22795,.T.) ;
#18500 = FACE_OUTER_BOUND('',#22796,.T.) ;
#18501 = FACE_OUTER_BOUND('',#22797,.T.) ;
#18502 = FACE_OUTER_BOUND('',#22798,.T.) ;
#18503 = FACE_OUTER_BOUND('',#22799,.T.) ;
#18504 = FACE_OUTER_BOUND('',#22800,.T.) ;
#18505 = FACE_OUTER_BOUND('',#22801,.T.) ;
#18506 = FACE_OUTER_BOUND('',#22802,.T.) ;
#18507 = FACE_OUTER_BOUND('',#22803,.T.) ;
#18508 = FACE_OUTER_BOUND('',#22804,.T.) ;
#18509 = FACE_OUTER_BOUND('',#22805,.T.) ;
#18510 = FACE_OUTER_BOUND('',#22806,.T.) ;
#18511 = FACE_OUTER_BOUND('',#22807,.T.) ;
#18512 = FACE_OUTER_BOUND('',#22808,.T.) ;
#18513 = FACE_OUTER_BOUND('',#22809,.T.) ;
#18514 = FACE_OUTER_BOUND('',#22810,.T.) ;
#18515 = FACE_OUTER_BOUND('',#22811,.T.) ;
#18516 = FACE_OUTER_BOUND('',#22812,.T.) ;
#18517 = FACE_OUTER_BOUND('',#22813,.T.) ;
#18518 = FACE_OUTER_BOUND('',#22814,.T.) ;
#18519 = FACE_OUTER_BOUND('',#22815,.T.) ;
#18520 = FACE_OUTER_BOUND('',#22816,.T.) ;
#18521 = FACE_OUTER_BOUND('',#22817,.T.) ;
#18522 = FACE_OUTER_BOUND('',#22818,.T.) ;
#18523 = FACE_OUTER_BOUND('',#22819,.T.) ;
#18524 = FACE_OUTER_BOUND('',#22820,.T.) ;
#18525 = FACE_OUTER_BOUND('',#22821,.T.) ;
#18526 = FACE_OUTER_BOUND('',#22823,.T.) ;
#18527 = FACE_OUTER_BOUND('',#22824,.T.) ;
#18528 = FACE_OUTER_BOUND('',#22825,.T.) ;
#18529 = FACE_OUTER_BOUND('',#22826,.T.) ;
#18530 = FACE_OUTER_BOUND('',#22827,.T.) ;
#18531 = FACE_OUTER_BOUND('',#22828,.T.) ;
#18532 = FACE_OUTER_BOUND('',#22829,.T.) ;
#18533 = FACE_OUTER_BOUND('',#22830,.T.) ;
#18534 = FACE_OUTER_BOUND('',#22831,.T.) ;
#18535 = FACE_OUTER_BOUND('',#22832,.T.) ;
#18536 = FACE_OUTER_BOUND('',#22833,.T.) ;
#18537 = FACE_OUTER_BOUND('',#22834,.T.) ;
#18538 = FACE_OUTER_BOUND('',#22835,.T.) ;
#18539 = FACE_OUTER_BOUND('',#22836,.T.) ;
#18540 = FACE_OUTER_BOUND('',#22837,.T.) ;
#18541 = FACE_OUTER_BOUND('',#22838,.T.) ;
#18542 = FACE_OUTER_BOUND('',#22839,.T.) ;
#18543 = FACE_OUTER_BOUND('',#22840,.T.) ;
#18544 = FACE_OUTER_BOUND('',#22841,.T.) ;
#18545 = FACE_OUTER_BOUND('',#22842,.T.) ;
#18546 = FACE_OUTER_BOUND('',#22843,.T.) ;
#18547 = FACE_OUTER_BOUND('',#22844,.T.) ;
#18548 = FACE_OUTER_BOUND('',#22845,.T.) ;
#18549 = FACE_OUTER_BOUND('',#22846,.T.) ;
#18550 = FACE_OUTER_BOUND('',#22847,.T.) ;
#18551 = FACE_OUTER_BOUND('',#22848,.T.) ;
#18552 = FACE_OUTER_BOUND('',#22849,.T.) ;
#18553 = FACE_OUTER_BOUND('',#22850,.T.) ;
#18554 = FACE_OUTER_BOUND('',#22852,.T.) ;
#18555 = FACE_OUTER_BOUND('',#22853,.T.) ;
#18556 = FACE_OUTER_BOUND('',#22854,.T.) ;
#18557 = FACE_OUTER_BOUND('',#22855,.T.) ;
#18558 = FACE_OUTER_BOUND('',#22856,.T.) ;
#18559 = FACE_OUTER_BOUND('',#22857,.T.) ;
#18560 = FACE_OUTER_BOUND('',#22858,.T.) ;
#18561 = FACE_OUTER_BOUND('',#22859,.T.) ;
#18562 = FACE_OUTER_BOUND('',#22860,.T.) ;
#18563 = FACE_OUTER_BOUND('',#22861,.T.) ;
#18564 = FACE_OUTER_BOUND('',#22862,.T.) ;
#18565 = FACE_OUTER_BOUND('',#22863,.T.) ;
#18566 = FACE_OUTER_BOUND('',#22864,.T.) ;
#18567 = FACE_OUTER_BOUND('',#22865,.T.) ;
#18568 = FACE_OUTER_BOUND('',#22866,.T.) ;
#18569 = FACE_OUTER_BOUND('',#22867,.T.) ;
#18570 = FACE_OUTER_BOUND('',#22868,.T.) ;
#18571 = FACE_OUTER_BOUND('',#22869,.T.) ;
#18572 = FACE_OUTER_BOUND('',#22870,.T.) ;
#18573 = FACE_OUTER_BOUND('',#22871,.T.) ;
#18574 = FACE_OUTER_BOUND('',#22872,.T.) ;
#18575 = FACE_OUTER_BOUND('',#22873,.T.) ;
#18576 = FACE_OUTER_BOUND('',#22874,.T.) ;
#18577 = FACE_OUTER_BOUND('',#22875,.T.) ;
#18578 = FACE_OUTER_BOUND('',#22876,.T.) ;
#18579 = FACE_OUTER_BOUND('',#22877,.T.) ;
#18580 = FACE_OUTER_BOUND('',#22878,.T.) ;
#18581 = FACE_OUTER_BOUND('',#22879,.T.) ;
#18582 = FACE_OUTER_BOUND('',#22881,.T.) ;
#18583 = FACE_OUTER_BOUND('',#22882,.T.) ;
#18584 = FACE_OUTER_BOUND('',#22883,.T.) ;
#18585 = FACE_OUTER_BOUND('',#22884,.T.) ;
#18586 = FACE_OUTER_BOUND('',#22885,.T.) ;
#18587 = FACE_OUTER_BOUND('',#22886,.T.) ;
#18588 = FACE_OUTER_BOUND('',#22887,.T.) ;
#18589 = FACE_OUTER_BOUND('',#22888,.T.) ;
#18590 = FACE_OUTER_BOUND('',#22889,.T.) ;
#18591 = FACE_OUTER_BOUND('',#22890,.T.) ;
#18592 = FACE_OUTER_BOUND('',#22891,.T.) ;
#18593 = FACE_OUTER_BOUND('',#22892,.T.) ;
#18594 = FACE_OUTER_BOUND('',#22893,.T.) ;
#18595 = FACE_OUTER_BOUND('',#22894,.T.) ;
#18596 = FACE_OUTER_BOUND('',#22895,.T.) ;
#18597 = FACE_OUTER_BOUND('',#22896,.T.) ;
#18598 = FACE_OUTER_BOUND('',#22897,.T.) ;
#18599 = FACE_OUTER_BOUND('',#22898,.T.) ;
#18600 = FACE_OUTER_BOUND('',#22899,.T.) ;
#18601 = FACE_OUTER_BOUND('',#22900,.T.) ;
#18602 = FACE_OUTER_BOUND('',#22901,.T.) ;
#18603 = FACE_OUTER_BOUND('',#22902,.T.) ;
#18604 = FACE_OUTER_BOUND('',#22903,.T.) ;
#18605 = FACE_OUTER_BOUND('',#22904,.T.) ;
#18606 = FACE_OUTER_BOUND('',#22905,.T.) ;
#18607 = FACE_OUTER_BOUND('',#22906,.T.) ;
#18608 = FACE_OUTER_BOUND('',#22907,.T.) ;
#18609 = FACE_OUTER_BOUND('',#22908,.T.) ;
#18610 = FACE_OUTER_BOUND('',#22910,.T.) ;
#18611 = FACE_OUTER_BOUND('',#22911,.T.) ;
#18612 = FACE_OUTER_BOUND('',#22912,.T.) ;
#18613 = FACE_OUTER_BOUND('',#22913,.T.) ;
#18614 = FACE_OUTER_BOUND('',#22914,.T.) ;
#18615 = FACE_OUTER_BOUND('',#22915,.T.) ;
#18616 = FACE_OUTER_BOUND('',#22916,.T.) ;
#18617 = FACE_OUTER_BOUND('',#22917,.T.) ;
#18618 = FACE_OUTER_BOUND('',#22918,.T.) ;
#18619 = FACE_OUTER_BOUND('',#22919,.T.) ;
#18620 = FACE_OUTER_BOUND('',#22920,.T.) ;
#18621 = FACE_OUTER_BOUND('',#22921,.T.) ;
#18622 = FACE_OUTER_BOUND('',#22922,.T.) ;
#18623 = FACE_OUTER_BOUND('',#22923,.T.) ;
#18624 = FACE_OUTER_BOUND('',#22924,.T.) ;
#18625 = FACE_OUTER_BOUND('',#22925,.T.) ;
#18626 = FACE_OUTER_BOUND('',#22926,.T.) ;
#18627 = FACE_OUTER_BOUND('',#22927,.T.) ;
#18628 = FACE_OUTER_BOUND('',#22928,.T.) ;
#18629 = FACE_OUTER_BOUND('',#22929,.T.) ;
#18630 = FACE_OUTER_BOUND('',#22930,.T.) ;
#18631 = FACE_OUTER_BOUND('',#22931,.T.) ;
#18632 = FACE_OUTER_BOUND('',#22932,.T.) ;
#18633 = FACE_OUTER_BOUND('',#22933,.T.) ;
#18634 = FACE_OUTER_BOUND('',#22934,.T.) ;
#18635 = FACE_OUTER_BOUND('',#22935,.T.) ;
#18636 = FACE_OUTER_BOUND('',#22936,.T.) ;
#18637 = FACE_OUTER_BOUND('',#22937,.T.) ;
#18638 = FACE_OUTER_BOUND('',#22939,.T.) ;
#18639 = FACE_OUTER_BOUND('',#22940,.T.) ;
#18640 = FACE_OUTER_BOUND('',#22941,.T.) ;
#18641 = FACE_OUTER_BOUND('',#22942,.T.) ;
#18642 = FACE_OUTER_BOUND('',#22943,.T.) ;
#18643 = FACE_OUTER_BOUND('',#22944,.T.) ;
#18644 = FACE_OUTER_BOUND('',#22945,.T.) ;
#18645 = FACE_OUTER_BOUND('',#22946,.T.) ;
#18646 = FACE_OUTER_BOUND('',#22947,.T.) ;
#18647 = FACE_OUTER_BOUND('',#22948,.T.) ;
#18648 = FACE_OUTER_BOUND('',#22949,.T.) ;
#18649 = FACE_OUTER_BOUND('',#22950,.T.) ;
#18650 = FACE_OUTER_BOUND('',#22951,.T.) ;
#18651 = FACE_OUTER_BOUND('',#22952,.T.) ;
#18652 = FACE_OUTER_BOUND('',#22953,.T.) ;
#18653 = FACE_OUTER_BOUND('',#22954,.T.) ;
#18654 = FACE_OUTER_BOUND('',#22955,.T.) ;
#18655 = FACE_OUTER_BOUND('',#22956,.T.) ;
#18656 = FACE_OUTER_BOUND('',#22957,.T.) ;
#18657 = FACE_OUTER_BOUND('',#22958,.T.) ;
#18658 = FACE_OUTER_BOUND('',#22959,.T.) ;
#18659 = FACE_OUTER_BOUND('',#22960,.T.) ;
#18660 = FACE_OUTER_BOUND('',#22961,.T.) ;
#18661 = FACE_OUTER_BOUND('',#22962,.T.) ;
#18662 = FACE_OUTER_BOUND('',#22963,.T.) ;
#18663 = FACE_OUTER_BOUND('',#22964,.T.) ;
#18664 = FACE_OUTER_BOUND('',#22965,.T.) ;
#18665 = FACE_OUTER_BOUND('',#22966,.T.) ;
#18666 = FACE_OUTER_BOUND('',#22968,.T.) ;
#18667 = FACE_OUTER_BOUND('',#22969,.T.) ;
#18668 = FACE_OUTER_BOUND('',#22970,.T.) ;
#18669 = FACE_OUTER_BOUND('',#22971,.T.) ;
#18670 = FACE_OUTER_BOUND('',#22972,.T.) ;
#18671 = FACE_OUTER_BOUND('',#22973,.T.) ;
#18672 = FACE_OUTER_BOUND('',#22974,.T.) ;
#18673 = FACE_OUTER_BOUND('',#22975,.T.) ;
#18674 = FACE_OUTER_BOUND('',#22976,.T.) ;
#18675 = FACE_OUTER_BOUND('',#22977,.T.) ;
#18676 = FACE_OUTER_BOUND('',#22978,.T.) ;
#18677 = FACE_OUTER_BOUND('',#22979,.T.) ;
#18678 = FACE_OUTER_BOUND('',#22980,.T.) ;
#18679 = FACE_OUTER_BOUND('',#22981,.T.) ;
#18680 = FACE_OUTER_BOUND('',#22982,.T.) ;
#18681 = FACE_OUTER_BOUND('',#22983,.T.) ;
#18682 = FACE_OUTER_BOUND('',#22984,.T.) ;
#18683 = FACE_OUTER_BOUND('',#22985,.T.) ;
#18684 = FACE_OUTER_BOUND('',#22986,.T.) ;
#18685 = FACE_OUTER_BOUND('',#22987,.T.) ;
#18686 = FACE_OUTER_BOUND('',#22988,.T.) ;
#18687 = FACE_OUTER_BOUND('',#22989,.T.) ;
#18688 = FACE_OUTER_BOUND('',#22990,.T.) ;
#18689 = FACE_OUTER_BOUND('',#22991,.T.) ;
#18690 = FACE_OUTER_BOUND('',#22992,.T.) ;
#18691 = FACE_OUTER_BOUND('',#22993,.T.) ;
#18692 = FACE_OUTER_BOUND('',#22994,.T.) ;
#18693 = FACE_OUTER_BOUND('',#22995,.T.) ;
#18694 = FACE_OUTER_BOUND('',#22997,.T.) ;
#18695 = FACE_OUTER_BOUND('',#22998,.T.) ;
#18696 = FACE_OUTER_BOUND('',#22999,.T.) ;
#18697 = FACE_OUTER_BOUND('',#23000,.T.) ;
#18698 = FACE_OUTER_BOUND('',#23001,.T.) ;
#18699 = FACE_OUTER_BOUND('',#23002,.T.) ;
#18700 = FACE_OUTER_BOUND('',#23003,.T.) ;
#18701 = FACE_OUTER_BOUND('',#23004,.T.) ;
#18702 = FACE_OUTER_BOUND('',#23005,.T.) ;
#18703 = FACE_OUTER_BOUND('',#23006,.T.) ;
#18704 = FACE_OUTER_BOUND('',#23007,.T.) ;
#18705 = FACE_OUTER_BOUND('',#23008,.T.) ;
#18706 = FACE_OUTER_BOUND('',#23009,.T.) ;
#18707 = FACE_OUTER_BOUND('',#23010,.T.) ;
#18708 = FACE_OUTER_BOUND('',#23011,.T.) ;
#18709 = FACE_OUTER_BOUND('',#23012,.T.) ;
#18710 = FACE_OUTER_BOUND('',#23013,.T.) ;
#18711 = FACE_OUTER_BOUND('',#23014,.T.) ;
#18712 = FACE_OUTER_BOUND('',#23015,.T.) ;
#18713 = FACE_OUTER_BOUND('',#23016,.T.) ;
#18714 = FACE_OUTER_BOUND('',#23017,.T.) ;
#18715 = FACE_OUTER_BOUND('',#23018,.T.) ;
#18716 = FACE_OUTER_BOUND('',#23019,.T.) ;
#18717 = FACE_OUTER_BOUND('',#23020,.T.) ;
#18718 = FACE_OUTER_BOUND('',#23021,.T.) ;
#18719 = FACE_OUTER_BOUND('',#23022,.T.) ;
#18720 = FACE_OUTER_BOUND('',#23023,.T.) ;
#18721 = FACE_OUTER_BOUND('',#23024,.T.) ;
#18722 = FACE_OUTER_BOUND('',#23026,.T.) ;
#18723 = FACE_OUTER_BOUND('',#23027,.T.) ;
#18724 = FACE_OUTER_BOUND('',#23028,.T.) ;
#18725 = FACE_OUTER_BOUND('',#23029,.T.) ;
#18726 = FACE_OUTER_BOUND('',#23030,.T.) ;
#18727 = FACE_OUTER_BOUND('',#23031,.T.) ;
#18728 = FACE_OUTER_BOUND('',#23032,.T.) ;
#18729 = FACE_OUTER_BOUND('',#23033,.T.) ;
#18730 = FACE_OUTER_BOUND('',#23034,.T.) ;
#18731 = FACE_OUTER_BOUND('',#23035,.T.) ;
#18732 = FACE_OUTER_BOUND('',#23036,.T.) ;
#18733 = FACE_OUTER_BOUND('',#23037,.T.) ;
#18734 = FACE_OUTER_BOUND('',#23038,.T.) ;
#18735 = FACE_OUTER_BOUND('',#23039,.T.) ;
#18736 = FACE_OUTER_BOUND('',#23040,.T.) ;
#18737 = FACE_OUTER_BOUND('',#23041,.T.) ;
#18738 = FACE_OUTER_BOUND('',#23042,.T.) ;
#18739 = FACE_OUTER_BOUND('',#23043,.T.) ;
#18740 = FACE_OUTER_BOUND('',#23044,.T.) ;
#18741 = FACE_OUTER_BOUND('',#23045,.T.) ;
#18742 = FACE_OUTER_BOUND('',#23046,.T.) ;
#18743 = FACE_OUTER_BOUND('',#23047,.T.) ;
#18744 = FACE_OUTER_BOUND('',#23048,.T.) ;
#18745 = FACE_OUTER_BOUND('',#23049,.T.) ;
#18746 = FACE_OUTER_BOUND('',#23050,.T.) ;
#18747 = FACE_OUTER_BOUND('',#23051,.T.) ;
#18748 = FACE_OUTER_BOUND('',#23052,.T.) ;
#18749 = FACE_OUTER_BOUND('',#23053,.T.) ;
#18750 = FACE_OUTER_BOUND('',#23055,.T.) ;
#18751 = FACE_OUTER_BOUND('',#23057,.T.) ;
#18752 = FACE_OUTER_BOUND('',#23059,.T.) ;
#18753 = FACE_OUTER_BOUND('',#23061,.T.) ;
#18754 = FACE_OUTER_BOUND('',#23063,.T.) ;
#18755 = FACE_OUTER_BOUND('',#23065,.T.) ;
#18756 = FACE_OUTER_BOUND('',#23067,.T.) ;
#18757 = FACE_OUTER_BOUND('',#23069,.T.) ;
#18758 = FACE_OUTER_BOUND('',#23071,.T.) ;
#18759 = FACE_OUTER_BOUND('',#23073,.T.) ;
#18760 = FACE_OUTER_BOUND('',#23074,.T.) ;
#18761 = FACE_OUTER_BOUND('',#23075,.T.) ;
#18762 = FACE_OUTER_BOUND('',#23076,.T.) ;
#18763 = FACE_OUTER_BOUND('',#23077,.T.) ;
#18764 = FACE_OUTER_BOUND('',#23078,.T.) ;
#18765 = FACE_OUTER_BOUND('',#23079,.T.) ;
#18766 = FACE_OUTER_BOUND('',#23080,.T.) ;
#18767 = FACE_OUTER_BOUND('',#23081,.T.) ;
#18768 = FACE_OUTER_BOUND('',#23082,.T.) ;
#18769 = FACE_OUTER_BOUND('',#23083,.T.) ;
#18770 = FACE_OUTER_BOUND('',#23084,.T.) ;
#18771 = FACE_OUTER_BOUND('',#23085,.T.) ;
#18772 = FACE_OUTER_BOUND('',#23086,.T.) ;
#18773 = FACE_OUTER_BOUND('',#23087,.T.) ;
#18774 = FACE_OUTER_BOUND('',#23088,.T.) ;
#18775 = FACE_OUTER_BOUND('',#23089,.T.) ;
#18776 = FACE_OUTER_BOUND('',#23090,.T.) ;
#18777 = FACE_OUTER_BOUND('',#23091,.T.) ;
#18778 = FACE_OUTER_BOUND('',#23092,.T.) ;
#18779 = FACE_OUTER_BOUND('',#23093,.T.) ;
#18780 = FACE_OUTER_BOUND('',#23094,.T.) ;
#18781 = FACE_OUTER_BOUND('',#23095,.T.) ;
#18782 = FACE_OUTER_BOUND('',#23096,.T.) ;
#18783 = FACE_OUTER_BOUND('',#23097,.T.) ;
#18784 = FACE_OUTER_BOUND('',#23098,.T.) ;
#18785 = FACE_OUTER_BOUND('',#23099,.T.) ;
#18786 = FACE_OUTER_BOUND('',#23100,.T.) ;
#18787 = FACE_OUTER_BOUND('',#23101,.T.) ;
#18788 = FACE_OUTER_BOUND('',#23102,.T.) ;
#18789 = FACE_OUTER_BOUND('',#23103,.T.) ;
#18790 = FACE_OUTER_BOUND('',#23104,.T.) ;
#18791 = FACE_OUTER_BOUND('',#23105,.T.) ;
#18792 = FACE_OUTER_BOUND('',#23106,.T.) ;
#18793 = FACE_OUTER_BOUND('',#23107,.T.) ;
#18794 = FACE_OUTER_BOUND('',#23108,.T.) ;
#18795 = FACE_OUTER_BOUND('',#23109,.T.) ;
#18796 = FACE_OUTER_BOUND('',#23110,.T.) ;
#18797 = FACE_OUTER_BOUND('',#23111,.T.) ;
#18798 = FACE_OUTER_BOUND('',#23112,.T.) ;
#18799 = FACE_OUTER_BOUND('',#23113,.T.) ;
#18800 = FACE_OUTER_BOUND('',#23114,.T.) ;
#18801 = FACE_OUTER_BOUND('',#23115,.T.) ;
#18802 = FACE_OUTER_BOUND('',#23116,.T.) ;
#18803 = FACE_OUTER_BOUND('',#23117,.T.) ;
#18804 = FACE_OUTER_BOUND('',#23118,.T.) ;
#18805 = FACE_OUTER_BOUND('',#23119,.T.) ;
#18806 = FACE_OUTER_BOUND('',#23120,.T.) ;
#18807 = FACE_OUTER_BOUND('',#23121,.T.) ;
#18808 = FACE_OUTER_BOUND('',#23122,.T.) ;
#18809 = FACE_OUTER_BOUND('',#23123,.T.) ;
#18810 = FACE_OUTER_BOUND('',#23124,.T.) ;
#18811 = FACE_OUTER_BOUND('',#23125,.T.) ;
#18812 = FACE_OUTER_BOUND('',#23126,.T.) ;
#18813 = FACE_OUTER_BOUND('',#23127,.T.) ;
#18814 = FACE_OUTER_BOUND('',#23128,.T.) ;
#18815 = FACE_OUTER_BOUND('',#23129,.T.) ;
#18816 = FACE_OUTER_BOUND('',#23130,.T.) ;
#18817 = FACE_OUTER_BOUND('',#23131,.T.) ;
#18818 = FACE_OUTER_BOUND('',#23132,.T.) ;
#18819 = FACE_OUTER_BOUND('',#23133,.T.) ;
#18820 = FACE_OUTER_BOUND('',#23134,.T.) ;
#18821 = FACE_OUTER_BOUND('',#23135,.T.) ;
#18822 = FACE_OUTER_BOUND('',#23136,.T.) ;
#18823 = FACE_OUTER_BOUND('',#23137,.T.) ;
#18824 = FACE_OUTER_BOUND('',#23138,.T.) ;
#18825 = FACE_OUTER_BOUND('',#23139,.T.) ;
#18826 = FACE_OUTER_BOUND('',#23140,.T.) ;
#18827 = FACE_OUTER_BOUND('',#23141,.T.) ;
#18828 = FACE_OUTER_BOUND('',#23142,.T.) ;
#18829 = FACE_OUTER_BOUND('',#23143,.T.) ;
#18830 = FACE_OUTER_BOUND('',#23144,.T.) ;
#18831 = FACE_OUTER_BOUND('',#23145,.T.) ;
#18832 = FACE_OUTER_BOUND('',#23146,.T.) ;
#18833 = FACE_OUTER_BOUND('',#23147,.T.) ;
#18834 = FACE_OUTER_BOUND('',#23148,.T.) ;
#18835 = FACE_OUTER_BOUND('',#23149,.T.) ;
#18836 = FACE_OUTER_BOUND('',#23150,.T.) ;
#18837 = FACE_OUTER_BOUND('',#23151,.T.) ;
#18838 = FACE_OUTER_BOUND('',#23152,.T.) ;
#18839 = FACE_OUTER_BOUND('',#23153,.T.) ;
#18840 = FACE_OUTER_BOUND('',#23154,.T.) ;
#18841 = FACE_OUTER_BOUND('',#23155,.T.) ;
#18842 = FACE_OUTER_BOUND('',#23156,.T.) ;
#18843 = FACE_OUTER_BOUND('',#23157,.T.) ;
#18844 = FACE_OUTER_BOUND('',#23158,.T.) ;
#18845 = FACE_OUTER_BOUND('',#23159,.T.) ;
#18846 = FACE_OUTER_BOUND('',#23160,.T.) ;
#18847 = FACE_OUTER_BOUND('',#23161,.T.) ;
#18848 = FACE_OUTER_BOUND('',#23162,.T.) ;
#18849 = FACE_OUTER_BOUND('',#23163,.T.) ;
#18850 = FACE_OUTER_BOUND('',#23164,.T.) ;
#18851 = FACE_OUTER_BOUND('',#23165,.T.) ;
#18852 = FACE_OUTER_BOUND('',#23166,.T.) ;
#18853 = FACE_OUTER_BOUND('',#23167,.T.) ;
#18854 = FACE_OUTER_BOUND('',#23168,.T.) ;
#18855 = FACE_OUTER_BOUND('',#23169,.T.) ;
#18856 = FACE_OUTER_BOUND('',#23170,.T.) ;
#18857 = FACE_OUTER_BOUND('',#23171,.T.) ;
#18858 = FACE_OUTER_BOUND('',#23172,.T.) ;
#18859 = FACE_OUTER_BOUND('',#23173,.T.) ;
#18860 = FACE_OUTER_BOUND('',#23174,.T.) ;
#18861 = FACE_OUTER_BOUND('',#23175,.T.) ;
#18862 = FACE_OUTER_BOUND('',#23176,.T.) ;
#18863 = FACE_OUTER_BOUND('',#23177,.T.) ;
#18864 = FACE_OUTER_BOUND('',#23178,.T.) ;
#18865 = FACE_OUTER_BOUND('',#23179,.T.) ;
#18866 = FACE_OUTER_BOUND('',#23180,.T.) ;
#18867 = FACE_OUTER_BOUND('',#23181,.T.) ;
#18868 = FACE_OUTER_BOUND('',#23182,.T.) ;
#18869 = FACE_OUTER_BOUND('',#23183,.T.) ;
#18870 = FACE_OUTER_BOUND('',#23184,.T.) ;
#18871 = FACE_OUTER_BOUND('',#23185,.T.) ;
#18872 = FACE_OUTER_BOUND('',#23186,.T.) ;
#18873 = FACE_OUTER_BOUND('',#23187,.T.) ;
#18874 = FACE_OUTER_BOUND('',#23188,.T.) ;
#18875 = FACE_OUTER_BOUND('',#23189,.T.) ;
#18876 = FACE_OUTER_BOUND('',#23190,.T.) ;
#18877 = FACE_OUTER_BOUND('',#23191,.T.) ;
#18878 = FACE_OUTER_BOUND('',#23192,.T.) ;
#18879 = FACE_OUTER_BOUND('',#23193,.T.) ;
#18880 = FACE_OUTER_BOUND('',#23194,.T.) ;
#18881 = FACE_OUTER_BOUND('',#23195,.T.) ;
#18882 = FACE_OUTER_BOUND('',#23196,.T.) ;
#18883 = FACE_OUTER_BOUND('',#23197,.T.) ;
#18884 = FACE_OUTER_BOUND('',#23198,.T.) ;
#18885 = FACE_OUTER_BOUND('',#23199,.T.) ;
#18886 = FACE_OUTER_BOUND('',#23200,.T.) ;
#18887 = FACE_OUTER_BOUND('',#23201,.T.) ;
#18888 = FACE_OUTER_BOUND('',#23202,.T.) ;
#18889 = FACE_OUTER_BOUND('',#23203,.T.) ;
#18890 = FACE_OUTER_BOUND('',#23204,.T.) ;
#18891 = FACE_OUTER_BOUND('',#23205,.T.) ;
#18892 = FACE_OUTER_BOUND('',#23206,.T.) ;
#18893 = FACE_OUTER_BOUND('',#23207,.T.) ;
#18894 = FACE_OUTER_BOUND('',#23208,.T.) ;
#18895 = FACE_OUTER_BOUND('',#23209,.T.) ;
#18896 = FACE_OUTER_BOUND('',#23210,.T.) ;
#18897 = FACE_OUTER_BOUND('',#23211,.T.) ;
#18898 = FACE_OUTER_BOUND('',#23212,.T.) ;
#18899 = FACE_OUTER_BOUND('',#23213,.T.) ;
#18900 = FACE_OUTER_BOUND('',#23214,.T.) ;
#18901 = FACE_OUTER_BOUND('',#23215,.T.) ;
#18902 = FACE_OUTER_BOUND('',#23216,.T.) ;
#18903 = FACE_OUTER_BOUND('',#23217,.T.) ;
#18904 = FACE_OUTER_BOUND('',#23218,.T.) ;
#18905 = FACE_OUTER_BOUND('',#23219,.T.) ;
#18906 = FACE_OUTER_BOUND('',#23220,.T.) ;
#18907 = FACE_OUTER_BOUND('',#23221,.T.) ;
#18908 = FACE_OUTER_BOUND('',#23222,.T.) ;
#18909 = FACE_OUTER_BOUND('',#23223,.T.) ;
#18910 = FACE_OUTER_BOUND('',#23224,.T.) ;
#18911 = FACE_OUTER_BOUND('',#23225,.T.) ;
#18912 = FACE_OUTER_BOUND('',#23226,.T.) ;
#18913 = FACE_OUTER_BOUND('',#23227,.T.) ;
#18914 = FACE_OUTER_BOUND('',#23228,.T.) ;
#18915 = FACE_OUTER_BOUND('',#23229,.T.) ;
#18916 = FACE_OUTER_BOUND('',#23230,.T.) ;
#18917 = FACE_OUTER_BOUND('',#23231,.T.) ;
#18918 = FACE_OUTER_BOUND('',#23232,.T.) ;
#18919 = FACE_OUTER_BOUND('',#23233,.T.) ;
#18920 = FACE_OUTER_BOUND('',#23234,.T.) ;
#18921 = FACE_OUTER_BOUND('',#23235,.T.) ;
#18922 = FACE_OUTER_BOUND('',#23236,.T.) ;
#18923 = FACE_OUTER_BOUND('',#23237,.T.) ;
#18924 = FACE_OUTER_BOUND('',#23238,.T.) ;
#18925 = FACE_OUTER_BOUND('',#23239,.T.) ;
#18926 = FACE_OUTER_BOUND('',#23240,.T.) ;
#18927 = FACE_OUTER_BOUND('',#23241,.T.) ;
#18928 = FACE_OUTER_BOUND('',#23242,.T.) ;
#18929 = FACE_OUTER_BOUND('',#23243,.T.) ;
#18930 = FACE_OUTER_BOUND('',#23244,.T.) ;
#18931 = FACE_OUTER_BOUND('',#23245,.T.) ;
#18932 = FACE_OUTER_BOUND('',#23246,.T.) ;
#18933 = FACE_OUTER_BOUND('',#23247,.T.) ;
#18934 = FACE_OUTER_BOUND('',#23248,.T.) ;
#18935 = FACE_OUTER_BOUND('',#23249,.T.) ;
#18936 = FACE_OUTER_BOUND('',#23250,.T.) ;
#18937 = FACE_OUTER_BOUND('',#23251,.T.) ;
#18938 = FACE_OUTER_BOUND('',#23252,.T.) ;
#18939 = FACE_OUTER_BOUND('',#23253,.T.) ;
#18940 = FACE_OUTER_BOUND('',#23254,.T.) ;
#18941 = FACE_OUTER_BOUND('',#23255,.T.) ;
#18942 = FACE_OUTER_BOUND('',#23256,.T.) ;
#18943 = FACE_OUTER_BOUND('',#23257,.T.) ;
#18944 = FACE_OUTER_BOUND('',#23258,.T.) ;
#18945 = FACE_OUTER_BOUND('',#23259,.T.) ;
#18946 = FACE_OUTER_BOUND('',#23260,.T.) ;
#18947 = FACE_OUTER_BOUND('',#23261,.T.) ;
#18948 = FACE_OUTER_BOUND('',#23262,.T.) ;
#18949 = FACE_OUTER_BOUND('',#23263,.T.) ;
#18950 = FACE_OUTER_BOUND('',#23264,.T.) ;
#18951 = FACE_OUTER_BOUND('',#23265,.T.) ;
#18952 = FACE_OUTER_BOUND('',#23266,.T.) ;
#18953 = FACE_OUTER_BOUND('',#23267,.T.) ;
#18954 = FACE_OUTER_BOUND('',#23268,.T.) ;
#18955 = FACE_OUTER_BOUND('',#23269,.T.) ;
#18956 = FACE_OUTER_BOUND('',#23270,.T.) ;
#18957 = FACE_OUTER_BOUND('',#23271,.T.) ;
#18958 = FACE_OUTER_BOUND('',#23272,.T.) ;
#18959 = FACE_OUTER_BOUND('',#23273,.T.) ;
#18960 = FACE_OUTER_BOUND('',#23274,.T.) ;
#18961 = FACE_OUTER_BOUND('',#23275,.T.) ;
#18962 = FACE_OUTER_BOUND('',#23276,.T.) ;
#18963 = FACE_OUTER_BOUND('',#23277,.T.) ;
#18964 = FACE_OUTER_BOUND('',#23278,.T.) ;
#18965 = FACE_OUTER_BOUND('',#23279,.T.) ;
#18966 = FACE_OUTER_BOUND('',#23280,.T.) ;
#18967 = FACE_OUTER_BOUND('',#23281,.T.) ;
#18968 = FACE_OUTER_BOUND('',#23282,.T.) ;
#18969 = FACE_OUTER_BOUND('',#23283,.T.) ;
#18970 = FACE_OUTER_BOUND('',#23284,.T.) ;
#18971 = FACE_OUTER_BOUND('',#23285,.T.) ;
#18972 = FACE_OUTER_BOUND('',#23286,.T.) ;
#18973 = FACE_OUTER_BOUND('',#23287,.T.) ;
#18974 = FACE_OUTER_BOUND('',#23288,.T.) ;
#18975 = FACE_OUTER_BOUND('',#23289,.T.) ;
#18976 = FACE_OUTER_BOUND('',#23290,.T.) ;
#18977 = FACE_OUTER_BOUND('',#23291,.T.) ;
#18978 = FACE_OUTER_BOUND('',#23292,.T.) ;
#18979 = FACE_OUTER_BOUND('',#23293,.T.) ;
#18980 = FACE_OUTER_BOUND('',#23294,.T.) ;
#18981 = FACE_OUTER_BOUND('',#23295,.T.) ;
#18982 = FACE_OUTER_BOUND('',#23296,.T.) ;
#18983 = FACE_OUTER_BOUND('',#23297,.T.) ;
#18984 = FACE_OUTER_BOUND('',#23298,.T.) ;
#18985 = FACE_OUTER_BOUND('',#23299,.T.) ;
#18986 = FACE_OUTER_BOUND('',#23300,.T.) ;
#18987 = FACE_OUTER_BOUND('',#23301,.T.) ;
#18988 = FACE_OUTER_BOUND('',#23302,.T.) ;
#18989 = FACE_OUTER_BOUND('',#23303,.T.) ;
#18990 = FACE_OUTER_BOUND('',#23304,.T.) ;
#18991 = FACE_OUTER_BOUND('',#23305,.T.) ;
#18992 = FACE_OUTER_BOUND('',#23306,.T.) ;
#18993 = FACE_OUTER_BOUND('',#23307,.T.) ;
#18994 = FACE_OUTER_BOUND('',#23308,.T.) ;
#18995 = FACE_OUTER_BOUND('',#23309,.T.) ;
#18996 = FACE_OUTER_BOUND('',#23310,.T.) ;
#18997 = FACE_OUTER_BOUND('',#23311,.T.) ;
#18998 = FACE_OUTER_BOUND('',#23312,.T.) ;
#18999 = FACE_OUTER_BOUND('',#23313,.T.) ;
#19000 = FACE_OUTER_BOUND('',#23314,.T.) ;
#19001 = FACE_OUTER_BOUND('',#23315,.T.) ;
#19002 = FACE_OUTER_BOUND('',#23316,.T.) ;
#19003 = FACE_OUTER_BOUND('',#23317,.T.) ;
#19004 = FACE_OUTER_BOUND('',#23318,.T.) ;
#19005 = FACE_OUTER_BOUND('',#23319,.T.) ;
#19006 = FACE_OUTER_BOUND('',#23320,.T.) ;
#19007 = FACE_OUTER_BOUND('',#23321,.T.) ;
#19008 = FACE_OUTER_BOUND('',#23322,.T.) ;
#19009 = FACE_OUTER_BOUND('',#23323,.T.) ;
#19010 = FACE_OUTER_BOUND('',#23324,.T.) ;
#19011 = FACE_OUTER_BOUND('',#23325,.T.) ;
#19012 = FACE_OUTER_BOUND('',#23326,.T.) ;
#19013 = FACE_OUTER_BOUND('',#23327,.T.) ;
#19014 = FACE_OUTER_BOUND('',#23328,.T.) ;
#19015 = FACE_OUTER_BOUND('',#23329,.T.) ;
#19016 = FACE_OUTER_BOUND('',#23330,.T.) ;
#19017 = FACE_OUTER_BOUND('',#23331,.T.) ;
#19018 = FACE_OUTER_BOUND('',#23332,.T.) ;
#19019 = FACE_OUTER_BOUND('',#23333,.T.) ;
#19020 = FACE_OUTER_BOUND('',#23334,.T.) ;
#19021 = FACE_OUTER_BOUND('',#23335,.T.) ;
#19022 = FACE_OUTER_BOUND('',#23336,.T.) ;
#19023 = FACE_OUTER_BOUND('',#23337,.T.) ;
#19024 = FACE_OUTER_BOUND('',#23338,.T.) ;
#19025 = FACE_OUTER_BOUND('',#23339,.T.) ;
#19026 = FACE_OUTER_BOUND('',#23340,.T.) ;
#19027 = FACE_OUTER_BOUND('',#23341,.T.) ;
#19028 = FACE_OUTER_BOUND('',#23342,.T.) ;
#19029 = FACE_OUTER_BOUND('',#23343,.T.) ;
#19030 = FACE_OUTER_BOUND('',#23344,.T.) ;
#19031 = FACE_OUTER_BOUND('',#23345,.T.) ;
#19032 = FACE_OUTER_BOUND('',#23346,.T.) ;
#19033 = FACE_OUTER_BOUND('',#23347,.T.) ;
#19034 = FACE_OUTER_BOUND('',#23348,.T.) ;
#19035 = FACE_OUTER_BOUND('',#23349,.T.) ;
#19036 = FACE_OUTER_BOUND('',#23350,.T.) ;
#19037 = FACE_OUTER_BOUND('',#23351,.T.) ;
#19038 = FACE_OUTER_BOUND('',#23352,.T.) ;
#19039 = FACE_OUTER_BOUND('',#23353,.T.) ;
#19040 = FACE_OUTER_BOUND('',#23354,.T.) ;
#19041 = FACE_OUTER_BOUND('',#23355,.T.) ;
#19042 = FACE_OUTER_BOUND('',#23356,.T.) ;
#19043 = FACE_OUTER_BOUND('',#23357,.T.) ;
#19044 = FACE_OUTER_BOUND('',#23358,.T.) ;
#19045 = FACE_OUTER_BOUND('',#23359,.T.) ;
#19046 = FACE_OUTER_BOUND('',#23360,.T.) ;
#19047 = FACE_OUTER_BOUND('',#23361,.T.) ;
#19048 = FACE_OUTER_BOUND('',#23362,.T.) ;
#19049 = FACE_OUTER_BOUND('',#23363,.T.) ;
#19050 = FACE_OUTER_BOUND('',#23364,.T.) ;
#19051 = FACE_OUTER_BOUND('',#23365,.T.) ;
#19052 = FACE_OUTER_BOUND('',#23366,.T.) ;
#19053 = FACE_OUTER_BOUND('',#23367,.T.) ;
#19054 = FACE_OUTER_BOUND('',#23368,.T.) ;
#19055 = FACE_OUTER_BOUND('',#23369,.T.) ;
#19056 = FACE_OUTER_BOUND('',#23370,.T.) ;
#19057 = FACE_OUTER_BOUND('',#23371,.T.) ;
#19058 = FACE_OUTER_BOUND('',#23372,.T.) ;
#19059 = FACE_OUTER_BOUND('',#23373,.T.) ;
#19060 = FACE_OUTER_BOUND('',#23374,.T.) ;
#19061 = FACE_OUTER_BOUND('',#23375,.T.) ;
#19062 = FACE_OUTER_BOUND('',#23376,.T.) ;
#19063 = FACE_OUTER_BOUND('',#23377,.T.) ;
#19064 = FACE_OUTER_BOUND('',#23378,.T.) ;
#19065 = FACE_OUTER_BOUND('',#23379,.T.) ;
#19066 = FACE_OUTER_BOUND('',#23380,.T.) ;
#19067 = FACE_OUTER_BOUND('',#23381,.T.) ;
#19068 = FACE_OUTER_BOUND('',#23382,.T.) ;
#19069 = FACE_OUTER_BOUND('',#23383,.T.) ;
#19070 = FACE_OUTER_BOUND('',#23384,.T.) ;
#19071 = FACE_OUTER_BOUND('',#23385,.T.) ;
#19072 = FACE_OUTER_BOUND('',#23386,.T.) ;
#19073 = FACE_OUTER_BOUND('',#23387,.T.) ;
#19074 = FACE_OUTER_BOUND('',#23388,.T.) ;
#19075 = FACE_OUTER_BOUND('',#23389,.T.) ;
#19076 = FACE_OUTER_BOUND('',#23390,.T.) ;
#19077 = FACE_OUTER_BOUND('',#23391,.T.) ;
#19078 = FACE_OUTER_BOUND('',#23392,.T.) ;
#19079 = FACE_OUTER_BOUND('',#23393,.T.) ;
#19080 = FACE_OUTER_BOUND('',#23394,.T.) ;
#19081 = FACE_OUTER_BOUND('',#23395,.T.) ;
#19082 = FACE_OUTER_BOUND('',#23396,.T.) ;
#19083 = FACE_OUTER_BOUND('',#23397,.T.) ;
#19084 = FACE_OUTER_BOUND('',#23398,.T.) ;
#19085 = FACE_OUTER_BOUND('',#23399,.T.) ;
#19086 = FACE_OUTER_BOUND('',#23400,.T.) ;
#19087 = FACE_OUTER_BOUND('',#23401,.T.) ;
#19088 = FACE_OUTER_BOUND('',#23402,.T.) ;
#19089 = FACE_OUTER_BOUND('',#23403,.T.) ;
#19090 = FACE_OUTER_BOUND('',#23404,.T.) ;
#19091 = FACE_OUTER_BOUND('',#23405,.T.) ;
#19092 = FACE_OUTER_BOUND('',#23406,.T.) ;
#19093 = FACE_OUTER_BOUND('',#23407,.T.) ;
#19094 = FACE_OUTER_BOUND('',#23408,.T.) ;
#19095 = FACE_OUTER_BOUND('',#23409,.T.) ;
#19096 = FACE_OUTER_BOUND('',#23410,.T.) ;
#19097 = FACE_OUTER_BOUND('',#23411,.T.) ;
#19098 = FACE_OUTER_BOUND('',#23412,.T.) ;
#19099 = FACE_OUTER_BOUND('',#23413,.T.) ;
#19100 = FACE_OUTER_BOUND('',#23414,.T.) ;
#19101 = FACE_OUTER_BOUND('',#23415,.T.) ;
#19102 = FACE_OUTER_BOUND('',#23416,.T.) ;
#19103 = FACE_OUTER_BOUND('',#23417,.T.) ;
#19104 = FACE_OUTER_BOUND('',#23418,.T.) ;
#19105 = FACE_OUTER_BOUND('',#23419,.T.) ;
#19106 = FACE_OUTER_BOUND('',#23420,.T.) ;
#19107 = FACE_OUTER_BOUND('',#23421,.T.) ;
#19108 = FACE_OUTER_BOUND('',#23422,.T.) ;
#19109 = FACE_OUTER_BOUND('',#23423,.T.) ;
#19110 = FACE_OUTER_BOUND('',#23424,.T.) ;
#19111 = FACE_OUTER_BOUND('',#23425,.T.) ;
#19112 = FACE_OUTER_BOUND('',#23426,.T.) ;
#19113 = FACE_OUTER_BOUND('',#23427,.T.) ;
#19114 = FACE_OUTER_BOUND('',#23428,.T.) ;
#19115 = FACE_OUTER_BOUND('',#23429,.T.) ;
#19116 = FACE_OUTER_BOUND('',#23430,.T.) ;
#19117 = FACE_OUTER_BOUND('',#23431,.T.) ;
#19118 = FACE_OUTER_BOUND('',#23432,.T.) ;
#19119 = FACE_OUTER_BOUND('',#23433,.T.) ;
#19120 = FACE_OUTER_BOUND('',#23434,.T.) ;
#19121 = FACE_OUTER_BOUND('',#23435,.T.) ;
#19122 = FACE_OUTER_BOUND('',#23436,.T.) ;
#19123 = FACE_OUTER_BOUND('',#23437,.T.) ;
#19124 = FACE_OUTER_BOUND('',#23438,.T.) ;
#19125 = FACE_OUTER_BOUND('',#23439,.T.) ;
#19126 = FACE_OUTER_BOUND('',#23440,.T.) ;
#19127 = FACE_OUTER_BOUND('',#23441,.T.) ;
#19128 = FACE_OUTER_BOUND('',#23442,.T.) ;
#19129 = FACE_OUTER_BOUND('',#23443,.T.) ;
#19130 = FACE_OUTER_BOUND('',#23444,.T.) ;
#19131 = FACE_OUTER_BOUND('',#23445,.T.) ;
#19132 = FACE_OUTER_BOUND('',#23446,.T.) ;
#19133 = FACE_OUTER_BOUND('',#23447,.T.) ;
#19134 = FACE_OUTER_BOUND('',#23448,.T.) ;
#19135 = FACE_OUTER_BOUND('',#23449,.T.) ;
#19136 = FACE_OUTER_BOUND('',#23450,.T.) ;
#19137 = FACE_OUTER_BOUND('',#23451,.T.) ;
#19138 = FACE_OUTER_BOUND('',#23452,.T.) ;
#19139 = FACE_OUTER_BOUND('',#23453,.T.) ;
#19140 = FACE_OUTER_BOUND('',#23454,.T.) ;
#19141 = FACE_OUTER_BOUND('',#23455,.T.) ;
#19142 = FACE_OUTER_BOUND('',#23456,.T.) ;
#19143 = FACE_OUTER_BOUND('',#23457,.T.) ;
#19144 = FACE_OUTER_BOUND('',#23458,.T.) ;
#19145 = FACE_OUTER_BOUND('',#23459,.T.) ;
#19146 = FACE_OUTER_BOUND('',#23460,.T.) ;
#19147 = FACE_OUTER_BOUND('',#23461,.T.) ;
#19148 = FACE_OUTER_BOUND('',#23462,.T.) ;
#19149 = FACE_OUTER_BOUND('',#23463,.T.) ;
#19150 = FACE_OUTER_BOUND('',#23464,.T.) ;
#19151 = FACE_OUTER_BOUND('',#23465,.T.) ;
#19152 = FACE_OUTER_BOUND('',#23466,.T.) ;
#19153 = FACE_OUTER_BOUND('',#23467,.T.) ;
#19154 = FACE_OUTER_BOUND('',#23468,.T.) ;
#19155 = FACE_OUTER_BOUND('',#23469,.T.) ;
#19156 = FACE_OUTER_BOUND('',#23470,.T.) ;
#19157 = FACE_OUTER_BOUND('',#23471,.T.) ;
#19158 = FACE_OUTER_BOUND('',#23472,.T.) ;
#19159 = FACE_OUTER_BOUND('',#23473,.T.) ;
#19160 = FACE_OUTER_BOUND('',#23474,.T.) ;
#19161 = FACE_OUTER_BOUND('',#23475,.T.) ;
#19162 = FACE_OUTER_BOUND('',#23476,.T.) ;
#19163 = FACE_OUTER_BOUND('',#23477,.T.) ;
#19164 = FACE_OUTER_BOUND('',#23478,.T.) ;
#19165 = FACE_OUTER_BOUND('',#23479,.T.) ;
#19166 = FACE_OUTER_BOUND('',#23480,.T.) ;
#19167 = FACE_OUTER_BOUND('',#23481,.T.) ;
#19168 = FACE_OUTER_BOUND('',#23482,.T.) ;
#19169 = FACE_OUTER_BOUND('',#23483,.T.) ;
#19170 = FACE_OUTER_BOUND('',#23484,.T.) ;
#19171 = FACE_OUTER_BOUND('',#23485,.T.) ;
#19172 = FACE_OUTER_BOUND('',#23486,.T.) ;
#19173 = FACE_OUTER_BOUND('',#23487,.T.) ;
#19174 = FACE_OUTER_BOUND('',#23488,.T.) ;
#19175 = FACE_OUTER_BOUND('',#23489,.T.) ;
#19176 = FACE_OUTER_BOUND('',#23490,.T.) ;
#19177 = FACE_OUTER_BOUND('',#23491,.T.) ;
#19178 = FACE_OUTER_BOUND('',#23492,.T.) ;
#19179 = FACE_OUTER_BOUND('',#23493,.T.) ;
#19180 = FACE_OUTER_BOUND('',#23494,.T.) ;
#19181 = FACE_OUTER_BOUND('',#23495,.T.) ;
#19182 = FACE_OUTER_BOUND('',#23496,.T.) ;
#19183 = FACE_OUTER_BOUND('',#23497,.T.) ;
#19184 = FACE_OUTER_BOUND('',#23498,.T.) ;
#19185 = FACE_OUTER_BOUND('',#23499,.T.) ;
#19186 = FACE_OUTER_BOUND('',#23500,.T.) ;
#19187 = FACE_OUTER_BOUND('',#23501,.T.) ;
#19188 = FACE_OUTER_BOUND('',#23502,.T.) ;
#19189 = FACE_OUTER_BOUND('',#23503,.T.) ;
#19190 = FACE_OUTER_BOUND('',#23504,.T.) ;
#19191 = FACE_OUTER_BOUND('',#23505,.T.) ;
#19192 = FACE_OUTER_BOUND('',#23506,.T.) ;
#19193 = FACE_OUTER_BOUND('',#23507,.T.) ;
#19194 = FACE_OUTER_BOUND('',#23508,.T.) ;
#19195 = FACE_OUTER_BOUND('',#23509,.T.) ;
#19196 = FACE_OUTER_BOUND('',#23510,.T.) ;
#19197 = FACE_OUTER_BOUND('',#23511,.T.) ;
#19198 = FACE_OUTER_BOUND('',#23512,.T.) ;
#19199 = FACE_OUTER_BOUND('',#23513,.T.) ;
#19200 = FACE_OUTER_BOUND('',#23514,.T.) ;
#19201 = FACE_OUTER_BOUND('',#23515,.T.) ;
#19202 = FACE_OUTER_BOUND('',#23516,.T.) ;
#19203 = FACE_OUTER_BOUND('',#23517,.T.) ;
#19204 = FACE_OUTER_BOUND('',#23518,.T.) ;
#19205 = FACE_OUTER_BOUND('',#23519,.T.) ;
#19206 = FACE_OUTER_BOUND('',#23520,.T.) ;
#19207 = FACE_OUTER_BOUND('',#23521,.T.) ;
#19208 = FACE_OUTER_BOUND('',#23522,.T.) ;
#19209 = FACE_OUTER_BOUND('',#23523,.T.) ;
#19210 = FACE_OUTER_BOUND('',#23524,.T.) ;
#19211 = FACE_OUTER_BOUND('',#23525,.T.) ;
#19212 = FACE_OUTER_BOUND('',#23526,.T.) ;
#19213 = FACE_OUTER_BOUND('',#23527,.T.) ;
#19214 = FACE_OUTER_BOUND('',#23528,.T.) ;
#19215 = FACE_OUTER_BOUND('',#23529,.T.) ;
#19216 = FACE_OUTER_BOUND('',#23530,.T.) ;
#19217 = FACE_OUTER_BOUND('',#23531,.T.) ;
#19218 = FACE_OUTER_BOUND('',#23532,.T.) ;
#19219 = FACE_OUTER_BOUND('',#23533,.T.) ;
#19220 = FACE_OUTER_BOUND('',#23534,.T.) ;
#19221 = FACE_OUTER_BOUND('',#23535,.T.) ;
#19222 = FACE_OUTER_BOUND('',#23536,.T.) ;
#19223 = FACE_OUTER_BOUND('',#23537,.T.) ;
#19224 = FACE_OUTER_BOUND('',#23538,.T.) ;
#19225 = FACE_OUTER_BOUND('',#23539,.T.) ;
#19226 = FACE_OUTER_BOUND('',#23540,.T.) ;
#19227 = FACE_OUTER_BOUND('',#23541,.T.) ;
#19228 = FACE_OUTER_BOUND('',#23542,.T.) ;
#19229 = FACE_OUTER_BOUND('',#23543,.T.) ;
#19230 = FACE_OUTER_BOUND('',#23544,.T.) ;
#19231 = FACE_OUTER_BOUND('',#23545,.T.) ;
#19232 = FACE_OUTER_BOUND('',#23546,.T.) ;
#19233 = FACE_OUTER_BOUND('',#23547,.T.) ;
#19234 = FACE_OUTER_BOUND('',#23548,.T.) ;
#19235 = FACE_OUTER_BOUND('',#23549,.T.) ;
#19236 = FACE_OUTER_BOUND('',#23550,.T.) ;
#19237 = FACE_OUTER_BOUND('',#23551,.T.) ;
#19238 = FACE_OUTER_BOUND('',#23552,.T.) ;
#19239 = FACE_OUTER_BOUND('',#23553,.T.) ;
#19240 = FACE_OUTER_BOUND('',#23554,.T.) ;
#19241 = FACE_OUTER_BOUND('',#23555,.T.) ;
#19242 = FACE_OUTER_BOUND('',#23556,.T.) ;
#19243 = FACE_OUTER_BOUND('',#23557,.T.) ;
#19244 = FACE_OUTER_BOUND('',#23558,.T.) ;
#19245 = FACE_OUTER_BOUND('',#23559,.T.) ;
#19246 = FACE_OUTER_BOUND('',#23560,.T.) ;
#19247 = FACE_OUTER_BOUND('',#23561,.T.) ;
#19248 = FACE_OUTER_BOUND('',#23562,.T.) ;
#19249 = FACE_OUTER_BOUND('',#23563,.T.) ;
#19250 = FACE_OUTER_BOUND('',#23564,.T.) ;
#19251 = FACE_OUTER_BOUND('',#23565,.T.) ;
#19252 = FACE_OUTER_BOUND('',#23566,.T.) ;
#19253 = FACE_OUTER_BOUND('',#23567,.T.) ;
#19254 = FACE_OUTER_BOUND('',#23568,.T.) ;
#19255 = FACE_OUTER_BOUND('',#23569,.T.) ;
#19256 = FACE_OUTER_BOUND('',#23570,.T.) ;
#19257 = FACE_OUTER_BOUND('',#23571,.T.) ;
#19258 = FACE_OUTER_BOUND('',#23572,.T.) ;
#19259 = FACE_OUTER_BOUND('',#23573,.T.) ;
#19260 = FACE_OUTER_BOUND('',#23574,.T.) ;
#19261 = FACE_OUTER_BOUND('',#23575,.T.) ;
#19262 = FACE_OUTER_BOUND('',#23576,.T.) ;
#19263 = FACE_OUTER_BOUND('',#23577,.T.) ;
#19264 = FACE_OUTER_BOUND('',#23578,.T.) ;
#19265 = FACE_OUTER_BOUND('',#23579,.T.) ;
#19266 = FACE_OUTER_BOUND('',#23580,.T.) ;
#19267 = FACE_OUTER_BOUND('',#23581,.T.) ;
#19268 = FACE_OUTER_BOUND('',#23582,.T.) ;
#19269 = FACE_OUTER_BOUND('',#23583,.T.) ;
#19270 = FACE_OUTER_BOUND('',#23584,.T.) ;
#19271 = FACE_OUTER_BOUND('',#23585,.T.) ;
#19272 = FACE_OUTER_BOUND('',#23586,.T.) ;
#19273 = FACE_OUTER_BOUND('',#23587,.T.) ;
#19274 = FACE_OUTER_BOUND('',#23588,.T.) ;
#19275 = FACE_OUTER_BOUND('',#23589,.T.) ;
#19276 = FACE_OUTER_BOUND('',#23590,.T.) ;
#19277 = FACE_OUTER_BOUND('',#23591,.T.) ;
#19278 = FACE_OUTER_BOUND('',#23592,.T.) ;
#19279 = FACE_OUTER_BOUND('',#23593,.T.) ;
#19280 = FACE_OUTER_BOUND('',#23594,.T.) ;
#19281 = FACE_OUTER_BOUND('',#23595,.T.) ;
#19282 = FACE_OUTER_BOUND('',#23596,.T.) ;
#19283 = FACE_OUTER_BOUND('',#23597,.T.) ;
#19284 = FACE_OUTER_BOUND('',#23598,.T.) ;
#19285 = FACE_OUTER_BOUND('',#23599,.T.) ;
#19286 = FACE_OUTER_BOUND('',#23600,.T.) ;
#19287 = FACE_OUTER_BOUND('',#23601,.T.) ;
#19288 = FACE_OUTER_BOUND('',#23602,.T.) ;
#19289 = FACE_OUTER_BOUND('',#23603,.T.) ;
#19290 = FACE_OUTER_BOUND('',#23604,.T.) ;
#19291 = FACE_OUTER_BOUND('',#23605,.T.) ;
#19292 = FACE_OUTER_BOUND('',#23606,.T.) ;
#19293 = FACE_OUTER_BOUND('',#23607,.T.) ;
#19294 = FACE_OUTER_BOUND('',#23608,.T.) ;
#19295 = FACE_OUTER_BOUND('',#23609,.T.) ;
#19296 = FACE_OUTER_BOUND('',#23610,.T.) ;
#19297 = FACE_OUTER_BOUND('',#23611,.T.) ;
#19298 = FACE_OUTER_BOUND('',#23612,.T.) ;
#19299 = FACE_OUTER_BOUND('',#23613,.T.) ;
#19300 = FACE_OUTER_BOUND('',#23614,.T.) ;
#19301 = FACE_OUTER_BOUND('',#23615,.T.) ;
#19302 = FACE_OUTER_BOUND('',#23616,.T.) ;
#19303 = FACE_OUTER_BOUND('',#23617,.T.) ;
#19304 = FACE_OUTER_BOUND('',#23618,.T.) ;
#19305 = FACE_OUTER_BOUND('',#23619,.T.) ;
#19306 = FACE_OUTER_BOUND('',#23620,.T.) ;
#19307 = FACE_OUTER_BOUND('',#23621,.T.) ;
#19308 = FACE_OUTER_BOUND('',#23622,.T.) ;
#19309 = FACE_OUTER_BOUND('',#23623,.T.) ;
#19310 = FACE_OUTER_BOUND('',#23624,.T.) ;
#19311 = FACE_OUTER_BOUND('',#23625,.T.) ;
#19312 = FACE_OUTER_BOUND('',#23626,.T.) ;
#19313 = FACE_OUTER_BOUND('',#23627,.T.) ;
#19314 = FACE_OUTER_BOUND('',#23628,.T.) ;
#19315 = FACE_OUTER_BOUND('',#23629,.T.) ;
#19316 = FACE_OUTER_BOUND('',#23630,.T.) ;
#19317 = FACE_OUTER_BOUND('',#23631,.T.) ;
#19318 = FACE_OUTER_BOUND('',#23632,.T.) ;
#19319 = FACE_OUTER_BOUND('',#23633,.T.) ;
#19320 = FACE_OUTER_BOUND('',#23634,.T.) ;
#19321 = FACE_OUTER_BOUND('',#23635,.T.) ;
#19322 = FACE_OUTER_BOUND('',#23636,.T.) ;
#19323 = FACE_OUTER_BOUND('',#23637,.T.) ;
#19324 = FACE_OUTER_BOUND('',#23638,.T.) ;
#19325 = FACE_OUTER_BOUND('',#23639,.T.) ;
#19326 = FACE_OUTER_BOUND('',#23640,.T.) ;
#19327 = FACE_OUTER_BOUND('',#23641,.T.) ;
#19328 = FACE_OUTER_BOUND('',#23642,.T.) ;
#19329 = FACE_OUTER_BOUND('',#23643,.T.) ;
#19330 = FACE_OUTER_BOUND('',#23644,.T.) ;
#19331 = FACE_OUTER_BOUND('',#23645,.T.) ;
#19332 = FACE_OUTER_BOUND('',#23646,.T.) ;
#19333 = FACE_OUTER_BOUND('',#23647,.T.) ;
#19334 = FACE_OUTER_BOUND('',#23648,.T.) ;
#19335 = FACE_OUTER_BOUND('',#23649,.T.) ;
#19336 = FACE_OUTER_BOUND('',#23650,.T.) ;
#19337 = FACE_OUTER_BOUND('',#23651,.T.) ;
#19338 = FACE_OUTER_BOUND('',#23652,.T.) ;
#19339 = FACE_OUTER_BOUND('',#23653,.T.) ;
#19340 = FACE_OUTER_BOUND('',#23654,.T.) ;
#19341 = FACE_OUTER_BOUND('',#23655,.T.) ;
#19342 = FACE_OUTER_BOUND('',#23656,.T.) ;
#19343 = FACE_OUTER_BOUND('',#23657,.T.) ;
#19344 = FACE_OUTER_BOUND('',#23658,.T.) ;
#19345 = FACE_OUTER_BOUND('',#23659,.T.) ;
#19346 = FACE_OUTER_BOUND('',#23660,.T.) ;
#19347 = FACE_OUTER_BOUND('',#23661,.T.) ;
#19348 = FACE_OUTER_BOUND('',#23662,.T.) ;
#19349 = FACE_OUTER_BOUND('',#23663,.T.) ;
#19350 = FACE_OUTER_BOUND('',#23664,.T.) ;
#19351 = FACE_OUTER_BOUND('',#23665,.T.) ;
#19352 = FACE_OUTER_BOUND('',#23666,.T.) ;
#19353 = FACE_OUTER_BOUND('',#23667,.T.) ;
#19354 = FACE_OUTER_BOUND('',#23668,.T.) ;
#19355 = FACE_OUTER_BOUND('',#23669,.T.) ;
#19356 = FACE_OUTER_BOUND('',#23670,.T.) ;
#19357 = FACE_OUTER_BOUND('',#23671,.T.) ;
#19358 = FACE_OUTER_BOUND('',#23672,.T.) ;
#19359 = FACE_OUTER_BOUND('',#23673,.T.) ;
#19360 = FACE_OUTER_BOUND('',#23674,.T.) ;
#19361 = FACE_OUTER_BOUND('',#23675,.T.) ;
#19362 = FACE_OUTER_BOUND('',#23676,.T.) ;
#19363 = FACE_OUTER_BOUND('',#23677,.T.) ;
#19364 = FACE_OUTER_BOUND('',#23678,.T.) ;
#19365 = FACE_OUTER_BOUND('',#23679,.T.) ;
#19366 = FACE_OUTER_BOUND('',#23680,.T.) ;
#19367 = FACE_OUTER_BOUND('',#23681,.T.) ;
#19368 = FACE_OUTER_BOUND('',#23682,.T.) ;
#19369 = FACE_OUTER_BOUND('',#23683,.T.) ;
#19370 = FACE_OUTER_BOUND('',#23684,.T.) ;
#19371 = FACE_OUTER_BOUND('',#23685,.T.) ;
#19372 = FACE_OUTER_BOUND('',#23686,.T.) ;
#19373 = FACE_OUTER_BOUND('',#23687,.T.) ;
#19374 = FACE_OUTER_BOUND('',#23688,.T.) ;
#19375 = FACE_OUTER_BOUND('',#23689,.T.) ;
#19376 = FACE_OUTER_BOUND('',#23690,.T.) ;
#19377 = FACE_OUTER_BOUND('',#23691,.T.) ;
#19378 = FACE_OUTER_BOUND('',#23692,.T.) ;
#19379 = FACE_OUTER_BOUND('',#23693,.T.) ;
#19380 = FACE_OUTER_BOUND('',#23694,.T.) ;
#19381 = FACE_OUTER_BOUND('',#23695,.T.) ;
#19382 = FACE_OUTER_BOUND('',#23696,.T.) ;
#19383 = FACE_OUTER_BOUND('',#23697,.T.) ;
#19384 = FACE_OUTER_BOUND('',#23698,.T.) ;
#19385 = FACE_OUTER_BOUND('',#23699,.T.) ;
#19386 = FACE_OUTER_BOUND('',#23700,.T.) ;
#19387 = FACE_OUTER_BOUND('',#23701,.T.) ;
#19388 = FACE_OUTER_BOUND('',#23702,.T.) ;
#19389 = FACE_OUTER_BOUND('',#23703,.T.) ;
#19390 = FACE_OUTER_BOUND('',#23704,.T.) ;
#19391 = FACE_OUTER_BOUND('',#23705,.T.) ;
#19392 = FACE_OUTER_BOUND('',#23706,.T.) ;
#19393 = FACE_OUTER_BOUND('',#23707,.T.) ;
#19394 = FACE_OUTER_BOUND('',#23708,.T.) ;
#19395 = FACE_OUTER_BOUND('',#23709,.T.) ;
#19396 = FACE_OUTER_BOUND('',#23710,.T.) ;
#19397 = FACE_OUTER_BOUND('',#23711,.T.) ;
#19398 = FACE_OUTER_BOUND('',#23712,.T.) ;
#19399 = FACE_OUTER_BOUND('',#23713,.T.) ;
#19400 = FACE_OUTER_BOUND('',#23714,.T.) ;
#19401 = FACE_OUTER_BOUND('',#23715,.T.) ;
#19402 = FACE_OUTER_BOUND('',#23716,.T.) ;
#19403 = FACE_OUTER_BOUND('',#23717,.T.) ;
#19404 = FACE_OUTER_BOUND('',#23718,.T.) ;
#19405 = FACE_OUTER_BOUND('',#23719,.T.) ;
#19406 = FACE_OUTER_BOUND('',#23720,.T.) ;
#19407 = FACE_OUTER_BOUND('',#23721,.T.) ;
#19408 = FACE_OUTER_BOUND('',#23722,.T.) ;
#19409 = FACE_OUTER_BOUND('',#23723,.T.) ;
#19410 = FACE_OUTER_BOUND('',#23724,.T.) ;
#19411 = FACE_OUTER_BOUND('',#23725,.T.) ;
#19412 = FACE_OUTER_BOUND('',#23726,.T.) ;
#19413 = FACE_OUTER_BOUND('',#23727,.T.) ;
#19414 = FACE_OUTER_BOUND('',#23728,.T.) ;
#19415 = FACE_OUTER_BOUND('',#23729,.T.) ;
#19416 = FACE_OUTER_BOUND('',#23730,.T.) ;
#19417 = FACE_OUTER_BOUND('',#23731,.T.) ;
#19418 = FACE_OUTER_BOUND('',#23732,.T.) ;
#19419 = FACE_OUTER_BOUND('',#23733,.T.) ;
#19420 = FACE_OUTER_BOUND('',#23734,.T.) ;
#19421 = FACE_OUTER_BOUND('',#23735,.T.) ;
#19422 = FACE_OUTER_BOUND('',#23736,.T.) ;
#19423 = FACE_OUTER_BOUND('',#23737,.T.) ;
#19424 = FACE_OUTER_BOUND('',#23738,.T.) ;
#19425 = FACE_OUTER_BOUND('',#23739,.T.) ;
#19426 = FACE_OUTER_BOUND('',#23740,.T.) ;
#19427 = FACE_OUTER_BOUND('',#23741,.T.) ;
#19428 = FACE_OUTER_BOUND('',#23742,.T.) ;
#19429 = FACE_OUTER_BOUND('',#23743,.T.) ;
#19430 = FACE_OUTER_BOUND('',#23744,.T.) ;
#19431 = FACE_OUTER_BOUND('',#23745,.T.) ;
#19432 = FACE_OUTER_BOUND('',#23746,.T.) ;
#19433 = FACE_OUTER_BOUND('',#23747,.T.) ;
#19434 = FACE_OUTER_BOUND('',#23748,.T.) ;
#19435 = FACE_OUTER_BOUND('',#23749,.T.) ;
#19436 = FACE_OUTER_BOUND('',#23750,.T.) ;
#19437 = FACE_OUTER_BOUND('',#23751,.T.) ;
#19438 = FACE_OUTER_BOUND('',#23752,.T.) ;
#19439 = FACE_OUTER_BOUND('',#23753,.T.) ;
#19440 = FACE_OUTER_BOUND('',#23754,.T.) ;
#19441 = FACE_OUTER_BOUND('',#23755,.T.) ;
#19442 = FACE_OUTER_BOUND('',#23756,.T.) ;
#19443 = FACE_OUTER_BOUND('',#23757,.T.) ;
#19444 = FACE_OUTER_BOUND('',#23758,.T.) ;
#19445 = FACE_OUTER_BOUND('',#23759,.T.) ;
#19446 = FACE_OUTER_BOUND('',#23760,.T.) ;
#19447 = FACE_OUTER_BOUND('',#23761,.T.) ;
#19448 = FACE_OUTER_BOUND('',#23762,.T.) ;
#19449 = FACE_OUTER_BOUND('',#23763,.T.) ;
#19450 = FACE_OUTER_BOUND('',#23764,.T.) ;
#19451 = FACE_OUTER_BOUND('',#23765,.T.) ;
#19452 = FACE_OUTER_BOUND('',#23766,.T.) ;
#19453 = FACE_OUTER_BOUND('',#23767,.T.) ;
#19454 = FACE_OUTER_BOUND('',#23768,.T.) ;
#19455 = FACE_OUTER_BOUND('',#23769,.T.) ;
#19456 = FACE_OUTER_BOUND('',#23770,.T.) ;
#19457 = FACE_OUTER_BOUND('',#23771,.T.) ;
#19458 = FACE_OUTER_BOUND('',#23772,.T.) ;
#19459 = FACE_OUTER_BOUND('',#23773,.T.) ;
#19460 = FACE_OUTER_BOUND('',#23774,.T.) ;
#19461 = FACE_OUTER_BOUND('',#23775,.T.) ;
#19462 = FACE_OUTER_BOUND('',#23776,.T.) ;
#19463 = FACE_OUTER_BOUND('',#23777,.T.) ;
#19464 = FACE_OUTER_BOUND('',#23778,.T.) ;
#19465 = FACE_OUTER_BOUND('',#23779,.T.) ;
#19466 = FACE_OUTER_BOUND('',#23780,.T.) ;
#19467 = FACE_OUTER_BOUND('',#23781,.T.) ;
#19468 = FACE_OUTER_BOUND('',#23782,.T.) ;
#19469 = FACE_OUTER_BOUND('',#23783,.T.) ;
#19470 = FACE_OUTER_BOUND('',#23784,.T.) ;
#19471 = FACE_OUTER_BOUND('',#23785,.T.) ;
#19472 = FACE_OUTER_BOUND('',#23786,.T.) ;
#19473 = FACE_OUTER_BOUND('',#23787,.T.) ;
#19474 = FACE_OUTER_BOUND('',#23788,.T.) ;
#19475 = FACE_OUTER_BOUND('',#23789,.T.) ;
#19476 = FACE_OUTER_BOUND('',#23790,.T.) ;
#19477 = FACE_OUTER_BOUND('',#23791,.T.) ;
#19478 = FACE_OUTER_BOUND('',#23792,.T.) ;
#19479 = FACE_OUTER_BOUND('',#23793,.T.) ;
#19480 = FACE_OUTER_BOUND('',#23794,.T.) ;
#19481 = FACE_OUTER_BOUND('',#23795,.T.) ;
#19482 = FACE_OUTER_BOUND('',#23796,.T.) ;
#19483 = FACE_OUTER_BOUND('',#23797,.T.) ;
#19484 = FACE_OUTER_BOUND('',#23798,.T.) ;
#19485 = FACE_OUTER_BOUND('',#23799,.T.) ;
#19486 = FACE_OUTER_BOUND('',#23800,.T.) ;
#19487 = FACE_OUTER_BOUND('',#23801,.T.) ;
#19488 = FACE_OUTER_BOUND('',#23802,.T.) ;
#19489 = FACE_OUTER_BOUND('',#23803,.T.) ;
#19490 = FACE_OUTER_BOUND('',#23804,.T.) ;
#19491 = FACE_OUTER_BOUND('',#23805,.T.) ;
#19492 = FACE_OUTER_BOUND('',#23806,.T.) ;
#19493 = FACE_OUTER_BOUND('',#23807,.T.) ;
#19494 = FACE_OUTER_BOUND('',#23808,.T.) ;
#19495 = FACE_OUTER_BOUND('',#23809,.T.) ;
#19496 = FACE_OUTER_BOUND('',#23810,.T.) ;
#19497 = FACE_OUTER_BOUND('',#23811,.T.) ;
#19498 = FACE_OUTER_BOUND('',#23812,.T.) ;
#19499 = FACE_OUTER_BOUND('',#23813,.T.) ;
#19500 = FACE_OUTER_BOUND('',#23814,.T.) ;
#19501 = FACE_OUTER_BOUND('',#23815,.T.) ;
#19502 = FACE_OUTER_BOUND('',#23816,.T.) ;
#19503 = FACE_OUTER_BOUND('',#23817,.T.) ;
#19504 = FACE_OUTER_BOUND('',#23818,.T.) ;
#19505 = FACE_OUTER_BOUND('',#23819,.T.) ;
#19506 = FACE_OUTER_BOUND('',#23820,.T.) ;
#19507 = FACE_OUTER_BOUND('',#23821,.T.) ;
#19508 = FACE_OUTER_BOUND('',#23822,.T.) ;
#19509 = FACE_OUTER_BOUND('',#23823,.T.) ;
#19510 = FACE_OUTER_BOUND('',#23824,.T.) ;
#19511 = FACE_OUTER_BOUND('',#23825,.T.) ;
#19512 = FACE_OUTER_BOUND('',#23826,.T.) ;
#19513 = FACE_OUTER_BOUND('',#23827,.T.) ;
#19514 = FACE_OUTER_BOUND('',#23828,.T.) ;
#19515 = FACE_OUTER_BOUND('',#23829,.T.) ;
#19516 = FACE_OUTER_BOUND('',#23830,.T.) ;
#19517 = FACE_OUTER_BOUND('',#23831,.T.) ;
#19518 = FACE_OUTER_BOUND('',#23832,.T.) ;
#19519 = FACE_OUTER_BOUND('',#23833,.T.) ;
#19520 = FACE_OUTER_BOUND('',#23834,.T.) ;
#19521 = FACE_OUTER_BOUND('',#23835,.T.) ;
#19522 = FACE_OUTER_BOUND('',#23836,.T.) ;
#19523 = FACE_OUTER_BOUND('',#23837,.T.) ;
#19524 = FACE_OUTER_BOUND('',#23838,.T.) ;
#19525 = FACE_OUTER_BOUND('',#23839,.T.) ;
#19526 = FACE_OUTER_BOUND('',#23840,.T.) ;
#19527 = FACE_OUTER_BOUND('',#23841,.T.) ;
#19528 = FACE_OUTER_BOUND('',#23842,.T.) ;
#19529 = FACE_OUTER_BOUND('',#23843,.T.) ;
#19530 = FACE_OUTER_BOUND('',#23844,.T.) ;
#19531 = FACE_OUTER_BOUND('',#23845,.T.) ;
#19532 = FACE_OUTER_BOUND('',#23846,.T.) ;
#19533 = FACE_OUTER_BOUND('',#23847,.T.) ;
#19534 = FACE_OUTER_BOUND('',#23848,.T.) ;
#19535 = FACE_OUTER_BOUND('',#23849,.T.) ;
#19536 = FACE_OUTER_BOUND('',#23850,.T.) ;
#19537 = FACE_OUTER_BOUND('',#23851,.T.) ;
#19538 = FACE_OUTER_BOUND('',#23852,.T.) ;
#19539 = FACE_OUTER_BOUND('',#23853,.T.) ;
#19540 = FACE_OUTER_BOUND('',#23854,.T.) ;
#19541 = FACE_OUTER_BOUND('',#23855,.T.) ;
#19542 = FACE_OUTER_BOUND('',#23856,.T.) ;
#19543 = FACE_OUTER_BOUND('',#23857,.T.) ;
#19544 = FACE_OUTER_BOUND('',#23858,.T.) ;
#19545 = FACE_OUTER_BOUND('',#23859,.T.) ;
#19546 = FACE_OUTER_BOUND('',#23860,.T.) ;
#19547 = FACE_OUTER_BOUND('',#23861,.T.) ;
#19548 = FACE_OUTER_BOUND('',#23862,.T.) ;
#19549 = FACE_OUTER_BOUND('',#23863,.T.) ;
#19550 = FACE_OUTER_BOUND('',#23864,.T.) ;
#19551 = FACE_OUTER_BOUND('',#23865,.T.) ;
#19552 = FACE_OUTER_BOUND('',#23866,.T.) ;
#19553 = FACE_OUTER_BOUND('',#23867,.T.) ;
#19554 = FACE_OUTER_BOUND('',#23868,.T.) ;
#19555 = FACE_OUTER_BOUND('',#23869,.T.) ;
#19556 = FACE_OUTER_BOUND('',#23870,.T.) ;
#19557 = FACE_OUTER_BOUND('',#23871,.T.) ;
#19558 = FACE_OUTER_BOUND('',#23872,.T.) ;
#19559 = FACE_OUTER_BOUND('',#23873,.T.) ;
#19560 = FACE_OUTER_BOUND('',#23874,.T.) ;
#19561 = FACE_OUTER_BOUND('',#23875,.T.) ;
#19562 = FACE_OUTER_BOUND('',#23876,.T.) ;
#19563 = FACE_OUTER_BOUND('',#23877,.T.) ;
#19564 = FACE_OUTER_BOUND('',#23878,.T.) ;
#19565 = FACE_OUTER_BOUND('',#23879,.T.) ;
#19566 = FACE_OUTER_BOUND('',#23880,.T.) ;
#19567 = FACE_OUTER_BOUND('',#23881,.T.) ;
#19568 = FACE_OUTER_BOUND('',#23882,.T.) ;
#19569 = FACE_OUTER_BOUND('',#23883,.T.) ;
#19570 = FACE_OUTER_BOUND('',#23884,.T.) ;
#19571 = FACE_OUTER_BOUND('',#23885,.T.) ;
#19572 = FACE_OUTER_BOUND('',#23886,.T.) ;
#19573 = FACE_OUTER_BOUND('',#23887,.T.) ;
#19574 = FACE_OUTER_BOUND('',#23888,.T.) ;
#19575 = FACE_OUTER_BOUND('',#23889,.T.) ;
#19576 = FACE_OUTER_BOUND('',#23890,.T.) ;
#19577 = FACE_OUTER_BOUND('',#23891,.T.) ;
#19578 = FACE_OUTER_BOUND('',#23892,.T.) ;
#19579 = FACE_OUTER_BOUND('',#23893,.T.) ;
#19580 = FACE_OUTER_BOUND('',#23894,.T.) ;
#19581 = FACE_OUTER_BOUND('',#23895,.T.) ;
#19582 = FACE_OUTER_BOUND('',#23896,.T.) ;
#19583 = FACE_OUTER_BOUND('',#23897,.T.) ;
#19584 = FACE_OUTER_BOUND('',#23898,.T.) ;
#19585 = FACE_OUTER_BOUND('',#23899,.T.) ;
#19586 = FACE_OUTER_BOUND('',#23900,.T.) ;
#19587 = FACE_OUTER_BOUND('',#23901,.T.) ;
#19588 = FACE_OUTER_BOUND('',#23902,.T.) ;
#19589 = FACE_OUTER_BOUND('',#23903,.T.) ;
#19590 = FACE_OUTER_BOUND('',#23904,.T.) ;
#19591 = FACE_OUTER_BOUND('',#23905,.T.) ;
#19592 = FACE_OUTER_BOUND('',#23906,.T.) ;
#19593 = FACE_OUTER_BOUND('',#23907,.T.) ;
#19594 = FACE_OUTER_BOUND('',#23908,.T.) ;
#19595 = FACE_OUTER_BOUND('',#23909,.T.) ;
#19596 = FACE_OUTER_BOUND('',#23910,.T.) ;
#19597 = FACE_OUTER_BOUND('',#23911,.T.) ;
#19598 = FACE_OUTER_BOUND('',#23912,.T.) ;
#19599 = FACE_OUTER_BOUND('',#23913,.T.) ;
#19600 = FACE_OUTER_BOUND('',#23914,.T.) ;
#19601 = FACE_OUTER_BOUND('',#23915,.T.) ;
#19602 = FACE_OUTER_BOUND('',#23916,.T.) ;
#19603 = FACE_OUTER_BOUND('',#23917,.T.) ;
#19604 = FACE_OUTER_BOUND('',#23918,.T.) ;
#19605 = FACE_OUTER_BOUND('',#23919,.T.) ;
#19606 = FACE_OUTER_BOUND('',#23920,.T.) ;
#19607 = FACE_OUTER_BOUND('',#23921,.T.) ;
#19608 = FACE_OUTER_BOUND('',#23922,.T.) ;
#19609 = FACE_OUTER_BOUND('',#23923,.T.) ;
#19610 = FACE_OUTER_BOUND('',#23924,.T.) ;
#19611 = FACE_OUTER_BOUND('',#23925,.T.) ;
#19612 = FACE_OUTER_BOUND('',#23926,.T.) ;
#19613 = FACE_OUTER_BOUND('',#23927,.T.) ;
#19614 = FACE_OUTER_BOUND('',#23928,.T.) ;
#19615 = FACE_OUTER_BOUND('',#23929,.T.) ;
#19616 = FACE_OUTER_BOUND('',#23930,.T.) ;
#19617 = FACE_OUTER_BOUND('',#23931,.T.) ;
#19618 = FACE_OUTER_BOUND('',#23932,.T.) ;
#19619 = FACE_OUTER_BOUND('',#23933,.T.) ;
#19620 = FACE_OUTER_BOUND('',#23934,.T.) ;
#19621 = FACE_OUTER_BOUND('',#23935,.T.) ;
#19622 = FACE_OUTER_BOUND('',#23936,.T.) ;
#19623 = FACE_OUTER_BOUND('',#23937,.T.) ;
#19624 = FACE_OUTER_BOUND('',#23938,.T.) ;
#19625 = FACE_OUTER_BOUND('',#23939,.T.) ;
#19626 = FACE_OUTER_BOUND('',#23940,.T.) ;
#19627 = FACE_OUTER_BOUND('',#23941,.T.) ;
#19628 = FACE_OUTER_BOUND('',#23942,.T.) ;
#19629 = FACE_OUTER_BOUND('',#23943,.T.) ;
#19630 = FACE_OUTER_BOUND('',#23944,.T.) ;
#19631 = FACE_OUTER_BOUND('',#23945,.T.) ;
#19632 = FACE_OUTER_BOUND('',#23946,.T.) ;
#19633 = FACE_OUTER_BOUND('',#23947,.T.) ;
#19634 = FACE_OUTER_BOUND('',#23948,.T.) ;
#19635 = FACE_OUTER_BOUND('',#23949,.T.) ;
#19636 = FACE_OUTER_BOUND('',#23950,.T.) ;
#19637 = FACE_OUTER_BOUND('',#23951,.T.) ;
#19638 = FACE_OUTER_BOUND('',#23952,.T.) ;
#19639 = FACE_OUTER_BOUND('',#23953,.T.) ;
#19640 = FACE_OUTER_BOUND('',#23954,.T.) ;
#19641 = FACE_OUTER_BOUND('',#23955,.T.) ;
#19642 = FACE_OUTER_BOUND('',#23956,.T.) ;
#19643 = FACE_OUTER_BOUND('',#23957,.T.) ;
#19644 = FACE_OUTER_BOUND('',#23958,.T.) ;
#19645 = FACE_OUTER_BOUND('',#23959,.T.) ;
#19646 = FACE_OUTER_BOUND('',#23960,.T.) ;
#19647 = FACE_OUTER_BOUND('',#23961,.T.) ;
#19648 = FACE_OUTER_BOUND('',#23962,.T.) ;
#19649 = FACE_OUTER_BOUND('',#23963,.T.) ;
#19650 = FACE_OUTER_BOUND('',#23964,.T.) ;
#19651 = FACE_OUTER_BOUND('',#23965,.T.) ;
#19652 = FACE_OUTER_BOUND('',#23966,.T.) ;
#19653 = FACE_OUTER_BOUND('',#23967,.T.) ;
#19654 = FACE_OUTER_BOUND('',#23968,.T.) ;
#19655 = FACE_OUTER_BOUND('',#23969,.T.) ;
#19656 = FACE_OUTER_BOUND('',#23970,.T.) ;
#19657 = FACE_OUTER_BOUND('',#23971,.T.) ;
#19658 = FACE_OUTER_BOUND('',#23972,.T.) ;
#19659 = FACE_OUTER_BOUND('',#23973,.T.) ;
#19660 = FACE_OUTER_BOUND('',#23974,.T.) ;
#19661 = FACE_OUTER_BOUND('',#23975,.T.) ;
#19662 = FACE_OUTER_BOUND('',#23976,.T.) ;
#19663 = FACE_OUTER_BOUND('',#23977,.T.) ;
#19664 = FACE_OUTER_BOUND('',#23978,.T.) ;
#19665 = FACE_OUTER_BOUND('',#23979,.T.) ;
#19666 = FACE_OUTER_BOUND('',#23980,.T.) ;
#19667 = FACE_OUTER_BOUND('',#23981,.T.) ;
#19668 = FACE_OUTER_BOUND('',#23982,.T.) ;
#19669 = FACE_OUTER_BOUND('',#23983,.T.) ;
#19670 = FACE_OUTER_BOUND('',#23984,.T.) ;
#19671 = FACE_OUTER_BOUND('',#23985,.T.) ;
#19672 = FACE_OUTER_BOUND('',#23986,.T.) ;
#19673 = FACE_OUTER_BOUND('',#23987,.T.) ;
#19674 = FACE_OUTER_BOUND('',#23988,.T.) ;
#19675 = FACE_OUTER_BOUND('',#23989,.T.) ;
#19676 = FACE_OUTER_BOUND('',#23990,.T.) ;
#19677 = FACE_OUTER_BOUND('',#23991,.T.) ;
#19678 = FACE_OUTER_BOUND('',#23992,.T.) ;
#19679 = FACE_OUTER_BOUND('',#23993,.T.) ;
#19680 = FACE_OUTER_BOUND('',#23994,.T.) ;
#19681 = FACE_OUTER_BOUND('',#23995,.T.) ;
#19682 = FACE_OUTER_BOUND('',#23996,.T.) ;
#19683 = FACE_OUTER_BOUND('',#23997,.T.) ;
#19684 = FACE_OUTER_BOUND('',#23998,.T.) ;
#19685 = FACE_OUTER_BOUND('',#23999,.T.) ;
#19686 = FACE_OUTER_BOUND('',#24000,.T.) ;
#19687 = FACE_OUTER_BOUND('',#24001,.T.) ;
#19688 = FACE_OUTER_BOUND('',#24002,.T.) ;
#19689 = FACE_OUTER_BOUND('',#24003,.T.) ;
#19690 = FACE_OUTER_BOUND('',#24004,.T.) ;
#19691 = FACE_OUTER_BOUND('',#24005,.T.) ;
#19692 = FACE_OUTER_BOUND('',#24006,.T.) ;
#19693 = FACE_OUTER_BOUND('',#24007,.T.) ;
#19694 = FACE_OUTER_BOUND('',#24008,.T.) ;
#19695 = FACE_OUTER_BOUND('',#24009,.T.) ;
#19696 = FACE_OUTER_BOUND('',#24010,.T.) ;
#19697 = FACE_OUTER_BOUND('',#24011,.T.) ;
#19698 = FACE_OUTER_BOUND('',#24012,.T.) ;
#19699 = FACE_OUTER_BOUND('',#24013,.T.) ;
#19700 = FACE_OUTER_BOUND('',#24014,.T.) ;
#19701 = FACE_OUTER_BOUND('',#24015,.T.) ;
#19702 = FACE_OUTER_BOUND('',#24016,.T.) ;
#19703 = FACE_OUTER_BOUND('',#24017,.T.) ;
#19704 = FACE_OUTER_BOUND('',#24018,.T.) ;
#19705 = FACE_OUTER_BOUND('',#24019,.T.) ;
#19706 = FACE_OUTER_BOUND('',#24020,.T.) ;
#19707 = FACE_OUTER_BOUND('',#24021,.T.) ;
#19708 = FACE_OUTER_BOUND('',#24022,.T.) ;
#19709 = FACE_OUTER_BOUND('',#24023,.T.) ;
#19710 = FACE_OUTER_BOUND('',#24024,.T.) ;
#19711 = FACE_OUTER_BOUND('',#24025,.T.) ;
#19712 = FACE_OUTER_BOUND('',#24026,.T.) ;
#19713 = FACE_OUTER_BOUND('',#24027,.T.) ;
#19714 = FACE_OUTER_BOUND('',#24028,.T.) ;
#19715 = FACE_OUTER_BOUND('',#24029,.T.) ;
#19716 = FACE_OUTER_BOUND('',#24030,.T.) ;
#19717 = FACE_OUTER_BOUND('',#24031,.T.) ;
#19718 = FACE_OUTER_BOUND('',#24032,.T.) ;
#19719 = FACE_OUTER_BOUND('',#24033,.T.) ;
#19720 = FACE_OUTER_BOUND('',#24034,.T.) ;
#19721 = FACE_OUTER_BOUND('',#24035,.T.) ;
#19722 = FACE_OUTER_BOUND('',#24036,.T.) ;
#19723 = FACE_OUTER_BOUND('',#24037,.T.) ;
#19724 = FACE_OUTER_BOUND('',#24038,.T.) ;
#19725 = FACE_OUTER_BOUND('',#24039,.T.) ;
#19726 = FACE_OUTER_BOUND('',#24040,.T.) ;
#19727 = FACE_OUTER_BOUND('',#24041,.T.) ;
#19728 = FACE_OUTER_BOUND('',#24042,.T.) ;
#19729 = FACE_OUTER_BOUND('',#24043,.T.) ;
#19730 = FACE_OUTER_BOUND('',#24044,.T.) ;
#19731 = FACE_OUTER_BOUND('',#24045,.T.) ;
#19732 = FACE_OUTER_BOUND('',#24046,.T.) ;
#19733 = FACE_OUTER_BOUND('',#24047,.T.) ;
#19734 = FACE_OUTER_BOUND('',#24048,.T.) ;
#19735 = FACE_OUTER_BOUND('',#24049,.T.) ;
#19736 = FACE_OUTER_BOUND('',#24050,.T.) ;
#19737 = FACE_OUTER_BOUND('',#24051,.T.) ;
#19738 = FACE_OUTER_BOUND('',#24052,.T.) ;
#19739 = FACE_OUTER_BOUND('',#24053,.T.) ;
#19740 = FACE_OUTER_BOUND('',#24054,.T.) ;
#19741 = FACE_OUTER_BOUND('',#24055,.T.) ;
#19742 = FACE_OUTER_BOUND('',#24056,.T.) ;
#19743 = FACE_OUTER_BOUND('',#24057,.T.) ;
#19744 = FACE_OUTER_BOUND('',#24058,.T.) ;
#19745 = FACE_OUTER_BOUND('',#24059,.T.) ;
#19746 = FACE_OUTER_BOUND('',#24060,.T.) ;
#19747 = FACE_OUTER_BOUND('',#24061,.T.) ;
#19748 = FACE_OUTER_BOUND('',#24062,.T.) ;
#19749 = FACE_OUTER_BOUND('',#24063,.T.) ;
#19750 = FACE_OUTER_BOUND('',#24064,.T.) ;
#19751 = FACE_OUTER_BOUND('',#24065,.T.) ;
#19752 = FACE_OUTER_BOUND('',#24066,.T.) ;
#19753 = FACE_OUTER_BOUND('',#24067,.T.) ;
#19754 = FACE_OUTER_BOUND('',#24068,.T.) ;
#19755 = FACE_OUTER_BOUND('',#24069,.T.) ;
#19756 = FACE_OUTER_BOUND('',#24070,.T.) ;
#19757 = FACE_OUTER_BOUND('',#24071,.T.) ;
#19758 = FACE_OUTER_BOUND('',#24072,.T.) ;
#19759 = FACE_OUTER_BOUND('',#24073,.T.) ;
#19760 = FACE_OUTER_BOUND('',#24074,.T.) ;
#19761 = FACE_OUTER_BOUND('',#24075,.T.) ;
#19762 = FACE_OUTER_BOUND('',#24076,.T.) ;
#19763 = FACE_OUTER_BOUND('',#24077,.T.) ;
#19764 = FACE_OUTER_BOUND('',#24078,.T.) ;
#19765 = FACE_OUTER_BOUND('',#24079,.T.) ;
#19766 = FACE_OUTER_BOUND('',#24080,.T.) ;
#19767 = FACE_OUTER_BOUND('',#24081,.T.) ;
#19768 = FACE_OUTER_BOUND('',#24082,.T.) ;
#19769 = FACE_OUTER_BOUND('',#24083,.T.) ;
#19770 = FACE_OUTER_BOUND('',#24084,.T.) ;
#19771 = FACE_OUTER_BOUND('',#24085,.T.) ;
#19772 = FACE_OUTER_BOUND('',#24086,.T.) ;
#19773 = FACE_OUTER_BOUND('',#24087,.T.) ;
#19774 = FACE_OUTER_BOUND('',#24088,.T.) ;
#19775 = FACE_OUTER_BOUND('',#24089,.T.) ;
#19776 = FACE_OUTER_BOUND('',#24090,.T.) ;
#19777 = FACE_OUTER_BOUND('',#24091,.T.) ;
#19778 = FACE_OUTER_BOUND('',#24092,.T.) ;
#19779 = FACE_OUTER_BOUND('',#24093,.T.) ;
#19780 = FACE_OUTER_BOUND('',#24094,.T.) ;
#19781 = FACE_OUTER_BOUND('',#24095,.T.) ;
#19782 = FACE_OUTER_BOUND('',#24096,.T.) ;
#19783 = FACE_OUTER_BOUND('',#24097,.T.) ;
#19784 = FACE_OUTER_BOUND('',#24098,.T.) ;
#19785 = FACE_OUTER_BOUND('',#24099,.T.) ;
#19786 = FACE_OUTER_BOUND('',#24100,.T.) ;
#19787 = FACE_OUTER_BOUND('',#24101,.T.) ;
#19788 = FACE_OUTER_BOUND('',#24102,.T.) ;
#19789 = FACE_OUTER_BOUND('',#24103,.T.) ;
#19790 = FACE_OUTER_BOUND('',#24104,.T.) ;
#19791 = FACE_OUTER_BOUND('',#24105,.T.) ;
#19792 = FACE_OUTER_BOUND('',#24106,.T.) ;
#19793 = FACE_OUTER_BOUND('',#24107,.T.) ;
#19794 = FACE_OUTER_BOUND('',#24108,.T.) ;
#19795 = FACE_OUTER_BOUND('',#24109,.T.) ;
#19796 = FACE_OUTER_BOUND('',#24110,.T.) ;
#19797 = FACE_OUTER_BOUND('',#24111,.T.) ;
#19798 = FACE_OUTER_BOUND('',#24112,.T.) ;
#19799 = FACE_OUTER_BOUND('',#24113,.T.) ;
#19800 = FACE_OUTER_BOUND('',#24114,.T.) ;
#19801 = FACE_OUTER_BOUND('',#24115,.T.) ;
#19802 = FACE_OUTER_BOUND('',#24116,.T.) ;
#19803 = FACE_OUTER_BOUND('',#24117,.T.) ;
#19804 = FACE_OUTER_BOUND('',#24118,.T.) ;
#19805 = FACE_OUTER_BOUND('',#24119,.T.) ;
#19806 = FACE_OUTER_BOUND('',#24120,.T.) ;
#19807 = FACE_OUTER_BOUND('',#24121,.T.) ;
#19808 = FACE_OUTER_BOUND('',#24122,.T.) ;
#19809 = FACE_OUTER_BOUND('',#24123,.T.) ;
#19810 = FACE_OUTER_BOUND('',#24124,.T.) ;
#19811 = FACE_OUTER_BOUND('',#24125,.T.) ;
#19812 = FACE_OUTER_BOUND('',#24126,.T.) ;
#19813 = FACE_OUTER_BOUND('',#24127,.T.) ;
#19814 = FACE_OUTER_BOUND('',#24128,.T.) ;
#19815 = FACE_OUTER_BOUND('',#24129,.T.) ;
#19816 = FACE_OUTER_BOUND('',#24130,.T.) ;
#19817 = FACE_OUTER_BOUND('',#24131,.T.) ;
#19818 = FACE_OUTER_BOUND('',#24132,.T.) ;
#19819 = FACE_OUTER_BOUND('',#24133,.T.) ;
#19820 = FACE_OUTER_BOUND('',#24134,.T.) ;
#19821 = FACE_OUTER_BOUND('',#24135,.T.) ;
#19822 = FACE_OUTER_BOUND('',#24136,.T.) ;
#19823 = FACE_OUTER_BOUND('',#24137,.T.) ;
#19824 = FACE_OUTER_BOUND('',#24138,.T.) ;
#19825 = FACE_OUTER_BOUND('',#24139,.T.) ;
#19826 = FACE_OUTER_BOUND('',#24140,.T.) ;
#19827 = FACE_OUTER_BOUND('',#24141,.T.) ;
#19828 = FACE_OUTER_BOUND('',#24142,.T.) ;
#19829 = FACE_OUTER_BOUND('',#24143,.T.) ;
#19830 = FACE_OUTER_BOUND('',#24144,.T.) ;
#19831 = FACE_OUTER_BOUND('',#24145,.T.) ;
#19832 = FACE_OUTER_BOUND('',#24146,.T.) ;
#19833 = FACE_OUTER_BOUND('',#24147,.T.) ;
#19834 = FACE_OUTER_BOUND('',#24148,.T.) ;
#19835 = FACE_OUTER_BOUND('',#24149,.T.) ;
#19836 = FACE_OUTER_BOUND('',#24150,.T.) ;
#19837 = FACE_OUTER_BOUND('',#24151,.T.) ;
#19838 = FACE_OUTER_BOUND('',#24152,.T.) ;
#19839 = FACE_OUTER_BOUND('',#24153,.T.) ;
#19840 = FACE_OUTER_BOUND('',#24154,.T.) ;
#19841 = FACE_OUTER_BOUND('',#24155,.T.) ;
#19842 = FACE_OUTER_BOUND('',#24156,.T.) ;
#19843 = FACE_OUTER_BOUND('',#24157,.T.) ;
#19844 = FACE_OUTER_BOUND('',#24158,.T.) ;
#19845 = FACE_OUTER_BOUND('',#24159,.T.) ;
#19846 = FACE_OUTER_BOUND('',#24160,.T.) ;
#19847 = FACE_OUTER_BOUND('',#24161,.T.) ;
#19848 = FACE_OUTER_BOUND('',#24162,.T.) ;
#19849 = FACE_OUTER_BOUND('',#24163,.T.) ;
#19850 = FACE_OUTER_BOUND('',#24164,.T.) ;
#19851 = FACE_OUTER_BOUND('',#24165,.T.) ;
#19852 = FACE_OUTER_BOUND('',#24166,.T.) ;
#19853 = FACE_OUTER_BOUND('',#24167,.T.) ;
#19854 = FACE_OUTER_BOUND('',#24168,.T.) ;
#19855 = FACE_OUTER_BOUND('',#24169,.T.) ;
#19856 = FACE_OUTER_BOUND('',#24170,.T.) ;
#19857 = FACE_OUTER_BOUND('',#24171,.T.) ;
#19858 = FACE_OUTER_BOUND('',#24172,.T.) ;
#19859 = FACE_OUTER_BOUND('',#24173,.T.) ;
#19860 = FACE_OUTER_BOUND('',#24174,.T.) ;
#19861 = FACE_OUTER_BOUND('',#24175,.T.) ;
#19862 = FACE_OUTER_BOUND('',#24176,.T.) ;
#19863 = FACE_OUTER_BOUND('',#24177,.T.) ;
#19864 = FACE_OUTER_BOUND('',#24178,.T.) ;
#19865 = FACE_OUTER_BOUND('',#24179,.T.) ;
#19866 = FACE_OUTER_BOUND('',#24180,.T.) ;
#19867 = FACE_OUTER_BOUND('',#24181,.T.) ;
#19868 = FACE_OUTER_BOUND('',#24182,.T.) ;
#19869 = FACE_OUTER_BOUND('',#24183,.T.) ;
#19870 = FACE_OUTER_BOUND('',#24184,.T.) ;
#19871 = FACE_OUTER_BOUND('',#24185,.T.) ;
#19872 = FACE_OUTER_BOUND('',#24186,.T.) ;
#19873 = FACE_OUTER_BOUND('',#24187,.T.) ;
#19874 = FACE_OUTER_BOUND('',#24188,.T.) ;
#19875 = FACE_OUTER_BOUND('',#24189,.T.) ;
#19876 = FACE_OUTER_BOUND('',#24190,.T.) ;
#19877 = FACE_OUTER_BOUND('',#24191,.T.) ;
#19878 = FACE_OUTER_BOUND('',#24192,.T.) ;
#19879 = FACE_OUTER_BOUND('',#24193,.T.) ;
#19880 = FACE_OUTER_BOUND('',#24194,.T.) ;
#19881 = FACE_OUTER_BOUND('',#24195,.T.) ;
#19882 = FACE_OUTER_BOUND('',#24196,.T.) ;
#19883 = FACE_OUTER_BOUND('',#24197,.T.) ;
#19884 = FACE_OUTER_BOUND('',#24198,.T.) ;
#19885 = FACE_OUTER_BOUND('',#24199,.T.) ;
#19886 = FACE_OUTER_BOUND('',#24200,.T.) ;
#19887 = FACE_OUTER_BOUND('',#24201,.T.) ;
#19888 = FACE_OUTER_BOUND('',#24202,.T.) ;
#19889 = FACE_OUTER_BOUND('',#24203,.T.) ;
#19890 = FACE_OUTER_BOUND('',#24204,.T.) ;
#19891 = FACE_OUTER_BOUND('',#24205,.T.) ;
#19892 = FACE_OUTER_BOUND('',#24206,.T.) ;
#19893 = FACE_OUTER_BOUND('',#24207,.T.) ;
#19894 = FACE_OUTER_BOUND('',#24208,.T.) ;
#19895 = FACE_OUTER_BOUND('',#24209,.T.) ;
#19896 = FACE_OUTER_BOUND('',#24210,.T.) ;
#19897 = FACE_OUTER_BOUND('',#24211,.T.) ;
#19898 = FACE_OUTER_BOUND('',#24212,.T.) ;
#19899 = FACE_OUTER_BOUND('',#24213,.T.) ;
#19900 = FACE_OUTER_BOUND('',#24214,.T.) ;
#19901 = FACE_OUTER_BOUND('',#24215,.T.) ;
#19902 = FACE_OUTER_BOUND('',#24216,.T.) ;
#19903 = FACE_OUTER_BOUND('',#24217,.T.) ;
#19904 = FACE_OUTER_BOUND('',#24218,.T.) ;
#19905 = FACE_OUTER_BOUND('',#24219,.T.) ;
#19906 = FACE_OUTER_BOUND('',#24220,.T.) ;
#19907 = FACE_OUTER_BOUND('',#24221,.T.) ;
#19908 = FACE_OUTER_BOUND('',#24222,.T.) ;
#19909 = FACE_OUTER_BOUND('',#24223,.T.) ;
#19910 = FACE_OUTER_BOUND('',#24224,.T.) ;
#19911 = FACE_OUTER_BOUND('',#24225,.T.) ;
#19912 = FACE_OUTER_BOUND('',#24226,.T.) ;
#19913 = FACE_OUTER_BOUND('',#24227,.T.) ;
#19914 = FACE_OUTER_BOUND('',#24228,.T.) ;
#19915 = FACE_OUTER_BOUND('',#24229,.T.) ;
#19916 = FACE_OUTER_BOUND('',#24230,.T.) ;
#19917 = FACE_OUTER_BOUND('',#24231,.T.) ;
#19918 = FACE_OUTER_BOUND('',#24232,.T.) ;
#19919 = FACE_OUTER_BOUND('',#24233,.T.) ;
#19920 = FACE_OUTER_BOUND('',#24234,.T.) ;
#19921 = FACE_OUTER_BOUND('',#24235,.T.) ;
#19922 = FACE_OUTER_BOUND('',#24236,.T.) ;
#19923 = FACE_OUTER_BOUND('',#24237,.T.) ;
#19924 = FACE_OUTER_BOUND('',#24238,.T.) ;
#19925 = FACE_OUTER_BOUND('',#24239,.T.) ;
#19926 = FACE_OUTER_BOUND('',#24240,.T.) ;
#19927 = FACE_OUTER_BOUND('',#24241,.T.) ;
#19928 = FACE_OUTER_BOUND('',#24242,.T.) ;
#19929 = FACE_OUTER_BOUND('',#24243,.T.) ;
#19930 = FACE_OUTER_BOUND('',#24244,.T.) ;
#19931 = FACE_OUTER_BOUND('',#24245,.T.) ;
#19932 = FACE_OUTER_BOUND('',#24246,.T.) ;
#19933 = FACE_OUTER_BOUND('',#24247,.T.) ;
#19934 = FACE_OUTER_BOUND('',#24248,.T.) ;
#19935 = FACE_OUTER_BOUND('',#24249,.T.) ;
#19936 = FACE_OUTER_BOUND('',#24250,.T.) ;
#19937 = FACE_OUTER_BOUND('',#24251,.T.) ;
#19938 = FACE_OUTER_BOUND('',#24252,.T.) ;
#19939 = FACE_OUTER_BOUND('',#24253,.T.) ;
#19940 = FACE_OUTER_BOUND('',#24254,.T.) ;
#19941 = FACE_OUTER_BOUND('',#24255,.T.) ;
#19942 = FACE_OUTER_BOUND('',#24256,.T.) ;
#19943 = FACE_OUTER_BOUND('',#24257,.T.) ;
#19944 = FACE_OUTER_BOUND('',#24258,.T.) ;
#19945 = FACE_OUTER_BOUND('',#24259,.T.) ;
#19946 = FACE_OUTER_BOUND('',#24260,.T.) ;
#19947 = FACE_OUTER_BOUND('',#24261,.T.) ;
#19948 = FACE_OUTER_BOUND('',#24262,.T.) ;
#19949 = FACE_OUTER_BOUND('',#24263,.T.) ;
#19950 = FACE_OUTER_BOUND('',#24264,.T.) ;
#19951 = FACE_OUTER_BOUND('',#24265,.T.) ;
#19952 = FACE_OUTER_BOUND('',#24266,.T.) ;
#19953 = FACE_OUTER_BOUND('',#24267,.T.) ;
#19954 = FACE_OUTER_BOUND('',#24268,.T.) ;
#19955 = FACE_OUTER_BOUND('',#24269,.T.) ;
#19956 = FACE_OUTER_BOUND('',#24270,.T.) ;
#19957 = FACE_OUTER_BOUND('',#24271,.T.) ;
#19958 = FACE_OUTER_BOUND('',#24272,.T.) ;
#19959 = FACE_OUTER_BOUND('',#24273,.T.) ;
#19960 = FACE_OUTER_BOUND('',#24274,.T.) ;
#19961 = FACE_OUTER_BOUND('',#24275,.T.) ;
#19962 = FACE_OUTER_BOUND('',#24276,.T.) ;
#19963 = FACE_OUTER_BOUND('',#24277,.T.) ;
#19964 = FACE_OUTER_BOUND('',#24278,.T.) ;
#19965 = FACE_OUTER_BOUND('',#24279,.T.) ;
#19966 = FACE_OUTER_BOUND('',#24280,.T.) ;
#19967 = FACE_OUTER_BOUND('',#24281,.T.) ;
#19968 = FACE_OUTER_BOUND('',#24282,.T.) ;
#19969 = FACE_OUTER_BOUND('',#24283,.T.) ;
#19970 = FACE_OUTER_BOUND('',#24284,.T.) ;
#19971 = FACE_OUTER_BOUND('',#24285,.T.) ;
#19972 = FACE_OUTER_BOUND('',#24286,.T.) ;
#19973 = FACE_OUTER_BOUND('',#24287,.T.) ;
#19974 = FACE_OUTER_BOUND('',#24288,.T.) ;
#19975 = FACE_OUTER_BOUND('',#24289,.T.) ;
#19976 = FACE_OUTER_BOUND('',#24290,.T.) ;
#19977 = FACE_OUTER_BOUND('',#24291,.T.) ;
#19978 = FACE_OUTER_BOUND('',#24292,.T.) ;
#19979 = FACE_OUTER_BOUND('',#24293,.T.) ;
#19980 = FACE_OUTER_BOUND('',#24294,.T.) ;
#19981 = FACE_OUTER_BOUND('',#24295,.T.) ;
#19982 = FACE_OUTER_BOUND('',#24296,.T.) ;
#19983 = FACE_OUTER_BOUND('',#24297,.T.) ;
#19984 = FACE_OUTER_BOUND('',#24298,.T.) ;
#19985 = FACE_OUTER_BOUND('',#24299,.T.) ;
#19986 = FACE_OUTER_BOUND('',#24300,.T.) ;
#19987 = FACE_OUTER_BOUND('',#24301,.T.) ;
#19988 = FACE_OUTER_BOUND('',#24302,.T.) ;
#19989 = FACE_OUTER_BOUND('',#24303,.T.) ;
#19990 = FACE_OUTER_BOUND('',#24304,.T.) ;
#19991 = FACE_OUTER_BOUND('',#24305,.T.) ;
#19992 = FACE_OUTER_BOUND('',#24306,.T.) ;
#19993 = FACE_OUTER_BOUND('',#24307,.T.) ;
#19994 = FACE_OUTER_BOUND('',#24308,.T.) ;
#19995 = FACE_OUTER_BOUND('',#24309,.T.) ;
#19996 = FACE_OUTER_BOUND('',#24310,.T.) ;
#19997 = FACE_OUTER_BOUND('',#24311,.T.) ;
#19998 = FACE_OUTER_BOUND('',#24312,.T.) ;
#19999 = FACE_OUTER_BOUND('',#24313,.T.) ;
#20000 = FACE_OUTER_BOUND('',#24314,.T.) ;
#20001 = FACE_OUTER_BOUND('',#24315,.T.) ;
#20002 = FACE_OUTER_BOUND('',#24316,.T.) ;
#20003 = FACE_OUTER_BOUND('',#24317,.T.) ;
#20004 = FACE_OUTER_BOUND('',#24318,.T.) ;
#20005 = FACE_OUTER_BOUND('',#24319,.T.) ;
#20006 = FACE_OUTER_BOUND('',#24320,.T.) ;
#20007 = FACE_OUTER_BOUND('',#24321,.T.) ;
#20008 = FACE_OUTER_BOUND('',#24322,.T.) ;
#20009 = FACE_OUTER_BOUND('',#24323,.T.) ;
#20010 = FACE_OUTER_BOUND('',#24324,.T.) ;
#20011 = FACE_OUTER_BOUND('',#24325,.T.) ;
#20012 = FACE_OUTER_BOUND('',#24326,.T.) ;
#20013 = FACE_OUTER_BOUND('',#24327,.T.) ;
#20014 = FACE_OUTER_BOUND('',#24328,.T.) ;
#20015 = FACE_OUTER_BOUND('',#24329,.T.) ;
#20016 = FACE_OUTER_BOUND('',#24330,.T.) ;
#20017 = FACE_OUTER_BOUND('',#24331,.T.) ;
#20018 = FACE_OUTER_BOUND('',#24332,.T.) ;
#20019 = FACE_OUTER_BOUND('',#24333,.T.) ;
#20020 = FACE_OUTER_BOUND('',#24334,.T.) ;
#20021 = FACE_OUTER_BOUND('',#24335,.T.) ;
#20022 = FACE_OUTER_BOUND('',#24336,.T.) ;
#20023 = FACE_OUTER_BOUND('',#24337,.T.) ;
#20024 = FACE_OUTER_BOUND('',#24338,.T.) ;
#20025 = FACE_OUTER_BOUND('',#24339,.T.) ;
#20026 = FACE_OUTER_BOUND('',#24340,.T.) ;
#20027 = FACE_OUTER_BOUND('',#24341,.T.) ;
#20028 = FACE_OUTER_BOUND('',#24342,.T.) ;
#20029 = FACE_OUTER_BOUND('',#24343,.T.) ;
#20030 = FACE_OUTER_BOUND('',#24344,.T.) ;
#20031 = FACE_OUTER_BOUND('',#24345,.T.) ;
#20032 = FACE_OUTER_BOUND('',#24346,.T.) ;
#20033 = FACE_OUTER_BOUND('',#24347,.T.) ;
#20034 = FACE_OUTER_BOUND('',#24348,.T.) ;
#20035 = FACE_OUTER_BOUND('',#24349,.T.) ;
#20036 = FACE_OUTER_BOUND('',#24350,.T.) ;
#20037 = FACE_OUTER_BOUND('',#24351,.T.) ;
#20038 = FACE_OUTER_BOUND('',#24352,.T.) ;
#20039 = FACE_OUTER_BOUND('',#24353,.T.) ;
#20040 = FACE_OUTER_BOUND('',#24354,.T.) ;
#20041 = FACE_OUTER_BOUND('',#24355,.T.) ;
#20042 = FACE_OUTER_BOUND('',#24356,.T.) ;
#20043 = FACE_OUTER_BOUND('',#24357,.T.) ;
#20044 = FACE_OUTER_BOUND('',#24358,.T.) ;
#20045 = FACE_OUTER_BOUND('',#24359,.T.) ;
#20046 = FACE_OUTER_BOUND('',#24360,.T.) ;
#20047 = FACE_OUTER_BOUND('',#24361,.T.) ;
#20048 = FACE_OUTER_BOUND('',#24362,.T.) ;
#20049 = FACE_OUTER_BOUND('',#24363,.T.) ;
#20050 = FACE_OUTER_BOUND('',#24364,.T.) ;
#20051 = FACE_OUTER_BOUND('',#24365,.T.) ;
#20052 = FACE_OUTER_BOUND('',#24366,.T.) ;
#20053 = FACE_OUTER_BOUND('',#24367,.T.) ;
#20054 = FACE_OUTER_BOUND('',#24368,.T.) ;
#20055 = FACE_OUTER_BOUND('',#24369,.T.) ;
#20056 = FACE_OUTER_BOUND('',#24370,.T.) ;
#20057 = FACE_OUTER_BOUND('',#24371,.T.) ;
#20058 = FACE_OUTER_BOUND('',#24372,.T.) ;
#20059 = FACE_OUTER_BOUND('',#24373,.T.) ;
#20060 = FACE_OUTER_BOUND('',#24374,.T.) ;
#20061 = FACE_OUTER_BOUND('',#24375,.T.) ;
#20062 = FACE_OUTER_BOUND('',#24376,.T.) ;
#20063 = FACE_OUTER_BOUND('',#24377,.T.) ;
#20064 = FACE_OUTER_BOUND('',#24378,.T.) ;
#20065 = FACE_OUTER_BOUND('',#24379,.T.) ;
#20066 = FACE_OUTER_BOUND('',#24380,.T.) ;
#20067 = FACE_OUTER_BOUND('',#24381,.T.) ;
#20068 = FACE_OUTER_BOUND('',#24382,.T.) ;
#20069 = FACE_OUTER_BOUND('',#24383,.T.) ;
#20070 = FACE_OUTER_BOUND('',#24384,.T.) ;
#20071 = FACE_OUTER_BOUND('',#24385,.T.) ;
#20072 = FACE_OUTER_BOUND('',#24386,.T.) ;
#20073 = FACE_OUTER_BOUND('',#24387,.T.) ;
#20074 = FACE_OUTER_BOUND('',#24388,.T.) ;
#20075 = FACE_OUTER_BOUND('',#24389,.T.) ;
#20076 = FACE_OUTER_BOUND('',#24390,.T.) ;
#20077 = FACE_OUTER_BOUND('',#24391,.T.) ;
#20078 = FACE_OUTER_BOUND('',#24392,.T.) ;
#20079 = FACE_OUTER_BOUND('',#24393,.T.) ;
#20080 = FACE_OUTER_BOUND('',#24394,.T.) ;
#20081 = FACE_OUTER_BOUND('',#24395,.T.) ;
#20082 = FACE_OUTER_BOUND('',#24396,.T.) ;
#20083 = FACE_OUTER_BOUND('',#24397,.T.) ;
#20084 = FACE_OUTER_BOUND('',#24398,.T.) ;
#20085 = FACE_OUTER_BOUND('',#24399,.T.) ;
#20086 = FACE_OUTER_BOUND('',#24400,.T.) ;
#20087 = FACE_OUTER_BOUND('',#24401,.T.) ;
#20088 = FACE_OUTER_BOUND('',#24402,.T.) ;
#20089 = FACE_OUTER_BOUND('',#24403,.T.) ;
#20090 = FACE_OUTER_BOUND('',#24404,.T.) ;
#20091 = FACE_OUTER_BOUND('',#24405,.T.) ;
#20092 = FACE_OUTER_BOUND('',#24406,.T.) ;
#20093 = FACE_OUTER_BOUND('',#24407,.T.) ;
#20094 = FACE_OUTER_BOUND('',#24408,.T.) ;
#20095 = FACE_OUTER_BOUND('',#24409,.T.) ;
#20096 = FACE_OUTER_BOUND('',#24410,.T.) ;
#20097 = FACE_OUTER_BOUND('',#24411,.T.) ;
#20098 = FACE_OUTER_BOUND('',#24412,.T.) ;
#20099 = FACE_OUTER_BOUND('',#24413,.T.) ;
#20100 = FACE_OUTER_BOUND('',#24414,.T.) ;
#20101 = FACE_OUTER_BOUND('',#24415,.T.) ;
#20102 = FACE_OUTER_BOUND('',#24416,.T.) ;
#20103 = FACE_OUTER_BOUND('',#24417,.T.) ;
#20104 = FACE_OUTER_BOUND('',#24418,.T.) ;
#20105 = FACE_OUTER_BOUND('',#24419,.T.) ;
#20106 = FACE_OUTER_BOUND('',#24420,.T.) ;
#20107 = FACE_OUTER_BOUND('',#24421,.T.) ;
#20108 = FACE_OUTER_BOUND('',#24422,.T.) ;
#20109 = FACE_OUTER_BOUND('',#24423,.T.) ;
#20110 = FACE_OUTER_BOUND('',#24424,.T.) ;
#20111 = FACE_OUTER_BOUND('',#24425,.T.) ;
#20112 = FACE_OUTER_BOUND('',#24426,.T.) ;
#20113 = FACE_OUTER_BOUND('',#24427,.T.) ;
#20114 = FACE_OUTER_BOUND('',#24428,.T.) ;
#20115 = FACE_OUTER_BOUND('',#24429,.T.) ;
#20116 = FACE_OUTER_BOUND('',#24430,.T.) ;
#20117 = FACE_OUTER_BOUND('',#24431,.T.) ;
#20118 = FACE_OUTER_BOUND('',#24432,.T.) ;
#20119 = FACE_OUTER_BOUND('',#24433,.T.) ;
#20120 = FACE_OUTER_BOUND('',#24434,.T.) ;
#20121 = FACE_OUTER_BOUND('',#24435,.T.) ;
#20122 = FACE_OUTER_BOUND('',#24436,.T.) ;
#20123 = FACE_OUTER_BOUND('',#24437,.T.) ;
#20124 = FACE_OUTER_BOUND('',#24438,.T.) ;
#20125 = FACE_OUTER_BOUND('',#24439,.T.) ;
#20126 = FACE_OUTER_BOUND('',#24440,.T.) ;
#20127 = FACE_OUTER_BOUND('',#24441,.T.) ;
#20128 = FACE_OUTER_BOUND('',#24442,.T.) ;
#20129 = FACE_OUTER_BOUND('',#24443,.T.) ;
#20130 = FACE_OUTER_BOUND('',#24444,.T.) ;
#20131 = FACE_OUTER_BOUND('',#24445,.T.) ;
#20132 = FACE_OUTER_BOUND('',#24446,.T.) ;
#20133 = FACE_OUTER_BOUND('',#24447,.T.) ;
#20134 = FACE_OUTER_BOUND('',#24448,.T.) ;
#20135 = FACE_OUTER_BOUND('',#24449,.T.) ;
#20136 = FACE_OUTER_BOUND('',#24450,.T.) ;
#20137 = FACE_OUTER_BOUND('',#24451,.T.) ;
#20138 = FACE_OUTER_BOUND('',#24452,.T.) ;
#20139 = FACE_OUTER_BOUND('',#24453,.T.) ;
#20140 = FACE_OUTER_BOUND('',#24454,.T.) ;
#20141 = FACE_OUTER_BOUND('',#24455,.T.) ;
#20142 = FACE_OUTER_BOUND('',#24456,.T.) ;
#20143 = FACE_OUTER_BOUND('',#24457,.T.) ;
#20144 = FACE_OUTER_BOUND('',#24458,.T.) ;
#20145 = FACE_OUTER_BOUND('',#24459,.T.) ;
#20146 = FACE_OUTER_BOUND('',#24460,.T.) ;
#20147 = FACE_OUTER_BOUND('',#24461,.T.) ;
#20148 = FACE_OUTER_BOUND('',#24462,.T.) ;
#20149 = FACE_OUTER_BOUND('',#24463,.T.) ;
#20150 = FACE_OUTER_BOUND('',#24464,.T.) ;
#20151 = FACE_OUTER_BOUND('',#24465,.T.) ;
#20152 = FACE_OUTER_BOUND('',#24466,.T.) ;
#20153 = FACE_OUTER_BOUND('',#24467,.T.) ;
#20154 = FACE_OUTER_BOUND('',#24468,.T.) ;
#20155 = FACE_OUTER_BOUND('',#24469,.T.) ;
#20156 = FACE_OUTER_BOUND('',#24470,.T.) ;
#20157 = FACE_OUTER_BOUND('',#24471,.T.) ;
#20158 = FACE_OUTER_BOUND('',#24472,.T.) ;
#20159 = FACE_OUTER_BOUND('',#24473,.T.) ;
#20160 = FACE_OUTER_BOUND('',#24474,.T.) ;
#20161 = FACE_OUTER_BOUND('',#24475,.T.) ;
#20162 = FACE_OUTER_BOUND('',#24476,.T.) ;
#20163 = FACE_OUTER_BOUND('',#24477,.T.) ;
#20164 = FACE_OUTER_BOUND('',#24478,.T.) ;
#20165 = FACE_OUTER_BOUND('',#24479,.T.) ;
#20166 = FACE_OUTER_BOUND('',#24480,.T.) ;
#20167 = FACE_OUTER_BOUND('',#24481,.T.) ;
#20168 = FACE_OUTER_BOUND('',#24482,.T.) ;
#20169 = FACE_OUTER_BOUND('',#24483,.T.) ;
#20170 = FACE_OUTER_BOUND('',#24484,.T.) ;
#20171 = FACE_OUTER_BOUND('',#24485,.T.) ;
#20172 = FACE_OUTER_BOUND('',#24486,.T.) ;
#20173 = FACE_OUTER_BOUND('',#24487,.T.) ;
#20174 = FACE_OUTER_BOUND('',#24488,.T.) ;
#20175 = FACE_OUTER_BOUND('',#24489,.T.) ;
#20176 = FACE_OUTER_BOUND('',#24490,.T.) ;
#20177 = FACE_OUTER_BOUND('',#24491,.T.) ;
#20178 = FACE_OUTER_BOUND('',#24492,.T.) ;
#20179 = FACE_OUTER_BOUND('',#24493,.T.) ;
#20180 = FACE_OUTER_BOUND('',#24494,.T.) ;
#20181 = FACE_OUTER_BOUND('',#24495,.T.) ;
#20182 = FACE_OUTER_BOUND('',#24496,.T.) ;
#20183 = FACE_OUTER_BOUND('',#24497,.T.) ;
#20184 = FACE_OUTER_BOUND('',#24498,.T.) ;
#20185 = FACE_OUTER_BOUND('',#24499,.T.) ;
#20186 = FACE_OUTER_BOUND('',#24500,.T.) ;
#20187 = FACE_OUTER_BOUND('',#24501,.T.) ;
#20188 = FACE_OUTER_BOUND('',#24502,.T.) ;
#20189 = FACE_OUTER_BOUND('',#24503,.T.) ;
#20190 = FACE_OUTER_BOUND('',#24504,.T.) ;
#20191 = FACE_OUTER_BOUND('',#24505,.T.) ;
#20192 = FACE_OUTER_BOUND('',#24506,.T.) ;
#20193 = FACE_OUTER_BOUND('',#24507,.T.) ;
#20194 = FACE_OUTER_BOUND('',#24508,.T.) ;
#20195 = FACE_OUTER_BOUND('',#24509,.T.) ;
#20196 = FACE_OUTER_BOUND('',#24510,.T.) ;
#20197 = FACE_OUTER_BOUND('',#24511,.T.) ;
#20198 = FACE_OUTER_BOUND('',#24512,.T.) ;
#20199 = FACE_OUTER_BOUND('',#24513,.T.) ;
#20200 = FACE_OUTER_BOUND('',#24514,.T.) ;
#20201 = FACE_OUTER_BOUND('',#24515,.T.) ;
#20202 = FACE_OUTER_BOUND('',#24516,.T.) ;
#20203 = FACE_OUTER_BOUND('',#24517,.T.) ;
#20204 = FACE_OUTER_BOUND('',#24518,.T.) ;
#20205 = FACE_OUTER_BOUND('',#24519,.T.) ;
#20206 = FACE_OUTER_BOUND('',#24520,.T.) ;
#20207 = FACE_OUTER_BOUND('',#24521,.T.) ;
#20208 = FACE_OUTER_BOUND('',#24522,.T.) ;
#20209 = FACE_OUTER_BOUND('',#24523,.T.) ;
#20210 = FACE_OUTER_BOUND('',#24524,.T.) ;
#20211 = FACE_OUTER_BOUND('',#24525,.T.) ;
#20212 = FACE_OUTER_BOUND('',#24526,.T.) ;
#20213 = FACE_OUTER_BOUND('',#24527,.T.) ;
#20214 = FACE_OUTER_BOUND('',#24528,.T.) ;
#20215 = FACE_OUTER_BOUND('',#24529,.T.) ;
#20216 = FACE_OUTER_BOUND('',#24530,.T.) ;
#20217 = FACE_OUTER_BOUND('',#24531,.T.) ;
#20218 = FACE_OUTER_BOUND('',#24532,.T.) ;
#20219 = FACE_OUTER_BOUND('',#24533,.T.) ;
#20220 = FACE_OUTER_BOUND('',#24534,.T.) ;
#20221 = FACE_OUTER_BOUND('',#24535,.T.) ;
#20222 = FACE_OUTER_BOUND('',#24536,.T.) ;
#20223 = FACE_OUTER_BOUND('',#24537,.T.) ;
#20224 = FACE_OUTER_BOUND('',#24538,.T.) ;
#20225 = FACE_OUTER_BOUND('',#24539,.T.) ;
#20226 = FACE_OUTER_BOUND('',#24540,.T.) ;
#20227 = FACE_OUTER_BOUND('',#24541,.T.) ;
#20228 = FACE_OUTER_BOUND('',#24542,.T.) ;
#20229 = FACE_OUTER_BOUND('',#24543,.T.) ;
#20230 = FACE_OUTER_BOUND('',#24544,.T.) ;
#20231 = FACE_OUTER_BOUND('',#24545,.T.) ;
#20232 = FACE_OUTER_BOUND('',#24546,.T.) ;
#20233 = FACE_OUTER_BOUND('',#24547,.T.) ;
#20234 = FACE_OUTER_BOUND('',#24548,.T.) ;
#20235 = FACE_OUTER_BOUND('',#24549,.T.) ;
#20236 = FACE_OUTER_BOUND('',#24550,.T.) ;
#20237 = FACE_OUTER_BOUND('',#24551,.T.) ;
#20238 = FACE_OUTER_BOUND('',#24552,.T.) ;
#20239 = FACE_OUTER_BOUND('',#24553,.T.) ;
#20240 = FACE_OUTER_BOUND('',#24554,.T.) ;
#20241 = FACE_OUTER_BOUND('',#24555,.T.) ;
#20242 = FACE_OUTER_BOUND('',#24556,.T.) ;
#20243 = FACE_OUTER_BOUND('',#24557,.T.) ;
#20244 = FACE_OUTER_BOUND('',#24558,.T.) ;
#20245 = FACE_OUTER_BOUND('',#24559,.T.) ;
#20246 = FACE_OUTER_BOUND('',#24560,.T.) ;
#20247 = FACE_OUTER_BOUND('',#24561,.T.) ;
#20248 = FACE_OUTER_BOUND('',#24562,.T.) ;
#20249 = FACE_OUTER_BOUND('',#24563,.T.) ;
#20250 = FACE_OUTER_BOUND('',#24564,.T.) ;
#20251 = FACE_OUTER_BOUND('',#24565,.T.) ;
#20252 = FACE_OUTER_BOUND('',#24566,.T.) ;
#20253 = FACE_OUTER_BOUND('',#24567,.T.) ;
#20254 = FACE_OUTER_BOUND('',#24568,.T.) ;
#20255 = FACE_OUTER_BOUND('',#24569,.T.) ;
#20256 = FACE_OUTER_BOUND('',#24570,.T.) ;
#20257 = FACE_OUTER_BOUND('',#24571,.T.) ;
#20258 = FACE_OUTER_BOUND('',#24572,.T.) ;
#20259 = FACE_OUTER_BOUND('',#24573,.T.) ;
#20260 = FACE_OUTER_BOUND('',#24574,.T.) ;
#20261 = FACE_OUTER_BOUND('',#24575,.T.) ;
#20262 = FACE_OUTER_BOUND('',#24576,.T.) ;
#20263 = FACE_OUTER_BOUND('',#24577,.T.) ;
#20264 = FACE_OUTER_BOUND('',#24578,.T.) ;
#20265 = FACE_OUTER_BOUND('',#24579,.T.) ;
#20266 = FACE_OUTER_BOUND('',#24580,.T.) ;
#20267 = FACE_OUTER_BOUND('',#24581,.T.) ;
#20268 = FACE_OUTER_BOUND('',#24582,.T.) ;
#20269 = FACE_OUTER_BOUND('',#24583,.T.) ;
#20270 = FACE_OUTER_BOUND('',#24584,.T.) ;
#20271 = FACE_OUTER_BOUND('',#24585,.T.) ;
#20272 = FACE_OUTER_BOUND('',#24586,.T.) ;
#20273 = FACE_OUTER_BOUND('',#24587,.T.) ;
#20274 = FACE_OUTER_BOUND('',#24588,.T.) ;
#20275 = FACE_OUTER_BOUND('',#24589,.T.) ;
#20276 = FACE_OUTER_BOUND('',#24590,.T.) ;
#20277 = FACE_OUTER_BOUND('',#24591,.T.) ;
#20278 = FACE_OUTER_BOUND('',#24592,.T.) ;
#20279 = FACE_OUTER_BOUND('',#24593,.T.) ;
#20280 = FACE_OUTER_BOUND('',#24594,.T.) ;
#20281 = FACE_OUTER_BOUND('',#24595,.T.) ;
#20282 = FACE_OUTER_BOUND('',#24596,.T.) ;
#20283 = FACE_OUTER_BOUND('',#24597,.T.) ;
#20284 = FACE_OUTER_BOUND('',#24598,.T.) ;
#20285 = FACE_OUTER_BOUND('',#24599,.T.) ;
#20286 = FACE_OUTER_BOUND('',#24600,.T.) ;
#20287 = FACE_OUTER_BOUND('',#24601,.T.) ;
#20288 = FACE_OUTER_BOUND('',#24602,.T.) ;
#20289 = FACE_OUTER_BOUND('',#24603,.T.) ;
#20290 = FACE_OUTER_BOUND('',#24604,.T.) ;
#20291 = FACE_OUTER_BOUND('',#24605,.T.) ;
#20292 = FACE_OUTER_BOUND('',#24606,.T.) ;
#20293 = FACE_OUTER_BOUND('',#24607,.T.) ;
#20294 = FACE_OUTER_BOUND('',#24608,.T.) ;
#20295 = FACE_OUTER_BOUND('',#24609,.T.) ;
#20296 = FACE_OUTER_BOUND('',#24610,.T.) ;
#20297 = FACE_OUTER_BOUND('',#24611,.T.) ;
#20298 = FACE_OUTER_BOUND('',#24612,.T.) ;
#20299 = FACE_OUTER_BOUND('',#24613,.T.) ;
#20300 = FACE_OUTER_BOUND('',#24614,.T.) ;
#20301 = FACE_OUTER_BOUND('',#24615,.T.) ;
#20302 = FACE_OUTER_BOUND('',#24616,.T.) ;
#20303 = FACE_OUTER_BOUND('',#24617,.T.) ;
#20304 = FACE_OUTER_BOUND('',#24618,.T.) ;
#20305 = FACE_OUTER_BOUND('',#24619,.T.) ;
#20306 = FACE_OUTER_BOUND('',#24620,.T.) ;
#20307 = FACE_OUTER_BOUND('',#24621,.T.) ;
#20308 = FACE_OUTER_BOUND('',#24622,.T.) ;
#20309 = FACE_OUTER_BOUND('',#24623,.T.) ;
#20310 = FACE_OUTER_BOUND('',#24624,.T.) ;
#20311 = FACE_OUTER_BOUND('',#24625,.T.) ;
#20312 = FACE_OUTER_BOUND('',#24626,.T.) ;
#20313 = FACE_OUTER_BOUND('',#24627,.T.) ;
#20314 = FACE_OUTER_BOUND('',#24628,.T.) ;
#20315 = FACE_OUTER_BOUND('',#24629,.T.) ;
#20316 = FACE_OUTER_BOUND('',#24630,.T.) ;
#20317 = FACE_OUTER_BOUND('',#24631,.T.) ;
#20318 = FACE_OUTER_BOUND('',#24632,.T.) ;
#20319 = FACE_OUTER_BOUND('',#24633,.T.) ;
#20320 = FACE_OUTER_BOUND('',#24634,.T.) ;
#20321 = FACE_OUTER_BOUND('',#24635,.T.) ;
#20322 = FACE_OUTER_BOUND('',#24636,.T.) ;
#20323 = FACE_OUTER_BOUND('',#24637,.T.) ;
#20324 = FACE_OUTER_BOUND('',#24638,.T.) ;
#20325 = FACE_OUTER_BOUND('',#24639,.T.) ;
#20326 = FACE_OUTER_BOUND('',#24640,.T.) ;
#20327 = FACE_OUTER_BOUND('',#24641,.T.) ;
#20328 = FACE_OUTER_BOUND('',#24642,.T.) ;
#20329 = FACE_OUTER_BOUND('',#24643,.T.) ;
#20330 = FACE_OUTER_BOUND('',#24644,.T.) ;
#20331 = FACE_OUTER_BOUND('',#24645,.T.) ;
#20332 = FACE_OUTER_BOUND('',#24646,.T.) ;
#20333 = FACE_OUTER_BOUND('',#24647,.T.) ;
#20334 = FACE_OUTER_BOUND('',#24648,.T.) ;
#20335 = FACE_OUTER_BOUND('',#24649,.T.) ;
#20336 = FACE_OUTER_BOUND('',#24650,.T.) ;
#20337 = FACE_OUTER_BOUND('',#24651,.T.) ;
#20338 = FACE_OUTER_BOUND('',#24652,.T.) ;
#20339 = FACE_OUTER_BOUND('',#24653,.T.) ;
#20340 = FACE_OUTER_BOUND('',#24654,.T.) ;
#20341 = FACE_OUTER_BOUND('',#24655,.T.) ;
#20342 = FACE_OUTER_BOUND('',#24656,.T.) ;
#20343 = FACE_OUTER_BOUND('',#24657,.T.) ;
#20344 = FACE_OUTER_BOUND('',#24658,.T.) ;
#20345 = FACE_OUTER_BOUND('',#24659,.T.) ;
#20346 = FACE_OUTER_BOUND('',#24660,.T.) ;
#20347 = FACE_OUTER_BOUND('',#24661,.T.) ;
#20348 = FACE_OUTER_BOUND('',#24662,.T.) ;
#20349 = FACE_OUTER_BOUND('',#24663,.T.) ;
#20350 = FACE_OUTER_BOUND('',#24664,.T.) ;
#20351 = FACE_OUTER_BOUND('',#24665,.T.) ;
#20352 = FACE_OUTER_BOUND('',#24667,.T.) ;
#20353 = FACE_OUTER_BOUND('',#24669,.T.) ;
#20354 = FACE_OUTER_BOUND('',#24670,.T.) ;
#20355 = FACE_OUTER_BOUND('',#24671,.T.) ;
#20356 = FACE_OUTER_BOUND('',#24672,.T.) ;
#20357 = FACE_OUTER_BOUND('',#24673,.T.) ;
#20358 = FACE_OUTER_BOUND('',#24674,.T.) ;
#20359 = FACE_OUTER_BOUND('',#24675,.T.) ;
#20360 = FACE_OUTER_BOUND('',#24676,.T.) ;
#20361 = FACE_OUTER_BOUND('',#24677,.T.) ;
#20362 = FACE_OUTER_BOUND('',#24678,.T.) ;
#20363 = FACE_OUTER_BOUND('',#24679,.T.) ;
#20364 = FACE_OUTER_BOUND('',#24680,.T.) ;
#20365 = FACE_OUTER_BOUND('',#24681,.T.) ;
#20366 = FACE_OUTER_BOUND('',#24682,.T.) ;
#20367 = FACE_OUTER_BOUND('',#24683,.T.) ;
#20368 = FACE_OUTER_BOUND('',#24684,.T.) ;
#20369 = FACE_OUTER_BOUND('',#24685,.T.) ;
#20370 = FACE_OUTER_BOUND('',#24686,.T.) ;
#20371 = FACE_OUTER_BOUND('',#24687,.T.) ;
#20372 = FACE_OUTER_BOUND('',#24689,.T.) ;
#20373 = FACE_OUTER_BOUND('',#24690,.T.) ;
#20374 = FACE_OUTER_BOUND('',#24691,.T.) ;
#20375 = FACE_OUTER_BOUND('',#24692,.T.) ;
#20376 = FACE_OUTER_BOUND('',#24693,.T.) ;
#20377 = FACE_OUTER_BOUND('',#24694,.T.) ;
#20378 = FACE_OUTER_BOUND('',#24695,.T.) ;
#20379 = FACE_OUTER_BOUND('',#24696,.T.) ;
#20380 = FACE_OUTER_BOUND('',#24697,.T.) ;
#20381 = FACE_OUTER_BOUND('',#24698,.T.) ;
#20382 = FACE_OUTER_BOUND('',#24699,.T.) ;
#20383 = FACE_OUTER_BOUND('',#24700,.T.) ;
#20384 = FACE_OUTER_BOUND('',#24701,.T.) ;
#20385 = FACE_OUTER_BOUND('',#24702,.T.) ;
#20386 = FACE_OUTER_BOUND('',#24703,.T.) ;
#20387 = FACE_OUTER_BOUND('',#24704,.T.) ;
#20388 = FACE_OUTER_BOUND('',#24705,.T.) ;
#20389 = FACE_OUTER_BOUND('',#24706,.T.) ;
#20390 = FACE_OUTER_BOUND('',#24707,.T.) ;
#20391 = FACE_OUTER_BOUND('',#24708,.T.) ;
#20392 = FACE_OUTER_BOUND('',#24710,.T.) ;
#20393 = FACE_OUTER_BOUND('',#24711,.T.) ;
#20394 = FACE_OUTER_BOUND('',#24712,.T.) ;
#20395 = FACE_OUTER_BOUND('',#24713,.T.) ;
#20396 = FACE_OUTER_BOUND('',#24714,.T.) ;
#20397 = FACE_OUTER_BOUND('',#24715,.T.) ;
#20398 = FACE_OUTER_BOUND('',#24716,.T.) ;
#20399 = FACE_OUTER_BOUND('',#24717,.T.) ;
#20400 = FACE_OUTER_BOUND('',#24718,.T.) ;
#20401 = EDGE_LOOP('',(#44066,#44067,#44068,#44069,#44070)) ;
#20402 = EDGE_LOOP('',(#44071,#44072,#44073,#44074,#44075)) ;
#20403 = EDGE_LOOP('',(#44076,#44077,#44078,#44079,#44080,#44081)) ;
#20404 = EDGE_LOOP('',(#44082,#44083,#44084,#44085)) ;
#20405 = EDGE_LOOP('',(#44086,#44087,#44088,#44089,#44090,#44091)) ;
#20406 = EDGE_LOOP('',(#44092,#44093,#44094,#44095)) ;
#20407 = EDGE_LOOP('',(#44096,#44097,#44098,#44099,#44100)) ;
#20408 = EDGE_LOOP('',(#44101,#44102,#44103,#44104,#44105)) ;
#20409 = EDGE_LOOP('',(#44106,#44107,#44108,#44109,#44110)) ;
#20410 = EDGE_LOOP('',(#44111,#44112,#44113,#44114,#44115)) ;
#20411 = EDGE_LOOP('',(#44116,#44117,#44118,#44119,#44120,#44121)) ;
#20412 = EDGE_LOOP('',(#44122,#44123,#44124,#44125,#44126,#44127)) ;
#20413 = EDGE_LOOP('',(#44128,#44129,#44130,#44131,#44132,#44133,#44134,#44135)) ;
#20414 = EDGE_LOOP('',(#44136)) ;
#20415 = EDGE_LOOP('',(#44137,#44138,#44139,#44140,#44141,#44142)) ;
#20416 = EDGE_LOOP('',(#44143,#44144,#44145,#44146,#44147,#44148,#44149,#44150)) ;
#20417 = EDGE_LOOP('',(#44151)) ;
#20418 = EDGE_LOOP('',(#44152,#44153,#44154,#44155,#44156,#44157,#44158,#44159,
#44160,#44161,#44162)) ;
#20419 = EDGE_LOOP('',(#44163,#44164,#44165,#44166,#44167,#44168,#44169,#44170)) ;
#20420 = EDGE_LOOP('',(#44171,#44172,#44173,#44174,#44175,#44176,#44177,#44178)) ;
#20421 = EDGE_LOOP('',(#44179,#44180,#44181,#44182,#44183,#44184,#44185,#44186)) ;
#20422 = EDGE_LOOP('',(#44187,#44188,#44189,#44190,#44191,#44192,#44193,#44194)) ;
#20423 = EDGE_LOOP('',(#44195,#44196,#44197,#44198,#44199,#44200,#44201,#44202,
#44203,#44204,#44205)) ;
#20424 = EDGE_LOOP('',(#44206,#44207,#44208,#44209,#44210,#44211,#44212,#44213)) ;
#20425 = EDGE_LOOP('',(#44214,#44215,#44216,#44217,#44218,#44219,#44220,#44221)) ;
#20426 = EDGE_LOOP('',(#44222,#44223,#44224,#44225,#44226,#44227,#44228,#44229)) ;
#20427 = EDGE_LOOP('',(#44230,#44231,#44232,#44233,#44234,#44235,#44236,#44237)) ;
#20428 = EDGE_LOOP('',(#44238,#44239,#44240,#44241,#44242,#44243,#44244,#44245,
#44246,#44247,#44248)) ;
#20429 = EDGE_LOOP('',(#44249,#44250,#44251,#44252,#44253,#44254,#44255,#44256)) ;
#20430 = EDGE_LOOP('',(#44257,#44258,#44259,#44260,#44261,#44262,#44263,#44264)) ;
#20431 = EDGE_LOOP('',(#44265,#44266,#44267,#44268,#44269,#44270,#44271,#44272)) ;
#20432 = EDGE_LOOP('',(#44273,#44274,#44275,#44276,#44277,#44278,#44279,#44280)) ;
#20433 = EDGE_LOOP('',(#44281,#44282,#44283,#44284,#44285,#44286,#44287,#44288)) ;
#20434 = EDGE_LOOP('',(#44289,#44290,#44291,#44292,#44293,#44294,#44295,#44296)) ;
#20435 = EDGE_LOOP('',(#44297,#44298,#44299,#44300,#44301,#44302,#44303,#44304)) ;
#20436 = EDGE_LOOP('',(#44305,#44306,#44307,#44308,#44309,#44310,#44311,#44312,
#44313,#44314,#44315)) ;
#20437 = EDGE_LOOP('',(#44316,#44317,#44318,#44319,#44320,#44321,#44322,#44323)) ;
#20438 = EDGE_LOOP('',(#44324,#44325,#44326,#44327,#44328,#44329,#44330,#44331)) ;
#20439 = EDGE_LOOP('',(#44332,#44333,#44334,#44335,#44336,#44337,#44338,#44339)) ;
#20440 = EDGE_LOOP('',(#44340,#44341,#44342,#44343,#44344,#44345,#44346,#44347)) ;
#20441 = EDGE_LOOP('',(#44348,#44349,#44350,#44351,#44352,#44353,#44354,#44355)) ;
#20442 = EDGE_LOOP('',(#44356,#44357,#44358,#44359,#44360,#44361,#44362,#44363)) ;
#20443 = EDGE_LOOP('',(#44364,#44365,#44366,#44367,#44368,#44369,#44370,#44371)) ;
#20444 = EDGE_LOOP('',(#44372,#44373,#44374,#44375,#44376,#44377,#44378,#44379,
#44380,#44381)) ;
#20445 = EDGE_LOOP('',(#44382)) ;
#20446 = EDGE_LOOP('',(#44383)) ;
#20447 = EDGE_LOOP('',(#44384,#44385,#44386,#44387,#44388,#44389,#44390,#44391,
#44392,#44393)) ;
#20448 = EDGE_LOOP('',(#44394)) ;
#20449 = EDGE_LOOP('',(#44395)) ;
#20450 = EDGE_LOOP('',(#44396,#44397,#44398,#44399)) ;
#20451 = EDGE_LOOP('',(#44400,#44401,#44402,#44403)) ;
#20452 = EDGE_LOOP('',(#44404,#44405,#44406,#44407)) ;
#20453 = EDGE_LOOP('',(#44408,#44409,#44410,#44411)) ;
#20454 = EDGE_LOOP('',(#44412,#44413,#44414,#44415)) ;
#20455 = EDGE_LOOP('',(#44416,#44417,#44418,#44419)) ;
#20456 = EDGE_LOOP('',(#44420,#44421,#44422,#44423)) ;
#20457 = EDGE_LOOP('',(#44424,#44425,#44426,#44427)) ;
#20458 = EDGE_LOOP('',(#44428,#44429,#44430,#44431)) ;
#20459 = EDGE_LOOP('',(#44432,#44433,#44434,#44435)) ;
#20460 = EDGE_LOOP('',(#44436,#44437,#44438,#44439)) ;
#20461 = EDGE_LOOP('',(#44440,#44441,#44442,#44443)) ;
#20462 = EDGE_LOOP('',(#44444,#44445,#44446,#44447)) ;
#20463 = EDGE_LOOP('',(#44448,#44449,#44450,#44451)) ;
#20464 = EDGE_LOOP('',(#44452,#44453,#44454,#44455)) ;
#20465 = EDGE_LOOP('',(#44456,#44457,#44458,#44459)) ;
#20466 = EDGE_LOOP('',(#44460,#44461,#44462,#44463)) ;
#20467 = EDGE_LOOP('',(#44464,#44465,#44466,#44467)) ;
#20468 = EDGE_LOOP('',(#44468,#44469,#44470,#44471)) ;
#20469 = EDGE_LOOP('',(#44472,#44473,#44474,#44475)) ;
#20470 = EDGE_LOOP('',(#44476,#44477,#44478,#44479)) ;
#20471 = EDGE_LOOP('',(#44480,#44481,#44482,#44483)) ;
#20472 = EDGE_LOOP('',(#44484,#44485,#44486,#44487)) ;
#20473 = EDGE_LOOP('',(#44488,#44489,#44490,#44491)) ;
#20474 = EDGE_LOOP('',(#44492,#44493,#44494,#44495)) ;
#20475 = EDGE_LOOP('',(#44496,#44497,#44498,#44499)) ;
#20476 = EDGE_LOOP('',(#44500,#44501,#44502,#44503)) ;
#20477 = EDGE_LOOP('',(#44504,#44505,#44506,#44507)) ;
#20478 = EDGE_LOOP('',(#44508,#44509,#44510,#44511)) ;
#20479 = EDGE_LOOP('',(#44512,#44513,#44514,#44515)) ;
#20480 = EDGE_LOOP('',(#44516,#44517,#44518,#44519)) ;
#20481 = EDGE_LOOP('',(#44520,#44521,#44522,#44523)) ;
#20482 = EDGE_LOOP('',(#44524,#44525,#44526,#44527)) ;
#20483 = EDGE_LOOP('',(#44528,#44529,#44530,#44531)) ;
#20484 = EDGE_LOOP('',(#44532,#44533,#44534,#44535)) ;
#20485 = EDGE_LOOP('',(#44536,#44537,#44538,#44539)) ;
#20486 = EDGE_LOOP('',(#44540,#44541,#44542,#44543)) ;
#20487 = EDGE_LOOP('',(#44544,#44545,#44546,#44547)) ;
#20488 = EDGE_LOOP('',(#44548,#44549,#44550,#44551)) ;
#20489 = EDGE_LOOP('',(#44552,#44553,#44554,#44555)) ;
#20490 = EDGE_LOOP('',(#44556,#44557,#44558,#44559)) ;
#20491 = EDGE_LOOP('',(#44560,#44561,#44562,#44563)) ;
#20492 = EDGE_LOOP('',(#44564,#44565,#44566,#44567)) ;
#20493 = EDGE_LOOP('',(#44568,#44569,#44570,#44571)) ;
#20494 = EDGE_LOOP('',(#44572,#44573,#44574,#44575)) ;
#20495 = EDGE_LOOP('',(#44576,#44577,#44578,#44579)) ;
#20496 = EDGE_LOOP('',(#44580,#44581,#44582,#44583)) ;
#20497 = EDGE_LOOP('',(#44584,#44585,#44586,#44587)) ;
#20498 = EDGE_LOOP('',(#44588,#44589,#44590,#44591)) ;
#20499 = EDGE_LOOP('',(#44592,#44593,#44594,#44595)) ;
#20500 = EDGE_LOOP('',(#44596,#44597,#44598,#44599)) ;
#20501 = EDGE_LOOP('',(#44600,#44601,#44602,#44603)) ;
#20502 = EDGE_LOOP('',(#44604,#44605,#44606,#44607)) ;
#20503 = EDGE_LOOP('',(#44608,#44609,#44610,#44611)) ;
#20504 = EDGE_LOOP('',(#44612,#44613,#44614,#44615)) ;
#20505 = EDGE_LOOP('',(#44616,#44617,#44618,#44619)) ;
#20506 = EDGE_LOOP('',(#44620,#44621,#44622,#44623)) ;
#20507 = EDGE_LOOP('',(#44624,#44625,#44626,#44627)) ;
#20508 = EDGE_LOOP('',(#44628,#44629,#44630,#44631)) ;
#20509 = EDGE_LOOP('',(#44632,#44633,#44634,#44635)) ;
#20510 = EDGE_LOOP('',(#44636,#44637,#44638,#44639)) ;
#20511 = EDGE_LOOP('',(#44640,#44641,#44642,#44643)) ;
#20512 = EDGE_LOOP('',(#44644,#44645,#44646,#44647)) ;
#20513 = EDGE_LOOP('',(#44648,#44649,#44650,#44651)) ;
#20514 = EDGE_LOOP('',(#44652,#44653,#44654,#44655)) ;
#20515 = EDGE_LOOP('',(#44656,#44657,#44658,#44659)) ;
#20516 = EDGE_LOOP('',(#44660,#44661,#44662,#44663)) ;
#20517 = EDGE_LOOP('',(#44664,#44665,#44666,#44667)) ;
#20518 = EDGE_LOOP('',(#44668,#44669,#44670,#44671)) ;
#20519 = EDGE_LOOP('',(#44672,#44673,#44674,#44675)) ;
#20520 = EDGE_LOOP('',(#44676,#44677,#44678,#44679)) ;
#20521 = EDGE_LOOP('',(#44680,#44681,#44682,#44683)) ;
#20522 = EDGE_LOOP('',(#44684,#44685,#44686,#44687)) ;
#20523 = EDGE_LOOP('',(#44688,#44689,#44690,#44691)) ;
#20524 = EDGE_LOOP('',(#44692,#44693,#44694,#44695)) ;
#20525 = EDGE_LOOP('',(#44696,#44697,#44698,#44699)) ;
#20526 = EDGE_LOOP('',(#44700,#44701,#44702,#44703)) ;
#20527 = EDGE_LOOP('',(#44704,#44705,#44706,#44707)) ;
#20528 = EDGE_LOOP('',(#44708,#44709,#44710,#44711)) ;
#20529 = EDGE_LOOP('',(#44712,#44713,#44714,#44715)) ;
#20530 = EDGE_LOOP('',(#44716,#44717,#44718,#44719)) ;
#20531 = EDGE_LOOP('',(#44720,#44721,#44722,#44723)) ;
#20532 = EDGE_LOOP('',(#44724,#44725,#44726,#44727)) ;
#20533 = EDGE_LOOP('',(#44728,#44729,#44730,#44731)) ;
#20534 = EDGE_LOOP('',(#44732,#44733,#44734,#44735)) ;
#20535 = EDGE_LOOP('',(#44736,#44737,#44738,#44739)) ;
#20536 = EDGE_LOOP('',(#44740,#44741,#44742,#44743)) ;
#20537 = EDGE_LOOP('',(#44744,#44745,#44746,#44747)) ;
#20538 = EDGE_LOOP('',(#44748,#44749,#44750)) ;
#20539 = EDGE_LOOP('',(#44751,#44752,#44753,#44754)) ;
#20540 = EDGE_LOOP('',(#44755,#44756,#44757,#44758)) ;
#20541 = EDGE_LOOP('',(#44759,#44760,#44761,#44762)) ;
#20542 = EDGE_LOOP('',(#44763,#44764,#44765)) ;
#20543 = EDGE_LOOP('',(#44766,#44767,#44768)) ;
#20544 = EDGE_LOOP('',(#44769,#44770,#44771,#44772)) ;
#20545 = EDGE_LOOP('',(#44773,#44774,#44775,#44776)) ;
#20546 = EDGE_LOOP('',(#44777,#44778,#44779,#44780)) ;
#20547 = EDGE_LOOP('',(#44781,#44782,#44783)) ;
#20548 = EDGE_LOOP('',(#44784,#44785,#44786,#44787)) ;
#20549 = EDGE_LOOP('',(#44788,#44789,#44790,#44791)) ;
#20550 = EDGE_LOOP('',(#44792,#44793,#44794,#44795)) ;
#20551 = EDGE_LOOP('',(#44796,#44797,#44798,#44799)) ;
#20552 = EDGE_LOOP('',(#44800,#44801,#44802,#44803)) ;
#20553 = EDGE_LOOP('',(#44804,#44805,#44806)) ;
#20554 = EDGE_LOOP('',(#44807,#44808,#44809,#44810)) ;
#20555 = EDGE_LOOP('',(#44811,#44812,#44813,#44814)) ;
#20556 = EDGE_LOOP('',(#44815,#44816,#44817,#44818)) ;
#20557 = EDGE_LOOP('',(#44819,#44820,#44821)) ;
#20558 = EDGE_LOOP('',(#44822,#44823,#44824)) ;
#20559 = EDGE_LOOP('',(#44825,#44826,#44827,#44828)) ;
#20560 = EDGE_LOOP('',(#44829,#44830,#44831,#44832)) ;
#20561 = EDGE_LOOP('',(#44833,#44834,#44835,#44836)) ;
#20562 = EDGE_LOOP('',(#44837,#44838,#44839,#44840)) ;
#20563 = EDGE_LOOP('',(#44841,#44842,#44843)) ;
#20564 = EDGE_LOOP('',(#44844,#44845,#44846,#44847)) ;
#20565 = EDGE_LOOP('',(#44848,#44849,#44850)) ;
#20566 = EDGE_LOOP('',(#44851,#44852,#44853,#44854)) ;
#20567 = EDGE_LOOP('',(#44855,#44856,#44857,#44858)) ;
#20568 = EDGE_LOOP('',(#44859,#44860,#44861,#44862)) ;
#20569 = EDGE_LOOP('',(#44863,#44864,#44865,#44866)) ;
#20570 = EDGE_LOOP('',(#44867,#44868,#44869,#44870)) ;
#20571 = EDGE_LOOP('',(#44871,#44872,#44873,#44874)) ;
#20572 = EDGE_LOOP('',(#44875,#44876,#44877,#44878)) ;
#20573 = EDGE_LOOP('',(#44879,#44880,#44881,#44882)) ;
#20574 = EDGE_LOOP('',(#44883,#44884,#44885,#44886)) ;
#20575 = EDGE_LOOP('',(#44887,#44888,#44889)) ;
#20576 = EDGE_LOOP('',(#44890,#44891,#44892)) ;
#20577 = EDGE_LOOP('',(#44893,#44894,#44895,#44896)) ;
#20578 = EDGE_LOOP('',(#44897,#44898,#44899,#44900)) ;
#20579 = EDGE_LOOP('',(#44901,#44902,#44903,#44904)) ;
#20580 = EDGE_LOOP('',(#44905,#44906,#44907,#44908)) ;
#20581 = EDGE_LOOP('',(#44909,#44910,#44911,#44912)) ;
#20582 = EDGE_LOOP('',(#44913,#44914,#44915,#44916)) ;
#20583 = EDGE_LOOP('',(#44917,#44918,#44919,#44920)) ;
#20584 = EDGE_LOOP('',(#44921,#44922,#44923,#44924)) ;
#20585 = EDGE_LOOP('',(#44925,#44926,#44927)) ;
#20586 = EDGE_LOOP('',(#44928,#44929,#44930,#44931)) ;
#20587 = EDGE_LOOP('',(#44932,#44933,#44934,#44935)) ;
#20588 = EDGE_LOOP('',(#44936,#44937,#44938,#44939)) ;
#20589 = EDGE_LOOP('',(#44940,#44941,#44942,#44943)) ;
#20590 = EDGE_LOOP('',(#44944,#44945,#44946,#44947)) ;
#20591 = EDGE_LOOP('',(#44948,#44949,#44950,#44951)) ;
#20592 = EDGE_LOOP('',(#44952,#44953,#44954,#44955)) ;
#20593 = EDGE_LOOP('',(#44956,#44957,#44958)) ;
#20594 = EDGE_LOOP('',(#44959,#44960,#44961)) ;
#20595 = EDGE_LOOP('',(#44962,#44963,#44964,#44965)) ;
#20596 = EDGE_LOOP('',(#44966,#44967,#44968,#44969)) ;
#20597 = EDGE_LOOP('',(#44970,#44971,#44972,#44973)) ;
#20598 = EDGE_LOOP('',(#44974,#44975,#44976,#44977)) ;
#20599 = EDGE_LOOP('',(#44978,#44979,#44980,#44981)) ;
#20600 = EDGE_LOOP('',(#44982,#44983,#44984,#44985)) ;
#20601 = EDGE_LOOP('',(#44986,#44987,#44988,#44989)) ;
#20602 = EDGE_LOOP('',(#44990,#44991,#44992)) ;
#20603 = EDGE_LOOP('',(#44993,#44994,#44995)) ;
#20604 = EDGE_LOOP('',(#44996,#44997,#44998,#44999)) ;
#20605 = EDGE_LOOP('',(#45000,#45001,#45002)) ;
#20606 = EDGE_LOOP('',(#45003,#45004,#45005)) ;
#20607 = EDGE_LOOP('',(#45006,#45007,#45008,#45009)) ;
#20608 = EDGE_LOOP('',(#45010,#45011,#45012,#45013)) ;
#20609 = EDGE_LOOP('',(#45014,#45015,#45016,#45017)) ;
#20610 = EDGE_LOOP('',(#45018,#45019,#45020,#45021)) ;
#20611 = EDGE_LOOP('',(#45022,#45023,#45024,#45025)) ;
#20612 = EDGE_LOOP('',(#45026,#45027,#45028,#45029)) ;
#20613 = EDGE_LOOP('',(#45030,#45031,#45032,#45033)) ;
#20614 = EDGE_LOOP('',(#45034,#45035,#45036,#45037)) ;
#20615 = EDGE_LOOP('',(#45038,#45039,#45040)) ;
#20616 = EDGE_LOOP('',(#45041,#45042,#45043,#45044)) ;
#20617 = EDGE_LOOP('',(#45045,#45046,#45047,#45048)) ;
#20618 = EDGE_LOOP('',(#45049,#45050,#45051)) ;
#20619 = EDGE_LOOP('',(#45052,#45053,#45054,#45055)) ;
#20620 = EDGE_LOOP('',(#45056,#45057,#45058,#45059)) ;
#20621 = EDGE_LOOP('',(#45060,#45061,#45062,#45063)) ;
#20622 = EDGE_LOOP('',(#45064,#45065,#45066,#45067)) ;
#20623 = EDGE_LOOP('',(#45068,#45069,#45070,#45071)) ;
#20624 = EDGE_LOOP('',(#45072,#45073,#45074,#45075)) ;
#20625 = EDGE_LOOP('',(#45076,#45077,#45078,#45079)) ;
#20626 = EDGE_LOOP('',(#45080,#45081,#45082,#45083)) ;
#20627 = EDGE_LOOP('',(#45084,#45085,#45086,#45087)) ;
#20628 = EDGE_LOOP('',(#45088,#45089,#45090,#45091)) ;
#20629 = EDGE_LOOP('',(#45092,#45093,#45094,#45095)) ;
#20630 = EDGE_LOOP('',(#45096,#45097,#45098,#45099)) ;
#20631 = EDGE_LOOP('',(#45100,#45101,#45102,#45103)) ;
#20632 = EDGE_LOOP('',(#45104,#45105,#45106,#45107)) ;
#20633 = EDGE_LOOP('',(#45108,#45109,#45110,#45111)) ;
#20634 = EDGE_LOOP('',(#45112,#45113,#45114,#45115)) ;
#20635 = EDGE_LOOP('',(#45116,#45117,#45118,#45119)) ;
#20636 = EDGE_LOOP('',(#45120,#45121,#45122,#45123)) ;
#20637 = EDGE_LOOP('',(#45124,#45125,#45126,#45127)) ;
#20638 = EDGE_LOOP('',(#45128,#45129,#45130,#45131)) ;
#20639 = EDGE_LOOP('',(#45132,#45133,#45134,#45135)) ;
#20640 = EDGE_LOOP('',(#45136,#45137,#45138,#45139)) ;
#20641 = EDGE_LOOP('',(#45140,#45141,#45142,#45143)) ;
#20642 = EDGE_LOOP('',(#45144,#45145,#45146,#45147)) ;
#20643 = EDGE_LOOP('',(#45148,#45149,#45150,#45151)) ;
#20644 = EDGE_LOOP('',(#45152,#45153,#45154,#45155)) ;
#20645 = EDGE_LOOP('',(#45156,#45157,#45158,#45159)) ;
#20646 = EDGE_LOOP('',(#45160,#45161,#45162,#45163)) ;
#20647 = EDGE_LOOP('',(#45164,#45165,#45166,#45167)) ;
#20648 = EDGE_LOOP('',(#45168,#45169,#45170,#45171)) ;
#20649 = EDGE_LOOP('',(#45172,#45173,#45174,#45175)) ;
#20650 = EDGE_LOOP('',(#45176,#45177,#45178,#45179)) ;
#20651 = EDGE_LOOP('',(#45180,#45181,#45182,#45183)) ;
#20652 = EDGE_LOOP('',(#45184,#45185,#45186,#45187)) ;
#20653 = EDGE_LOOP('',(#45188,#45189,#45190,#45191)) ;
#20654 = EDGE_LOOP('',(#45192,#45193,#45194,#45195)) ;
#20655 = EDGE_LOOP('',(#45196,#45197,#45198,#45199)) ;
#20656 = EDGE_LOOP('',(#45200,#45201,#45202,#45203)) ;
#20657 = EDGE_LOOP('',(#45204,#45205,#45206,#45207)) ;
#20658 = EDGE_LOOP('',(#45208,#45209,#45210,#45211)) ;
#20659 = EDGE_LOOP('',(#45212,#45213,#45214,#45215)) ;
#20660 = EDGE_LOOP('',(#45216,#45217,#45218,#45219)) ;
#20661 = EDGE_LOOP('',(#45220,#45221,#45222,#45223)) ;
#20662 = EDGE_LOOP('',(#45224,#45225,#45226,#45227)) ;
#20663 = EDGE_LOOP('',(#45228,#45229,#45230,#45231)) ;
#20664 = EDGE_LOOP('',(#45232,#45233,#45234,#45235)) ;
#20665 = EDGE_LOOP('',(#45236,#45237,#45238,#45239)) ;
#20666 = EDGE_LOOP('',(#45240,#45241,#45242,#45243)) ;
#20667 = EDGE_LOOP('',(#45244,#45245,#45246,#45247)) ;
#20668 = EDGE_LOOP('',(#45248,#45249,#45250,#45251)) ;
#20669 = EDGE_LOOP('',(#45252,#45253,#45254,#45255)) ;
#20670 = EDGE_LOOP('',(#45256,#45257,#45258,#45259)) ;
#20671 = EDGE_LOOP('',(#45260,#45261,#45262,#45263)) ;
#20672 = EDGE_LOOP('',(#45264,#45265,#45266,#45267)) ;
#20673 = EDGE_LOOP('',(#45268,#45269,#45270,#45271)) ;
#20674 = EDGE_LOOP('',(#45272,#45273,#45274,#45275)) ;
#20675 = EDGE_LOOP('',(#45276,#45277,#45278,#45279)) ;
#20676 = EDGE_LOOP('',(#45280,#45281,#45282,#45283)) ;
#20677 = EDGE_LOOP('',(#45284,#45285,#45286,#45287)) ;
#20678 = EDGE_LOOP('',(#45288,#45289,#45290,#45291)) ;
#20679 = EDGE_LOOP('',(#45292,#45293,#45294,#45295)) ;
#20680 = EDGE_LOOP('',(#45296,#45297,#45298,#45299)) ;
#20681 = EDGE_LOOP('',(#45300,#45301,#45302,#45303)) ;
#20682 = EDGE_LOOP('',(#45304,#45305,#45306,#45307)) ;
#20683 = EDGE_LOOP('',(#45308,#45309,#45310,#45311)) ;
#20684 = EDGE_LOOP('',(#45312,#45313,#45314,#45315)) ;
#20685 = EDGE_LOOP('',(#45316,#45317,#45318,#45319)) ;
#20686 = EDGE_LOOP('',(#45320,#45321,#45322,#45323)) ;
#20687 = EDGE_LOOP('',(#45324,#45325,#45326,#45327)) ;
#20688 = EDGE_LOOP('',(#45328,#45329,#45330,#45331)) ;
#20689 = EDGE_LOOP('',(#45332,#45333,#45334,#45335)) ;
#20690 = EDGE_LOOP('',(#45336,#45337,#45338,#45339)) ;
#20691 = EDGE_LOOP('',(#45340,#45341,#45342,#45343)) ;
#20692 = EDGE_LOOP('',(#45344,#45345,#45346,#45347)) ;
#20693 = EDGE_LOOP('',(#45348,#45349,#45350,#45351)) ;
#20694 = EDGE_LOOP('',(#45352,#45353,#45354,#45355)) ;
#20695 = EDGE_LOOP('',(#45356,#45357,#45358,#45359)) ;
#20696 = EDGE_LOOP('',(#45360,#45361,#45362,#45363)) ;
#20697 = EDGE_LOOP('',(#45364,#45365,#45366,#45367)) ;
#20698 = EDGE_LOOP('',(#45368,#45369,#45370,#45371)) ;
#20699 = EDGE_LOOP('',(#45372,#45373,#45374,#45375)) ;
#20700 = EDGE_LOOP('',(#45376,#45377,#45378,#45379)) ;
#20701 = EDGE_LOOP('',(#45380,#45381,#45382,#45383)) ;
#20702 = EDGE_LOOP('',(#45384,#45385,#45386,#45387)) ;
#20703 = EDGE_LOOP('',(#45388,#45389,#45390,#45391)) ;
#20704 = EDGE_LOOP('',(#45392,#45393,#45394,#45395)) ;
#20705 = EDGE_LOOP('',(#45396,#45397,#45398,#45399)) ;
#20706 = EDGE_LOOP('',(#45400,#45401,#45402,#45403)) ;
#20707 = EDGE_LOOP('',(#45404,#45405,#45406,#45407)) ;
#20708 = EDGE_LOOP('',(#45408,#45409,#45410,#45411)) ;
#20709 = EDGE_LOOP('',(#45412,#45413,#45414,#45415)) ;
#20710 = EDGE_LOOP('',(#45416,#45417,#45418,#45419)) ;
#20711 = EDGE_LOOP('',(#45420,#45421,#45422,#45423)) ;
#20712 = EDGE_LOOP('',(#45424,#45425,#45426,#45427)) ;
#20713 = EDGE_LOOP('',(#45428,#45429,#45430,#45431)) ;
#20714 = EDGE_LOOP('',(#45432,#45433,#45434,#45435)) ;
#20715 = EDGE_LOOP('',(#45436,#45437,#45438,#45439)) ;
#20716 = EDGE_LOOP('',(#45440,#45441,#45442,#45443)) ;
#20717 = EDGE_LOOP('',(#45444,#45445,#45446,#45447)) ;
#20718 = EDGE_LOOP('',(#45448,#45449,#45450,#45451)) ;
#20719 = EDGE_LOOP('',(#45452,#45453,#45454,#45455)) ;
#20720 = EDGE_LOOP('',(#45456,#45457,#45458,#45459)) ;
#20721 = EDGE_LOOP('',(#45460,#45461,#45462,#45463)) ;
#20722 = EDGE_LOOP('',(#45464,#45465,#45466,#45467)) ;
#20723 = EDGE_LOOP('',(#45468,#45469,#45470,#45471)) ;
#20724 = EDGE_LOOP('',(#45472,#45473,#45474,#45475)) ;
#20725 = EDGE_LOOP('',(#45476,#45477,#45478,#45479)) ;
#20726 = EDGE_LOOP('',(#45480,#45481,#45482,#45483)) ;
#20727 = EDGE_LOOP('',(#45484,#45485,#45486,#45487)) ;
#20728 = EDGE_LOOP('',(#45488,#45489,#45490,#45491)) ;
#20729 = EDGE_LOOP('',(#45492,#45493,#45494,#45495)) ;
#20730 = EDGE_LOOP('',(#45496,#45497,#45498,#45499)) ;
#20731 = EDGE_LOOP('',(#45500,#45501,#45502,#45503)) ;
#20732 = EDGE_LOOP('',(#45504,#45505,#45506,#45507)) ;
#20733 = EDGE_LOOP('',(#45508,#45509,#45510,#45511)) ;
#20734 = EDGE_LOOP('',(#45512,#45513,#45514,#45515)) ;
#20735 = EDGE_LOOP('',(#45516,#45517,#45518,#45519)) ;
#20736 = EDGE_LOOP('',(#45520,#45521,#45522,#45523)) ;
#20737 = EDGE_LOOP('',(#45524,#45525,#45526,#45527)) ;
#20738 = EDGE_LOOP('',(#45528,#45529,#45530,#45531)) ;
#20739 = EDGE_LOOP('',(#45532,#45533,#45534,#45535)) ;
#20740 = EDGE_LOOP('',(#45536,#45537,#45538,#45539)) ;
#20741 = EDGE_LOOP('',(#45540,#45541,#45542,#45543)) ;
#20742 = EDGE_LOOP('',(#45544,#45545,#45546,#45547)) ;
#20743 = EDGE_LOOP('',(#45548,#45549,#45550,#45551)) ;
#20744 = EDGE_LOOP('',(#45552,#45553,#45554,#45555)) ;
#20745 = EDGE_LOOP('',(#45556,#45557,#45558,#45559)) ;
#20746 = EDGE_LOOP('',(#45560,#45561,#45562,#45563)) ;
#20747 = EDGE_LOOP('',(#45564,#45565,#45566,#45567)) ;
#20748 = EDGE_LOOP('',(#45568,#45569,#45570,#45571)) ;
#20749 = EDGE_LOOP('',(#45572,#45573,#45574,#45575)) ;
#20750 = EDGE_LOOP('',(#45576,#45577,#45578,#45579)) ;
#20751 = EDGE_LOOP('',(#45580,#45581,#45582,#45583)) ;
#20752 = EDGE_LOOP('',(#45584,#45585,#45586,#45587)) ;
#20753 = EDGE_LOOP('',(#45588,#45589,#45590,#45591)) ;
#20754 = EDGE_LOOP('',(#45592,#45593,#45594,#45595)) ;
#20755 = EDGE_LOOP('',(#45596,#45597,#45598,#45599)) ;
#20756 = EDGE_LOOP('',(#45600,#45601,#45602,#45603)) ;
#20757 = EDGE_LOOP('',(#45604,#45605,#45606,#45607)) ;
#20758 = EDGE_LOOP('',(#45608,#45609,#45610,#45611)) ;
#20759 = EDGE_LOOP('',(#45612,#45613,#45614,#45615)) ;
#20760 = EDGE_LOOP('',(#45616,#45617,#45618,#45619)) ;
#20761 = EDGE_LOOP('',(#45620,#45621,#45622,#45623)) ;
#20762 = EDGE_LOOP('',(#45624,#45625,#45626,#45627)) ;
#20763 = EDGE_LOOP('',(#45628,#45629,#45630,#45631)) ;
#20764 = EDGE_LOOP('',(#45632,#45633,#45634,#45635)) ;
#20765 = EDGE_LOOP('',(#45636,#45637,#45638,#45639)) ;
#20766 = EDGE_LOOP('',(#45640,#45641,#45642,#45643)) ;
#20767 = EDGE_LOOP('',(#45644,#45645,#45646,#45647)) ;
#20768 = EDGE_LOOP('',(#45648,#45649,#45650,#45651)) ;
#20769 = EDGE_LOOP('',(#45652,#45653,#45654,#45655)) ;
#20770 = EDGE_LOOP('',(#45656,#45657,#45658,#45659)) ;
#20771 = EDGE_LOOP('',(#45660,#45661,#45662,#45663)) ;
#20772 = EDGE_LOOP('',(#45664,#45665,#45666,#45667)) ;
#20773 = EDGE_LOOP('',(#45668,#45669,#45670,#45671)) ;
#20774 = EDGE_LOOP('',(#45672,#45673,#45674,#45675)) ;
#20775 = EDGE_LOOP('',(#45676,#45677,#45678,#45679)) ;
#20776 = EDGE_LOOP('',(#45680,#45681,#45682,#45683)) ;
#20777 = EDGE_LOOP('',(#45684,#45685,#45686,#45687)) ;
#20778 = EDGE_LOOP('',(#45688,#45689,#45690,#45691)) ;
#20779 = EDGE_LOOP('',(#45692,#45693,#45694,#45695)) ;
#20780 = EDGE_LOOP('',(#45696,#45697,#45698,#45699)) ;
#20781 = EDGE_LOOP('',(#45700,#45701,#45702,#45703)) ;
#20782 = EDGE_LOOP('',(#45704,#45705,#45706,#45707)) ;
#20783 = EDGE_LOOP('',(#45708,#45709,#45710,#45711)) ;
#20784 = EDGE_LOOP('',(#45712,#45713,#45714,#45715)) ;
#20785 = EDGE_LOOP('',(#45716,#45717,#45718,#45719)) ;
#20786 = EDGE_LOOP('',(#45720,#45721,#45722,#45723)) ;
#20787 = EDGE_LOOP('',(#45724,#45725,#45726,#45727)) ;
#20788 = EDGE_LOOP('',(#45728,#45729,#45730,#45731)) ;
#20789 = EDGE_LOOP('',(#45732,#45733,#45734,#45735)) ;
#20790 = EDGE_LOOP('',(#45736,#45737,#45738,#45739)) ;
#20791 = EDGE_LOOP('',(#45740,#45741,#45742,#45743)) ;
#20792 = EDGE_LOOP('',(#45744,#45745,#45746,#45747)) ;
#20793 = EDGE_LOOP('',(#45748,#45749,#45750,#45751)) ;
#20794 = EDGE_LOOP('',(#45752,#45753,#45754,#45755)) ;
#20795 = EDGE_LOOP('',(#45756,#45757,#45758,#45759)) ;
#20796 = EDGE_LOOP('',(#45760,#45761,#45762,#45763)) ;
#20797 = EDGE_LOOP('',(#45764,#45765,#45766,#45767)) ;
#20798 = EDGE_LOOP('',(#45768,#45769,#45770,#45771)) ;
#20799 = EDGE_LOOP('',(#45772,#45773,#45774,#45775)) ;
#20800 = EDGE_LOOP('',(#45776,#45777,#45778,#45779)) ;
#20801 = EDGE_LOOP('',(#45780,#45781,#45782,#45783)) ;
#20802 = EDGE_LOOP('',(#45784,#45785,#45786,#45787)) ;
#20803 = EDGE_LOOP('',(#45788,#45789,#45790,#45791)) ;
#20804 = EDGE_LOOP('',(#45792,#45793,#45794,#45795)) ;
#20805 = EDGE_LOOP('',(#45796,#45797,#45798,#45799)) ;
#20806 = EDGE_LOOP('',(#45800,#45801,#45802,#45803)) ;
#20807 = EDGE_LOOP('',(#45804,#45805,#45806,#45807)) ;
#20808 = EDGE_LOOP('',(#45808,#45809,#45810,#45811)) ;
#20809 = EDGE_LOOP('',(#45812,#45813,#45814,#45815)) ;
#20810 = EDGE_LOOP('',(#45816,#45817,#45818,#45819)) ;
#20811 = EDGE_LOOP('',(#45820,#45821,#45822,#45823)) ;
#20812 = EDGE_LOOP('',(#45824,#45825,#45826,#45827)) ;
#20813 = EDGE_LOOP('',(#45828,#45829,#45830,#45831)) ;
#20814 = EDGE_LOOP('',(#45832,#45833,#45834,#45835)) ;
#20815 = EDGE_LOOP('',(#45836,#45837,#45838,#45839)) ;
#20816 = EDGE_LOOP('',(#45840,#45841,#45842,#45843)) ;
#20817 = EDGE_LOOP('',(#45844,#45845,#45846,#45847)) ;
#20818 = EDGE_LOOP('',(#45848,#45849,#45850,#45851)) ;
#20819 = EDGE_LOOP('',(#45852,#45853,#45854,#45855)) ;
#20820 = EDGE_LOOP('',(#45856,#45857,#45858,#45859)) ;
#20821 = EDGE_LOOP('',(#45860,#45861,#45862,#45863)) ;
#20822 = EDGE_LOOP('',(#45864,#45865,#45866,#45867)) ;
#20823 = EDGE_LOOP('',(#45868,#45869,#45870,#45871)) ;
#20824 = EDGE_LOOP('',(#45872,#45873,#45874,#45875)) ;
#20825 = EDGE_LOOP('',(#45876,#45877,#45878,#45879)) ;
#20826 = EDGE_LOOP('',(#45880,#45881,#45882,#45883)) ;
#20827 = EDGE_LOOP('',(#45884,#45885,#45886,#45887)) ;
#20828 = EDGE_LOOP('',(#45888,#45889,#45890,#45891)) ;
#20829 = EDGE_LOOP('',(#45892,#45893,#45894,#45895)) ;
#20830 = EDGE_LOOP('',(#45896,#45897,#45898,#45899)) ;
#20831 = EDGE_LOOP('',(#45900,#45901,#45902,#45903)) ;
#20832 = EDGE_LOOP('',(#45904,#45905,#45906,#45907)) ;
#20833 = EDGE_LOOP('',(#45908,#45909,#45910,#45911)) ;
#20834 = EDGE_LOOP('',(#45912,#45913,#45914,#45915)) ;
#20835 = EDGE_LOOP('',(#45916,#45917,#45918,#45919)) ;
#20836 = EDGE_LOOP('',(#45920,#45921,#45922,#45923)) ;
#20837 = EDGE_LOOP('',(#45924,#45925,#45926,#45927)) ;
#20838 = EDGE_LOOP('',(#45928,#45929,#45930,#45931)) ;
#20839 = EDGE_LOOP('',(#45932,#45933,#45934,#45935)) ;
#20840 = EDGE_LOOP('',(#45936,#45937,#45938,#45939)) ;
#20841 = EDGE_LOOP('',(#45940,#45941,#45942,#45943)) ;
#20842 = EDGE_LOOP('',(#45944,#45945,#45946,#45947)) ;
#20843 = EDGE_LOOP('',(#45948,#45949,#45950,#45951)) ;
#20844 = EDGE_LOOP('',(#45952,#45953,#45954,#45955)) ;
#20845 = EDGE_LOOP('',(#45956,#45957,#45958,#45959)) ;
#20846 = EDGE_LOOP('',(#45960,#45961,#45962,#45963)) ;
#20847 = EDGE_LOOP('',(#45964,#45965,#45966,#45967)) ;
#20848 = EDGE_LOOP('',(#45968,#45969,#45970,#45971)) ;
#20849 = EDGE_LOOP('',(#45972,#45973,#45974,#45975)) ;
#20850 = EDGE_LOOP('',(#45976,#45977,#45978,#45979)) ;
#20851 = EDGE_LOOP('',(#45980,#45981,#45982,#45983)) ;
#20852 = EDGE_LOOP('',(#45984,#45985,#45986,#45987)) ;
#20853 = EDGE_LOOP('',(#45988,#45989,#45990,#45991)) ;
#20854 = EDGE_LOOP('',(#45992,#45993,#45994,#45995)) ;
#20855 = EDGE_LOOP('',(#45996,#45997,#45998,#45999)) ;
#20856 = EDGE_LOOP('',(#46000,#46001,#46002,#46003)) ;
#20857 = EDGE_LOOP('',(#46004,#46005,#46006,#46007)) ;
#20858 = EDGE_LOOP('',(#46008,#46009,#46010,#46011)) ;
#20859 = EDGE_LOOP('',(#46012,#46013,#46014,#46015)) ;
#20860 = EDGE_LOOP('',(#46016,#46017,#46018,#46019)) ;
#20861 = EDGE_LOOP('',(#46020,#46021,#46022,#46023)) ;
#20862 = EDGE_LOOP('',(#46024,#46025,#46026,#46027)) ;
#20863 = EDGE_LOOP('',(#46028,#46029,#46030,#46031)) ;
#20864 = EDGE_LOOP('',(#46032,#46033,#46034,#46035)) ;
#20865 = EDGE_LOOP('',(#46036,#46037,#46038,#46039)) ;
#20866 = EDGE_LOOP('',(#46040,#46041,#46042,#46043)) ;
#20867 = EDGE_LOOP('',(#46044,#46045,#46046,#46047)) ;
#20868 = EDGE_LOOP('',(#46048,#46049,#46050,#46051)) ;
#20869 = EDGE_LOOP('',(#46052,#46053,#46054,#46055)) ;
#20870 = EDGE_LOOP('',(#46056,#46057,#46058,#46059)) ;
#20871 = EDGE_LOOP('',(#46060,#46061,#46062)) ;
#20872 = EDGE_LOOP('',(#46063,#46064,#46065,#46066)) ;
#20873 = EDGE_LOOP('',(#46067,#46068,#46069,#46070)) ;
#20874 = EDGE_LOOP('',(#46071,#46072,#46073)) ;
#20875 = EDGE_LOOP('',(#46074,#46075,#46076,#46077)) ;
#20876 = EDGE_LOOP('',(#46078,#46079,#46080,#46081)) ;
#20877 = EDGE_LOOP('',(#46082,#46083,#46084,#46085)) ;
#20878 = EDGE_LOOP('',(#46086,#46087,#46088,#46089)) ;
#20879 = EDGE_LOOP('',(#46090,#46091,#46092)) ;
#20880 = EDGE_LOOP('',(#46093,#46094,#46095)) ;
#20881 = EDGE_LOOP('',(#46096,#46097,#46098,#46099)) ;
#20882 = EDGE_LOOP('',(#46100,#46101,#46102,#46103,#46104)) ;
#20883 = EDGE_LOOP('',(#46105,#46106,#46107,#46108,#46109)) ;
#20884 = EDGE_LOOP('',(#46110,#46111,#46112,#46113)) ;
#20885 = EDGE_LOOP('',(#46114,#46115,#46116,#46117)) ;
#20886 = EDGE_LOOP('',(#46118,#46119,#46120,#46121,#46122)) ;
#20887 = EDGE_LOOP('',(#46123,#46124,#46125,#46126)) ;
#20888 = EDGE_LOOP('',(#46127,#46128,#46129,#46130)) ;
#20889 = EDGE_LOOP('',(#46131,#46132,#46133,#46134)) ;
#20890 = EDGE_LOOP('',(#46135,#46136,#46137,#46138,#46139,#46140,#46141,#46142,
#46143,#46144)) ;
#20891 = EDGE_LOOP('',(#46145,#46146,#46147,#46148,#46149,#46150)) ;
#20892 = EDGE_LOOP('',(#46151,#46152,#46153,#46154,#46155,#46156)) ;
#20893 = EDGE_LOOP('',(#46157,#46158,#46159,#46160)) ;
#20894 = EDGE_LOOP('',(#46161,#46162,#46163,#46164,#46165,#46166)) ;
#20895 = EDGE_LOOP('',(#46167,#46168,#46169,#46170)) ;
#20896 = EDGE_LOOP('',(#46171,#46172,#46173,#46174)) ;
#20897 = EDGE_LOOP('',(#46175,#46176,#46177,#46178,#46179,#46180)) ;
#20898 = EDGE_LOOP('',(#46181,#46182,#46183,#46184,#46185,#46186,#46187,#46188,
#46189,#46190,#46191,#46192,#46193,#46194,#46195,#46196,#46197,#46198,#46199,
#46200,#46201,#46202,#46203,#46204,#46205,#46206,#46207,#46208,#46209,#46210,
#46211,#46212,#46213)) ;
#20899 = EDGE_LOOP('',(#46214,#46215,#46216,#46217,#46218,#46219,#46220,#46221,
#46222,#46223,#46224,#46225,#46226,#46227,#46228,#46229,#46230,#46231,#46232,
#46233,#46234,#46235,#46236,#46237,#46238,#46239,#46240,#46241,#46242,#46243,
#46244,#46245,#46246)) ;
#20900 = EDGE_LOOP('',(#46247,#46248,#46249,#46250)) ;
#20901 = EDGE_LOOP('',(#46251,#46252,#46253,#46254)) ;
#20902 = EDGE_LOOP('',(#46255,#46256,#46257,#46258,#46259,#46260,#46261,#46262)) ;
#20903 = EDGE_LOOP('',(#46263,#46264,#46265,#46266,#46267,#46268)) ;
#20904 = EDGE_LOOP('',(#46269,#46270,#46271,#46272)) ;
#20905 = EDGE_LOOP('',(#46273,#46274,#46275,#46276,#46277,#46278)) ;
#20906 = EDGE_LOOP('',(#46279,#46280,#46281,#46282,#46283,#46284,#46285,#46286,
#46287,#46288,#46289,#46290,#46291,#46292)) ;
#20907 = EDGE_LOOP('',(#46293,#46294,#46295,#46296,#46297,#46298,#46299,#46300,
#46301,#46302,#46303,#46304,#46305,#46306,#46307,#46308,#46309,#46310,#46311,
#46312,#46313,#46314,#46315,#46316)) ;
#20908 = EDGE_LOOP('',(#46317)) ;
#20909 = EDGE_LOOP('',(#46318,#46319,#46320,#46321,#46322,#46323,#46324,#46325,
#46326,#46327)) ;
#20910 = EDGE_LOOP('',(#46328,#46329,#46330,#46331,#46332,#46333,#46334,#46335,
#46336,#46337)) ;
#20911 = EDGE_LOOP('',(#46338,#46339,#46340)) ;
#20912 = EDGE_LOOP('',(#46341,#46342,#46343)) ;
#20913 = EDGE_LOOP('',(#46344,#46345,#46346,#46347,#46348,#46349,#46350,#46351)) ;
#20914 = EDGE_LOOP('',(#46352,#46353,#46354,#46355)) ;
#20915 = EDGE_LOOP('',(#46356,#46357,#46358,#46359)) ;
#20916 = EDGE_LOOP('',(#46360,#46361,#46362,#46363)) ;
#20917 = EDGE_LOOP('',(#46364,#46365,#46366,#46367,#46368,#46369)) ;
#20918 = EDGE_LOOP('',(#46370,#46371,#46372,#46373,#46374,#46375,#46376,#46377)) ;
#20919 = EDGE_LOOP('',(#46378)) ;
#20920 = EDGE_LOOP('',(#46379,#46380,#46381,#46382,#46383,#46384,#46385,#46386)) ;
#20921 = EDGE_LOOP('',(#46387,#46388,#46389,#46390,#46391,#46392,#46393)) ;
#20922 = EDGE_LOOP('',(#46394,#46395,#46396,#46397)) ;
#20923 = EDGE_LOOP('',(#46398,#46399,#46400,#46401)) ;
#20924 = EDGE_LOOP('',(#46402,#46403,#46404,#46405)) ;
#20925 = EDGE_LOOP('',(#46406,#46407,#46408,#46409)) ;
#20926 = EDGE_LOOP('',(#46410,#46411,#46412,#46413)) ;
#20927 = EDGE_LOOP('',(#46414,#46415,#46416,#46417)) ;
#20928 = EDGE_LOOP('',(#46418,#46419,#46420,#46421,#46422,#46423,#46424)) ;
#20929 = EDGE_LOOP('',(#46425,#46426,#46427,#46428,#46429)) ;
#20930 = EDGE_LOOP('',(#46430,#46431,#46432,#46433)) ;
#20931 = EDGE_LOOP('',(#46434,#46435,#46436,#46437)) ;
#20932 = EDGE_LOOP('',(#46438,#46439,#46440,#46441)) ;
#20933 = EDGE_LOOP('',(#46442,#46443,#46444,#46445)) ;
#20934 = EDGE_LOOP('',(#46446,#46447,#46448,#46449)) ;
#20935 = EDGE_LOOP('',(#46450,#46451,#46452,#46453)) ;
#20936 = EDGE_LOOP('',(#46454,#46455,#46456,#46457,#46458)) ;
#20937 = EDGE_LOOP('',(#46459,#46460,#46461,#46462)) ;
#20938 = EDGE_LOOP('',(#46463,#46464,#46465,#46466,#46467,#46468,#46469,#46470)) ;
#20939 = EDGE_LOOP('',(#46471,#46472,#46473,#46474)) ;
#20940 = EDGE_LOOP('',(#46475,#46476,#46477,#46478)) ;
#20941 = EDGE_LOOP('',(#46479,#46480,#46481,#46482)) ;
#20942 = EDGE_LOOP('',(#46483,#46484,#46485,#46486)) ;
#20943 = EDGE_LOOP('',(#46487,#46488,#46489,#46490)) ;
#20944 = EDGE_LOOP('',(#46491,#46492,#46493,#46494)) ;
#20945 = EDGE_LOOP('',(#46495,#46496,#46497,#46498)) ;
#20946 = EDGE_LOOP('',(#46499,#46500,#46501,#46502)) ;
#20947 = EDGE_LOOP('',(#46503,#46504,#46505,#46506,#46507,#46508)) ;
#20948 = EDGE_LOOP('',(#46509,#46510,#46511,#46512,#46513,#46514)) ;
#20949 = EDGE_LOOP('',(#46515,#46516,#46517,#46518)) ;
#20950 = EDGE_LOOP('',(#46519,#46520,#46521,#46522)) ;
#20951 = EDGE_LOOP('',(#46523,#46524,#46525,#46526)) ;
#20952 = EDGE_LOOP('',(#46527,#46528,#46529,#46530)) ;
#20953 = EDGE_LOOP('',(#46531,#46532,#46533,#46534)) ;
#20954 = EDGE_LOOP('',(#46535,#46536,#46537,#46538)) ;
#20955 = EDGE_LOOP('',(#46539,#46540,#46541,#46542)) ;
#20956 = EDGE_LOOP('',(#46543,#46544,#46545,#46546)) ;
#20957 = EDGE_LOOP('',(#46547,#46548,#46549,#46550)) ;
#20958 = EDGE_LOOP('',(#46551,#46552,#46553,#46554)) ;
#20959 = EDGE_LOOP('',(#46555,#46556,#46557,#46558)) ;
#20960 = EDGE_LOOP('',(#46559,#46560,#46561,#46562)) ;
#20961 = EDGE_LOOP('',(#46563,#46564,#46565,#46566)) ;
#20962 = EDGE_LOOP('',(#46567,#46568,#46569,#46570)) ;
#20963 = EDGE_LOOP('',(#46571,#46572,#46573,#46574)) ;
#20964 = EDGE_LOOP('',(#46575,#46576,#46577)) ;
#20965 = EDGE_LOOP('',(#46578,#46579,#46580,#46581)) ;
#20966 = EDGE_LOOP('',(#46582,#46583,#46584,#46585)) ;
#20967 = EDGE_LOOP('',(#46586,#46587,#46588,#46589)) ;
#20968 = EDGE_LOOP('',(#46590,#46591,#46592,#46593)) ;
#20969 = EDGE_LOOP('',(#46594,#46595,#46596)) ;
#20970 = EDGE_LOOP('',(#46597,#46598,#46599,#46600)) ;
#20971 = EDGE_LOOP('',(#46601,#46602,#46603,#46604)) ;
#20972 = EDGE_LOOP('',(#46605,#46606,#46607,#46608)) ;
#20973 = EDGE_LOOP('',(#46609,#46610,#46611,#46612)) ;
#20974 = EDGE_LOOP('',(#46613,#46614,#46615,#46616)) ;
#20975 = EDGE_LOOP('',(#46617,#46618,#46619,#46620)) ;
#20976 = EDGE_LOOP('',(#46621,#46622,#46623,#46624)) ;
#20977 = EDGE_LOOP('',(#46625,#46626,#46627)) ;
#20978 = EDGE_LOOP('',(#46628,#46629,#46630,#46631)) ;
#20979 = EDGE_LOOP('',(#46632,#46633,#46634,#46635)) ;
#20980 = EDGE_LOOP('',(#46636,#46637,#46638)) ;
#20981 = EDGE_LOOP('',(#46639,#46640,#46641,#46642)) ;
#20982 = EDGE_LOOP('',(#46643,#46644,#46645,#46646)) ;
#20983 = EDGE_LOOP('',(#46647,#46648,#46649,#46650)) ;
#20984 = EDGE_LOOP('',(#46651,#46652,#46653,#46654)) ;
#20985 = EDGE_LOOP('',(#46655,#46656,#46657,#46658)) ;
#20986 = EDGE_LOOP('',(#46659,#46660,#46661)) ;
#20987 = EDGE_LOOP('',(#46662,#46663,#46664,#46665)) ;
#20988 = EDGE_LOOP('',(#46666,#46667,#46668,#46669)) ;
#20989 = EDGE_LOOP('',(#46670,#46671,#46672,#46673)) ;
#20990 = EDGE_LOOP('',(#46674,#46675,#46676,#46677)) ;
#20991 = EDGE_LOOP('',(#46678,#46679,#46680,#46681)) ;
#20992 = EDGE_LOOP('',(#46682,#46683,#46684,#46685)) ;
#20993 = EDGE_LOOP('',(#46686,#46687,#46688)) ;
#20994 = EDGE_LOOP('',(#46689,#46690,#46691,#46692)) ;
#20995 = EDGE_LOOP('',(#46693,#46694,#46695,#46696)) ;
#20996 = EDGE_LOOP('',(#46697,#46698,#46699)) ;
#20997 = EDGE_LOOP('',(#46700,#46701,#46702,#46703,#46704)) ;
#20998 = EDGE_LOOP('',(#46705,#46706,#46707,#46708,#46709)) ;
#20999 = EDGE_LOOP('',(#46710,#46711,#46712,#46713)) ;
#21000 = EDGE_LOOP('',(#46714,#46715,#46716,#46717,#46718,#46719)) ;
#21001 = EDGE_LOOP('',(#46720,#46721,#46722,#46723,#46724,#46725)) ;
#21002 = EDGE_LOOP('',(#46726,#46727,#46728,#46729)) ;
#21003 = EDGE_LOOP('',(#46730,#46731,#46732,#46733)) ;
#21004 = EDGE_LOOP('',(#46734,#46735,#46736)) ;
#21005 = EDGE_LOOP('',(#46737,#46738,#46739,#46740,#46741)) ;
#21006 = EDGE_LOOP('',(#46742,#46743,#46744,#46745,#46746)) ;
#21007 = EDGE_LOOP('',(#46747,#46748,#46749,#46750)) ;
#21008 = EDGE_LOOP('',(#46751,#46752,#46753,#46754,#46755)) ;
#21009 = EDGE_LOOP('',(#46756,#46757,#46758,#46759)) ;
#21010 = EDGE_LOOP('',(#46760,#46761,#46762,#46763)) ;
#21011 = EDGE_LOOP('',(#46764,#46765,#46766)) ;
#21012 = EDGE_LOOP('',(#46767,#46768,#46769)) ;
#21013 = EDGE_LOOP('',(#46770,#46771,#46772,#46773,#46774)) ;
#21014 = EDGE_LOOP('',(#46775,#46776,#46777,#46778)) ;
#21015 = EDGE_LOOP('',(#46779,#46780,#46781)) ;
#21016 = EDGE_LOOP('',(#46782,#46783,#46784,#46785)) ;
#21017 = EDGE_LOOP('',(#46786,#46787,#46788,#46789)) ;
#21018 = EDGE_LOOP('',(#46790,#46791,#46792,#46793)) ;
#21019 = EDGE_LOOP('',(#46794,#46795,#46796,#46797)) ;
#21020 = EDGE_LOOP('',(#46798,#46799,#46800,#46801)) ;
#21021 = EDGE_LOOP('',(#46802,#46803,#46804,#46805)) ;
#21022 = EDGE_LOOP('',(#46806,#46807,#46808)) ;
#21023 = EDGE_LOOP('',(#46809,#46810,#46811,#46812)) ;
#21024 = EDGE_LOOP('',(#46813,#46814,#46815,#46816,#46817)) ;
#21025 = EDGE_LOOP('',(#46818,#46819,#46820,#46821)) ;
#21026 = EDGE_LOOP('',(#46822,#46823,#46824,#46825)) ;
#21027 = EDGE_LOOP('',(#46826,#46827,#46828,#46829,#46830)) ;
#21028 = EDGE_LOOP('',(#46831,#46832,#46833,#46834)) ;
#21029 = EDGE_LOOP('',(#46835,#46836,#46837)) ;
#21030 = EDGE_LOOP('',(#46838,#46839,#46840,#46841)) ;
#21031 = EDGE_LOOP('',(#46842,#46843,#46844,#46845)) ;
#21032 = EDGE_LOOP('',(#46846,#46847,#46848,#46849)) ;
#21033 = EDGE_LOOP('',(#46850,#46851,#46852,#46853)) ;
#21034 = EDGE_LOOP('',(#46854,#46855,#46856,#46857)) ;
#21035 = EDGE_LOOP('',(#46858,#46859,#46860,#46861)) ;
#21036 = EDGE_LOOP('',(#46862,#46863,#46864)) ;
#21037 = EDGE_LOOP('',(#46865,#46866,#46867,#46868)) ;
#21038 = EDGE_LOOP('',(#46869,#46870,#46871,#46872)) ;
#21039 = EDGE_LOOP('',(#46873,#46874,#46875,#46876)) ;
#21040 = EDGE_LOOP('',(#46877,#46878,#46879,#46880)) ;
#21041 = EDGE_LOOP('',(#46881,#46882,#46883,#46884)) ;
#21042 = EDGE_LOOP('',(#46885,#46886,#46887,#46888)) ;
#21043 = EDGE_LOOP('',(#46889,#46890,#46891,#46892)) ;
#21044 = EDGE_LOOP('',(#46893,#46894,#46895,#46896)) ;
#21045 = EDGE_LOOP('',(#46897,#46898,#46899,#46900)) ;
#21046 = EDGE_LOOP('',(#46901,#46902,#46903)) ;
#21047 = EDGE_LOOP('',(#46904,#46905,#46906,#46907)) ;
#21048 = EDGE_LOOP('',(#46908,#46909,#46910)) ;
#21049 = EDGE_LOOP('',(#46911,#46912,#46913,#46914)) ;
#21050 = EDGE_LOOP('',(#46915,#46916,#46917,#46918)) ;
#21051 = EDGE_LOOP('',(#46919,#46920,#46921,#46922)) ;
#21052 = EDGE_LOOP('',(#46923,#46924,#46925,#46926)) ;
#21053 = EDGE_LOOP('',(#46927,#46928,#46929,#46930)) ;
#21054 = EDGE_LOOP('',(#46931,#46932,#46933,#46934)) ;
#21055 = EDGE_LOOP('',(#46935,#46936,#46937,#46938)) ;
#21056 = EDGE_LOOP('',(#46939,#46940,#46941,#46942,#46943,#46944)) ;
#21057 = EDGE_LOOP('',(#46945,#46946,#46947)) ;
#21058 = EDGE_LOOP('',(#46948,#46949,#46950,#46951)) ;
#21059 = EDGE_LOOP('',(#46952,#46953,#46954,#46955)) ;
#21060 = EDGE_LOOP('',(#46956,#46957,#46958,#46959)) ;
#21061 = EDGE_LOOP('',(#46960,#46961,#46962,#46963)) ;
#21062 = EDGE_LOOP('',(#46964,#46965,#46966,#46967)) ;
#21063 = EDGE_LOOP('',(#46968,#46969,#46970,#46971)) ;
#21064 = EDGE_LOOP('',(#46972,#46973,#46974,#46975)) ;
#21065 = EDGE_LOOP('',(#46976,#46977,#46978,#46979,#46980)) ;
#21066 = EDGE_LOOP('',(#46981,#46982,#46983,#46984)) ;
#21067 = EDGE_LOOP('',(#46985,#46986,#46987,#46988,#46989)) ;
#21068 = EDGE_LOOP('',(#46990,#46991,#46992,#46993)) ;
#21069 = EDGE_LOOP('',(#46994,#46995,#46996,#46997,#46998)) ;
#21070 = EDGE_LOOP('',(#46999,#47000,#47001,#47002)) ;
#21071 = EDGE_LOOP('',(#47003,#47004,#47005)) ;
#21072 = EDGE_LOOP('',(#47006,#47007,#47008,#47009)) ;
#21073 = EDGE_LOOP('',(#47010,#47011,#47012,#47013)) ;
#21074 = EDGE_LOOP('',(#47014,#47015,#47016,#47017)) ;
#21075 = EDGE_LOOP('',(#47018,#47019,#47020,#47021)) ;
#21076 = EDGE_LOOP('',(#47022,#47023,#47024,#47025)) ;
#21077 = EDGE_LOOP('',(#47026,#47027,#47028)) ;
#21078 = EDGE_LOOP('',(#47029,#47030,#47031)) ;
#21079 = EDGE_LOOP('',(#47032,#47033,#47034,#47035)) ;
#21080 = EDGE_LOOP('',(#47036,#47037,#47038,#47039)) ;
#21081 = EDGE_LOOP('',(#47040,#47041,#47042)) ;
#21082 = EDGE_LOOP('',(#47043,#47044,#47045,#47046)) ;
#21083 = EDGE_LOOP('',(#47047,#47048,#47049,#47050)) ;
#21084 = EDGE_LOOP('',(#47051,#47052,#47053,#47054,#47055)) ;
#21085 = EDGE_LOOP('',(#47056,#47057,#47058,#47059)) ;
#21086 = EDGE_LOOP('',(#47060,#47061,#47062,#47063)) ;
#21087 = EDGE_LOOP('',(#47064,#47065,#47066,#47067)) ;
#21088 = EDGE_LOOP('',(#47068,#47069,#47070,#47071)) ;
#21089 = EDGE_LOOP('',(#47072,#47073,#47074,#47075)) ;
#21090 = EDGE_LOOP('',(#47076,#47077,#47078)) ;
#21091 = EDGE_LOOP('',(#47079,#47080,#47081,#47082)) ;
#21092 = EDGE_LOOP('',(#47083,#47084,#47085,#47086)) ;
#21093 = EDGE_LOOP('',(#47087,#47088,#47089)) ;
#21094 = EDGE_LOOP('',(#47090,#47091,#47092,#47093)) ;
#21095 = EDGE_LOOP('',(#47094,#47095,#47096,#47097)) ;
#21096 = EDGE_LOOP('',(#47098,#47099,#47100,#47101)) ;
#21097 = EDGE_LOOP('',(#47102,#47103,#47104,#47105)) ;
#21098 = EDGE_LOOP('',(#47106,#47107,#47108)) ;
#21099 = EDGE_LOOP('',(#47109,#47110,#47111)) ;
#21100 = EDGE_LOOP('',(#47112,#47113,#47114,#47115)) ;
#21101 = EDGE_LOOP('',(#47116,#47117,#47118,#47119)) ;
#21102 = EDGE_LOOP('',(#47120,#47121,#47122,#47123)) ;
#21103 = EDGE_LOOP('',(#47124,#47125,#47126)) ;
#21104 = EDGE_LOOP('',(#47127,#47128,#47129,#47130)) ;
#21105 = EDGE_LOOP('',(#47131,#47132,#47133,#47134)) ;
#21106 = EDGE_LOOP('',(#47135,#47136,#47137)) ;
#21107 = EDGE_LOOP('',(#47138,#47139,#47140,#47141)) ;
#21108 = EDGE_LOOP('',(#47142,#47143,#47144,#47145,#47146)) ;
#21109 = EDGE_LOOP('',(#47147,#47148,#47149,#47150)) ;
#21110 = EDGE_LOOP('',(#47151,#47152,#47153)) ;
#21111 = EDGE_LOOP('',(#47154,#47155,#47156,#47157)) ;
#21112 = EDGE_LOOP('',(#47158,#47159,#47160,#47161)) ;
#21113 = EDGE_LOOP('',(#47162,#47163,#47164)) ;
#21114 = EDGE_LOOP('',(#47165,#47166,#47167,#47168,#47169)) ;
#21115 = EDGE_LOOP('',(#47170,#47171,#47172,#47173)) ;
#21116 = EDGE_LOOP('',(#47174,#47175,#47176,#47177)) ;
#21117 = EDGE_LOOP('',(#47178,#47179,#47180,#47181)) ;
#21118 = EDGE_LOOP('',(#47182,#47183,#47184,#47185)) ;
#21119 = EDGE_LOOP('',(#47186,#47187,#47188,#47189)) ;
#21120 = EDGE_LOOP('',(#47190,#47191,#47192,#47193)) ;
#21121 = EDGE_LOOP('',(#47194,#47195,#47196,#47197)) ;
#21122 = EDGE_LOOP('',(#47198,#47199,#47200,#47201)) ;
#21123 = EDGE_LOOP('',(#47202,#47203,#47204,#47205,#47206)) ;
#21124 = EDGE_LOOP('',(#47207,#47208,#47209,#47210,#47211,#47212,#47213,#47214)) ;
#21125 = EDGE_LOOP('',(#47215,#47216,#47217)) ;
#21126 = EDGE_LOOP('',(#47218,#47219,#47220,#47221)) ;
#21127 = EDGE_LOOP('',(#47222,#47223,#47224,#47225,#47226)) ;
#21128 = EDGE_LOOP('',(#47227,#47228,#47229,#47230,#47231)) ;
#21129 = EDGE_LOOP('',(#47232,#47233,#47234,#47235)) ;
#21130 = EDGE_LOOP('',(#47236,#47237,#47238)) ;
#21131 = EDGE_LOOP('',(#47239,#47240,#47241,#47242,#47243,#47244,#47245,#47246)) ;
#21132 = EDGE_LOOP('',(#47247,#47248,#47249,#47250,#47251)) ;
#21133 = EDGE_LOOP('',(#47252,#47253,#47254,#47255,#47256)) ;
#21134 = EDGE_LOOP('',(#47257,#47258,#47259,#47260)) ;
#21135 = EDGE_LOOP('',(#47261,#47262,#47263,#47264,#47265,#47266,#47267,#47268)) ;
#21136 = EDGE_LOOP('',(#47269,#47270,#47271,#47272)) ;
#21137 = EDGE_LOOP('',(#47273,#47274,#47275,#47276,#47277,#47278,#47279,#47280)) ;
#21138 = EDGE_LOOP('',(#47281,#47282,#47283,#47284)) ;
#21139 = EDGE_LOOP('',(#47285,#47286,#47287,#47288)) ;
#21140 = EDGE_LOOP('',(#47289,#47290,#47291,#47292)) ;
#21141 = EDGE_LOOP('',(#47293,#47294,#47295,#47296)) ;
#21142 = EDGE_LOOP('',(#47297,#47298,#47299,#47300,#47301,#47302,#47303,#47304,
#47305)) ;
#21143 = EDGE_LOOP('',(#47306,#47307,#47308,#47309,#47310,#47311,#47312)) ;
#21144 = EDGE_LOOP('',(#47313,#47314,#47315,#47316)) ;
#21145 = EDGE_LOOP('',(#47317,#47318,#47319,#47320)) ;
#21146 = EDGE_LOOP('',(#47321,#47322,#47323,#47324)) ;
#21147 = EDGE_LOOP('',(#47325,#47326,#47327)) ;
#21148 = EDGE_LOOP('',(#47328,#47329,#47330,#47331)) ;
#21149 = EDGE_LOOP('',(#47332,#47333,#47334,#47335)) ;
#21150 = EDGE_LOOP('',(#47336,#47337,#47338,#47339)) ;
#21151 = EDGE_LOOP('',(#47340,#47341,#47342,#47343)) ;
#21152 = EDGE_LOOP('',(#47344,#47345,#47346,#47347)) ;
#21153 = EDGE_LOOP('',(#47348,#47349,#47350,#47351)) ;
#21154 = EDGE_LOOP('',(#47352,#47353,#47354,#47355)) ;
#21155 = EDGE_LOOP('',(#47356,#47357,#47358,#47359)) ;
#21156 = EDGE_LOOP('',(#47360,#47361,#47362,#47363)) ;
#21157 = EDGE_LOOP('',(#47364,#47365,#47366,#47367)) ;
#21158 = EDGE_LOOP('',(#47368,#47369,#47370,#47371)) ;
#21159 = EDGE_LOOP('',(#47372,#47373,#47374,#47375)) ;
#21160 = EDGE_LOOP('',(#47376,#47377,#47378,#47379)) ;
#21161 = EDGE_LOOP('',(#47380,#47381,#47382,#47383)) ;
#21162 = EDGE_LOOP('',(#47384,#47385,#47386,#47387)) ;
#21163 = EDGE_LOOP('',(#47388,#47389,#47390,#47391)) ;
#21164 = EDGE_LOOP('',(#47392,#47393,#47394,#47395)) ;
#21165 = EDGE_LOOP('',(#47396,#47397,#47398,#47399)) ;
#21166 = EDGE_LOOP('',(#47400,#47401,#47402,#47403)) ;
#21167 = EDGE_LOOP('',(#47404,#47405,#47406)) ;
#21168 = EDGE_LOOP('',(#47407,#47408,#47409,#47410)) ;
#21169 = EDGE_LOOP('',(#47411,#47412,#47413,#47414,#47415,#47416)) ;
#21170 = EDGE_LOOP('',(#47417,#47418,#47419,#47420)) ;
#21171 = EDGE_LOOP('',(#47421,#47422,#47423,#47424,#47425)) ;
#21172 = EDGE_LOOP('',(#47426,#47427,#47428,#47429)) ;
#21173 = EDGE_LOOP('',(#47430,#47431,#47432,#47433,#47434)) ;
#21174 = EDGE_LOOP('',(#47435,#47436,#47437,#47438,#47439)) ;
#21175 = EDGE_LOOP('',(#47440,#47441,#47442,#47443)) ;
#21176 = EDGE_LOOP('',(#47444,#47445,#47446,#47447)) ;
#21177 = EDGE_LOOP('',(#47448,#47449,#47450,#47451,#47452)) ;
#21178 = EDGE_LOOP('',(#47453,#47454,#47455,#47456)) ;
#21179 = EDGE_LOOP('',(#47457,#47458,#47459,#47460)) ;
#21180 = EDGE_LOOP('',(#47461,#47462,#47463,#47464)) ;
#21181 = EDGE_LOOP('',(#47465,#47466,#47467,#47468,#47469,#47470,#47471,#47472,
#47473,#47474)) ;
#21182 = EDGE_LOOP('',(#47475,#47476,#47477,#47478,#47479,#47480)) ;
#21183 = EDGE_LOOP('',(#47481,#47482,#47483,#47484,#47485,#47486)) ;
#21184 = EDGE_LOOP('',(#47487,#47488,#47489,#47490)) ;
#21185 = EDGE_LOOP('',(#47491,#47492,#47493,#47494,#47495,#47496)) ;
#21186 = EDGE_LOOP('',(#47497,#47498,#47499,#47500)) ;
#21187 = EDGE_LOOP('',(#47501,#47502,#47503,#47504)) ;
#21188 = EDGE_LOOP('',(#47505,#47506,#47507,#47508,#47509,#47510)) ;
#21189 = EDGE_LOOP('',(#47511,#47512,#47513,#47514,#47515,#47516,#47517,#47518,
#47519,#47520,#47521,#47522,#47523,#47524,#47525,#47526,#47527,#47528,#47529,
#47530,#47531,#47532,#47533,#47534,#47535,#47536,#47537,#47538,#47539,#47540,
#47541,#47542,#47543)) ;
#21190 = EDGE_LOOP('',(#47544,#47545,#47546,#47547,#47548,#47549,#47550,#47551,
#47552,#47553,#47554,#47555,#47556,#47557,#47558,#47559,#47560,#47561,#47562,
#47563,#47564,#47565,#47566,#47567,#47568,#47569,#47570,#47571,#47572,#47573,
#47574,#47575,#47576)) ;
#21191 = EDGE_LOOP('',(#47577,#47578,#47579,#47580)) ;
#21192 = EDGE_LOOP('',(#47581,#47582,#47583,#47584)) ;
#21193 = EDGE_LOOP('',(#47585,#47586,#47587,#47588,#47589,#47590,#47591,#47592)) ;
#21194 = EDGE_LOOP('',(#47593,#47594,#47595,#47596,#47597,#47598)) ;
#21195 = EDGE_LOOP('',(#47599,#47600,#47601,#47602)) ;
#21196 = EDGE_LOOP('',(#47603,#47604,#47605,#47606,#47607,#47608)) ;
#21197 = EDGE_LOOP('',(#47609,#47610,#47611,#47612,#47613,#47614,#47615,#47616,
#47617,#47618,#47619,#47620,#47621,#47622)) ;
#21198 = EDGE_LOOP('',(#47623,#47624,#47625,#47626,#47627,#47628,#47629,#47630,
#47631,#47632,#47633,#47634,#47635,#47636,#47637,#47638,#47639,#47640,#47641,
#47642,#47643,#47644,#47645,#47646)) ;
#21199 = EDGE_LOOP('',(#47647)) ;
#21200 = EDGE_LOOP('',(#47648,#47649,#47650,#47651,#47652,#47653,#47654,#47655,
#47656,#47657)) ;
#21201 = EDGE_LOOP('',(#47658,#47659,#47660,#47661,#47662,#47663,#47664,#47665,
#47666,#47667)) ;
#21202 = EDGE_LOOP('',(#47668,#47669,#47670)) ;
#21203 = EDGE_LOOP('',(#47671,#47672,#47673)) ;
#21204 = EDGE_LOOP('',(#47674,#47675,#47676,#47677,#47678,#47679,#47680,#47681)) ;
#21205 = EDGE_LOOP('',(#47682,#47683,#47684,#47685)) ;
#21206 = EDGE_LOOP('',(#47686,#47687,#47688,#47689)) ;
#21207 = EDGE_LOOP('',(#47690,#47691,#47692,#47693)) ;
#21208 = EDGE_LOOP('',(#47694,#47695,#47696,#47697,#47698,#47699)) ;
#21209 = EDGE_LOOP('',(#47700,#47701,#47702,#47703,#47704,#47705,#47706,#47707)) ;
#21210 = EDGE_LOOP('',(#47708)) ;
#21211 = EDGE_LOOP('',(#47709,#47710,#47711,#47712,#47713,#47714,#47715,#47716)) ;
#21212 = EDGE_LOOP('',(#47717,#47718,#47719,#47720,#47721,#47722,#47723)) ;
#21213 = EDGE_LOOP('',(#47724,#47725,#47726,#47727)) ;
#21214 = EDGE_LOOP('',(#47728,#47729,#47730,#47731)) ;
#21215 = EDGE_LOOP('',(#47732,#47733,#47734,#47735)) ;
#21216 = EDGE_LOOP('',(#47736,#47737,#47738,#47739)) ;
#21217 = EDGE_LOOP('',(#47740,#47741,#47742,#47743)) ;
#21218 = EDGE_LOOP('',(#47744,#47745,#47746,#47747)) ;
#21219 = EDGE_LOOP('',(#47748,#47749,#47750,#47751,#47752,#47753,#47754)) ;
#21220 = EDGE_LOOP('',(#47755,#47756,#47757,#47758,#47759)) ;
#21221 = EDGE_LOOP('',(#47760,#47761,#47762,#47763)) ;
#21222 = EDGE_LOOP('',(#47764,#47765,#47766,#47767)) ;
#21223 = EDGE_LOOP('',(#47768,#47769,#47770,#47771)) ;
#21224 = EDGE_LOOP('',(#47772,#47773,#47774,#47775)) ;
#21225 = EDGE_LOOP('',(#47776,#47777,#47778,#47779)) ;
#21226 = EDGE_LOOP('',(#47780,#47781,#47782,#47783)) ;
#21227 = EDGE_LOOP('',(#47784,#47785,#47786,#47787,#47788)) ;
#21228 = EDGE_LOOP('',(#47789,#47790,#47791,#47792)) ;
#21229 = EDGE_LOOP('',(#47793,#47794,#47795,#47796,#47797,#47798,#47799,#47800)) ;
#21230 = EDGE_LOOP('',(#47801,#47802,#47803,#47804)) ;
#21231 = EDGE_LOOP('',(#47805,#47806,#47807,#47808)) ;
#21232 = EDGE_LOOP('',(#47809,#47810,#47811,#47812)) ;
#21233 = EDGE_LOOP('',(#47813,#47814,#47815,#47816)) ;
#21234 = EDGE_LOOP('',(#47817,#47818,#47819,#47820)) ;
#21235 = EDGE_LOOP('',(#47821,#47822,#47823,#47824)) ;
#21236 = EDGE_LOOP('',(#47825,#47826,#47827,#47828)) ;
#21237 = EDGE_LOOP('',(#47829,#47830,#47831,#47832)) ;
#21238 = EDGE_LOOP('',(#47833,#47834,#47835,#47836,#47837,#47838)) ;
#21239 = EDGE_LOOP('',(#47839,#47840,#47841,#47842,#47843,#47844)) ;
#21240 = EDGE_LOOP('',(#47845,#47846,#47847,#47848)) ;
#21241 = EDGE_LOOP('',(#47849,#47850,#47851,#47852)) ;
#21242 = EDGE_LOOP('',(#47853,#47854,#47855,#47856)) ;
#21243 = EDGE_LOOP('',(#47857,#47858,#47859,#47860)) ;
#21244 = EDGE_LOOP('',(#47861,#47862,#47863,#47864)) ;
#21245 = EDGE_LOOP('',(#47865,#47866,#47867,#47868)) ;
#21246 = EDGE_LOOP('',(#47869,#47870,#47871,#47872)) ;
#21247 = EDGE_LOOP('',(#47873,#47874,#47875,#47876)) ;
#21248 = EDGE_LOOP('',(#47877,#47878,#47879,#47880)) ;
#21249 = EDGE_LOOP('',(#47881,#47882,#47883,#47884)) ;
#21250 = EDGE_LOOP('',(#47885,#47886,#47887,#47888)) ;
#21251 = EDGE_LOOP('',(#47889,#47890,#47891,#47892)) ;
#21252 = EDGE_LOOP('',(#47893,#47894,#47895,#47896)) ;
#21253 = EDGE_LOOP('',(#47897,#47898,#47899,#47900)) ;
#21254 = EDGE_LOOP('',(#47901,#47902,#47903,#47904)) ;
#21255 = EDGE_LOOP('',(#47905,#47906,#47907)) ;
#21256 = EDGE_LOOP('',(#47908,#47909,#47910,#47911)) ;
#21257 = EDGE_LOOP('',(#47912,#47913,#47914,#47915)) ;
#21258 = EDGE_LOOP('',(#47916,#47917,#47918,#47919)) ;
#21259 = EDGE_LOOP('',(#47920,#47921,#47922,#47923)) ;
#21260 = EDGE_LOOP('',(#47924,#47925,#47926)) ;
#21261 = EDGE_LOOP('',(#47927,#47928,#47929,#47930)) ;
#21262 = EDGE_LOOP('',(#47931,#47932,#47933,#47934)) ;
#21263 = EDGE_LOOP('',(#47935,#47936,#47937,#47938)) ;
#21264 = EDGE_LOOP('',(#47939,#47940,#47941,#47942)) ;
#21265 = EDGE_LOOP('',(#47943,#47944,#47945,#47946)) ;
#21266 = EDGE_LOOP('',(#47947,#47948,#47949,#47950)) ;
#21267 = EDGE_LOOP('',(#47951,#47952,#47953,#47954)) ;
#21268 = EDGE_LOOP('',(#47955,#47956,#47957)) ;
#21269 = EDGE_LOOP('',(#47958,#47959,#47960,#47961)) ;
#21270 = EDGE_LOOP('',(#47962,#47963,#47964,#47965)) ;
#21271 = EDGE_LOOP('',(#47966,#47967,#47968)) ;
#21272 = EDGE_LOOP('',(#47969,#47970,#47971,#47972)) ;
#21273 = EDGE_LOOP('',(#47973,#47974,#47975,#47976)) ;
#21274 = EDGE_LOOP('',(#47977,#47978,#47979,#47980)) ;
#21275 = EDGE_LOOP('',(#47981,#47982,#47983,#47984)) ;
#21276 = EDGE_LOOP('',(#47985,#47986,#47987,#47988)) ;
#21277 = EDGE_LOOP('',(#47989,#47990,#47991)) ;
#21278 = EDGE_LOOP('',(#47992,#47993,#47994,#47995)) ;
#21279 = EDGE_LOOP('',(#47996,#47997,#47998,#47999)) ;
#21280 = EDGE_LOOP('',(#48000,#48001,#48002,#48003)) ;
#21281 = EDGE_LOOP('',(#48004,#48005,#48006,#48007)) ;
#21282 = EDGE_LOOP('',(#48008,#48009,#48010,#48011)) ;
#21283 = EDGE_LOOP('',(#48012,#48013,#48014,#48015)) ;
#21284 = EDGE_LOOP('',(#48016,#48017,#48018)) ;
#21285 = EDGE_LOOP('',(#48019,#48020,#48021,#48022)) ;
#21286 = EDGE_LOOP('',(#48023,#48024,#48025,#48026)) ;
#21287 = EDGE_LOOP('',(#48027,#48028,#48029)) ;
#21288 = EDGE_LOOP('',(#48030,#48031,#48032,#48033,#48034)) ;
#21289 = EDGE_LOOP('',(#48035,#48036,#48037,#48038,#48039)) ;
#21290 = EDGE_LOOP('',(#48040,#48041,#48042,#48043)) ;
#21291 = EDGE_LOOP('',(#48044,#48045,#48046,#48047,#48048,#48049)) ;
#21292 = EDGE_LOOP('',(#48050,#48051,#48052,#48053,#48054,#48055)) ;
#21293 = EDGE_LOOP('',(#48056,#48057,#48058,#48059)) ;
#21294 = EDGE_LOOP('',(#48060,#48061,#48062,#48063)) ;
#21295 = EDGE_LOOP('',(#48064,#48065,#48066)) ;
#21296 = EDGE_LOOP('',(#48067,#48068,#48069,#48070,#48071)) ;
#21297 = EDGE_LOOP('',(#48072,#48073,#48074,#48075,#48076)) ;
#21298 = EDGE_LOOP('',(#48077,#48078,#48079,#48080)) ;
#21299 = EDGE_LOOP('',(#48081,#48082,#48083,#48084,#48085)) ;
#21300 = EDGE_LOOP('',(#48086,#48087,#48088,#48089)) ;
#21301 = EDGE_LOOP('',(#48090,#48091,#48092,#48093)) ;
#21302 = EDGE_LOOP('',(#48094,#48095,#48096)) ;
#21303 = EDGE_LOOP('',(#48097,#48098,#48099)) ;
#21304 = EDGE_LOOP('',(#48100,#48101,#48102,#48103,#48104)) ;
#21305 = EDGE_LOOP('',(#48105,#48106,#48107,#48108)) ;
#21306 = EDGE_LOOP('',(#48109,#48110,#48111)) ;
#21307 = EDGE_LOOP('',(#48112,#48113,#48114,#48115)) ;
#21308 = EDGE_LOOP('',(#48116,#48117,#48118,#48119)) ;
#21309 = EDGE_LOOP('',(#48120,#48121,#48122,#48123)) ;
#21310 = EDGE_LOOP('',(#48124,#48125,#48126,#48127)) ;
#21311 = EDGE_LOOP('',(#48128,#48129,#48130,#48131)) ;
#21312 = EDGE_LOOP('',(#48132,#48133,#48134,#48135)) ;
#21313 = EDGE_LOOP('',(#48136,#48137,#48138)) ;
#21314 = EDGE_LOOP('',(#48139,#48140,#48141,#48142)) ;
#21315 = EDGE_LOOP('',(#48143,#48144,#48145,#48146,#48147)) ;
#21316 = EDGE_LOOP('',(#48148,#48149,#48150,#48151)) ;
#21317 = EDGE_LOOP('',(#48152,#48153,#48154,#48155)) ;
#21318 = EDGE_LOOP('',(#48156,#48157,#48158,#48159,#48160)) ;
#21319 = EDGE_LOOP('',(#48161,#48162,#48163,#48164)) ;
#21320 = EDGE_LOOP('',(#48165,#48166,#48167)) ;
#21321 = EDGE_LOOP('',(#48168,#48169,#48170,#48171)) ;
#21322 = EDGE_LOOP('',(#48172,#48173,#48174,#48175)) ;
#21323 = EDGE_LOOP('',(#48176,#48177,#48178,#48179)) ;
#21324 = EDGE_LOOP('',(#48180,#48181,#48182,#48183)) ;
#21325 = EDGE_LOOP('',(#48184,#48185,#48186,#48187)) ;
#21326 = EDGE_LOOP('',(#48188,#48189,#48190,#48191)) ;
#21327 = EDGE_LOOP('',(#48192,#48193,#48194)) ;
#21328 = EDGE_LOOP('',(#48195,#48196,#48197,#48198)) ;
#21329 = EDGE_LOOP('',(#48199,#48200,#48201,#48202)) ;
#21330 = EDGE_LOOP('',(#48203,#48204,#48205,#48206)) ;
#21331 = EDGE_LOOP('',(#48207,#48208,#48209,#48210)) ;
#21332 = EDGE_LOOP('',(#48211,#48212,#48213,#48214)) ;
#21333 = EDGE_LOOP('',(#48215,#48216,#48217,#48218)) ;
#21334 = EDGE_LOOP('',(#48219,#48220,#48221,#48222)) ;
#21335 = EDGE_LOOP('',(#48223,#48224,#48225,#48226)) ;
#21336 = EDGE_LOOP('',(#48227,#48228,#48229,#48230)) ;
#21337 = EDGE_LOOP('',(#48231,#48232,#48233)) ;
#21338 = EDGE_LOOP('',(#48234,#48235,#48236,#48237)) ;
#21339 = EDGE_LOOP('',(#48238,#48239,#48240)) ;
#21340 = EDGE_LOOP('',(#48241,#48242,#48243,#48244)) ;
#21341 = EDGE_LOOP('',(#48245,#48246,#48247,#48248)) ;
#21342 = EDGE_LOOP('',(#48249,#48250,#48251,#48252)) ;
#21343 = EDGE_LOOP('',(#48253,#48254,#48255,#48256)) ;
#21344 = EDGE_LOOP('',(#48257,#48258,#48259,#48260)) ;
#21345 = EDGE_LOOP('',(#48261,#48262,#48263,#48264)) ;
#21346 = EDGE_LOOP('',(#48265,#48266,#48267,#48268)) ;
#21347 = EDGE_LOOP('',(#48269,#48270,#48271,#48272,#48273,#48274)) ;
#21348 = EDGE_LOOP('',(#48275,#48276,#48277)) ;
#21349 = EDGE_LOOP('',(#48278,#48279,#48280,#48281)) ;
#21350 = EDGE_LOOP('',(#48282,#48283,#48284,#48285)) ;
#21351 = EDGE_LOOP('',(#48286,#48287,#48288,#48289)) ;
#21352 = EDGE_LOOP('',(#48290,#48291,#48292,#48293)) ;
#21353 = EDGE_LOOP('',(#48294,#48295,#48296,#48297)) ;
#21354 = EDGE_LOOP('',(#48298,#48299,#48300,#48301)) ;
#21355 = EDGE_LOOP('',(#48302,#48303,#48304,#48305)) ;
#21356 = EDGE_LOOP('',(#48306,#48307,#48308,#48309,#48310)) ;
#21357 = EDGE_LOOP('',(#48311,#48312,#48313,#48314)) ;
#21358 = EDGE_LOOP('',(#48315,#48316,#48317,#48318,#48319)) ;
#21359 = EDGE_LOOP('',(#48320,#48321,#48322,#48323)) ;
#21360 = EDGE_LOOP('',(#48324,#48325,#48326,#48327,#48328)) ;
#21361 = EDGE_LOOP('',(#48329,#48330,#48331,#48332)) ;
#21362 = EDGE_LOOP('',(#48333,#48334,#48335)) ;
#21363 = EDGE_LOOP('',(#48336,#48337,#48338,#48339)) ;
#21364 = EDGE_LOOP('',(#48340,#48341,#48342,#48343)) ;
#21365 = EDGE_LOOP('',(#48344,#48345,#48346,#48347)) ;
#21366 = EDGE_LOOP('',(#48348,#48349,#48350,#48351)) ;
#21367 = EDGE_LOOP('',(#48352,#48353,#48354,#48355)) ;
#21368 = EDGE_LOOP('',(#48356,#48357,#48358)) ;
#21369 = EDGE_LOOP('',(#48359,#48360,#48361)) ;
#21370 = EDGE_LOOP('',(#48362,#48363,#48364,#48365)) ;
#21371 = EDGE_LOOP('',(#48366,#48367,#48368,#48369)) ;
#21372 = EDGE_LOOP('',(#48370,#48371,#48372)) ;
#21373 = EDGE_LOOP('',(#48373,#48374,#48375,#48376)) ;
#21374 = EDGE_LOOP('',(#48377,#48378,#48379,#48380)) ;
#21375 = EDGE_LOOP('',(#48381,#48382,#48383,#48384,#48385)) ;
#21376 = EDGE_LOOP('',(#48386,#48387,#48388,#48389)) ;
#21377 = EDGE_LOOP('',(#48390,#48391,#48392,#48393)) ;
#21378 = EDGE_LOOP('',(#48394,#48395,#48396,#48397)) ;
#21379 = EDGE_LOOP('',(#48398,#48399,#48400,#48401)) ;
#21380 = EDGE_LOOP('',(#48402,#48403,#48404,#48405)) ;
#21381 = EDGE_LOOP('',(#48406,#48407,#48408)) ;
#21382 = EDGE_LOOP('',(#48409,#48410,#48411,#48412)) ;
#21383 = EDGE_LOOP('',(#48413,#48414,#48415,#48416)) ;
#21384 = EDGE_LOOP('',(#48417,#48418,#48419)) ;
#21385 = EDGE_LOOP('',(#48420,#48421,#48422,#48423)) ;
#21386 = EDGE_LOOP('',(#48424,#48425,#48426,#48427)) ;
#21387 = EDGE_LOOP('',(#48428,#48429,#48430,#48431)) ;
#21388 = EDGE_LOOP('',(#48432,#48433,#48434,#48435)) ;
#21389 = EDGE_LOOP('',(#48436,#48437,#48438)) ;
#21390 = EDGE_LOOP('',(#48439,#48440,#48441)) ;
#21391 = EDGE_LOOP('',(#48442,#48443,#48444,#48445)) ;
#21392 = EDGE_LOOP('',(#48446,#48447,#48448,#48449)) ;
#21393 = EDGE_LOOP('',(#48450,#48451,#48452,#48453)) ;
#21394 = EDGE_LOOP('',(#48454,#48455,#48456)) ;
#21395 = EDGE_LOOP('',(#48457,#48458,#48459,#48460)) ;
#21396 = EDGE_LOOP('',(#48461,#48462,#48463,#48464)) ;
#21397 = EDGE_LOOP('',(#48465,#48466,#48467)) ;
#21398 = EDGE_LOOP('',(#48468,#48469,#48470,#48471)) ;
#21399 = EDGE_LOOP('',(#48472,#48473,#48474,#48475,#48476)) ;
#21400 = EDGE_LOOP('',(#48477,#48478,#48479,#48480)) ;
#21401 = EDGE_LOOP('',(#48481,#48482,#48483)) ;
#21402 = EDGE_LOOP('',(#48484,#48485,#48486,#48487)) ;
#21403 = EDGE_LOOP('',(#48488,#48489,#48490,#48491)) ;
#21404 = EDGE_LOOP('',(#48492,#48493,#48494)) ;
#21405 = EDGE_LOOP('',(#48495,#48496,#48497,#48498,#48499)) ;
#21406 = EDGE_LOOP('',(#48500,#48501,#48502,#48503)) ;
#21407 = EDGE_LOOP('',(#48504,#48505,#48506,#48507)) ;
#21408 = EDGE_LOOP('',(#48508,#48509,#48510,#48511)) ;
#21409 = EDGE_LOOP('',(#48512,#48513,#48514,#48515)) ;
#21410 = EDGE_LOOP('',(#48516,#48517,#48518,#48519)) ;
#21411 = EDGE_LOOP('',(#48520,#48521,#48522,#48523)) ;
#21412 = EDGE_LOOP('',(#48524,#48525,#48526,#48527)) ;
#21413 = EDGE_LOOP('',(#48528,#48529,#48530,#48531)) ;
#21414 = EDGE_LOOP('',(#48532,#48533,#48534,#48535,#48536)) ;
#21415 = EDGE_LOOP('',(#48537,#48538,#48539,#48540,#48541,#48542,#48543,#48544)) ;
#21416 = EDGE_LOOP('',(#48545,#48546,#48547)) ;
#21417 = EDGE_LOOP('',(#48548,#48549,#48550,#48551)) ;
#21418 = EDGE_LOOP('',(#48552,#48553,#48554,#48555,#48556)) ;
#21419 = EDGE_LOOP('',(#48557,#48558,#48559,#48560,#48561)) ;
#21420 = EDGE_LOOP('',(#48562,#48563,#48564,#48565)) ;
#21421 = EDGE_LOOP('',(#48566,#48567,#48568)) ;
#21422 = EDGE_LOOP('',(#48569,#48570,#48571,#48572,#48573,#48574,#48575,#48576)) ;
#21423 = EDGE_LOOP('',(#48577,#48578,#48579,#48580,#48581)) ;
#21424 = EDGE_LOOP('',(#48582,#48583,#48584,#48585,#48586)) ;
#21425 = EDGE_LOOP('',(#48587,#48588,#48589,#48590)) ;
#21426 = EDGE_LOOP('',(#48591,#48592,#48593,#48594,#48595,#48596,#48597,#48598)) ;
#21427 = EDGE_LOOP('',(#48599,#48600,#48601,#48602)) ;
#21428 = EDGE_LOOP('',(#48603,#48604,#48605,#48606,#48607,#48608,#48609,#48610)) ;
#21429 = EDGE_LOOP('',(#48611,#48612,#48613,#48614)) ;
#21430 = EDGE_LOOP('',(#48615,#48616,#48617,#48618)) ;
#21431 = EDGE_LOOP('',(#48619,#48620,#48621,#48622)) ;
#21432 = EDGE_LOOP('',(#48623,#48624,#48625,#48626)) ;
#21433 = EDGE_LOOP('',(#48627,#48628,#48629,#48630,#48631,#48632,#48633,#48634,
#48635)) ;
#21434 = EDGE_LOOP('',(#48636,#48637,#48638,#48639,#48640,#48641,#48642)) ;
#21435 = EDGE_LOOP('',(#48643,#48644,#48645,#48646)) ;
#21436 = EDGE_LOOP('',(#48647,#48648,#48649,#48650)) ;
#21437 = EDGE_LOOP('',(#48651,#48652,#48653,#48654)) ;
#21438 = EDGE_LOOP('',(#48655,#48656,#48657)) ;
#21439 = EDGE_LOOP('',(#48658,#48659,#48660,#48661)) ;
#21440 = EDGE_LOOP('',(#48662,#48663,#48664,#48665)) ;
#21441 = EDGE_LOOP('',(#48666,#48667,#48668,#48669)) ;
#21442 = EDGE_LOOP('',(#48670,#48671,#48672,#48673)) ;
#21443 = EDGE_LOOP('',(#48674,#48675,#48676,#48677)) ;
#21444 = EDGE_LOOP('',(#48678,#48679,#48680,#48681)) ;
#21445 = EDGE_LOOP('',(#48682,#48683,#48684,#48685)) ;
#21446 = EDGE_LOOP('',(#48686,#48687,#48688,#48689)) ;
#21447 = EDGE_LOOP('',(#48690,#48691,#48692,#48693)) ;
#21448 = EDGE_LOOP('',(#48694,#48695,#48696,#48697)) ;
#21449 = EDGE_LOOP('',(#48698,#48699,#48700,#48701)) ;
#21450 = EDGE_LOOP('',(#48702,#48703,#48704,#48705)) ;
#21451 = EDGE_LOOP('',(#48706,#48707,#48708,#48709)) ;
#21452 = EDGE_LOOP('',(#48710,#48711,#48712,#48713)) ;
#21453 = EDGE_LOOP('',(#48714,#48715,#48716,#48717)) ;
#21454 = EDGE_LOOP('',(#48718,#48719,#48720,#48721)) ;
#21455 = EDGE_LOOP('',(#48722,#48723,#48724,#48725)) ;
#21456 = EDGE_LOOP('',(#48726,#48727,#48728,#48729)) ;
#21457 = EDGE_LOOP('',(#48730,#48731,#48732,#48733)) ;
#21458 = EDGE_LOOP('',(#48734,#48735,#48736)) ;
#21459 = EDGE_LOOP('',(#48737,#48738,#48739,#48740)) ;
#21460 = EDGE_LOOP('',(#48741,#48742,#48743,#48744,#48745,#48746)) ;
#21461 = EDGE_LOOP('',(#48747,#48748,#48749,#48750)) ;
#21462 = EDGE_LOOP('',(#48751,#48752,#48753,#48754,#48755)) ;
#21463 = EDGE_LOOP('',(#48756,#48757,#48758,#48759)) ;
#21464 = EDGE_LOOP('',(#48760,#48761,#48762,#48763,#48764)) ;
#21465 = EDGE_LOOP('',(#48765,#48766,#48767,#48768,#48769)) ;
#21466 = EDGE_LOOP('',(#48770,#48771,#48772,#48773)) ;
#21467 = EDGE_LOOP('',(#48774,#48775,#48776,#48777)) ;
#21468 = EDGE_LOOP('',(#48778,#48779,#48780,#48781,#48782)) ;
#21469 = EDGE_LOOP('',(#48783,#48784,#48785,#48786)) ;
#21470 = EDGE_LOOP('',(#48787,#48788,#48789,#48790)) ;
#21471 = EDGE_LOOP('',(#48791,#48792,#48793,#48794)) ;
#21472 = EDGE_LOOP('',(#48795,#48796,#48797,#48798,#48799,#48800,#48801,#48802,
#48803,#48804)) ;
#21473 = EDGE_LOOP('',(#48805,#48806,#48807,#48808,#48809,#48810)) ;
#21474 = EDGE_LOOP('',(#48811,#48812,#48813,#48814,#48815,#48816)) ;
#21475 = EDGE_LOOP('',(#48817,#48818,#48819,#48820)) ;
#21476 = EDGE_LOOP('',(#48821,#48822,#48823,#48824,#48825,#48826)) ;
#21477 = EDGE_LOOP('',(#48827,#48828,#48829,#48830)) ;
#21478 = EDGE_LOOP('',(#48831,#48832,#48833,#48834)) ;
#21479 = EDGE_LOOP('',(#48835,#48836,#48837,#48838,#48839,#48840)) ;
#21480 = EDGE_LOOP('',(#48841,#48842,#48843,#48844,#48845,#48846,#48847,#48848,
#48849,#48850,#48851,#48852,#48853,#48854,#48855,#48856,#48857,#48858,#48859,
#48860,#48861,#48862,#48863,#48864,#48865,#48866,#48867,#48868,#48869,#48870,
#48871,#48872,#48873)) ;
#21481 = EDGE_LOOP('',(#48874,#48875,#48876,#48877,#48878,#48879,#48880,#48881,
#48882,#48883,#48884,#48885,#48886,#48887,#48888,#48889,#48890,#48891,#48892,
#48893,#48894,#48895,#48896,#48897,#48898,#48899,#48900,#48901,#48902,#48903,
#48904,#48905,#48906)) ;
#21482 = EDGE_LOOP('',(#48907,#48908,#48909,#48910)) ;
#21483 = EDGE_LOOP('',(#48911,#48912,#48913,#48914)) ;
#21484 = EDGE_LOOP('',(#48915,#48916,#48917,#48918,#48919,#48920,#48921,#48922)) ;
#21485 = EDGE_LOOP('',(#48923,#48924,#48925,#48926,#48927,#48928)) ;
#21486 = EDGE_LOOP('',(#48929,#48930,#48931,#48932)) ;
#21487 = EDGE_LOOP('',(#48933,#48934,#48935,#48936,#48937,#48938)) ;
#21488 = EDGE_LOOP('',(#48939,#48940,#48941,#48942,#48943,#48944,#48945,#48946,
#48947,#48948,#48949,#48950,#48951,#48952)) ;
#21489 = EDGE_LOOP('',(#48953,#48954,#48955,#48956,#48957,#48958,#48959,#48960,
#48961,#48962,#48963,#48964,#48965,#48966,#48967,#48968,#48969,#48970,#48971,
#48972,#48973,#48974,#48975,#48976)) ;
#21490 = EDGE_LOOP('',(#48977)) ;
#21491 = EDGE_LOOP('',(#48978,#48979,#48980,#48981,#48982,#48983,#48984,#48985,
#48986,#48987)) ;
#21492 = EDGE_LOOP('',(#48988,#48989,#48990,#48991,#48992,#48993,#48994,#48995,
#48996,#48997)) ;
#21493 = EDGE_LOOP('',(#48998,#48999,#49000)) ;
#21494 = EDGE_LOOP('',(#49001,#49002,#49003)) ;
#21495 = EDGE_LOOP('',(#49004,#49005,#49006,#49007,#49008,#49009,#49010,#49011)) ;
#21496 = EDGE_LOOP('',(#49012,#49013,#49014,#49015)) ;
#21497 = EDGE_LOOP('',(#49016,#49017,#49018,#49019)) ;
#21498 = EDGE_LOOP('',(#49020,#49021,#49022,#49023)) ;
#21499 = EDGE_LOOP('',(#49024,#49025,#49026,#49027,#49028,#49029)) ;
#21500 = EDGE_LOOP('',(#49030,#49031,#49032,#49033,#49034,#49035,#49036,#49037)) ;
#21501 = EDGE_LOOP('',(#49038)) ;
#21502 = EDGE_LOOP('',(#49039,#49040,#49041,#49042,#49043,#49044,#49045,#49046)) ;
#21503 = EDGE_LOOP('',(#49047,#49048,#49049,#49050,#49051,#49052,#49053)) ;
#21504 = EDGE_LOOP('',(#49054,#49055,#49056,#49057)) ;
#21505 = EDGE_LOOP('',(#49058,#49059,#49060,#49061)) ;
#21506 = EDGE_LOOP('',(#49062,#49063,#49064,#49065)) ;
#21507 = EDGE_LOOP('',(#49066,#49067,#49068,#49069)) ;
#21508 = EDGE_LOOP('',(#49070,#49071,#49072,#49073)) ;
#21509 = EDGE_LOOP('',(#49074,#49075,#49076,#49077)) ;
#21510 = EDGE_LOOP('',(#49078,#49079,#49080,#49081,#49082,#49083,#49084)) ;
#21511 = EDGE_LOOP('',(#49085,#49086,#49087,#49088,#49089)) ;
#21512 = EDGE_LOOP('',(#49090,#49091,#49092,#49093)) ;
#21513 = EDGE_LOOP('',(#49094,#49095,#49096,#49097)) ;
#21514 = EDGE_LOOP('',(#49098,#49099,#49100,#49101)) ;
#21515 = EDGE_LOOP('',(#49102,#49103,#49104,#49105)) ;
#21516 = EDGE_LOOP('',(#49106,#49107,#49108,#49109)) ;
#21517 = EDGE_LOOP('',(#49110,#49111,#49112,#49113)) ;
#21518 = EDGE_LOOP('',(#49114,#49115,#49116,#49117,#49118)) ;
#21519 = EDGE_LOOP('',(#49119,#49120,#49121,#49122)) ;
#21520 = EDGE_LOOP('',(#49123,#49124,#49125,#49126,#49127,#49128,#49129,#49130)) ;
#21521 = EDGE_LOOP('',(#49131,#49132,#49133,#49134)) ;
#21522 = EDGE_LOOP('',(#49135,#49136,#49137,#49138)) ;
#21523 = EDGE_LOOP('',(#49139,#49140,#49141,#49142)) ;
#21524 = EDGE_LOOP('',(#49143,#49144,#49145,#49146)) ;
#21525 = EDGE_LOOP('',(#49147,#49148,#49149,#49150)) ;
#21526 = EDGE_LOOP('',(#49151,#49152,#49153,#49154)) ;
#21527 = EDGE_LOOP('',(#49155,#49156,#49157,#49158)) ;
#21528 = EDGE_LOOP('',(#49159,#49160,#49161,#49162)) ;
#21529 = EDGE_LOOP('',(#49163,#49164,#49165,#49166,#49167,#49168)) ;
#21530 = EDGE_LOOP('',(#49169,#49170,#49171,#49172,#49173,#49174)) ;
#21531 = EDGE_LOOP('',(#49175,#49176,#49177,#49178)) ;
#21532 = EDGE_LOOP('',(#49179,#49180,#49181,#49182)) ;
#21533 = EDGE_LOOP('',(#49183,#49184,#49185,#49186)) ;
#21534 = EDGE_LOOP('',(#49187,#49188,#49189,#49190)) ;
#21535 = EDGE_LOOP('',(#49191,#49192,#49193,#49194)) ;
#21536 = EDGE_LOOP('',(#49195,#49196,#49197,#49198)) ;
#21537 = EDGE_LOOP('',(#49199,#49200,#49201,#49202)) ;
#21538 = EDGE_LOOP('',(#49203,#49204,#49205,#49206)) ;
#21539 = EDGE_LOOP('',(#49207,#49208,#49209,#49210)) ;
#21540 = EDGE_LOOP('',(#49211,#49212,#49213,#49214)) ;
#21541 = EDGE_LOOP('',(#49215,#49216,#49217,#49218)) ;
#21542 = EDGE_LOOP('',(#49219,#49220,#49221,#49222)) ;
#21543 = EDGE_LOOP('',(#49223,#49224,#49225,#49226)) ;
#21544 = EDGE_LOOP('',(#49227,#49228,#49229,#49230)) ;
#21545 = EDGE_LOOP('',(#49231,#49232,#49233,#49234)) ;
#21546 = EDGE_LOOP('',(#49235,#49236,#49237)) ;
#21547 = EDGE_LOOP('',(#49238,#49239,#49240,#49241)) ;
#21548 = EDGE_LOOP('',(#49242,#49243,#49244,#49245)) ;
#21549 = EDGE_LOOP('',(#49246,#49247,#49248,#49249)) ;
#21550 = EDGE_LOOP('',(#49250,#49251,#49252,#49253)) ;
#21551 = EDGE_LOOP('',(#49254,#49255,#49256)) ;
#21552 = EDGE_LOOP('',(#49257,#49258,#49259,#49260)) ;
#21553 = EDGE_LOOP('',(#49261,#49262,#49263,#49264)) ;
#21554 = EDGE_LOOP('',(#49265,#49266,#49267,#49268)) ;
#21555 = EDGE_LOOP('',(#49269,#49270,#49271,#49272)) ;
#21556 = EDGE_LOOP('',(#49273,#49274,#49275,#49276)) ;
#21557 = EDGE_LOOP('',(#49277,#49278,#49279,#49280)) ;
#21558 = EDGE_LOOP('',(#49281,#49282,#49283,#49284)) ;
#21559 = EDGE_LOOP('',(#49285,#49286,#49287)) ;
#21560 = EDGE_LOOP('',(#49288,#49289,#49290,#49291)) ;
#21561 = EDGE_LOOP('',(#49292,#49293,#49294,#49295)) ;
#21562 = EDGE_LOOP('',(#49296,#49297,#49298)) ;
#21563 = EDGE_LOOP('',(#49299,#49300,#49301,#49302)) ;
#21564 = EDGE_LOOP('',(#49303,#49304,#49305,#49306)) ;
#21565 = EDGE_LOOP('',(#49307,#49308,#49309,#49310)) ;
#21566 = EDGE_LOOP('',(#49311,#49312,#49313,#49314)) ;
#21567 = EDGE_LOOP('',(#49315,#49316,#49317,#49318)) ;
#21568 = EDGE_LOOP('',(#49319,#49320,#49321)) ;
#21569 = EDGE_LOOP('',(#49322,#49323,#49324,#49325)) ;
#21570 = EDGE_LOOP('',(#49326,#49327,#49328,#49329)) ;
#21571 = EDGE_LOOP('',(#49330,#49331,#49332,#49333)) ;
#21572 = EDGE_LOOP('',(#49334,#49335,#49336,#49337)) ;
#21573 = EDGE_LOOP('',(#49338,#49339,#49340,#49341)) ;
#21574 = EDGE_LOOP('',(#49342,#49343,#49344,#49345)) ;
#21575 = EDGE_LOOP('',(#49346,#49347,#49348)) ;
#21576 = EDGE_LOOP('',(#49349,#49350,#49351,#49352)) ;
#21577 = EDGE_LOOP('',(#49353,#49354,#49355,#49356)) ;
#21578 = EDGE_LOOP('',(#49357,#49358,#49359)) ;
#21579 = EDGE_LOOP('',(#49360,#49361,#49362,#49363,#49364)) ;
#21580 = EDGE_LOOP('',(#49365,#49366,#49367,#49368,#49369)) ;
#21581 = EDGE_LOOP('',(#49370,#49371,#49372,#49373)) ;
#21582 = EDGE_LOOP('',(#49374,#49375,#49376,#49377,#49378,#49379)) ;
#21583 = EDGE_LOOP('',(#49380,#49381,#49382,#49383,#49384,#49385)) ;
#21584 = EDGE_LOOP('',(#49386,#49387,#49388,#49389)) ;
#21585 = EDGE_LOOP('',(#49390,#49391,#49392,#49393)) ;
#21586 = EDGE_LOOP('',(#49394,#49395,#49396)) ;
#21587 = EDGE_LOOP('',(#49397,#49398,#49399,#49400,#49401)) ;
#21588 = EDGE_LOOP('',(#49402,#49403,#49404,#49405,#49406)) ;
#21589 = EDGE_LOOP('',(#49407,#49408,#49409,#49410)) ;
#21590 = EDGE_LOOP('',(#49411,#49412,#49413,#49414,#49415)) ;
#21591 = EDGE_LOOP('',(#49416,#49417,#49418,#49419)) ;
#21592 = EDGE_LOOP('',(#49420,#49421,#49422,#49423)) ;
#21593 = EDGE_LOOP('',(#49424,#49425,#49426)) ;
#21594 = EDGE_LOOP('',(#49427,#49428,#49429)) ;
#21595 = EDGE_LOOP('',(#49430,#49431,#49432,#49433,#49434)) ;
#21596 = EDGE_LOOP('',(#49435,#49436,#49437,#49438)) ;
#21597 = EDGE_LOOP('',(#49439,#49440,#49441)) ;
#21598 = EDGE_LOOP('',(#49442,#49443,#49444,#49445)) ;
#21599 = EDGE_LOOP('',(#49446,#49447,#49448,#49449)) ;
#21600 = EDGE_LOOP('',(#49450,#49451,#49452,#49453)) ;
#21601 = EDGE_LOOP('',(#49454,#49455,#49456,#49457)) ;
#21602 = EDGE_LOOP('',(#49458,#49459,#49460,#49461)) ;
#21603 = EDGE_LOOP('',(#49462,#49463,#49464,#49465)) ;
#21604 = EDGE_LOOP('',(#49466,#49467,#49468)) ;
#21605 = EDGE_LOOP('',(#49469,#49470,#49471,#49472)) ;
#21606 = EDGE_LOOP('',(#49473,#49474,#49475,#49476,#49477)) ;
#21607 = EDGE_LOOP('',(#49478,#49479,#49480,#49481)) ;
#21608 = EDGE_LOOP('',(#49482,#49483,#49484,#49485)) ;
#21609 = EDGE_LOOP('',(#49486,#49487,#49488,#49489,#49490)) ;
#21610 = EDGE_LOOP('',(#49491,#49492,#49493,#49494)) ;
#21611 = EDGE_LOOP('',(#49495,#49496,#49497)) ;
#21612 = EDGE_LOOP('',(#49498,#49499,#49500,#49501)) ;
#21613 = EDGE_LOOP('',(#49502,#49503,#49504,#49505)) ;
#21614 = EDGE_LOOP('',(#49506,#49507,#49508,#49509)) ;
#21615 = EDGE_LOOP('',(#49510,#49511,#49512,#49513)) ;
#21616 = EDGE_LOOP('',(#49514,#49515,#49516,#49517)) ;
#21617 = EDGE_LOOP('',(#49518,#49519,#49520,#49521)) ;
#21618 = EDGE_LOOP('',(#49522,#49523,#49524)) ;
#21619 = EDGE_LOOP('',(#49525,#49526,#49527,#49528)) ;
#21620 = EDGE_LOOP('',(#49529,#49530,#49531,#49532)) ;
#21621 = EDGE_LOOP('',(#49533,#49534,#49535,#49536)) ;
#21622 = EDGE_LOOP('',(#49537,#49538,#49539,#49540)) ;
#21623 = EDGE_LOOP('',(#49541,#49542,#49543,#49544)) ;
#21624 = EDGE_LOOP('',(#49545,#49546,#49547,#49548)) ;
#21625 = EDGE_LOOP('',(#49549,#49550,#49551,#49552)) ;
#21626 = EDGE_LOOP('',(#49553,#49554,#49555,#49556)) ;
#21627 = EDGE_LOOP('',(#49557,#49558,#49559,#49560)) ;
#21628 = EDGE_LOOP('',(#49561,#49562,#49563)) ;
#21629 = EDGE_LOOP('',(#49564,#49565,#49566,#49567)) ;
#21630 = EDGE_LOOP('',(#49568,#49569,#49570)) ;
#21631 = EDGE_LOOP('',(#49571,#49572,#49573,#49574)) ;
#21632 = EDGE_LOOP('',(#49575,#49576,#49577,#49578)) ;
#21633 = EDGE_LOOP('',(#49579,#49580,#49581,#49582)) ;
#21634 = EDGE_LOOP('',(#49583,#49584,#49585,#49586)) ;
#21635 = EDGE_LOOP('',(#49587,#49588,#49589,#49590)) ;
#21636 = EDGE_LOOP('',(#49591,#49592,#49593,#49594)) ;
#21637 = EDGE_LOOP('',(#49595,#49596,#49597,#49598)) ;
#21638 = EDGE_LOOP('',(#49599,#49600,#49601,#49602,#49603,#49604)) ;
#21639 = EDGE_LOOP('',(#49605,#49606,#49607)) ;
#21640 = EDGE_LOOP('',(#49608,#49609,#49610,#49611)) ;
#21641 = EDGE_LOOP('',(#49612,#49613,#49614,#49615)) ;
#21642 = EDGE_LOOP('',(#49616,#49617,#49618,#49619)) ;
#21643 = EDGE_LOOP('',(#49620,#49621,#49622,#49623)) ;
#21644 = EDGE_LOOP('',(#49624,#49625,#49626,#49627)) ;
#21645 = EDGE_LOOP('',(#49628,#49629,#49630,#49631)) ;
#21646 = EDGE_LOOP('',(#49632,#49633,#49634,#49635)) ;
#21647 = EDGE_LOOP('',(#49636,#49637,#49638,#49639,#49640)) ;
#21648 = EDGE_LOOP('',(#49641,#49642,#49643,#49644)) ;
#21649 = EDGE_LOOP('',(#49645,#49646,#49647,#49648,#49649)) ;
#21650 = EDGE_LOOP('',(#49650,#49651,#49652,#49653)) ;
#21651 = EDGE_LOOP('',(#49654,#49655,#49656,#49657,#49658)) ;
#21652 = EDGE_LOOP('',(#49659,#49660,#49661,#49662)) ;
#21653 = EDGE_LOOP('',(#49663,#49664,#49665)) ;
#21654 = EDGE_LOOP('',(#49666,#49667,#49668,#49669)) ;
#21655 = EDGE_LOOP('',(#49670,#49671,#49672,#49673)) ;
#21656 = EDGE_LOOP('',(#49674,#49675,#49676,#49677)) ;
#21657 = EDGE_LOOP('',(#49678,#49679,#49680,#49681)) ;
#21658 = EDGE_LOOP('',(#49682,#49683,#49684,#49685)) ;
#21659 = EDGE_LOOP('',(#49686,#49687,#49688)) ;
#21660 = EDGE_LOOP('',(#49689,#49690,#49691)) ;
#21661 = EDGE_LOOP('',(#49692,#49693,#49694,#49695)) ;
#21662 = EDGE_LOOP('',(#49696,#49697,#49698,#49699)) ;
#21663 = EDGE_LOOP('',(#49700,#49701,#49702)) ;
#21664 = EDGE_LOOP('',(#49703,#49704,#49705,#49706)) ;
#21665 = EDGE_LOOP('',(#49707,#49708,#49709,#49710)) ;
#21666 = EDGE_LOOP('',(#49711,#49712,#49713,#49714,#49715)) ;
#21667 = EDGE_LOOP('',(#49716,#49717,#49718,#49719)) ;
#21668 = EDGE_LOOP('',(#49720,#49721,#49722,#49723)) ;
#21669 = EDGE_LOOP('',(#49724,#49725,#49726,#49727)) ;
#21670 = EDGE_LOOP('',(#49728,#49729,#49730,#49731)) ;
#21671 = EDGE_LOOP('',(#49732,#49733,#49734,#49735)) ;
#21672 = EDGE_LOOP('',(#49736,#49737,#49738)) ;
#21673 = EDGE_LOOP('',(#49739,#49740,#49741,#49742)) ;
#21674 = EDGE_LOOP('',(#49743,#49744,#49745,#49746)) ;
#21675 = EDGE_LOOP('',(#49747,#49748,#49749)) ;
#21676 = EDGE_LOOP('',(#49750,#49751,#49752,#49753)) ;
#21677 = EDGE_LOOP('',(#49754,#49755,#49756,#49757)) ;
#21678 = EDGE_LOOP('',(#49758,#49759,#49760,#49761)) ;
#21679 = EDGE_LOOP('',(#49762,#49763,#49764,#49765)) ;
#21680 = EDGE_LOOP('',(#49766,#49767,#49768)) ;
#21681 = EDGE_LOOP('',(#49769,#49770,#49771)) ;
#21682 = EDGE_LOOP('',(#49772,#49773,#49774,#49775)) ;
#21683 = EDGE_LOOP('',(#49776,#49777,#49778,#49779)) ;
#21684 = EDGE_LOOP('',(#49780,#49781,#49782,#49783)) ;
#21685 = EDGE_LOOP('',(#49784,#49785,#49786)) ;
#21686 = EDGE_LOOP('',(#49787,#49788,#49789,#49790)) ;
#21687 = EDGE_LOOP('',(#49791,#49792,#49793,#49794)) ;
#21688 = EDGE_LOOP('',(#49795,#49796,#49797)) ;
#21689 = EDGE_LOOP('',(#49798,#49799,#49800,#49801)) ;
#21690 = EDGE_LOOP('',(#49802,#49803,#49804,#49805,#49806)) ;
#21691 = EDGE_LOOP('',(#49807,#49808,#49809,#49810)) ;
#21692 = EDGE_LOOP('',(#49811,#49812,#49813)) ;
#21693 = EDGE_LOOP('',(#49814,#49815,#49816,#49817)) ;
#21694 = EDGE_LOOP('',(#49818,#49819,#49820,#49821)) ;
#21695 = EDGE_LOOP('',(#49822,#49823,#49824)) ;
#21696 = EDGE_LOOP('',(#49825,#49826,#49827,#49828,#49829)) ;
#21697 = EDGE_LOOP('',(#49830,#49831,#49832,#49833)) ;
#21698 = EDGE_LOOP('',(#49834,#49835,#49836,#49837)) ;
#21699 = EDGE_LOOP('',(#49838,#49839,#49840,#49841)) ;
#21700 = EDGE_LOOP('',(#49842,#49843,#49844,#49845)) ;
#21701 = EDGE_LOOP('',(#49846,#49847,#49848,#49849)) ;
#21702 = EDGE_LOOP('',(#49850,#49851,#49852,#49853)) ;
#21703 = EDGE_LOOP('',(#49854,#49855,#49856,#49857)) ;
#21704 = EDGE_LOOP('',(#49858,#49859,#49860,#49861)) ;
#21705 = EDGE_LOOP('',(#49862,#49863,#49864,#49865,#49866)) ;
#21706 = EDGE_LOOP('',(#49867,#49868,#49869,#49870,#49871,#49872,#49873,#49874)) ;
#21707 = EDGE_LOOP('',(#49875,#49876,#49877)) ;
#21708 = EDGE_LOOP('',(#49878,#49879,#49880,#49881)) ;
#21709 = EDGE_LOOP('',(#49882,#49883,#49884,#49885,#49886)) ;
#21710 = EDGE_LOOP('',(#49887,#49888,#49889,#49890,#49891)) ;
#21711 = EDGE_LOOP('',(#49892,#49893,#49894,#49895)) ;
#21712 = EDGE_LOOP('',(#49896,#49897,#49898)) ;
#21713 = EDGE_LOOP('',(#49899,#49900,#49901,#49902,#49903,#49904,#49905,#49906)) ;
#21714 = EDGE_LOOP('',(#49907,#49908,#49909,#49910,#49911)) ;
#21715 = EDGE_LOOP('',(#49912,#49913,#49914,#49915,#49916)) ;
#21716 = EDGE_LOOP('',(#49917,#49918,#49919,#49920)) ;
#21717 = EDGE_LOOP('',(#49921,#49922,#49923,#49924,#49925,#49926,#49927,#49928)) ;
#21718 = EDGE_LOOP('',(#49929,#49930,#49931,#49932)) ;
#21719 = EDGE_LOOP('',(#49933,#49934,#49935,#49936,#49937,#49938,#49939,#49940)) ;
#21720 = EDGE_LOOP('',(#49941,#49942,#49943,#49944)) ;
#21721 = EDGE_LOOP('',(#49945,#49946,#49947,#49948)) ;
#21722 = EDGE_LOOP('',(#49949,#49950,#49951,#49952)) ;
#21723 = EDGE_LOOP('',(#49953,#49954,#49955,#49956)) ;
#21724 = EDGE_LOOP('',(#49957,#49958,#49959,#49960,#49961,#49962,#49963,#49964,
#49965)) ;
#21725 = EDGE_LOOP('',(#49966,#49967,#49968,#49969,#49970,#49971,#49972)) ;
#21726 = EDGE_LOOP('',(#49973,#49974,#49975,#49976)) ;
#21727 = EDGE_LOOP('',(#49977,#49978,#49979,#49980)) ;
#21728 = EDGE_LOOP('',(#49981,#49982,#49983,#49984)) ;
#21729 = EDGE_LOOP('',(#49985,#49986,#49987)) ;
#21730 = EDGE_LOOP('',(#49988,#49989,#49990,#49991)) ;
#21731 = EDGE_LOOP('',(#49992,#49993,#49994,#49995)) ;
#21732 = EDGE_LOOP('',(#49996,#49997,#49998,#49999)) ;
#21733 = EDGE_LOOP('',(#50000,#50001,#50002,#50003)) ;
#21734 = EDGE_LOOP('',(#50004,#50005,#50006,#50007)) ;
#21735 = EDGE_LOOP('',(#50008,#50009,#50010,#50011)) ;
#21736 = EDGE_LOOP('',(#50012,#50013,#50014,#50015)) ;
#21737 = EDGE_LOOP('',(#50016,#50017,#50018,#50019)) ;
#21738 = EDGE_LOOP('',(#50020,#50021,#50022,#50023)) ;
#21739 = EDGE_LOOP('',(#50024,#50025,#50026,#50027)) ;
#21740 = EDGE_LOOP('',(#50028,#50029,#50030,#50031)) ;
#21741 = EDGE_LOOP('',(#50032,#50033,#50034,#50035)) ;
#21742 = EDGE_LOOP('',(#50036,#50037,#50038,#50039)) ;
#21743 = EDGE_LOOP('',(#50040,#50041,#50042,#50043)) ;
#21744 = EDGE_LOOP('',(#50044,#50045,#50046,#50047)) ;
#21745 = EDGE_LOOP('',(#50048,#50049,#50050,#50051)) ;
#21746 = EDGE_LOOP('',(#50052,#50053,#50054,#50055)) ;
#21747 = EDGE_LOOP('',(#50056,#50057,#50058,#50059)) ;
#21748 = EDGE_LOOP('',(#50060,#50061,#50062,#50063)) ;
#21749 = EDGE_LOOP('',(#50064,#50065,#50066)) ;
#21750 = EDGE_LOOP('',(#50067,#50068,#50069,#50070)) ;
#21751 = EDGE_LOOP('',(#50071,#50072,#50073,#50074,#50075,#50076)) ;
#21752 = EDGE_LOOP('',(#50077,#50078,#50079,#50080)) ;
#21753 = EDGE_LOOP('',(#50081,#50082,#50083,#50084,#50085)) ;
#21754 = EDGE_LOOP('',(#50086,#50087,#50088,#50089)) ;
#21755 = EDGE_LOOP('',(#50090,#50091,#50092,#50093,#50094)) ;
#21756 = EDGE_LOOP('',(#50095,#50096,#50097,#50098,#50099)) ;
#21757 = EDGE_LOOP('',(#50100,#50101,#50102,#50103)) ;
#21758 = EDGE_LOOP('',(#50104,#50105,#50106,#50107)) ;
#21759 = EDGE_LOOP('',(#50108,#50109,#50110,#50111,#50112)) ;
#21760 = EDGE_LOOP('',(#50113,#50114,#50115,#50116)) ;
#21761 = EDGE_LOOP('',(#50117,#50118,#50119,#50120)) ;
#21762 = EDGE_LOOP('',(#50121,#50122,#50123,#50124)) ;
#21763 = EDGE_LOOP('',(#50125,#50126,#50127,#50128,#50129,#50130,#50131,#50132,
#50133,#50134)) ;
#21764 = EDGE_LOOP('',(#50135,#50136,#50137,#50138,#50139,#50140)) ;
#21765 = EDGE_LOOP('',(#50141,#50142,#50143,#50144,#50145,#50146)) ;
#21766 = EDGE_LOOP('',(#50147,#50148,#50149,#50150)) ;
#21767 = EDGE_LOOP('',(#50151,#50152,#50153,#50154,#50155,#50156)) ;
#21768 = EDGE_LOOP('',(#50157,#50158,#50159,#50160)) ;
#21769 = EDGE_LOOP('',(#50161,#50162,#50163,#50164)) ;
#21770 = EDGE_LOOP('',(#50165,#50166,#50167,#50168,#50169,#50170)) ;
#21771 = EDGE_LOOP('',(#50171,#50172,#50173,#50174,#50175,#50176,#50177,#50178,
#50179,#50180,#50181,#50182,#50183,#50184,#50185,#50186,#50187,#50188,#50189,
#50190,#50191,#50192,#50193,#50194,#50195,#50196,#50197,#50198,#50199,#50200,
#50201,#50202,#50203)) ;
#21772 = EDGE_LOOP('',(#50204,#50205,#50206,#50207,#50208,#50209,#50210,#50211,
#50212,#50213,#50214,#50215,#50216,#50217,#50218,#50219,#50220,#50221,#50222,
#50223,#50224,#50225,#50226,#50227,#50228,#50229,#50230,#50231,#50232,#50233,
#50234,#50235,#50236)) ;
#21773 = EDGE_LOOP('',(#50237,#50238,#50239,#50240)) ;
#21774 = EDGE_LOOP('',(#50241,#50242,#50243,#50244)) ;
#21775 = EDGE_LOOP('',(#50245,#50246,#50247,#50248,#50249,#50250,#50251,#50252)) ;
#21776 = EDGE_LOOP('',(#50253,#50254,#50255,#50256,#50257,#50258)) ;
#21777 = EDGE_LOOP('',(#50259,#50260,#50261,#50262)) ;
#21778 = EDGE_LOOP('',(#50263,#50264,#50265,#50266,#50267,#50268)) ;
#21779 = EDGE_LOOP('',(#50269,#50270,#50271,#50272,#50273,#50274,#50275,#50276,
#50277,#50278,#50279,#50280,#50281,#50282)) ;
#21780 = EDGE_LOOP('',(#50283,#50284,#50285,#50286,#50287,#50288,#50289,#50290,
#50291,#50292,#50293,#50294,#50295,#50296,#50297,#50298,#50299,#50300,#50301,
#50302,#50303,#50304,#50305,#50306)) ;
#21781 = EDGE_LOOP('',(#50307)) ;
#21782 = EDGE_LOOP('',(#50308,#50309,#50310,#50311,#50312,#50313,#50314,#50315,
#50316,#50317)) ;
#21783 = EDGE_LOOP('',(#50318,#50319,#50320,#50321,#50322,#50323,#50324,#50325,
#50326,#50327)) ;
#21784 = EDGE_LOOP('',(#50328,#50329,#50330)) ;
#21785 = EDGE_LOOP('',(#50331,#50332,#50333)) ;
#21786 = EDGE_LOOP('',(#50334,#50335,#50336,#50337,#50338,#50339,#50340,#50341)) ;
#21787 = EDGE_LOOP('',(#50342,#50343,#50344,#50345)) ;
#21788 = EDGE_LOOP('',(#50346,#50347,#50348,#50349)) ;
#21789 = EDGE_LOOP('',(#50350,#50351,#50352,#50353)) ;
#21790 = EDGE_LOOP('',(#50354,#50355,#50356,#50357,#50358,#50359)) ;
#21791 = EDGE_LOOP('',(#50360,#50361,#50362,#50363,#50364,#50365,#50366,#50367)) ;
#21792 = EDGE_LOOP('',(#50368)) ;
#21793 = EDGE_LOOP('',(#50369,#50370,#50371,#50372,#50373,#50374,#50375,#50376)) ;
#21794 = EDGE_LOOP('',(#50377,#50378,#50379,#50380,#50381,#50382,#50383)) ;
#21795 = EDGE_LOOP('',(#50384,#50385,#50386,#50387)) ;
#21796 = EDGE_LOOP('',(#50388,#50389,#50390,#50391)) ;
#21797 = EDGE_LOOP('',(#50392,#50393,#50394,#50395)) ;
#21798 = EDGE_LOOP('',(#50396,#50397,#50398,#50399)) ;
#21799 = EDGE_LOOP('',(#50400,#50401,#50402,#50403)) ;
#21800 = EDGE_LOOP('',(#50404,#50405,#50406,#50407)) ;
#21801 = EDGE_LOOP('',(#50408,#50409,#50410,#50411,#50412,#50413,#50414)) ;
#21802 = EDGE_LOOP('',(#50415,#50416,#50417,#50418,#50419)) ;
#21803 = EDGE_LOOP('',(#50420,#50421,#50422,#50423)) ;
#21804 = EDGE_LOOP('',(#50424,#50425,#50426,#50427)) ;
#21805 = EDGE_LOOP('',(#50428,#50429,#50430,#50431)) ;
#21806 = EDGE_LOOP('',(#50432,#50433,#50434,#50435)) ;
#21807 = EDGE_LOOP('',(#50436,#50437,#50438,#50439)) ;
#21808 = EDGE_LOOP('',(#50440,#50441,#50442,#50443)) ;
#21809 = EDGE_LOOP('',(#50444,#50445,#50446,#50447,#50448)) ;
#21810 = EDGE_LOOP('',(#50449,#50450,#50451,#50452)) ;
#21811 = EDGE_LOOP('',(#50453,#50454,#50455,#50456,#50457,#50458,#50459,#50460)) ;
#21812 = EDGE_LOOP('',(#50461,#50462,#50463,#50464)) ;
#21813 = EDGE_LOOP('',(#50465,#50466,#50467,#50468)) ;
#21814 = EDGE_LOOP('',(#50469,#50470,#50471,#50472)) ;
#21815 = EDGE_LOOP('',(#50473,#50474,#50475,#50476)) ;
#21816 = EDGE_LOOP('',(#50477,#50478,#50479,#50480)) ;
#21817 = EDGE_LOOP('',(#50481,#50482,#50483,#50484)) ;
#21818 = EDGE_LOOP('',(#50485,#50486,#50487,#50488)) ;
#21819 = EDGE_LOOP('',(#50489,#50490,#50491,#50492)) ;
#21820 = EDGE_LOOP('',(#50493,#50494,#50495,#50496,#50497,#50498)) ;
#21821 = EDGE_LOOP('',(#50499,#50500,#50501,#50502,#50503,#50504)) ;
#21822 = EDGE_LOOP('',(#50505,#50506,#50507,#50508)) ;
#21823 = EDGE_LOOP('',(#50509,#50510,#50511,#50512)) ;
#21824 = EDGE_LOOP('',(#50513,#50514,#50515,#50516)) ;
#21825 = EDGE_LOOP('',(#50517,#50518,#50519,#50520)) ;
#21826 = EDGE_LOOP('',(#50521,#50522,#50523,#50524)) ;
#21827 = EDGE_LOOP('',(#50525,#50526,#50527,#50528)) ;
#21828 = EDGE_LOOP('',(#50529,#50530,#50531,#50532)) ;
#21829 = EDGE_LOOP('',(#50533,#50534,#50535,#50536)) ;
#21830 = EDGE_LOOP('',(#50537,#50538,#50539,#50540)) ;
#21831 = EDGE_LOOP('',(#50541,#50542,#50543,#50544)) ;
#21832 = EDGE_LOOP('',(#50545,#50546,#50547,#50548)) ;
#21833 = EDGE_LOOP('',(#50549,#50550,#50551,#50552)) ;
#21834 = EDGE_LOOP('',(#50553,#50554,#50555,#50556)) ;
#21835 = EDGE_LOOP('',(#50557,#50558,#50559,#50560)) ;
#21836 = EDGE_LOOP('',(#50561,#50562,#50563,#50564)) ;
#21837 = EDGE_LOOP('',(#50565,#50566,#50567)) ;
#21838 = EDGE_LOOP('',(#50568,#50569,#50570,#50571)) ;
#21839 = EDGE_LOOP('',(#50572,#50573,#50574,#50575)) ;
#21840 = EDGE_LOOP('',(#50576,#50577,#50578,#50579)) ;
#21841 = EDGE_LOOP('',(#50580,#50581,#50582,#50583)) ;
#21842 = EDGE_LOOP('',(#50584,#50585,#50586)) ;
#21843 = EDGE_LOOP('',(#50587,#50588,#50589,#50590)) ;
#21844 = EDGE_LOOP('',(#50591,#50592,#50593,#50594)) ;
#21845 = EDGE_LOOP('',(#50595,#50596,#50597,#50598)) ;
#21846 = EDGE_LOOP('',(#50599,#50600,#50601,#50602)) ;
#21847 = EDGE_LOOP('',(#50603,#50604,#50605,#50606)) ;
#21848 = EDGE_LOOP('',(#50607,#50608,#50609,#50610)) ;
#21849 = EDGE_LOOP('',(#50611,#50612,#50613,#50614)) ;
#21850 = EDGE_LOOP('',(#50615,#50616,#50617)) ;
#21851 = EDGE_LOOP('',(#50618,#50619,#50620,#50621)) ;
#21852 = EDGE_LOOP('',(#50622,#50623,#50624,#50625)) ;
#21853 = EDGE_LOOP('',(#50626,#50627,#50628)) ;
#21854 = EDGE_LOOP('',(#50629,#50630,#50631,#50632)) ;
#21855 = EDGE_LOOP('',(#50633,#50634,#50635,#50636)) ;
#21856 = EDGE_LOOP('',(#50637,#50638,#50639,#50640)) ;
#21857 = EDGE_LOOP('',(#50641,#50642,#50643,#50644)) ;
#21858 = EDGE_LOOP('',(#50645,#50646,#50647,#50648)) ;
#21859 = EDGE_LOOP('',(#50649,#50650,#50651)) ;
#21860 = EDGE_LOOP('',(#50652,#50653,#50654,#50655)) ;
#21861 = EDGE_LOOP('',(#50656,#50657,#50658,#50659)) ;
#21862 = EDGE_LOOP('',(#50660,#50661,#50662,#50663)) ;
#21863 = EDGE_LOOP('',(#50664,#50665,#50666,#50667)) ;
#21864 = EDGE_LOOP('',(#50668,#50669,#50670,#50671)) ;
#21865 = EDGE_LOOP('',(#50672,#50673,#50674,#50675)) ;
#21866 = EDGE_LOOP('',(#50676,#50677,#50678)) ;
#21867 = EDGE_LOOP('',(#50679,#50680,#50681,#50682)) ;
#21868 = EDGE_LOOP('',(#50683,#50684,#50685,#50686)) ;
#21869 = EDGE_LOOP('',(#50687,#50688,#50689)) ;
#21870 = EDGE_LOOP('',(#50690,#50691,#50692,#50693,#50694)) ;
#21871 = EDGE_LOOP('',(#50695,#50696,#50697,#50698,#50699)) ;
#21872 = EDGE_LOOP('',(#50700,#50701,#50702,#50703)) ;
#21873 = EDGE_LOOP('',(#50704,#50705,#50706,#50707,#50708,#50709)) ;
#21874 = EDGE_LOOP('',(#50710,#50711,#50712,#50713,#50714,#50715)) ;
#21875 = EDGE_LOOP('',(#50716,#50717,#50718,#50719)) ;
#21876 = EDGE_LOOP('',(#50720,#50721,#50722,#50723)) ;
#21877 = EDGE_LOOP('',(#50724,#50725,#50726)) ;
#21878 = EDGE_LOOP('',(#50727,#50728,#50729,#50730,#50731)) ;
#21879 = EDGE_LOOP('',(#50732,#50733,#50734,#50735,#50736)) ;
#21880 = EDGE_LOOP('',(#50737,#50738,#50739,#50740)) ;
#21881 = EDGE_LOOP('',(#50741,#50742,#50743,#50744,#50745)) ;
#21882 = EDGE_LOOP('',(#50746,#50747,#50748,#50749)) ;
#21883 = EDGE_LOOP('',(#50750,#50751,#50752,#50753)) ;
#21884 = EDGE_LOOP('',(#50754,#50755,#50756)) ;
#21885 = EDGE_LOOP('',(#50757,#50758,#50759)) ;
#21886 = EDGE_LOOP('',(#50760,#50761,#50762,#50763,#50764)) ;
#21887 = EDGE_LOOP('',(#50765,#50766,#50767,#50768)) ;
#21888 = EDGE_LOOP('',(#50769,#50770,#50771)) ;
#21889 = EDGE_LOOP('',(#50772,#50773,#50774,#50775)) ;
#21890 = EDGE_LOOP('',(#50776,#50777,#50778,#50779)) ;
#21891 = EDGE_LOOP('',(#50780,#50781,#50782,#50783)) ;
#21892 = EDGE_LOOP('',(#50784,#50785,#50786,#50787)) ;
#21893 = EDGE_LOOP('',(#50788,#50789,#50790,#50791)) ;
#21894 = EDGE_LOOP('',(#50792,#50793,#50794,#50795)) ;
#21895 = EDGE_LOOP('',(#50796,#50797,#50798)) ;
#21896 = EDGE_LOOP('',(#50799,#50800,#50801,#50802)) ;
#21897 = EDGE_LOOP('',(#50803,#50804,#50805,#50806,#50807)) ;
#21898 = EDGE_LOOP('',(#50808,#50809,#50810,#50811)) ;
#21899 = EDGE_LOOP('',(#50812,#50813,#50814,#50815)) ;
#21900 = EDGE_LOOP('',(#50816,#50817,#50818,#50819,#50820)) ;
#21901 = EDGE_LOOP('',(#50821,#50822,#50823,#50824)) ;
#21902 = EDGE_LOOP('',(#50825,#50826,#50827)) ;
#21903 = EDGE_LOOP('',(#50828,#50829,#50830,#50831)) ;
#21904 = EDGE_LOOP('',(#50832,#50833,#50834,#50835)) ;
#21905 = EDGE_LOOP('',(#50836,#50837,#50838,#50839)) ;
#21906 = EDGE_LOOP('',(#50840,#50841,#50842,#50843)) ;
#21907 = EDGE_LOOP('',(#50844,#50845,#50846,#50847)) ;
#21908 = EDGE_LOOP('',(#50848,#50849,#50850,#50851)) ;
#21909 = EDGE_LOOP('',(#50852,#50853,#50854)) ;
#21910 = EDGE_LOOP('',(#50855,#50856,#50857,#50858)) ;
#21911 = EDGE_LOOP('',(#50859,#50860,#50861,#50862)) ;
#21912 = EDGE_LOOP('',(#50863,#50864,#50865,#50866)) ;
#21913 = EDGE_LOOP('',(#50867,#50868,#50869,#50870)) ;
#21914 = EDGE_LOOP('',(#50871,#50872,#50873,#50874)) ;
#21915 = EDGE_LOOP('',(#50875,#50876,#50877,#50878)) ;
#21916 = EDGE_LOOP('',(#50879,#50880,#50881,#50882)) ;
#21917 = EDGE_LOOP('',(#50883,#50884,#50885,#50886)) ;
#21918 = EDGE_LOOP('',(#50887,#50888,#50889,#50890)) ;
#21919 = EDGE_LOOP('',(#50891,#50892,#50893)) ;
#21920 = EDGE_LOOP('',(#50894,#50895,#50896,#50897)) ;
#21921 = EDGE_LOOP('',(#50898,#50899,#50900)) ;
#21922 = EDGE_LOOP('',(#50901,#50902,#50903,#50904)) ;
#21923 = EDGE_LOOP('',(#50905,#50906,#50907,#50908)) ;
#21924 = EDGE_LOOP('',(#50909,#50910,#50911,#50912)) ;
#21925 = EDGE_LOOP('',(#50913,#50914,#50915,#50916)) ;
#21926 = EDGE_LOOP('',(#50917,#50918,#50919,#50920)) ;
#21927 = EDGE_LOOP('',(#50921,#50922,#50923,#50924)) ;
#21928 = EDGE_LOOP('',(#50925,#50926,#50927,#50928)) ;
#21929 = EDGE_LOOP('',(#50929,#50930,#50931,#50932,#50933,#50934)) ;
#21930 = EDGE_LOOP('',(#50935,#50936,#50937)) ;
#21931 = EDGE_LOOP('',(#50938,#50939,#50940,#50941)) ;
#21932 = EDGE_LOOP('',(#50942,#50943,#50944,#50945)) ;
#21933 = EDGE_LOOP('',(#50946,#50947,#50948,#50949)) ;
#21934 = EDGE_LOOP('',(#50950,#50951,#50952,#50953)) ;
#21935 = EDGE_LOOP('',(#50954,#50955,#50956,#50957)) ;
#21936 = EDGE_LOOP('',(#50958,#50959,#50960,#50961)) ;
#21937 = EDGE_LOOP('',(#50962,#50963,#50964,#50965)) ;
#21938 = EDGE_LOOP('',(#50966,#50967,#50968,#50969,#50970)) ;
#21939 = EDGE_LOOP('',(#50971,#50972,#50973,#50974)) ;
#21940 = EDGE_LOOP('',(#50975,#50976,#50977,#50978,#50979)) ;
#21941 = EDGE_LOOP('',(#50980,#50981,#50982,#50983)) ;
#21942 = EDGE_LOOP('',(#50984,#50985,#50986,#50987,#50988)) ;
#21943 = EDGE_LOOP('',(#50989,#50990,#50991,#50992)) ;
#21944 = EDGE_LOOP('',(#50993,#50994,#50995)) ;
#21945 = EDGE_LOOP('',(#50996,#50997,#50998,#50999)) ;
#21946 = EDGE_LOOP('',(#51000,#51001,#51002,#51003)) ;
#21947 = EDGE_LOOP('',(#51004,#51005,#51006,#51007)) ;
#21948 = EDGE_LOOP('',(#51008,#51009,#51010,#51011)) ;
#21949 = EDGE_LOOP('',(#51012,#51013,#51014,#51015)) ;
#21950 = EDGE_LOOP('',(#51016,#51017,#51018)) ;
#21951 = EDGE_LOOP('',(#51019,#51020,#51021)) ;
#21952 = EDGE_LOOP('',(#51022,#51023,#51024,#51025)) ;
#21953 = EDGE_LOOP('',(#51026,#51027,#51028,#51029)) ;
#21954 = EDGE_LOOP('',(#51030,#51031,#51032)) ;
#21955 = EDGE_LOOP('',(#51033,#51034,#51035,#51036)) ;
#21956 = EDGE_LOOP('',(#51037,#51038,#51039,#51040)) ;
#21957 = EDGE_LOOP('',(#51041,#51042,#51043,#51044,#51045)) ;
#21958 = EDGE_LOOP('',(#51046,#51047,#51048,#51049)) ;
#21959 = EDGE_LOOP('',(#51050,#51051,#51052,#51053)) ;
#21960 = EDGE_LOOP('',(#51054,#51055,#51056,#51057)) ;
#21961 = EDGE_LOOP('',(#51058,#51059,#51060,#51061)) ;
#21962 = EDGE_LOOP('',(#51062,#51063,#51064,#51065)) ;
#21963 = EDGE_LOOP('',(#51066,#51067,#51068)) ;
#21964 = EDGE_LOOP('',(#51069,#51070,#51071,#51072)) ;
#21965 = EDGE_LOOP('',(#51073,#51074,#51075,#51076)) ;
#21966 = EDGE_LOOP('',(#51077,#51078,#51079)) ;
#21967 = EDGE_LOOP('',(#51080,#51081,#51082,#51083)) ;
#21968 = EDGE_LOOP('',(#51084,#51085,#51086,#51087)) ;
#21969 = EDGE_LOOP('',(#51088,#51089,#51090,#51091)) ;
#21970 = EDGE_LOOP('',(#51092,#51093,#51094,#51095)) ;
#21971 = EDGE_LOOP('',(#51096,#51097,#51098)) ;
#21972 = EDGE_LOOP('',(#51099,#51100,#51101)) ;
#21973 = EDGE_LOOP('',(#51102,#51103,#51104,#51105)) ;
#21974 = EDGE_LOOP('',(#51106,#51107,#51108,#51109)) ;
#21975 = EDGE_LOOP('',(#51110,#51111,#51112,#51113)) ;
#21976 = EDGE_LOOP('',(#51114,#51115,#51116)) ;
#21977 = EDGE_LOOP('',(#51117,#51118,#51119,#51120)) ;
#21978 = EDGE_LOOP('',(#51121,#51122,#51123,#51124)) ;
#21979 = EDGE_LOOP('',(#51125,#51126,#51127)) ;
#21980 = EDGE_LOOP('',(#51128,#51129,#51130,#51131)) ;
#21981 = EDGE_LOOP('',(#51132,#51133,#51134,#51135,#51136)) ;
#21982 = EDGE_LOOP('',(#51137,#51138,#51139,#51140)) ;
#21983 = EDGE_LOOP('',(#51141,#51142,#51143)) ;
#21984 = EDGE_LOOP('',(#51144,#51145,#51146,#51147)) ;
#21985 = EDGE_LOOP('',(#51148,#51149,#51150,#51151)) ;
#21986 = EDGE_LOOP('',(#51152,#51153,#51154)) ;
#21987 = EDGE_LOOP('',(#51155,#51156,#51157,#51158,#51159)) ;
#21988 = EDGE_LOOP('',(#51160,#51161,#51162,#51163)) ;
#21989 = EDGE_LOOP('',(#51164,#51165,#51166,#51167)) ;
#21990 = EDGE_LOOP('',(#51168,#51169,#51170,#51171)) ;
#21991 = EDGE_LOOP('',(#51172,#51173,#51174,#51175)) ;
#21992 = EDGE_LOOP('',(#51176,#51177,#51178,#51179)) ;
#21993 = EDGE_LOOP('',(#51180,#51181,#51182,#51183)) ;
#21994 = EDGE_LOOP('',(#51184,#51185,#51186,#51187)) ;
#21995 = EDGE_LOOP('',(#51188,#51189,#51190,#51191)) ;
#21996 = EDGE_LOOP('',(#51192,#51193,#51194,#51195,#51196)) ;
#21997 = EDGE_LOOP('',(#51197,#51198,#51199,#51200,#51201,#51202,#51203,#51204)) ;
#21998 = EDGE_LOOP('',(#51205,#51206,#51207)) ;
#21999 = EDGE_LOOP('',(#51208,#51209,#51210,#51211)) ;
#22000 = EDGE_LOOP('',(#51212,#51213,#51214,#51215,#51216)) ;
#22001 = EDGE_LOOP('',(#51217,#51218,#51219,#51220,#51221)) ;
#22002 = EDGE_LOOP('',(#51222,#51223,#51224,#51225)) ;
#22003 = EDGE_LOOP('',(#51226,#51227,#51228)) ;
#22004 = EDGE_LOOP('',(#51229,#51230,#51231,#51232,#51233,#51234,#51235,#51236)) ;
#22005 = EDGE_LOOP('',(#51237,#51238,#51239,#51240,#51241)) ;
#22006 = EDGE_LOOP('',(#51242,#51243,#51244,#51245,#51246)) ;
#22007 = EDGE_LOOP('',(#51247,#51248,#51249,#51250)) ;
#22008 = EDGE_LOOP('',(#51251,#51252,#51253,#51254,#51255,#51256,#51257,#51258)) ;
#22009 = EDGE_LOOP('',(#51259,#51260,#51261,#51262)) ;
#22010 = EDGE_LOOP('',(#51263,#51264,#51265,#51266,#51267,#51268,#51269,#51270)) ;
#22011 = EDGE_LOOP('',(#51271,#51272,#51273,#51274)) ;
#22012 = EDGE_LOOP('',(#51275,#51276,#51277,#51278)) ;
#22013 = EDGE_LOOP('',(#51279,#51280,#51281,#51282)) ;
#22014 = EDGE_LOOP('',(#51283,#51284,#51285,#51286)) ;
#22015 = EDGE_LOOP('',(#51287,#51288,#51289,#51290,#51291,#51292,#51293,#51294,
#51295)) ;
#22016 = EDGE_LOOP('',(#51296,#51297,#51298,#51299,#51300,#51301,#51302)) ;
#22017 = EDGE_LOOP('',(#51303,#51304,#51305,#51306)) ;
#22018 = EDGE_LOOP('',(#51307,#51308,#51309,#51310)) ;
#22019 = EDGE_LOOP('',(#51311,#51312,#51313,#51314)) ;
#22020 = EDGE_LOOP('',(#51315,#51316,#51317)) ;
#22021 = EDGE_LOOP('',(#51318,#51319,#51320,#51321)) ;
#22022 = EDGE_LOOP('',(#51322,#51323,#51324,#51325)) ;
#22023 = EDGE_LOOP('',(#51326,#51327,#51328,#51329)) ;
#22024 = EDGE_LOOP('',(#51330,#51331,#51332,#51333)) ;
#22025 = EDGE_LOOP('',(#51334,#51335,#51336,#51337)) ;
#22026 = EDGE_LOOP('',(#51338,#51339,#51340,#51341)) ;
#22027 = EDGE_LOOP('',(#51342,#51343,#51344,#51345)) ;
#22028 = EDGE_LOOP('',(#51346,#51347,#51348,#51349)) ;
#22029 = EDGE_LOOP('',(#51350,#51351,#51352,#51353)) ;
#22030 = EDGE_LOOP('',(#51354,#51355,#51356,#51357)) ;
#22031 = EDGE_LOOP('',(#51358,#51359,#51360,#51361)) ;
#22032 = EDGE_LOOP('',(#51362,#51363,#51364,#51365)) ;
#22033 = EDGE_LOOP('',(#51366,#51367,#51368,#51369)) ;
#22034 = EDGE_LOOP('',(#51370,#51371,#51372,#51373)) ;
#22035 = EDGE_LOOP('',(#51374,#51375,#51376,#51377)) ;
#22036 = EDGE_LOOP('',(#51378,#51379,#51380,#51381)) ;
#22037 = EDGE_LOOP('',(#51382,#51383,#51384,#51385)) ;
#22038 = EDGE_LOOP('',(#51386,#51387,#51388,#51389)) ;
#22039 = EDGE_LOOP('',(#51390,#51391,#51392,#51393)) ;
#22040 = EDGE_LOOP('',(#51394,#51395,#51396)) ;
#22041 = EDGE_LOOP('',(#51397,#51398,#51399,#51400)) ;
#22042 = EDGE_LOOP('',(#51401,#51402,#51403,#51404,#51405,#51406)) ;
#22043 = EDGE_LOOP('',(#51407,#51408,#51409,#51410)) ;
#22044 = EDGE_LOOP('',(#51411,#51412,#51413,#51414,#51415)) ;
#22045 = EDGE_LOOP('',(#51416,#51417,#51418,#51419)) ;
#22046 = EDGE_LOOP('',(#51420,#51421,#51422,#51423,#51424)) ;
#22047 = EDGE_LOOP('',(#51425,#51426,#51427,#51428,#51429)) ;
#22048 = EDGE_LOOP('',(#51430,#51431,#51432,#51433)) ;
#22049 = EDGE_LOOP('',(#51434,#51435,#51436,#51437)) ;
#22050 = EDGE_LOOP('',(#51438,#51439,#51440,#51441,#51442)) ;
#22051 = EDGE_LOOP('',(#51443,#51444,#51445,#51446)) ;
#22052 = EDGE_LOOP('',(#51447,#51448,#51449,#51450)) ;
#22053 = EDGE_LOOP('',(#51451,#51452,#51453,#51454)) ;
#22054 = EDGE_LOOP('',(#51455,#51456,#51457,#51458,#51459,#51460,#51461,#51462,
#51463,#51464)) ;
#22055 = EDGE_LOOP('',(#51465,#51466,#51467,#51468,#51469,#51470)) ;
#22056 = EDGE_LOOP('',(#51471,#51472,#51473,#51474,#51475,#51476)) ;
#22057 = EDGE_LOOP('',(#51477,#51478,#51479,#51480)) ;
#22058 = EDGE_LOOP('',(#51481,#51482,#51483,#51484,#51485,#51486)) ;
#22059 = EDGE_LOOP('',(#51487,#51488,#51489,#51490)) ;
#22060 = EDGE_LOOP('',(#51491,#51492,#51493,#51494)) ;
#22061 = EDGE_LOOP('',(#51495,#51496,#51497,#51498,#51499,#51500)) ;
#22062 = EDGE_LOOP('',(#51501,#51502,#51503,#51504,#51505,#51506,#51507,#51508,
#51509,#51510,#51511,#51512,#51513,#51514,#51515,#51516,#51517,#51518,#51519,
#51520,#51521,#51522,#51523,#51524,#51525,#51526,#51527,#51528,#51529,#51530,
#51531,#51532,#51533)) ;
#22063 = EDGE_LOOP('',(#51534,#51535,#51536,#51537,#51538,#51539,#51540,#51541,
#51542,#51543,#51544,#51545,#51546,#51547,#51548,#51549,#51550,#51551,#51552,
#51553,#51554,#51555,#51556,#51557,#51558,#51559,#51560,#51561,#51562,#51563,
#51564,#51565,#51566)) ;
#22064 = EDGE_LOOP('',(#51567,#51568,#51569,#51570)) ;
#22065 = EDGE_LOOP('',(#51571,#51572,#51573,#51574)) ;
#22066 = EDGE_LOOP('',(#51575,#51576,#51577,#51578,#51579,#51580,#51581,#51582)) ;
#22067 = EDGE_LOOP('',(#51583,#51584,#51585,#51586,#51587,#51588)) ;
#22068 = EDGE_LOOP('',(#51589,#51590,#51591,#51592)) ;
#22069 = EDGE_LOOP('',(#51593,#51594,#51595,#51596,#51597,#51598)) ;
#22070 = EDGE_LOOP('',(#51599,#51600,#51601,#51602,#51603,#51604,#51605,#51606,
#51607,#51608,#51609,#51610,#51611,#51612)) ;
#22071 = EDGE_LOOP('',(#51613,#51614,#51615,#51616,#51617,#51618,#51619,#51620,
#51621,#51622,#51623,#51624,#51625,#51626,#51627,#51628,#51629,#51630,#51631,
#51632,#51633,#51634,#51635,#51636)) ;
#22072 = EDGE_LOOP('',(#51637)) ;
#22073 = EDGE_LOOP('',(#51638,#51639,#51640,#51641,#51642,#51643,#51644,#51645,
#51646,#51647)) ;
#22074 = EDGE_LOOP('',(#51648,#51649,#51650,#51651,#51652,#51653,#51654,#51655,
#51656,#51657)) ;
#22075 = EDGE_LOOP('',(#51658,#51659,#51660)) ;
#22076 = EDGE_LOOP('',(#51661,#51662,#51663)) ;
#22077 = EDGE_LOOP('',(#51664,#51665,#51666,#51667,#51668,#51669,#51670,#51671)) ;
#22078 = EDGE_LOOP('',(#51672,#51673,#51674,#51675)) ;
#22079 = EDGE_LOOP('',(#51676,#51677,#51678,#51679)) ;
#22080 = EDGE_LOOP('',(#51680,#51681,#51682,#51683)) ;
#22081 = EDGE_LOOP('',(#51684,#51685,#51686,#51687,#51688,#51689)) ;
#22082 = EDGE_LOOP('',(#51690,#51691,#51692,#51693,#51694,#51695,#51696,#51697)) ;
#22083 = EDGE_LOOP('',(#51698)) ;
#22084 = EDGE_LOOP('',(#51699,#51700,#51701,#51702,#51703,#51704,#51705,#51706)) ;
#22085 = EDGE_LOOP('',(#51707,#51708,#51709,#51710,#51711,#51712,#51713)) ;
#22086 = EDGE_LOOP('',(#51714,#51715,#51716,#51717)) ;
#22087 = EDGE_LOOP('',(#51718,#51719,#51720,#51721)) ;
#22088 = EDGE_LOOP('',(#51722,#51723,#51724,#51725)) ;
#22089 = EDGE_LOOP('',(#51726,#51727,#51728,#51729)) ;
#22090 = EDGE_LOOP('',(#51730,#51731,#51732,#51733)) ;
#22091 = EDGE_LOOP('',(#51734,#51735,#51736,#51737)) ;
#22092 = EDGE_LOOP('',(#51738,#51739,#51740,#51741,#51742,#51743,#51744)) ;
#22093 = EDGE_LOOP('',(#51745,#51746,#51747,#51748,#51749)) ;
#22094 = EDGE_LOOP('',(#51750,#51751,#51752,#51753)) ;
#22095 = EDGE_LOOP('',(#51754,#51755,#51756,#51757)) ;
#22096 = EDGE_LOOP('',(#51758,#51759,#51760,#51761)) ;
#22097 = EDGE_LOOP('',(#51762,#51763,#51764,#51765)) ;
#22098 = EDGE_LOOP('',(#51766,#51767,#51768,#51769)) ;
#22099 = EDGE_LOOP('',(#51770,#51771,#51772,#51773)) ;
#22100 = EDGE_LOOP('',(#51774,#51775,#51776,#51777,#51778)) ;
#22101 = EDGE_LOOP('',(#51779,#51780,#51781,#51782)) ;
#22102 = EDGE_LOOP('',(#51783,#51784,#51785,#51786,#51787,#51788,#51789,#51790)) ;
#22103 = EDGE_LOOP('',(#51791,#51792,#51793,#51794)) ;
#22104 = EDGE_LOOP('',(#51795,#51796,#51797,#51798)) ;
#22105 = EDGE_LOOP('',(#51799,#51800,#51801,#51802)) ;
#22106 = EDGE_LOOP('',(#51803,#51804,#51805,#51806)) ;
#22107 = EDGE_LOOP('',(#51807,#51808,#51809,#51810)) ;
#22108 = EDGE_LOOP('',(#51811,#51812,#51813,#51814)) ;
#22109 = EDGE_LOOP('',(#51815,#51816,#51817,#51818)) ;
#22110 = EDGE_LOOP('',(#51819,#51820,#51821,#51822)) ;
#22111 = EDGE_LOOP('',(#51823,#51824,#51825,#51826,#51827,#51828)) ;
#22112 = EDGE_LOOP('',(#51829,#51830,#51831,#51832,#51833,#51834)) ;
#22113 = EDGE_LOOP('',(#51835,#51836,#51837,#51838)) ;
#22114 = EDGE_LOOP('',(#51839,#51840,#51841,#51842)) ;
#22115 = EDGE_LOOP('',(#51843,#51844,#51845,#51846)) ;
#22116 = EDGE_LOOP('',(#51847,#51848,#51849,#51850)) ;
#22117 = EDGE_LOOP('',(#51851,#51852,#51853,#51854)) ;
#22118 = EDGE_LOOP('',(#51855,#51856,#51857,#51858)) ;
#22119 = EDGE_LOOP('',(#51859,#51860,#51861,#51862)) ;
#22120 = EDGE_LOOP('',(#51863,#51864,#51865,#51866)) ;
#22121 = EDGE_LOOP('',(#51867,#51868,#51869,#51870)) ;
#22122 = EDGE_LOOP('',(#51871,#51872,#51873,#51874)) ;
#22123 = EDGE_LOOP('',(#51875,#51876,#51877,#51878)) ;
#22124 = EDGE_LOOP('',(#51879,#51880,#51881,#51882)) ;
#22125 = EDGE_LOOP('',(#51883,#51884,#51885,#51886)) ;
#22126 = EDGE_LOOP('',(#51887,#51888,#51889,#51890)) ;
#22127 = EDGE_LOOP('',(#51891,#51892,#51893,#51894)) ;
#22128 = EDGE_LOOP('',(#51895,#51896,#51897)) ;
#22129 = EDGE_LOOP('',(#51898,#51899,#51900,#51901)) ;
#22130 = EDGE_LOOP('',(#51902,#51903,#51904,#51905)) ;
#22131 = EDGE_LOOP('',(#51906,#51907,#51908,#51909)) ;
#22132 = EDGE_LOOP('',(#51910,#51911,#51912,#51913)) ;
#22133 = EDGE_LOOP('',(#51914,#51915,#51916)) ;
#22134 = EDGE_LOOP('',(#51917,#51918,#51919,#51920)) ;
#22135 = EDGE_LOOP('',(#51921,#51922,#51923,#51924)) ;
#22136 = EDGE_LOOP('',(#51925,#51926,#51927,#51928)) ;
#22137 = EDGE_LOOP('',(#51929,#51930,#51931,#51932)) ;
#22138 = EDGE_LOOP('',(#51933,#51934,#51935,#51936)) ;
#22139 = EDGE_LOOP('',(#51937,#51938,#51939,#51940)) ;
#22140 = EDGE_LOOP('',(#51941,#51942,#51943,#51944)) ;
#22141 = EDGE_LOOP('',(#51945,#51946,#51947)) ;
#22142 = EDGE_LOOP('',(#51948,#51949,#51950,#51951)) ;
#22143 = EDGE_LOOP('',(#51952,#51953,#51954,#51955)) ;
#22144 = EDGE_LOOP('',(#51956,#51957,#51958)) ;
#22145 = EDGE_LOOP('',(#51959,#51960,#51961,#51962)) ;
#22146 = EDGE_LOOP('',(#51963,#51964,#51965,#51966)) ;
#22147 = EDGE_LOOP('',(#51967,#51968,#51969,#51970)) ;
#22148 = EDGE_LOOP('',(#51971,#51972,#51973,#51974)) ;
#22149 = EDGE_LOOP('',(#51975,#51976,#51977,#51978)) ;
#22150 = EDGE_LOOP('',(#51979,#51980,#51981)) ;
#22151 = EDGE_LOOP('',(#51982,#51983,#51984,#51985)) ;
#22152 = EDGE_LOOP('',(#51986,#51987,#51988,#51989)) ;
#22153 = EDGE_LOOP('',(#51990,#51991,#51992,#51993)) ;
#22154 = EDGE_LOOP('',(#51994,#51995,#51996,#51997)) ;
#22155 = EDGE_LOOP('',(#51998,#51999,#52000,#52001)) ;
#22156 = EDGE_LOOP('',(#52002,#52003,#52004,#52005)) ;
#22157 = EDGE_LOOP('',(#52006,#52007,#52008)) ;
#22158 = EDGE_LOOP('',(#52009,#52010,#52011,#52012)) ;
#22159 = EDGE_LOOP('',(#52013,#52014,#52015,#52016)) ;
#22160 = EDGE_LOOP('',(#52017,#52018,#52019)) ;
#22161 = EDGE_LOOP('',(#52020,#52021,#52022,#52023,#52024)) ;
#22162 = EDGE_LOOP('',(#52025,#52026,#52027,#52028,#52029)) ;
#22163 = EDGE_LOOP('',(#52030,#52031,#52032,#52033)) ;
#22164 = EDGE_LOOP('',(#52034,#52035,#52036,#52037,#52038,#52039)) ;
#22165 = EDGE_LOOP('',(#52040,#52041,#52042,#52043,#52044,#52045)) ;
#22166 = EDGE_LOOP('',(#52046,#52047,#52048,#52049)) ;
#22167 = EDGE_LOOP('',(#52050,#52051,#52052,#52053)) ;
#22168 = EDGE_LOOP('',(#52054,#52055,#52056)) ;
#22169 = EDGE_LOOP('',(#52057,#52058,#52059,#52060,#52061)) ;
#22170 = EDGE_LOOP('',(#52062,#52063,#52064,#52065,#52066)) ;
#22171 = EDGE_LOOP('',(#52067,#52068,#52069,#52070)) ;
#22172 = EDGE_LOOP('',(#52071,#52072,#52073,#52074,#52075)) ;
#22173 = EDGE_LOOP('',(#52076,#52077,#52078,#52079)) ;
#22174 = EDGE_LOOP('',(#52080,#52081,#52082,#52083)) ;
#22175 = EDGE_LOOP('',(#52084,#52085,#52086)) ;
#22176 = EDGE_LOOP('',(#52087,#52088,#52089)) ;
#22177 = EDGE_LOOP('',(#52090,#52091,#52092,#52093,#52094)) ;
#22178 = EDGE_LOOP('',(#52095,#52096,#52097,#52098)) ;
#22179 = EDGE_LOOP('',(#52099,#52100,#52101)) ;
#22180 = EDGE_LOOP('',(#52102,#52103,#52104,#52105)) ;
#22181 = EDGE_LOOP('',(#52106,#52107,#52108,#52109)) ;
#22182 = EDGE_LOOP('',(#52110,#52111,#52112,#52113)) ;
#22183 = EDGE_LOOP('',(#52114,#52115,#52116,#52117)) ;
#22184 = EDGE_LOOP('',(#52118,#52119,#52120,#52121)) ;
#22185 = EDGE_LOOP('',(#52122,#52123,#52124,#52125)) ;
#22186 = EDGE_LOOP('',(#52126,#52127,#52128)) ;
#22187 = EDGE_LOOP('',(#52129,#52130,#52131,#52132)) ;
#22188 = EDGE_LOOP('',(#52133,#52134,#52135,#52136,#52137)) ;
#22189 = EDGE_LOOP('',(#52138,#52139,#52140,#52141)) ;
#22190 = EDGE_LOOP('',(#52142,#52143,#52144,#52145)) ;
#22191 = EDGE_LOOP('',(#52146,#52147,#52148,#52149,#52150)) ;
#22192 = EDGE_LOOP('',(#52151,#52152,#52153,#52154)) ;
#22193 = EDGE_LOOP('',(#52155,#52156,#52157)) ;
#22194 = EDGE_LOOP('',(#52158,#52159,#52160,#52161)) ;
#22195 = EDGE_LOOP('',(#52162,#52163,#52164,#52165)) ;
#22196 = EDGE_LOOP('',(#52166,#52167,#52168,#52169)) ;
#22197 = EDGE_LOOP('',(#52170,#52171,#52172,#52173)) ;
#22198 = EDGE_LOOP('',(#52174,#52175,#52176,#52177)) ;
#22199 = EDGE_LOOP('',(#52178,#52179,#52180,#52181)) ;
#22200 = EDGE_LOOP('',(#52182,#52183,#52184)) ;
#22201 = EDGE_LOOP('',(#52185,#52186,#52187,#52188)) ;
#22202 = EDGE_LOOP('',(#52189,#52190,#52191,#52192)) ;
#22203 = EDGE_LOOP('',(#52193,#52194,#52195,#52196)) ;
#22204 = EDGE_LOOP('',(#52197,#52198,#52199,#52200)) ;
#22205 = EDGE_LOOP('',(#52201,#52202,#52203,#52204)) ;
#22206 = EDGE_LOOP('',(#52205,#52206,#52207,#52208)) ;
#22207 = EDGE_LOOP('',(#52209,#52210,#52211,#52212)) ;
#22208 = EDGE_LOOP('',(#52213,#52214,#52215,#52216)) ;
#22209 = EDGE_LOOP('',(#52217,#52218,#52219,#52220)) ;
#22210 = EDGE_LOOP('',(#52221,#52222,#52223)) ;
#22211 = EDGE_LOOP('',(#52224,#52225,#52226,#52227)) ;
#22212 = EDGE_LOOP('',(#52228,#52229,#52230)) ;
#22213 = EDGE_LOOP('',(#52231,#52232,#52233,#52234)) ;
#22214 = EDGE_LOOP('',(#52235,#52236,#52237,#52238)) ;
#22215 = EDGE_LOOP('',(#52239,#52240,#52241,#52242)) ;
#22216 = EDGE_LOOP('',(#52243,#52244,#52245,#52246)) ;
#22217 = EDGE_LOOP('',(#52247,#52248,#52249,#52250)) ;
#22218 = EDGE_LOOP('',(#52251,#52252,#52253,#52254)) ;
#22219 = EDGE_LOOP('',(#52255,#52256,#52257,#52258)) ;
#22220 = EDGE_LOOP('',(#52259,#52260,#52261,#52262,#52263,#52264)) ;
#22221 = EDGE_LOOP('',(#52265,#52266,#52267)) ;
#22222 = EDGE_LOOP('',(#52268,#52269,#52270,#52271)) ;
#22223 = EDGE_LOOP('',(#52272,#52273,#52274,#52275)) ;
#22224 = EDGE_LOOP('',(#52276,#52277,#52278,#52279)) ;
#22225 = EDGE_LOOP('',(#52280,#52281,#52282,#52283)) ;
#22226 = EDGE_LOOP('',(#52284,#52285,#52286,#52287)) ;
#22227 = EDGE_LOOP('',(#52288,#52289,#52290,#52291)) ;
#22228 = EDGE_LOOP('',(#52292,#52293,#52294,#52295)) ;
#22229 = EDGE_LOOP('',(#52296,#52297,#52298,#52299,#52300)) ;
#22230 = EDGE_LOOP('',(#52301,#52302,#52303,#52304)) ;
#22231 = EDGE_LOOP('',(#52305,#52306,#52307,#52308,#52309)) ;
#22232 = EDGE_LOOP('',(#52310,#52311,#52312,#52313)) ;
#22233 = EDGE_LOOP('',(#52314,#52315,#52316,#52317,#52318)) ;
#22234 = EDGE_LOOP('',(#52319,#52320,#52321,#52322)) ;
#22235 = EDGE_LOOP('',(#52323,#52324,#52325)) ;
#22236 = EDGE_LOOP('',(#52326,#52327,#52328,#52329)) ;
#22237 = EDGE_LOOP('',(#52330,#52331,#52332,#52333)) ;
#22238 = EDGE_LOOP('',(#52334,#52335,#52336,#52337)) ;
#22239 = EDGE_LOOP('',(#52338,#52339,#52340,#52341)) ;
#22240 = EDGE_LOOP('',(#52342,#52343,#52344,#52345)) ;
#22241 = EDGE_LOOP('',(#52346,#52347,#52348)) ;
#22242 = EDGE_LOOP('',(#52349,#52350,#52351)) ;
#22243 = EDGE_LOOP('',(#52352,#52353,#52354,#52355)) ;
#22244 = EDGE_LOOP('',(#52356,#52357,#52358,#52359)) ;
#22245 = EDGE_LOOP('',(#52360,#52361,#52362)) ;
#22246 = EDGE_LOOP('',(#52363,#52364,#52365,#52366)) ;
#22247 = EDGE_LOOP('',(#52367,#52368,#52369,#52370)) ;
#22248 = EDGE_LOOP('',(#52371,#52372,#52373,#52374,#52375)) ;
#22249 = EDGE_LOOP('',(#52376,#52377,#52378,#52379)) ;
#22250 = EDGE_LOOP('',(#52380,#52381,#52382,#52383)) ;
#22251 = EDGE_LOOP('',(#52384,#52385,#52386,#52387)) ;
#22252 = EDGE_LOOP('',(#52388,#52389,#52390,#52391)) ;
#22253 = EDGE_LOOP('',(#52392,#52393,#52394,#52395)) ;
#22254 = EDGE_LOOP('',(#52396,#52397,#52398)) ;
#22255 = EDGE_LOOP('',(#52399,#52400,#52401,#52402)) ;
#22256 = EDGE_LOOP('',(#52403,#52404,#52405,#52406)) ;
#22257 = EDGE_LOOP('',(#52407,#52408,#52409)) ;
#22258 = EDGE_LOOP('',(#52410,#52411,#52412,#52413)) ;
#22259 = EDGE_LOOP('',(#52414,#52415,#52416,#52417)) ;
#22260 = EDGE_LOOP('',(#52418,#52419,#52420,#52421)) ;
#22261 = EDGE_LOOP('',(#52422,#52423,#52424,#52425)) ;
#22262 = EDGE_LOOP('',(#52426,#52427,#52428)) ;
#22263 = EDGE_LOOP('',(#52429,#52430,#52431)) ;
#22264 = EDGE_LOOP('',(#52432,#52433,#52434,#52435)) ;
#22265 = EDGE_LOOP('',(#52436,#52437,#52438,#52439)) ;
#22266 = EDGE_LOOP('',(#52440,#52441,#52442,#52443)) ;
#22267 = EDGE_LOOP('',(#52444,#52445,#52446)) ;
#22268 = EDGE_LOOP('',(#52447,#52448,#52449,#52450)) ;
#22269 = EDGE_LOOP('',(#52451,#52452,#52453,#52454)) ;
#22270 = EDGE_LOOP('',(#52455,#52456,#52457)) ;
#22271 = EDGE_LOOP('',(#52458,#52459,#52460,#52461)) ;
#22272 = EDGE_LOOP('',(#52462,#52463,#52464,#52465,#52466)) ;
#22273 = EDGE_LOOP('',(#52467,#52468,#52469,#52470)) ;
#22274 = EDGE_LOOP('',(#52471,#52472,#52473)) ;
#22275 = EDGE_LOOP('',(#52474,#52475,#52476,#52477)) ;
#22276 = EDGE_LOOP('',(#52478,#52479,#52480,#52481)) ;
#22277 = EDGE_LOOP('',(#52482,#52483,#52484)) ;
#22278 = EDGE_LOOP('',(#52485,#52486,#52487,#52488,#52489)) ;
#22279 = EDGE_LOOP('',(#52490,#52491,#52492,#52493)) ;
#22280 = EDGE_LOOP('',(#52494,#52495,#52496,#52497)) ;
#22281 = EDGE_LOOP('',(#52498,#52499,#52500,#52501)) ;
#22282 = EDGE_LOOP('',(#52502,#52503,#52504,#52505)) ;
#22283 = EDGE_LOOP('',(#52506,#52507,#52508,#52509)) ;
#22284 = EDGE_LOOP('',(#52510,#52511,#52512,#52513)) ;
#22285 = EDGE_LOOP('',(#52514,#52515,#52516,#52517)) ;
#22286 = EDGE_LOOP('',(#52518,#52519,#52520,#52521)) ;
#22287 = EDGE_LOOP('',(#52522,#52523,#52524,#52525,#52526)) ;
#22288 = EDGE_LOOP('',(#52527,#52528,#52529,#52530,#52531,#52532,#52533,#52534)) ;
#22289 = EDGE_LOOP('',(#52535,#52536,#52537)) ;
#22290 = EDGE_LOOP('',(#52538,#52539,#52540,#52541)) ;
#22291 = EDGE_LOOP('',(#52542,#52543,#52544,#52545,#52546)) ;
#22292 = EDGE_LOOP('',(#52547,#52548,#52549,#52550,#52551)) ;
#22293 = EDGE_LOOP('',(#52552,#52553,#52554,#52555)) ;
#22294 = EDGE_LOOP('',(#52556,#52557,#52558)) ;
#22295 = EDGE_LOOP('',(#52559,#52560,#52561,#52562,#52563,#52564,#52565,#52566)) ;
#22296 = EDGE_LOOP('',(#52567,#52568,#52569,#52570,#52571)) ;
#22297 = EDGE_LOOP('',(#52572,#52573,#52574,#52575,#52576)) ;
#22298 = EDGE_LOOP('',(#52577,#52578,#52579,#52580)) ;
#22299 = EDGE_LOOP('',(#52581,#52582,#52583,#52584,#52585,#52586,#52587,#52588)) ;
#22300 = EDGE_LOOP('',(#52589,#52590,#52591,#52592)) ;
#22301 = EDGE_LOOP('',(#52593,#52594,#52595,#52596,#52597,#52598,#52599,#52600)) ;
#22302 = EDGE_LOOP('',(#52601,#52602,#52603,#52604)) ;
#22303 = EDGE_LOOP('',(#52605,#52606,#52607,#52608)) ;
#22304 = EDGE_LOOP('',(#52609,#52610,#52611,#52612)) ;
#22305 = EDGE_LOOP('',(#52613,#52614,#52615,#52616)) ;
#22306 = EDGE_LOOP('',(#52617,#52618,#52619,#52620,#52621,#52622,#52623,#52624,
#52625)) ;
#22307 = EDGE_LOOP('',(#52626,#52627,#52628,#52629,#52630,#52631,#52632)) ;
#22308 = EDGE_LOOP('',(#52633,#52634,#52635,#52636)) ;
#22309 = EDGE_LOOP('',(#52637,#52638,#52639,#52640)) ;
#22310 = EDGE_LOOP('',(#52641,#52642,#52643,#52644)) ;
#22311 = EDGE_LOOP('',(#52645,#52646,#52647)) ;
#22312 = EDGE_LOOP('',(#52648,#52649,#52650,#52651)) ;
#22313 = EDGE_LOOP('',(#52652,#52653,#52654,#52655)) ;
#22314 = EDGE_LOOP('',(#52656,#52657,#52658,#52659)) ;
#22315 = EDGE_LOOP('',(#52660,#52661,#52662,#52663)) ;
#22316 = EDGE_LOOP('',(#52664,#52665,#52666,#52667)) ;
#22317 = EDGE_LOOP('',(#52668,#52669,#52670,#52671)) ;
#22318 = EDGE_LOOP('',(#52672,#52673,#52674,#52675)) ;
#22319 = EDGE_LOOP('',(#52676,#52677,#52678,#52679)) ;
#22320 = EDGE_LOOP('',(#52680,#52681,#52682,#52683)) ;
#22321 = EDGE_LOOP('',(#52684,#52685,#52686,#52687)) ;
#22322 = EDGE_LOOP('',(#52688,#52689,#52690,#52691)) ;
#22323 = EDGE_LOOP('',(#52692,#52693,#52694,#52695)) ;
#22324 = EDGE_LOOP('',(#52696,#52697,#52698,#52699)) ;
#22325 = EDGE_LOOP('',(#52700,#52701,#52702,#52703)) ;
#22326 = EDGE_LOOP('',(#52704,#52705,#52706,#52707)) ;
#22327 = EDGE_LOOP('',(#52708,#52709,#52710,#52711)) ;
#22328 = EDGE_LOOP('',(#52712,#52713,#52714,#52715)) ;
#22329 = EDGE_LOOP('',(#52716,#52717,#52718,#52719)) ;
#22330 = EDGE_LOOP('',(#52720,#52721,#52722,#52723)) ;
#22331 = EDGE_LOOP('',(#52724,#52725,#52726)) ;
#22332 = EDGE_LOOP('',(#52727,#52728,#52729,#52730)) ;
#22333 = EDGE_LOOP('',(#52731,#52732,#52733,#52734,#52735,#52736)) ;
#22334 = EDGE_LOOP('',(#52737,#52738,#52739,#52740)) ;
#22335 = EDGE_LOOP('',(#52741,#52742,#52743,#52744,#52745)) ;
#22336 = EDGE_LOOP('',(#52746,#52747,#52748,#52749)) ;
#22337 = EDGE_LOOP('',(#52750,#52751,#52752,#52753,#52754)) ;
#22338 = EDGE_LOOP('',(#52755,#52756,#52757,#52758)) ;
#22339 = EDGE_LOOP('',(#52759,#52760,#52761,#52762,#52763,#52764,#52765)) ;
#22340 = EDGE_LOOP('',(#52766,#52767,#52768,#52769,#52770,#52771,#52772)) ;
#22341 = EDGE_LOOP('',(#52773,#52774,#52775,#52776)) ;
#22342 = EDGE_LOOP('',(#52777,#52778,#52779,#52780,#52781,#52782,#52783)) ;
#22343 = EDGE_LOOP('',(#52784,#52785,#52786,#52787)) ;
#22344 = EDGE_LOOP('',(#52788,#52789,#52790,#52791,#52792,#52793,#52794)) ;
#22345 = EDGE_LOOP('',(#52795,#52796,#52797,#52798)) ;
#22346 = EDGE_LOOP('',(#52799,#52800,#52801,#52802)) ;
#22347 = EDGE_LOOP('',(#52803,#52804,#52805,#52806)) ;
#22348 = EDGE_LOOP('',(#52807,#52808,#52809,#52810)) ;
#22349 = EDGE_LOOP('',(#52811,#52812,#52813,#52814)) ;
#22350 = EDGE_LOOP('',(#52815,#52816,#52817,#52818)) ;
#22351 = EDGE_LOOP('',(#52819,#52820,#52821,#52822)) ;
#22352 = EDGE_LOOP('',(#52823,#52824,#52825,#52826)) ;
#22353 = EDGE_LOOP('',(#52827,#52828)) ;
#22354 = EDGE_LOOP('',(#52829,#52830,#52831,#52832)) ;
#22355 = EDGE_LOOP('',(#52833,#52834,#52835,#52836)) ;
#22356 = EDGE_LOOP('',(#52837,#52838,#52839,#52840,#52841)) ;
#22357 = EDGE_LOOP('',(#52842,#52843,#52844,#52845)) ;
#22358 = EDGE_LOOP('',(#52846,#52847,#52848,#52849)) ;
#22359 = EDGE_LOOP('',(#52850,#52851,#52852,#52853)) ;
#22360 = EDGE_LOOP('',(#52854,#52855,#52856,#52857)) ;
#22361 = EDGE_LOOP('',(#52858,#52859,#52860,#52861,#52862)) ;
#22362 = EDGE_LOOP('',(#52863,#52864,#52865,#52866)) ;
#22363 = EDGE_LOOP('',(#52867,#52868,#52869)) ;
#22364 = EDGE_LOOP('',(#52870,#52871,#52872,#52873,#52874,#52875,#52876)) ;
#22365 = EDGE_LOOP('',(#52877,#52878,#52879,#52880,#52881)) ;
#22366 = EDGE_LOOP('',(#52882,#52883,#52884,#52885)) ;
#22367 = EDGE_LOOP('',(#52886,#52887,#52888)) ;
#22368 = EDGE_LOOP('',(#52889,#52890,#52891,#52892,#52893,#52894,#52895)) ;
#22369 = EDGE_LOOP('',(#52896,#52897,#52898,#52899,#52900)) ;
#22370 = EDGE_LOOP('',(#52901,#52902,#52903,#52904)) ;
#22371 = EDGE_LOOP('',(#52905,#52906,#52907)) ;
#22372 = EDGE_LOOP('',(#52908,#52909,#52910,#52911,#52912,#52913,#52914)) ;
#22373 = EDGE_LOOP('',(#52915,#52916,#52917,#52918,#52919)) ;
#22374 = EDGE_LOOP('',(#52920,#52921,#52922,#52923)) ;
#22375 = EDGE_LOOP('',(#52924,#52925,#52926)) ;
#22376 = EDGE_LOOP('',(#52927,#52928,#52929,#52930,#52931,#52932,#52933)) ;
#22377 = EDGE_LOOP('',(#52934,#52935,#52936,#52937,#52938)) ;
#22378 = EDGE_LOOP('',(#52939,#52940,#52941,#52942)) ;
#22379 = EDGE_LOOP('',(#52943,#52944,#52945)) ;
#22380 = EDGE_LOOP('',(#52946,#52947,#52948,#52949,#52950,#52951,#52952)) ;
#22381 = EDGE_LOOP('',(#52953,#52954,#52955,#52956,#52957)) ;
#22382 = EDGE_LOOP('',(#52958,#52959,#52960,#52961)) ;
#22383 = EDGE_LOOP('',(#52962,#52963,#52964)) ;
#22384 = EDGE_LOOP('',(#52965,#52966,#52967,#52968,#52969,#52970,#52971)) ;
#22385 = EDGE_LOOP('',(#52972,#52973,#52974,#52975,#52976)) ;
#22386 = EDGE_LOOP('',(#52977,#52978,#52979,#52980)) ;
#22387 = EDGE_LOOP('',(#52981,#52982,#52983)) ;
#22388 = EDGE_LOOP('',(#52984,#52985,#52986,#52987,#52988,#52989,#52990)) ;
#22389 = EDGE_LOOP('',(#52991,#52992,#52993,#52994,#52995)) ;
#22390 = EDGE_LOOP('',(#52996,#52997,#52998,#52999)) ;
#22391 = EDGE_LOOP('',(#53000,#53001,#53002)) ;
#22392 = EDGE_LOOP('',(#53003,#53004,#53005,#53006,#53007,#53008,#53009)) ;
#22393 = EDGE_LOOP('',(#53010,#53011,#53012,#53013,#53014)) ;
#22394 = EDGE_LOOP('',(#53015,#53016,#53017,#53018)) ;
#22395 = EDGE_LOOP('',(#53019,#53020,#53021,#53022)) ;
#22396 = EDGE_LOOP('',(#53023,#53024,#53025,#53026)) ;
#22397 = EDGE_LOOP('',(#53027,#53028,#53029,#53030)) ;
#22398 = EDGE_LOOP('',(#53031,#53032,#53033,#53034)) ;
#22399 = EDGE_LOOP('',(#53035,#53036,#53037,#53038)) ;
#22400 = EDGE_LOOP('',(#53039,#53040,#53041,#53042)) ;
#22401 = EDGE_LOOP('',(#53043,#53044,#53045,#53046)) ;
#22402 = EDGE_LOOP('',(#53047,#53048,#53049,#53050)) ;
#22403 = EDGE_LOOP('',(#53051,#53052,#53053,#53054)) ;
#22404 = EDGE_LOOP('',(#53055,#53056,#53057)) ;
#22405 = EDGE_LOOP('',(#53058,#53059,#53060,#53061,#53062,#53063,#53064)) ;
#22406 = EDGE_LOOP('',(#53065,#53066,#53067,#53068,#53069)) ;
#22407 = EDGE_LOOP('',(#53070,#53071,#53072,#53073,#53074)) ;
#22408 = EDGE_LOOP('',(#53075,#53076,#53077,#53078,#53079)) ;
#22409 = EDGE_LOOP('',(#53080,#53081,#53082,#53083,#53084)) ;
#22410 = EDGE_LOOP('',(#53085,#53086,#53087,#53088,#53089)) ;
#22411 = EDGE_LOOP('',(#53090,#53091,#53092,#53093,#53094)) ;
#22412 = EDGE_LOOP('',(#53095,#53096,#53097,#53098,#53099)) ;
#22413 = EDGE_LOOP('',(#53100,#53101,#53102,#53103,#53104)) ;
#22414 = EDGE_LOOP('',(#53105,#53106,#53107,#53108,#53109)) ;
#22415 = EDGE_LOOP('',(#53110,#53111,#53112,#53113)) ;
#22416 = EDGE_LOOP('',(#53114,#53115,#53116,#53117)) ;
#22417 = EDGE_LOOP('',(#53118,#53119,#53120,#53121)) ;
#22418 = EDGE_LOOP('',(#53122,#53123,#53124,#53125)) ;
#22419 = EDGE_LOOP('',(#53126,#53127,#53128,#53129)) ;
#22420 = EDGE_LOOP('',(#53130,#53131,#53132,#53133)) ;
#22421 = EDGE_LOOP('',(#53134,#53135,#53136,#53137)) ;
#22422 = EDGE_LOOP('',(#53138,#53139,#53140,#53141)) ;
#22423 = EDGE_LOOP('',(#53142,#53143,#53144,#53145)) ;
#22424 = EDGE_LOOP('',(#53146,#53147,#53148,#53149,#53150)) ;
#22425 = EDGE_LOOP('',(#53151,#53152,#53153,#53154)) ;
#22426 = EDGE_LOOP('',(#53155,#53156,#53157,#53158)) ;
#22427 = EDGE_LOOP('',(#53159,#53160,#53161)) ;
#22428 = EDGE_LOOP('',(#53162,#53163,#53164,#53165,#53166,#53167,#53168)) ;
#22429 = EDGE_LOOP('',(#53169,#53170,#53171,#53172,#53173)) ;
#22430 = EDGE_LOOP('',(#53174,#53175,#53176,#53177)) ;
#22431 = EDGE_LOOP('',(#53178,#53179,#53180,#53181,#53182,#53183,#53184,#53185,
#53186,#53187,#53188,#53189)) ;
#22432 = EDGE_LOOP('',(#53190,#53191,#53192,#53193,#53194,#53195,#53196,#53197,
#53198,#53199,#53200,#53201)) ;
#22433 = EDGE_LOOP('',(#53202,#53203,#53204,#53205,#53206,#53207,#53208,#53209,
#53210,#53211,#53212,#53213)) ;
#22434 = EDGE_LOOP('',(#53214,#53215,#53216,#53217,#53218,#53219,#53220,#53221,
#53222,#53223,#53224,#53225)) ;
#22435 = EDGE_LOOP('',(#53226,#53227,#53228,#53229,#53230,#53231,#53232,#53233,
#53234,#53235,#53236,#53237)) ;
#22436 = EDGE_LOOP('',(#53238,#53239,#53240,#53241,#53242,#53243,#53244,#53245,
#53246,#53247,#53248,#53249)) ;
#22437 = EDGE_LOOP('',(#53250,#53251,#53252,#53253,#53254,#53255,#53256,#53257,
#53258,#53259,#53260,#53261)) ;
#22438 = EDGE_LOOP('',(#53262,#53263,#53264,#53265,#53266,#53267,#53268,#53269,
#53270,#53271,#53272,#53273)) ;
#22439 = EDGE_LOOP('',(#53274,#53275,#53276,#53277,#53278,#53279,#53280,#53281,
#53282,#53283,#53284,#53285)) ;
#22440 = EDGE_LOOP('',(#53286,#53287,#53288,#53289,#53290)) ;
#22441 = EDGE_LOOP('',(#53291,#53292,#53293,#53294,#53295)) ;
#22442 = EDGE_LOOP('',(#53296,#53297,#53298,#53299,#53300)) ;
#22443 = EDGE_LOOP('',(#53301,#53302,#53303,#53304,#53305)) ;
#22444 = EDGE_LOOP('',(#53306,#53307,#53308,#53309,#53310)) ;
#22445 = EDGE_LOOP('',(#53311,#53312,#53313,#53314,#53315)) ;
#22446 = EDGE_LOOP('',(#53316,#53317,#53318,#53319,#53320)) ;
#22447 = EDGE_LOOP('',(#53321,#53322,#53323,#53324,#53325)) ;
#22448 = EDGE_LOOP('',(#53326,#53327,#53328,#53329,#53330)) ;
#22449 = EDGE_LOOP('',(#53331,#53332,#53333,#53334,#53335)) ;
#22450 = EDGE_LOOP('',(#53336,#53337,#53338,#53339,#53340)) ;
#22451 = EDGE_LOOP('',(#53341,#53342,#53343,#53344,#53345)) ;
#22452 = EDGE_LOOP('',(#53346,#53347,#53348,#53349,#53350)) ;
#22453 = EDGE_LOOP('',(#53351,#53352,#53353,#53354,#53355)) ;
#22454 = EDGE_LOOP('',(#53356,#53357,#53358,#53359,#53360)) ;
#22455 = EDGE_LOOP('',(#53361,#53362,#53363,#53364,#53365)) ;
#22456 = EDGE_LOOP('',(#53366,#53367,#53368,#53369,#53370)) ;
#22457 = EDGE_LOOP('',(#53371,#53372,#53373,#53374,#53375)) ;
#22458 = EDGE_LOOP('',(#53376,#53377,#53378,#53379)) ;
#22459 = EDGE_LOOP('',(#53380,#53381,#53382,#53383)) ;
#22460 = EDGE_LOOP('',(#53384,#53385,#53386,#53387)) ;
#22461 = EDGE_LOOP('',(#53388,#53389,#53390,#53391)) ;
#22462 = EDGE_LOOP('',(#53392,#53393,#53394,#53395)) ;
#22463 = EDGE_LOOP('',(#53396,#53397,#53398,#53399)) ;
#22464 = EDGE_LOOP('',(#53400,#53401,#53402,#53403)) ;
#22465 = EDGE_LOOP('',(#53404,#53405,#53406,#53407)) ;
#22466 = EDGE_LOOP('',(#53408,#53409,#53410,#53411)) ;
#22467 = EDGE_LOOP('',(#53412,#53413,#53414,#53415,#53416,#53417,#53418,#53419,
#53420,#53421,#53422,#53423)) ;
#22468 = EDGE_LOOP('',(#53424,#53425,#53426,#53427,#53428)) ;
#22469 = EDGE_LOOP('',(#53429,#53430,#53431,#53432,#53433)) ;
#22470 = EDGE_LOOP('',(#53434,#53435,#53436,#53437)) ;
#22471 = EDGE_LOOP('',(#53438,#53439,#53440,#53441)) ;
#22472 = EDGE_LOOP('',(#53442,#53443,#53444,#53445,#53446,#53447,#53448,#53449,
#53450,#53451,#53452,#53453,#53454,#53455,#53456,#53457,#53458,#53459,#53460,
#53461,#53462,#53463,#53464,#53465,#53466,#53467,#53468,#53469,#53470,#53471,
#53472,#53473,#53474,#53475,#53476,#53477,#53478,#53479,#53480,#53481,#53482,
#53483,#53484,#53485,#53486,#53487,#53488,#53489,#53490,#53491,#53492,#53493,
#53494,#53495,#53496,#53497,#53498,#53499,#53500,#53501,#53502,#53503,#53504,
#53505)) ;
#22473 = EDGE_LOOP('',(#53506,#53507,#53508,#53509)) ;
#22474 = EDGE_LOOP('',(#53510,#53511,#53512,#53513,#53514,#53515,#53516,#53517,
#53518,#53519,#53520,#53521,#53522,#53523,#53524,#53525,#53526,#53527,#53528,
#53529,#53530,#53531,#53532,#53533,#53534,#53535,#53536,#53537,#53538,#53539,
#53540,#53541,#53542,#53543,#53544,#53545,#53546,#53547,#53548,#53549,#53550,
#53551,#53552,#53553,#53554,#53555,#53556,#53557,#53558,#53559,#53560,#53561,
#53562,#53563,#53564,#53565,#53566,#53567,#53568,#53569,#53570,#53571,#53572,
#53573)) ;
#22475 = EDGE_LOOP('',(#53574,#53575,#53576,#53577)) ;
#22476 = EDGE_LOOP('',(#53578,#53579,#53580,#53581)) ;
#22477 = EDGE_LOOP('',(#53582,#53583,#53584,#53585)) ;
#22478 = EDGE_LOOP('',(#53586,#53587,#53588,#53589)) ;
#22479 = EDGE_LOOP('',(#53590,#53591,#53592,#53593)) ;
#22480 = EDGE_LOOP('',(#53594,#53595,#53596,#53597)) ;
#22481 = EDGE_LOOP('',(#53598,#53599,#53600,#53601)) ;
#22482 = EDGE_LOOP('',(#53602,#53603,#53604,#53605)) ;
#22483 = EDGE_LOOP('',(#53606,#53607,#53608,#53609)) ;
#22484 = EDGE_LOOP('',(#53610,#53611,#53612,#53613)) ;
#22485 = EDGE_LOOP('',(#53614,#53615,#53616,#53617)) ;
#22486 = EDGE_LOOP('',(#53618,#53619,#53620,#53621)) ;
#22487 = EDGE_LOOP('',(#53622,#53623,#53624,#53625,#53626,#53627,#53628,#53629,
#53630,#53631,#53632,#53633,#53634,#53635,#53636,#53637,#53638,#53639,#53640,
#53641,#53642,#53643,#53644,#53645)) ;
#22488 = EDGE_LOOP('',(#53646,#53647,#53648,#53649,#53650,#53651,#53652,#53653,
#53654,#53655,#53656,#53657,#53658,#53659,#53660,#53661,#53662,#53663,#53664,
#53665,#53666,#53667,#53668,#53669)) ;
#22489 = EDGE_LOOP('',(#53670,#53671,#53672,#53673,#53674,#53675,#53676,#53677,
#53678,#53679,#53680,#53681,#53682,#53683,#53684,#53685,#53686,#53687,#53688,
#53689,#53690,#53691,#53692,#53693)) ;
#22490 = EDGE_LOOP('',(#53694,#53695,#53696,#53697,#53698,#53699,#53700,#53701,
#53702,#53703,#53704,#53705,#53706,#53707,#53708,#53709,#53710,#53711,#53712,
#53713,#53714,#53715,#53716,#53717)) ;
#22491 = EDGE_LOOP('',(#53718,#53719,#53720,#53721,#53722,#53723,#53724,#53725,
#53726,#53727,#53728,#53729,#53730,#53731,#53732,#53733,#53734,#53735,#53736,
#53737,#53738,#53739,#53740,#53741)) ;
#22492 = EDGE_LOOP('',(#53742,#53743,#53744,#53745,#53746,#53747,#53748,#53749,
#53750,#53751,#53752,#53753,#53754,#53755,#53756,#53757,#53758,#53759,#53760,
#53761,#53762,#53763,#53764,#53765)) ;
#22493 = EDGE_LOOP('',(#53766,#53767,#53768,#53769,#53770,#53771,#53772,#53773,
#53774,#53775,#53776,#53777,#53778,#53779,#53780,#53781,#53782,#53783,#53784,
#53785,#53786,#53787,#53788,#53789)) ;
#22494 = EDGE_LOOP('',(#53790,#53791,#53792,#53793,#53794,#53795,#53796,#53797,
#53798,#53799,#53800,#53801,#53802,#53803,#53804,#53805,#53806,#53807,#53808,
#53809,#53810,#53811,#53812,#53813)) ;
#22495 = EDGE_LOOP('',(#53814,#53815,#53816,#53817,#53818,#53819,#53820,#53821,
#53822,#53823,#53824,#53825,#53826,#53827,#53828,#53829,#53830,#53831,#53832,
#53833,#53834,#53835,#53836,#53837)) ;
#22496 = EDGE_LOOP('',(#53838,#53839,#53840,#53841,#53842,#53843,#53844,#53845,
#53846,#53847,#53848,#53849,#53850,#53851,#53852,#53853,#53854,#53855,#53856,
#53857,#53858,#53859,#53860,#53861)) ;
#22497 = EDGE_LOOP('',(#53862,#53863,#53864,#53865,#53866,#53867,#53868,#53869,
#53870,#53871)) ;
#22498 = EDGE_LOOP('',(#53872,#53873,#53874,#53875,#53876,#53877,#53878,#53879,
#53880,#53881)) ;
#22499 = EDGE_LOOP('',(#53882,#53883,#53884,#53885,#53886,#53887,#53888,#53889,
#53890,#53891)) ;
#22500 = EDGE_LOOP('',(#53892,#53893,#53894,#53895)) ;
#22501 = EDGE_LOOP('',(#53896,#53897,#53898,#53899)) ;
#22502 = EDGE_LOOP('',(#53900,#53901,#53902,#53903)) ;
#22503 = EDGE_LOOP('',(#53904,#53905,#53906,#53907)) ;
#22504 = EDGE_LOOP('',(#53908,#53909,#53910,#53911)) ;
#22505 = EDGE_LOOP('',(#53912,#53913,#53914,#53915)) ;
#22506 = EDGE_LOOP('',(#53916,#53917,#53918,#53919)) ;
#22507 = EDGE_LOOP('',(#53920,#53921,#53922,#53923)) ;
#22508 = EDGE_LOOP('',(#53924,#53925,#53926,#53927)) ;
#22509 = EDGE_LOOP('',(#53928,#53929,#53930,#53931)) ;
#22510 = EDGE_LOOP('',(#53932,#53933,#53934,#53935)) ;
#22511 = EDGE_LOOP('',(#53936,#53937,#53938,#53939)) ;
#22512 = EDGE_LOOP('',(#53940,#53941,#53942,#53943)) ;
#22513 = EDGE_LOOP('',(#53944,#53945,#53946,#53947)) ;
#22514 = EDGE_LOOP('',(#53948,#53949,#53950,#53951)) ;
#22515 = EDGE_LOOP('',(#53952,#53953,#53954,#53955)) ;
#22516 = EDGE_LOOP('',(#53956,#53957,#53958,#53959)) ;
#22517 = EDGE_LOOP('',(#53960,#53961,#53962,#53963)) ;
#22518 = EDGE_LOOP('',(#53964,#53965,#53966,#53967)) ;
#22519 = EDGE_LOOP('',(#53968,#53969,#53970,#53971)) ;
#22520 = EDGE_LOOP('',(#53972,#53973,#53974,#53975)) ;
#22521 = EDGE_LOOP('',(#53976,#53977,#53978,#53979)) ;
#22522 = EDGE_LOOP('',(#53980,#53981,#53982,#53983)) ;
#22523 = EDGE_LOOP('',(#53984,#53985,#53986,#53987)) ;
#22524 = EDGE_LOOP('',(#53988,#53989,#53990,#53991)) ;
#22525 = EDGE_LOOP('',(#53992,#53993,#53994,#53995)) ;
#22526 = EDGE_LOOP('',(#53996,#53997,#53998,#53999)) ;
#22527 = EDGE_LOOP('',(#54000,#54001,#54002,#54003)) ;
#22528 = EDGE_LOOP('',(#54004,#54005,#54006,#54007)) ;
#22529 = EDGE_LOOP('',(#54008,#54009,#54010,#54011)) ;
#22530 = EDGE_LOOP('',(#54012,#54013,#54014,#54015)) ;
#22531 = EDGE_LOOP('',(#54016,#54017,#54018,#54019)) ;
#22532 = EDGE_LOOP('',(#54020,#54021,#54022,#54023,#54024,#54025,#54026,#54027,
#54028,#54029,#54030,#54031,#54032,#54033,#54034,#54035,#54036,#54037)) ;
#22533 = EDGE_LOOP('',(#54038)) ;
#22534 = EDGE_LOOP('',(#54039)) ;
#22535 = EDGE_LOOP('',(#54040,#54041,#54042,#54043,#54044,#54045,#54046,#54047)) ;
#22536 = EDGE_LOOP('',(#54048,#54049,#54050,#54051)) ;
#22537 = EDGE_LOOP('',(#54052,#54053,#54054,#54055)) ;
#22538 = EDGE_LOOP('',(#54056,#54057,#54058)) ;
#22539 = EDGE_LOOP('',(#54059,#54060,#54061)) ;
#22540 = EDGE_LOOP('',(#54062,#54063,#54064,#54065)) ;
#22541 = EDGE_LOOP('',(#54066,#54067,#54068,#54069,#54070,#54071)) ;
#22542 = EDGE_LOOP('',(#54072,#54073,#54074,#54075,#54076,#54077,#54078)) ;
#22543 = EDGE_LOOP('',(#54079,#54080,#54081,#54082)) ;
#22544 = EDGE_LOOP('',(#54083,#54084,#54085,#54086)) ;
#22545 = EDGE_LOOP('',(#54087,#54088,#54089,#54090)) ;
#22546 = EDGE_LOOP('',(#54091,#54092,#54093,#54094)) ;
#22547 = EDGE_LOOP('',(#54095,#54096,#54097)) ;
#22548 = EDGE_LOOP('',(#54098,#54099,#54100,#54101)) ;
#22549 = EDGE_LOOP('',(#54102,#54103,#54104,#54105)) ;
#22550 = EDGE_LOOP('',(#54106,#54107,#54108,#54109)) ;
#22551 = EDGE_LOOP('',(#54110,#54111,#54112,#54113)) ;
#22552 = EDGE_LOOP('',(#54114,#54115,#54116,#54117)) ;
#22553 = EDGE_LOOP('',(#54118,#54119,#54120,#54121)) ;
#22554 = EDGE_LOOP('',(#54122,#54123,#54124,#54125)) ;
#22555 = EDGE_LOOP('',(#54126,#54127,#54128,#54129)) ;
#22556 = EDGE_LOOP('',(#54130,#54131,#54132,#54133)) ;
#22557 = EDGE_LOOP('',(#54134,#54135,#54136)) ;
#22558 = EDGE_LOOP('',(#54137,#54138,#54139)) ;
#22559 = EDGE_LOOP('',(#54140,#54141,#54142,#54143,#54144)) ;
#22560 = EDGE_LOOP('',(#54145,#54146,#54147)) ;
#22561 = EDGE_LOOP('',(#54148,#54149,#54150)) ;
#22562 = EDGE_LOOP('',(#54151,#54152,#54153,#54154)) ;
#22563 = EDGE_LOOP('',(#54155,#54156,#54157,#54158)) ;
#22564 = EDGE_LOOP('',(#54159,#54160,#54161,#54162)) ;
#22565 = EDGE_LOOP('',(#54163,#54164,#54165,#54166)) ;
#22566 = EDGE_LOOP('',(#54167,#54168,#54169,#54170)) ;
#22567 = EDGE_LOOP('',(#54171,#54172,#54173,#54174)) ;
#22568 = EDGE_LOOP('',(#54175,#54176,#54177,#54178)) ;
#22569 = EDGE_LOOP('',(#54179,#54180,#54181)) ;
#22570 = EDGE_LOOP('',(#54182,#54183,#54184,#54185)) ;
#22571 = EDGE_LOOP('',(#54186,#54187,#54188,#54189)) ;
#22572 = EDGE_LOOP('',(#54190,#54191,#54192)) ;
#22573 = EDGE_LOOP('',(#54193,#54194,#54195,#54196)) ;
#22574 = EDGE_LOOP('',(#54197,#54198,#54199,#54200)) ;
#22575 = EDGE_LOOP('',(#54201,#54202,#54203,#54204)) ;
#22576 = EDGE_LOOP('',(#54205,#54206,#54207,#54208)) ;
#22577 = EDGE_LOOP('',(#54209,#54210,#54211,#54212)) ;
#22578 = EDGE_LOOP('',(#54213,#54214,#54215,#54216)) ;
#22579 = EDGE_LOOP('',(#54217,#54218,#54219,#54220,#54221)) ;
#22580 = EDGE_LOOP('',(#54222,#54223,#54224,#54225)) ;
#22581 = EDGE_LOOP('',(#54226,#54227,#54228)) ;
#22582 = EDGE_LOOP('',(#54229,#54230,#54231)) ;
#22583 = EDGE_LOOP('',(#54232,#54233,#54234,#54235)) ;
#22584 = EDGE_LOOP('',(#54236,#54237,#54238,#54239)) ;
#22585 = EDGE_LOOP('',(#54240,#54241,#54242,#54243)) ;
#22586 = EDGE_LOOP('',(#54244,#54245,#54246)) ;
#22587 = EDGE_LOOP('',(#54247,#54248,#54249,#54250)) ;
#22588 = EDGE_LOOP('',(#54251,#54252,#54253,#54254)) ;
#22589 = EDGE_LOOP('',(#54255,#54256,#54257)) ;
#22590 = EDGE_LOOP('',(#54258,#54259,#54260,#54261)) ;
#22591 = EDGE_LOOP('',(#54262,#54263,#54264,#54265)) ;
#22592 = EDGE_LOOP('',(#54266,#54267,#54268,#54269)) ;
#22593 = EDGE_LOOP('',(#54270,#54271,#54272)) ;
#22594 = EDGE_LOOP('',(#54273,#54274,#54275)) ;
#22595 = EDGE_LOOP('',(#54276,#54277,#54278,#54279)) ;
#22596 = EDGE_LOOP('',(#54280,#54281,#54282,#54283)) ;
#22597 = EDGE_LOOP('',(#54284,#54285,#54286)) ;
#22598 = EDGE_LOOP('',(#54287,#54288,#54289)) ;
#22599 = EDGE_LOOP('',(#54290,#54291,#54292,#54293)) ;
#22600 = EDGE_LOOP('',(#54294,#54295,#54296,#54297)) ;
#22601 = EDGE_LOOP('',(#54298,#54299,#54300,#54301)) ;
#22602 = EDGE_LOOP('',(#54302,#54303,#54304)) ;
#22603 = EDGE_LOOP('',(#54305,#54306,#54307,#54308)) ;
#22604 = EDGE_LOOP('',(#54309,#54310,#54311,#54312)) ;
#22605 = EDGE_LOOP('',(#54313,#54314,#54315)) ;
#22606 = EDGE_LOOP('',(#54316,#54317,#54318,#54319)) ;
#22607 = EDGE_LOOP('',(#54320,#54321,#54322,#54323)) ;
#22608 = EDGE_LOOP('',(#54324,#54325,#54326,#54327)) ;
#22609 = EDGE_LOOP('',(#54328,#54329,#54330)) ;
#22610 = EDGE_LOOP('',(#54331,#54332,#54333)) ;
#22611 = EDGE_LOOP('',(#54334,#54335,#54336,#54337)) ;
#22612 = EDGE_LOOP('',(#54338,#54339,#54340,#54341)) ;
#22613 = EDGE_LOOP('',(#54342,#54343,#54344)) ;
#22614 = EDGE_LOOP('',(#54345,#54346,#54347,#54348)) ;
#22615 = EDGE_LOOP('',(#54349,#54350,#54351,#54352)) ;
#22616 = EDGE_LOOP('',(#54353,#54354,#54355)) ;
#22617 = EDGE_LOOP('',(#54356,#54357,#54358,#54359)) ;
#22618 = EDGE_LOOP('',(#54360,#54361,#54362,#54363)) ;
#22619 = EDGE_LOOP('',(#54364,#54365,#54366,#54367)) ;
#22620 = EDGE_LOOP('',(#54368,#54369,#54370)) ;
#22621 = EDGE_LOOP('',(#54371,#54372,#54373,#54374)) ;
#22622 = EDGE_LOOP('',(#54375,#54376,#54377,#54378)) ;
#22623 = EDGE_LOOP('',(#54379,#54380,#54381)) ;
#22624 = EDGE_LOOP('',(#54382,#54383,#54384)) ;
#22625 = EDGE_LOOP('',(#54385,#54386,#54387,#54388)) ;
#22626 = EDGE_LOOP('',(#54389,#54390,#54391,#54392)) ;
#22627 = EDGE_LOOP('',(#54393,#54394,#54395)) ;
#22628 = EDGE_LOOP('',(#54396,#54397,#54398)) ;
#22629 = EDGE_LOOP('',(#54399,#54400,#54401,#54402)) ;
#22630 = EDGE_LOOP('',(#54403,#54404,#54405,#54406)) ;
#22631 = EDGE_LOOP('',(#54407,#54408,#54409)) ;
#22632 = EDGE_LOOP('',(#54410,#54411,#54412,#54413)) ;
#22633 = EDGE_LOOP('',(#54414,#54415,#54416,#54417)) ;
#22634 = EDGE_LOOP('',(#54418,#54419,#54420)) ;
#22635 = EDGE_LOOP('',(#54421,#54422,#54423)) ;
#22636 = EDGE_LOOP('',(#54424,#54425,#54426,#54427)) ;
#22637 = EDGE_LOOP('',(#54428,#54429,#54430,#54431)) ;
#22638 = EDGE_LOOP('',(#54432,#54433,#54434,#54435)) ;
#22639 = EDGE_LOOP('',(#54436,#54437,#54438,#54439)) ;
#22640 = EDGE_LOOP('',(#54440,#54441,#54442,#54443)) ;
#22641 = EDGE_LOOP('',(#54444,#54445,#54446,#54447)) ;
#22642 = EDGE_LOOP('',(#54448,#54449,#54450)) ;
#22643 = EDGE_LOOP('',(#54451,#54452,#54453)) ;
#22644 = EDGE_LOOP('',(#54454,#54455,#54456,#54457)) ;
#22645 = EDGE_LOOP('',(#54458,#54459,#54460,#54461)) ;
#22646 = EDGE_LOOP('',(#54462,#54463,#54464,#54465)) ;
#22647 = EDGE_LOOP('',(#54466,#54467,#54468,#54469)) ;
#22648 = EDGE_LOOP('',(#54470,#54471,#54472,#54473)) ;
#22649 = EDGE_LOOP('',(#54474,#54475,#54476,#54477)) ;
#22650 = EDGE_LOOP('',(#54478,#54479,#54480,#54481)) ;
#22651 = EDGE_LOOP('',(#54482,#54483,#54484,#54485)) ;
#22652 = EDGE_LOOP('',(#54486,#54487,#54488,#54489)) ;
#22653 = EDGE_LOOP('',(#54490,#54491,#54492,#54493)) ;
#22654 = EDGE_LOOP('',(#54494,#54495,#54496,#54497)) ;
#22655 = EDGE_LOOP('',(#54498,#54499,#54500,#54501)) ;
#22656 = EDGE_LOOP('',(#54502,#54503,#54504,#54505)) ;
#22657 = EDGE_LOOP('',(#54506,#54507,#54508,#54509)) ;
#22658 = EDGE_LOOP('',(#54510,#54511,#54512,#54513)) ;
#22659 = EDGE_LOOP('',(#54514,#54515,#54516,#54517)) ;
#22660 = EDGE_LOOP('',(#54518,#54519,#54520,#54521)) ;
#22661 = EDGE_LOOP('',(#54522,#54523,#54524)) ;
#22662 = EDGE_LOOP('',(#54525,#54526,#54527,#54528)) ;
#22663 = EDGE_LOOP('',(#54529,#54530,#54531,#54532)) ;
#22664 = EDGE_LOOP('',(#54533,#54534,#54535,#54536)) ;
#22665 = EDGE_LOOP('',(#54537,#54538,#54539)) ;
#22666 = EDGE_LOOP('',(#54540,#54541,#54542,#54543)) ;
#22667 = EDGE_LOOP('',(#54544,#54545,#54546,#54547)) ;
#22668 = EDGE_LOOP('',(#54548,#54549,#54550,#54551)) ;
#22669 = EDGE_LOOP('',(#54552,#54553,#54554,#54555)) ;
#22670 = EDGE_LOOP('',(#54556,#54557,#54558,#54559)) ;
#22671 = EDGE_LOOP('',(#54560,#54561,#54562,#54563)) ;
#22672 = EDGE_LOOP('',(#54564,#54565,#54566,#54567)) ;
#22673 = EDGE_LOOP('',(#54568,#54569,#54570,#54571,#54572,#54573)) ;
#22674 = EDGE_LOOP('',(#54574,#54575,#54576,#54577,#54578,#54579)) ;
#22675 = EDGE_LOOP('',(#54580,#54581,#54582,#54583,#54584)) ;
#22676 = EDGE_LOOP('',(#54585,#54586,#54587,#54588)) ;
#22677 = EDGE_LOOP('',(#54589,#54590,#54591,#54592)) ;
#22678 = EDGE_LOOP('',(#54593,#54594,#54595,#54596)) ;
#22679 = EDGE_LOOP('',(#54597,#54598,#54599,#54600)) ;
#22680 = EDGE_LOOP('',(#54601,#54602,#54603,#54604)) ;
#22681 = EDGE_LOOP('',(#54605,#54606,#54607,#54608)) ;
#22682 = EDGE_LOOP('',(#54609,#54610,#54611,#54612)) ;
#22683 = EDGE_LOOP('',(#54613,#54614,#54615,#54616)) ;
#22684 = EDGE_LOOP('',(#54617,#54618,#54619,#54620)) ;
#22685 = EDGE_LOOP('',(#54621,#54622,#54623,#54624)) ;
#22686 = EDGE_LOOP('',(#54625,#54626,#54627,#54628)) ;
#22687 = EDGE_LOOP('',(#54629,#54630,#54631,#54632)) ;
#22688 = EDGE_LOOP('',(#54633,#54634,#54635,#54636)) ;
#22689 = EDGE_LOOP('',(#54637,#54638,#54639,#54640)) ;
#22690 = EDGE_LOOP('',(#54641,#54642,#54643)) ;
#22691 = EDGE_LOOP('',(#54644,#54645,#54646,#54647)) ;
#22692 = EDGE_LOOP('',(#54648,#54649,#54650,#54651)) ;
#22693 = EDGE_LOOP('',(#54652,#54653,#54654,#54655)) ;
#22694 = EDGE_LOOP('',(#54656,#54657,#54658)) ;
#22695 = EDGE_LOOP('',(#54659,#54660,#54661)) ;
#22696 = EDGE_LOOP('',(#54662,#54663,#54664,#54665)) ;
#22697 = EDGE_LOOP('',(#54666,#54667,#54668,#54669)) ;
#22698 = EDGE_LOOP('',(#54670,#54671,#54672,#54673)) ;
#22699 = EDGE_LOOP('',(#54674,#54675,#54676)) ;
#22700 = EDGE_LOOP('',(#54677,#54678,#54679,#54680)) ;
#22701 = EDGE_LOOP('',(#54681,#54682,#54683,#54684)) ;
#22702 = EDGE_LOOP('',(#54685,#54686,#54687,#54688)) ;
#22703 = EDGE_LOOP('',(#54689,#54690,#54691,#54692)) ;
#22704 = EDGE_LOOP('',(#54693,#54694,#54695)) ;
#22705 = EDGE_LOOP('',(#54696,#54697,#54698,#54699)) ;
#22706 = EDGE_LOOP('',(#54700,#54701,#54702,#54703)) ;
#22707 = EDGE_LOOP('',(#54704,#54705,#54706,#54707)) ;
#22708 = EDGE_LOOP('',(#54708,#54709,#54710)) ;
#22709 = EDGE_LOOP('',(#54711,#54712,#54713)) ;
#22710 = EDGE_LOOP('',(#54714,#54715,#54716,#54717)) ;
#22711 = EDGE_LOOP('',(#54718,#54719,#54720,#54721)) ;
#22712 = EDGE_LOOP('',(#54722,#54723,#54724,#54725)) ;
#22713 = EDGE_LOOP('',(#54726,#54727,#54728)) ;
#22714 = EDGE_LOOP('',(#54729,#54730,#54731,#54732)) ;
#22715 = EDGE_LOOP('',(#54733,#54734,#54735,#54736)) ;
#22716 = EDGE_LOOP('',(#54737,#54738,#54739,#54740)) ;
#22717 = EDGE_LOOP('',(#54741,#54742,#54743,#54744)) ;
#22718 = EDGE_LOOP('',(#54745,#54746,#54747,#54748)) ;
#22719 = EDGE_LOOP('',(#54749,#54750,#54751,#54752)) ;
#22720 = EDGE_LOOP('',(#54753,#54754,#54755,#54756)) ;
#22721 = EDGE_LOOP('',(#54757,#54758,#54759,#54760)) ;
#22722 = EDGE_LOOP('',(#54761,#54762,#54763,#54764,#54765)) ;
#22723 = EDGE_LOOP('',(#54766,#54767,#54768,#54769)) ;
#22724 = EDGE_LOOP('',(#54770,#54771,#54772,#54773)) ;
#22725 = EDGE_LOOP('',(#54774,#54775,#54776,#54777)) ;
#22726 = EDGE_LOOP('',(#54778,#54779,#54780,#54781)) ;
#22727 = EDGE_LOOP('',(#54782,#54783,#54784,#54785)) ;
#22728 = EDGE_LOOP('',(#54786,#54787,#54788,#54789)) ;
#22729 = EDGE_LOOP('',(#54790,#54791,#54792,#54793)) ;
#22730 = EDGE_LOOP('',(#54794,#54795,#54796,#54797)) ;
#22731 = EDGE_LOOP('',(#54798,#54799,#54800,#54801)) ;
#22732 = EDGE_LOOP('',(#54802,#54803,#54804,#54805)) ;
#22733 = EDGE_LOOP('',(#54806,#54807,#54808,#54809)) ;
#22734 = EDGE_LOOP('',(#54810,#54811,#54812,#54813)) ;
#22735 = EDGE_LOOP('',(#54814,#54815,#54816,#54817)) ;
#22736 = EDGE_LOOP('',(#54818,#54819,#54820,#54821)) ;
#22737 = EDGE_LOOP('',(#54822,#54823,#54824,#54825)) ;
#22738 = EDGE_LOOP('',(#54826,#54827,#54828,#54829)) ;
#22739 = EDGE_LOOP('',(#54830,#54831,#54832,#54833)) ;
#22740 = EDGE_LOOP('',(#54834,#54835,#54836,#54837,#54838,#54839,#54840,#54841,
#54842,#54843)) ;
#22741 = EDGE_LOOP('',(#54844,#54845,#54846,#54847,#54848,#54849,#54850,#54851,
#54852,#54853)) ;
#22742 = EDGE_LOOP('',(#54854,#54855,#54856,#54857,#54858,#54859,#54860,#54861,
#54862,#54863)) ;
#22743 = EDGE_LOOP('',(#54864,#54865,#54866,#54867,#54868,#54869,#54870,#54871,
#54872,#54873)) ;
#22744 = EDGE_LOOP('',(#54874,#54875,#54876,#54877,#54878,#54879,#54880,#54881,
#54882,#54883)) ;
#22745 = EDGE_LOOP('',(#54884,#54885,#54886,#54887,#54888,#54889,#54890,#54891,
#54892,#54893)) ;
#22746 = EDGE_LOOP('',(#54894,#54895,#54896,#54897,#54898,#54899,#54900,#54901,
#54902,#54903)) ;
#22747 = EDGE_LOOP('',(#54904,#54905,#54906,#54907,#54908,#54909,#54910,#54911,
#54912,#54913)) ;
#22748 = EDGE_LOOP('',(#54914,#54915,#54916,#54917,#54918,#54919,#54920,#54921,
#54922,#54923)) ;
#22749 = EDGE_LOOP('',(#54924,#54925,#54926,#54927)) ;
#22750 = EDGE_LOOP('',(#54928,#54929,#54930,#54931)) ;
#22751 = EDGE_LOOP('',(#54932,#54933,#54934,#54935)) ;
#22752 = EDGE_LOOP('',(#54936,#54937,#54938,#54939)) ;
#22753 = EDGE_LOOP('',(#54940,#54941,#54942,#54943)) ;
#22754 = EDGE_LOOP('',(#54944,#54945,#54946,#54947)) ;
#22755 = EDGE_LOOP('',(#54948,#54949,#54950,#54951)) ;
#22756 = EDGE_LOOP('',(#54952,#54953,#54954,#54955)) ;
#22757 = EDGE_LOOP('',(#54956,#54957,#54958,#54959)) ;
#22758 = EDGE_LOOP('',(#54960,#54961,#54962,#54963)) ;
#22759 = EDGE_LOOP('',(#54964,#54965,#54966,#54967)) ;
#22760 = EDGE_LOOP('',(#54968,#54969,#54970,#54971)) ;
#22761 = EDGE_LOOP('',(#54972,#54973,#54974,#54975)) ;
#22762 = EDGE_LOOP('',(#54976,#54977,#54978,#54979)) ;
#22763 = EDGE_LOOP('',(#54980,#54981,#54982,#54983)) ;
#22764 = EDGE_LOOP('',(#54984,#54985,#54986,#54987)) ;
#22765 = EDGE_LOOP('',(#54988,#54989,#54990,#54991)) ;
#22766 = EDGE_LOOP('',(#54992,#54993,#54994,#54995)) ;
#22767 = EDGE_LOOP('',(#54996,#54997,#54998,#54999)) ;
#22768 = EDGE_LOOP('',(#55000,#55001,#55002,#55003)) ;
#22769 = EDGE_LOOP('',(#55004,#55005,#55006,#55007)) ;
#22770 = EDGE_LOOP('',(#55008,#55009,#55010,#55011)) ;
#22771 = EDGE_LOOP('',(#55012,#55013,#55014,#55015)) ;
#22772 = EDGE_LOOP('',(#55016,#55017,#55018,#55019)) ;
#22773 = EDGE_LOOP('',(#55020,#55021,#55022,#55023)) ;
#22774 = EDGE_LOOP('',(#55024,#55025,#55026,#55027)) ;
#22775 = EDGE_LOOP('',(#55028,#55029,#55030,#55031)) ;
#22776 = EDGE_LOOP('',(#55032,#55033,#55034,#55035)) ;
#22777 = EDGE_LOOP('',(#55036,#55037,#55038,#55039)) ;
#22778 = EDGE_LOOP('',(#55040,#55041,#55042,#55043)) ;
#22779 = EDGE_LOOP('',(#55044,#55045,#55046,#55047)) ;
#22780 = EDGE_LOOP('',(#55048,#55049,#55050,#55051)) ;
#22781 = EDGE_LOOP('',(#55052,#55053,#55054,#55055)) ;
#22782 = EDGE_LOOP('',(#55056,#55057,#55058,#55059)) ;
#22783 = EDGE_LOOP('',(#55060,#55061,#55062,#55063)) ;
#22784 = EDGE_LOOP('',(#55064,#55065,#55066,#55067)) ;
#22785 = EDGE_LOOP('',(#55068,#55069,#55070,#55071)) ;
#22786 = EDGE_LOOP('',(#55072,#55073,#55074,#55075)) ;
#22787 = EDGE_LOOP('',(#55076,#55077,#55078,#55079)) ;
#22788 = EDGE_LOOP('',(#55080,#55081,#55082,#55083)) ;
#22789 = EDGE_LOOP('',(#55084,#55085,#55086,#55087)) ;
#22790 = EDGE_LOOP('',(#55088,#55089,#55090,#55091)) ;
#22791 = EDGE_LOOP('',(#55092,#55093,#55094,#55095)) ;
#22792 = EDGE_LOOP('',(#55096,#55097,#55098,#55099)) ;
#22793 = EDGE_LOOP('',(#55100,#55101,#55102,#55103)) ;
#22794 = EDGE_LOOP('',(#55104,#55105,#55106,#55107)) ;
#22795 = EDGE_LOOP('',(#55108,#55109,#55110,#55111)) ;
#22796 = EDGE_LOOP('',(#55112,#55113,#55114,#55115)) ;
#22797 = EDGE_LOOP('',(#55116,#55117,#55118,#55119)) ;
#22798 = EDGE_LOOP('',(#55120,#55121,#55122,#55123)) ;
#22799 = EDGE_LOOP('',(#55124,#55125,#55126,#55127)) ;
#22800 = EDGE_LOOP('',(#55128,#55129,#55130,#55131)) ;
#22801 = EDGE_LOOP('',(#55132,#55133,#55134,#55135)) ;
#22802 = EDGE_LOOP('',(#55136,#55137,#55138,#55139)) ;
#22803 = EDGE_LOOP('',(#55140,#55141,#55142,#55143)) ;
#22804 = EDGE_LOOP('',(#55144,#55145,#55146,#55147)) ;
#22805 = EDGE_LOOP('',(#55148,#55149,#55150,#55151)) ;
#22806 = EDGE_LOOP('',(#55152,#55153,#55154,#55155)) ;
#22807 = EDGE_LOOP('',(#55156,#55157,#55158,#55159)) ;
#22808 = EDGE_LOOP('',(#55160,#55161,#55162,#55163)) ;
#22809 = EDGE_LOOP('',(#55164,#55165,#55166,#55167)) ;
#22810 = EDGE_LOOP('',(#55168,#55169,#55170,#55171)) ;
#22811 = EDGE_LOOP('',(#55172,#55173,#55174,#55175)) ;
#22812 = EDGE_LOOP('',(#55176,#55177,#55178,#55179)) ;
#22813 = EDGE_LOOP('',(#55180,#55181,#55182,#55183)) ;
#22814 = EDGE_LOOP('',(#55184,#55185,#55186,#55187)) ;
#22815 = EDGE_LOOP('',(#55188,#55189,#55190,#55191)) ;
#22816 = EDGE_LOOP('',(#55192,#55193,#55194,#55195)) ;
#22817 = EDGE_LOOP('',(#55196,#55197,#55198,#55199)) ;
#22818 = EDGE_LOOP('',(#55200,#55201,#55202,#55203)) ;
#22819 = EDGE_LOOP('',(#55204,#55205,#55206,#55207)) ;
#22820 = EDGE_LOOP('',(#55208,#55209,#55210,#55211)) ;
#22821 = EDGE_LOOP('',(#55212,#55213,#55214,#55215,#55216,#55217,#55218,#55219,
#55220,#55221,#55222,#55223,#55224,#55225,#55226,#55227,#55228,#55229)) ;
#22822 = EDGE_LOOP('',(#55230)) ;
#22823 = EDGE_LOOP('',(#55231,#55232,#55233,#55234)) ;
#22824 = EDGE_LOOP('',(#55235,#55236,#55237,#55238)) ;
#22825 = EDGE_LOOP('',(#55239,#55240,#55241,#55242)) ;
#22826 = EDGE_LOOP('',(#55243,#55244,#55245,#55246)) ;
#22827 = EDGE_LOOP('',(#55247,#55248,#55249,#55250)) ;
#22828 = EDGE_LOOP('',(#55251,#55252,#55253,#55254)) ;
#22829 = EDGE_LOOP('',(#55255,#55256,#55257,#55258)) ;
#22830 = EDGE_LOOP('',(#55259,#55260,#55261,#55262)) ;
#22831 = EDGE_LOOP('',(#55263,#55264,#55265,#55266)) ;
#22832 = EDGE_LOOP('',(#55267,#55268,#55269,#55270)) ;
#22833 = EDGE_LOOP('',(#55271,#55272,#55273,#55274)) ;
#22834 = EDGE_LOOP('',(#55275,#55276,#55277,#55278)) ;
#22835 = EDGE_LOOP('',(#55279,#55280,#55281,#55282)) ;
#22836 = EDGE_LOOP('',(#55283,#55284,#55285,#55286)) ;
#22837 = EDGE_LOOP('',(#55287,#55288,#55289,#55290)) ;
#22838 = EDGE_LOOP('',(#55291,#55292,#55293,#55294)) ;
#22839 = EDGE_LOOP('',(#55295,#55296,#55297,#55298)) ;
#22840 = EDGE_LOOP('',(#55299,#55300,#55301,#55302)) ;
#22841 = EDGE_LOOP('',(#55303,#55304,#55305,#55306)) ;
#22842 = EDGE_LOOP('',(#55307,#55308,#55309,#55310)) ;
#22843 = EDGE_LOOP('',(#55311,#55312,#55313,#55314)) ;
#22844 = EDGE_LOOP('',(#55315,#55316,#55317,#55318)) ;
#22845 = EDGE_LOOP('',(#55319,#55320,#55321,#55322)) ;
#22846 = EDGE_LOOP('',(#55323,#55324,#55325,#55326)) ;
#22847 = EDGE_LOOP('',(#55327,#55328,#55329,#55330)) ;
#22848 = EDGE_LOOP('',(#55331,#55332,#55333,#55334)) ;
#22849 = EDGE_LOOP('',(#55335,#55336,#55337,#55338)) ;
#22850 = EDGE_LOOP('',(#55339,#55340,#55341,#55342,#55343,#55344,#55345,#55346,
#55347,#55348,#55349,#55350,#55351,#55352,#55353,#55354,#55355,#55356)) ;
#22851 = EDGE_LOOP('',(#55357)) ;
#22852 = EDGE_LOOP('',(#55358,#55359,#55360,#55361)) ;
#22853 = EDGE_LOOP('',(#55362,#55363,#55364,#55365)) ;
#22854 = EDGE_LOOP('',(#55366,#55367,#55368,#55369)) ;
#22855 = EDGE_LOOP('',(#55370,#55371,#55372,#55373)) ;
#22856 = EDGE_LOOP('',(#55374,#55375,#55376,#55377)) ;
#22857 = EDGE_LOOP('',(#55378,#55379,#55380,#55381)) ;
#22858 = EDGE_LOOP('',(#55382,#55383,#55384,#55385)) ;
#22859 = EDGE_LOOP('',(#55386,#55387,#55388,#55389)) ;
#22860 = EDGE_LOOP('',(#55390,#55391,#55392,#55393)) ;
#22861 = EDGE_LOOP('',(#55394,#55395,#55396,#55397)) ;
#22862 = EDGE_LOOP('',(#55398,#55399,#55400,#55401)) ;
#22863 = EDGE_LOOP('',(#55402,#55403,#55404,#55405)) ;
#22864 = EDGE_LOOP('',(#55406,#55407,#55408,#55409)) ;
#22865 = EDGE_LOOP('',(#55410,#55411,#55412,#55413)) ;
#22866 = EDGE_LOOP('',(#55414,#55415,#55416,#55417)) ;
#22867 = EDGE_LOOP('',(#55418,#55419,#55420,#55421)) ;
#22868 = EDGE_LOOP('',(#55422,#55423,#55424,#55425)) ;
#22869 = EDGE_LOOP('',(#55426,#55427,#55428,#55429)) ;
#22870 = EDGE_LOOP('',(#55430,#55431,#55432,#55433)) ;
#22871 = EDGE_LOOP('',(#55434,#55435,#55436,#55437)) ;
#22872 = EDGE_LOOP('',(#55438,#55439,#55440,#55441)) ;
#22873 = EDGE_LOOP('',(#55442,#55443,#55444,#55445)) ;
#22874 = EDGE_LOOP('',(#55446,#55447,#55448,#55449)) ;
#22875 = EDGE_LOOP('',(#55450,#55451,#55452,#55453)) ;
#22876 = EDGE_LOOP('',(#55454,#55455,#55456,#55457)) ;
#22877 = EDGE_LOOP('',(#55458,#55459,#55460,#55461)) ;
#22878 = EDGE_LOOP('',(#55462,#55463,#55464,#55465)) ;
#22879 = EDGE_LOOP('',(#55466,#55467,#55468,#55469,#55470,#55471,#55472,#55473,
#55474,#55475,#55476,#55477,#55478,#55479,#55480,#55481,#55482,#55483)) ;
#22880 = EDGE_LOOP('',(#55484)) ;
#22881 = EDGE_LOOP('',(#55485,#55486,#55487,#55488)) ;
#22882 = EDGE_LOOP('',(#55489,#55490,#55491,#55492)) ;
#22883 = EDGE_LOOP('',(#55493,#55494,#55495,#55496)) ;
#22884 = EDGE_LOOP('',(#55497,#55498,#55499,#55500)) ;
#22885 = EDGE_LOOP('',(#55501,#55502,#55503,#55504)) ;
#22886 = EDGE_LOOP('',(#55505,#55506,#55507,#55508)) ;
#22887 = EDGE_LOOP('',(#55509,#55510,#55511,#55512)) ;
#22888 = EDGE_LOOP('',(#55513,#55514,#55515,#55516)) ;
#22889 = EDGE_LOOP('',(#55517,#55518,#55519,#55520)) ;
#22890 = EDGE_LOOP('',(#55521,#55522,#55523,#55524)) ;
#22891 = EDGE_LOOP('',(#55525,#55526,#55527,#55528)) ;
#22892 = EDGE_LOOP('',(#55529,#55530,#55531,#55532)) ;
#22893 = EDGE_LOOP('',(#55533,#55534,#55535,#55536)) ;
#22894 = EDGE_LOOP('',(#55537,#55538,#55539,#55540)) ;
#22895 = EDGE_LOOP('',(#55541,#55542,#55543,#55544)) ;
#22896 = EDGE_LOOP('',(#55545,#55546,#55547,#55548)) ;
#22897 = EDGE_LOOP('',(#55549,#55550,#55551,#55552)) ;
#22898 = EDGE_LOOP('',(#55553,#55554,#55555,#55556)) ;
#22899 = EDGE_LOOP('',(#55557,#55558,#55559,#55560)) ;
#22900 = EDGE_LOOP('',(#55561,#55562,#55563,#55564)) ;
#22901 = EDGE_LOOP('',(#55565,#55566,#55567,#55568)) ;
#22902 = EDGE_LOOP('',(#55569,#55570,#55571,#55572)) ;
#22903 = EDGE_LOOP('',(#55573,#55574,#55575,#55576)) ;
#22904 = EDGE_LOOP('',(#55577,#55578,#55579,#55580)) ;
#22905 = EDGE_LOOP('',(#55581,#55582,#55583,#55584)) ;
#22906 = EDGE_LOOP('',(#55585,#55586,#55587,#55588)) ;
#22907 = EDGE_LOOP('',(#55589,#55590,#55591,#55592)) ;
#22908 = EDGE_LOOP('',(#55593,#55594,#55595,#55596,#55597,#55598,#55599,#55600,
#55601,#55602,#55603,#55604,#55605,#55606,#55607,#55608,#55609,#55610)) ;
#22909 = EDGE_LOOP('',(#55611)) ;
#22910 = EDGE_LOOP('',(#55612,#55613,#55614,#55615)) ;
#22911 = EDGE_LOOP('',(#55616,#55617,#55618,#55619)) ;
#22912 = EDGE_LOOP('',(#55620,#55621,#55622,#55623)) ;
#22913 = EDGE_LOOP('',(#55624,#55625,#55626,#55627)) ;
#22914 = EDGE_LOOP('',(#55628,#55629,#55630,#55631)) ;
#22915 = EDGE_LOOP('',(#55632,#55633,#55634,#55635)) ;
#22916 = EDGE_LOOP('',(#55636,#55637,#55638,#55639)) ;
#22917 = EDGE_LOOP('',(#55640,#55641,#55642,#55643)) ;
#22918 = EDGE_LOOP('',(#55644,#55645,#55646,#55647)) ;
#22919 = EDGE_LOOP('',(#55648,#55649,#55650,#55651)) ;
#22920 = EDGE_LOOP('',(#55652,#55653,#55654,#55655)) ;
#22921 = EDGE_LOOP('',(#55656,#55657,#55658,#55659)) ;
#22922 = EDGE_LOOP('',(#55660,#55661,#55662,#55663)) ;
#22923 = EDGE_LOOP('',(#55664,#55665,#55666,#55667)) ;
#22924 = EDGE_LOOP('',(#55668,#55669,#55670,#55671)) ;
#22925 = EDGE_LOOP('',(#55672,#55673,#55674,#55675)) ;
#22926 = EDGE_LOOP('',(#55676,#55677,#55678,#55679)) ;
#22927 = EDGE_LOOP('',(#55680,#55681,#55682,#55683)) ;
#22928 = EDGE_LOOP('',(#55684,#55685,#55686,#55687)) ;
#22929 = EDGE_LOOP('',(#55688,#55689,#55690,#55691)) ;
#22930 = EDGE_LOOP('',(#55692,#55693,#55694,#55695)) ;
#22931 = EDGE_LOOP('',(#55696,#55697,#55698,#55699)) ;
#22932 = EDGE_LOOP('',(#55700,#55701,#55702,#55703)) ;
#22933 = EDGE_LOOP('',(#55704,#55705,#55706,#55707)) ;
#22934 = EDGE_LOOP('',(#55708,#55709,#55710,#55711)) ;
#22935 = EDGE_LOOP('',(#55712,#55713,#55714,#55715)) ;
#22936 = EDGE_LOOP('',(#55716,#55717,#55718,#55719)) ;
#22937 = EDGE_LOOP('',(#55720,#55721,#55722,#55723,#55724,#55725,#55726,#55727,
#55728,#55729,#55730,#55731,#55732,#55733,#55734,#55735,#55736,#55737)) ;
#22938 = EDGE_LOOP('',(#55738)) ;
#22939 = EDGE_LOOP('',(#55739,#55740,#55741,#55742)) ;
#22940 = EDGE_LOOP('',(#55743,#55744,#55745,#55746)) ;
#22941 = EDGE_LOOP('',(#55747,#55748,#55749,#55750)) ;
#22942 = EDGE_LOOP('',(#55751,#55752,#55753,#55754)) ;
#22943 = EDGE_LOOP('',(#55755,#55756,#55757,#55758)) ;
#22944 = EDGE_LOOP('',(#55759,#55760,#55761,#55762)) ;
#22945 = EDGE_LOOP('',(#55763,#55764,#55765,#55766)) ;
#22946 = EDGE_LOOP('',(#55767,#55768,#55769,#55770)) ;
#22947 = EDGE_LOOP('',(#55771,#55772,#55773,#55774)) ;
#22948 = EDGE_LOOP('',(#55775,#55776,#55777,#55778)) ;
#22949 = EDGE_LOOP('',(#55779,#55780,#55781,#55782)) ;
#22950 = EDGE_LOOP('',(#55783,#55784,#55785,#55786)) ;
#22951 = EDGE_LOOP('',(#55787,#55788,#55789,#55790)) ;
#22952 = EDGE_LOOP('',(#55791,#55792,#55793,#55794)) ;
#22953 = EDGE_LOOP('',(#55795,#55796,#55797,#55798)) ;
#22954 = EDGE_LOOP('',(#55799,#55800,#55801,#55802)) ;
#22955 = EDGE_LOOP('',(#55803,#55804,#55805,#55806)) ;
#22956 = EDGE_LOOP('',(#55807,#55808,#55809,#55810)) ;
#22957 = EDGE_LOOP('',(#55811,#55812,#55813,#55814)) ;
#22958 = EDGE_LOOP('',(#55815,#55816,#55817,#55818)) ;
#22959 = EDGE_LOOP('',(#55819,#55820,#55821,#55822)) ;
#22960 = EDGE_LOOP('',(#55823,#55824,#55825,#55826)) ;
#22961 = EDGE_LOOP('',(#55827,#55828,#55829,#55830)) ;
#22962 = EDGE_LOOP('',(#55831,#55832,#55833,#55834)) ;
#22963 = EDGE_LOOP('',(#55835,#55836,#55837,#55838)) ;
#22964 = EDGE_LOOP('',(#55839,#55840,#55841,#55842)) ;
#22965 = EDGE_LOOP('',(#55843,#55844,#55845,#55846)) ;
#22966 = EDGE_LOOP('',(#55847,#55848,#55849,#55850,#55851,#55852,#55853,#55854,
#55855,#55856,#55857,#55858,#55859,#55860,#55861,#55862,#55863,#55864)) ;
#22967 = EDGE_LOOP('',(#55865)) ;
#22968 = EDGE_LOOP('',(#55866,#55867,#55868,#55869)) ;
#22969 = EDGE_LOOP('',(#55870,#55871,#55872,#55873)) ;
#22970 = EDGE_LOOP('',(#55874,#55875,#55876,#55877)) ;
#22971 = EDGE_LOOP('',(#55878,#55879,#55880,#55881)) ;
#22972 = EDGE_LOOP('',(#55882,#55883,#55884,#55885)) ;
#22973 = EDGE_LOOP('',(#55886,#55887,#55888,#55889)) ;
#22974 = EDGE_LOOP('',(#55890,#55891,#55892,#55893)) ;
#22975 = EDGE_LOOP('',(#55894,#55895,#55896,#55897)) ;
#22976 = EDGE_LOOP('',(#55898,#55899,#55900,#55901)) ;
#22977 = EDGE_LOOP('',(#55902,#55903,#55904,#55905)) ;
#22978 = EDGE_LOOP('',(#55906,#55907,#55908,#55909)) ;
#22979 = EDGE_LOOP('',(#55910,#55911,#55912,#55913)) ;
#22980 = EDGE_LOOP('',(#55914,#55915,#55916,#55917)) ;
#22981 = EDGE_LOOP('',(#55918,#55919,#55920,#55921)) ;
#22982 = EDGE_LOOP('',(#55922,#55923,#55924,#55925)) ;
#22983 = EDGE_LOOP('',(#55926,#55927,#55928,#55929)) ;
#22984 = EDGE_LOOP('',(#55930,#55931,#55932,#55933)) ;
#22985 = EDGE_LOOP('',(#55934,#55935,#55936,#55937)) ;
#22986 = EDGE_LOOP('',(#55938,#55939,#55940,#55941)) ;
#22987 = EDGE_LOOP('',(#55942,#55943,#55944,#55945)) ;
#22988 = EDGE_LOOP('',(#55946,#55947,#55948,#55949)) ;
#22989 = EDGE_LOOP('',(#55950,#55951,#55952,#55953)) ;
#22990 = EDGE_LOOP('',(#55954,#55955,#55956,#55957)) ;
#22991 = EDGE_LOOP('',(#55958,#55959,#55960,#55961)) ;
#22992 = EDGE_LOOP('',(#55962,#55963,#55964,#55965)) ;
#22993 = EDGE_LOOP('',(#55966,#55967,#55968,#55969)) ;
#22994 = EDGE_LOOP('',(#55970,#55971,#55972,#55973)) ;
#22995 = EDGE_LOOP('',(#55974,#55975,#55976,#55977,#55978,#55979,#55980,#55981,
#55982,#55983,#55984,#55985,#55986,#55987,#55988,#55989,#55990,#55991)) ;
#22996 = EDGE_LOOP('',(#55992)) ;
#22997 = EDGE_LOOP('',(#55993,#55994,#55995,#55996)) ;
#22998 = EDGE_LOOP('',(#55997,#55998,#55999,#56000)) ;
#22999 = EDGE_LOOP('',(#56001,#56002,#56003,#56004)) ;
#23000 = EDGE_LOOP('',(#56005,#56006,#56007,#56008)) ;
#23001 = EDGE_LOOP('',(#56009,#56010,#56011,#56012)) ;
#23002 = EDGE_LOOP('',(#56013,#56014,#56015,#56016)) ;
#23003 = EDGE_LOOP('',(#56017,#56018,#56019,#56020)) ;
#23004 = EDGE_LOOP('',(#56021,#56022,#56023,#56024)) ;
#23005 = EDGE_LOOP('',(#56025,#56026,#56027,#56028)) ;
#23006 = EDGE_LOOP('',(#56029,#56030,#56031,#56032)) ;
#23007 = EDGE_LOOP('',(#56033,#56034,#56035,#56036)) ;
#23008 = EDGE_LOOP('',(#56037,#56038,#56039,#56040)) ;
#23009 = EDGE_LOOP('',(#56041,#56042,#56043,#56044)) ;
#23010 = EDGE_LOOP('',(#56045,#56046,#56047,#56048)) ;
#23011 = EDGE_LOOP('',(#56049,#56050,#56051,#56052)) ;
#23012 = EDGE_LOOP('',(#56053,#56054,#56055,#56056)) ;
#23013 = EDGE_LOOP('',(#56057,#56058,#56059,#56060)) ;
#23014 = EDGE_LOOP('',(#56061,#56062,#56063,#56064)) ;
#23015 = EDGE_LOOP('',(#56065,#56066,#56067,#56068)) ;
#23016 = EDGE_LOOP('',(#56069,#56070,#56071,#56072)) ;
#23017 = EDGE_LOOP('',(#56073,#56074,#56075,#56076)) ;
#23018 = EDGE_LOOP('',(#56077,#56078,#56079,#56080)) ;
#23019 = EDGE_LOOP('',(#56081,#56082,#56083,#56084)) ;
#23020 = EDGE_LOOP('',(#56085,#56086,#56087,#56088)) ;
#23021 = EDGE_LOOP('',(#56089,#56090,#56091,#56092)) ;
#23022 = EDGE_LOOP('',(#56093,#56094,#56095,#56096)) ;
#23023 = EDGE_LOOP('',(#56097,#56098,#56099,#56100)) ;
#23024 = EDGE_LOOP('',(#56101,#56102,#56103,#56104,#56105,#56106,#56107,#56108,
#56109,#56110,#56111,#56112,#56113,#56114,#56115,#56116,#56117,#56118)) ;
#23025 = EDGE_LOOP('',(#56119)) ;
#23026 = EDGE_LOOP('',(#56120,#56121,#56122,#56123)) ;
#23027 = EDGE_LOOP('',(#56124,#56125,#56126,#56127)) ;
#23028 = EDGE_LOOP('',(#56128,#56129,#56130,#56131)) ;
#23029 = EDGE_LOOP('',(#56132,#56133,#56134,#56135)) ;
#23030 = EDGE_LOOP('',(#56136,#56137,#56138,#56139)) ;
#23031 = EDGE_LOOP('',(#56140,#56141,#56142,#56143)) ;
#23032 = EDGE_LOOP('',(#56144,#56145,#56146,#56147)) ;
#23033 = EDGE_LOOP('',(#56148,#56149,#56150,#56151)) ;
#23034 = EDGE_LOOP('',(#56152,#56153,#56154,#56155)) ;
#23035 = EDGE_LOOP('',(#56156,#56157,#56158,#56159)) ;
#23036 = EDGE_LOOP('',(#56160,#56161,#56162,#56163)) ;
#23037 = EDGE_LOOP('',(#56164,#56165,#56166,#56167)) ;
#23038 = EDGE_LOOP('',(#56168,#56169,#56170,#56171)) ;
#23039 = EDGE_LOOP('',(#56172,#56173,#56174,#56175)) ;
#23040 = EDGE_LOOP('',(#56176,#56177,#56178,#56179)) ;
#23041 = EDGE_LOOP('',(#56180,#56181,#56182,#56183)) ;
#23042 = EDGE_LOOP('',(#56184,#56185,#56186,#56187)) ;
#23043 = EDGE_LOOP('',(#56188,#56189,#56190,#56191)) ;
#23044 = EDGE_LOOP('',(#56192,#56193,#56194,#56195)) ;
#23045 = EDGE_LOOP('',(#56196,#56197,#56198,#56199)) ;
#23046 = EDGE_LOOP('',(#56200,#56201,#56202,#56203)) ;
#23047 = EDGE_LOOP('',(#56204,#56205,#56206,#56207)) ;
#23048 = EDGE_LOOP('',(#56208,#56209,#56210,#56211)) ;
#23049 = EDGE_LOOP('',(#56212,#56213,#56214,#56215)) ;
#23050 = EDGE_LOOP('',(#56216,#56217,#56218,#56219)) ;
#23051 = EDGE_LOOP('',(#56220,#56221,#56222,#56223)) ;
#23052 = EDGE_LOOP('',(#56224,#56225,#56226,#56227)) ;
#23053 = EDGE_LOOP('',(#56228,#56229,#56230,#56231,#56232,#56233,#56234,#56235,
#56236,#56237,#56238,#56239,#56240,#56241,#56242,#56243,#56244,#56245)) ;
#23054 = EDGE_LOOP('',(#56246)) ;
#23055 = EDGE_LOOP('',(#56247)) ;
#23056 = EDGE_LOOP('',(#56248,#56249,#56250,#56251,#56252,#56253,#56254,#56255)) ;
#23057 = EDGE_LOOP('',(#56256)) ;
#23058 = EDGE_LOOP('',(#56257,#56258,#56259,#56260,#56261,#56262,#56263,#56264)) ;
#23059 = EDGE_LOOP('',(#56265)) ;
#23060 = EDGE_LOOP('',(#56266,#56267,#56268,#56269,#56270,#56271,#56272,#56273)) ;
#23061 = EDGE_LOOP('',(#56274)) ;
#23062 = EDGE_LOOP('',(#56275,#56276,#56277,#56278,#56279,#56280,#56281,#56282)) ;
#23063 = EDGE_LOOP('',(#56283)) ;
#23064 = EDGE_LOOP('',(#56284,#56285,#56286,#56287,#56288,#56289,#56290,#56291)) ;
#23065 = EDGE_LOOP('',(#56292)) ;
#23066 = EDGE_LOOP('',(#56293,#56294,#56295,#56296,#56297,#56298,#56299,#56300)) ;
#23067 = EDGE_LOOP('',(#56301)) ;
#23068 = EDGE_LOOP('',(#56302,#56303,#56304,#56305,#56306,#56307,#56308,#56309)) ;
#23069 = EDGE_LOOP('',(#56310)) ;
#23070 = EDGE_LOOP('',(#56311,#56312,#56313,#56314,#56315,#56316,#56317,#56318)) ;
#23071 = EDGE_LOOP('',(#56319)) ;
#23072 = EDGE_LOOP('',(#56320,#56321,#56322,#56323,#56324,#56325,#56326,#56327)) ;
#23073 = EDGE_LOOP('',(#56328,#56329,#56330,#56331)) ;
#23074 = EDGE_LOOP('',(#56332,#56333,#56334,#56335)) ;
#23075 = EDGE_LOOP('',(#56336,#56337,#56338)) ;
#23076 = EDGE_LOOP('',(#56339,#56340,#56341)) ;
#23077 = EDGE_LOOP('',(#56342,#56343,#56344,#56345)) ;
#23078 = EDGE_LOOP('',(#56346,#56347,#56348,#56349,#56350,#56351)) ;
#23079 = EDGE_LOOP('',(#56352,#56353,#56354,#56355,#56356,#56357,#56358)) ;
#23080 = EDGE_LOOP('',(#56359,#56360,#56361,#56362)) ;
#23081 = EDGE_LOOP('',(#56363,#56364,#56365,#56366)) ;
#23082 = EDGE_LOOP('',(#56367,#56368,#56369,#56370)) ;
#23083 = EDGE_LOOP('',(#56371,#56372,#56373,#56374)) ;
#23084 = EDGE_LOOP('',(#56375,#56376,#56377)) ;
#23085 = EDGE_LOOP('',(#56378,#56379,#56380,#56381)) ;
#23086 = EDGE_LOOP('',(#56382,#56383,#56384,#56385)) ;
#23087 = EDGE_LOOP('',(#56386,#56387,#56388,#56389)) ;
#23088 = EDGE_LOOP('',(#56390,#56391,#56392,#56393)) ;
#23089 = EDGE_LOOP('',(#56394,#56395,#56396,#56397)) ;
#23090 = EDGE_LOOP('',(#56398,#56399,#56400,#56401)) ;
#23091 = EDGE_LOOP('',(#56402,#56403,#56404,#56405)) ;
#23092 = EDGE_LOOP('',(#56406,#56407,#56408,#56409)) ;
#23093 = EDGE_LOOP('',(#56410,#56411,#56412,#56413)) ;
#23094 = EDGE_LOOP('',(#56414,#56415,#56416)) ;
#23095 = EDGE_LOOP('',(#56417,#56418,#56419)) ;
#23096 = EDGE_LOOP('',(#56420,#56421,#56422,#56423,#56424)) ;
#23097 = EDGE_LOOP('',(#56425,#56426,#56427)) ;
#23098 = EDGE_LOOP('',(#56428,#56429,#56430)) ;
#23099 = EDGE_LOOP('',(#56431,#56432,#56433,#56434)) ;
#23100 = EDGE_LOOP('',(#56435,#56436,#56437,#56438)) ;
#23101 = EDGE_LOOP('',(#56439,#56440,#56441,#56442)) ;
#23102 = EDGE_LOOP('',(#56443,#56444,#56445,#56446)) ;
#23103 = EDGE_LOOP('',(#56447,#56448,#56449,#56450)) ;
#23104 = EDGE_LOOP('',(#56451,#56452,#56453,#56454)) ;
#23105 = EDGE_LOOP('',(#56455,#56456,#56457,#56458)) ;
#23106 = EDGE_LOOP('',(#56459,#56460,#56461)) ;
#23107 = EDGE_LOOP('',(#56462,#56463,#56464,#56465)) ;
#23108 = EDGE_LOOP('',(#56466,#56467,#56468,#56469)) ;
#23109 = EDGE_LOOP('',(#56470,#56471,#56472)) ;
#23110 = EDGE_LOOP('',(#56473,#56474,#56475,#56476)) ;
#23111 = EDGE_LOOP('',(#56477,#56478,#56479,#56480)) ;
#23112 = EDGE_LOOP('',(#56481,#56482,#56483,#56484)) ;
#23113 = EDGE_LOOP('',(#56485,#56486,#56487,#56488)) ;
#23114 = EDGE_LOOP('',(#56489,#56490,#56491,#56492)) ;
#23115 = EDGE_LOOP('',(#56493,#56494,#56495,#56496)) ;
#23116 = EDGE_LOOP('',(#56497,#56498,#56499,#56500,#56501)) ;
#23117 = EDGE_LOOP('',(#56502,#56503,#56504,#56505)) ;
#23118 = EDGE_LOOP('',(#56506,#56507,#56508)) ;
#23119 = EDGE_LOOP('',(#56509,#56510,#56511,#56512)) ;
#23120 = EDGE_LOOP('',(#56513,#56514,#56515,#56516)) ;
#23121 = EDGE_LOOP('',(#56517,#56518,#56519)) ;
#23122 = EDGE_LOOP('',(#56520,#56521,#56522,#56523)) ;
#23123 = EDGE_LOOP('',(#56524,#56525,#56526,#56527)) ;
#23124 = EDGE_LOOP('',(#56528,#56529,#56530,#56531)) ;
#23125 = EDGE_LOOP('',(#56532,#56533,#56534)) ;
#23126 = EDGE_LOOP('',(#56535,#56536,#56537,#56538)) ;
#23127 = EDGE_LOOP('',(#56539,#56540,#56541,#56542)) ;
#23128 = EDGE_LOOP('',(#56543,#56544,#56545)) ;
#23129 = EDGE_LOOP('',(#56546,#56547,#56548)) ;
#23130 = EDGE_LOOP('',(#56549,#56550,#56551,#56552)) ;
#23131 = EDGE_LOOP('',(#56553,#56554,#56555,#56556)) ;
#23132 = EDGE_LOOP('',(#56557,#56558,#56559)) ;
#23133 = EDGE_LOOP('',(#56560,#56561,#56562)) ;
#23134 = EDGE_LOOP('',(#56563,#56564,#56565,#56566)) ;
#23135 = EDGE_LOOP('',(#56567,#56568,#56569,#56570)) ;
#23136 = EDGE_LOOP('',(#56571,#56572,#56573)) ;
#23137 = EDGE_LOOP('',(#56574,#56575,#56576,#56577)) ;
#23138 = EDGE_LOOP('',(#56578,#56579,#56580,#56581)) ;
#23139 = EDGE_LOOP('',(#56582,#56583,#56584)) ;
#23140 = EDGE_LOOP('',(#56585,#56586,#56587)) ;
#23141 = EDGE_LOOP('',(#56588,#56589,#56590,#56591)) ;
#23142 = EDGE_LOOP('',(#56592,#56593,#56594,#56595)) ;
#23143 = EDGE_LOOP('',(#56596,#56597,#56598,#56599)) ;
#23144 = EDGE_LOOP('',(#56600,#56601,#56602,#56603)) ;
#23145 = EDGE_LOOP('',(#56604,#56605,#56606,#56607)) ;
#23146 = EDGE_LOOP('',(#56608,#56609,#56610,#56611)) ;
#23147 = EDGE_LOOP('',(#56612,#56613,#56614)) ;
#23148 = EDGE_LOOP('',(#56615,#56616,#56617)) ;
#23149 = EDGE_LOOP('',(#56618,#56619,#56620,#56621)) ;
#23150 = EDGE_LOOP('',(#56622,#56623,#56624,#56625)) ;
#23151 = EDGE_LOOP('',(#56626,#56627,#56628,#56629)) ;
#23152 = EDGE_LOOP('',(#56630,#56631,#56632,#56633)) ;
#23153 = EDGE_LOOP('',(#56634,#56635,#56636,#56637)) ;
#23154 = EDGE_LOOP('',(#56638,#56639,#56640,#56641)) ;
#23155 = EDGE_LOOP('',(#56642,#56643,#56644,#56645)) ;
#23156 = EDGE_LOOP('',(#56646,#56647,#56648,#56649)) ;
#23157 = EDGE_LOOP('',(#56650,#56651,#56652,#56653)) ;
#23158 = EDGE_LOOP('',(#56654,#56655,#56656,#56657)) ;
#23159 = EDGE_LOOP('',(#56658,#56659,#56660,#56661)) ;
#23160 = EDGE_LOOP('',(#56662,#56663,#56664,#56665)) ;
#23161 = EDGE_LOOP('',(#56666,#56667,#56668,#56669)) ;
#23162 = EDGE_LOOP('',(#56670,#56671,#56672,#56673)) ;
#23163 = EDGE_LOOP('',(#56674,#56675,#56676,#56677)) ;
#23164 = EDGE_LOOP('',(#56678,#56679,#56680,#56681)) ;
#23165 = EDGE_LOOP('',(#56682,#56683,#56684,#56685)) ;
#23166 = EDGE_LOOP('',(#56686,#56687,#56688)) ;
#23167 = EDGE_LOOP('',(#56689,#56690,#56691,#56692)) ;
#23168 = EDGE_LOOP('',(#56693,#56694,#56695,#56696)) ;
#23169 = EDGE_LOOP('',(#56697,#56698,#56699,#56700)) ;
#23170 = EDGE_LOOP('',(#56701,#56702,#56703)) ;
#23171 = EDGE_LOOP('',(#56704,#56705,#56706,#56707)) ;
#23172 = EDGE_LOOP('',(#56708,#56709,#56710,#56711)) ;
#23173 = EDGE_LOOP('',(#56712,#56713,#56714,#56715)) ;
#23174 = EDGE_LOOP('',(#56716,#56717,#56718)) ;
#23175 = EDGE_LOOP('',(#56719,#56720,#56721)) ;
#23176 = EDGE_LOOP('',(#56722,#56723,#56724,#56725)) ;
#23177 = EDGE_LOOP('',(#56726,#56727,#56728,#56729)) ;
#23178 = EDGE_LOOP('',(#56730,#56731,#56732,#56733)) ;
#23179 = EDGE_LOOP('',(#56734,#56735,#56736,#56737)) ;
#23180 = EDGE_LOOP('',(#56738,#56739,#56740,#56741)) ;
#23181 = EDGE_LOOP('',(#56742,#56743,#56744,#56745)) ;
#23182 = EDGE_LOOP('',(#56746,#56747,#56748,#56749)) ;
#23183 = EDGE_LOOP('',(#56750,#56751,#56752,#56753)) ;
#23184 = EDGE_LOOP('',(#56754,#56755,#56756,#56757)) ;
#23185 = EDGE_LOOP('',(#56758,#56759,#56760,#56761)) ;
#23186 = EDGE_LOOP('',(#56762,#56763,#56764,#56765)) ;
#23187 = EDGE_LOOP('',(#56766,#56767,#56768,#56769)) ;
#23188 = EDGE_LOOP('',(#56770,#56771,#56772,#56773)) ;
#23189 = EDGE_LOOP('',(#56774,#56775,#56776,#56777)) ;
#23190 = EDGE_LOOP('',(#56778,#56779,#56780,#56781)) ;
#23191 = EDGE_LOOP('',(#56782,#56783,#56784,#56785)) ;
#23192 = EDGE_LOOP('',(#56786,#56787,#56788,#56789)) ;
#23193 = EDGE_LOOP('',(#56790,#56791,#56792)) ;
#23194 = EDGE_LOOP('',(#56793,#56794,#56795,#56796)) ;
#23195 = EDGE_LOOP('',(#56797,#56798,#56799,#56800)) ;
#23196 = EDGE_LOOP('',(#56801,#56802,#56803,#56804)) ;
#23197 = EDGE_LOOP('',(#56805,#56806,#56807)) ;
#23198 = EDGE_LOOP('',(#56808,#56809,#56810,#56811)) ;
#23199 = EDGE_LOOP('',(#56812,#56813,#56814,#56815)) ;
#23200 = EDGE_LOOP('',(#56816,#56817,#56818,#56819)) ;
#23201 = EDGE_LOOP('',(#56820,#56821,#56822)) ;
#23202 = EDGE_LOOP('',(#56823,#56824,#56825)) ;
#23203 = EDGE_LOOP('',(#56826,#56827,#56828,#56829)) ;
#23204 = EDGE_LOOP('',(#56830,#56831,#56832,#56833)) ;
#23205 = EDGE_LOOP('',(#56834,#56835,#56836,#56837)) ;
#23206 = EDGE_LOOP('',(#56838,#56839,#56840,#56841)) ;
#23207 = EDGE_LOOP('',(#56842,#56843,#56844,#56845)) ;
#23208 = EDGE_LOOP('',(#56846,#56847,#56848,#56849)) ;
#23209 = EDGE_LOOP('',(#56850,#56851,#56852,#56853)) ;
#23210 = EDGE_LOOP('',(#56854,#56855,#56856,#56857)) ;
#23211 = EDGE_LOOP('',(#56858,#56859,#56860,#56861)) ;
#23212 = EDGE_LOOP('',(#56862,#56863,#56864,#56865)) ;
#23213 = EDGE_LOOP('',(#56866,#56867,#56868,#56869)) ;
#23214 = EDGE_LOOP('',(#56870,#56871,#56872,#56873)) ;
#23215 = EDGE_LOOP('',(#56874,#56875,#56876,#56877)) ;
#23216 = EDGE_LOOP('',(#56878,#56879,#56880,#56881)) ;
#23217 = EDGE_LOOP('',(#56882,#56883,#56884,#56885)) ;
#23218 = EDGE_LOOP('',(#56886,#56887,#56888,#56889)) ;
#23219 = EDGE_LOOP('',(#56890,#56891,#56892,#56893)) ;
#23220 = EDGE_LOOP('',(#56894,#56895,#56896)) ;
#23221 = EDGE_LOOP('',(#56897,#56898,#56899,#56900)) ;
#23222 = EDGE_LOOP('',(#56901,#56902,#56903,#56904)) ;
#23223 = EDGE_LOOP('',(#56905,#56906,#56907,#56908)) ;
#23224 = EDGE_LOOP('',(#56909,#56910,#56911)) ;
#23225 = EDGE_LOOP('',(#56912,#56913,#56914,#56915)) ;
#23226 = EDGE_LOOP('',(#56916,#56917,#56918,#56919)) ;
#23227 = EDGE_LOOP('',(#56920,#56921,#56922,#56923)) ;
#23228 = EDGE_LOOP('',(#56924,#56925,#56926)) ;
#23229 = EDGE_LOOP('',(#56927,#56928,#56929)) ;
#23230 = EDGE_LOOP('',(#56930,#56931,#56932,#56933)) ;
#23231 = EDGE_LOOP('',(#56934,#56935,#56936,#56937)) ;
#23232 = EDGE_LOOP('',(#56938,#56939,#56940,#56941)) ;
#23233 = EDGE_LOOP('',(#56942,#56943,#56944,#56945)) ;
#23234 = EDGE_LOOP('',(#56946,#56947,#56948,#56949)) ;
#23235 = EDGE_LOOP('',(#56950,#56951,#56952,#56953)) ;
#23236 = EDGE_LOOP('',(#56954,#56955,#56956,#56957)) ;
#23237 = EDGE_LOOP('',(#56958,#56959,#56960,#56961)) ;
#23238 = EDGE_LOOP('',(#56962,#56963,#56964,#56965)) ;
#23239 = EDGE_LOOP('',(#56966,#56967,#56968,#56969)) ;
#23240 = EDGE_LOOP('',(#56970,#56971,#56972,#56973)) ;
#23241 = EDGE_LOOP('',(#56974,#56975,#56976,#56977)) ;
#23242 = EDGE_LOOP('',(#56978,#56979,#56980,#56981)) ;
#23243 = EDGE_LOOP('',(#56982,#56983,#56984,#56985)) ;
#23244 = EDGE_LOOP('',(#56986,#56987,#56988,#56989)) ;
#23245 = EDGE_LOOP('',(#56990,#56991,#56992,#56993)) ;
#23246 = EDGE_LOOP('',(#56994,#56995,#56996,#56997)) ;
#23247 = EDGE_LOOP('',(#56998,#56999,#57000)) ;
#23248 = EDGE_LOOP('',(#57001,#57002,#57003,#57004)) ;
#23249 = EDGE_LOOP('',(#57005,#57006,#57007,#57008)) ;
#23250 = EDGE_LOOP('',(#57009,#57010,#57011,#57012)) ;
#23251 = EDGE_LOOP('',(#57013,#57014,#57015)) ;
#23252 = EDGE_LOOP('',(#57016,#57017,#57018,#57019)) ;
#23253 = EDGE_LOOP('',(#57020,#57021,#57022,#57023)) ;
#23254 = EDGE_LOOP('',(#57024,#57025,#57026,#57027)) ;
#23255 = EDGE_LOOP('',(#57028,#57029,#57030)) ;
#23256 = EDGE_LOOP('',(#57031,#57032,#57033)) ;
#23257 = EDGE_LOOP('',(#57034,#57035,#57036,#57037)) ;
#23258 = EDGE_LOOP('',(#57038,#57039,#57040,#57041)) ;
#23259 = EDGE_LOOP('',(#57042,#57043,#57044,#57045)) ;
#23260 = EDGE_LOOP('',(#57046,#57047,#57048,#57049)) ;
#23261 = EDGE_LOOP('',(#57050,#57051,#57052,#57053)) ;
#23262 = EDGE_LOOP('',(#57054,#57055,#57056,#57057)) ;
#23263 = EDGE_LOOP('',(#57058,#57059,#57060,#57061)) ;
#23264 = EDGE_LOOP('',(#57062,#57063,#57064,#57065)) ;
#23265 = EDGE_LOOP('',(#57066,#57067,#57068,#57069)) ;
#23266 = EDGE_LOOP('',(#57070,#57071,#57072,#57073)) ;
#23267 = EDGE_LOOP('',(#57074,#57075,#57076,#57077)) ;
#23268 = EDGE_LOOP('',(#57078,#57079,#57080,#57081)) ;
#23269 = EDGE_LOOP('',(#57082,#57083,#57084,#57085)) ;
#23270 = EDGE_LOOP('',(#57086,#57087,#57088,#57089)) ;
#23271 = EDGE_LOOP('',(#57090,#57091,#57092,#57093)) ;
#23272 = EDGE_LOOP('',(#57094,#57095,#57096,#57097)) ;
#23273 = EDGE_LOOP('',(#57098,#57099,#57100,#57101)) ;
#23274 = EDGE_LOOP('',(#57102,#57103,#57104)) ;
#23275 = EDGE_LOOP('',(#57105,#57106,#57107,#57108)) ;
#23276 = EDGE_LOOP('',(#57109,#57110,#57111,#57112)) ;
#23277 = EDGE_LOOP('',(#57113,#57114,#57115,#57116)) ;
#23278 = EDGE_LOOP('',(#57117,#57118,#57119)) ;
#23279 = EDGE_LOOP('',(#57120,#57121,#57122,#57123)) ;
#23280 = EDGE_LOOP('',(#57124,#57125,#57126,#57127)) ;
#23281 = EDGE_LOOP('',(#57128,#57129,#57130,#57131)) ;
#23282 = EDGE_LOOP('',(#57132,#57133,#57134)) ;
#23283 = EDGE_LOOP('',(#57135,#57136,#57137)) ;
#23284 = EDGE_LOOP('',(#57138,#57139,#57140,#57141)) ;
#23285 = EDGE_LOOP('',(#57142,#57143,#57144,#57145)) ;
#23286 = EDGE_LOOP('',(#57146,#57147,#57148,#57149)) ;
#23287 = EDGE_LOOP('',(#57150,#57151,#57152,#57153)) ;
#23288 = EDGE_LOOP('',(#57154,#57155,#57156,#57157)) ;
#23289 = EDGE_LOOP('',(#57158,#57159,#57160,#57161)) ;
#23290 = EDGE_LOOP('',(#57162,#57163,#57164,#57165)) ;
#23291 = EDGE_LOOP('',(#57166,#57167,#57168,#57169)) ;
#23292 = EDGE_LOOP('',(#57170,#57171,#57172,#57173)) ;
#23293 = EDGE_LOOP('',(#57174,#57175,#57176,#57177)) ;
#23294 = EDGE_LOOP('',(#57178,#57179,#57180,#57181)) ;
#23295 = EDGE_LOOP('',(#57182,#57183,#57184,#57185)) ;
#23296 = EDGE_LOOP('',(#57186,#57187,#57188,#57189)) ;
#23297 = EDGE_LOOP('',(#57190,#57191,#57192,#57193)) ;
#23298 = EDGE_LOOP('',(#57194,#57195,#57196,#57197)) ;
#23299 = EDGE_LOOP('',(#57198,#57199,#57200,#57201)) ;
#23300 = EDGE_LOOP('',(#57202,#57203,#57204,#57205)) ;
#23301 = EDGE_LOOP('',(#57206,#57207,#57208)) ;
#23302 = EDGE_LOOP('',(#57209,#57210,#57211,#57212)) ;
#23303 = EDGE_LOOP('',(#57213,#57214,#57215,#57216)) ;
#23304 = EDGE_LOOP('',(#57217,#57218,#57219,#57220)) ;
#23305 = EDGE_LOOP('',(#57221,#57222,#57223)) ;
#23306 = EDGE_LOOP('',(#57224,#57225,#57226,#57227)) ;
#23307 = EDGE_LOOP('',(#57228,#57229,#57230,#57231)) ;
#23308 = EDGE_LOOP('',(#57232,#57233,#57234,#57235)) ;
#23309 = EDGE_LOOP('',(#57236,#57237,#57238)) ;
#23310 = EDGE_LOOP('',(#57239,#57240,#57241)) ;
#23311 = EDGE_LOOP('',(#57242,#57243,#57244,#57245)) ;
#23312 = EDGE_LOOP('',(#57246,#57247,#57248,#57249)) ;
#23313 = EDGE_LOOP('',(#57250,#57251,#57252,#57253)) ;
#23314 = EDGE_LOOP('',(#57254,#57255,#57256,#57257)) ;
#23315 = EDGE_LOOP('',(#57258,#57259,#57260,#57261)) ;
#23316 = EDGE_LOOP('',(#57262,#57263,#57264,#57265)) ;
#23317 = EDGE_LOOP('',(#57266,#57267,#57268,#57269)) ;
#23318 = EDGE_LOOP('',(#57270,#57271,#57272,#57273)) ;
#23319 = EDGE_LOOP('',(#57274,#57275,#57276,#57277)) ;
#23320 = EDGE_LOOP('',(#57278,#57279,#57280,#57281)) ;
#23321 = EDGE_LOOP('',(#57282,#57283,#57284,#57285)) ;
#23322 = EDGE_LOOP('',(#57286,#57287,#57288,#57289)) ;
#23323 = EDGE_LOOP('',(#57290,#57291,#57292,#57293)) ;
#23324 = EDGE_LOOP('',(#57294,#57295,#57296,#57297)) ;
#23325 = EDGE_LOOP('',(#57298,#57299,#57300,#57301)) ;
#23326 = EDGE_LOOP('',(#57302,#57303,#57304,#57305)) ;
#23327 = EDGE_LOOP('',(#57306,#57307,#57308,#57309)) ;
#23328 = EDGE_LOOP('',(#57310,#57311,#57312)) ;
#23329 = EDGE_LOOP('',(#57313,#57314,#57315,#57316)) ;
#23330 = EDGE_LOOP('',(#57317,#57318,#57319,#57320)) ;
#23331 = EDGE_LOOP('',(#57321,#57322,#57323,#57324)) ;
#23332 = EDGE_LOOP('',(#57325,#57326,#57327)) ;
#23333 = EDGE_LOOP('',(#57328,#57329,#57330,#57331)) ;
#23334 = EDGE_LOOP('',(#57332,#57333,#57334,#57335)) ;
#23335 = EDGE_LOOP('',(#57336,#57337,#57338,#57339)) ;
#23336 = EDGE_LOOP('',(#57340,#57341,#57342)) ;
#23337 = EDGE_LOOP('',(#57343,#57344,#57345)) ;
#23338 = EDGE_LOOP('',(#57346,#57347,#57348,#57349)) ;
#23339 = EDGE_LOOP('',(#57350,#57351,#57352,#57353)) ;
#23340 = EDGE_LOOP('',(#57354,#57355,#57356,#57357)) ;
#23341 = EDGE_LOOP('',(#57358,#57359,#57360,#57361)) ;
#23342 = EDGE_LOOP('',(#57362,#57363,#57364,#57365)) ;
#23343 = EDGE_LOOP('',(#57366,#57367,#57368,#57369)) ;
#23344 = EDGE_LOOP('',(#57370,#57371,#57372,#57373)) ;
#23345 = EDGE_LOOP('',(#57374,#57375,#57376,#57377)) ;
#23346 = EDGE_LOOP('',(#57378,#57379,#57380,#57381)) ;
#23347 = EDGE_LOOP('',(#57382,#57383,#57384,#57385)) ;
#23348 = EDGE_LOOP('',(#57386,#57387,#57388,#57389)) ;
#23349 = EDGE_LOOP('',(#57390,#57391,#57392,#57393)) ;
#23350 = EDGE_LOOP('',(#57394,#57395,#57396,#57397)) ;
#23351 = EDGE_LOOP('',(#57398,#57399,#57400,#57401)) ;
#23352 = EDGE_LOOP('',(#57402,#57403,#57404,#57405)) ;
#23353 = EDGE_LOOP('',(#57406,#57407,#57408,#57409)) ;
#23354 = EDGE_LOOP('',(#57410,#57411,#57412,#57413)) ;
#23355 = EDGE_LOOP('',(#57414,#57415,#57416)) ;
#23356 = EDGE_LOOP('',(#57417,#57418,#57419,#57420)) ;
#23357 = EDGE_LOOP('',(#57421,#57422,#57423,#57424)) ;
#23358 = EDGE_LOOP('',(#57425,#57426,#57427,#57428)) ;
#23359 = EDGE_LOOP('',(#57429,#57430,#57431)) ;
#23360 = EDGE_LOOP('',(#57432,#57433,#57434,#57435)) ;
#23361 = EDGE_LOOP('',(#57436,#57437,#57438,#57439)) ;
#23362 = EDGE_LOOP('',(#57440,#57441,#57442,#57443)) ;
#23363 = EDGE_LOOP('',(#57444,#57445,#57446)) ;
#23364 = EDGE_LOOP('',(#57447,#57448,#57449)) ;
#23365 = EDGE_LOOP('',(#57450,#57451,#57452,#57453)) ;
#23366 = EDGE_LOOP('',(#57454,#57455,#57456,#57457)) ;
#23367 = EDGE_LOOP('',(#57458,#57459,#57460,#57461)) ;
#23368 = EDGE_LOOP('',(#57462,#57463,#57464,#57465)) ;
#23369 = EDGE_LOOP('',(#57466,#57467,#57468,#57469)) ;
#23370 = EDGE_LOOP('',(#57470,#57471,#57472,#57473)) ;
#23371 = EDGE_LOOP('',(#57474,#57475,#57476,#57477)) ;
#23372 = EDGE_LOOP('',(#57478,#57479,#57480,#57481)) ;
#23373 = EDGE_LOOP('',(#57482,#57483,#57484,#57485)) ;
#23374 = EDGE_LOOP('',(#57486,#57487,#57488,#57489)) ;
#23375 = EDGE_LOOP('',(#57490,#57491,#57492,#57493)) ;
#23376 = EDGE_LOOP('',(#57494,#57495,#57496,#57497)) ;
#23377 = EDGE_LOOP('',(#57498,#57499,#57500,#57501)) ;
#23378 = EDGE_LOOP('',(#57502,#57503,#57504,#57505)) ;
#23379 = EDGE_LOOP('',(#57506,#57507,#57508,#57509)) ;
#23380 = EDGE_LOOP('',(#57510,#57511,#57512,#57513)) ;
#23381 = EDGE_LOOP('',(#57514,#57515,#57516,#57517)) ;
#23382 = EDGE_LOOP('',(#57518,#57519,#57520)) ;
#23383 = EDGE_LOOP('',(#57521,#57522,#57523,#57524)) ;
#23384 = EDGE_LOOP('',(#57525,#57526,#57527,#57528)) ;
#23385 = EDGE_LOOP('',(#57529,#57530,#57531,#57532)) ;
#23386 = EDGE_LOOP('',(#57533,#57534,#57535)) ;
#23387 = EDGE_LOOP('',(#57536,#57537,#57538,#57539)) ;
#23388 = EDGE_LOOP('',(#57540,#57541,#57542,#57543)) ;
#23389 = EDGE_LOOP('',(#57544,#57545,#57546,#57547)) ;
#23390 = EDGE_LOOP('',(#57548,#57549,#57550,#57551)) ;
#23391 = EDGE_LOOP('',(#57552,#57553,#57554)) ;
#23392 = EDGE_LOOP('',(#57555,#57556,#57557)) ;
#23393 = EDGE_LOOP('',(#57558,#57559,#57560,#57561)) ;
#23394 = EDGE_LOOP('',(#57562,#57563,#57564,#57565,#57566,#57567)) ;
#23395 = EDGE_LOOP('',(#57568,#57569,#57570,#57571,#57572,#57573,#57574)) ;
#23396 = EDGE_LOOP('',(#57575,#57576,#57577,#57578)) ;
#23397 = EDGE_LOOP('',(#57579,#57580,#57581,#57582)) ;
#23398 = EDGE_LOOP('',(#57583,#57584,#57585,#57586)) ;
#23399 = EDGE_LOOP('',(#57587,#57588,#57589,#57590)) ;
#23400 = EDGE_LOOP('',(#57591,#57592,#57593)) ;
#23401 = EDGE_LOOP('',(#57594,#57595,#57596,#57597)) ;
#23402 = EDGE_LOOP('',(#57598,#57599,#57600,#57601)) ;
#23403 = EDGE_LOOP('',(#57602,#57603,#57604,#57605)) ;
#23404 = EDGE_LOOP('',(#57606,#57607,#57608,#57609)) ;
#23405 = EDGE_LOOP('',(#57610,#57611,#57612,#57613)) ;
#23406 = EDGE_LOOP('',(#57614,#57615,#57616,#57617)) ;
#23407 = EDGE_LOOP('',(#57618,#57619,#57620,#57621)) ;
#23408 = EDGE_LOOP('',(#57622,#57623,#57624,#57625)) ;
#23409 = EDGE_LOOP('',(#57626,#57627,#57628,#57629)) ;
#23410 = EDGE_LOOP('',(#57630,#57631,#57632)) ;
#23411 = EDGE_LOOP('',(#57633,#57634,#57635)) ;
#23412 = EDGE_LOOP('',(#57636,#57637,#57638,#57639,#57640)) ;
#23413 = EDGE_LOOP('',(#57641,#57642,#57643)) ;
#23414 = EDGE_LOOP('',(#57644,#57645,#57646)) ;
#23415 = EDGE_LOOP('',(#57647,#57648,#57649,#57650)) ;
#23416 = EDGE_LOOP('',(#57651,#57652,#57653,#57654)) ;
#23417 = EDGE_LOOP('',(#57655,#57656,#57657,#57658)) ;
#23418 = EDGE_LOOP('',(#57659,#57660,#57661,#57662)) ;
#23419 = EDGE_LOOP('',(#57663,#57664,#57665,#57666)) ;
#23420 = EDGE_LOOP('',(#57667,#57668,#57669,#57670)) ;
#23421 = EDGE_LOOP('',(#57671,#57672,#57673,#57674)) ;
#23422 = EDGE_LOOP('',(#57675,#57676,#57677)) ;
#23423 = EDGE_LOOP('',(#57678,#57679,#57680,#57681)) ;
#23424 = EDGE_LOOP('',(#57682,#57683,#57684,#57685)) ;
#23425 = EDGE_LOOP('',(#57686,#57687,#57688)) ;
#23426 = EDGE_LOOP('',(#57689,#57690,#57691,#57692)) ;
#23427 = EDGE_LOOP('',(#57693,#57694,#57695,#57696)) ;
#23428 = EDGE_LOOP('',(#57697,#57698,#57699,#57700)) ;
#23429 = EDGE_LOOP('',(#57701,#57702,#57703,#57704)) ;
#23430 = EDGE_LOOP('',(#57705,#57706,#57707,#57708)) ;
#23431 = EDGE_LOOP('',(#57709,#57710,#57711,#57712)) ;
#23432 = EDGE_LOOP('',(#57713,#57714,#57715,#57716,#57717)) ;
#23433 = EDGE_LOOP('',(#57718,#57719,#57720,#57721)) ;
#23434 = EDGE_LOOP('',(#57722,#57723,#57724)) ;
#23435 = EDGE_LOOP('',(#57725,#57726,#57727,#57728)) ;
#23436 = EDGE_LOOP('',(#57729,#57730,#57731,#57732)) ;
#23437 = EDGE_LOOP('',(#57733,#57734,#57735)) ;
#23438 = EDGE_LOOP('',(#57736,#57737,#57738,#57739)) ;
#23439 = EDGE_LOOP('',(#57740,#57741,#57742,#57743)) ;
#23440 = EDGE_LOOP('',(#57744,#57745,#57746,#57747)) ;
#23441 = EDGE_LOOP('',(#57748,#57749,#57750)) ;
#23442 = EDGE_LOOP('',(#57751,#57752,#57753,#57754)) ;
#23443 = EDGE_LOOP('',(#57755,#57756,#57757,#57758)) ;
#23444 = EDGE_LOOP('',(#57759,#57760,#57761)) ;
#23445 = EDGE_LOOP('',(#57762,#57763,#57764)) ;
#23446 = EDGE_LOOP('',(#57765,#57766,#57767,#57768)) ;
#23447 = EDGE_LOOP('',(#57769,#57770,#57771,#57772)) ;
#23448 = EDGE_LOOP('',(#57773,#57774,#57775)) ;
#23449 = EDGE_LOOP('',(#57776,#57777,#57778)) ;
#23450 = EDGE_LOOP('',(#57779,#57780,#57781,#57782)) ;
#23451 = EDGE_LOOP('',(#57783,#57784,#57785,#57786)) ;
#23452 = EDGE_LOOP('',(#57787,#57788,#57789)) ;
#23453 = EDGE_LOOP('',(#57790,#57791,#57792,#57793)) ;
#23454 = EDGE_LOOP('',(#57794,#57795,#57796,#57797)) ;
#23455 = EDGE_LOOP('',(#57798,#57799,#57800)) ;
#23456 = EDGE_LOOP('',(#57801,#57802,#57803)) ;
#23457 = EDGE_LOOP('',(#57804,#57805,#57806,#57807)) ;
#23458 = EDGE_LOOP('',(#57808,#57809,#57810,#57811)) ;
#23459 = EDGE_LOOP('',(#57812,#57813,#57814,#57815)) ;
#23460 = EDGE_LOOP('',(#57816,#57817,#57818,#57819)) ;
#23461 = EDGE_LOOP('',(#57820,#57821,#57822,#57823)) ;
#23462 = EDGE_LOOP('',(#57824,#57825,#57826,#57827)) ;
#23463 = EDGE_LOOP('',(#57828,#57829,#57830,#57831)) ;
#23464 = EDGE_LOOP('',(#57832,#57833,#57834)) ;
#23465 = EDGE_LOOP('',(#57835,#57836,#57837)) ;
#23466 = EDGE_LOOP('',(#57838,#57839,#57840,#57841)) ;
#23467 = EDGE_LOOP('',(#57842,#57843,#57844,#57845,#57846,#57847)) ;
#23468 = EDGE_LOOP('',(#57848,#57849,#57850,#57851,#57852,#57853,#57854)) ;
#23469 = EDGE_LOOP('',(#57855,#57856,#57857,#57858)) ;
#23470 = EDGE_LOOP('',(#57859,#57860,#57861,#57862)) ;
#23471 = EDGE_LOOP('',(#57863,#57864,#57865,#57866)) ;
#23472 = EDGE_LOOP('',(#57867,#57868,#57869,#57870)) ;
#23473 = EDGE_LOOP('',(#57871,#57872,#57873)) ;
#23474 = EDGE_LOOP('',(#57874,#57875,#57876,#57877)) ;
#23475 = EDGE_LOOP('',(#57878,#57879,#57880,#57881)) ;
#23476 = EDGE_LOOP('',(#57882,#57883,#57884,#57885)) ;
#23477 = EDGE_LOOP('',(#57886,#57887,#57888,#57889)) ;
#23478 = EDGE_LOOP('',(#57890,#57891,#57892,#57893)) ;
#23479 = EDGE_LOOP('',(#57894,#57895,#57896,#57897)) ;
#23480 = EDGE_LOOP('',(#57898,#57899,#57900,#57901)) ;
#23481 = EDGE_LOOP('',(#57902,#57903,#57904,#57905)) ;
#23482 = EDGE_LOOP('',(#57906,#57907,#57908,#57909)) ;
#23483 = EDGE_LOOP('',(#57910,#57911,#57912)) ;
#23484 = EDGE_LOOP('',(#57913,#57914,#57915)) ;
#23485 = EDGE_LOOP('',(#57916,#57917,#57918,#57919,#57920)) ;
#23486 = EDGE_LOOP('',(#57921,#57922,#57923)) ;
#23487 = EDGE_LOOP('',(#57924,#57925,#57926)) ;
#23488 = EDGE_LOOP('',(#57927,#57928,#57929,#57930)) ;
#23489 = EDGE_LOOP('',(#57931,#57932,#57933,#57934)) ;
#23490 = EDGE_LOOP('',(#57935,#57936,#57937,#57938)) ;
#23491 = EDGE_LOOP('',(#57939,#57940,#57941,#57942)) ;
#23492 = EDGE_LOOP('',(#57943,#57944,#57945,#57946)) ;
#23493 = EDGE_LOOP('',(#57947,#57948,#57949,#57950)) ;
#23494 = EDGE_LOOP('',(#57951,#57952,#57953,#57954)) ;
#23495 = EDGE_LOOP('',(#57955,#57956,#57957)) ;
#23496 = EDGE_LOOP('',(#57958,#57959,#57960,#57961)) ;
#23497 = EDGE_LOOP('',(#57962,#57963,#57964,#57965)) ;
#23498 = EDGE_LOOP('',(#57966,#57967,#57968)) ;
#23499 = EDGE_LOOP('',(#57969,#57970,#57971,#57972)) ;
#23500 = EDGE_LOOP('',(#57973,#57974,#57975,#57976)) ;
#23501 = EDGE_LOOP('',(#57977,#57978,#57979,#57980)) ;
#23502 = EDGE_LOOP('',(#57981,#57982,#57983,#57984)) ;
#23503 = EDGE_LOOP('',(#57985,#57986,#57987,#57988)) ;
#23504 = EDGE_LOOP('',(#57989,#57990,#57991,#57992)) ;
#23505 = EDGE_LOOP('',(#57993,#57994,#57995,#57996,#57997)) ;
#23506 = EDGE_LOOP('',(#57998,#57999,#58000,#58001)) ;
#23507 = EDGE_LOOP('',(#58002,#58003,#58004)) ;
#23508 = EDGE_LOOP('',(#58005,#58006,#58007,#58008)) ;
#23509 = EDGE_LOOP('',(#58009,#58010,#58011,#58012)) ;
#23510 = EDGE_LOOP('',(#58013,#58014,#58015)) ;
#23511 = EDGE_LOOP('',(#58016,#58017,#58018,#58019)) ;
#23512 = EDGE_LOOP('',(#58020,#58021,#58022,#58023)) ;
#23513 = EDGE_LOOP('',(#58024,#58025,#58026,#58027)) ;
#23514 = EDGE_LOOP('',(#58028,#58029,#58030)) ;
#23515 = EDGE_LOOP('',(#58031,#58032,#58033,#58034)) ;
#23516 = EDGE_LOOP('',(#58035,#58036,#58037,#58038)) ;
#23517 = EDGE_LOOP('',(#58039,#58040,#58041)) ;
#23518 = EDGE_LOOP('',(#58042,#58043,#58044)) ;
#23519 = EDGE_LOOP('',(#58045,#58046,#58047,#58048)) ;
#23520 = EDGE_LOOP('',(#58049,#58050,#58051,#58052)) ;
#23521 = EDGE_LOOP('',(#58053,#58054,#58055)) ;
#23522 = EDGE_LOOP('',(#58056,#58057,#58058)) ;
#23523 = EDGE_LOOP('',(#58059,#58060,#58061,#58062)) ;
#23524 = EDGE_LOOP('',(#58063,#58064,#58065,#58066)) ;
#23525 = EDGE_LOOP('',(#58067,#58068,#58069)) ;
#23526 = EDGE_LOOP('',(#58070,#58071,#58072,#58073)) ;
#23527 = EDGE_LOOP('',(#58074,#58075,#58076,#58077)) ;
#23528 = EDGE_LOOP('',(#58078,#58079,#58080)) ;
#23529 = EDGE_LOOP('',(#58081,#58082,#58083)) ;
#23530 = EDGE_LOOP('',(#58084,#58085,#58086,#58087)) ;
#23531 = EDGE_LOOP('',(#58088,#58089,#58090,#58091)) ;
#23532 = EDGE_LOOP('',(#58092,#58093,#58094,#58095)) ;
#23533 = EDGE_LOOP('',(#58096,#58097,#58098,#58099)) ;
#23534 = EDGE_LOOP('',(#58100,#58101,#58102,#58103)) ;
#23535 = EDGE_LOOP('',(#58104,#58105,#58106,#58107)) ;
#23536 = EDGE_LOOP('',(#58108,#58109,#58110,#58111)) ;
#23537 = EDGE_LOOP('',(#58112,#58113,#58114)) ;
#23538 = EDGE_LOOP('',(#58115,#58116,#58117)) ;
#23539 = EDGE_LOOP('',(#58118,#58119,#58120,#58121)) ;
#23540 = EDGE_LOOP('',(#58122,#58123,#58124,#58125,#58126,#58127)) ;
#23541 = EDGE_LOOP('',(#58128,#58129,#58130,#58131,#58132,#58133,#58134)) ;
#23542 = EDGE_LOOP('',(#58135,#58136,#58137,#58138)) ;
#23543 = EDGE_LOOP('',(#58139,#58140,#58141,#58142)) ;
#23544 = EDGE_LOOP('',(#58143,#58144,#58145,#58146)) ;
#23545 = EDGE_LOOP('',(#58147,#58148,#58149,#58150)) ;
#23546 = EDGE_LOOP('',(#58151,#58152,#58153)) ;
#23547 = EDGE_LOOP('',(#58154,#58155,#58156,#58157)) ;
#23548 = EDGE_LOOP('',(#58158,#58159,#58160,#58161)) ;
#23549 = EDGE_LOOP('',(#58162,#58163,#58164,#58165)) ;
#23550 = EDGE_LOOP('',(#58166,#58167,#58168,#58169)) ;
#23551 = EDGE_LOOP('',(#58170,#58171,#58172,#58173)) ;
#23552 = EDGE_LOOP('',(#58174,#58175,#58176,#58177)) ;
#23553 = EDGE_LOOP('',(#58178,#58179,#58180,#58181)) ;
#23554 = EDGE_LOOP('',(#58182,#58183,#58184,#58185)) ;
#23555 = EDGE_LOOP('',(#58186,#58187,#58188,#58189)) ;
#23556 = EDGE_LOOP('',(#58190,#58191,#58192)) ;
#23557 = EDGE_LOOP('',(#58193,#58194,#58195)) ;
#23558 = EDGE_LOOP('',(#58196,#58197,#58198,#58199,#58200)) ;
#23559 = EDGE_LOOP('',(#58201,#58202,#58203)) ;
#23560 = EDGE_LOOP('',(#58204,#58205,#58206)) ;
#23561 = EDGE_LOOP('',(#58207,#58208,#58209,#58210)) ;
#23562 = EDGE_LOOP('',(#58211,#58212,#58213,#58214)) ;
#23563 = EDGE_LOOP('',(#58215,#58216,#58217,#58218)) ;
#23564 = EDGE_LOOP('',(#58219,#58220,#58221,#58222)) ;
#23565 = EDGE_LOOP('',(#58223,#58224,#58225,#58226)) ;
#23566 = EDGE_LOOP('',(#58227,#58228,#58229,#58230)) ;
#23567 = EDGE_LOOP('',(#58231,#58232,#58233,#58234)) ;
#23568 = EDGE_LOOP('',(#58235,#58236,#58237)) ;
#23569 = EDGE_LOOP('',(#58238,#58239,#58240,#58241)) ;
#23570 = EDGE_LOOP('',(#58242,#58243,#58244,#58245)) ;
#23571 = EDGE_LOOP('',(#58246,#58247,#58248)) ;
#23572 = EDGE_LOOP('',(#58249,#58250,#58251,#58252)) ;
#23573 = EDGE_LOOP('',(#58253,#58254,#58255,#58256)) ;
#23574 = EDGE_LOOP('',(#58257,#58258,#58259,#58260)) ;
#23575 = EDGE_LOOP('',(#58261,#58262,#58263,#58264)) ;
#23576 = EDGE_LOOP('',(#58265,#58266,#58267,#58268)) ;
#23577 = EDGE_LOOP('',(#58269,#58270,#58271,#58272)) ;
#23578 = EDGE_LOOP('',(#58273,#58274,#58275,#58276,#58277)) ;
#23579 = EDGE_LOOP('',(#58278,#58279,#58280,#58281)) ;
#23580 = EDGE_LOOP('',(#58282,#58283,#58284)) ;
#23581 = EDGE_LOOP('',(#58285,#58286,#58287,#58288)) ;
#23582 = EDGE_LOOP('',(#58289,#58290,#58291,#58292)) ;
#23583 = EDGE_LOOP('',(#58293,#58294,#58295)) ;
#23584 = EDGE_LOOP('',(#58296,#58297,#58298,#58299)) ;
#23585 = EDGE_LOOP('',(#58300,#58301,#58302,#58303)) ;
#23586 = EDGE_LOOP('',(#58304,#58305,#58306,#58307)) ;
#23587 = EDGE_LOOP('',(#58308,#58309,#58310)) ;
#23588 = EDGE_LOOP('',(#58311,#58312,#58313,#58314)) ;
#23589 = EDGE_LOOP('',(#58315,#58316,#58317,#58318)) ;
#23590 = EDGE_LOOP('',(#58319,#58320,#58321)) ;
#23591 = EDGE_LOOP('',(#58322,#58323,#58324)) ;
#23592 = EDGE_LOOP('',(#58325,#58326,#58327,#58328)) ;
#23593 = EDGE_LOOP('',(#58329,#58330,#58331,#58332)) ;
#23594 = EDGE_LOOP('',(#58333,#58334,#58335)) ;
#23595 = EDGE_LOOP('',(#58336,#58337,#58338)) ;
#23596 = EDGE_LOOP('',(#58339,#58340,#58341,#58342)) ;
#23597 = EDGE_LOOP('',(#58343,#58344,#58345,#58346)) ;
#23598 = EDGE_LOOP('',(#58347,#58348,#58349)) ;
#23599 = EDGE_LOOP('',(#58350,#58351,#58352,#58353)) ;
#23600 = EDGE_LOOP('',(#58354,#58355,#58356,#58357)) ;
#23601 = EDGE_LOOP('',(#58358,#58359,#58360)) ;
#23602 = EDGE_LOOP('',(#58361,#58362,#58363)) ;
#23603 = EDGE_LOOP('',(#58364,#58365,#58366,#58367)) ;
#23604 = EDGE_LOOP('',(#58368,#58369,#58370,#58371)) ;
#23605 = EDGE_LOOP('',(#58372,#58373,#58374,#58375)) ;
#23606 = EDGE_LOOP('',(#58376,#58377,#58378,#58379)) ;
#23607 = EDGE_LOOP('',(#58380,#58381,#58382,#58383)) ;
#23608 = EDGE_LOOP('',(#58384,#58385,#58386,#58387)) ;
#23609 = EDGE_LOOP('',(#58388,#58389,#58390,#58391)) ;
#23610 = EDGE_LOOP('',(#58392,#58393,#58394)) ;
#23611 = EDGE_LOOP('',(#58395,#58396,#58397)) ;
#23612 = EDGE_LOOP('',(#58398,#58399,#58400,#58401)) ;
#23613 = EDGE_LOOP('',(#58402,#58403,#58404,#58405,#58406,#58407)) ;
#23614 = EDGE_LOOP('',(#58408,#58409,#58410,#58411,#58412,#58413,#58414)) ;
#23615 = EDGE_LOOP('',(#58415,#58416,#58417,#58418)) ;
#23616 = EDGE_LOOP('',(#58419,#58420,#58421,#58422)) ;
#23617 = EDGE_LOOP('',(#58423,#58424,#58425,#58426)) ;
#23618 = EDGE_LOOP('',(#58427,#58428,#58429,#58430)) ;
#23619 = EDGE_LOOP('',(#58431,#58432,#58433)) ;
#23620 = EDGE_LOOP('',(#58434,#58435,#58436,#58437)) ;
#23621 = EDGE_LOOP('',(#58438,#58439,#58440,#58441)) ;
#23622 = EDGE_LOOP('',(#58442,#58443,#58444,#58445)) ;
#23623 = EDGE_LOOP('',(#58446,#58447,#58448,#58449)) ;
#23624 = EDGE_LOOP('',(#58450,#58451,#58452,#58453)) ;
#23625 = EDGE_LOOP('',(#58454,#58455,#58456,#58457)) ;
#23626 = EDGE_LOOP('',(#58458,#58459,#58460,#58461)) ;
#23627 = EDGE_LOOP('',(#58462,#58463,#58464,#58465)) ;
#23628 = EDGE_LOOP('',(#58466,#58467,#58468,#58469)) ;
#23629 = EDGE_LOOP('',(#58470,#58471,#58472)) ;
#23630 = EDGE_LOOP('',(#58473,#58474,#58475)) ;
#23631 = EDGE_LOOP('',(#58476,#58477,#58478,#58479,#58480)) ;
#23632 = EDGE_LOOP('',(#58481,#58482,#58483)) ;
#23633 = EDGE_LOOP('',(#58484,#58485,#58486)) ;
#23634 = EDGE_LOOP('',(#58487,#58488,#58489,#58490)) ;
#23635 = EDGE_LOOP('',(#58491,#58492,#58493,#58494)) ;
#23636 = EDGE_LOOP('',(#58495,#58496,#58497,#58498)) ;
#23637 = EDGE_LOOP('',(#58499,#58500,#58501,#58502)) ;
#23638 = EDGE_LOOP('',(#58503,#58504,#58505,#58506)) ;
#23639 = EDGE_LOOP('',(#58507,#58508,#58509,#58510)) ;
#23640 = EDGE_LOOP('',(#58511,#58512,#58513,#58514)) ;
#23641 = EDGE_LOOP('',(#58515,#58516,#58517)) ;
#23642 = EDGE_LOOP('',(#58518,#58519,#58520,#58521)) ;
#23643 = EDGE_LOOP('',(#58522,#58523,#58524,#58525)) ;
#23644 = EDGE_LOOP('',(#58526,#58527,#58528)) ;
#23645 = EDGE_LOOP('',(#58529,#58530,#58531,#58532)) ;
#23646 = EDGE_LOOP('',(#58533,#58534,#58535,#58536)) ;
#23647 = EDGE_LOOP('',(#58537,#58538,#58539,#58540)) ;
#23648 = EDGE_LOOP('',(#58541,#58542,#58543,#58544)) ;
#23649 = EDGE_LOOP('',(#58545,#58546,#58547,#58548)) ;
#23650 = EDGE_LOOP('',(#58549,#58550,#58551,#58552)) ;
#23651 = EDGE_LOOP('',(#58553,#58554,#58555,#58556,#58557)) ;
#23652 = EDGE_LOOP('',(#58558,#58559,#58560,#58561)) ;
#23653 = EDGE_LOOP('',(#58562,#58563,#58564)) ;
#23654 = EDGE_LOOP('',(#58565,#58566,#58567,#58568)) ;
#23655 = EDGE_LOOP('',(#58569,#58570,#58571,#58572)) ;
#23656 = EDGE_LOOP('',(#58573,#58574,#58575)) ;
#23657 = EDGE_LOOP('',(#58576,#58577,#58578,#58579)) ;
#23658 = EDGE_LOOP('',(#58580,#58581,#58582,#58583)) ;
#23659 = EDGE_LOOP('',(#58584,#58585,#58586,#58587)) ;
#23660 = EDGE_LOOP('',(#58588,#58589,#58590)) ;
#23661 = EDGE_LOOP('',(#58591,#58592,#58593,#58594)) ;
#23662 = EDGE_LOOP('',(#58595,#58596,#58597,#58598)) ;
#23663 = EDGE_LOOP('',(#58599,#58600,#58601)) ;
#23664 = EDGE_LOOP('',(#58602,#58603,#58604)) ;
#23665 = EDGE_LOOP('',(#58605,#58606,#58607,#58608)) ;
#23666 = EDGE_LOOP('',(#58609,#58610,#58611,#58612)) ;
#23667 = EDGE_LOOP('',(#58613,#58614,#58615)) ;
#23668 = EDGE_LOOP('',(#58616,#58617,#58618)) ;
#23669 = EDGE_LOOP('',(#58619,#58620,#58621,#58622)) ;
#23670 = EDGE_LOOP('',(#58623,#58624,#58625,#58626)) ;
#23671 = EDGE_LOOP('',(#58627,#58628,#58629)) ;
#23672 = EDGE_LOOP('',(#58630,#58631,#58632,#58633)) ;
#23673 = EDGE_LOOP('',(#58634,#58635,#58636,#58637)) ;
#23674 = EDGE_LOOP('',(#58638,#58639,#58640)) ;
#23675 = EDGE_LOOP('',(#58641,#58642,#58643)) ;
#23676 = EDGE_LOOP('',(#58644,#58645,#58646,#58647)) ;
#23677 = EDGE_LOOP('',(#58648,#58649,#58650,#58651)) ;
#23678 = EDGE_LOOP('',(#58652,#58653,#58654,#58655)) ;
#23679 = EDGE_LOOP('',(#58656,#58657,#58658,#58659)) ;
#23680 = EDGE_LOOP('',(#58660,#58661,#58662,#58663)) ;
#23681 = EDGE_LOOP('',(#58664,#58665,#58666,#58667)) ;
#23682 = EDGE_LOOP('',(#58668,#58669,#58670,#58671)) ;
#23683 = EDGE_LOOP('',(#58672,#58673,#58674)) ;
#23684 = EDGE_LOOP('',(#58675,#58676,#58677)) ;
#23685 = EDGE_LOOP('',(#58678,#58679,#58680,#58681)) ;
#23686 = EDGE_LOOP('',(#58682,#58683,#58684,#58685,#58686,#58687)) ;
#23687 = EDGE_LOOP('',(#58688,#58689,#58690,#58691,#58692,#58693,#58694)) ;
#23688 = EDGE_LOOP('',(#58695,#58696,#58697,#58698)) ;
#23689 = EDGE_LOOP('',(#58699,#58700,#58701,#58702)) ;
#23690 = EDGE_LOOP('',(#58703,#58704,#58705,#58706)) ;
#23691 = EDGE_LOOP('',(#58707,#58708,#58709,#58710)) ;
#23692 = EDGE_LOOP('',(#58711,#58712,#58713)) ;
#23693 = EDGE_LOOP('',(#58714,#58715,#58716,#58717)) ;
#23694 = EDGE_LOOP('',(#58718,#58719,#58720,#58721)) ;
#23695 = EDGE_LOOP('',(#58722,#58723,#58724,#58725)) ;
#23696 = EDGE_LOOP('',(#58726,#58727,#58728,#58729)) ;
#23697 = EDGE_LOOP('',(#58730,#58731,#58732,#58733)) ;
#23698 = EDGE_LOOP('',(#58734,#58735,#58736,#58737)) ;
#23699 = EDGE_LOOP('',(#58738,#58739,#58740,#58741)) ;
#23700 = EDGE_LOOP('',(#58742,#58743,#58744,#58745)) ;
#23701 = EDGE_LOOP('',(#58746,#58747,#58748,#58749)) ;
#23702 = EDGE_LOOP('',(#58750,#58751,#58752)) ;
#23703 = EDGE_LOOP('',(#58753,#58754,#58755)) ;
#23704 = EDGE_LOOP('',(#58756,#58757,#58758,#58759,#58760)) ;
#23705 = EDGE_LOOP('',(#58761,#58762,#58763)) ;
#23706 = EDGE_LOOP('',(#58764,#58765,#58766)) ;
#23707 = EDGE_LOOP('',(#58767,#58768,#58769,#58770)) ;
#23708 = EDGE_LOOP('',(#58771,#58772,#58773,#58774)) ;
#23709 = EDGE_LOOP('',(#58775,#58776,#58777,#58778)) ;
#23710 = EDGE_LOOP('',(#58779,#58780,#58781,#58782)) ;
#23711 = EDGE_LOOP('',(#58783,#58784,#58785,#58786)) ;
#23712 = EDGE_LOOP('',(#58787,#58788,#58789,#58790)) ;
#23713 = EDGE_LOOP('',(#58791,#58792,#58793,#58794)) ;
#23714 = EDGE_LOOP('',(#58795,#58796,#58797)) ;
#23715 = EDGE_LOOP('',(#58798,#58799,#58800,#58801)) ;
#23716 = EDGE_LOOP('',(#58802,#58803,#58804,#58805)) ;
#23717 = EDGE_LOOP('',(#58806,#58807,#58808)) ;
#23718 = EDGE_LOOP('',(#58809,#58810,#58811,#58812)) ;
#23719 = EDGE_LOOP('',(#58813,#58814,#58815,#58816)) ;
#23720 = EDGE_LOOP('',(#58817,#58818,#58819,#58820)) ;
#23721 = EDGE_LOOP('',(#58821,#58822,#58823,#58824)) ;
#23722 = EDGE_LOOP('',(#58825,#58826,#58827,#58828)) ;
#23723 = EDGE_LOOP('',(#58829,#58830,#58831,#58832)) ;
#23724 = EDGE_LOOP('',(#58833,#58834,#58835,#58836,#58837)) ;
#23725 = EDGE_LOOP('',(#58838,#58839,#58840,#58841)) ;
#23726 = EDGE_LOOP('',(#58842,#58843,#58844)) ;
#23727 = EDGE_LOOP('',(#58845,#58846,#58847,#58848)) ;
#23728 = EDGE_LOOP('',(#58849,#58850,#58851,#58852)) ;
#23729 = EDGE_LOOP('',(#58853,#58854,#58855)) ;
#23730 = EDGE_LOOP('',(#58856,#58857,#58858,#58859)) ;
#23731 = EDGE_LOOP('',(#58860,#58861,#58862,#58863)) ;
#23732 = EDGE_LOOP('',(#58864,#58865,#58866,#58867)) ;
#23733 = EDGE_LOOP('',(#58868,#58869,#58870)) ;
#23734 = EDGE_LOOP('',(#58871,#58872,#58873,#58874)) ;
#23735 = EDGE_LOOP('',(#58875,#58876,#58877,#58878)) ;
#23736 = EDGE_LOOP('',(#58879,#58880,#58881)) ;
#23737 = EDGE_LOOP('',(#58882,#58883,#58884)) ;
#23738 = EDGE_LOOP('',(#58885,#58886,#58887,#58888)) ;
#23739 = EDGE_LOOP('',(#58889,#58890,#58891,#58892)) ;
#23740 = EDGE_LOOP('',(#58893,#58894,#58895)) ;
#23741 = EDGE_LOOP('',(#58896,#58897,#58898)) ;
#23742 = EDGE_LOOP('',(#58899,#58900,#58901,#58902)) ;
#23743 = EDGE_LOOP('',(#58903,#58904,#58905,#58906)) ;
#23744 = EDGE_LOOP('',(#58907,#58908,#58909)) ;
#23745 = EDGE_LOOP('',(#58910,#58911,#58912,#58913)) ;
#23746 = EDGE_LOOP('',(#58914,#58915,#58916,#58917)) ;
#23747 = EDGE_LOOP('',(#58918,#58919,#58920)) ;
#23748 = EDGE_LOOP('',(#58921,#58922,#58923)) ;
#23749 = EDGE_LOOP('',(#58924,#58925,#58926,#58927)) ;
#23750 = EDGE_LOOP('',(#58928,#58929,#58930,#58931)) ;
#23751 = EDGE_LOOP('',(#58932,#58933,#58934,#58935)) ;
#23752 = EDGE_LOOP('',(#58936,#58937,#58938,#58939)) ;
#23753 = EDGE_LOOP('',(#58940,#58941,#58942,#58943)) ;
#23754 = EDGE_LOOP('',(#58944,#58945,#58946,#58947)) ;
#23755 = EDGE_LOOP('',(#58948,#58949,#58950,#58951)) ;
#23756 = EDGE_LOOP('',(#58952,#58953,#58954)) ;
#23757 = EDGE_LOOP('',(#58955,#58956,#58957)) ;
#23758 = EDGE_LOOP('',(#58958,#58959,#58960,#58961)) ;
#23759 = EDGE_LOOP('',(#58962,#58963,#58964,#58965,#58966,#58967)) ;
#23760 = EDGE_LOOP('',(#58968,#58969,#58970,#58971,#58972,#58973,#58974)) ;
#23761 = EDGE_LOOP('',(#58975,#58976,#58977,#58978)) ;
#23762 = EDGE_LOOP('',(#58979,#58980,#58981,#58982)) ;
#23763 = EDGE_LOOP('',(#58983,#58984,#58985,#58986)) ;
#23764 = EDGE_LOOP('',(#58987,#58988,#58989,#58990)) ;
#23765 = EDGE_LOOP('',(#58991,#58992,#58993)) ;
#23766 = EDGE_LOOP('',(#58994,#58995,#58996,#58997)) ;
#23767 = EDGE_LOOP('',(#58998,#58999,#59000,#59001)) ;
#23768 = EDGE_LOOP('',(#59002,#59003,#59004,#59005)) ;
#23769 = EDGE_LOOP('',(#59006,#59007,#59008,#59009)) ;
#23770 = EDGE_LOOP('',(#59010,#59011,#59012,#59013)) ;
#23771 = EDGE_LOOP('',(#59014,#59015,#59016,#59017)) ;
#23772 = EDGE_LOOP('',(#59018,#59019,#59020,#59021)) ;
#23773 = EDGE_LOOP('',(#59022,#59023,#59024,#59025)) ;
#23774 = EDGE_LOOP('',(#59026,#59027,#59028,#59029)) ;
#23775 = EDGE_LOOP('',(#59030,#59031,#59032)) ;
#23776 = EDGE_LOOP('',(#59033,#59034,#59035)) ;
#23777 = EDGE_LOOP('',(#59036,#59037,#59038,#59039,#59040)) ;
#23778 = EDGE_LOOP('',(#59041,#59042,#59043)) ;
#23779 = EDGE_LOOP('',(#59044,#59045,#59046)) ;
#23780 = EDGE_LOOP('',(#59047,#59048,#59049,#59050)) ;
#23781 = EDGE_LOOP('',(#59051,#59052,#59053,#59054)) ;
#23782 = EDGE_LOOP('',(#59055,#59056,#59057,#59058)) ;
#23783 = EDGE_LOOP('',(#59059,#59060,#59061,#59062)) ;
#23784 = EDGE_LOOP('',(#59063,#59064,#59065,#59066)) ;
#23785 = EDGE_LOOP('',(#59067,#59068,#59069,#59070)) ;
#23786 = EDGE_LOOP('',(#59071,#59072,#59073,#59074)) ;
#23787 = EDGE_LOOP('',(#59075,#59076,#59077)) ;
#23788 = EDGE_LOOP('',(#59078,#59079,#59080,#59081)) ;
#23789 = EDGE_LOOP('',(#59082,#59083,#59084,#59085)) ;
#23790 = EDGE_LOOP('',(#59086,#59087,#59088)) ;
#23791 = EDGE_LOOP('',(#59089,#59090,#59091,#59092)) ;
#23792 = EDGE_LOOP('',(#59093,#59094,#59095,#59096)) ;
#23793 = EDGE_LOOP('',(#59097,#59098,#59099,#59100)) ;
#23794 = EDGE_LOOP('',(#59101,#59102,#59103,#59104)) ;
#23795 = EDGE_LOOP('',(#59105,#59106,#59107,#59108)) ;
#23796 = EDGE_LOOP('',(#59109,#59110,#59111,#59112)) ;
#23797 = EDGE_LOOP('',(#59113,#59114,#59115,#59116,#59117)) ;
#23798 = EDGE_LOOP('',(#59118,#59119,#59120,#59121)) ;
#23799 = EDGE_LOOP('',(#59122,#59123,#59124)) ;
#23800 = EDGE_LOOP('',(#59125,#59126,#59127,#59128)) ;
#23801 = EDGE_LOOP('',(#59129,#59130,#59131,#59132)) ;
#23802 = EDGE_LOOP('',(#59133,#59134,#59135)) ;
#23803 = EDGE_LOOP('',(#59136,#59137,#59138,#59139)) ;
#23804 = EDGE_LOOP('',(#59140,#59141,#59142,#59143)) ;
#23805 = EDGE_LOOP('',(#59144,#59145,#59146,#59147)) ;
#23806 = EDGE_LOOP('',(#59148,#59149,#59150)) ;
#23807 = EDGE_LOOP('',(#59151,#59152,#59153,#59154)) ;
#23808 = EDGE_LOOP('',(#59155,#59156,#59157,#59158)) ;
#23809 = EDGE_LOOP('',(#59159,#59160,#59161)) ;
#23810 = EDGE_LOOP('',(#59162,#59163,#59164)) ;
#23811 = EDGE_LOOP('',(#59165,#59166,#59167,#59168)) ;
#23812 = EDGE_LOOP('',(#59169,#59170,#59171,#59172)) ;
#23813 = EDGE_LOOP('',(#59173,#59174,#59175)) ;
#23814 = EDGE_LOOP('',(#59176,#59177,#59178)) ;
#23815 = EDGE_LOOP('',(#59179,#59180,#59181,#59182)) ;
#23816 = EDGE_LOOP('',(#59183,#59184,#59185,#59186)) ;
#23817 = EDGE_LOOP('',(#59187,#59188,#59189)) ;
#23818 = EDGE_LOOP('',(#59190,#59191,#59192,#59193)) ;
#23819 = EDGE_LOOP('',(#59194,#59195,#59196,#59197)) ;
#23820 = EDGE_LOOP('',(#59198,#59199,#59200)) ;
#23821 = EDGE_LOOP('',(#59201,#59202,#59203)) ;
#23822 = EDGE_LOOP('',(#59204,#59205,#59206,#59207)) ;
#23823 = EDGE_LOOP('',(#59208,#59209,#59210,#59211)) ;
#23824 = EDGE_LOOP('',(#59212,#59213,#59214,#59215)) ;
#23825 = EDGE_LOOP('',(#59216,#59217,#59218,#59219)) ;
#23826 = EDGE_LOOP('',(#59220,#59221,#59222,#59223)) ;
#23827 = EDGE_LOOP('',(#59224,#59225,#59226,#59227)) ;
#23828 = EDGE_LOOP('',(#59228,#59229,#59230,#59231)) ;
#23829 = EDGE_LOOP('',(#59232,#59233,#59234)) ;
#23830 = EDGE_LOOP('',(#59235,#59236,#59237)) ;
#23831 = EDGE_LOOP('',(#59238,#59239,#59240,#59241)) ;
#23832 = EDGE_LOOP('',(#59242,#59243,#59244,#59245,#59246,#59247)) ;
#23833 = EDGE_LOOP('',(#59248,#59249,#59250,#59251,#59252,#59253,#59254)) ;
#23834 = EDGE_LOOP('',(#59255,#59256,#59257,#59258)) ;
#23835 = EDGE_LOOP('',(#59259,#59260,#59261,#59262)) ;
#23836 = EDGE_LOOP('',(#59263,#59264,#59265,#59266)) ;
#23837 = EDGE_LOOP('',(#59267,#59268,#59269,#59270)) ;
#23838 = EDGE_LOOP('',(#59271,#59272,#59273)) ;
#23839 = EDGE_LOOP('',(#59274,#59275,#59276,#59277)) ;
#23840 = EDGE_LOOP('',(#59278,#59279,#59280,#59281)) ;
#23841 = EDGE_LOOP('',(#59282,#59283,#59284,#59285)) ;
#23842 = EDGE_LOOP('',(#59286,#59287,#59288,#59289)) ;
#23843 = EDGE_LOOP('',(#59290,#59291,#59292,#59293)) ;
#23844 = EDGE_LOOP('',(#59294,#59295,#59296,#59297)) ;
#23845 = EDGE_LOOP('',(#59298,#59299,#59300,#59301)) ;
#23846 = EDGE_LOOP('',(#59302,#59303,#59304,#59305)) ;
#23847 = EDGE_LOOP('',(#59306,#59307,#59308,#59309)) ;
#23848 = EDGE_LOOP('',(#59310,#59311,#59312)) ;
#23849 = EDGE_LOOP('',(#59313,#59314,#59315)) ;
#23850 = EDGE_LOOP('',(#59316,#59317,#59318,#59319,#59320)) ;
#23851 = EDGE_LOOP('',(#59321,#59322,#59323)) ;
#23852 = EDGE_LOOP('',(#59324,#59325,#59326)) ;
#23853 = EDGE_LOOP('',(#59327,#59328,#59329,#59330)) ;
#23854 = EDGE_LOOP('',(#59331,#59332,#59333,#59334)) ;
#23855 = EDGE_LOOP('',(#59335,#59336,#59337,#59338)) ;
#23856 = EDGE_LOOP('',(#59339,#59340,#59341,#59342)) ;
#23857 = EDGE_LOOP('',(#59343,#59344,#59345,#59346)) ;
#23858 = EDGE_LOOP('',(#59347,#59348,#59349,#59350)) ;
#23859 = EDGE_LOOP('',(#59351,#59352,#59353,#59354)) ;
#23860 = EDGE_LOOP('',(#59355,#59356,#59357)) ;
#23861 = EDGE_LOOP('',(#59358,#59359,#59360,#59361)) ;
#23862 = EDGE_LOOP('',(#59362,#59363,#59364,#59365)) ;
#23863 = EDGE_LOOP('',(#59366,#59367,#59368)) ;
#23864 = EDGE_LOOP('',(#59369,#59370,#59371,#59372)) ;
#23865 = EDGE_LOOP('',(#59373,#59374,#59375,#59376)) ;
#23866 = EDGE_LOOP('',(#59377,#59378,#59379,#59380)) ;
#23867 = EDGE_LOOP('',(#59381,#59382,#59383,#59384)) ;
#23868 = EDGE_LOOP('',(#59385,#59386,#59387,#59388)) ;
#23869 = EDGE_LOOP('',(#59389,#59390,#59391,#59392)) ;
#23870 = EDGE_LOOP('',(#59393,#59394,#59395,#59396,#59397)) ;
#23871 = EDGE_LOOP('',(#59398,#59399,#59400,#59401)) ;
#23872 = EDGE_LOOP('',(#59402,#59403,#59404)) ;
#23873 = EDGE_LOOP('',(#59405,#59406,#59407,#59408)) ;
#23874 = EDGE_LOOP('',(#59409,#59410,#59411,#59412)) ;
#23875 = EDGE_LOOP('',(#59413,#59414,#59415)) ;
#23876 = EDGE_LOOP('',(#59416,#59417,#59418,#59419)) ;
#23877 = EDGE_LOOP('',(#59420,#59421,#59422,#59423)) ;
#23878 = EDGE_LOOP('',(#59424,#59425,#59426,#59427)) ;
#23879 = EDGE_LOOP('',(#59428,#59429,#59430)) ;
#23880 = EDGE_LOOP('',(#59431,#59432,#59433,#59434)) ;
#23881 = EDGE_LOOP('',(#59435,#59436,#59437,#59438)) ;
#23882 = EDGE_LOOP('',(#59439,#59440,#59441)) ;
#23883 = EDGE_LOOP('',(#59442,#59443,#59444)) ;
#23884 = EDGE_LOOP('',(#59445,#59446,#59447,#59448)) ;
#23885 = EDGE_LOOP('',(#59449,#59450,#59451,#59452)) ;
#23886 = EDGE_LOOP('',(#59453,#59454,#59455)) ;
#23887 = EDGE_LOOP('',(#59456,#59457,#59458)) ;
#23888 = EDGE_LOOP('',(#59459,#59460,#59461,#59462)) ;
#23889 = EDGE_LOOP('',(#59463,#59464,#59465,#59466)) ;
#23890 = EDGE_LOOP('',(#59467,#59468,#59469)) ;
#23891 = EDGE_LOOP('',(#59470,#59471,#59472,#59473)) ;
#23892 = EDGE_LOOP('',(#59474,#59475,#59476,#59477)) ;
#23893 = EDGE_LOOP('',(#59478,#59479,#59480)) ;
#23894 = EDGE_LOOP('',(#59481,#59482,#59483)) ;
#23895 = EDGE_LOOP('',(#59484,#59485,#59486,#59487)) ;
#23896 = EDGE_LOOP('',(#59488,#59489,#59490,#59491)) ;
#23897 = EDGE_LOOP('',(#59492,#59493,#59494,#59495)) ;
#23898 = EDGE_LOOP('',(#59496,#59497,#59498,#59499)) ;
#23899 = EDGE_LOOP('',(#59500,#59501,#59502,#59503)) ;
#23900 = EDGE_LOOP('',(#59504,#59505,#59506,#59507)) ;
#23901 = EDGE_LOOP('',(#59508,#59509,#59510,#59511)) ;
#23902 = EDGE_LOOP('',(#59512,#59513,#59514)) ;
#23903 = EDGE_LOOP('',(#59515,#59516,#59517)) ;
#23904 = EDGE_LOOP('',(#59518,#59519,#59520,#59521)) ;
#23905 = EDGE_LOOP('',(#59522,#59523,#59524,#59525,#59526,#59527)) ;
#23906 = EDGE_LOOP('',(#59528,#59529,#59530,#59531,#59532,#59533,#59534)) ;
#23907 = EDGE_LOOP('',(#59535,#59536,#59537,#59538)) ;
#23908 = EDGE_LOOP('',(#59539,#59540,#59541,#59542)) ;
#23909 = EDGE_LOOP('',(#59543,#59544,#59545,#59546)) ;
#23910 = EDGE_LOOP('',(#59547,#59548,#59549,#59550)) ;
#23911 = EDGE_LOOP('',(#59551,#59552,#59553)) ;
#23912 = EDGE_LOOP('',(#59554,#59555,#59556,#59557)) ;
#23913 = EDGE_LOOP('',(#59558,#59559,#59560,#59561)) ;
#23914 = EDGE_LOOP('',(#59562,#59563,#59564,#59565)) ;
#23915 = EDGE_LOOP('',(#59566,#59567,#59568,#59569)) ;
#23916 = EDGE_LOOP('',(#59570,#59571,#59572,#59573)) ;
#23917 = EDGE_LOOP('',(#59574,#59575,#59576,#59577)) ;
#23918 = EDGE_LOOP('',(#59578,#59579,#59580,#59581)) ;
#23919 = EDGE_LOOP('',(#59582,#59583,#59584,#59585)) ;
#23920 = EDGE_LOOP('',(#59586,#59587,#59588,#59589)) ;
#23921 = EDGE_LOOP('',(#59590,#59591,#59592)) ;
#23922 = EDGE_LOOP('',(#59593,#59594,#59595)) ;
#23923 = EDGE_LOOP('',(#59596,#59597,#59598,#59599,#59600)) ;
#23924 = EDGE_LOOP('',(#59601,#59602,#59603)) ;
#23925 = EDGE_LOOP('',(#59604,#59605,#59606)) ;
#23926 = EDGE_LOOP('',(#59607,#59608,#59609,#59610)) ;
#23927 = EDGE_LOOP('',(#59611,#59612,#59613,#59614)) ;
#23928 = EDGE_LOOP('',(#59615,#59616,#59617,#59618)) ;
#23929 = EDGE_LOOP('',(#59619,#59620,#59621,#59622)) ;
#23930 = EDGE_LOOP('',(#59623,#59624,#59625,#59626)) ;
#23931 = EDGE_LOOP('',(#59627,#59628,#59629,#59630)) ;
#23932 = EDGE_LOOP('',(#59631,#59632,#59633,#59634)) ;
#23933 = EDGE_LOOP('',(#59635,#59636,#59637)) ;
#23934 = EDGE_LOOP('',(#59638,#59639,#59640,#59641)) ;
#23935 = EDGE_LOOP('',(#59642,#59643,#59644,#59645)) ;
#23936 = EDGE_LOOP('',(#59646,#59647,#59648)) ;
#23937 = EDGE_LOOP('',(#59649,#59650,#59651,#59652)) ;
#23938 = EDGE_LOOP('',(#59653,#59654,#59655,#59656)) ;
#23939 = EDGE_LOOP('',(#59657,#59658,#59659,#59660)) ;
#23940 = EDGE_LOOP('',(#59661,#59662,#59663,#59664)) ;
#23941 = EDGE_LOOP('',(#59665,#59666,#59667,#59668)) ;
#23942 = EDGE_LOOP('',(#59669,#59670,#59671,#59672)) ;
#23943 = EDGE_LOOP('',(#59673,#59674,#59675,#59676,#59677)) ;
#23944 = EDGE_LOOP('',(#59678,#59679,#59680,#59681)) ;
#23945 = EDGE_LOOP('',(#59682,#59683,#59684)) ;
#23946 = EDGE_LOOP('',(#59685,#59686,#59687,#59688)) ;
#23947 = EDGE_LOOP('',(#59689,#59690,#59691,#59692)) ;
#23948 = EDGE_LOOP('',(#59693,#59694,#59695)) ;
#23949 = EDGE_LOOP('',(#59696,#59697,#59698,#59699)) ;
#23950 = EDGE_LOOP('',(#59700,#59701,#59702,#59703)) ;
#23951 = EDGE_LOOP('',(#59704,#59705,#59706,#59707)) ;
#23952 = EDGE_LOOP('',(#59708,#59709,#59710)) ;
#23953 = EDGE_LOOP('',(#59711,#59712,#59713,#59714)) ;
#23954 = EDGE_LOOP('',(#59715,#59716,#59717,#59718)) ;
#23955 = EDGE_LOOP('',(#59719,#59720,#59721)) ;
#23956 = EDGE_LOOP('',(#59722,#59723,#59724)) ;
#23957 = EDGE_LOOP('',(#59725,#59726,#59727,#59728)) ;
#23958 = EDGE_LOOP('',(#59729,#59730,#59731,#59732)) ;
#23959 = EDGE_LOOP('',(#59733,#59734,#59735)) ;
#23960 = EDGE_LOOP('',(#59736,#59737,#59738)) ;
#23961 = EDGE_LOOP('',(#59739,#59740,#59741,#59742)) ;
#23962 = EDGE_LOOP('',(#59743,#59744,#59745,#59746)) ;
#23963 = EDGE_LOOP('',(#59747,#59748,#59749)) ;
#23964 = EDGE_LOOP('',(#59750,#59751,#59752,#59753)) ;
#23965 = EDGE_LOOP('',(#59754,#59755,#59756,#59757)) ;
#23966 = EDGE_LOOP('',(#59758,#59759,#59760)) ;
#23967 = EDGE_LOOP('',(#59761,#59762,#59763)) ;
#23968 = EDGE_LOOP('',(#59764,#59765,#59766,#59767)) ;
#23969 = EDGE_LOOP('',(#59768,#59769,#59770,#59771)) ;
#23970 = EDGE_LOOP('',(#59772,#59773,#59774,#59775)) ;
#23971 = EDGE_LOOP('',(#59776,#59777,#59778,#59779)) ;
#23972 = EDGE_LOOP('',(#59780,#59781,#59782,#59783)) ;
#23973 = EDGE_LOOP('',(#59784,#59785,#59786,#59787)) ;
#23974 = EDGE_LOOP('',(#59788,#59789,#59790,#59791)) ;
#23975 = EDGE_LOOP('',(#59792,#59793,#59794,#59795)) ;
#23976 = EDGE_LOOP('',(#59796,#59797,#59798,#59799)) ;
#23977 = EDGE_LOOP('',(#59800,#59801,#59802,#59803)) ;
#23978 = EDGE_LOOP('',(#59804,#59805,#59806,#59807,#59808,#59809)) ;
#23979 = EDGE_LOOP('',(#59810,#59811,#59812,#59813,#59814,#59815)) ;
#23980 = EDGE_LOOP('',(#59816,#59817,#59818,#59819,#59820)) ;
#23981 = EDGE_LOOP('',(#59821,#59822,#59823,#59824)) ;
#23982 = EDGE_LOOP('',(#59825,#59826,#59827,#59828)) ;
#23983 = EDGE_LOOP('',(#59829,#59830,#59831,#59832)) ;
#23984 = EDGE_LOOP('',(#59833,#59834,#59835,#59836)) ;
#23985 = EDGE_LOOP('',(#59837,#59838,#59839,#59840)) ;
#23986 = EDGE_LOOP('',(#59841,#59842,#59843,#59844)) ;
#23987 = EDGE_LOOP('',(#59845,#59846,#59847,#59848)) ;
#23988 = EDGE_LOOP('',(#59849,#59850,#59851,#59852)) ;
#23989 = EDGE_LOOP('',(#59853,#59854,#59855,#59856)) ;
#23990 = EDGE_LOOP('',(#59857,#59858,#59859,#59860)) ;
#23991 = EDGE_LOOP('',(#59861,#59862,#59863,#59864)) ;
#23992 = EDGE_LOOP('',(#59865,#59866,#59867,#59868)) ;
#23993 = EDGE_LOOP('',(#59869,#59870,#59871,#59872)) ;
#23994 = EDGE_LOOP('',(#59873,#59874,#59875,#59876,#59877,#59878)) ;
#23995 = EDGE_LOOP('',(#59879,#59880,#59881,#59882,#59883,#59884)) ;
#23996 = EDGE_LOOP('',(#59885,#59886,#59887,#59888,#59889)) ;
#23997 = EDGE_LOOP('',(#59890,#59891,#59892,#59893)) ;
#23998 = EDGE_LOOP('',(#59894,#59895,#59896,#59897)) ;
#23999 = EDGE_LOOP('',(#59898,#59899,#59900,#59901)) ;
#24000 = EDGE_LOOP('',(#59902,#59903,#59904,#59905)) ;
#24001 = EDGE_LOOP('',(#59906,#59907,#59908,#59909)) ;
#24002 = EDGE_LOOP('',(#59910,#59911,#59912,#59913)) ;
#24003 = EDGE_LOOP('',(#59914,#59915,#59916,#59917)) ;
#24004 = EDGE_LOOP('',(#59918,#59919,#59920,#59921)) ;
#24005 = EDGE_LOOP('',(#59922,#59923,#59924,#59925)) ;
#24006 = EDGE_LOOP('',(#59926,#59927,#59928,#59929)) ;
#24007 = EDGE_LOOP('',(#59930,#59931,#59932,#59933)) ;
#24008 = EDGE_LOOP('',(#59934,#59935,#59936,#59937)) ;
#24009 = EDGE_LOOP('',(#59938,#59939,#59940,#59941)) ;
#24010 = EDGE_LOOP('',(#59942,#59943,#59944,#59945,#59946,#59947)) ;
#24011 = EDGE_LOOP('',(#59948,#59949,#59950,#59951,#59952,#59953)) ;
#24012 = EDGE_LOOP('',(#59954,#59955,#59956,#59957,#59958)) ;
#24013 = EDGE_LOOP('',(#59959,#59960,#59961,#59962)) ;
#24014 = EDGE_LOOP('',(#59963,#59964,#59965,#59966)) ;
#24015 = EDGE_LOOP('',(#59967,#59968,#59969,#59970)) ;
#24016 = EDGE_LOOP('',(#59971,#59972,#59973,#59974)) ;
#24017 = EDGE_LOOP('',(#59975,#59976,#59977,#59978)) ;
#24018 = EDGE_LOOP('',(#59979,#59980,#59981,#59982)) ;
#24019 = EDGE_LOOP('',(#59983,#59984,#59985,#59986)) ;
#24020 = EDGE_LOOP('',(#59987,#59988,#59989,#59990)) ;
#24021 = EDGE_LOOP('',(#59991,#59992,#59993,#59994)) ;
#24022 = EDGE_LOOP('',(#59995,#59996,#59997,#59998)) ;
#24023 = EDGE_LOOP('',(#59999,#60000,#60001,#60002)) ;
#24024 = EDGE_LOOP('',(#60003,#60004,#60005,#60006)) ;
#24025 = EDGE_LOOP('',(#60007,#60008,#60009,#60010)) ;
#24026 = EDGE_LOOP('',(#60011,#60012,#60013,#60014,#60015,#60016)) ;
#24027 = EDGE_LOOP('',(#60017,#60018,#60019,#60020,#60021,#60022)) ;
#24028 = EDGE_LOOP('',(#60023,#60024,#60025,#60026,#60027)) ;
#24029 = EDGE_LOOP('',(#60028,#60029,#60030,#60031)) ;
#24030 = EDGE_LOOP('',(#60032,#60033,#60034,#60035)) ;
#24031 = EDGE_LOOP('',(#60036,#60037,#60038,#60039)) ;
#24032 = EDGE_LOOP('',(#60040,#60041,#60042,#60043)) ;
#24033 = EDGE_LOOP('',(#60044,#60045,#60046,#60047)) ;
#24034 = EDGE_LOOP('',(#60048,#60049,#60050,#60051)) ;
#24035 = EDGE_LOOP('',(#60052,#60053,#60054,#60055)) ;
#24036 = EDGE_LOOP('',(#60056,#60057,#60058,#60059)) ;
#24037 = EDGE_LOOP('',(#60060,#60061,#60062,#60063)) ;
#24038 = EDGE_LOOP('',(#60064,#60065,#60066,#60067)) ;
#24039 = EDGE_LOOP('',(#60068,#60069,#60070,#60071)) ;
#24040 = EDGE_LOOP('',(#60072,#60073,#60074,#60075)) ;
#24041 = EDGE_LOOP('',(#60076,#60077,#60078,#60079)) ;
#24042 = EDGE_LOOP('',(#60080,#60081,#60082,#60083,#60084,#60085)) ;
#24043 = EDGE_LOOP('',(#60086,#60087,#60088,#60089,#60090,#60091)) ;
#24044 = EDGE_LOOP('',(#60092,#60093,#60094,#60095,#60096)) ;
#24045 = EDGE_LOOP('',(#60097,#60098,#60099,#60100)) ;
#24046 = EDGE_LOOP('',(#60101,#60102,#60103,#60104)) ;
#24047 = EDGE_LOOP('',(#60105,#60106,#60107,#60108)) ;
#24048 = EDGE_LOOP('',(#60109,#60110,#60111,#60112)) ;
#24049 = EDGE_LOOP('',(#60113,#60114,#60115,#60116)) ;
#24050 = EDGE_LOOP('',(#60117,#60118,#60119,#60120)) ;
#24051 = EDGE_LOOP('',(#60121,#60122,#60123,#60124)) ;
#24052 = EDGE_LOOP('',(#60125,#60126,#60127,#60128)) ;
#24053 = EDGE_LOOP('',(#60129,#60130,#60131,#60132)) ;
#24054 = EDGE_LOOP('',(#60133,#60134,#60135,#60136)) ;
#24055 = EDGE_LOOP('',(#60137,#60138,#60139,#60140)) ;
#24056 = EDGE_LOOP('',(#60141,#60142,#60143,#60144)) ;
#24057 = EDGE_LOOP('',(#60145,#60146,#60147,#60148)) ;
#24058 = EDGE_LOOP('',(#60149,#60150,#60151,#60152,#60153,#60154)) ;
#24059 = EDGE_LOOP('',(#60155,#60156,#60157,#60158,#60159,#60160)) ;
#24060 = EDGE_LOOP('',(#60161,#60162,#60163,#60164,#60165)) ;
#24061 = EDGE_LOOP('',(#60166,#60167,#60168,#60169)) ;
#24062 = EDGE_LOOP('',(#60170,#60171,#60172,#60173)) ;
#24063 = EDGE_LOOP('',(#60174,#60175,#60176,#60177)) ;
#24064 = EDGE_LOOP('',(#60178,#60179,#60180,#60181)) ;
#24065 = EDGE_LOOP('',(#60182,#60183,#60184,#60185)) ;
#24066 = EDGE_LOOP('',(#60186,#60187,#60188,#60189)) ;
#24067 = EDGE_LOOP('',(#60190,#60191,#60192,#60193)) ;
#24068 = EDGE_LOOP('',(#60194,#60195,#60196,#60197)) ;
#24069 = EDGE_LOOP('',(#60198,#60199,#60200,#60201)) ;
#24070 = EDGE_LOOP('',(#60202,#60203,#60204,#60205)) ;
#24071 = EDGE_LOOP('',(#60206,#60207,#60208,#60209)) ;
#24072 = EDGE_LOOP('',(#60210,#60211,#60212,#60213)) ;
#24073 = EDGE_LOOP('',(#60214,#60215,#60216,#60217)) ;
#24074 = EDGE_LOOP('',(#60218,#60219,#60220,#60221,#60222,#60223)) ;
#24075 = EDGE_LOOP('',(#60224,#60225,#60226,#60227,#60228,#60229)) ;
#24076 = EDGE_LOOP('',(#60230,#60231,#60232,#60233,#60234)) ;
#24077 = EDGE_LOOP('',(#60235,#60236,#60237,#60238)) ;
#24078 = EDGE_LOOP('',(#60239,#60240,#60241,#60242)) ;
#24079 = EDGE_LOOP('',(#60243,#60244,#60245,#60246)) ;
#24080 = EDGE_LOOP('',(#60247,#60248,#60249,#60250)) ;
#24081 = EDGE_LOOP('',(#60251,#60252,#60253,#60254)) ;
#24082 = EDGE_LOOP('',(#60255,#60256,#60257,#60258)) ;
#24083 = EDGE_LOOP('',(#60259,#60260,#60261,#60262)) ;
#24084 = EDGE_LOOP('',(#60263,#60264,#60265,#60266)) ;
#24085 = EDGE_LOOP('',(#60267,#60268,#60269,#60270)) ;
#24086 = EDGE_LOOP('',(#60271,#60272,#60273,#60274)) ;
#24087 = EDGE_LOOP('',(#60275,#60276,#60277,#60278)) ;
#24088 = EDGE_LOOP('',(#60279,#60280,#60281,#60282)) ;
#24089 = EDGE_LOOP('',(#60283,#60284,#60285,#60286)) ;
#24090 = EDGE_LOOP('',(#60287,#60288,#60289,#60290,#60291,#60292)) ;
#24091 = EDGE_LOOP('',(#60293,#60294,#60295,#60296,#60297,#60298)) ;
#24092 = EDGE_LOOP('',(#60299,#60300,#60301,#60302,#60303)) ;
#24093 = EDGE_LOOP('',(#60304,#60305,#60306,#60307)) ;
#24094 = EDGE_LOOP('',(#60308,#60309,#60310,#60311)) ;
#24095 = EDGE_LOOP('',(#60312,#60313,#60314,#60315)) ;
#24096 = EDGE_LOOP('',(#60316,#60317,#60318,#60319)) ;
#24097 = EDGE_LOOP('',(#60320,#60321,#60322,#60323)) ;
#24098 = EDGE_LOOP('',(#60324,#60325,#60326,#60327)) ;
#24099 = EDGE_LOOP('',(#60328,#60329,#60330,#60331)) ;
#24100 = EDGE_LOOP('',(#60332,#60333,#60334,#60335)) ;
#24101 = EDGE_LOOP('',(#60336,#60337,#60338,#60339)) ;
#24102 = EDGE_LOOP('',(#60340,#60341,#60342,#60343)) ;
#24103 = EDGE_LOOP('',(#60344,#60345,#60346,#60347)) ;
#24104 = EDGE_LOOP('',(#60348,#60349,#60350,#60351)) ;
#24105 = EDGE_LOOP('',(#60352,#60353,#60354,#60355)) ;
#24106 = EDGE_LOOP('',(#60356,#60357,#60358,#60359,#60360,#60361)) ;
#24107 = EDGE_LOOP('',(#60362,#60363,#60364,#60365,#60366,#60367)) ;
#24108 = EDGE_LOOP('',(#60368,#60369,#60370,#60371,#60372)) ;
#24109 = EDGE_LOOP('',(#60373,#60374,#60375,#60376)) ;
#24110 = EDGE_LOOP('',(#60377,#60378,#60379,#60380)) ;
#24111 = EDGE_LOOP('',(#60381,#60382,#60383,#60384)) ;
#24112 = EDGE_LOOP('',(#60385,#60386,#60387,#60388)) ;
#24113 = EDGE_LOOP('',(#60389,#60390,#60391,#60392)) ;
#24114 = EDGE_LOOP('',(#60393,#60394,#60395,#60396)) ;
#24115 = EDGE_LOOP('',(#60397,#60398,#60399,#60400)) ;
#24116 = EDGE_LOOP('',(#60401,#60402,#60403,#60404)) ;
#24117 = EDGE_LOOP('',(#60405,#60406,#60407,#60408)) ;
#24118 = EDGE_LOOP('',(#60409,#60410,#60411,#60412)) ;
#24119 = EDGE_LOOP('',(#60413,#60414,#60415,#60416)) ;
#24120 = EDGE_LOOP('',(#60417,#60418,#60419,#60420)) ;
#24121 = EDGE_LOOP('',(#60421,#60422,#60423,#60424)) ;
#24122 = EDGE_LOOP('',(#60425,#60426,#60427,#60428)) ;
#24123 = EDGE_LOOP('',(#60429,#60430,#60431,#60432)) ;
#24124 = EDGE_LOOP('',(#60433,#60434,#60435,#60436)) ;
#24125 = EDGE_LOOP('',(#60437,#60438,#60439,#60440)) ;
#24126 = EDGE_LOOP('',(#60441,#60442,#60443,#60444)) ;
#24127 = EDGE_LOOP('',(#60445,#60446,#60447,#60448)) ;
#24128 = EDGE_LOOP('',(#60449,#60450,#60451,#60452)) ;
#24129 = EDGE_LOOP('',(#60453,#60454,#60455,#60456)) ;
#24130 = EDGE_LOOP('',(#60457,#60458,#60459,#60460)) ;
#24131 = EDGE_LOOP('',(#60461,#60462,#60463,#60464)) ;
#24132 = EDGE_LOOP('',(#60465,#60466,#60467,#60468)) ;
#24133 = EDGE_LOOP('',(#60469,#60470,#60471,#60472)) ;
#24134 = EDGE_LOOP('',(#60473,#60474,#60475,#60476)) ;
#24135 = EDGE_LOOP('',(#60477,#60478,#60479,#60480)) ;
#24136 = EDGE_LOOP('',(#60481,#60482,#60483,#60484)) ;
#24137 = EDGE_LOOP('',(#60485,#60486,#60487,#60488)) ;
#24138 = EDGE_LOOP('',(#60489,#60490,#60491,#60492)) ;
#24139 = EDGE_LOOP('',(#60493,#60494,#60495,#60496)) ;
#24140 = EDGE_LOOP('',(#60497,#60498,#60499,#60500)) ;
#24141 = EDGE_LOOP('',(#60501,#60502,#60503,#60504)) ;
#24142 = EDGE_LOOP('',(#60505,#60506,#60507,#60508)) ;
#24143 = EDGE_LOOP('',(#60509,#60510,#60511,#60512)) ;
#24144 = EDGE_LOOP('',(#60513,#60514,#60515,#60516)) ;
#24145 = EDGE_LOOP('',(#60517,#60518,#60519,#60520)) ;
#24146 = EDGE_LOOP('',(#60521,#60522,#60523,#60524)) ;
#24147 = EDGE_LOOP('',(#60525,#60526,#60527,#60528)) ;
#24148 = EDGE_LOOP('',(#60529,#60530,#60531,#60532)) ;
#24149 = EDGE_LOOP('',(#60533,#60534,#60535,#60536)) ;
#24150 = EDGE_LOOP('',(#60537,#60538,#60539,#60540)) ;
#24151 = EDGE_LOOP('',(#60541,#60542,#60543,#60544)) ;
#24152 = EDGE_LOOP('',(#60545,#60546,#60547,#60548)) ;
#24153 = EDGE_LOOP('',(#60549,#60550,#60551,#60552)) ;
#24154 = EDGE_LOOP('',(#60553,#60554,#60555,#60556)) ;
#24155 = EDGE_LOOP('',(#60557,#60558,#60559)) ;
#24156 = EDGE_LOOP('',(#60560,#60561,#60562,#60563)) ;
#24157 = EDGE_LOOP('',(#60564,#60565,#60566,#60567)) ;
#24158 = EDGE_LOOP('',(#60568,#60569,#60570,#60571)) ;
#24159 = EDGE_LOOP('',(#60572,#60573,#60574)) ;
#24160 = EDGE_LOOP('',(#60575,#60576,#60577)) ;
#24161 = EDGE_LOOP('',(#60578,#60579,#60580,#60581)) ;
#24162 = EDGE_LOOP('',(#60582,#60583,#60584,#60585)) ;
#24163 = EDGE_LOOP('',(#60586,#60587,#60588,#60589)) ;
#24164 = EDGE_LOOP('',(#60590,#60591,#60592)) ;
#24165 = EDGE_LOOP('',(#60593,#60594,#60595,#60596)) ;
#24166 = EDGE_LOOP('',(#60597,#60598,#60599,#60600)) ;
#24167 = EDGE_LOOP('',(#60601,#60602,#60603,#60604)) ;
#24168 = EDGE_LOOP('',(#60605,#60606,#60607,#60608)) ;
#24169 = EDGE_LOOP('',(#60609,#60610,#60611)) ;
#24170 = EDGE_LOOP('',(#60612,#60613,#60614,#60615)) ;
#24171 = EDGE_LOOP('',(#60616,#60617,#60618,#60619)) ;
#24172 = EDGE_LOOP('',(#60620,#60621,#60622,#60623)) ;
#24173 = EDGE_LOOP('',(#60624,#60625,#60626)) ;
#24174 = EDGE_LOOP('',(#60627,#60628,#60629)) ;
#24175 = EDGE_LOOP('',(#60630,#60631,#60632,#60633)) ;
#24176 = EDGE_LOOP('',(#60634,#60635,#60636,#60637)) ;
#24177 = EDGE_LOOP('',(#60638,#60639,#60640,#60641)) ;
#24178 = EDGE_LOOP('',(#60642,#60643,#60644)) ;
#24179 = EDGE_LOOP('',(#60645,#60646,#60647,#60648)) ;
#24180 = EDGE_LOOP('',(#60649,#60650,#60651,#60652)) ;
#24181 = EDGE_LOOP('',(#60653,#60654,#60655,#60656)) ;
#24182 = EDGE_LOOP('',(#60657,#60658,#60659,#60660)) ;
#24183 = EDGE_LOOP('',(#60661,#60662,#60663)) ;
#24184 = EDGE_LOOP('',(#60664,#60665,#60666,#60667)) ;
#24185 = EDGE_LOOP('',(#60668,#60669,#60670,#60671)) ;
#24186 = EDGE_LOOP('',(#60672,#60673,#60674,#60675)) ;
#24187 = EDGE_LOOP('',(#60676,#60677,#60678)) ;
#24188 = EDGE_LOOP('',(#60679,#60680,#60681)) ;
#24189 = EDGE_LOOP('',(#60682,#60683,#60684,#60685)) ;
#24190 = EDGE_LOOP('',(#60686,#60687,#60688,#60689)) ;
#24191 = EDGE_LOOP('',(#60690,#60691,#60692,#60693)) ;
#24192 = EDGE_LOOP('',(#60694,#60695,#60696)) ;
#24193 = EDGE_LOOP('',(#60697,#60698,#60699,#60700)) ;
#24194 = EDGE_LOOP('',(#60701,#60702,#60703,#60704)) ;
#24195 = EDGE_LOOP('',(#60705,#60706,#60707,#60708)) ;
#24196 = EDGE_LOOP('',(#60709,#60710,#60711,#60712)) ;
#24197 = EDGE_LOOP('',(#60713,#60714,#60715)) ;
#24198 = EDGE_LOOP('',(#60716,#60717,#60718,#60719)) ;
#24199 = EDGE_LOOP('',(#60720,#60721,#60722,#60723)) ;
#24200 = EDGE_LOOP('',(#60724,#60725,#60726,#60727)) ;
#24201 = EDGE_LOOP('',(#60728,#60729,#60730)) ;
#24202 = EDGE_LOOP('',(#60731,#60732,#60733)) ;
#24203 = EDGE_LOOP('',(#60734,#60735,#60736,#60737)) ;
#24204 = EDGE_LOOP('',(#60738,#60739,#60740,#60741)) ;
#24205 = EDGE_LOOP('',(#60742,#60743,#60744,#60745)) ;
#24206 = EDGE_LOOP('',(#60746,#60747,#60748)) ;
#24207 = EDGE_LOOP('',(#60749,#60750,#60751,#60752)) ;
#24208 = EDGE_LOOP('',(#60753,#60754,#60755,#60756)) ;
#24209 = EDGE_LOOP('',(#60757,#60758,#60759,#60760)) ;
#24210 = EDGE_LOOP('',(#60761,#60762,#60763,#60764)) ;
#24211 = EDGE_LOOP('',(#60765,#60766,#60767)) ;
#24212 = EDGE_LOOP('',(#60768,#60769,#60770,#60771)) ;
#24213 = EDGE_LOOP('',(#60772,#60773,#60774,#60775)) ;
#24214 = EDGE_LOOP('',(#60776,#60777,#60778,#60779)) ;
#24215 = EDGE_LOOP('',(#60780,#60781,#60782)) ;
#24216 = EDGE_LOOP('',(#60783,#60784,#60785)) ;
#24217 = EDGE_LOOP('',(#60786,#60787,#60788,#60789)) ;
#24218 = EDGE_LOOP('',(#60790,#60791,#60792,#60793)) ;
#24219 = EDGE_LOOP('',(#60794,#60795,#60796,#60797)) ;
#24220 = EDGE_LOOP('',(#60798,#60799,#60800)) ;
#24221 = EDGE_LOOP('',(#60801,#60802,#60803,#60804)) ;
#24222 = EDGE_LOOP('',(#60805,#60806,#60807,#60808)) ;
#24223 = EDGE_LOOP('',(#60809,#60810,#60811,#60812)) ;
#24224 = EDGE_LOOP('',(#60813,#60814,#60815,#60816)) ;
#24225 = EDGE_LOOP('',(#60817,#60818,#60819)) ;
#24226 = EDGE_LOOP('',(#60820,#60821,#60822,#60823)) ;
#24227 = EDGE_LOOP('',(#60824,#60825,#60826,#60827)) ;
#24228 = EDGE_LOOP('',(#60828,#60829,#60830,#60831)) ;
#24229 = EDGE_LOOP('',(#60832,#60833,#60834)) ;
#24230 = EDGE_LOOP('',(#60835,#60836,#60837)) ;
#24231 = EDGE_LOOP('',(#60838,#60839,#60840,#60841)) ;
#24232 = EDGE_LOOP('',(#60842,#60843,#60844,#60845)) ;
#24233 = EDGE_LOOP('',(#60846,#60847,#60848,#60849)) ;
#24234 = EDGE_LOOP('',(#60850,#60851,#60852)) ;
#24235 = EDGE_LOOP('',(#60853,#60854,#60855,#60856)) ;
#24236 = EDGE_LOOP('',(#60857,#60858,#60859,#60860)) ;
#24237 = EDGE_LOOP('',(#60861,#60862,#60863,#60864)) ;
#24238 = EDGE_LOOP('',(#60865,#60866,#60867,#60868)) ;
#24239 = EDGE_LOOP('',(#60869,#60870,#60871)) ;
#24240 = EDGE_LOOP('',(#60872,#60873,#60874,#60875)) ;
#24241 = EDGE_LOOP('',(#60876,#60877,#60878,#60879)) ;
#24242 = EDGE_LOOP('',(#60880,#60881,#60882,#60883)) ;
#24243 = EDGE_LOOP('',(#60884,#60885,#60886)) ;
#24244 = EDGE_LOOP('',(#60887,#60888,#60889)) ;
#24245 = EDGE_LOOP('',(#60890,#60891,#60892,#60893)) ;
#24246 = EDGE_LOOP('',(#60894,#60895,#60896,#60897)) ;
#24247 = EDGE_LOOP('',(#60898,#60899,#60900,#60901)) ;
#24248 = EDGE_LOOP('',(#60902,#60903,#60904)) ;
#24249 = EDGE_LOOP('',(#60905,#60906,#60907,#60908)) ;
#24250 = EDGE_LOOP('',(#60909,#60910,#60911,#60912)) ;
#24251 = EDGE_LOOP('',(#60913,#60914,#60915,#60916)) ;
#24252 = EDGE_LOOP('',(#60917,#60918,#60919,#60920)) ;
#24253 = EDGE_LOOP('',(#60921,#60922,#60923)) ;
#24254 = EDGE_LOOP('',(#60924,#60925,#60926,#60927)) ;
#24255 = EDGE_LOOP('',(#60928,#60929,#60930,#60931)) ;
#24256 = EDGE_LOOP('',(#60932,#60933,#60934,#60935)) ;
#24257 = EDGE_LOOP('',(#60936,#60937,#60938)) ;
#24258 = EDGE_LOOP('',(#60939,#60940,#60941)) ;
#24259 = EDGE_LOOP('',(#60942,#60943,#60944,#60945)) ;
#24260 = EDGE_LOOP('',(#60946,#60947,#60948,#60949)) ;
#24261 = EDGE_LOOP('',(#60950,#60951,#60952,#60953)) ;
#24262 = EDGE_LOOP('',(#60954,#60955,#60956)) ;
#24263 = EDGE_LOOP('',(#60957,#60958,#60959,#60960)) ;
#24264 = EDGE_LOOP('',(#60961,#60962,#60963,#60964)) ;
#24265 = EDGE_LOOP('',(#60965,#60966,#60967,#60968)) ;
#24266 = EDGE_LOOP('',(#60969,#60970,#60971,#60972)) ;
#24267 = EDGE_LOOP('',(#60973,#60974,#60975)) ;
#24268 = EDGE_LOOP('',(#60976,#60977,#60978,#60979)) ;
#24269 = EDGE_LOOP('',(#60980,#60981,#60982,#60983)) ;
#24270 = EDGE_LOOP('',(#60984,#60985,#60986,#60987)) ;
#24271 = EDGE_LOOP('',(#60988,#60989,#60990)) ;
#24272 = EDGE_LOOP('',(#60991,#60992,#60993)) ;
#24273 = EDGE_LOOP('',(#60994,#60995,#60996,#60997)) ;
#24274 = EDGE_LOOP('',(#60998,#60999,#61000,#61001)) ;
#24275 = EDGE_LOOP('',(#61002,#61003,#61004,#61005)) ;
#24276 = EDGE_LOOP('',(#61006,#61007,#61008)) ;
#24277 = EDGE_LOOP('',(#61009,#61010,#61011,#61012)) ;
#24278 = EDGE_LOOP('',(#61013,#61014,#61015,#61016)) ;
#24279 = EDGE_LOOP('',(#61017,#61018,#61019,#61020)) ;
#24280 = EDGE_LOOP('',(#61021,#61022,#61023,#61024)) ;
#24281 = EDGE_LOOP('',(#61025,#61026,#61027)) ;
#24282 = EDGE_LOOP('',(#61028,#61029,#61030,#61031)) ;
#24283 = EDGE_LOOP('',(#61032,#61033,#61034,#61035)) ;
#24284 = EDGE_LOOP('',(#61036,#61037,#61038,#61039)) ;
#24285 = EDGE_LOOP('',(#61040,#61041,#61042)) ;
#24286 = EDGE_LOOP('',(#61043,#61044,#61045)) ;
#24287 = EDGE_LOOP('',(#61046,#61047,#61048,#61049)) ;
#24288 = EDGE_LOOP('',(#61050,#61051,#61052,#61053)) ;
#24289 = EDGE_LOOP('',(#61054,#61055,#61056,#61057)) ;
#24290 = EDGE_LOOP('',(#61058,#61059,#61060)) ;
#24291 = EDGE_LOOP('',(#61061,#61062,#61063,#61064)) ;
#24292 = EDGE_LOOP('',(#61065,#61066,#61067,#61068)) ;
#24293 = EDGE_LOOP('',(#61069,#61070,#61071,#61072)) ;
#24294 = EDGE_LOOP('',(#61073,#61074,#61075,#61076)) ;
#24295 = EDGE_LOOP('',(#61077,#61078,#61079)) ;
#24296 = EDGE_LOOP('',(#61080,#61081,#61082,#61083)) ;
#24297 = EDGE_LOOP('',(#61084,#61085,#61086,#61087)) ;
#24298 = EDGE_LOOP('',(#61088,#61089,#61090,#61091)) ;
#24299 = EDGE_LOOP('',(#61092,#61093,#61094)) ;
#24300 = EDGE_LOOP('',(#61095,#61096,#61097)) ;
#24301 = EDGE_LOOP('',(#61098,#61099,#61100,#61101)) ;
#24302 = EDGE_LOOP('',(#61102,#61103,#61104,#61105)) ;
#24303 = EDGE_LOOP('',(#61106,#61107,#61108,#61109)) ;
#24304 = EDGE_LOOP('',(#61110,#61111,#61112)) ;
#24305 = EDGE_LOOP('',(#61113,#61114,#61115,#61116)) ;
#24306 = EDGE_LOOP('',(#61117,#61118,#61119,#61120)) ;
#24307 = EDGE_LOOP('',(#61121,#61122,#61123,#61124)) ;
#24308 = EDGE_LOOP('',(#61125,#61126,#61127,#61128)) ;
#24309 = EDGE_LOOP('',(#61129,#61130,#61131)) ;
#24310 = EDGE_LOOP('',(#61132,#61133,#61134,#61135)) ;
#24311 = EDGE_LOOP('',(#61136,#61137,#61138,#61139)) ;
#24312 = EDGE_LOOP('',(#61140,#61141,#61142,#61143)) ;
#24313 = EDGE_LOOP('',(#61144,#61145,#61146)) ;
#24314 = EDGE_LOOP('',(#61147,#61148,#61149)) ;
#24315 = EDGE_LOOP('',(#61150,#61151,#61152,#61153)) ;
#24316 = EDGE_LOOP('',(#61154,#61155,#61156,#61157)) ;
#24317 = EDGE_LOOP('',(#61158,#61159,#61160,#61161)) ;
#24318 = EDGE_LOOP('',(#61162,#61163,#61164)) ;
#24319 = EDGE_LOOP('',(#61165,#61166,#61167,#61168)) ;
#24320 = EDGE_LOOP('',(#61169,#61170,#61171,#61172)) ;
#24321 = EDGE_LOOP('',(#61173,#61174,#61175,#61176)) ;
#24322 = EDGE_LOOP('',(#61177,#61178,#61179,#61180)) ;
#24323 = EDGE_LOOP('',(#61181,#61182,#61183)) ;
#24324 = EDGE_LOOP('',(#61184,#61185,#61186,#61187)) ;
#24325 = EDGE_LOOP('',(#61188,#61189,#61190,#61191)) ;
#24326 = EDGE_LOOP('',(#61192,#61193,#61194,#61195)) ;
#24327 = EDGE_LOOP('',(#61196,#61197,#61198)) ;
#24328 = EDGE_LOOP('',(#61199,#61200,#61201)) ;
#24329 = EDGE_LOOP('',(#61202,#61203,#61204,#61205)) ;
#24330 = EDGE_LOOP('',(#61206,#61207,#61208,#61209)) ;
#24331 = EDGE_LOOP('',(#61210,#61211,#61212,#61213)) ;
#24332 = EDGE_LOOP('',(#61214,#61215,#61216)) ;
#24333 = EDGE_LOOP('',(#61217,#61218,#61219,#61220)) ;
#24334 = EDGE_LOOP('',(#61221,#61222,#61223,#61224)) ;
#24335 = EDGE_LOOP('',(#61225,#61226,#61227,#61228)) ;
#24336 = EDGE_LOOP('',(#61229,#61230,#61231,#61232)) ;
#24337 = EDGE_LOOP('',(#61233,#61234,#61235)) ;
#24338 = EDGE_LOOP('',(#61236,#61237,#61238,#61239)) ;
#24339 = EDGE_LOOP('',(#61240,#61241,#61242,#61243)) ;
#24340 = EDGE_LOOP('',(#61244,#61245,#61246,#61247)) ;
#24341 = EDGE_LOOP('',(#61248,#61249,#61250)) ;
#24342 = EDGE_LOOP('',(#61251,#61252,#61253)) ;
#24343 = EDGE_LOOP('',(#61254,#61255,#61256,#61257)) ;
#24344 = EDGE_LOOP('',(#61258,#61259,#61260,#61261)) ;
#24345 = EDGE_LOOP('',(#61262,#61263,#61264,#61265)) ;
#24346 = EDGE_LOOP('',(#61266,#61267,#61268)) ;
#24347 = EDGE_LOOP('',(#61269,#61270,#61271,#61272)) ;
#24348 = EDGE_LOOP('',(#61273,#61274,#61275,#61276)) ;
#24349 = EDGE_LOOP('',(#61277,#61278,#61279,#61280)) ;
#24350 = EDGE_LOOP('',(#61281,#61282,#61283,#61284)) ;
#24351 = EDGE_LOOP('',(#61285,#61286,#61287)) ;
#24352 = EDGE_LOOP('',(#61288,#61289,#61290,#61291)) ;
#24353 = EDGE_LOOP('',(#61292,#61293,#61294,#61295)) ;
#24354 = EDGE_LOOP('',(#61296,#61297,#61298,#61299)) ;
#24355 = EDGE_LOOP('',(#61300,#61301,#61302)) ;
#24356 = EDGE_LOOP('',(#61303,#61304,#61305)) ;
#24357 = EDGE_LOOP('',(#61306,#61307,#61308,#61309)) ;
#24358 = EDGE_LOOP('',(#61310,#61311,#61312,#61313)) ;
#24359 = EDGE_LOOP('',(#61314,#61315,#61316,#61317)) ;
#24360 = EDGE_LOOP('',(#61318,#61319,#61320)) ;
#24361 = EDGE_LOOP('',(#61321,#61322,#61323,#61324)) ;
#24362 = EDGE_LOOP('',(#61325,#61326,#61327,#61328)) ;
#24363 = EDGE_LOOP('',(#61329,#61330,#61331,#61332)) ;
#24364 = EDGE_LOOP('',(#61333,#61334,#61335,#61336)) ;
#24365 = EDGE_LOOP('',(#61337,#61338,#61339)) ;
#24366 = EDGE_LOOP('',(#61340,#61341,#61342,#61343)) ;
#24367 = EDGE_LOOP('',(#61344,#61345,#61346,#61347)) ;
#24368 = EDGE_LOOP('',(#61348,#61349,#61350,#61351)) ;
#24369 = EDGE_LOOP('',(#61352,#61353,#61354)) ;
#24370 = EDGE_LOOP('',(#61355,#61356,#61357)) ;
#24371 = EDGE_LOOP('',(#61358,#61359,#61360,#61361)) ;
#24372 = EDGE_LOOP('',(#61362,#61363,#61364,#61365)) ;
#24373 = EDGE_LOOP('',(#61366,#61367,#61368,#61369)) ;
#24374 = EDGE_LOOP('',(#61370,#61371,#61372)) ;
#24375 = EDGE_LOOP('',(#61373,#61374,#61375,#61376)) ;
#24376 = EDGE_LOOP('',(#61377,#61378,#61379,#61380)) ;
#24377 = EDGE_LOOP('',(#61381,#61382,#61383,#61384)) ;
#24378 = EDGE_LOOP('',(#61385,#61386,#61387,#61388)) ;
#24379 = EDGE_LOOP('',(#61389,#61390,#61391)) ;
#24380 = EDGE_LOOP('',(#61392,#61393,#61394,#61395)) ;
#24381 = EDGE_LOOP('',(#61396,#61397,#61398,#61399)) ;
#24382 = EDGE_LOOP('',(#61400,#61401,#61402,#61403)) ;
#24383 = EDGE_LOOP('',(#61404,#61405,#61406)) ;
#24384 = EDGE_LOOP('',(#61407,#61408,#61409)) ;
#24385 = EDGE_LOOP('',(#61410,#61411,#61412,#61413)) ;
#24386 = EDGE_LOOP('',(#61414,#61415,#61416,#61417)) ;
#24387 = EDGE_LOOP('',(#61418,#61419,#61420,#61421)) ;
#24388 = EDGE_LOOP('',(#61422,#61423,#61424)) ;
#24389 = EDGE_LOOP('',(#61425,#61426,#61427,#61428)) ;
#24390 = EDGE_LOOP('',(#61429,#61430,#61431,#61432)) ;
#24391 = EDGE_LOOP('',(#61433,#61434,#61435,#61436)) ;
#24392 = EDGE_LOOP('',(#61437,#61438,#61439,#61440)) ;
#24393 = EDGE_LOOP('',(#61441,#61442,#61443)) ;
#24394 = EDGE_LOOP('',(#61444,#61445,#61446,#61447)) ;
#24395 = EDGE_LOOP('',(#61448,#61449,#61450,#61451)) ;
#24396 = EDGE_LOOP('',(#61452,#61453,#61454,#61455)) ;
#24397 = EDGE_LOOP('',(#61456,#61457,#61458)) ;
#24398 = EDGE_LOOP('',(#61459,#61460,#61461)) ;
#24399 = EDGE_LOOP('',(#61462,#61463,#61464,#61465)) ;
#24400 = EDGE_LOOP('',(#61466,#61467,#61468,#61469)) ;
#24401 = EDGE_LOOP('',(#61470,#61471,#61472,#61473)) ;
#24402 = EDGE_LOOP('',(#61474,#61475,#61476)) ;
#24403 = EDGE_LOOP('',(#61477,#61478,#61479,#61480)) ;
#24404 = EDGE_LOOP('',(#61481,#61482,#61483,#61484)) ;
#24405 = EDGE_LOOP('',(#61485,#61486,#61487,#61488)) ;
#24406 = EDGE_LOOP('',(#61489,#61490,#61491,#61492)) ;
#24407 = EDGE_LOOP('',(#61493,#61494,#61495,#61496)) ;
#24408 = EDGE_LOOP('',(#61497,#61498,#61499,#61500)) ;
#24409 = EDGE_LOOP('',(#61501,#61502,#61503,#61504)) ;
#24410 = EDGE_LOOP('',(#61505,#61506,#61507,#61508)) ;
#24411 = EDGE_LOOP('',(#61509,#61510,#61511,#61512,#61513)) ;
#24412 = EDGE_LOOP('',(#61514,#61515,#61516,#61517)) ;
#24413 = EDGE_LOOP('',(#61518,#61519,#61520,#61521)) ;
#24414 = EDGE_LOOP('',(#61522,#61523,#61524,#61525)) ;
#24415 = EDGE_LOOP('',(#61526,#61527,#61528,#61529)) ;
#24416 = EDGE_LOOP('',(#61530,#61531,#61532,#61533)) ;
#24417 = EDGE_LOOP('',(#61534,#61535,#61536,#61537)) ;
#24418 = EDGE_LOOP('',(#61538,#61539,#61540,#61541)) ;
#24419 = EDGE_LOOP('',(#61542,#61543,#61544,#61545)) ;
#24420 = EDGE_LOOP('',(#61546,#61547,#61548,#61549)) ;
#24421 = EDGE_LOOP('',(#61550,#61551,#61552,#61553)) ;
#24422 = EDGE_LOOP('',(#61554,#61555,#61556,#61557)) ;
#24423 = EDGE_LOOP('',(#61558,#61559,#61560,#61561)) ;
#24424 = EDGE_LOOP('',(#61562,#61563,#61564,#61565)) ;
#24425 = EDGE_LOOP('',(#61566,#61567,#61568,#61569)) ;
#24426 = EDGE_LOOP('',(#61570,#61571,#61572,#61573)) ;
#24427 = EDGE_LOOP('',(#61574,#61575,#61576,#61577)) ;
#24428 = EDGE_LOOP('',(#61578,#61579,#61580,#61581)) ;
#24429 = EDGE_LOOP('',(#61582,#61583,#61584,#61585)) ;
#24430 = EDGE_LOOP('',(#61586,#61587,#61588,#61589)) ;
#24431 = EDGE_LOOP('',(#61590,#61591,#61592,#61593)) ;
#24432 = EDGE_LOOP('',(#61594,#61595,#61596,#61597)) ;
#24433 = EDGE_LOOP('',(#61598,#61599,#61600,#61601)) ;
#24434 = EDGE_LOOP('',(#61602,#61603,#61604,#61605)) ;
#24435 = EDGE_LOOP('',(#61606,#61607,#61608,#61609,#61610)) ;
#24436 = EDGE_LOOP('',(#61611,#61612,#61613,#61614)) ;
#24437 = EDGE_LOOP('',(#61615,#61616,#61617,#61618)) ;
#24438 = EDGE_LOOP('',(#61619,#61620,#61621,#61622)) ;
#24439 = EDGE_LOOP('',(#61623,#61624,#61625,#61626)) ;
#24440 = EDGE_LOOP('',(#61627,#61628,#61629,#61630)) ;
#24441 = EDGE_LOOP('',(#61631,#61632,#61633,#61634)) ;
#24442 = EDGE_LOOP('',(#61635,#61636,#61637,#61638)) ;
#24443 = EDGE_LOOP('',(#61639,#61640,#61641,#61642)) ;
#24444 = EDGE_LOOP('',(#61643,#61644,#61645,#61646)) ;
#24445 = EDGE_LOOP('',(#61647,#61648,#61649,#61650)) ;
#24446 = EDGE_LOOP('',(#61651,#61652,#61653,#61654)) ;
#24447 = EDGE_LOOP('',(#61655,#61656,#61657,#61658)) ;
#24448 = EDGE_LOOP('',(#61659,#61660,#61661,#61662)) ;
#24449 = EDGE_LOOP('',(#61663,#61664,#61665,#61666)) ;
#24450 = EDGE_LOOP('',(#61667,#61668,#61669,#61670)) ;
#24451 = EDGE_LOOP('',(#61671,#61672,#61673,#61674)) ;
#24452 = EDGE_LOOP('',(#61675,#61676,#61677,#61678)) ;
#24453 = EDGE_LOOP('',(#61679,#61680,#61681,#61682)) ;
#24454 = EDGE_LOOP('',(#61683,#61684,#61685,#61686)) ;
#24455 = EDGE_LOOP('',(#61687,#61688,#61689,#61690)) ;
#24456 = EDGE_LOOP('',(#61691,#61692,#61693,#61694)) ;
#24457 = EDGE_LOOP('',(#61695,#61696,#61697,#61698)) ;
#24458 = EDGE_LOOP('',(#61699,#61700,#61701,#61702)) ;
#24459 = EDGE_LOOP('',(#61703,#61704,#61705,#61706,#61707)) ;
#24460 = EDGE_LOOP('',(#61708,#61709,#61710,#61711)) ;
#24461 = EDGE_LOOP('',(#61712,#61713,#61714,#61715)) ;
#24462 = EDGE_LOOP('',(#61716,#61717,#61718,#61719)) ;
#24463 = EDGE_LOOP('',(#61720,#61721,#61722,#61723)) ;
#24464 = EDGE_LOOP('',(#61724,#61725,#61726,#61727)) ;
#24465 = EDGE_LOOP('',(#61728,#61729,#61730,#61731)) ;
#24466 = EDGE_LOOP('',(#61732,#61733,#61734,#61735)) ;
#24467 = EDGE_LOOP('',(#61736,#61737,#61738,#61739)) ;
#24468 = EDGE_LOOP('',(#61740,#61741,#61742,#61743)) ;
#24469 = EDGE_LOOP('',(#61744,#61745,#61746,#61747)) ;
#24470 = EDGE_LOOP('',(#61748,#61749,#61750,#61751)) ;
#24471 = EDGE_LOOP('',(#61752,#61753,#61754,#61755)) ;
#24472 = EDGE_LOOP('',(#61756,#61757,#61758,#61759)) ;
#24473 = EDGE_LOOP('',(#61760,#61761,#61762,#61763)) ;
#24474 = EDGE_LOOP('',(#61764,#61765,#61766,#61767)) ;
#24475 = EDGE_LOOP('',(#61768,#61769,#61770,#61771)) ;
#24476 = EDGE_LOOP('',(#61772,#61773,#61774,#61775)) ;
#24477 = EDGE_LOOP('',(#61776,#61777,#61778,#61779)) ;
#24478 = EDGE_LOOP('',(#61780,#61781,#61782,#61783)) ;
#24479 = EDGE_LOOP('',(#61784,#61785,#61786,#61787)) ;
#24480 = EDGE_LOOP('',(#61788,#61789,#61790,#61791)) ;
#24481 = EDGE_LOOP('',(#61792,#61793,#61794,#61795)) ;
#24482 = EDGE_LOOP('',(#61796,#61797,#61798,#61799)) ;
#24483 = EDGE_LOOP('',(#61800,#61801,#61802,#61803,#61804)) ;
#24484 = EDGE_LOOP('',(#61805,#61806,#61807,#61808)) ;
#24485 = EDGE_LOOP('',(#61809,#61810,#61811,#61812)) ;
#24486 = EDGE_LOOP('',(#61813,#61814,#61815,#61816)) ;
#24487 = EDGE_LOOP('',(#61817,#61818,#61819,#61820)) ;
#24488 = EDGE_LOOP('',(#61821,#61822,#61823,#61824)) ;
#24489 = EDGE_LOOP('',(#61825,#61826,#61827,#61828)) ;
#24490 = EDGE_LOOP('',(#61829,#61830,#61831,#61832)) ;
#24491 = EDGE_LOOP('',(#61833,#61834,#61835,#61836)) ;
#24492 = EDGE_LOOP('',(#61837,#61838,#61839,#61840)) ;
#24493 = EDGE_LOOP('',(#61841,#61842,#61843,#61844)) ;
#24494 = EDGE_LOOP('',(#61845,#61846,#61847,#61848)) ;
#24495 = EDGE_LOOP('',(#61849,#61850,#61851,#61852)) ;
#24496 = EDGE_LOOP('',(#61853,#61854,#61855,#61856)) ;
#24497 = EDGE_LOOP('',(#61857,#61858,#61859,#61860)) ;
#24498 = EDGE_LOOP('',(#61861,#61862,#61863,#61864)) ;
#24499 = EDGE_LOOP('',(#61865,#61866,#61867,#61868)) ;
#24500 = EDGE_LOOP('',(#61869,#61870,#61871,#61872)) ;
#24501 = EDGE_LOOP('',(#61873,#61874,#61875,#61876)) ;
#24502 = EDGE_LOOP('',(#61877,#61878,#61879,#61880)) ;
#24503 = EDGE_LOOP('',(#61881,#61882,#61883,#61884)) ;
#24504 = EDGE_LOOP('',(#61885,#61886,#61887,#61888)) ;
#24505 = EDGE_LOOP('',(#61889,#61890,#61891,#61892)) ;
#24506 = EDGE_LOOP('',(#61893,#61894,#61895,#61896)) ;
#24507 = EDGE_LOOP('',(#61897,#61898,#61899,#61900,#61901)) ;
#24508 = EDGE_LOOP('',(#61902,#61903,#61904,#61905)) ;
#24509 = EDGE_LOOP('',(#61906,#61907,#61908,#61909)) ;
#24510 = EDGE_LOOP('',(#61910,#61911,#61912,#61913)) ;
#24511 = EDGE_LOOP('',(#61914,#61915,#61916,#61917)) ;
#24512 = EDGE_LOOP('',(#61918,#61919,#61920,#61921)) ;
#24513 = EDGE_LOOP('',(#61922,#61923,#61924,#61925)) ;
#24514 = EDGE_LOOP('',(#61926,#61927,#61928,#61929)) ;
#24515 = EDGE_LOOP('',(#61930,#61931,#61932,#61933)) ;
#24516 = EDGE_LOOP('',(#61934,#61935,#61936,#61937)) ;
#24517 = EDGE_LOOP('',(#61938,#61939,#61940,#61941)) ;
#24518 = EDGE_LOOP('',(#61942,#61943,#61944,#61945)) ;
#24519 = EDGE_LOOP('',(#61946,#61947,#61948,#61949)) ;
#24520 = EDGE_LOOP('',(#61950,#61951,#61952,#61953)) ;
#24521 = EDGE_LOOP('',(#61954,#61955,#61956,#61957)) ;
#24522 = EDGE_LOOP('',(#61958,#61959,#61960,#61961)) ;
#24523 = EDGE_LOOP('',(#61962,#61963,#61964,#61965)) ;
#24524 = EDGE_LOOP('',(#61966,#61967,#61968,#61969)) ;
#24525 = EDGE_LOOP('',(#61970,#61971,#61972,#61973)) ;
#24526 = EDGE_LOOP('',(#61974,#61975,#61976,#61977)) ;
#24527 = EDGE_LOOP('',(#61978,#61979,#61980,#61981)) ;
#24528 = EDGE_LOOP('',(#61982,#61983,#61984,#61985)) ;
#24529 = EDGE_LOOP('',(#61986,#61987,#61988,#61989)) ;
#24530 = EDGE_LOOP('',(#61990,#61991,#61992,#61993)) ;
#24531 = EDGE_LOOP('',(#61994,#61995,#61996,#61997,#61998)) ;
#24532 = EDGE_LOOP('',(#61999,#62000,#62001,#62002)) ;
#24533 = EDGE_LOOP('',(#62003,#62004,#62005,#62006)) ;
#24534 = EDGE_LOOP('',(#62007,#62008,#62009,#62010)) ;
#24535 = EDGE_LOOP('',(#62011,#62012,#62013,#62014)) ;
#24536 = EDGE_LOOP('',(#62015,#62016,#62017,#62018)) ;
#24537 = EDGE_LOOP('',(#62019,#62020,#62021,#62022)) ;
#24538 = EDGE_LOOP('',(#62023,#62024,#62025,#62026)) ;
#24539 = EDGE_LOOP('',(#62027,#62028,#62029,#62030)) ;
#24540 = EDGE_LOOP('',(#62031,#62032,#62033,#62034)) ;
#24541 = EDGE_LOOP('',(#62035,#62036,#62037,#62038)) ;
#24542 = EDGE_LOOP('',(#62039,#62040,#62041,#62042)) ;
#24543 = EDGE_LOOP('',(#62043,#62044,#62045,#62046)) ;
#24544 = EDGE_LOOP('',(#62047,#62048,#62049,#62050)) ;
#24545 = EDGE_LOOP('',(#62051,#62052,#62053,#62054)) ;
#24546 = EDGE_LOOP('',(#62055,#62056,#62057,#62058)) ;
#24547 = EDGE_LOOP('',(#62059,#62060,#62061,#62062)) ;
#24548 = EDGE_LOOP('',(#62063,#62064,#62065,#62066)) ;
#24549 = EDGE_LOOP('',(#62067,#62068,#62069,#62070)) ;
#24550 = EDGE_LOOP('',(#62071,#62072,#62073,#62074)) ;
#24551 = EDGE_LOOP('',(#62075,#62076,#62077,#62078)) ;
#24552 = EDGE_LOOP('',(#62079,#62080,#62081,#62082)) ;
#24553 = EDGE_LOOP('',(#62083,#62084,#62085,#62086)) ;
#24554 = EDGE_LOOP('',(#62087,#62088,#62089,#62090)) ;
#24555 = EDGE_LOOP('',(#62091,#62092,#62093,#62094,#62095)) ;
#24556 = EDGE_LOOP('',(#62096,#62097,#62098,#62099)) ;
#24557 = EDGE_LOOP('',(#62100,#62101,#62102,#62103)) ;
#24558 = EDGE_LOOP('',(#62104,#62105,#62106,#62107)) ;
#24559 = EDGE_LOOP('',(#62108,#62109,#62110,#62111)) ;
#24560 = EDGE_LOOP('',(#62112,#62113,#62114,#62115)) ;
#24561 = EDGE_LOOP('',(#62116,#62117,#62118,#62119)) ;
#24562 = EDGE_LOOP('',(#62120,#62121,#62122,#62123)) ;
#24563 = EDGE_LOOP('',(#62124,#62125,#62126,#62127)) ;
#24564 = EDGE_LOOP('',(#62128,#62129,#62130,#62131)) ;
#24565 = EDGE_LOOP('',(#62132,#62133,#62134,#62135)) ;
#24566 = EDGE_LOOP('',(#62136,#62137,#62138,#62139)) ;
#24567 = EDGE_LOOP('',(#62140,#62141,#62142,#62143)) ;
#24568 = EDGE_LOOP('',(#62144,#62145,#62146,#62147)) ;
#24569 = EDGE_LOOP('',(#62148,#62149,#62150,#62151)) ;
#24570 = EDGE_LOOP('',(#62152,#62153,#62154,#62155)) ;
#24571 = EDGE_LOOP('',(#62156,#62157,#62158,#62159)) ;
#24572 = EDGE_LOOP('',(#62160,#62161,#62162,#62163)) ;
#24573 = EDGE_LOOP('',(#62164,#62165,#62166,#62167)) ;
#24574 = EDGE_LOOP('',(#62168,#62169,#62170,#62171)) ;
#24575 = EDGE_LOOP('',(#62172,#62173,#62174,#62175)) ;
#24576 = EDGE_LOOP('',(#62176,#62177,#62178,#62179)) ;
#24577 = EDGE_LOOP('',(#62180,#62181,#62182,#62183)) ;
#24578 = EDGE_LOOP('',(#62184,#62185,#62186,#62187)) ;
#24579 = EDGE_LOOP('',(#62188,#62189,#62190,#62191,#62192)) ;
#24580 = EDGE_LOOP('',(#62193,#62194,#62195,#62196)) ;
#24581 = EDGE_LOOP('',(#62197,#62198,#62199,#62200)) ;
#24582 = EDGE_LOOP('',(#62201,#62202,#62203,#62204)) ;
#24583 = EDGE_LOOP('',(#62205,#62206,#62207,#62208)) ;
#24584 = EDGE_LOOP('',(#62209,#62210,#62211,#62212)) ;
#24585 = EDGE_LOOP('',(#62213,#62214,#62215,#62216)) ;
#24586 = EDGE_LOOP('',(#62217,#62218,#62219,#62220)) ;
#24587 = EDGE_LOOP('',(#62221,#62222,#62223,#62224)) ;
#24588 = EDGE_LOOP('',(#62225,#62226,#62227,#62228)) ;
#24589 = EDGE_LOOP('',(#62229,#62230,#62231,#62232)) ;
#24590 = EDGE_LOOP('',(#62233,#62234,#62235,#62236)) ;
#24591 = EDGE_LOOP('',(#62237,#62238,#62239,#62240)) ;
#24592 = EDGE_LOOP('',(#62241,#62242,#62243,#62244)) ;
#24593 = EDGE_LOOP('',(#62245,#62246,#62247,#62248)) ;
#24594 = EDGE_LOOP('',(#62249,#62250,#62251,#62252)) ;
#24595 = EDGE_LOOP('',(#62253,#62254,#62255,#62256)) ;
#24596 = EDGE_LOOP('',(#62257,#62258,#62259,#62260)) ;
#24597 = EDGE_LOOP('',(#62261,#62262,#62263,#62264)) ;
#24598 = EDGE_LOOP('',(#62265,#62266,#62267,#62268)) ;
#24599 = EDGE_LOOP('',(#62269,#62270,#62271,#62272)) ;
#24600 = EDGE_LOOP('',(#62273,#62274,#62275,#62276)) ;
#24601 = EDGE_LOOP('',(#62277,#62278,#62279,#62280)) ;
#24602 = EDGE_LOOP('',(#62281,#62282,#62283,#62284)) ;
#24603 = EDGE_LOOP('',(#62285,#62286,#62287,#62288,#62289)) ;
#24604 = EDGE_LOOP('',(#62290,#62291,#62292,#62293)) ;
#24605 = EDGE_LOOP('',(#62294,#62295,#62296,#62297)) ;
#24606 = EDGE_LOOP('',(#62298,#62299,#62300,#62301)) ;
#24607 = EDGE_LOOP('',(#62302,#62303,#62304,#62305)) ;
#24608 = EDGE_LOOP('',(#62306,#62307,#62308,#62309)) ;
#24609 = EDGE_LOOP('',(#62310,#62311,#62312,#62313)) ;
#24610 = EDGE_LOOP('',(#62314,#62315,#62316,#62317)) ;
#24611 = EDGE_LOOP('',(#62318,#62319,#62320,#62321)) ;
#24612 = EDGE_LOOP('',(#62322,#62323,#62324,#62325)) ;
#24613 = EDGE_LOOP('',(#62326,#62327,#62328,#62329)) ;
#24614 = EDGE_LOOP('',(#62330,#62331,#62332,#62333)) ;
#24615 = EDGE_LOOP('',(#62334,#62335,#62336,#62337)) ;
#24616 = EDGE_LOOP('',(#62338,#62339,#62340,#62341)) ;
#24617 = EDGE_LOOP('',(#62342,#62343,#62344,#62345)) ;
#24618 = EDGE_LOOP('',(#62346,#62347,#62348,#62349)) ;
#24619 = EDGE_LOOP('',(#62350,#62351,#62352,#62353)) ;
#24620 = EDGE_LOOP('',(#62354,#62355,#62356,#62357)) ;
#24621 = EDGE_LOOP('',(#62358,#62359,#62360,#62361)) ;
#24622 = EDGE_LOOP('',(#62362,#62363,#62364,#62365)) ;
#24623 = EDGE_LOOP('',(#62366,#62367,#62368,#62369)) ;
#24624 = EDGE_LOOP('',(#62370,#62371,#62372,#62373)) ;
#24625 = EDGE_LOOP('',(#62374,#62375,#62376,#62377)) ;
#24626 = EDGE_LOOP('',(#62378,#62379,#62380,#62381)) ;
#24627 = EDGE_LOOP('',(#62382,#62383,#62384,#62385)) ;
#24628 = EDGE_LOOP('',(#62386,#62387,#62388,#62389)) ;
#24629 = EDGE_LOOP('',(#62390,#62391,#62392,#62393)) ;
#24630 = EDGE_LOOP('',(#62394,#62395,#62396,#62397)) ;
#24631 = EDGE_LOOP('',(#62398,#62399,#62400,#62401)) ;
#24632 = EDGE_LOOP('',(#62402,#62403,#62404,#62405)) ;
#24633 = EDGE_LOOP('',(#62406,#62407,#62408,#62409)) ;
#24634 = EDGE_LOOP('',(#62410,#62411,#62412,#62413)) ;
#24635 = EDGE_LOOP('',(#62414,#62415,#62416,#62417)) ;
#24636 = EDGE_LOOP('',(#62418,#62419,#62420,#62421)) ;
#24637 = EDGE_LOOP('',(#62422,#62423,#62424,#62425)) ;
#24638 = EDGE_LOOP('',(#62426,#62427,#62428,#62429)) ;
#24639 = EDGE_LOOP('',(#62430,#62431,#62432,#62433,#62434,#62435,#62436,#62437,
#62438,#62439)) ;
#24640 = EDGE_LOOP('',(#62440,#62441,#62442,#62443)) ;
#24641 = EDGE_LOOP('',(#62444,#62445,#62446,#62447)) ;
#24642 = EDGE_LOOP('',(#62448,#62449,#62450,#62451)) ;
#24643 = EDGE_LOOP('',(#62452,#62453,#62454,#62455)) ;
#24644 = EDGE_LOOP('',(#62456,#62457,#62458)) ;
#24645 = EDGE_LOOP('',(#62459,#62460,#62461,#62462)) ;
#24646 = EDGE_LOOP('',(#62463,#62464,#62465,#62466,#62467,#62468,#62469,#62470)) ;
#24647 = EDGE_LOOP('',(#62471,#62472,#62473,#62474)) ;
#24648 = EDGE_LOOP('',(#62475,#62476,#62477,#62478)) ;
#24649 = EDGE_LOOP('',(#62479,#62480,#62481,#62482)) ;
#24650 = EDGE_LOOP('',(#62483,#62484,#62485,#62486)) ;
#24651 = EDGE_LOOP('',(#62487,#62488,#62489,#62490)) ;
#24652 = EDGE_LOOP('',(#62491,#62492,#62493,#62494)) ;
#24653 = EDGE_LOOP('',(#62495,#62496,#62497,#62498)) ;
#24654 = EDGE_LOOP('',(#62499,#62500,#62501,#62502)) ;
#24655 = EDGE_LOOP('',(#62503,#62504,#62505,#62506)) ;
#24656 = EDGE_LOOP('',(#62507,#62508,#62509,#62510)) ;
#24657 = EDGE_LOOP('',(#62511,#62512,#62513,#62514)) ;
#24658 = EDGE_LOOP('',(#62515,#62516,#62517,#62518)) ;
#24659 = EDGE_LOOP('',(#62519,#62520,#62521,#62522)) ;
#24660 = EDGE_LOOP('',(#62523,#62524,#62525,#62526)) ;
#24661 = EDGE_LOOP('',(#62527,#62528,#62529,#62530)) ;
#24662 = EDGE_LOOP('',(#62531,#62532,#62533,#62534)) ;
#24663 = EDGE_LOOP('',(#62535,#62536,#62537,#62538)) ;
#24664 = EDGE_LOOP('',(#62539,#62540,#62541,#62542)) ;
#24665 = EDGE_LOOP('',(#62543,#62544,#62545,#62546,#62547,#62548)) ;
#24666 = EDGE_LOOP('',(#62549)) ;
#24667 = EDGE_LOOP('',(#62550,#62551,#62552,#62553,#62554,#62555)) ;
#24668 = EDGE_LOOP('',(#62556)) ;
#24669 = EDGE_LOOP('',(#62557)) ;
#24670 = EDGE_LOOP('',(#62558,#62559,#62560,#62561,#62562,#62563)) ;
#24671 = EDGE_LOOP('',(#62564,#62565,#62566,#62567,#62568,#62569)) ;
#24672 = EDGE_LOOP('',(#62570,#62571,#62572,#62573,#62574,#62575)) ;
#24673 = EDGE_LOOP('',(#62576,#62577,#62578,#62579,#62580,#62581)) ;
#24674 = EDGE_LOOP('',(#62582,#62583,#62584,#62585,#62586,#62587)) ;
#24675 = EDGE_LOOP('',(#62588,#62589,#62590,#62591,#62592,#62593)) ;
#24676 = EDGE_LOOP('',(#62594,#62595,#62596,#62597,#62598,#62599,#62600,#62601,
#62602,#62603,#62604,#62605,#62606,#62607,#62608,#62609,#62610,#62611,#62612,
#62613,#62614,#62615,#62616,#62617)) ;
#24677 = EDGE_LOOP('',(#62618,#62619,#62620,#62621,#62622,#62623,#62624,#62625,
#62626,#62627,#62628,#62629,#62630,#62631,#62632,#62633,#62634,#62635,#62636,
#62637,#62638,#62639,#62640,#62641,#62642)) ;
#24678 = EDGE_LOOP('',(#62643,#62644,#62645)) ;
#24679 = EDGE_LOOP('',(#62646,#62647,#62648,#62649)) ;
#24680 = EDGE_LOOP('',(#62650,#62651,#62652,#62653)) ;
#24681 = EDGE_LOOP('',(#62654,#62655,#62656,#62657,#62658,#62659,#62660,#62661,
#62662,#62663,#62664,#62665,#62666,#62667,#62668,#62669,#62670,#62671,#62672)) ;
#24682 = EDGE_LOOP('',(#62673,#62674)) ;
#24683 = EDGE_LOOP('',(#62675,#62676,#62677,#62678)) ;
#24684 = EDGE_LOOP('',(#62679,#62680,#62681,#62682)) ;
#24685 = EDGE_LOOP('',(#62683,#62684,#62685,#62686)) ;
#24686 = EDGE_LOOP('',(#62687,#62688,#62689,#62690)) ;
#24687 = EDGE_LOOP('',(#62691)) ;
#24688 = EDGE_LOOP('',(#62692,#62693,#62694,#62695,#62696,#62697,#62698,#62699,
#62700,#62701,#62702,#62703,#62704,#62705,#62706,#62707)) ;
#24689 = EDGE_LOOP('',(#62708,#62709,#62710,#62711)) ;
#24690 = EDGE_LOOP('',(#62712,#62713,#62714,#62715)) ;
#24691 = EDGE_LOOP('',(#62716,#62717,#62718,#62719)) ;
#24692 = EDGE_LOOP('',(#62720,#62721,#62722,#62723)) ;
#24693 = EDGE_LOOP('',(#62724,#62725,#62726,#62727,#62728,#62729)) ;
#24694 = EDGE_LOOP('',(#62730,#62731,#62732,#62733,#62734,#62735)) ;
#24695 = EDGE_LOOP('',(#62736,#62737,#62738)) ;
#24696 = EDGE_LOOP('',(#62739,#62740,#62741)) ;
#24697 = EDGE_LOOP('',(#62742,#62743,#62744)) ;
#24698 = EDGE_LOOP('',(#62745,#62746,#62747)) ;
#24699 = EDGE_LOOP('',(#62748,#62749,#62750)) ;
#24700 = EDGE_LOOP('',(#62751,#62752,#62753)) ;
#24701 = EDGE_LOOP('',(#62754,#62755,#62756)) ;
#24702 = EDGE_LOOP('',(#62757,#62758,#62759,#62760)) ;
#24703 = EDGE_LOOP('',(#62761,#62762,#62763,#62764)) ;
#24704 = EDGE_LOOP('',(#62765,#62766,#62767,#62768,#62769,#62770)) ;
#24705 = EDGE_LOOP('',(#62771,#62772,#62773,#62774,#62775,#62776)) ;
#24706 = EDGE_LOOP('',(#62777,#62778,#62779,#62780)) ;
#24707 = EDGE_LOOP('',(#62781,#62782,#62783,#62784)) ;
#24708 = EDGE_LOOP('',(#62785)) ;
#24709 = EDGE_LOOP('',(#62786)) ;
#24710 = EDGE_LOOP('',(#62787)) ;
#24711 = EDGE_LOOP('',(#62788,#62789,#62790)) ;
#24712 = EDGE_LOOP('',(#62791,#62792)) ;
#24713 = EDGE_LOOP('',(#62793,#62794)) ;
#24714 = EDGE_LOOP('',(#62795,#62796,#62797,#62798)) ;
#24715 = EDGE_LOOP('',(#62799,#62800,#62801)) ;
#24716 = EDGE_LOOP('',(#62802,#62803,#62804,#62805)) ;
#24717 = EDGE_LOOP('',(#62806,#62807,#62808,#62809)) ;
#24718 = EDGE_LOOP('',(#62810,#62811,#62812,#62813)) ;
#24719 = CIRCLE('',#67766,1.6) ;
#24720 = CIRCLE('',#67767,1.6) ;
#24721 = CIRCLE('',#67768,0.15) ;
#24722 = CIRCLE('',#67769,1.75) ;
#24723 = CIRCLE('',#67771,1.75) ;
#24724 = CIRCLE('',#67772,0.15) ;
#24725 = CIRCLE('',#67773,1.6) ;
#24726 = CIRCLE('',#67774,1.6) ;
#24727 = CIRCLE('',#67776,1.54393398282201) ;
#24728 = CIRCLE('',#67777,1.54393398282201) ;
#24729 = CIRCLE('',#67778,0.15) ;
#24730 = CIRCLE('',#67779,1.49999999999999) ;
#24731 = CIRCLE('',#67780,1.49999999999999) ;
#24732 = CIRCLE('',#67782,1.64999999999999) ;
#24733 = CIRCLE('',#67783,0.15) ;
#24734 = CIRCLE('',#67784,1.49999999999999) ;
#24735 = CIRCLE('',#67786,1.54393398282201) ;
#24736 = CIRCLE('',#67787,1.54393398282201) ;
#24737 = CIRCLE('',#67788,0.15) ;
#24738 = CIRCLE('',#67789,1.49999999999999) ;
#24739 = CIRCLE('',#67790,1.49999999999999) ;
#24740 = CIRCLE('',#67792,1.64999999999999) ;
#24741 = CIRCLE('',#67793,0.15) ;
#24742 = CIRCLE('',#67794,1.49999999999999) ;
#24743 = CIRCLE('',#67796,1.6) ;
#24744 = CIRCLE('',#67799,1.6) ;
#24745 = CIRCLE('',#67803,0.3) ;
#24746 = CIRCLE('',#67804,0.3) ;
#24747 = CIRCLE('',#67805,0.3) ;
#24748 = CIRCLE('',#67806,0.3) ;
#24749 = CIRCLE('',#67808,0.3) ;
#24750 = CIRCLE('',#67809,0.3) ;
#24751 = CIRCLE('',#67810,0.3) ;
#24752 = CIRCLE('',#67811,0.3) ;
#24753 = CIRCLE('',#67813,0.3) ;
#24754 = CIRCLE('',#67814,0.3) ;
#24755 = CIRCLE('',#67815,0.3) ;
#24756 = CIRCLE('',#67816,0.3) ;
#24757 = CIRCLE('',#67817,0.3) ;
#24758 = CIRCLE('',#67818,0.3) ;
#24759 = CIRCLE('',#67819,0.3) ;
#24760 = CIRCLE('',#67820,0.3) ;
#24761 = CIRCLE('',#67821,0.3) ;
#24762 = CIRCLE('',#67822,0.3) ;
#24763 = CIRCLE('',#67823,0.3) ;
#24764 = CIRCLE('',#67824,0.3) ;
#24765 = CIRCLE('',#67825,0.3) ;
#24766 = CIRCLE('',#67826,0.3) ;
#24767 = CIRCLE('',#67827,0.3) ;
#24768 = CIRCLE('',#67828,0.3) ;
#24769 = CIRCLE('',#67829,0.3) ;
#24770 = CIRCLE('',#67830,0.3) ;
#24771 = CIRCLE('',#67832,0.3) ;
#24772 = CIRCLE('',#67833,0.3) ;
#24773 = CIRCLE('',#67834,0.3) ;
#24774 = CIRCLE('',#67835,0.3) ;
#24775 = CIRCLE('',#67836,0.3) ;
#24776 = CIRCLE('',#67837,0.3) ;
#24777 = CIRCLE('',#67838,0.3) ;
#24778 = CIRCLE('',#67839,0.3) ;
#24779 = CIRCLE('',#67840,0.3) ;
#24780 = CIRCLE('',#67841,0.3) ;
#24781 = CIRCLE('',#67842,0.3) ;
#24782 = CIRCLE('',#67843,0.3) ;
#24783 = CIRCLE('',#67844,0.3) ;
#24784 = CIRCLE('',#67845,0.3) ;
#24785 = CIRCLE('',#67846,0.3) ;
#24786 = CIRCLE('',#67847,0.3) ;
#24787 = CIRCLE('',#67848,0.3) ;
#24788 = CIRCLE('',#67849,0.3) ;
#24789 = CIRCLE('',#67851,0.3) ;
#24790 = CIRCLE('',#67852,0.3) ;
#24791 = CIRCLE('',#67853,0.3) ;
#24792 = CIRCLE('',#67854,0.3) ;
#24793 = CIRCLE('',#67855,0.300000000000001) ;
#24794 = CIRCLE('',#67856,0.3) ;
#24795 = CIRCLE('',#67857,0.300000000000002) ;
#24796 = CIRCLE('',#67858,0.300000000000002) ;
#24797 = CIRCLE('',#67859,0.300000000000002) ;
#24798 = CIRCLE('',#67860,0.300000000000002) ;
#24799 = CIRCLE('',#67861,0.300000000000002) ;
#24800 = CIRCLE('',#67862,0.300000000000002) ;
#24801 = CIRCLE('',#67863,0.300000000000002) ;
#24802 = CIRCLE('',#67864,0.300000000000002) ;
#24803 = CIRCLE('',#67865,0.300000000000002) ;
#24804 = CIRCLE('',#67866,0.300000000000002) ;
#24805 = CIRCLE('',#67867,0.300000000000002) ;
#24806 = CIRCLE('',#67868,0.300000000000002) ;
#24807 = CIRCLE('',#67869,0.300000000000002) ;
#24808 = CIRCLE('',#67870,0.300000000000002) ;
#24809 = CIRCLE('',#67871,0.300000000000002) ;
#24810 = CIRCLE('',#67872,0.300000000000002) ;
#24811 = CIRCLE('',#67873,0.300000000000002) ;
#24812 = CIRCLE('',#67874,0.300000000000002) ;
#24813 = CIRCLE('',#67875,0.300000000000002) ;
#24814 = CIRCLE('',#67876,0.300000000000002) ;
#24815 = CIRCLE('',#67877,0.3) ;
#24816 = CIRCLE('',#67878,0.3) ;
#24817 = CIRCLE('',#67879,0.300000000000002) ;
#24818 = CIRCLE('',#67880,0.300000000000002) ;
#24819 = CIRCLE('',#67882,0.3) ;
#24820 = CIRCLE('',#67883,0.3) ;
#24821 = CIRCLE('',#67884,0.3) ;
#24822 = CIRCLE('',#67885,0.3) ;
#24823 = CIRCLE('',#67886,0.3) ;
#24824 = CIRCLE('',#67887,0.300000000000001) ;
#24825 = CIRCLE('',#67888,0.300000000000002) ;
#24826 = CIRCLE('',#67889,0.300000000000002) ;
#24827 = CIRCLE('',#67890,0.300000000000002) ;
#24828 = CIRCLE('',#67891,0.300000000000002) ;
#24829 = CIRCLE('',#67892,0.300000000000002) ;
#24830 = CIRCLE('',#67893,0.300000000000002) ;
#24831 = CIRCLE('',#67894,0.300000000000002) ;
#24832 = CIRCLE('',#67895,0.300000000000002) ;
#24833 = CIRCLE('',#67896,0.300000000000002) ;
#24834 = CIRCLE('',#67897,0.300000000000002) ;
#24835 = CIRCLE('',#67898,0.300000000000002) ;
#24836 = CIRCLE('',#67899,0.300000000000002) ;
#24837 = CIRCLE('',#67900,0.300000000000002) ;
#24838 = CIRCLE('',#67901,0.300000000000002) ;
#24839 = CIRCLE('',#67902,0.300000000000002) ;
#24840 = CIRCLE('',#67903,0.300000000000002) ;
#24841 = CIRCLE('',#67904,0.300000000000002) ;
#24842 = CIRCLE('',#67905,0.300000000000002) ;
#24843 = CIRCLE('',#67906,0.300000000000002) ;
#24844 = CIRCLE('',#67907,0.300000000000002) ;
#24845 = CIRCLE('',#67908,0.3) ;
#24846 = CIRCLE('',#67909,0.3) ;
#24847 = CIRCLE('',#67910,0.300000000000002) ;
#24848 = CIRCLE('',#67911,0.300000000000002) ;
#24849 = CIRCLE('',#67913,0.3) ;
#24850 = CIRCLE('',#67914,0.3) ;
#24851 = CIRCLE('',#67916,0.3) ;
#24852 = CIRCLE('',#67917,0.3) ;
#24853 = CIRCLE('',#67924,1.15) ;
#24854 = CIRCLE('',#67925,1.6) ;
#24855 = CIRCLE('',#67927,1.) ;
#24856 = CIRCLE('',#67928,1.75) ;
#24857 = CIRCLE('',#67930,1.75) ;
#24858 = CIRCLE('',#67932,1.) ;
#24859 = CIRCLE('',#67947,1.) ;
#24860 = CIRCLE('',#67948,1.75) ;
#24861 = CIRCLE('',#67950,1.) ;
#24862 = CIRCLE('',#67951,1.75) ;
#24863 = CIRCLE('',#67955,1.15) ;
#24864 = CIRCLE('',#67956,1.6) ;
#24865 = CIRCLE('',#67958,1.) ;
#24866 = CIRCLE('',#67959,1.75) ;
#24867 = CIRCLE('',#67961,1.75) ;
#24868 = CIRCLE('',#67963,1.) ;
#24869 = CIRCLE('',#68021,0.149999999999997) ;
#24870 = CIRCLE('',#68026,0.149999999999997) ;
#24871 = CIRCLE('',#68027,0.149999999999997) ;
#24872 = CIRCLE('',#68029,0.149999999999997) ;
#24873 = CIRCLE('',#68031,0.149999999999997) ;
#24874 = CIRCLE('',#68033,0.149999999999997) ;
#24875 = CIRCLE('',#68035,0.149999999999997) ;
#24876 = CIRCLE('',#68037,0.149999999999997) ;
#24877 = CIRCLE('',#68038,0.15) ;
#24878 = CIRCLE('',#68040,0.149999999999997) ;
#24879 = CIRCLE('',#68042,0.15) ;
#24880 = CIRCLE('',#68044,0.149999999999997) ;
#24881 = CIRCLE('',#68046,0.149999999999997) ;
#24882 = CIRCLE('',#68048,0.15) ;
#24883 = CIRCLE('',#68049,0.149999999999997) ;
#24884 = CIRCLE('',#68051,0.149999999999997) ;
#24885 = CIRCLE('',#68053,0.15) ;
#24886 = CIRCLE('',#68055,0.149999999999997) ;
#24887 = CIRCLE('',#68057,0.149999999999997) ;
#24888 = CIRCLE('',#68059,0.149999999999997) ;
#24889 = CIRCLE('',#68060,0.15) ;
#24890 = CIRCLE('',#68062,0.149999999999997) ;
#24891 = CIRCLE('',#68064,0.15) ;
#24892 = CIRCLE('',#68066,0.149999999999997) ;
#24893 = CIRCLE('',#68068,0.149999999999997) ;
#24894 = CIRCLE('',#68070,0.149999999999997) ;
#24895 = CIRCLE('',#68071,0.15) ;
#24896 = CIRCLE('',#68073,0.149999999999997) ;
#24897 = CIRCLE('',#68075,0.15) ;
#24898 = CIRCLE('',#68077,0.149999999999997) ;
#24899 = CIRCLE('',#68080,0.149999999999997) ;
#24900 = CIRCLE('',#68082,0.15) ;
#24901 = CIRCLE('',#68084,0.15) ;
#24902 = CIRCLE('',#68085,0.149999999999997) ;
#24903 = CIRCLE('',#68087,0.149999999999997) ;
#24904 = CIRCLE('',#68088,0.149999999999997) ;
#24905 = CIRCLE('',#68092,0.149999999999997) ;
#24906 = CIRCLE('',#68094,0.15) ;
#24907 = CIRCLE('',#68096,0.15) ;
#24908 = CIRCLE('',#68098,0.149999999999997) ;
#24909 = CIRCLE('',#68100,0.149999999999997) ;
#24910 = CIRCLE('',#68102,0.149999999999997) ;
#24911 = CIRCLE('',#68104,0.149999999999997) ;
#24912 = CIRCLE('',#68106,0.15) ;
#24913 = CIRCLE('',#68108,0.15) ;
#24914 = CIRCLE('',#68109,0.149999999999997) ;
#24915 = CIRCLE('',#68111,0.149999999999997) ;
#24916 = CIRCLE('',#68113,0.149999999999997) ;
#24917 = CIRCLE('',#68115,0.15) ;
#24918 = CIRCLE('',#68117,0.149999999999997) ;
#24919 = CIRCLE('',#68119,0.15) ;
#24920 = CIRCLE('',#68121,0.150000000000001) ;
#24921 = CIRCLE('',#68123,0.15) ;
#24922 = CIRCLE('',#68125,0.150000000000001) ;
#24923 = CIRCLE('',#68126,0.150000000000001) ;
#24924 = CIRCLE('',#68128,0.149999999999997) ;
#24925 = CIRCLE('',#68129,0.15) ;
#24926 = CIRCLE('',#68131,0.149999999999997) ;
#24927 = CIRCLE('',#68133,0.15) ;
#24928 = CIRCLE('',#68135,0.150000000000001) ;
#24929 = CIRCLE('',#68137,0.150000000000001) ;
#24930 = CIRCLE('',#68139,0.149999999999997) ;
#24931 = CIRCLE('',#68141,0.15) ;
#24932 = CIRCLE('',#68143,0.149999999999997) ;
#24933 = CIRCLE('',#68145,0.150000000000001) ;
#24934 = CIRCLE('',#68147,0.15) ;
#24935 = CIRCLE('',#68148,0.150000000000001) ;
#24936 = CIRCLE('',#68150,0.15) ;
#24937 = CIRCLE('',#68151,0.15) ;
#24938 = CIRCLE('',#68153,0.149999999999997) ;
#24939 = CIRCLE('',#68155,0.150000000000001) ;
#24940 = CIRCLE('',#68157,0.150000000000001) ;
#24941 = CIRCLE('',#68159,0.15) ;
#24942 = CIRCLE('',#68161,0.149999999999997) ;
#24943 = CIRCLE('',#68163,0.15) ;
#24944 = CIRCLE('',#68165,0.149999999999997) ;
#24945 = CIRCLE('',#68167,0.15) ;
#24946 = CIRCLE('',#68169,0.15) ;
#24947 = CIRCLE('',#68170,0.150000000000001) ;
#24948 = CIRCLE('',#68172,0.15) ;
#24949 = CIRCLE('',#68173,0.15) ;
#24950 = CIRCLE('',#68175,0.15) ;
#24951 = CIRCLE('',#68176,0.15) ;
#24952 = CIRCLE('',#68178,0.149999999999997) ;
#24953 = CIRCLE('',#68180,0.15) ;
#24954 = CIRCLE('',#68182,0.150000000000001) ;
#24955 = CIRCLE('',#68184,0.150000000000001) ;
#24956 = CIRCLE('',#68186,0.15) ;
#24957 = CIRCLE('',#68188,0.149999999999997) ;
#24958 = CIRCLE('',#68190,0.149999999999997) ;
#24959 = CIRCLE('',#68192,0.15) ;
#24960 = CIRCLE('',#68194,0.149999999999997) ;
#24961 = CIRCLE('',#68196,0.150000000000001) ;
#24962 = CIRCLE('',#68198,0.150000000000001) ;
#24963 = CIRCLE('',#68200,0.15) ;
#24964 = CIRCLE('',#68202,0.149999999999997) ;
#24965 = CIRCLE('',#68204,0.150000000000001) ;
#24966 = CIRCLE('',#68206,0.150000000000001) ;
#24967 = CIRCLE('',#68208,0.15) ;
#24968 = CIRCLE('',#68210,0.149999999999997) ;
#24969 = CIRCLE('',#68212,0.15) ;
#24970 = CIRCLE('',#68214,0.149999999999997) ;
#24971 = CIRCLE('',#68216,0.15) ;
#24972 = CIRCLE('',#68218,0.15) ;
#24973 = CIRCLE('',#68221,0.149999999999997) ;
#24974 = CIRCLE('',#68222,0.149999999999997) ;
#24975 = CIRCLE('',#68224,0.15) ;
#24976 = CIRCLE('',#68225,0.149999999999997) ;
#24977 = CIRCLE('',#68227,0.149999999999997) ;
#24978 = CIRCLE('',#68228,0.15) ;
#24979 = CIRCLE('',#68230,0.15) ;
#24980 = CIRCLE('',#68232,0.149999999999997) ;
#24981 = CIRCLE('',#68234,0.149999999999997) ;
#24982 = CIRCLE('',#68235,0.149999999999997) ;
#24983 = CIRCLE('',#68237,0.149999999999997) ;
#24984 = CIRCLE('',#68239,0.15) ;
#24985 = CIRCLE('',#68241,0.149999999999997) ;
#24986 = CIRCLE('',#68242,0.149999999999997) ;
#24987 = CIRCLE('',#68244,0.149999999999997) ;
#24988 = CIRCLE('',#68246,0.150000000000001) ;
#24989 = CIRCLE('',#68248,0.150000000000001) ;
#24990 = CIRCLE('',#68250,0.149999999999997) ;
#24991 = CIRCLE('',#68252,0.149999999999997) ;
#24992 = CIRCLE('',#68254,0.150000000000001) ;
#24993 = CIRCLE('',#68256,0.150000000000001) ;
#24994 = CIRCLE('',#68258,0.149999999999997) ;
#24995 = CIRCLE('',#68260,0.149999999999997) ;
#24996 = CIRCLE('',#68262,0.149999999999997) ;
#24997 = CIRCLE('',#68265,0.149999999999997) ;
#24998 = CIRCLE('',#68266,0.149999999999997) ;
#24999 = CIRCLE('',#68268,0.150000000000001) ;
#25000 = CIRCLE('',#68269,0.149999999999997) ;
#25001 = CIRCLE('',#68271,0.149999999999997) ;
#25002 = CIRCLE('',#68272,0.150000000000001) ;
#25003 = CIRCLE('',#68274,0.150000000000001) ;
#25004 = CIRCLE('',#68276,0.149999999999997) ;
#25005 = CIRCLE('',#68278,0.149999999999997) ;
#25006 = CIRCLE('',#68279,0.149999999999997) ;
#25007 = CIRCLE('',#68281,0.149999999999997) ;
#25008 = CIRCLE('',#68283,0.150000000000001) ;
#25009 = CIRCLE('',#68285,0.149999999999997) ;
#25010 = CIRCLE('',#68286,0.149999999999997) ;
#25011 = CIRCLE('',#68288,0.149999999999997) ;
#25012 = CIRCLE('',#68290,0.15) ;
#25013 = CIRCLE('',#68292,0.15) ;
#25014 = CIRCLE('',#68294,0.149999999999997) ;
#25015 = CIRCLE('',#68296,0.149999999999997) ;
#25016 = CIRCLE('',#68298,0.15) ;
#25017 = CIRCLE('',#68300,0.15) ;
#25018 = CIRCLE('',#68302,0.149999999999997) ;
#25019 = CIRCLE('',#68304,0.149999999999997) ;
#25020 = CIRCLE('',#68306,0.149999999999997) ;
#25021 = CIRCLE('',#68309,0.149999999999997) ;
#25022 = CIRCLE('',#68310,0.149999999999997) ;
#25023 = CIRCLE('',#68312,0.15) ;
#25024 = CIRCLE('',#68313,0.149999999999997) ;
#25025 = CIRCLE('',#68315,0.149999999999997) ;
#25026 = CIRCLE('',#68316,0.15) ;
#25027 = CIRCLE('',#68318,0.15) ;
#25028 = CIRCLE('',#68320,0.149999999999997) ;
#25029 = CIRCLE('',#68322,0.149999999999997) ;
#25030 = CIRCLE('',#68323,0.149999999999997) ;
#25031 = CIRCLE('',#68325,0.149999999999997) ;
#25032 = CIRCLE('',#68327,0.15) ;
#25033 = CIRCLE('',#68329,0.149999999999997) ;
#25034 = CIRCLE('',#68330,0.149999999999997) ;
#25035 = CIRCLE('',#68332,0.149999999999997) ;
#25036 = CIRCLE('',#68334,0.150000000000001) ;
#25037 = CIRCLE('',#68336,0.150000000000001) ;
#25038 = CIRCLE('',#68338,0.149999999999997) ;
#25039 = CIRCLE('',#68340,0.149999999999997) ;
#25040 = CIRCLE('',#68342,0.150000000000001) ;
#25041 = CIRCLE('',#68344,0.150000000000001) ;
#25042 = CIRCLE('',#68346,0.149999999999997) ;
#25043 = CIRCLE('',#68348,0.149999999999997) ;
#25044 = CIRCLE('',#68350,0.149999999999997) ;
#25045 = CIRCLE('',#68353,0.149999999999997) ;
#25046 = CIRCLE('',#68354,0.149999999999997) ;
#25047 = CIRCLE('',#68356,0.150000000000001) ;
#25048 = CIRCLE('',#68357,0.149999999999997) ;
#25049 = CIRCLE('',#68359,0.149999999999997) ;
#25050 = CIRCLE('',#68360,0.150000000000001) ;
#25051 = CIRCLE('',#68362,0.150000000000001) ;
#25052 = CIRCLE('',#68364,0.149999999999997) ;
#25053 = CIRCLE('',#68366,0.149999999999997) ;
#25054 = CIRCLE('',#68367,0.149999999999997) ;
#25055 = CIRCLE('',#68369,0.149999999999997) ;
#25056 = CIRCLE('',#68371,0.150000000000001) ;
#25057 = CIRCLE('',#68373,0.149999999999997) ;
#25058 = CIRCLE('',#68374,0.149999999999997) ;
#25059 = CIRCLE('',#68376,0.149999999999997) ;
#25060 = CIRCLE('',#68378,0.15) ;
#25061 = CIRCLE('',#68380,0.15) ;
#25062 = CIRCLE('',#68382,0.149999999999997) ;
#25063 = CIRCLE('',#68384,0.149999999999997) ;
#25064 = CIRCLE('',#68386,0.15) ;
#25065 = CIRCLE('',#68388,0.15) ;
#25066 = CIRCLE('',#68390,0.149999999999997) ;
#25067 = CIRCLE('',#68392,0.149999999999997) ;
#25068 = CIRCLE('',#68394,0.149999999999997) ;
#25069 = CIRCLE('',#68397,0.149999999999997) ;
#25070 = CIRCLE('',#68398,0.149999999999997) ;
#25071 = CIRCLE('',#68400,0.149999999999997) ;
#25072 = CIRCLE('',#68401,0.150000000000001) ;
#25073 = CIRCLE('',#68403,0.150000000000001) ;
#25074 = CIRCLE('',#68404,0.149999999999997) ;
#25075 = CIRCLE('',#68406,0.149999999999997) ;
#25076 = CIRCLE('',#68408,0.150000000000001) ;
#25077 = CIRCLE('',#68410,0.149999999999997) ;
#25078 = CIRCLE('',#68411,0.149999999999997) ;
#25079 = CIRCLE('',#68413,0.150000000000001) ;
#25080 = CIRCLE('',#68415,0.149999999999997) ;
#25081 = CIRCLE('',#68417,0.149999999999997) ;
#25082 = CIRCLE('',#68418,0.149999999999997) ;
#25083 = CIRCLE('',#68420,0.15) ;
#25084 = CIRCLE('',#68422,0.149999999999997) ;
#25085 = CIRCLE('',#68424,0.149999999999997) ;
#25086 = CIRCLE('',#68426,0.15) ;
#25087 = CIRCLE('',#68428,0.15) ;
#25088 = CIRCLE('',#68430,0.149999999999997) ;
#25089 = CIRCLE('',#68432,0.149999999999997) ;
#25090 = CIRCLE('',#68434,0.15) ;
#25091 = CIRCLE('',#68436,0.149999999999997) ;
#25092 = CIRCLE('',#68438,0.149999999999997) ;
#25093 = CIRCLE('',#68441,0.149999999999997) ;
#25094 = CIRCLE('',#68442,0.149999999999997) ;
#25095 = CIRCLE('',#68444,0.149999999999997) ;
#25096 = CIRCLE('',#68445,0.149999999999997) ;
#25097 = CIRCLE('',#68447,0.149999999999997) ;
#25098 = CIRCLE('',#68448,0.149999999999997) ;
#25099 = CIRCLE('',#68450,0.149999999999997) ;
#25100 = CIRCLE('',#68452,0.149999999999997) ;
#25101 = CIRCLE('',#68454,0.149999999999997) ;
#25102 = CIRCLE('',#68455,0.149999999999997) ;
#25103 = CIRCLE('',#68457,0.149999999999997) ;
#25104 = CIRCLE('',#68459,0.149999999999997) ;
#25105 = CIRCLE('',#68461,0.149999999999997) ;
#25106 = CIRCLE('',#68462,0.149999999999997) ;
#25107 = CIRCLE('',#68464,0.149999999999997) ;
#25108 = CIRCLE('',#68466,0.149999999999997) ;
#25109 = CIRCLE('',#68468,0.149999999999997) ;
#25110 = CIRCLE('',#68470,0.149999999999997) ;
#25111 = CIRCLE('',#68472,0.149999999999997) ;
#25112 = CIRCLE('',#68474,0.149999999999997) ;
#25113 = CIRCLE('',#68476,0.149999999999997) ;
#25114 = CIRCLE('',#68478,0.149999999999997) ;
#25115 = CIRCLE('',#68480,0.149999999999997) ;
#25116 = CIRCLE('',#68482,0.149999999999997) ;
#25117 = CIRCLE('',#68485,0.149999999999997) ;
#25118 = CIRCLE('',#68486,0.149999999999997) ;
#25119 = CIRCLE('',#68488,0.149999999999997) ;
#25120 = CIRCLE('',#68489,0.149999999999997) ;
#25121 = CIRCLE('',#68491,0.149999999999997) ;
#25122 = CIRCLE('',#68492,0.149999999999997) ;
#25123 = CIRCLE('',#68494,0.149999999999997) ;
#25124 = CIRCLE('',#68496,0.149999999999997) ;
#25125 = CIRCLE('',#68498,0.149999999999997) ;
#25126 = CIRCLE('',#68499,0.149999999999997) ;
#25127 = CIRCLE('',#68501,0.149999999999997) ;
#25128 = CIRCLE('',#68503,0.149999999999997) ;
#25129 = CIRCLE('',#68505,0.149999999999997) ;
#25130 = CIRCLE('',#68506,0.149999999999997) ;
#25131 = CIRCLE('',#68508,0.149999999999997) ;
#25132 = CIRCLE('',#68510,0.149999999999997) ;
#25133 = CIRCLE('',#68512,0.149999999999997) ;
#25134 = CIRCLE('',#68514,0.149999999999997) ;
#25135 = CIRCLE('',#68516,0.149999999999997) ;
#25136 = CIRCLE('',#68518,0.149999999999997) ;
#25137 = CIRCLE('',#68520,0.149999999999997) ;
#25138 = CIRCLE('',#68522,0.149999999999997) ;
#25139 = CIRCLE('',#68524,0.149999999999997) ;
#25140 = CIRCLE('',#68526,0.149999999999997) ;
#25141 = CIRCLE('',#68529,0.149999999999997) ;
#25142 = CIRCLE('',#68530,0.149999999999997) ;
#25143 = CIRCLE('',#68532,0.149999999999997) ;
#25144 = CIRCLE('',#68533,0.149999999999997) ;
#25145 = CIRCLE('',#68535,0.149999999999997) ;
#25146 = CIRCLE('',#68536,0.149999999999997) ;
#25147 = CIRCLE('',#68538,0.149999999999997) ;
#25148 = CIRCLE('',#68540,0.149999999999997) ;
#25149 = CIRCLE('',#68542,0.149999999999997) ;
#25150 = CIRCLE('',#68543,0.149999999999997) ;
#25151 = CIRCLE('',#68545,0.149999999999997) ;
#25152 = CIRCLE('',#68547,0.149999999999997) ;
#25153 = CIRCLE('',#68549,0.149999999999997) ;
#25154 = CIRCLE('',#68550,0.149999999999997) ;
#25155 = CIRCLE('',#68552,0.149999999999997) ;
#25156 = CIRCLE('',#68554,0.149999999999997) ;
#25157 = CIRCLE('',#68556,0.149999999999997) ;
#25158 = CIRCLE('',#68558,0.149999999999997) ;
#25159 = CIRCLE('',#68560,0.149999999999997) ;
#25160 = CIRCLE('',#68562,0.149999999999997) ;
#25161 = CIRCLE('',#68564,0.149999999999997) ;
#25162 = CIRCLE('',#68566,0.149999999999997) ;
#25163 = CIRCLE('',#68568,0.149999999999997) ;
#25164 = CIRCLE('',#68570,0.149999999999997) ;
#25165 = CIRCLE('',#68573,0.149999999999997) ;
#25166 = CIRCLE('',#68574,0.149999999999997) ;
#25167 = CIRCLE('',#68576,0.150000000000001) ;
#25168 = CIRCLE('',#68577,0.149999999999997) ;
#25169 = CIRCLE('',#68579,0.149999999999997) ;
#25170 = CIRCLE('',#68580,0.150000000000001) ;
#25171 = CIRCLE('',#68582,0.150000000000001) ;
#25172 = CIRCLE('',#68584,0.149999999999997) ;
#25173 = CIRCLE('',#68586,0.149999999999997) ;
#25174 = CIRCLE('',#68587,0.149999999999997) ;
#25175 = CIRCLE('',#68589,0.149999999999997) ;
#25176 = CIRCLE('',#68591,0.150000000000001) ;
#25177 = CIRCLE('',#68593,0.149999999999997) ;
#25178 = CIRCLE('',#68594,0.149999999999997) ;
#25179 = CIRCLE('',#68596,0.149999999999997) ;
#25180 = CIRCLE('',#68598,0.150000000000001) ;
#25181 = CIRCLE('',#68600,0.150000000000001) ;
#25182 = CIRCLE('',#68602,0.149999999999997) ;
#25183 = CIRCLE('',#68604,0.149999999999997) ;
#25184 = CIRCLE('',#68606,0.150000000000001) ;
#25185 = CIRCLE('',#68608,0.150000000000001) ;
#25186 = CIRCLE('',#68610,0.149999999999997) ;
#25187 = CIRCLE('',#68612,0.149999999999997) ;
#25188 = CIRCLE('',#68614,0.149999999999997) ;
#25189 = CIRCLE('',#68617,0.149999999999997) ;
#25190 = CIRCLE('',#68618,0.149999999999997) ;
#25191 = CIRCLE('',#68620,0.150000000000001) ;
#25192 = CIRCLE('',#68621,0.149999999999997) ;
#25193 = CIRCLE('',#68623,0.149999999999997) ;
#25194 = CIRCLE('',#68624,0.150000000000001) ;
#25195 = CIRCLE('',#68626,0.150000000000001) ;
#25196 = CIRCLE('',#68628,0.149999999999997) ;
#25197 = CIRCLE('',#68630,0.149999999999997) ;
#25198 = CIRCLE('',#68631,0.149999999999997) ;
#25199 = CIRCLE('',#68633,0.149999999999997) ;
#25200 = CIRCLE('',#68635,0.150000000000001) ;
#25201 = CIRCLE('',#68637,0.149999999999997) ;
#25202 = CIRCLE('',#68638,0.149999999999997) ;
#25203 = CIRCLE('',#68640,0.149999999999997) ;
#25204 = CIRCLE('',#68642,0.150000000000001) ;
#25205 = CIRCLE('',#68644,0.150000000000001) ;
#25206 = CIRCLE('',#68646,0.149999999999997) ;
#25207 = CIRCLE('',#68648,0.149999999999997) ;
#25208 = CIRCLE('',#68650,0.150000000000001) ;
#25209 = CIRCLE('',#68652,0.150000000000001) ;
#25210 = CIRCLE('',#68654,0.149999999999997) ;
#25211 = CIRCLE('',#68656,0.149999999999997) ;
#25212 = CIRCLE('',#68658,0.149999999999997) ;
#25213 = CIRCLE('',#68661,0.149999999999997) ;
#25214 = CIRCLE('',#68662,0.149999999999997) ;
#25215 = CIRCLE('',#68664,0.150000000000001) ;
#25216 = CIRCLE('',#68665,0.149999999999997) ;
#25217 = CIRCLE('',#68667,0.149999999999997) ;
#25218 = CIRCLE('',#68668,0.150000000000001) ;
#25219 = CIRCLE('',#68670,0.150000000000001) ;
#25220 = CIRCLE('',#68672,0.149999999999997) ;
#25221 = CIRCLE('',#68674,0.149999999999997) ;
#25222 = CIRCLE('',#68675,0.149999999999997) ;
#25223 = CIRCLE('',#68677,0.149999999999997) ;
#25224 = CIRCLE('',#68679,0.150000000000001) ;
#25225 = CIRCLE('',#68681,0.149999999999997) ;
#25226 = CIRCLE('',#68682,0.149999999999997) ;
#25227 = CIRCLE('',#68684,0.149999999999997) ;
#25228 = CIRCLE('',#68686,0.150000000000001) ;
#25229 = CIRCLE('',#68688,0.150000000000001) ;
#25230 = CIRCLE('',#68690,0.149999999999997) ;
#25231 = CIRCLE('',#68692,0.149999999999997) ;
#25232 = CIRCLE('',#68694,0.150000000000001) ;
#25233 = CIRCLE('',#68696,0.150000000000001) ;
#25234 = CIRCLE('',#68698,0.149999999999997) ;
#25235 = CIRCLE('',#68700,0.149999999999997) ;
#25236 = CIRCLE('',#68702,0.149999999999997) ;
#25237 = CIRCLE('',#68705,0.149999999999997) ;
#25238 = CIRCLE('',#68706,0.149999999999997) ;
#25239 = CIRCLE('',#68708,0.150000000000001) ;
#25240 = CIRCLE('',#68709,0.149999999999997) ;
#25241 = CIRCLE('',#68711,0.149999999999997) ;
#25242 = CIRCLE('',#68712,0.15) ;
#25243 = CIRCLE('',#68714,0.150000000000001) ;
#25244 = CIRCLE('',#68716,0.149999999999997) ;
#25245 = CIRCLE('',#68718,0.149999999999997) ;
#25246 = CIRCLE('',#68719,0.149999999999997) ;
#25247 = CIRCLE('',#68721,0.149999999999997) ;
#25248 = CIRCLE('',#68723,0.15) ;
#25249 = CIRCLE('',#68725,0.149999999999997) ;
#25250 = CIRCLE('',#68726,0.149999999999997) ;
#25251 = CIRCLE('',#68728,0.149999999999997) ;
#25252 = CIRCLE('',#68730,0.150000000000001) ;
#25253 = CIRCLE('',#68732,0.15) ;
#25254 = CIRCLE('',#68734,0.149999999999997) ;
#25255 = CIRCLE('',#68736,0.149999999999997) ;
#25256 = CIRCLE('',#68738,0.150000000000001) ;
#25257 = CIRCLE('',#68740,0.15) ;
#25258 = CIRCLE('',#68742,0.149999999999997) ;
#25259 = CIRCLE('',#68744,0.149999999999997) ;
#25260 = CIRCLE('',#68746,0.149999999999997) ;
#25261 = CIRCLE('',#68750,0.149999999999997) ;
#25262 = CIRCLE('',#68752,0.149999999999997) ;
#25263 = CIRCLE('',#68755,0.150000000000001) ;
#25264 = CIRCLE('',#68756,0.149999999999997) ;
#25265 = CIRCLE('',#68758,0.149999999999997) ;
#25266 = CIRCLE('',#68764,0.149999999999997) ;
#25267 = CIRCLE('',#68766,0.149999999999997) ;
#25268 = CIRCLE('',#68768,0.149999999999997) ;
#25269 = CIRCLE('',#68770,0.149999999999997) ;
#25270 = CIRCLE('',#68772,0.149999999999997) ;
#25271 = CIRCLE('',#68774,0.149999999999997) ;
#25272 = CIRCLE('',#68776,0.149999999999997) ;
#25273 = CIRCLE('',#68780,0.1) ;
#25274 = CIRCLE('',#68782,0.1) ;
#25275 = CIRCLE('',#68784,0.1) ;
#25276 = CIRCLE('',#68787,1.4) ;
#25277 = CIRCLE('',#68788,0.1) ;
#25278 = CIRCLE('',#68789,1.5) ;
#25279 = CIRCLE('',#68791,1.5) ;
#25280 = CIRCLE('',#68792,0.1) ;
#25281 = CIRCLE('',#68793,1.6) ;
#25282 = CIRCLE('',#68795,0.1) ;
#25283 = CIRCLE('',#68796,0.1) ;
#25284 = CIRCLE('',#68797,0.1) ;
#25285 = CIRCLE('',#68799,0.1) ;
#25286 = CIRCLE('',#68800,0.1) ;
#25287 = CIRCLE('',#68802,3.) ;
#25288 = CIRCLE('',#68803,0.1) ;
#25289 = CIRCLE('',#68804,3.00136060761679) ;
#25290 = CIRCLE('',#68805,0.1) ;
#25291 = CIRCLE('',#68808,3.) ;
#25292 = CIRCLE('',#68809,3.) ;
#25293 = CIRCLE('',#68810,3.) ;
#25294 = CIRCLE('',#68819,3.33471270883832) ;
#25295 = CIRCLE('',#68821,0.0999999999999994) ;
#25296 = CIRCLE('',#68822,0.0999999999999994) ;
#25297 = CIRCLE('',#68823,0.0999999999999994) ;
#25298 = CIRCLE('',#68824,0.0999999999999994) ;
#25299 = CIRCLE('',#68825,0.1) ;
#25300 = CIRCLE('',#68826,0.1) ;
#25301 = CIRCLE('',#68827,0.1) ;
#25302 = CIRCLE('',#68828,0.1) ;
#25303 = CIRCLE('',#68829,0.1) ;
#25304 = CIRCLE('',#68830,0.1) ;
#25305 = CIRCLE('',#68831,0.0999999999999994) ;
#25306 = CIRCLE('',#68832,0.0999999999999994) ;
#25307 = CIRCLE('',#68833,0.0999999999999994) ;
#25308 = CIRCLE('',#68834,0.1) ;
#25309 = CIRCLE('',#68835,0.1) ;
#25310 = CIRCLE('',#68836,0.1) ;
#25311 = CIRCLE('',#68838,0.0999999999999994) ;
#25312 = CIRCLE('',#68839,0.1) ;
#25313 = CIRCLE('',#68840,0.1) ;
#25314 = CIRCLE('',#68841,0.1) ;
#25315 = CIRCLE('',#68842,0.0999999999999994) ;
#25316 = CIRCLE('',#68843,0.0999999999999994) ;
#25317 = CIRCLE('',#68844,0.0999999999999994) ;
#25318 = CIRCLE('',#68845,0.1) ;
#25319 = CIRCLE('',#68846,0.1) ;
#25320 = CIRCLE('',#68847,0.1) ;
#25321 = CIRCLE('',#68848,0.1) ;
#25322 = CIRCLE('',#68849,0.1) ;
#25323 = CIRCLE('',#68850,0.1) ;
#25324 = CIRCLE('',#68851,0.0999999999999994) ;
#25325 = CIRCLE('',#68852,0.0999999999999994) ;
#25326 = CIRCLE('',#68853,0.0999999999999994) ;
#25327 = CIRCLE('',#68862,0.2) ;
#25328 = CIRCLE('',#68863,0.2) ;
#25329 = CIRCLE('',#68865,0.2) ;
#25330 = CIRCLE('',#68866,0.2) ;
#25331 = CIRCLE('',#68867,1.65) ;
#25332 = CIRCLE('',#68868,0.2) ;
#25333 = CIRCLE('',#68869,0.2) ;
#25334 = CIRCLE('',#68870,1.65) ;
#25335 = CIRCLE('',#68871,0.2) ;
#25336 = CIRCLE('',#68872,0.2) ;
#25337 = CIRCLE('',#68873,1.65) ;
#25338 = CIRCLE('',#68874,0.2) ;
#25339 = CIRCLE('',#68875,2.9) ;
#25340 = CIRCLE('',#68876,0.2) ;
#25341 = CIRCLE('',#68877,1.65) ;
#25342 = CIRCLE('',#68879,0.2) ;
#25343 = CIRCLE('',#68880,0.2) ;
#25344 = CIRCLE('',#68882,0.2) ;
#25345 = CIRCLE('',#68883,0.2) ;
#25346 = CIRCLE('',#68885,0.2) ;
#25347 = CIRCLE('',#68887,0.2) ;
#25348 = CIRCLE('',#68895,0.1) ;
#25349 = CIRCLE('',#68896,0.1) ;
#25350 = CIRCLE('',#68897,0.0999999999999998) ;
#25351 = CIRCLE('',#68898,0.0999999999999998) ;
#25352 = CIRCLE('',#68900,0.2) ;
#25353 = CIRCLE('',#68901,1.85) ;
#25354 = CIRCLE('',#68902,2.9) ;
#25355 = CIRCLE('',#68906,1.75) ;
#25356 = CIRCLE('',#68907,1.75) ;
#25357 = CIRCLE('',#68909,1.75) ;
#25358 = CIRCLE('',#68910,1.75) ;
#25359 = CIRCLE('',#68914,1.85) ;
#25360 = CIRCLE('',#68915,0.2) ;
#25361 = CIRCLE('',#68916,2.9) ;
#25362 = CIRCLE('',#68918,1.85) ;
#25363 = CIRCLE('',#68921,1.75) ;
#25364 = CIRCLE('',#68922,1.75) ;
#25365 = CIRCLE('',#68925,1.75) ;
#25366 = CIRCLE('',#68926,1.75) ;
#25367 = CIRCLE('',#68930,1.85) ;
#25368 = CIRCLE('',#68945,1.1) ;
#25369 = CIRCLE('',#68946,1.9) ;
#25370 = CIRCLE('',#68948,1.9) ;
#25371 = CIRCLE('',#68949,1.1) ;
#25372 = CIRCLE('',#68951,2.) ;
#25373 = CIRCLE('',#68952,2.) ;
#25374 = CIRCLE('',#68959,1.) ;
#25375 = CIRCLE('',#68960,1.) ;
#25376 = CIRCLE('',#68966,609.695407949973) ;
#25377 = CIRCLE('',#68968,3.23607331645511) ;
#25378 = CIRCLE('',#68969,576.383429116614) ;
#25379 = CIRCLE('',#68970,576.383429126766) ;
#25380 = CIRCLE('',#68972,609.695407938939) ;
#25381 = CIRCLE('',#68974,0.1) ;
#25382 = CIRCLE('',#68976,0.1) ;
#25383 = CIRCLE('',#68977,0.1) ;
#25384 = CIRCLE('',#68979,0.1) ;
#25385 = CIRCLE('',#68981,0.1) ;
#25386 = CIRCLE('',#68983,0.1) ;
#25387 = CIRCLE('',#68985,0.1) ;
#25388 = CIRCLE('',#68987,0.1) ;
#25389 = CIRCLE('',#68988,0.1) ;
#25390 = CIRCLE('',#68990,0.1) ;
#25391 = CIRCLE('',#68992,0.1) ;
#25392 = CIRCLE('',#68993,0.1) ;
#25393 = CIRCLE('',#68995,0.1) ;
#25394 = CIRCLE('',#68997,0.1) ;
#25395 = CIRCLE('',#68999,0.1) ;
#25396 = CIRCLE('',#69001,0.1) ;
#25397 = CIRCLE('',#69003,0.1) ;
#25398 = CIRCLE('',#69005,0.1) ;
#25399 = CIRCLE('',#69007,0.1) ;
#25400 = CIRCLE('',#69009,0.1) ;
#25401 = CIRCLE('',#69011,0.1) ;
#25402 = CIRCLE('',#69013,0.1) ;
#25403 = CIRCLE('',#69015,0.1) ;
#25404 = CIRCLE('',#69016,0.1) ;
#25405 = CIRCLE('',#69018,0.1) ;
#25406 = CIRCLE('',#69020,0.1) ;
#25407 = CIRCLE('',#69022,0.1) ;
#25408 = CIRCLE('',#69024,0.1) ;
#25409 = CIRCLE('',#69026,0.1) ;
#25410 = CIRCLE('',#69028,0.1) ;
#25411 = CIRCLE('',#69030,0.1) ;
#25412 = CIRCLE('',#69032,0.1) ;
#25413 = CIRCLE('',#69034,0.1) ;
#25414 = CIRCLE('',#69036,0.1) ;
#25415 = CIRCLE('',#69038,0.1) ;
#25416 = CIRCLE('',#69040,0.1) ;
#25417 = CIRCLE('',#69043,0.1) ;
#25418 = CIRCLE('',#69044,0.1) ;
#25419 = CIRCLE('',#69045,0.1) ;
#25420 = CIRCLE('',#69051,0.1) ;
#25421 = CIRCLE('',#69059,0.1) ;
#25422 = CIRCLE('',#69060,0.1) ;
#25423 = CIRCLE('',#69062,0.1) ;
#25424 = CIRCLE('',#69064,0.1) ;
#25425 = CIRCLE('',#69065,0.1) ;
#25426 = CIRCLE('',#69068,0.1) ;
#25427 = CIRCLE('',#69071,0.1) ;
#25428 = CIRCLE('',#69073,0.1) ;
#25429 = CIRCLE('',#69076,0.1) ;
#25430 = CIRCLE('',#69078,0.1) ;
#25431 = CIRCLE('',#69080,0.1) ;
#25432 = CIRCLE('',#69082,0.1) ;
#25433 = CIRCLE('',#69084,0.1) ;
#25434 = CIRCLE('',#69085,0.1) ;
#25435 = CIRCLE('',#69087,0.1) ;
#25436 = CIRCLE('',#69089,0.1) ;
#25437 = CIRCLE('',#69091,0.1) ;
#25438 = CIRCLE('',#69092,0.1) ;
#25439 = CIRCLE('',#69094,0.1) ;
#25440 = CIRCLE('',#69096,0.1) ;
#25441 = CIRCLE('',#69098,0.1) ;
#25442 = CIRCLE('',#69100,0.1) ;
#25443 = CIRCLE('',#69102,0.1) ;
#25444 = CIRCLE('',#69104,0.1) ;
#25445 = CIRCLE('',#69106,0.1) ;
#25446 = CIRCLE('',#69107,0.1) ;
#25447 = CIRCLE('',#69109,0.1) ;
#25448 = CIRCLE('',#69114,0.1) ;
#25449 = CIRCLE('',#69117,0.0999999999999998) ;
#25450 = CIRCLE('',#69119,0.1) ;
#25451 = CIRCLE('',#69120,0.1) ;
#25452 = CIRCLE('',#69122,0.1) ;
#25453 = CIRCLE('',#69124,0.0999999999999998) ;
#25454 = CIRCLE('',#69126,0.1) ;
#25455 = CIRCLE('',#69128,0.1) ;
#25456 = CIRCLE('',#69130,0.1) ;
#25457 = CIRCLE('',#69131,0.1) ;
#25458 = CIRCLE('',#69133,0.0999999999999999) ;
#25459 = CIRCLE('',#69135,0.1) ;
#25460 = CIRCLE('',#69136,0.1) ;
#25461 = CIRCLE('',#69138,0.1) ;
#25462 = CIRCLE('',#69140,0.0999999999999999) ;
#25463 = CIRCLE('',#69142,0.0999999999999998) ;
#25464 = CIRCLE('',#69144,0.1) ;
#25465 = CIRCLE('',#69146,0.1) ;
#25466 = CIRCLE('',#69148,0.1) ;
#25467 = CIRCLE('',#69149,0.1) ;
#25468 = CIRCLE('',#69151,0.1) ;
#25469 = CIRCLE('',#69153,0.1) ;
#25470 = CIRCLE('',#69155,0.1) ;
#25471 = CIRCLE('',#69158,0.1) ;
#25472 = CIRCLE('',#69160,0.1) ;
#25473 = CIRCLE('',#69161,0.1) ;
#25474 = CIRCLE('',#69164,0.1) ;
#25475 = CIRCLE('',#69166,0.1) ;
#25476 = CIRCLE('',#69167,0.1) ;
#25477 = CIRCLE('',#69169,0.0999999999999999) ;
#25478 = CIRCLE('',#69171,0.0999999999999998) ;
#25479 = CIRCLE('',#69173,0.1) ;
#25480 = CIRCLE('',#69174,0.1) ;
#25481 = CIRCLE('',#69176,0.1) ;
#25482 = CIRCLE('',#69178,0.1) ;
#25483 = CIRCLE('',#69180,0.1) ;
#25484 = CIRCLE('',#69182,0.1) ;
#25485 = CIRCLE('',#69184,0.0999999999999998) ;
#25486 = CIRCLE('',#69186,0.0999999999999999) ;
#25487 = CIRCLE('',#69188,0.1) ;
#25488 = CIRCLE('',#69191,0.1) ;
#25489 = CIRCLE('',#69193,0.1) ;
#25490 = CIRCLE('',#69195,0.1) ;
#25491 = CIRCLE('',#69197,0.1) ;
#25492 = CIRCLE('',#69198,0.1) ;
#25493 = CIRCLE('',#69200,0.1) ;
#25494 = CIRCLE('',#69202,0.1) ;
#25495 = CIRCLE('',#69204,0.1) ;
#25496 = CIRCLE('',#69205,0.0999999999999998) ;
#25497 = CIRCLE('',#69207,0.1) ;
#25498 = CIRCLE('',#69209,0.1) ;
#25499 = CIRCLE('',#69210,0.1) ;
#25500 = CIRCLE('',#69212,0.1) ;
#25501 = CIRCLE('',#69214,0.0999999999999998) ;
#25502 = CIRCLE('',#69216,0.1) ;
#25503 = CIRCLE('',#69217,0.1) ;
#25504 = CIRCLE('',#69219,0.0999999999999998) ;
#25505 = CIRCLE('',#69221,0.1) ;
#25506 = CIRCLE('',#69223,0.1) ;
#25507 = CIRCLE('',#69225,0.0999999999999998) ;
#25508 = CIRCLE('',#69227,0.1) ;
#25509 = CIRCLE('',#69229,0.1) ;
#25510 = CIRCLE('',#69231,0.1) ;
#25511 = CIRCLE('',#69232,0.1) ;
#25512 = CIRCLE('',#69235,0.0999999999999998) ;
#25513 = CIRCLE('',#69237,0.1) ;
#25514 = CIRCLE('',#69239,0.1) ;
#25515 = CIRCLE('',#69240,0.1) ;
#25516 = CIRCLE('',#69242,0.1) ;
#25517 = CIRCLE('',#69243,0.0999999999999998) ;
#25518 = CIRCLE('',#69245,0.0999999999999994) ;
#25519 = CIRCLE('',#69246,0.1) ;
#25520 = CIRCLE('',#69248,0.0999999999999998) ;
#25521 = CIRCLE('',#69250,0.0999999999999998) ;
#25522 = CIRCLE('',#69252,0.1) ;
#25523 = CIRCLE('',#69254,0.0999999999999994) ;
#25524 = CIRCLE('',#69256,0.0999999999999994) ;
#25525 = CIRCLE('',#69258,0.1) ;
#25526 = CIRCLE('',#69259,0.1) ;
#25527 = CIRCLE('',#69261,0.1) ;
#25528 = CIRCLE('',#69262,0.1) ;
#25529 = CIRCLE('',#69264,0.0999999999999998) ;
#25530 = CIRCLE('',#69266,0.1) ;
#25531 = CIRCLE('',#69268,0.0999999999999994) ;
#25532 = CIRCLE('',#69271,0.0999999999999994) ;
#25533 = CIRCLE('',#69273,0.0999999999999999) ;
#25534 = CIRCLE('',#69275,0.1) ;
#25535 = CIRCLE('',#69277,0.1) ;
#25536 = CIRCLE('',#69279,0.0999999999999994) ;
#25537 = CIRCLE('',#69281,0.0999999999999998) ;
#25538 = CIRCLE('',#69285,0.1) ;
#25539 = CIRCLE('',#69287,0.1) ;
#25540 = CIRCLE('',#69289,0.0999999999999994) ;
#25541 = CIRCLE('',#69291,0.1) ;
#25542 = CIRCLE('',#69293,0.0999999999999994) ;
#25543 = CIRCLE('',#69295,0.100000000000001) ;
#25544 = CIRCLE('',#69299,0.1) ;
#25545 = CIRCLE('',#69300,0.1) ;
#25546 = CIRCLE('',#69306,0.0999999999999994) ;
#25547 = CIRCLE('',#69308,0.1) ;
#25548 = CIRCLE('',#69309,0.0999999999999999) ;
#25549 = CIRCLE('',#69311,0.0999999999999994) ;
#25550 = CIRCLE('',#69312,0.1) ;
#25551 = CIRCLE('',#69314,0.1) ;
#25552 = CIRCLE('',#69316,0.1) ;
#25553 = CIRCLE('',#69318,0.1) ;
#25554 = CIRCLE('',#69319,0.1) ;
#25555 = CIRCLE('',#69321,0.1) ;
#25556 = CIRCLE('',#69323,0.1) ;
#25557 = CIRCLE('',#69325,0.1) ;
#25558 = CIRCLE('',#69326,0.1) ;
#25559 = CIRCLE('',#69328,0.1) ;
#25560 = CIRCLE('',#69331,0.0999999999999994) ;
#25561 = CIRCLE('',#69333,0.0999999999999994) ;
#25562 = CIRCLE('',#69337,0.1) ;
#25563 = CIRCLE('',#69339,0.0999999999999994) ;
#25564 = CIRCLE('',#69341,0.0999999999999999) ;
#25565 = CIRCLE('',#69342,0.1) ;
#25566 = CIRCLE('',#69345,0.1) ;
#25567 = CIRCLE('',#69346,0.0999999999999998) ;
#25568 = CIRCLE('',#69348,0.1) ;
#25569 = CIRCLE('',#69350,0.1) ;
#25570 = CIRCLE('',#69352,0.0999999999999998) ;
#25571 = CIRCLE('',#69354,0.1) ;
#25572 = CIRCLE('',#69356,0.1) ;
#25573 = CIRCLE('',#69358,0.1) ;
#25574 = CIRCLE('',#69361,0.0999999999999994) ;
#25575 = CIRCLE('',#69362,0.1) ;
#25576 = CIRCLE('',#69364,0.0999999999999994) ;
#25577 = CIRCLE('',#69366,0.1) ;
#25578 = CIRCLE('',#69368,0.1) ;
#25579 = CIRCLE('',#69370,0.1) ;
#25580 = CIRCLE('',#69372,0.1) ;
#25581 = CIRCLE('',#69374,0.0999999999999994) ;
#25582 = CIRCLE('',#69377,0.0999999999999994) ;
#25583 = CIRCLE('',#69379,0.0999999999999999) ;
#25584 = CIRCLE('',#69380,0.0999999999999999) ;
#25585 = CIRCLE('',#69384,0.0999999999999994) ;
#25586 = CIRCLE('',#69386,0.0999999999999994) ;
#25587 = CIRCLE('',#69390,0.1) ;
#25588 = CIRCLE('',#69392,0.1) ;
#25589 = CIRCLE('',#69394,0.1) ;
#25590 = CIRCLE('',#69397,1.4) ;
#25591 = CIRCLE('',#69398,0.1) ;
#25592 = CIRCLE('',#69399,1.5) ;
#25593 = CIRCLE('',#69401,1.5) ;
#25594 = CIRCLE('',#69402,0.1) ;
#25595 = CIRCLE('',#69403,1.6) ;
#25596 = CIRCLE('',#69405,0.1) ;
#25597 = CIRCLE('',#69406,0.1) ;
#25598 = CIRCLE('',#69407,0.1) ;
#25599 = CIRCLE('',#69409,0.1) ;
#25600 = CIRCLE('',#69410,0.1) ;
#25601 = CIRCLE('',#69412,3.) ;
#25602 = CIRCLE('',#69413,0.1) ;
#25603 = CIRCLE('',#69414,3.00136060761679) ;
#25604 = CIRCLE('',#69415,0.1) ;
#25605 = CIRCLE('',#69418,3.) ;
#25606 = CIRCLE('',#69419,3.) ;
#25607 = CIRCLE('',#69420,3.) ;
#25608 = CIRCLE('',#69429,3.33471270883832) ;
#25609 = CIRCLE('',#69431,0.0999999999999994) ;
#25610 = CIRCLE('',#69432,0.0999999999999994) ;
#25611 = CIRCLE('',#69433,0.0999999999999994) ;
#25612 = CIRCLE('',#69434,0.0999999999999994) ;
#25613 = CIRCLE('',#69435,0.1) ;
#25614 = CIRCLE('',#69436,0.1) ;
#25615 = CIRCLE('',#69437,0.1) ;
#25616 = CIRCLE('',#69438,0.1) ;
#25617 = CIRCLE('',#69439,0.1) ;
#25618 = CIRCLE('',#69440,0.1) ;
#25619 = CIRCLE('',#69441,0.0999999999999994) ;
#25620 = CIRCLE('',#69442,0.0999999999999994) ;
#25621 = CIRCLE('',#69443,0.0999999999999994) ;
#25622 = CIRCLE('',#69444,0.1) ;
#25623 = CIRCLE('',#69445,0.1) ;
#25624 = CIRCLE('',#69446,0.1) ;
#25625 = CIRCLE('',#69448,0.0999999999999994) ;
#25626 = CIRCLE('',#69449,0.1) ;
#25627 = CIRCLE('',#69450,0.1) ;
#25628 = CIRCLE('',#69451,0.1) ;
#25629 = CIRCLE('',#69452,0.0999999999999994) ;
#25630 = CIRCLE('',#69453,0.0999999999999994) ;
#25631 = CIRCLE('',#69454,0.0999999999999994) ;
#25632 = CIRCLE('',#69455,0.1) ;
#25633 = CIRCLE('',#69456,0.1) ;
#25634 = CIRCLE('',#69457,0.1) ;
#25635 = CIRCLE('',#69458,0.1) ;
#25636 = CIRCLE('',#69459,0.1) ;
#25637 = CIRCLE('',#69460,0.1) ;
#25638 = CIRCLE('',#69461,0.0999999999999994) ;
#25639 = CIRCLE('',#69462,0.0999999999999994) ;
#25640 = CIRCLE('',#69463,0.0999999999999994) ;
#25641 = CIRCLE('',#69472,0.2) ;
#25642 = CIRCLE('',#69473,0.2) ;
#25643 = CIRCLE('',#69475,0.2) ;
#25644 = CIRCLE('',#69476,0.2) ;
#25645 = CIRCLE('',#69477,1.65) ;
#25646 = CIRCLE('',#69478,0.2) ;
#25647 = CIRCLE('',#69479,0.2) ;
#25648 = CIRCLE('',#69480,1.65) ;
#25649 = CIRCLE('',#69481,0.2) ;
#25650 = CIRCLE('',#69482,0.2) ;
#25651 = CIRCLE('',#69483,1.65) ;
#25652 = CIRCLE('',#69484,0.2) ;
#25653 = CIRCLE('',#69485,2.9) ;
#25654 = CIRCLE('',#69486,0.2) ;
#25655 = CIRCLE('',#69487,1.65) ;
#25656 = CIRCLE('',#69489,0.2) ;
#25657 = CIRCLE('',#69490,0.2) ;
#25658 = CIRCLE('',#69492,0.2) ;
#25659 = CIRCLE('',#69493,0.2) ;
#25660 = CIRCLE('',#69495,0.2) ;
#25661 = CIRCLE('',#69497,0.2) ;
#25662 = CIRCLE('',#69505,0.1) ;
#25663 = CIRCLE('',#69506,0.1) ;
#25664 = CIRCLE('',#69507,0.0999999999999998) ;
#25665 = CIRCLE('',#69508,0.0999999999999998) ;
#25666 = CIRCLE('',#69510,0.2) ;
#25667 = CIRCLE('',#69511,1.85) ;
#25668 = CIRCLE('',#69512,2.9) ;
#25669 = CIRCLE('',#69516,1.75) ;
#25670 = CIRCLE('',#69517,1.75) ;
#25671 = CIRCLE('',#69519,1.75) ;
#25672 = CIRCLE('',#69520,1.75) ;
#25673 = CIRCLE('',#69524,1.85) ;
#25674 = CIRCLE('',#69525,0.2) ;
#25675 = CIRCLE('',#69526,2.9) ;
#25676 = CIRCLE('',#69528,1.85) ;
#25677 = CIRCLE('',#69531,1.75) ;
#25678 = CIRCLE('',#69532,1.75) ;
#25679 = CIRCLE('',#69535,1.75) ;
#25680 = CIRCLE('',#69536,1.75) ;
#25681 = CIRCLE('',#69540,1.85) ;
#25682 = CIRCLE('',#69555,1.1) ;
#25683 = CIRCLE('',#69556,1.9) ;
#25684 = CIRCLE('',#69558,1.9) ;
#25685 = CIRCLE('',#69559,1.1) ;
#25686 = CIRCLE('',#69561,2.) ;
#25687 = CIRCLE('',#69562,2.) ;
#25688 = CIRCLE('',#69569,1.) ;
#25689 = CIRCLE('',#69570,1.) ;
#25690 = CIRCLE('',#69576,609.695407951934) ;
#25691 = CIRCLE('',#69578,3.23607331645511) ;
#25692 = CIRCLE('',#69579,576.383429245353) ;
#25693 = CIRCLE('',#69580,576.383429191305) ;
#25694 = CIRCLE('',#69582,609.695408159653) ;
#25695 = CIRCLE('',#69584,0.1) ;
#25696 = CIRCLE('',#69586,0.0999999999999999) ;
#25697 = CIRCLE('',#69587,0.0999999999999998) ;
#25698 = CIRCLE('',#69589,0.1) ;
#25699 = CIRCLE('',#69591,0.1) ;
#25700 = CIRCLE('',#69593,0.1) ;
#25701 = CIRCLE('',#69595,0.0999999999999999) ;
#25702 = CIRCLE('',#69597,0.1) ;
#25703 = CIRCLE('',#69598,0.1) ;
#25704 = CIRCLE('',#69600,0.1) ;
#25705 = CIRCLE('',#69602,0.1) ;
#25706 = CIRCLE('',#69603,0.1) ;
#25707 = CIRCLE('',#69605,0.1) ;
#25708 = CIRCLE('',#69607,0.1) ;
#25709 = CIRCLE('',#69609,0.1) ;
#25710 = CIRCLE('',#69611,0.1) ;
#25711 = CIRCLE('',#69613,0.1) ;
#25712 = CIRCLE('',#69615,0.1) ;
#25713 = CIRCLE('',#69617,0.1) ;
#25714 = CIRCLE('',#69619,0.1) ;
#25715 = CIRCLE('',#69621,0.1) ;
#25716 = CIRCLE('',#69623,0.1) ;
#25717 = CIRCLE('',#69625,0.1) ;
#25718 = CIRCLE('',#69626,0.1) ;
#25719 = CIRCLE('',#69628,0.1) ;
#25720 = CIRCLE('',#69630,0.1) ;
#25721 = CIRCLE('',#69632,0.1) ;
#25722 = CIRCLE('',#69634,0.1) ;
#25723 = CIRCLE('',#69636,0.1) ;
#25724 = CIRCLE('',#69638,0.1) ;
#25725 = CIRCLE('',#69640,0.1) ;
#25726 = CIRCLE('',#69642,0.1) ;
#25727 = CIRCLE('',#69644,0.1) ;
#25728 = CIRCLE('',#69646,0.1) ;
#25729 = CIRCLE('',#69648,0.1) ;
#25730 = CIRCLE('',#69650,0.1) ;
#25731 = CIRCLE('',#69653,0.1) ;
#25732 = CIRCLE('',#69654,0.1) ;
#25733 = CIRCLE('',#69655,0.1) ;
#25734 = CIRCLE('',#69661,0.1) ;
#25735 = CIRCLE('',#69669,0.1) ;
#25736 = CIRCLE('',#69670,0.1) ;
#25737 = CIRCLE('',#69672,0.1) ;
#25738 = CIRCLE('',#69674,0.1) ;
#25739 = CIRCLE('',#69675,0.1) ;
#25740 = CIRCLE('',#69678,0.1) ;
#25741 = CIRCLE('',#69681,0.1) ;
#25742 = CIRCLE('',#69683,0.1) ;
#25743 = CIRCLE('',#69686,0.1) ;
#25744 = CIRCLE('',#69688,0.1) ;
#25745 = CIRCLE('',#69690,0.1) ;
#25746 = CIRCLE('',#69692,0.1) ;
#25747 = CIRCLE('',#69694,0.1) ;
#25748 = CIRCLE('',#69695,0.1) ;
#25749 = CIRCLE('',#69697,0.1) ;
#25750 = CIRCLE('',#69699,0.1) ;
#25751 = CIRCLE('',#69701,0.0999999999999998) ;
#25752 = CIRCLE('',#69702,0.1) ;
#25753 = CIRCLE('',#69704,0.1) ;
#25754 = CIRCLE('',#69706,0.1) ;
#25755 = CIRCLE('',#69708,0.1) ;
#25756 = CIRCLE('',#69710,0.0999999999999998) ;
#25757 = CIRCLE('',#69712,0.0999999999999998) ;
#25758 = CIRCLE('',#69714,0.0999999999999998) ;
#25759 = CIRCLE('',#69716,0.0999999999999998) ;
#25760 = CIRCLE('',#69717,0.0999999999999998) ;
#25761 = CIRCLE('',#69719,0.1) ;
#25762 = CIRCLE('',#69724,0.0999999999999998) ;
#25763 = CIRCLE('',#69727,0.0999999999999998) ;
#25764 = CIRCLE('',#69729,0.1) ;
#25765 = CIRCLE('',#69730,0.1) ;
#25766 = CIRCLE('',#69732,0.1) ;
#25767 = CIRCLE('',#69734,0.0999999999999998) ;
#25768 = CIRCLE('',#69736,0.1) ;
#25769 = CIRCLE('',#69738,0.1) ;
#25770 = CIRCLE('',#69740,0.1) ;
#25771 = CIRCLE('',#69741,0.1) ;
#25772 = CIRCLE('',#69743,0.1) ;
#25773 = CIRCLE('',#69745,0.1) ;
#25774 = CIRCLE('',#69746,0.1) ;
#25775 = CIRCLE('',#69748,0.0999999999999999) ;
#25776 = CIRCLE('',#69750,0.0999999999999999) ;
#25777 = CIRCLE('',#69752,0.0999999999999998) ;
#25778 = CIRCLE('',#69754,0.1) ;
#25779 = CIRCLE('',#69756,0.1) ;
#25780 = CIRCLE('',#69758,0.1) ;
#25781 = CIRCLE('',#69759,0.1) ;
#25782 = CIRCLE('',#69761,0.1) ;
#25783 = CIRCLE('',#69763,0.1) ;
#25784 = CIRCLE('',#69765,0.1) ;
#25785 = CIRCLE('',#69768,0.1) ;
#25786 = CIRCLE('',#69770,0.0999999999999998) ;
#25787 = CIRCLE('',#69771,0.1) ;
#25788 = CIRCLE('',#69774,0.1) ;
#25789 = CIRCLE('',#69776,0.1) ;
#25790 = CIRCLE('',#69777,0.1) ;
#25791 = CIRCLE('',#69779,0.0999999999999999) ;
#25792 = CIRCLE('',#69781,0.0999999999999998) ;
#25793 = CIRCLE('',#69783,0.1) ;
#25794 = CIRCLE('',#69784,0.1) ;
#25795 = CIRCLE('',#69786,0.1) ;
#25796 = CIRCLE('',#69788,0.1) ;
#25797 = CIRCLE('',#69790,0.0999999999999999) ;
#25798 = CIRCLE('',#69792,0.1) ;
#25799 = CIRCLE('',#69794,0.0999999999999998) ;
#25800 = CIRCLE('',#69796,0.0999999999999999) ;
#25801 = CIRCLE('',#69798,0.1) ;
#25802 = CIRCLE('',#69801,0.1) ;
#25803 = CIRCLE('',#69803,0.1) ;
#25804 = CIRCLE('',#69805,0.1) ;
#25805 = CIRCLE('',#69807,0.1) ;
#25806 = CIRCLE('',#69808,0.1) ;
#25807 = CIRCLE('',#69810,0.1) ;
#25808 = CIRCLE('',#69812,0.1) ;
#25809 = CIRCLE('',#69814,0.1) ;
#25810 = CIRCLE('',#69815,0.0999999999999998) ;
#25811 = CIRCLE('',#69817,0.1) ;
#25812 = CIRCLE('',#69819,0.1) ;
#25813 = CIRCLE('',#69820,0.1) ;
#25814 = CIRCLE('',#69822,0.1) ;
#25815 = CIRCLE('',#69824,0.0999999999999998) ;
#25816 = CIRCLE('',#69826,0.1) ;
#25817 = CIRCLE('',#69827,0.1) ;
#25818 = CIRCLE('',#69829,0.0999999999999998) ;
#25819 = CIRCLE('',#69831,0.1) ;
#25820 = CIRCLE('',#69833,0.1) ;
#25821 = CIRCLE('',#69835,0.0999999999999998) ;
#25822 = CIRCLE('',#69837,0.1) ;
#25823 = CIRCLE('',#69839,0.1) ;
#25824 = CIRCLE('',#69841,0.1) ;
#25825 = CIRCLE('',#69842,0.1) ;
#25826 = CIRCLE('',#69845,0.0999999999999998) ;
#25827 = CIRCLE('',#69847,0.1) ;
#25828 = CIRCLE('',#69849,0.1) ;
#25829 = CIRCLE('',#69850,0.1) ;
#25830 = CIRCLE('',#69852,0.1) ;
#25831 = CIRCLE('',#69853,0.0999999999999998) ;
#25832 = CIRCLE('',#69855,0.0999999999999994) ;
#25833 = CIRCLE('',#69856,0.1) ;
#25834 = CIRCLE('',#69858,0.0999999999999998) ;
#25835 = CIRCLE('',#69860,0.0999999999999998) ;
#25836 = CIRCLE('',#69862,0.1) ;
#25837 = CIRCLE('',#69864,0.0999999999999994) ;
#25838 = CIRCLE('',#69866,0.0999999999999994) ;
#25839 = CIRCLE('',#69868,0.1) ;
#25840 = CIRCLE('',#69869,0.1) ;
#25841 = CIRCLE('',#69871,0.1) ;
#25842 = CIRCLE('',#69872,0.1) ;
#25843 = CIRCLE('',#69874,0.0999999999999998) ;
#25844 = CIRCLE('',#69876,0.1) ;
#25845 = CIRCLE('',#69878,0.0999999999999994) ;
#25846 = CIRCLE('',#69881,0.0999999999999994) ;
#25847 = CIRCLE('',#69883,0.1) ;
#25848 = CIRCLE('',#69885,0.1) ;
#25849 = CIRCLE('',#69887,0.1) ;
#25850 = CIRCLE('',#69889,0.0999999999999994) ;
#25851 = CIRCLE('',#69891,0.0999999999999998) ;
#25852 = CIRCLE('',#69895,0.1) ;
#25853 = CIRCLE('',#69897,0.1) ;
#25854 = CIRCLE('',#69899,0.0999999999999994) ;
#25855 = CIRCLE('',#69901,0.1) ;
#25856 = CIRCLE('',#69903,0.0999999999999994) ;
#25857 = CIRCLE('',#69905,0.100000000000001) ;
#25858 = CIRCLE('',#69909,0.1) ;
#25859 = CIRCLE('',#69910,0.1) ;
#25860 = CIRCLE('',#69916,0.0999999999999994) ;
#25861 = CIRCLE('',#69918,0.1) ;
#25862 = CIRCLE('',#69919,0.0999999999999997) ;
#25863 = CIRCLE('',#69921,0.0999999999999994) ;
#25864 = CIRCLE('',#69922,0.1) ;
#25865 = CIRCLE('',#69924,0.1) ;
#25866 = CIRCLE('',#69926,0.1) ;
#25867 = CIRCLE('',#69928,0.1) ;
#25868 = CIRCLE('',#69929,0.1) ;
#25869 = CIRCLE('',#69931,0.1) ;
#25870 = CIRCLE('',#69933,0.1) ;
#25871 = CIRCLE('',#69935,0.1) ;
#25872 = CIRCLE('',#69936,0.1) ;
#25873 = CIRCLE('',#69938,0.1) ;
#25874 = CIRCLE('',#69941,0.0999999999999994) ;
#25875 = CIRCLE('',#69943,0.0999999999999994) ;
#25876 = CIRCLE('',#69947,0.1) ;
#25877 = CIRCLE('',#69949,0.0999999999999994) ;
#25878 = CIRCLE('',#69951,0.0999999999999999) ;
#25879 = CIRCLE('',#69952,0.1) ;
#25880 = CIRCLE('',#69955,0.1) ;
#25881 = CIRCLE('',#69956,0.0999999999999998) ;
#25882 = CIRCLE('',#69958,0.1) ;
#25883 = CIRCLE('',#69960,0.1) ;
#25884 = CIRCLE('',#69962,0.0999999999999998) ;
#25885 = CIRCLE('',#69964,0.1) ;
#25886 = CIRCLE('',#69966,0.1) ;
#25887 = CIRCLE('',#69968,0.1) ;
#25888 = CIRCLE('',#69971,0.0999999999999994) ;
#25889 = CIRCLE('',#69972,0.1) ;
#25890 = CIRCLE('',#69974,0.0999999999999994) ;
#25891 = CIRCLE('',#69976,0.1) ;
#25892 = CIRCLE('',#69978,0.1) ;
#25893 = CIRCLE('',#69980,0.1) ;
#25894 = CIRCLE('',#69982,0.1) ;
#25895 = CIRCLE('',#69984,0.0999999999999994) ;
#25896 = CIRCLE('',#69987,0.0999999999999994) ;
#25897 = CIRCLE('',#69989,0.0999999999999999) ;
#25898 = CIRCLE('',#69990,0.0999999999999999) ;
#25899 = CIRCLE('',#69994,0.0999999999999994) ;
#25900 = CIRCLE('',#69996,0.0999999999999994) ;
#25901 = CIRCLE('',#70000,0.1) ;
#25902 = CIRCLE('',#70002,0.0999999999999997) ;
#25903 = CIRCLE('',#70004,0.0999999999999994) ;
#25904 = CIRCLE('',#70007,1.4) ;
#25905 = CIRCLE('',#70008,0.1) ;
#25906 = CIRCLE('',#70009,1.5) ;
#25907 = CIRCLE('',#70011,1.5) ;
#25908 = CIRCLE('',#70012,0.1) ;
#25909 = CIRCLE('',#70013,1.6) ;
#25910 = CIRCLE('',#70015,0.0999999999999994) ;
#25911 = CIRCLE('',#70016,0.0999999999999994) ;
#25912 = CIRCLE('',#70017,0.0999999999999994) ;
#25913 = CIRCLE('',#70019,0.0999999999999994) ;
#25914 = CIRCLE('',#70020,0.1) ;
#25915 = CIRCLE('',#70022,3.) ;
#25916 = CIRCLE('',#70023,0.1) ;
#25917 = CIRCLE('',#70024,3.00136060761679) ;
#25918 = CIRCLE('',#70025,0.1) ;
#25919 = CIRCLE('',#70028,3.) ;
#25920 = CIRCLE('',#70029,3.) ;
#25921 = CIRCLE('',#70030,3.) ;
#25922 = CIRCLE('',#70039,3.33471270883832) ;
#25923 = CIRCLE('',#70041,0.0999999999999994) ;
#25924 = CIRCLE('',#70042,0.0999999999999994) ;
#25925 = CIRCLE('',#70043,0.0999999999999994) ;
#25926 = CIRCLE('',#70044,0.0999999999999994) ;
#25927 = CIRCLE('',#70045,0.1) ;
#25928 = CIRCLE('',#70046,0.1) ;
#25929 = CIRCLE('',#70047,0.1) ;
#25930 = CIRCLE('',#70048,0.1) ;
#25931 = CIRCLE('',#70049,0.1) ;
#25932 = CIRCLE('',#70050,0.1) ;
#25933 = CIRCLE('',#70051,0.0999999999999994) ;
#25934 = CIRCLE('',#70052,0.0999999999999994) ;
#25935 = CIRCLE('',#70053,0.0999999999999994) ;
#25936 = CIRCLE('',#70054,0.1) ;
#25937 = CIRCLE('',#70055,0.1) ;
#25938 = CIRCLE('',#70056,0.1) ;
#25939 = CIRCLE('',#70058,0.0999999999999994) ;
#25940 = CIRCLE('',#70059,0.1) ;
#25941 = CIRCLE('',#70060,0.1) ;
#25942 = CIRCLE('',#70061,0.1) ;
#25943 = CIRCLE('',#70062,0.0999999999999994) ;
#25944 = CIRCLE('',#70063,0.0999999999999994) ;
#25945 = CIRCLE('',#70064,0.0999999999999994) ;
#25946 = CIRCLE('',#70065,0.1) ;
#25947 = CIRCLE('',#70066,0.1) ;
#25948 = CIRCLE('',#70067,0.1) ;
#25949 = CIRCLE('',#70068,0.1) ;
#25950 = CIRCLE('',#70069,0.1) ;
#25951 = CIRCLE('',#70070,0.1) ;
#25952 = CIRCLE('',#70071,0.0999999999999994) ;
#25953 = CIRCLE('',#70072,0.0999999999999994) ;
#25954 = CIRCLE('',#70073,0.0999999999999994) ;
#25955 = CIRCLE('',#70082,0.200000000000001) ;
#25956 = CIRCLE('',#70083,0.200000000000001) ;
#25957 = CIRCLE('',#70085,0.2) ;
#25958 = CIRCLE('',#70086,0.2) ;
#25959 = CIRCLE('',#70087,1.65) ;
#25960 = CIRCLE('',#70088,0.2) ;
#25961 = CIRCLE('',#70089,0.2) ;
#25962 = CIRCLE('',#70090,1.65) ;
#25963 = CIRCLE('',#70091,0.2) ;
#25964 = CIRCLE('',#70092,0.2) ;
#25965 = CIRCLE('',#70093,1.65) ;
#25966 = CIRCLE('',#70094,0.2) ;
#25967 = CIRCLE('',#70095,2.9) ;
#25968 = CIRCLE('',#70096,0.2) ;
#25969 = CIRCLE('',#70097,1.65) ;
#25970 = CIRCLE('',#70099,0.200000000000001) ;
#25971 = CIRCLE('',#70100,0.200000000000001) ;
#25972 = CIRCLE('',#70102,0.2) ;
#25973 = CIRCLE('',#70103,0.2) ;
#25974 = CIRCLE('',#70105,0.2) ;
#25975 = CIRCLE('',#70107,0.2) ;
#25976 = CIRCLE('',#70115,0.1) ;
#25977 = CIRCLE('',#70116,0.1) ;
#25978 = CIRCLE('',#70117,0.0999999999999998) ;
#25979 = CIRCLE('',#70118,0.0999999999999998) ;
#25980 = CIRCLE('',#70120,0.2) ;
#25981 = CIRCLE('',#70121,1.85) ;
#25982 = CIRCLE('',#70122,2.9) ;
#25983 = CIRCLE('',#70126,1.75) ;
#25984 = CIRCLE('',#70127,1.75) ;
#25985 = CIRCLE('',#70129,1.75) ;
#25986 = CIRCLE('',#70130,1.75) ;
#25987 = CIRCLE('',#70134,1.85) ;
#25988 = CIRCLE('',#70135,0.2) ;
#25989 = CIRCLE('',#70136,2.9) ;
#25990 = CIRCLE('',#70138,1.85) ;
#25991 = CIRCLE('',#70141,1.75) ;
#25992 = CIRCLE('',#70142,1.75) ;
#25993 = CIRCLE('',#70145,1.75) ;
#25994 = CIRCLE('',#70146,1.75) ;
#25995 = CIRCLE('',#70150,1.85) ;
#25996 = CIRCLE('',#70165,1.1) ;
#25997 = CIRCLE('',#70166,1.9) ;
#25998 = CIRCLE('',#70168,1.9) ;
#25999 = CIRCLE('',#70169,1.1) ;
#26000 = CIRCLE('',#70171,2.) ;
#26001 = CIRCLE('',#70172,2.) ;
#26002 = CIRCLE('',#70179,1.) ;
#26003 = CIRCLE('',#70180,1.) ;
#26004 = CIRCLE('',#70186,609.695408627795) ;
#26005 = CIRCLE('',#70188,3.23607331645511) ;
#26006 = CIRCLE('',#70189,576.383428977096) ;
#26007 = CIRCLE('',#70190,576.383429600196) ;
#26008 = CIRCLE('',#70192,609.695407714902) ;
#26009 = CIRCLE('',#70194,0.1) ;
#26010 = CIRCLE('',#70196,0.0999999999999995) ;
#26011 = CIRCLE('',#70197,0.0999999999999994) ;
#26012 = CIRCLE('',#70199,0.1) ;
#26013 = CIRCLE('',#70201,0.1) ;
#26014 = CIRCLE('',#70203,0.0999999999999999) ;
#26015 = CIRCLE('',#70205,0.0999999999999995) ;
#26016 = CIRCLE('',#70207,0.0999999999999994) ;
#26017 = CIRCLE('',#70208,0.0999999999999994) ;
#26018 = CIRCLE('',#70210,0.1) ;
#26019 = CIRCLE('',#70212,0.1) ;
#26020 = CIRCLE('',#70213,0.0999999999999994) ;
#26021 = CIRCLE('',#70215,0.1) ;
#26022 = CIRCLE('',#70217,0.0999999999999999) ;
#26023 = CIRCLE('',#70219,0.1) ;
#26024 = CIRCLE('',#70221,0.0999999999999994) ;
#26025 = CIRCLE('',#70223,0.1) ;
#26026 = CIRCLE('',#70225,0.0999999999999995) ;
#26027 = CIRCLE('',#70227,0.0999999999999995) ;
#26028 = CIRCLE('',#70229,0.0999999999999994) ;
#26029 = CIRCLE('',#70231,0.0999999999999994) ;
#26030 = CIRCLE('',#70233,0.0999999999999999) ;
#26031 = CIRCLE('',#70235,0.1) ;
#26032 = CIRCLE('',#70236,0.0999999999999994) ;
#26033 = CIRCLE('',#70238,0.0999999999999999) ;
#26034 = CIRCLE('',#70240,0.0999999999999994) ;
#26035 = CIRCLE('',#70242,0.0999999999999994) ;
#26036 = CIRCLE('',#70244,0.0999999999999994) ;
#26037 = CIRCLE('',#70246,0.0999999999999994) ;
#26038 = CIRCLE('',#70248,0.1) ;
#26039 = CIRCLE('',#70250,0.1) ;
#26040 = CIRCLE('',#70252,0.0999999999999994) ;
#26041 = CIRCLE('',#70254,0.0999999999999994) ;
#26042 = CIRCLE('',#70256,0.1) ;
#26043 = CIRCLE('',#70258,0.0999999999999994) ;
#26044 = CIRCLE('',#70260,0.0999999999999994) ;
#26045 = CIRCLE('',#70263,0.1) ;
#26046 = CIRCLE('',#70264,0.0999999999999994) ;
#26047 = CIRCLE('',#70265,0.1) ;
#26048 = CIRCLE('',#70271,0.1) ;
#26049 = CIRCLE('',#70279,0.0999999999999994) ;
#26050 = CIRCLE('',#70280,0.0999999999999994) ;
#26051 = CIRCLE('',#70282,0.0999999999999994) ;
#26052 = CIRCLE('',#70284,0.0999999999999994) ;
#26053 = CIRCLE('',#70285,0.1) ;
#26054 = CIRCLE('',#70288,0.0999999999999994) ;
#26055 = CIRCLE('',#70291,0.0999999999999994) ;
#26056 = CIRCLE('',#70293,0.0999999999999994) ;
#26057 = CIRCLE('',#70296,0.0999999999999994) ;
#26058 = CIRCLE('',#70298,0.1) ;
#26059 = CIRCLE('',#70300,0.1) ;
#26060 = CIRCLE('',#70302,0.1) ;
#26061 = CIRCLE('',#70304,0.0999999999999994) ;
#26062 = CIRCLE('',#70305,0.1) ;
#26063 = CIRCLE('',#70307,0.0999999999999994) ;
#26064 = CIRCLE('',#70309,0.1) ;
#26065 = CIRCLE('',#70311,0.0999999999999994) ;
#26066 = CIRCLE('',#70312,0.1) ;
#26067 = CIRCLE('',#70314,0.1) ;
#26068 = CIRCLE('',#70316,0.1) ;
#26069 = CIRCLE('',#70318,0.1) ;
#26070 = CIRCLE('',#70320,0.0999999999999994) ;
#26071 = CIRCLE('',#70322,0.0999999999999994) ;
#26072 = CIRCLE('',#70324,0.0999999999999994) ;
#26073 = CIRCLE('',#70326,0.0999999999999994) ;
#26074 = CIRCLE('',#70327,0.0999999999999994) ;
#26075 = CIRCLE('',#70329,0.1) ;
#26076 = CIRCLE('',#70334,0.0999999999999994) ;
#26077 = CIRCLE('',#70337,0.0999999999999998) ;
#26078 = CIRCLE('',#70339,0.0999999999999995) ;
#26079 = CIRCLE('',#70340,0.0999999999999994) ;
#26080 = CIRCLE('',#70342,0.1) ;
#26081 = CIRCLE('',#70344,0.0999999999999998) ;
#26082 = CIRCLE('',#70346,0.0999999999999999) ;
#26083 = CIRCLE('',#70348,0.1) ;
#26084 = CIRCLE('',#70350,0.1) ;
#26085 = CIRCLE('',#70351,0.1) ;
#26086 = CIRCLE('',#70353,0.0999999999999995) ;
#26087 = CIRCLE('',#70355,0.0999999999999994) ;
#26088 = CIRCLE('',#70356,0.0999999999999994) ;
#26089 = CIRCLE('',#70358,0.0999999999999999) ;
#26090 = CIRCLE('',#70360,0.0999999999999995) ;
#26091 = CIRCLE('',#70362,0.0999999999999998) ;
#26092 = CIRCLE('',#70364,0.0999999999999994) ;
#26093 = CIRCLE('',#70366,0.1) ;
#26094 = CIRCLE('',#70368,0.1) ;
#26095 = CIRCLE('',#70369,0.1) ;
#26096 = CIRCLE('',#70371,0.1) ;
#26097 = CIRCLE('',#70373,0.1) ;
#26098 = CIRCLE('',#70375,0.0999999999999994) ;
#26099 = CIRCLE('',#70378,0.0999999999999999) ;
#26100 = CIRCLE('',#70380,0.0999999999999994) ;
#26101 = CIRCLE('',#70381,0.0999999999999993) ;
#26102 = CIRCLE('',#70384,0.1) ;
#26103 = CIRCLE('',#70386,0.0999999999999994) ;
#26104 = CIRCLE('',#70387,0.0999999999999994) ;
#26105 = CIRCLE('',#70389,0.0999999999999995) ;
#26106 = CIRCLE('',#70391,0.0999999999999998) ;
#26107 = CIRCLE('',#70393,0.1) ;
#26108 = CIRCLE('',#70394,0.1) ;
#26109 = CIRCLE('',#70396,0.1) ;
#26110 = CIRCLE('',#70398,0.0999999999999994) ;
#26111 = CIRCLE('',#70400,0.0999999999999995) ;
#26112 = CIRCLE('',#70402,0.1) ;
#26113 = CIRCLE('',#70404,0.0999999999999998) ;
#26114 = CIRCLE('',#70406,0.0999999999999995) ;
#26115 = CIRCLE('',#70408,0.0999999999999994) ;
#26116 = CIRCLE('',#70411,0.0999999999999994) ;
#26117 = CIRCLE('',#70413,0.0999999999999994) ;
#26118 = CIRCLE('',#70415,0.1) ;
#26119 = CIRCLE('',#70417,0.1) ;
#26120 = CIRCLE('',#70418,0.0999999999999995) ;
#26121 = CIRCLE('',#70420,0.0999999999999994) ;
#26122 = CIRCLE('',#70422,0.0999999999999994) ;
#26123 = CIRCLE('',#70424,0.1) ;
#26124 = CIRCLE('',#70425,0.0999999999999998) ;
#26125 = CIRCLE('',#70427,0.0999999999999994) ;
#26126 = CIRCLE('',#70429,0.1) ;
#26127 = CIRCLE('',#70430,0.1) ;
#26128 = CIRCLE('',#70432,0.0999999999999994) ;
#26129 = CIRCLE('',#70434,0.0999999999999998) ;
#26130 = CIRCLE('',#70436,0.1) ;
#26131 = CIRCLE('',#70437,0.1) ;
#26132 = CIRCLE('',#70439,0.0999999999999998) ;
#26133 = CIRCLE('',#70441,0.0999999999999994) ;
#26134 = CIRCLE('',#70443,0.1) ;
#26135 = CIRCLE('',#70445,0.0999999999999998) ;
#26136 = CIRCLE('',#70447,0.100000000000001) ;
#26137 = CIRCLE('',#70449,0.1) ;
#26138 = CIRCLE('',#70451,0.0999999999999994) ;
#26139 = CIRCLE('',#70452,0.1) ;
#26140 = CIRCLE('',#70455,0.0999999999999998) ;
#26141 = CIRCLE('',#70457,0.1) ;
#26142 = CIRCLE('',#70459,0.1) ;
#26143 = CIRCLE('',#70460,0.0999999999999995) ;
#26144 = CIRCLE('',#70462,0.0999999999999995) ;
#26145 = CIRCLE('',#70463,0.0999999999999998) ;
#26146 = CIRCLE('',#70465,0.0999999999999994) ;
#26147 = CIRCLE('',#70466,0.0999999999999994) ;
#26148 = CIRCLE('',#70468,0.0999999999999998) ;
#26149 = CIRCLE('',#70470,0.0999999999999998) ;
#26150 = CIRCLE('',#70472,0.1) ;
#26151 = CIRCLE('',#70474,0.0999999999999994) ;
#26152 = CIRCLE('',#70476,0.0999999999999994) ;
#26153 = CIRCLE('',#70478,0.1) ;
#26154 = CIRCLE('',#70479,0.0999999999999995) ;
#26155 = CIRCLE('',#70481,0.1) ;
#26156 = CIRCLE('',#70482,0.0999999999999995) ;
#26157 = CIRCLE('',#70484,0.0999999999999998) ;
#26158 = CIRCLE('',#70486,0.0999999999999994) ;
#26159 = CIRCLE('',#70488,0.0999999999999994) ;
#26160 = CIRCLE('',#70491,0.0999999999999994) ;
#26161 = CIRCLE('',#70493,0.0999999999999995) ;
#26162 = CIRCLE('',#70495,0.0999999999999994) ;
#26163 = CIRCLE('',#70497,0.1) ;
#26164 = CIRCLE('',#70499,0.0999999999999994) ;
#26165 = CIRCLE('',#70501,0.0999999999999998) ;
#26166 = CIRCLE('',#70505,0.0999999999999995) ;
#26167 = CIRCLE('',#70507,0.1) ;
#26168 = CIRCLE('',#70509,0.0999999999999994) ;
#26169 = CIRCLE('',#70511,0.0999999999999994) ;
#26170 = CIRCLE('',#70513,0.0999999999999994) ;
#26171 = CIRCLE('',#70515,0.100000000000001) ;
#26172 = CIRCLE('',#70519,0.1) ;
#26173 = CIRCLE('',#70520,0.1) ;
#26174 = CIRCLE('',#70526,0.0999999999999994) ;
#26175 = CIRCLE('',#70528,0.1) ;
#26176 = CIRCLE('',#70529,0.1) ;
#26177 = CIRCLE('',#70531,0.0999999999999994) ;
#26178 = CIRCLE('',#70532,0.1) ;
#26179 = CIRCLE('',#70534,0.0999999999999994) ;
#26180 = CIRCLE('',#70536,0.0999999999999994) ;
#26181 = CIRCLE('',#70538,0.0999999999999994) ;
#26182 = CIRCLE('',#70539,0.0999999999999994) ;
#26183 = CIRCLE('',#70541,0.0999999999999994) ;
#26184 = CIRCLE('',#70543,0.0999999999999994) ;
#26185 = CIRCLE('',#70545,0.1) ;
#26186 = CIRCLE('',#70546,0.0999999999999994) ;
#26187 = CIRCLE('',#70548,0.0999999999999994) ;
#26188 = CIRCLE('',#70551,0.0999999999999994) ;
#26189 = CIRCLE('',#70553,0.0999999999999994) ;
#26190 = CIRCLE('',#70557,0.0999999999999994) ;
#26191 = CIRCLE('',#70559,0.0999999999999994) ;
#26192 = CIRCLE('',#70561,0.0999999999999999) ;
#26193 = CIRCLE('',#70562,0.1) ;
#26194 = CIRCLE('',#70565,0.1) ;
#26195 = CIRCLE('',#70566,0.0999999999999998) ;
#26196 = CIRCLE('',#70568,0.1) ;
#26197 = CIRCLE('',#70570,0.0999999999999994) ;
#26198 = CIRCLE('',#70572,0.0999999999999998) ;
#26199 = CIRCLE('',#70574,0.1) ;
#26200 = CIRCLE('',#70576,0.0999999999999994) ;
#26201 = CIRCLE('',#70578,0.1) ;
#26202 = CIRCLE('',#70581,0.0999999999999994) ;
#26203 = CIRCLE('',#70582,0.0999999999999994) ;
#26204 = CIRCLE('',#70584,0.0999999999999994) ;
#26205 = CIRCLE('',#70586,0.0999999999999994) ;
#26206 = CIRCLE('',#70588,0.0999999999999994) ;
#26207 = CIRCLE('',#70590,0.1) ;
#26208 = CIRCLE('',#70592,0.0999999999999994) ;
#26209 = CIRCLE('',#70594,0.0999999999999994) ;
#26210 = CIRCLE('',#70597,0.0999999999999994) ;
#26211 = CIRCLE('',#70599,0.0999999999999999) ;
#26212 = CIRCLE('',#70600,0.0999999999999999) ;
#26213 = CIRCLE('',#70604,0.0999999999999994) ;
#26214 = CIRCLE('',#70606,0.0999999999999994) ;
#26215 = CIRCLE('',#70610,0.1) ;
#26216 = CIRCLE('',#70612,0.0999999999999997) ;
#26217 = CIRCLE('',#70614,0.0999999999999994) ;
#26218 = CIRCLE('',#70617,1.4) ;
#26219 = CIRCLE('',#70618,0.1) ;
#26220 = CIRCLE('',#70619,1.5) ;
#26221 = CIRCLE('',#70621,1.5) ;
#26222 = CIRCLE('',#70622,0.1) ;
#26223 = CIRCLE('',#70623,1.6) ;
#26224 = CIRCLE('',#70625,0.0999999999999994) ;
#26225 = CIRCLE('',#70626,0.0999999999999994) ;
#26226 = CIRCLE('',#70627,0.0999999999999994) ;
#26227 = CIRCLE('',#70629,0.0999999999999994) ;
#26228 = CIRCLE('',#70630,0.1) ;
#26229 = CIRCLE('',#70632,3.) ;
#26230 = CIRCLE('',#70633,0.1) ;
#26231 = CIRCLE('',#70634,3.00136060761679) ;
#26232 = CIRCLE('',#70635,0.100000000000001) ;
#26233 = CIRCLE('',#70638,3.) ;
#26234 = CIRCLE('',#70639,3.) ;
#26235 = CIRCLE('',#70640,3.) ;
#26236 = CIRCLE('',#70649,3.33471270883832) ;
#26237 = CIRCLE('',#70651,0.0999999999999994) ;
#26238 = CIRCLE('',#70652,0.0999999999999994) ;
#26239 = CIRCLE('',#70653,0.0999999999999994) ;
#26240 = CIRCLE('',#70654,0.0999999999999994) ;
#26241 = CIRCLE('',#70655,0.1) ;
#26242 = CIRCLE('',#70656,0.1) ;
#26243 = CIRCLE('',#70657,0.1) ;
#26244 = CIRCLE('',#70658,0.1) ;
#26245 = CIRCLE('',#70659,0.1) ;
#26246 = CIRCLE('',#70660,0.1) ;
#26247 = CIRCLE('',#70661,0.0999999999999994) ;
#26248 = CIRCLE('',#70662,0.0999999999999994) ;
#26249 = CIRCLE('',#70663,0.0999999999999994) ;
#26250 = CIRCLE('',#70664,0.1) ;
#26251 = CIRCLE('',#70665,0.1) ;
#26252 = CIRCLE('',#70666,0.1) ;
#26253 = CIRCLE('',#70668,0.0999999999999994) ;
#26254 = CIRCLE('',#70669,0.1) ;
#26255 = CIRCLE('',#70670,0.1) ;
#26256 = CIRCLE('',#70671,0.1) ;
#26257 = CIRCLE('',#70672,0.0999999999999994) ;
#26258 = CIRCLE('',#70673,0.0999999999999994) ;
#26259 = CIRCLE('',#70674,0.0999999999999994) ;
#26260 = CIRCLE('',#70675,0.1) ;
#26261 = CIRCLE('',#70676,0.1) ;
#26262 = CIRCLE('',#70677,0.1) ;
#26263 = CIRCLE('',#70678,0.1) ;
#26264 = CIRCLE('',#70679,0.1) ;
#26265 = CIRCLE('',#70680,0.1) ;
#26266 = CIRCLE('',#70681,0.0999999999999994) ;
#26267 = CIRCLE('',#70682,0.0999999999999994) ;
#26268 = CIRCLE('',#70683,0.0999999999999994) ;
#26269 = CIRCLE('',#70692,0.200000000000001) ;
#26270 = CIRCLE('',#70693,0.199999999999999) ;
#26271 = CIRCLE('',#70695,0.2) ;
#26272 = CIRCLE('',#70696,0.2) ;
#26273 = CIRCLE('',#70697,1.65) ;
#26274 = CIRCLE('',#70698,0.2) ;
#26275 = CIRCLE('',#70699,0.2) ;
#26276 = CIRCLE('',#70700,1.65) ;
#26277 = CIRCLE('',#70701,0.2) ;
#26278 = CIRCLE('',#70702,0.2) ;
#26279 = CIRCLE('',#70703,1.65) ;
#26280 = CIRCLE('',#70704,0.2) ;
#26281 = CIRCLE('',#70705,2.9) ;
#26282 = CIRCLE('',#70706,0.2) ;
#26283 = CIRCLE('',#70707,1.65) ;
#26284 = CIRCLE('',#70709,0.199999999999999) ;
#26285 = CIRCLE('',#70710,0.200000000000001) ;
#26286 = CIRCLE('',#70712,0.2) ;
#26287 = CIRCLE('',#70713,0.2) ;
#26288 = CIRCLE('',#70715,0.2) ;
#26289 = CIRCLE('',#70717,0.2) ;
#26290 = CIRCLE('',#70725,0.1) ;
#26291 = CIRCLE('',#70726,0.1) ;
#26292 = CIRCLE('',#70727,0.0999999999999998) ;
#26293 = CIRCLE('',#70728,0.0999999999999998) ;
#26294 = CIRCLE('',#70730,0.2) ;
#26295 = CIRCLE('',#70731,1.85) ;
#26296 = CIRCLE('',#70732,2.9) ;
#26297 = CIRCLE('',#70736,1.75) ;
#26298 = CIRCLE('',#70737,1.75) ;
#26299 = CIRCLE('',#70739,1.75) ;
#26300 = CIRCLE('',#70740,1.75) ;
#26301 = CIRCLE('',#70744,1.85) ;
#26302 = CIRCLE('',#70745,0.2) ;
#26303 = CIRCLE('',#70746,2.9) ;
#26304 = CIRCLE('',#70748,1.85) ;
#26305 = CIRCLE('',#70751,1.75) ;
#26306 = CIRCLE('',#70752,1.75) ;
#26307 = CIRCLE('',#70755,1.75) ;
#26308 = CIRCLE('',#70756,1.75) ;
#26309 = CIRCLE('',#70760,1.85) ;
#26310 = CIRCLE('',#70775,1.1) ;
#26311 = CIRCLE('',#70776,1.9) ;
#26312 = CIRCLE('',#70778,1.9) ;
#26313 = CIRCLE('',#70779,1.1) ;
#26314 = CIRCLE('',#70781,2.) ;
#26315 = CIRCLE('',#70782,2.) ;
#26316 = CIRCLE('',#70789,1.) ;
#26317 = CIRCLE('',#70790,1.) ;
#26318 = CIRCLE('',#70796,609.695408630063) ;
#26319 = CIRCLE('',#70798,3.23607331645511) ;
#26320 = CIRCLE('',#70799,576.383429457373) ;
#26321 = CIRCLE('',#70800,576.38342959882) ;
#26322 = CIRCLE('',#70802,609.695409345007) ;
#26323 = CIRCLE('',#70804,0.1) ;
#26324 = CIRCLE('',#70806,0.0999999999999995) ;
#26325 = CIRCLE('',#70807,0.0999999999999994) ;
#26326 = CIRCLE('',#70809,0.1) ;
#26327 = CIRCLE('',#70811,0.1) ;
#26328 = CIRCLE('',#70813,0.0999999999999999) ;
#26329 = CIRCLE('',#70815,0.0999999999999995) ;
#26330 = CIRCLE('',#70817,0.0999999999999994) ;
#26331 = CIRCLE('',#70818,0.0999999999999994) ;
#26332 = CIRCLE('',#70820,0.1) ;
#26333 = CIRCLE('',#70822,0.1) ;
#26334 = CIRCLE('',#70823,0.0999999999999994) ;
#26335 = CIRCLE('',#70825,0.1) ;
#26336 = CIRCLE('',#70827,0.0999999999999999) ;
#26337 = CIRCLE('',#70829,0.1) ;
#26338 = CIRCLE('',#70831,0.0999999999999994) ;
#26339 = CIRCLE('',#70833,0.1) ;
#26340 = CIRCLE('',#70835,0.0999999999999995) ;
#26341 = CIRCLE('',#70837,0.0999999999999995) ;
#26342 = CIRCLE('',#70839,0.0999999999999994) ;
#26343 = CIRCLE('',#70841,0.0999999999999994) ;
#26344 = CIRCLE('',#70843,0.0999999999999999) ;
#26345 = CIRCLE('',#70845,0.1) ;
#26346 = CIRCLE('',#70846,0.0999999999999994) ;
#26347 = CIRCLE('',#70848,0.0999999999999999) ;
#26348 = CIRCLE('',#70850,0.0999999999999994) ;
#26349 = CIRCLE('',#70852,0.0999999999999994) ;
#26350 = CIRCLE('',#70854,0.0999999999999994) ;
#26351 = CIRCLE('',#70856,0.0999999999999994) ;
#26352 = CIRCLE('',#70858,0.1) ;
#26353 = CIRCLE('',#70860,0.1) ;
#26354 = CIRCLE('',#70862,0.0999999999999994) ;
#26355 = CIRCLE('',#70864,0.0999999999999994) ;
#26356 = CIRCLE('',#70866,0.1) ;
#26357 = CIRCLE('',#70868,0.0999999999999994) ;
#26358 = CIRCLE('',#70870,0.0999999999999994) ;
#26359 = CIRCLE('',#70873,0.1) ;
#26360 = CIRCLE('',#70874,0.0999999999999994) ;
#26361 = CIRCLE('',#70875,0.1) ;
#26362 = CIRCLE('',#70881,0.1) ;
#26363 = CIRCLE('',#70889,0.0999999999999994) ;
#26364 = CIRCLE('',#70890,0.0999999999999994) ;
#26365 = CIRCLE('',#70892,0.0999999999999994) ;
#26366 = CIRCLE('',#70894,0.0999999999999994) ;
#26367 = CIRCLE('',#70895,0.1) ;
#26368 = CIRCLE('',#70898,0.0999999999999994) ;
#26369 = CIRCLE('',#70901,0.0999999999999994) ;
#26370 = CIRCLE('',#70903,0.0999999999999994) ;
#26371 = CIRCLE('',#70906,0.0999999999999994) ;
#26372 = CIRCLE('',#70908,0.1) ;
#26373 = CIRCLE('',#70910,0.1) ;
#26374 = CIRCLE('',#70912,0.1) ;
#26375 = CIRCLE('',#70914,0.0999999999999994) ;
#26376 = CIRCLE('',#70915,0.1) ;
#26377 = CIRCLE('',#70917,0.0999999999999994) ;
#26378 = CIRCLE('',#70919,0.1) ;
#26379 = CIRCLE('',#70921,0.0999999999999994) ;
#26380 = CIRCLE('',#70922,0.1) ;
#26381 = CIRCLE('',#70924,0.1) ;
#26382 = CIRCLE('',#70926,0.1) ;
#26383 = CIRCLE('',#70928,0.1) ;
#26384 = CIRCLE('',#70930,0.0999999999999994) ;
#26385 = CIRCLE('',#70932,0.0999999999999994) ;
#26386 = CIRCLE('',#70934,0.0999999999999994) ;
#26387 = CIRCLE('',#70936,0.0999999999999994) ;
#26388 = CIRCLE('',#70937,0.0999999999999994) ;
#26389 = CIRCLE('',#70939,0.1) ;
#26390 = CIRCLE('',#70944,0.0999999999999994) ;
#26391 = CIRCLE('',#70947,0.0999999999999998) ;
#26392 = CIRCLE('',#70949,0.0999999999999995) ;
#26393 = CIRCLE('',#70950,0.0999999999999994) ;
#26394 = CIRCLE('',#70952,0.1) ;
#26395 = CIRCLE('',#70954,0.0999999999999998) ;
#26396 = CIRCLE('',#70956,0.0999999999999999) ;
#26397 = CIRCLE('',#70958,0.1) ;
#26398 = CIRCLE('',#70960,0.1) ;
#26399 = CIRCLE('',#70961,0.1) ;
#26400 = CIRCLE('',#70963,0.0999999999999995) ;
#26401 = CIRCLE('',#70965,0.0999999999999994) ;
#26402 = CIRCLE('',#70966,0.0999999999999994) ;
#26403 = CIRCLE('',#70968,0.100000000000001) ;
#26404 = CIRCLE('',#70970,0.0999999999999995) ;
#26405 = CIRCLE('',#70972,0.0999999999999998) ;
#26406 = CIRCLE('',#70974,0.0999999999999994) ;
#26407 = CIRCLE('',#70976,0.100000000000001) ;
#26408 = CIRCLE('',#70978,0.1) ;
#26409 = CIRCLE('',#70979,0.1) ;
#26410 = CIRCLE('',#70981,0.1) ;
#26411 = CIRCLE('',#70983,0.1) ;
#26412 = CIRCLE('',#70985,0.0999999999999994) ;
#26413 = CIRCLE('',#70988,0.0999999999999999) ;
#26414 = CIRCLE('',#70990,0.0999999999999994) ;
#26415 = CIRCLE('',#70991,0.0999999999999993) ;
#26416 = CIRCLE('',#70994,0.1) ;
#26417 = CIRCLE('',#70996,0.0999999999999994) ;
#26418 = CIRCLE('',#70997,0.0999999999999994) ;
#26419 = CIRCLE('',#70999,0.0999999999999995) ;
#26420 = CIRCLE('',#71001,0.0999999999999998) ;
#26421 = CIRCLE('',#71003,0.1) ;
#26422 = CIRCLE('',#71004,0.1) ;
#26423 = CIRCLE('',#71006,0.1) ;
#26424 = CIRCLE('',#71008,0.0999999999999994) ;
#26425 = CIRCLE('',#71010,0.0999999999999995) ;
#26426 = CIRCLE('',#71012,0.1) ;
#26427 = CIRCLE('',#71014,0.0999999999999998) ;
#26428 = CIRCLE('',#71016,0.0999999999999995) ;
#26429 = CIRCLE('',#71018,0.0999999999999994) ;
#26430 = CIRCLE('',#71021,0.0999999999999994) ;
#26431 = CIRCLE('',#71023,0.0999999999999994) ;
#26432 = CIRCLE('',#71025,0.1) ;
#26433 = CIRCLE('',#71027,0.1) ;
#26434 = CIRCLE('',#71028,0.0999999999999995) ;
#26435 = CIRCLE('',#71030,0.0999999999999994) ;
#26436 = CIRCLE('',#71032,0.0999999999999994) ;
#26437 = CIRCLE('',#71034,0.1) ;
#26438 = CIRCLE('',#71035,0.0999999999999998) ;
#26439 = CIRCLE('',#71037,0.0999999999999994) ;
#26440 = CIRCLE('',#71039,0.1) ;
#26441 = CIRCLE('',#71040,0.1) ;
#26442 = CIRCLE('',#71042,0.0999999999999994) ;
#26443 = CIRCLE('',#71044,0.0999999999999998) ;
#26444 = CIRCLE('',#71046,0.1) ;
#26445 = CIRCLE('',#71047,0.1) ;
#26446 = CIRCLE('',#71049,0.0999999999999998) ;
#26447 = CIRCLE('',#71051,0.0999999999999994) ;
#26448 = CIRCLE('',#71053,0.1) ;
#26449 = CIRCLE('',#71055,0.0999999999999998) ;
#26450 = CIRCLE('',#71057,0.100000000000001) ;
#26451 = CIRCLE('',#71059,0.1) ;
#26452 = CIRCLE('',#71061,0.0999999999999994) ;
#26453 = CIRCLE('',#71062,0.1) ;
#26454 = CIRCLE('',#71065,0.0999999999999998) ;
#26455 = CIRCLE('',#71067,0.1) ;
#26456 = CIRCLE('',#71069,0.1) ;
#26457 = CIRCLE('',#71070,0.0999999999999995) ;
#26458 = CIRCLE('',#71072,0.1) ;
#26459 = CIRCLE('',#71073,0.0999999999999998) ;
#26460 = CIRCLE('',#71075,0.0999999999999994) ;
#26461 = CIRCLE('',#71076,0.0999999999999994) ;
#26462 = CIRCLE('',#71078,0.0999999999999998) ;
#26463 = CIRCLE('',#71080,0.0999999999999998) ;
#26464 = CIRCLE('',#71082,0.1) ;
#26465 = CIRCLE('',#71084,0.0999999999999994) ;
#26466 = CIRCLE('',#71086,0.0999999999999994) ;
#26467 = CIRCLE('',#71088,0.1) ;
#26468 = CIRCLE('',#71089,0.0999999999999995) ;
#26469 = CIRCLE('',#71091,0.1) ;
#26470 = CIRCLE('',#71092,0.0999999999999995) ;
#26471 = CIRCLE('',#71094,0.0999999999999998) ;
#26472 = CIRCLE('',#71096,0.0999999999999994) ;
#26473 = CIRCLE('',#71098,0.0999999999999994) ;
#26474 = CIRCLE('',#71101,0.0999999999999994) ;
#26475 = CIRCLE('',#71103,0.0999999999999995) ;
#26476 = CIRCLE('',#71105,0.0999999999999994) ;
#26477 = CIRCLE('',#71107,0.1) ;
#26478 = CIRCLE('',#71109,0.0999999999999994) ;
#26479 = CIRCLE('',#71111,0.0999999999999998) ;
#26480 = CIRCLE('',#71115,0.0999999999999995) ;
#26481 = CIRCLE('',#71117,0.1) ;
#26482 = CIRCLE('',#71119,0.0999999999999994) ;
#26483 = CIRCLE('',#71121,0.0999999999999994) ;
#26484 = CIRCLE('',#71123,0.0999999999999994) ;
#26485 = CIRCLE('',#71125,0.100000000000001) ;
#26486 = CIRCLE('',#71129,0.1) ;
#26487 = CIRCLE('',#71130,0.1) ;
#26488 = CIRCLE('',#71136,0.0999999999999994) ;
#26489 = CIRCLE('',#71138,0.1) ;
#26490 = CIRCLE('',#71139,0.1) ;
#26491 = CIRCLE('',#71141,0.0999999999999994) ;
#26492 = CIRCLE('',#71142,0.1) ;
#26493 = CIRCLE('',#71144,0.0999999999999994) ;
#26494 = CIRCLE('',#71146,0.0999999999999994) ;
#26495 = CIRCLE('',#71148,0.0999999999999994) ;
#26496 = CIRCLE('',#71149,0.0999999999999994) ;
#26497 = CIRCLE('',#71151,0.0999999999999994) ;
#26498 = CIRCLE('',#71153,0.0999999999999994) ;
#26499 = CIRCLE('',#71155,0.1) ;
#26500 = CIRCLE('',#71156,0.0999999999999994) ;
#26501 = CIRCLE('',#71158,0.0999999999999994) ;
#26502 = CIRCLE('',#71161,0.0999999999999994) ;
#26503 = CIRCLE('',#71163,0.0999999999999994) ;
#26504 = CIRCLE('',#71167,0.0999999999999994) ;
#26505 = CIRCLE('',#71169,0.0999999999999994) ;
#26506 = CIRCLE('',#71171,0.0999999999999999) ;
#26507 = CIRCLE('',#71172,0.1) ;
#26508 = CIRCLE('',#71175,0.1) ;
#26509 = CIRCLE('',#71176,0.0999999999999998) ;
#26510 = CIRCLE('',#71178,0.1) ;
#26511 = CIRCLE('',#71180,0.0999999999999994) ;
#26512 = CIRCLE('',#71182,0.0999999999999998) ;
#26513 = CIRCLE('',#71184,0.1) ;
#26514 = CIRCLE('',#71186,0.0999999999999994) ;
#26515 = CIRCLE('',#71188,0.1) ;
#26516 = CIRCLE('',#71191,0.0999999999999994) ;
#26517 = CIRCLE('',#71192,0.0999999999999994) ;
#26518 = CIRCLE('',#71194,0.0999999999999994) ;
#26519 = CIRCLE('',#71196,0.0999999999999994) ;
#26520 = CIRCLE('',#71198,0.0999999999999994) ;
#26521 = CIRCLE('',#71200,0.1) ;
#26522 = CIRCLE('',#71202,0.0999999999999994) ;
#26523 = CIRCLE('',#71204,0.0999999999999994) ;
#26524 = CIRCLE('',#71207,0.0999999999999994) ;
#26525 = CIRCLE('',#71209,0.0999999999999999) ;
#26526 = CIRCLE('',#71210,0.0999999999999999) ;
#26527 = CIRCLE('',#71214,0.0999999999999994) ;
#26528 = CIRCLE('',#71216,0.0999999999999994) ;
#26529 = CIRCLE('',#71220,0.100000000000001) ;
#26530 = CIRCLE('',#71222,0.0999999999999997) ;
#26531 = CIRCLE('',#71224,0.0999999999999994) ;
#26532 = CIRCLE('',#71227,1.4) ;
#26533 = CIRCLE('',#71228,0.1) ;
#26534 = CIRCLE('',#71229,1.5) ;
#26535 = CIRCLE('',#71231,1.5) ;
#26536 = CIRCLE('',#71232,0.1) ;
#26537 = CIRCLE('',#71233,1.6) ;
#26538 = CIRCLE('',#71235,0.0999999999999994) ;
#26539 = CIRCLE('',#71236,0.0999999999999994) ;
#26540 = CIRCLE('',#71237,0.0999999999999994) ;
#26541 = CIRCLE('',#71239,0.0999999999999994) ;
#26542 = CIRCLE('',#71240,0.1) ;
#26543 = CIRCLE('',#71242,3.) ;
#26544 = CIRCLE('',#71243,0.100000000000001) ;
#26545 = CIRCLE('',#71244,3.00136060761679) ;
#26546 = CIRCLE('',#71245,0.100000000000001) ;
#26547 = CIRCLE('',#71248,3.) ;
#26548 = CIRCLE('',#71249,3.) ;
#26549 = CIRCLE('',#71250,3.) ;
#26550 = CIRCLE('',#71259,3.33471270883832) ;
#26551 = CIRCLE('',#71261,0.0999999999999994) ;
#26552 = CIRCLE('',#71262,0.0999999999999994) ;
#26553 = CIRCLE('',#71263,0.0999999999999994) ;
#26554 = CIRCLE('',#71264,0.0999999999999994) ;
#26555 = CIRCLE('',#71265,0.1) ;
#26556 = CIRCLE('',#71266,0.1) ;
#26557 = CIRCLE('',#71267,0.1) ;
#26558 = CIRCLE('',#71268,0.1) ;
#26559 = CIRCLE('',#71269,0.1) ;
#26560 = CIRCLE('',#71270,0.1) ;
#26561 = CIRCLE('',#71271,0.0999999999999994) ;
#26562 = CIRCLE('',#71272,0.0999999999999994) ;
#26563 = CIRCLE('',#71273,0.0999999999999994) ;
#26564 = CIRCLE('',#71274,0.1) ;
#26565 = CIRCLE('',#71275,0.1) ;
#26566 = CIRCLE('',#71276,0.1) ;
#26567 = CIRCLE('',#71278,0.0999999999999994) ;
#26568 = CIRCLE('',#71279,0.1) ;
#26569 = CIRCLE('',#71280,0.1) ;
#26570 = CIRCLE('',#71281,0.1) ;
#26571 = CIRCLE('',#71282,0.0999999999999994) ;
#26572 = CIRCLE('',#71283,0.0999999999999994) ;
#26573 = CIRCLE('',#71284,0.0999999999999994) ;
#26574 = CIRCLE('',#71285,0.1) ;
#26575 = CIRCLE('',#71286,0.1) ;
#26576 = CIRCLE('',#71287,0.1) ;
#26577 = CIRCLE('',#71288,0.1) ;
#26578 = CIRCLE('',#71289,0.1) ;
#26579 = CIRCLE('',#71290,0.1) ;
#26580 = CIRCLE('',#71291,0.0999999999999994) ;
#26581 = CIRCLE('',#71292,0.0999999999999994) ;
#26582 = CIRCLE('',#71293,0.0999999999999994) ;
#26583 = CIRCLE('',#71302,0.199999999999999) ;
#26584 = CIRCLE('',#71303,0.199999999999999) ;
#26585 = CIRCLE('',#71305,0.2) ;
#26586 = CIRCLE('',#71306,0.2) ;
#26587 = CIRCLE('',#71307,1.65) ;
#26588 = CIRCLE('',#71308,0.2) ;
#26589 = CIRCLE('',#71309,0.2) ;
#26590 = CIRCLE('',#71310,1.65) ;
#26591 = CIRCLE('',#71311,0.2) ;
#26592 = CIRCLE('',#71312,0.2) ;
#26593 = CIRCLE('',#71313,1.65) ;
#26594 = CIRCLE('',#71314,0.2) ;
#26595 = CIRCLE('',#71315,2.9) ;
#26596 = CIRCLE('',#71316,0.2) ;
#26597 = CIRCLE('',#71317,1.65) ;
#26598 = CIRCLE('',#71319,0.199999999999999) ;
#26599 = CIRCLE('',#71320,0.199999999999999) ;
#26600 = CIRCLE('',#71322,0.2) ;
#26601 = CIRCLE('',#71323,0.2) ;
#26602 = CIRCLE('',#71325,0.2) ;
#26603 = CIRCLE('',#71327,0.2) ;
#26604 = CIRCLE('',#71335,0.1) ;
#26605 = CIRCLE('',#71336,0.1) ;
#26606 = CIRCLE('',#71337,0.0999999999999998) ;
#26607 = CIRCLE('',#71338,0.0999999999999998) ;
#26608 = CIRCLE('',#71340,0.2) ;
#26609 = CIRCLE('',#71341,1.85) ;
#26610 = CIRCLE('',#71342,2.9) ;
#26611 = CIRCLE('',#71346,1.75) ;
#26612 = CIRCLE('',#71347,1.75) ;
#26613 = CIRCLE('',#71349,1.75) ;
#26614 = CIRCLE('',#71350,1.75) ;
#26615 = CIRCLE('',#71354,1.85) ;
#26616 = CIRCLE('',#71355,0.2) ;
#26617 = CIRCLE('',#71356,2.9) ;
#26618 = CIRCLE('',#71358,1.85) ;
#26619 = CIRCLE('',#71361,1.75) ;
#26620 = CIRCLE('',#71362,1.75) ;
#26621 = CIRCLE('',#71365,1.75) ;
#26622 = CIRCLE('',#71366,1.75) ;
#26623 = CIRCLE('',#71370,1.85) ;
#26624 = CIRCLE('',#71385,1.1) ;
#26625 = CIRCLE('',#71386,1.9) ;
#26626 = CIRCLE('',#71388,1.9) ;
#26627 = CIRCLE('',#71389,1.1) ;
#26628 = CIRCLE('',#71391,2.) ;
#26629 = CIRCLE('',#71392,2.) ;
#26630 = CIRCLE('',#71399,1.) ;
#26631 = CIRCLE('',#71400,1.) ;
#26632 = CIRCLE('',#71406,609.695407994444) ;
#26633 = CIRCLE('',#71408,3.23607331645511) ;
#26634 = CIRCLE('',#71409,576.383429460242) ;
#26635 = CIRCLE('',#71410,576.383428783031) ;
#26636 = CIRCLE('',#71412,609.695409343247) ;
#26637 = CIRCLE('',#71414,0.1) ;
#26638 = CIRCLE('',#71416,0.0999999999999995) ;
#26639 = CIRCLE('',#71417,0.0999999999999994) ;
#26640 = CIRCLE('',#71419,0.1) ;
#26641 = CIRCLE('',#71421,0.1) ;
#26642 = CIRCLE('',#71423,0.0999999999999999) ;
#26643 = CIRCLE('',#71425,0.0999999999999995) ;
#26644 = CIRCLE('',#71427,0.0999999999999994) ;
#26645 = CIRCLE('',#71428,0.0999999999999994) ;
#26646 = CIRCLE('',#71430,0.1) ;
#26647 = CIRCLE('',#71432,0.1) ;
#26648 = CIRCLE('',#71433,0.0999999999999994) ;
#26649 = CIRCLE('',#71435,0.1) ;
#26650 = CIRCLE('',#71437,0.0999999999999999) ;
#26651 = CIRCLE('',#71439,0.1) ;
#26652 = CIRCLE('',#71441,0.0999999999999994) ;
#26653 = CIRCLE('',#71443,0.1) ;
#26654 = CIRCLE('',#71445,0.0999999999999995) ;
#26655 = CIRCLE('',#71447,0.0999999999999995) ;
#26656 = CIRCLE('',#71449,0.0999999999999994) ;
#26657 = CIRCLE('',#71451,0.0999999999999994) ;
#26658 = CIRCLE('',#71453,0.0999999999999999) ;
#26659 = CIRCLE('',#71455,0.1) ;
#26660 = CIRCLE('',#71456,0.0999999999999994) ;
#26661 = CIRCLE('',#71458,0.0999999999999999) ;
#26662 = CIRCLE('',#71460,0.0999999999999994) ;
#26663 = CIRCLE('',#71462,0.0999999999999994) ;
#26664 = CIRCLE('',#71464,0.0999999999999994) ;
#26665 = CIRCLE('',#71466,0.0999999999999994) ;
#26666 = CIRCLE('',#71468,0.1) ;
#26667 = CIRCLE('',#71470,0.1) ;
#26668 = CIRCLE('',#71472,0.0999999999999994) ;
#26669 = CIRCLE('',#71474,0.0999999999999994) ;
#26670 = CIRCLE('',#71476,0.1) ;
#26671 = CIRCLE('',#71478,0.0999999999999994) ;
#26672 = CIRCLE('',#71480,0.0999999999999994) ;
#26673 = CIRCLE('',#71483,0.1) ;
#26674 = CIRCLE('',#71484,0.0999999999999994) ;
#26675 = CIRCLE('',#71485,0.1) ;
#26676 = CIRCLE('',#71491,0.1) ;
#26677 = CIRCLE('',#71499,0.0999999999999994) ;
#26678 = CIRCLE('',#71500,0.0999999999999994) ;
#26679 = CIRCLE('',#71502,0.0999999999999994) ;
#26680 = CIRCLE('',#71504,0.0999999999999994) ;
#26681 = CIRCLE('',#71505,0.1) ;
#26682 = CIRCLE('',#71508,0.0999999999999994) ;
#26683 = CIRCLE('',#71511,0.0999999999999994) ;
#26684 = CIRCLE('',#71513,0.0999999999999994) ;
#26685 = CIRCLE('',#71516,0.0999999999999994) ;
#26686 = CIRCLE('',#71518,0.1) ;
#26687 = CIRCLE('',#71520,0.1) ;
#26688 = CIRCLE('',#71522,0.1) ;
#26689 = CIRCLE('',#71524,0.0999999999999994) ;
#26690 = CIRCLE('',#71525,0.1) ;
#26691 = CIRCLE('',#71527,0.0999999999999994) ;
#26692 = CIRCLE('',#71529,0.1) ;
#26693 = CIRCLE('',#71531,0.0999999999999994) ;
#26694 = CIRCLE('',#71532,0.1) ;
#26695 = CIRCLE('',#71534,0.1) ;
#26696 = CIRCLE('',#71536,0.1) ;
#26697 = CIRCLE('',#71538,0.1) ;
#26698 = CIRCLE('',#71540,0.0999999999999994) ;
#26699 = CIRCLE('',#71542,0.0999999999999994) ;
#26700 = CIRCLE('',#71544,0.0999999999999994) ;
#26701 = CIRCLE('',#71546,0.0999999999999994) ;
#26702 = CIRCLE('',#71547,0.0999999999999994) ;
#26703 = CIRCLE('',#71549,0.1) ;
#26704 = CIRCLE('',#71554,0.0999999999999994) ;
#26705 = CIRCLE('',#71557,0.0999999999999998) ;
#26706 = CIRCLE('',#71559,0.0999999999999995) ;
#26707 = CIRCLE('',#71560,0.0999999999999994) ;
#26708 = CIRCLE('',#71562,0.1) ;
#26709 = CIRCLE('',#71564,0.0999999999999998) ;
#26710 = CIRCLE('',#71566,0.0999999999999999) ;
#26711 = CIRCLE('',#71568,0.1) ;
#26712 = CIRCLE('',#71570,0.1) ;
#26713 = CIRCLE('',#71571,0.1) ;
#26714 = CIRCLE('',#71573,0.0999999999999995) ;
#26715 = CIRCLE('',#71575,0.0999999999999994) ;
#26716 = CIRCLE('',#71576,0.0999999999999994) ;
#26717 = CIRCLE('',#71578,0.100000000000001) ;
#26718 = CIRCLE('',#71580,0.0999999999999995) ;
#26719 = CIRCLE('',#71582,0.0999999999999998) ;
#26720 = CIRCLE('',#71584,0.0999999999999994) ;
#26721 = CIRCLE('',#71586,0.100000000000001) ;
#26722 = CIRCLE('',#71588,0.1) ;
#26723 = CIRCLE('',#71589,0.1) ;
#26724 = CIRCLE('',#71591,0.1) ;
#26725 = CIRCLE('',#71593,0.1) ;
#26726 = CIRCLE('',#71595,0.0999999999999994) ;
#26727 = CIRCLE('',#71598,0.100000000000001) ;
#26728 = CIRCLE('',#71600,0.0999999999999994) ;
#26729 = CIRCLE('',#71601,0.0999999999999993) ;
#26730 = CIRCLE('',#71604,0.1) ;
#26731 = CIRCLE('',#71606,0.0999999999999994) ;
#26732 = CIRCLE('',#71607,0.0999999999999994) ;
#26733 = CIRCLE('',#71609,0.0999999999999995) ;
#26734 = CIRCLE('',#71611,0.0999999999999998) ;
#26735 = CIRCLE('',#71613,0.1) ;
#26736 = CIRCLE('',#71614,0.1) ;
#26737 = CIRCLE('',#71616,0.1) ;
#26738 = CIRCLE('',#71618,0.0999999999999994) ;
#26739 = CIRCLE('',#71620,0.0999999999999995) ;
#26740 = CIRCLE('',#71622,0.1) ;
#26741 = CIRCLE('',#71624,0.0999999999999998) ;
#26742 = CIRCLE('',#71626,0.0999999999999995) ;
#26743 = CIRCLE('',#71628,0.0999999999999994) ;
#26744 = CIRCLE('',#71631,0.0999999999999994) ;
#26745 = CIRCLE('',#71633,0.0999999999999994) ;
#26746 = CIRCLE('',#71635,0.1) ;
#26747 = CIRCLE('',#71637,0.1) ;
#26748 = CIRCLE('',#71638,0.0999999999999995) ;
#26749 = CIRCLE('',#71640,0.0999999999999994) ;
#26750 = CIRCLE('',#71642,0.0999999999999994) ;
#26751 = CIRCLE('',#71644,0.1) ;
#26752 = CIRCLE('',#71645,0.0999999999999998) ;
#26753 = CIRCLE('',#71647,0.0999999999999994) ;
#26754 = CIRCLE('',#71649,0.1) ;
#26755 = CIRCLE('',#71650,0.1) ;
#26756 = CIRCLE('',#71652,0.0999999999999994) ;
#26757 = CIRCLE('',#71654,0.0999999999999998) ;
#26758 = CIRCLE('',#71656,0.1) ;
#26759 = CIRCLE('',#71657,0.1) ;
#26760 = CIRCLE('',#71659,0.0999999999999998) ;
#26761 = CIRCLE('',#71661,0.0999999999999994) ;
#26762 = CIRCLE('',#71663,0.1) ;
#26763 = CIRCLE('',#71665,0.0999999999999998) ;
#26764 = CIRCLE('',#71667,0.099999999999999) ;
#26765 = CIRCLE('',#71669,0.1) ;
#26766 = CIRCLE('',#71671,0.0999999999999994) ;
#26767 = CIRCLE('',#71672,0.1) ;
#26768 = CIRCLE('',#71675,0.0999999999999998) ;
#26769 = CIRCLE('',#71677,0.1) ;
#26770 = CIRCLE('',#71679,0.1) ;
#26771 = CIRCLE('',#71680,0.0999999999999995) ;
#26772 = CIRCLE('',#71682,0.1) ;
#26773 = CIRCLE('',#71683,0.0999999999999998) ;
#26774 = CIRCLE('',#71685,0.0999999999999994) ;
#26775 = CIRCLE('',#71686,0.0999999999999994) ;
#26776 = CIRCLE('',#71688,0.0999999999999998) ;
#26777 = CIRCLE('',#71690,0.0999999999999998) ;
#26778 = CIRCLE('',#71692,0.1) ;
#26779 = CIRCLE('',#71694,0.0999999999999994) ;
#26780 = CIRCLE('',#71696,0.0999999999999994) ;
#26781 = CIRCLE('',#71698,0.1) ;
#26782 = CIRCLE('',#71699,0.0999999999999995) ;
#26783 = CIRCLE('',#71701,0.1) ;
#26784 = CIRCLE('',#71702,0.0999999999999995) ;
#26785 = CIRCLE('',#71704,0.0999999999999998) ;
#26786 = CIRCLE('',#71706,0.0999999999999994) ;
#26787 = CIRCLE('',#71708,0.0999999999999994) ;
#26788 = CIRCLE('',#71711,0.0999999999999994) ;
#26789 = CIRCLE('',#71713,0.0999999999999995) ;
#26790 = CIRCLE('',#71715,0.0999999999999994) ;
#26791 = CIRCLE('',#71717,0.1) ;
#26792 = CIRCLE('',#71719,0.0999999999999994) ;
#26793 = CIRCLE('',#71721,0.0999999999999998) ;
#26794 = CIRCLE('',#71725,0.0999999999999995) ;
#26795 = CIRCLE('',#71727,0.1) ;
#26796 = CIRCLE('',#71729,0.0999999999999994) ;
#26797 = CIRCLE('',#71731,0.0999999999999994) ;
#26798 = CIRCLE('',#71733,0.0999999999999994) ;
#26799 = CIRCLE('',#71735,0.100000000000001) ;
#26800 = CIRCLE('',#71739,0.1) ;
#26801 = CIRCLE('',#71740,0.1) ;
#26802 = CIRCLE('',#71746,0.0999999999999994) ;
#26803 = CIRCLE('',#71748,0.1) ;
#26804 = CIRCLE('',#71749,0.1) ;
#26805 = CIRCLE('',#71751,0.0999999999999994) ;
#26806 = CIRCLE('',#71752,0.1) ;
#26807 = CIRCLE('',#71754,0.0999999999999994) ;
#26808 = CIRCLE('',#71756,0.0999999999999994) ;
#26809 = CIRCLE('',#71758,0.0999999999999994) ;
#26810 = CIRCLE('',#71759,0.0999999999999994) ;
#26811 = CIRCLE('',#71761,0.0999999999999994) ;
#26812 = CIRCLE('',#71763,0.0999999999999994) ;
#26813 = CIRCLE('',#71765,0.1) ;
#26814 = CIRCLE('',#71766,0.0999999999999994) ;
#26815 = CIRCLE('',#71768,0.0999999999999994) ;
#26816 = CIRCLE('',#71771,0.0999999999999994) ;
#26817 = CIRCLE('',#71773,0.0999999999999994) ;
#26818 = CIRCLE('',#71777,0.0999999999999994) ;
#26819 = CIRCLE('',#71779,0.0999999999999994) ;
#26820 = CIRCLE('',#71781,0.0999999999999999) ;
#26821 = CIRCLE('',#71782,0.1) ;
#26822 = CIRCLE('',#71785,0.1) ;
#26823 = CIRCLE('',#71786,0.0999999999999998) ;
#26824 = CIRCLE('',#71788,0.1) ;
#26825 = CIRCLE('',#71790,0.0999999999999994) ;
#26826 = CIRCLE('',#71792,0.0999999999999998) ;
#26827 = CIRCLE('',#71794,0.1) ;
#26828 = CIRCLE('',#71796,0.0999999999999994) ;
#26829 = CIRCLE('',#71798,0.1) ;
#26830 = CIRCLE('',#71801,0.0999999999999994) ;
#26831 = CIRCLE('',#71802,0.0999999999999994) ;
#26832 = CIRCLE('',#71804,0.0999999999999994) ;
#26833 = CIRCLE('',#71806,0.0999999999999994) ;
#26834 = CIRCLE('',#71808,0.0999999999999994) ;
#26835 = CIRCLE('',#71810,0.1) ;
#26836 = CIRCLE('',#71812,0.0999999999999994) ;
#26837 = CIRCLE('',#71814,0.0999999999999994) ;
#26838 = CIRCLE('',#71817,0.0999999999999994) ;
#26839 = CIRCLE('',#71819,0.0999999999999999) ;
#26840 = CIRCLE('',#71820,0.0999999999999999) ;
#26841 = CIRCLE('',#71824,0.0999999999999994) ;
#26842 = CIRCLE('',#71826,0.0999999999999994) ;
#26843 = CIRCLE('',#71831,1.4986) ;
#26844 = CIRCLE('',#71832,1.4986) ;
#26845 = CIRCLE('',#71833,1.4986) ;
#26846 = CIRCLE('',#71835,1.9939) ;
#26847 = CIRCLE('',#71836,1.9939) ;
#26848 = CIRCLE('',#71838,0.254) ;
#26849 = CIRCLE('',#71839,0.254) ;
#26850 = CIRCLE('',#71841,0.254) ;
#26851 = CIRCLE('',#71842,0.254) ;
#26852 = CIRCLE('',#71845,0.254) ;
#26853 = CIRCLE('',#71846,0.254) ;
#26854 = CIRCLE('',#71849,0.254) ;
#26855 = CIRCLE('',#71850,0.254) ;
#26856 = CIRCLE('',#71863,1.4986) ;
#26857 = CIRCLE('',#71868,0.899999999999998) ;
#26858 = CIRCLE('',#71869,0.1) ;
#26859 = CIRCLE('',#71870,1.) ;
#26860 = CIRCLE('',#71871,1.) ;
#26861 = CIRCLE('',#71873,1.1) ;
#26862 = CIRCLE('',#71874,0.1) ;
#26863 = CIRCLE('',#71875,1.) ;
#26864 = CIRCLE('',#71877,0.100000000000003) ;
#26865 = CIRCLE('',#71878,0.0999999999999999) ;
#26866 = CIRCLE('',#71879,0.1) ;
#26867 = CIRCLE('',#71882,0.1) ;
#26868 = CIRCLE('',#71883,0.100000000000003) ;
#26869 = CIRCLE('',#71885,0.899999999999998) ;
#26870 = CIRCLE('',#71886,0.1) ;
#26871 = CIRCLE('',#71887,1.) ;
#26872 = CIRCLE('',#71888,1.) ;
#26873 = CIRCLE('',#71890,1.1) ;
#26874 = CIRCLE('',#71891,0.1) ;
#26875 = CIRCLE('',#71892,1.) ;
#26876 = CIRCLE('',#71894,0.0999999999999994) ;
#26877 = CIRCLE('',#71895,0.1) ;
#26878 = CIRCLE('',#71896,0.1) ;
#26879 = CIRCLE('',#71899,0.1) ;
#26880 = CIRCLE('',#71900,0.0999999999999994) ;
#26881 = CIRCLE('',#71902,0.899999999999998) ;
#26882 = CIRCLE('',#71903,0.1) ;
#26883 = CIRCLE('',#71904,1.) ;
#26884 = CIRCLE('',#71905,1.) ;
#26885 = CIRCLE('',#71907,1.1) ;
#26886 = CIRCLE('',#71908,0.1) ;
#26887 = CIRCLE('',#71909,1.) ;
#26888 = CIRCLE('',#71911,0.0999999999999994) ;
#26889 = CIRCLE('',#71912,0.1) ;
#26890 = CIRCLE('',#71913,0.1) ;
#26891 = CIRCLE('',#71916,0.1) ;
#26892 = CIRCLE('',#71917,0.0999999999999994) ;
#26893 = CIRCLE('',#71919,0.899999999999998) ;
#26894 = CIRCLE('',#71920,0.1) ;
#26895 = CIRCLE('',#71921,1.) ;
#26896 = CIRCLE('',#71922,1.) ;
#26897 = CIRCLE('',#71924,1.1) ;
#26898 = CIRCLE('',#71925,0.1) ;
#26899 = CIRCLE('',#71926,1.) ;
#26900 = CIRCLE('',#71928,0.0999999999999994) ;
#26901 = CIRCLE('',#71929,0.1) ;
#26902 = CIRCLE('',#71930,0.1) ;
#26903 = CIRCLE('',#71933,0.1) ;
#26904 = CIRCLE('',#71934,0.0999999999999994) ;
#26905 = CIRCLE('',#71936,0.900000000000001) ;
#26906 = CIRCLE('',#71937,0.1) ;
#26907 = CIRCLE('',#71938,1.) ;
#26908 = CIRCLE('',#71939,1.) ;
#26909 = CIRCLE('',#71941,1.1) ;
#26910 = CIRCLE('',#71942,0.1) ;
#26911 = CIRCLE('',#71943,1.) ;
#26912 = CIRCLE('',#71945,0.0999999999999994) ;
#26913 = CIRCLE('',#71946,0.1) ;
#26914 = CIRCLE('',#71947,0.1) ;
#26915 = CIRCLE('',#71950,0.1) ;
#26916 = CIRCLE('',#71951,0.0999999999999994) ;
#26917 = CIRCLE('',#71953,0.900000000000001) ;
#26918 = CIRCLE('',#71954,0.1) ;
#26919 = CIRCLE('',#71955,1.) ;
#26920 = CIRCLE('',#71956,1.) ;
#26921 = CIRCLE('',#71958,1.1) ;
#26922 = CIRCLE('',#71959,0.1) ;
#26923 = CIRCLE('',#71960,0.999999999999999) ;
#26924 = CIRCLE('',#71962,0.100000000000001) ;
#26925 = CIRCLE('',#71963,0.1) ;
#26926 = CIRCLE('',#71964,0.1) ;
#26927 = CIRCLE('',#71967,0.1) ;
#26928 = CIRCLE('',#71968,0.0999999999999994) ;
#26929 = CIRCLE('',#71970,0.9) ;
#26930 = CIRCLE('',#71971,0.1) ;
#26931 = CIRCLE('',#71972,0.999999999999999) ;
#26932 = CIRCLE('',#71973,0.999999999999999) ;
#26933 = CIRCLE('',#71975,1.1) ;
#26934 = CIRCLE('',#71976,0.1) ;
#26935 = CIRCLE('',#71977,0.999999999999999) ;
#26936 = CIRCLE('',#71979,0.100000000000001) ;
#26937 = CIRCLE('',#71980,0.1) ;
#26938 = CIRCLE('',#71981,0.1) ;
#26939 = CIRCLE('',#71984,0.1) ;
#26940 = CIRCLE('',#71985,0.0999999999999994) ;
#26941 = CIRCLE('',#71987,0.9) ;
#26942 = CIRCLE('',#71988,0.1) ;
#26943 = CIRCLE('',#71989,0.999999999999999) ;
#26944 = CIRCLE('',#71990,0.999999999999999) ;
#26945 = CIRCLE('',#71992,1.1) ;
#26946 = CIRCLE('',#71993,0.1) ;
#26947 = CIRCLE('',#71994,1.) ;
#26948 = CIRCLE('',#71996,0.1) ;
#26949 = CIRCLE('',#71997,0.1) ;
#26950 = CIRCLE('',#71998,0.1) ;
#26951 = CIRCLE('',#72001,0.1) ;
#26952 = CIRCLE('',#72002,0.0999999999999994) ;
#26953 = CIRCLE('',#72004,0.9) ;
#26954 = CIRCLE('',#72005,0.1) ;
#26955 = CIRCLE('',#72006,1.) ;
#26956 = CIRCLE('',#72007,1.) ;
#26957 = CIRCLE('',#72009,0.200000000000001) ;
#26958 = CIRCLE('',#72010,0.0999999999999994) ;
#26959 = CIRCLE('',#72011,0.1) ;
#26960 = CIRCLE('',#72012,0.1) ;
#26961 = CIRCLE('',#72014,0.200000000000001) ;
#26962 = CIRCLE('',#72015,0.0999999999999994) ;
#26963 = CIRCLE('',#72016,0.100000000000001) ;
#26964 = CIRCLE('',#72017,0.1) ;
#26965 = CIRCLE('',#72019,0.200000000000001) ;
#26966 = CIRCLE('',#72020,0.0999999999999994) ;
#26967 = CIRCLE('',#72021,0.100000000000001) ;
#26968 = CIRCLE('',#72022,0.1) ;
#26969 = CIRCLE('',#72024,0.199999999999999) ;
#26970 = CIRCLE('',#72025,0.0999999999999994) ;
#26971 = CIRCLE('',#72026,0.0999999999999994) ;
#26972 = CIRCLE('',#72027,0.0999999999999995) ;
#26973 = CIRCLE('',#72029,0.199999999999999) ;
#26974 = CIRCLE('',#72030,0.0999999999999994) ;
#26975 = CIRCLE('',#72031,0.0999999999999994) ;
#26976 = CIRCLE('',#72032,0.0999999999999995) ;
#26977 = CIRCLE('',#72034,0.199999999999999) ;
#26978 = CIRCLE('',#72035,0.0999999999999994) ;
#26979 = CIRCLE('',#72036,0.0999999999999994) ;
#26980 = CIRCLE('',#72037,0.0999999999999995) ;
#26981 = CIRCLE('',#72039,0.199999999999999) ;
#26982 = CIRCLE('',#72040,0.0999999999999994) ;
#26983 = CIRCLE('',#72041,0.0999999999999994) ;
#26984 = CIRCLE('',#72042,0.0999999999999995) ;
#26985 = CIRCLE('',#72044,0.199999999999999) ;
#26986 = CIRCLE('',#72045,0.0999999999999994) ;
#26987 = CIRCLE('',#72046,0.100000000000003) ;
#26988 = CIRCLE('',#72047,0.0999999999999995) ;
#26989 = CIRCLE('',#72049,0.199999999999999) ;
#26990 = CIRCLE('',#72050,0.0999999999999994) ;
#26991 = CIRCLE('',#72051,0.100000000000003) ;
#26992 = CIRCLE('',#72052,0.0999999999999995) ;
#26993 = CIRCLE('',#72054,1.1) ;
#26994 = CIRCLE('',#72055,0.1) ;
#26995 = CIRCLE('',#72056,1.) ;
#26996 = CIRCLE('',#72058,0.100000000000001) ;
#26997 = CIRCLE('',#72059,0.0999999999999998) ;
#26998 = CIRCLE('',#72060,0.1) ;
#26999 = CIRCLE('',#72063,0.1) ;
#27000 = CIRCLE('',#72064,0.1) ;
#27001 = CIRCLE('',#72075,0.1) ;
#27002 = CIRCLE('',#72077,0.100000000000001) ;
#27003 = CIRCLE('',#72079,0.100000000000001) ;
#27004 = CIRCLE('',#72081,0.0999999999999994) ;
#27005 = CIRCLE('',#72083,0.0999999999999994) ;
#27006 = CIRCLE('',#72085,0.0999999999999994) ;
#27007 = CIRCLE('',#72087,0.0999999999999994) ;
#27008 = CIRCLE('',#72089,0.100000000000003) ;
#27009 = CIRCLE('',#72091,0.100000000000003) ;
#27010 = CIRCLE('',#72093,0.9) ;
#27011 = CIRCLE('',#72094,0.1) ;
#27012 = CIRCLE('',#72095,1.) ;
#27013 = CIRCLE('',#72096,1.) ;
#27014 = CIRCLE('',#72098,0.200000000000001) ;
#27015 = CIRCLE('',#72099,0.0999999999999994) ;
#27016 = CIRCLE('',#72100,0.1) ;
#27017 = CIRCLE('',#72101,0.1) ;
#27018 = CIRCLE('',#72103,1.1) ;
#27019 = CIRCLE('',#72104,0.1) ;
#27020 = CIRCLE('',#72105,1.) ;
#27021 = CIRCLE('',#72107,0.1) ;
#27022 = CIRCLE('',#72108,0.1) ;
#27023 = CIRCLE('',#72109,0.1) ;
#27024 = CIRCLE('',#72112,0.1) ;
#27025 = CIRCLE('',#72113,0.1) ;
#27026 = CIRCLE('',#72116,0.1) ;
#27027 = CIRCLE('',#72118,0.1) ;
#27028 = CIRCLE('',#72119,0.1) ;
#27029 = CIRCLE('',#72120,0.2) ;
#27030 = CIRCLE('',#72121,0.2) ;
#27031 = CIRCLE('',#72123,0.1) ;
#27032 = CIRCLE('',#72124,0.1) ;
#27033 = CIRCLE('',#72125,0.2) ;
#27034 = CIRCLE('',#72126,0.2) ;
#27035 = CIRCLE('',#72128,0.1) ;
#27036 = CIRCLE('',#72129,0.1) ;
#27037 = CIRCLE('',#72130,0.2) ;
#27038 = CIRCLE('',#72131,0.2) ;
#27039 = CIRCLE('',#72133,0.1) ;
#27040 = CIRCLE('',#72134,0.1) ;
#27041 = CIRCLE('',#72135,0.2) ;
#27042 = CIRCLE('',#72136,0.2) ;
#27043 = CIRCLE('',#72138,0.1) ;
#27044 = CIRCLE('',#72139,0.1) ;
#27045 = CIRCLE('',#72140,0.2) ;
#27046 = CIRCLE('',#72141,0.2) ;
#27047 = CIRCLE('',#72143,0.1) ;
#27048 = CIRCLE('',#72144,0.1) ;
#27049 = CIRCLE('',#72145,0.2) ;
#27050 = CIRCLE('',#72146,0.2) ;
#27051 = CIRCLE('',#72148,0.1) ;
#27052 = CIRCLE('',#72149,0.1) ;
#27053 = CIRCLE('',#72150,0.2) ;
#27054 = CIRCLE('',#72151,0.2) ;
#27055 = CIRCLE('',#72153,0.1) ;
#27056 = CIRCLE('',#72154,0.1) ;
#27057 = CIRCLE('',#72155,0.2) ;
#27058 = CIRCLE('',#72156,0.2) ;
#27059 = CIRCLE('',#72158,0.1) ;
#27060 = CIRCLE('',#72159,0.1) ;
#27061 = CIRCLE('',#72160,0.2) ;
#27062 = CIRCLE('',#72161,0.2) ;
#27063 = CIRCLE('',#72163,0.2) ;
#27064 = CIRCLE('',#72165,0.2) ;
#27065 = CIRCLE('',#72167,0.2) ;
#27066 = CIRCLE('',#72169,0.2) ;
#27067 = CIRCLE('',#72171,0.2) ;
#27068 = CIRCLE('',#72173,0.2) ;
#27069 = CIRCLE('',#72175,0.2) ;
#27070 = CIRCLE('',#72177,0.2) ;
#27071 = CIRCLE('',#72179,0.2) ;
#27072 = CIRCLE('',#72181,0.2) ;
#27073 = CIRCLE('',#72183,0.2) ;
#27074 = CIRCLE('',#72185,0.2) ;
#27075 = CIRCLE('',#72187,0.2) ;
#27076 = CIRCLE('',#72189,0.2) ;
#27077 = CIRCLE('',#72191,0.2) ;
#27078 = CIRCLE('',#72193,0.2) ;
#27079 = CIRCLE('',#72195,0.2) ;
#27080 = CIRCLE('',#72197,0.2) ;
#27081 = CIRCLE('',#72199,0.1) ;
#27082 = CIRCLE('',#72200,0.1) ;
#27083 = CIRCLE('',#72202,0.1) ;
#27084 = CIRCLE('',#72203,0.1) ;
#27085 = CIRCLE('',#72205,0.1) ;
#27086 = CIRCLE('',#72206,0.1) ;
#27087 = CIRCLE('',#72208,0.1) ;
#27088 = CIRCLE('',#72209,0.1) ;
#27089 = CIRCLE('',#72211,0.1) ;
#27090 = CIRCLE('',#72212,0.1) ;
#27091 = CIRCLE('',#72214,0.1) ;
#27092 = CIRCLE('',#72215,0.1) ;
#27093 = CIRCLE('',#72217,0.1) ;
#27094 = CIRCLE('',#72218,0.1) ;
#27095 = CIRCLE('',#72220,0.1) ;
#27096 = CIRCLE('',#72221,0.1) ;
#27097 = CIRCLE('',#72223,0.1) ;
#27098 = CIRCLE('',#72224,0.1) ;
#27099 = CIRCLE('',#72226,0.1) ;
#27100 = CIRCLE('',#72227,0.1) ;
#27101 = CIRCLE('',#72228,0.2) ;
#27102 = CIRCLE('',#72229,0.2) ;
#27103 = CIRCLE('',#72231,0.2) ;
#27104 = CIRCLE('',#72233,0.2) ;
#27105 = CIRCLE('',#72235,0.1) ;
#27106 = CIRCLE('',#72236,0.1) ;
#27107 = CIRCLE('',#72238,0.0999999999999994) ;
#27108 = CIRCLE('',#72239,0.0999999999999994) ;
#27109 = CIRCLE('',#72241,0.199999999999999) ;
#27110 = CIRCLE('',#72242,0.2) ;
#27111 = CIRCLE('',#72243,0.2) ;
#27112 = CIRCLE('',#72244,0.2) ;
#27113 = CIRCLE('',#72245,0.2) ;
#27114 = CIRCLE('',#72246,0.2) ;
#27115 = CIRCLE('',#72247,0.200000000000001) ;
#27116 = CIRCLE('',#72248,0.200000000000001) ;
#27117 = CIRCLE('',#72249,0.200000000000001) ;
#27118 = CIRCLE('',#72250,0.200000000000001) ;
#27119 = CIRCLE('',#72251,0.199999999999999) ;
#27120 = CIRCLE('',#72252,0.199999999999999) ;
#27121 = CIRCLE('',#72253,0.199999999999999) ;
#27122 = CIRCLE('',#72254,0.199999999999999) ;
#27123 = CIRCLE('',#72255,0.199999999999999) ;
#27124 = CIRCLE('',#72256,0.199999999999999) ;
#27125 = CIRCLE('',#72257,0.199999999999999) ;
#27126 = CIRCLE('',#72258,0.199999999999999) ;
#27127 = CIRCLE('',#72259,0.199999999999999) ;
#27128 = CIRCLE('',#72260,0.199999999999999) ;
#27129 = CIRCLE('',#72262,0.1) ;
#27130 = CIRCLE('',#72263,0.1) ;
#27131 = CIRCLE('',#72265,0.2) ;
#27132 = CIRCLE('',#72266,0.2) ;
#27133 = CIRCLE('',#72267,0.2) ;
#27134 = CIRCLE('',#72268,0.2) ;
#27135 = CIRCLE('',#72269,0.2) ;
#27136 = CIRCLE('',#72270,0.2) ;
#27137 = CIRCLE('',#72271,0.2) ;
#27138 = CIRCLE('',#72272,0.2) ;
#27139 = CIRCLE('',#72273,0.2) ;
#27140 = CIRCLE('',#72274,0.2) ;
#27141 = CIRCLE('',#72275,0.2) ;
#27142 = CIRCLE('',#72276,0.2) ;
#27143 = CIRCLE('',#72277,0.2) ;
#27144 = CIRCLE('',#72278,0.2) ;
#27145 = CIRCLE('',#72279,0.2) ;
#27146 = CIRCLE('',#72280,0.2) ;
#27147 = CIRCLE('',#72281,0.2) ;
#27148 = CIRCLE('',#72282,0.2) ;
#27149 = CIRCLE('',#72283,0.2) ;
#27150 = CIRCLE('',#72284,0.2) ;
#27151 = CIRCLE('',#72286,0.1) ;
#27152 = CIRCLE('',#72287,0.1) ;
#27153 = CIRCLE('',#72290,0.1) ;
#27154 = CIRCLE('',#72291,0.1) ;
#27155 = CIRCLE('',#72294,0.1) ;
#27156 = CIRCLE('',#72295,0.1) ;
#27157 = CIRCLE('',#72298,0.100000000000001) ;
#27158 = CIRCLE('',#72299,0.100000000000001) ;
#27159 = CIRCLE('',#72302,0.1) ;
#27160 = CIRCLE('',#72303,0.1) ;
#27161 = CIRCLE('',#72306,0.0999999999999994) ;
#27162 = CIRCLE('',#72307,0.0999999999999994) ;
#27163 = CIRCLE('',#72309,0.199999999999999) ;
#27164 = CIRCLE('',#72310,0.199999999999999) ;
#27165 = CIRCLE('',#72311,0.199999999999999) ;
#27166 = CIRCLE('',#72312,0.199999999999999) ;
#27167 = CIRCLE('',#72313,0.199999999999999) ;
#27168 = CIRCLE('',#72314,0.199999999999999) ;
#27169 = CIRCLE('',#72315,0.199999999999999) ;
#27170 = CIRCLE('',#72316,1.55625) ;
#27171 = CIRCLE('',#72317,0.199999999999999) ;
#27172 = CIRCLE('',#72318,0.199999999999999) ;
#27173 = CIRCLE('',#72319,0.199999999999999) ;
#27174 = CIRCLE('',#72320,0.199999999999999) ;
#27175 = CIRCLE('',#72321,0.199999999999999) ;
#27176 = CIRCLE('',#72322,0.199999999999999) ;
#27177 = CIRCLE('',#72323,0.199999999999999) ;
#27178 = CIRCLE('',#72324,0.199999999999999) ;
#27179 = CIRCLE('',#72325,0.199999999999999) ;
#27180 = CIRCLE('',#72326,1.55625) ;
#27181 = CIRCLE('',#72327,0.199999999999999) ;
#27182 = CIRCLE('',#72328,0.199999999999999) ;
#27183 = CIRCLE('',#72329,0.199999999999999) ;
#27184 = CIRCLE('',#72330,0.199999999999999) ;
#27185 = CIRCLE('',#72331,0.199999999999999) ;
#27186 = CIRCLE('',#72332,0.199999999999999) ;
#27187 = CIRCLE('',#72333,0.199999999999999) ;
#27188 = CIRCLE('',#72334,0.199999999999999) ;
#27189 = CIRCLE('',#72335,0.199999999999999) ;
#27190 = CIRCLE('',#72336,1.55625) ;
#27191 = CIRCLE('',#72337,0.199999999999999) ;
#27192 = CIRCLE('',#72338,0.199999999999999) ;
#27193 = CIRCLE('',#72339,0.199999999999999) ;
#27194 = CIRCLE('',#72340,0.199999999999999) ;
#27195 = CIRCLE('',#72341,0.199999999999999) ;
#27196 = CIRCLE('',#72342,0.199999999999999) ;
#27197 = CIRCLE('',#72343,0.199999999999999) ;
#27198 = CIRCLE('',#72344,0.199999999999999) ;
#27199 = CIRCLE('',#72345,0.199999999999999) ;
#27200 = CIRCLE('',#72346,1.55625) ;
#27201 = CIRCLE('',#72347,0.199999999999999) ;
#27202 = CIRCLE('',#72348,0.199999999999999) ;
#27203 = CIRCLE('',#72349,0.199999999999999) ;
#27204 = CIRCLE('',#72350,0.199999999999999) ;
#27205 = CIRCLE('',#72351,0.199999999999999) ;
#27206 = CIRCLE('',#72352,0.199999999999999) ;
#27207 = CIRCLE('',#72353,0.199999999999999) ;
#27208 = CIRCLE('',#72354,0.199999999999999) ;
#27209 = CIRCLE('',#72355,0.199999999999999) ;
#27210 = CIRCLE('',#72356,1.55625) ;
#27211 = CIRCLE('',#72357,0.199999999999999) ;
#27212 = CIRCLE('',#72358,0.199999999999999) ;
#27213 = CIRCLE('',#72359,0.200000000000001) ;
#27214 = CIRCLE('',#72360,0.199999999999999) ;
#27215 = CIRCLE('',#72361,0.200000000000001) ;
#27216 = CIRCLE('',#72362,0.199999999999999) ;
#27217 = CIRCLE('',#72363,0.199999999999999) ;
#27218 = CIRCLE('',#72364,0.199999999999999) ;
#27219 = CIRCLE('',#72365,0.199999999999999) ;
#27220 = CIRCLE('',#72366,1.55625) ;
#27221 = CIRCLE('',#72367,0.200000000000001) ;
#27222 = CIRCLE('',#72368,0.200000000000001) ;
#27223 = CIRCLE('',#72369,0.200000000000001) ;
#27224 = CIRCLE('',#72370,0.199999999999999) ;
#27225 = CIRCLE('',#72371,0.200000000000001) ;
#27226 = CIRCLE('',#72372,0.200000000000001) ;
#27227 = CIRCLE('',#72373,0.200000000000001) ;
#27228 = CIRCLE('',#72374,0.200000000000001) ;
#27229 = CIRCLE('',#72375,0.200000000000001) ;
#27230 = CIRCLE('',#72376,1.55625) ;
#27231 = CIRCLE('',#72377,0.200000000000001) ;
#27232 = CIRCLE('',#72378,0.200000000000001) ;
#27233 = CIRCLE('',#72379,0.2) ;
#27234 = CIRCLE('',#72380,0.2) ;
#27235 = CIRCLE('',#72381,0.200000000000001) ;
#27236 = CIRCLE('',#72382,0.200000000000001) ;
#27237 = CIRCLE('',#72383,0.200000000000001) ;
#27238 = CIRCLE('',#72384,0.200000000000001) ;
#27239 = CIRCLE('',#72385,0.200000000000001) ;
#27240 = CIRCLE('',#72386,1.55625) ;
#27241 = CIRCLE('',#72387,0.2) ;
#27242 = CIRCLE('',#72388,0.2) ;
#27243 = CIRCLE('',#72389,0.2) ;
#27244 = CIRCLE('',#72390,0.199999999999999) ;
#27245 = CIRCLE('',#72391,0.200000000000001) ;
#27246 = CIRCLE('',#72392,0.200000000000001) ;
#27247 = CIRCLE('',#72393,0.2) ;
#27248 = CIRCLE('',#72394,0.2) ;
#27249 = CIRCLE('',#72395,0.2) ;
#27250 = CIRCLE('',#72396,1.55625) ;
#27251 = CIRCLE('',#72397,0.2) ;
#27252 = CIRCLE('',#72398,0.2) ;
#27253 = CIRCLE('',#72399,0.2) ;
#27254 = CIRCLE('',#72400,0.199999999999999) ;
#27255 = CIRCLE('',#72401,0.200000000000001) ;
#27256 = CIRCLE('',#72402,0.2) ;
#27257 = CIRCLE('',#72403,0.2) ;
#27258 = CIRCLE('',#72404,0.2) ;
#27259 = CIRCLE('',#72405,0.2) ;
#27260 = CIRCLE('',#72406,1.55625) ;
#27261 = CIRCLE('',#72407,0.2) ;
#27262 = CIRCLE('',#72408,0.2) ;
#27263 = CIRCLE('',#72410,0.200000000000001) ;
#27264 = CIRCLE('',#72411,0.200000000000001) ;
#27265 = CIRCLE('',#72413,0.200000000000001) ;
#27266 = CIRCLE('',#72414,0.200000000000001) ;
#27267 = CIRCLE('',#72416,0.2) ;
#27268 = CIRCLE('',#72417,0.2) ;
#27269 = CIRCLE('',#72424,0.1) ;
#27270 = CIRCLE('',#72425,0.1) ;
#27271 = CIRCLE('',#72428,0.1) ;
#27272 = CIRCLE('',#72429,0.1) ;
#27273 = CIRCLE('',#72432,0.0999999999999994) ;
#27274 = CIRCLE('',#72433,0.0999999999999994) ;
#27275 = CIRCLE('',#72436,0.1) ;
#27276 = CIRCLE('',#72440,0.1) ;
#27277 = CIRCLE('',#72441,0.1) ;
#27278 = CIRCLE('',#72444,0.1) ;
#27279 = CIRCLE('',#72445,0.1) ;
#27280 = CIRCLE('',#72448,0.1) ;
#27281 = CIRCLE('',#72449,0.1) ;
#27282 = CIRCLE('',#72452,0.1) ;
#27283 = CIRCLE('',#72453,0.1) ;
#27284 = CIRCLE('',#72456,0.1) ;
#27285 = CIRCLE('',#72457,0.1) ;
#27286 = CIRCLE('',#72460,0.1) ;
#27287 = CIRCLE('',#72461,0.1) ;
#27288 = CIRCLE('',#72463,1.65625) ;
#27289 = CIRCLE('',#72464,1.65625) ;
#27290 = CIRCLE('',#72466,0.1) ;
#27291 = CIRCLE('',#72467,0.1) ;
#27292 = CIRCLE('',#72470,0.1) ;
#27293 = CIRCLE('',#72471,0.1) ;
#27294 = CIRCLE('',#72474,0.1) ;
#27295 = CIRCLE('',#72475,0.1) ;
#27296 = CIRCLE('',#72478,0.2) ;
#27297 = CIRCLE('',#72479,0.2) ;
#27298 = CIRCLE('',#72480,1.75625) ;
#27299 = CIRCLE('',#72481,0.2) ;
#27300 = CIRCLE('',#72482,0.2) ;
#27301 = CIRCLE('',#72484,0.1) ;
#27302 = CIRCLE('',#72485,0.1) ;
#27303 = CIRCLE('',#72486,0.1) ;
#27304 = CIRCLE('',#72487,0.1) ;
#27305 = CIRCLE('',#72489,0.1) ;
#27306 = CIRCLE('',#72490,0.1) ;
#27307 = CIRCLE('',#72492,0.1) ;
#27308 = CIRCLE('',#72493,0.1) ;
#27309 = CIRCLE('',#72495,0.1) ;
#27310 = CIRCLE('',#72496,0.1) ;
#27311 = CIRCLE('',#72498,0.1) ;
#27312 = CIRCLE('',#72499,0.0999999999999998) ;
#27313 = CIRCLE('',#72501,0.1) ;
#27314 = CIRCLE('',#72503,0.1) ;
#27315 = CIRCLE('',#72505,0.1) ;
#27316 = CIRCLE('',#72507,0.1) ;
#27317 = CIRCLE('',#72509,0.0999999999999998) ;
#27318 = CIRCLE('',#72511,0.1) ;
#27319 = CIRCLE('',#72513,0.1) ;
#27320 = CIRCLE('',#72514,0.1) ;
#27321 = CIRCLE('',#72517,0.1) ;
#27322 = CIRCLE('',#72519,0.1) ;
#27323 = CIRCLE('',#72520,0.1) ;
#27324 = CIRCLE('',#72522,0.1) ;
#27325 = CIRCLE('',#72524,0.1) ;
#27326 = CIRCLE('',#72526,0.1) ;
#27327 = CIRCLE('',#72528,0.1) ;
#27328 = CIRCLE('',#72530,0.1) ;
#27329 = CIRCLE('',#72532,0.1) ;
#27330 = CIRCLE('',#72533,0.1) ;
#27331 = CIRCLE('',#72535,0.1) ;
#27332 = CIRCLE('',#72537,0.1) ;
#27333 = CIRCLE('',#72539,0.0999999999999998) ;
#27334 = CIRCLE('',#72540,0.1) ;
#27335 = CIRCLE('',#72542,0.1) ;
#27336 = CIRCLE('',#72544,0.1) ;
#27337 = CIRCLE('',#72545,0.1) ;
#27338 = CIRCLE('',#72547,0.1) ;
#27339 = CIRCLE('',#72549,0.1) ;
#27340 = CIRCLE('',#72551,0.1) ;
#27341 = CIRCLE('',#72553,0.1) ;
#27342 = CIRCLE('',#72555,0.1) ;
#27343 = CIRCLE('',#72557,0.1) ;
#27344 = CIRCLE('',#72559,0.1) ;
#27345 = CIRCLE('',#72561,0.1) ;
#27346 = CIRCLE('',#72562,0.1) ;
#27347 = CIRCLE('',#72564,0.1) ;
#27348 = CIRCLE('',#72566,0.1) ;
#27349 = CIRCLE('',#72568,0.1) ;
#27350 = CIRCLE('',#72570,0.1) ;
#27351 = CIRCLE('',#72571,0.1) ;
#27352 = CIRCLE('',#72573,0.1) ;
#27353 = CIRCLE('',#72575,0.1) ;
#27354 = CIRCLE('',#72577,0.1) ;
#27355 = CIRCLE('',#72579,0.1) ;
#27356 = CIRCLE('',#72582,0.1) ;
#27357 = CIRCLE('',#72584,0.1) ;
#27358 = CIRCLE('',#72586,0.1) ;
#27359 = CIRCLE('',#72589,0.100000000000003) ;
#27360 = CIRCLE('',#72590,0.100000000000003) ;
#27361 = CIRCLE('',#72592,0.100000000000003) ;
#27362 = CIRCLE('',#72594,0.100000000000003) ;
#27363 = CIRCLE('',#72596,0.1) ;
#27364 = CIRCLE('',#72598,0.100000000000003) ;
#27365 = CIRCLE('',#72600,0.100000000000003) ;
#27366 = CIRCLE('',#72602,0.1) ;
#27367 = CIRCLE('',#72604,0.1) ;
#27368 = CIRCLE('',#72606,0.1) ;
#27369 = CIRCLE('',#72608,0.100000000000003) ;
#27370 = CIRCLE('',#72610,0.100000000000003) ;
#27371 = CIRCLE('',#72612,0.0999999999999998) ;
#27372 = CIRCLE('',#72614,0.100000000000003) ;
#27373 = CIRCLE('',#72616,0.100000000000003) ;
#27374 = CIRCLE('',#72618,0.0999999999999994) ;
#27375 = CIRCLE('',#72621,0.0999999999999998) ;
#27376 = CIRCLE('',#72622,0.0999999999999998) ;
#27377 = CIRCLE('',#72624,0.0999999999999998) ;
#27378 = CIRCLE('',#72626,0.0999999999999998) ;
#27379 = CIRCLE('',#72628,0.0999999999999998) ;
#27380 = CIRCLE('',#72630,0.0999999999999998) ;
#27381 = CIRCLE('',#72632,0.1) ;
#27382 = CIRCLE('',#72634,0.1) ;
#27383 = CIRCLE('',#72636,0.1) ;
#27384 = CIRCLE('',#72638,0.1) ;
#27385 = CIRCLE('',#72640,0.1) ;
#27386 = CIRCLE('',#72642,0.0999999999999998) ;
#27387 = CIRCLE('',#72644,0.0999999999999998) ;
#27388 = CIRCLE('',#72646,0.0999999999999998) ;
#27389 = CIRCLE('',#72648,0.0999999999999998) ;
#27390 = CIRCLE('',#72650,0.0999999999999998) ;
#27391 = CIRCLE('',#72653,0.1) ;
#27392 = CIRCLE('',#72654,0.1) ;
#27393 = CIRCLE('',#72656,0.1) ;
#27394 = CIRCLE('',#72658,0.1) ;
#27395 = CIRCLE('',#72660,0.1) ;
#27396 = CIRCLE('',#72662,0.1) ;
#27397 = CIRCLE('',#72664,0.1) ;
#27398 = CIRCLE('',#72666,0.0999999999999998) ;
#27399 = CIRCLE('',#72668,0.0999999999999998) ;
#27400 = CIRCLE('',#72670,0.1) ;
#27401 = CIRCLE('',#72672,0.1) ;
#27402 = CIRCLE('',#72674,0.1) ;
#27403 = CIRCLE('',#72676,0.1) ;
#27404 = CIRCLE('',#72678,0.1) ;
#27405 = CIRCLE('',#72680,0.1) ;
#27406 = CIRCLE('',#72682,0.1) ;
#27407 = CIRCLE('',#72685,0.1) ;
#27408 = CIRCLE('',#72687,0.1) ;
#27409 = CIRCLE('',#72689,0.1) ;
#27410 = CIRCLE('',#72691,0.1) ;
#27411 = CIRCLE('',#72693,0.0999999999999998) ;
#27412 = CIRCLE('',#72695,0.1) ;
#27413 = CIRCLE('',#72697,0.1) ;
#27414 = CIRCLE('',#72699,0.1) ;
#27415 = CIRCLE('',#72701,0.1) ;
#27416 = CIRCLE('',#72703,0.1) ;
#27417 = CIRCLE('',#72706,0.1) ;
#27418 = CIRCLE('',#72707,0.1) ;
#27419 = CIRCLE('',#72709,0.0999999999999998) ;
#27420 = CIRCLE('',#72711,0.1) ;
#27421 = CIRCLE('',#72713,0.1) ;
#27422 = CIRCLE('',#72715,0.0999999999999998) ;
#27423 = CIRCLE('',#72717,0.1) ;
#27424 = CIRCLE('',#72719,0.1) ;
#27425 = CIRCLE('',#72722,0.1) ;
#27426 = CIRCLE('',#72724,0.0999999999999994) ;
#27427 = CIRCLE('',#72726,0.0999999999999994) ;
#27428 = CIRCLE('',#72728,0.0999999999999994) ;
#27429 = CIRCLE('',#72730,0.1) ;
#27430 = CIRCLE('',#72732,0.1) ;
#27431 = CIRCLE('',#72734,0.1) ;
#27432 = CIRCLE('',#72736,0.1) ;
#27433 = CIRCLE('',#72738,0.0999999999999998) ;
#27434 = CIRCLE('',#72740,0.0999999999999994) ;
#27435 = CIRCLE('',#72742,0.0999999999999998) ;
#27436 = CIRCLE('',#72744,0.0999999999999998) ;
#27437 = CIRCLE('',#72746,0.1) ;
#27438 = CIRCLE('',#72748,0.1) ;
#27439 = CIRCLE('',#72750,0.1) ;
#27440 = CIRCLE('',#72752,0.1) ;
#27441 = CIRCLE('',#72754,0.0999999999999994) ;
#27442 = CIRCLE('',#72756,0.1) ;
#27443 = CIRCLE('',#72764,0.3) ;
#27444 = CIRCLE('',#72765,0.9) ;
#27445 = CIRCLE('',#72767,0.9) ;
#27446 = CIRCLE('',#72768,0.3) ;
#27447 = CIRCLE('',#72770,1.) ;
#27448 = CIRCLE('',#72771,1.) ;
#27449 = CIRCLE('',#72773,0.2) ;
#27450 = CIRCLE('',#72774,0.2) ;
#27451 = CIRCLE('',#72787,0.1) ;
#27452 = CIRCLE('',#72788,0.1) ;
#27453 = CIRCLE('',#72790,0.1) ;
#27454 = CIRCLE('',#72791,0.1) ;
#27455 = CIRCLE('',#72793,0.1) ;
#27456 = CIRCLE('',#72794,0.1) ;
#27457 = CIRCLE('',#72796,0.1) ;
#27458 = CIRCLE('',#72797,0.1) ;
#27459 = CIRCLE('',#72799,0.1) ;
#27460 = CIRCLE('',#72801,0.1) ;
#27461 = CIRCLE('',#72803,0.1) ;
#27462 = CIRCLE('',#72805,0.1) ;
#27463 = CIRCLE('',#72806,0.1) ;
#27464 = CIRCLE('',#72808,0.1) ;
#27465 = CIRCLE('',#72810,0.1) ;
#27466 = CIRCLE('',#72812,0.1) ;
#27467 = CIRCLE('',#72814,0.1) ;
#27468 = CIRCLE('',#72816,0.1) ;
#27469 = CIRCLE('',#72817,0.1) ;
#27470 = CIRCLE('',#72819,0.1) ;
#27471 = CIRCLE('',#72821,0.1) ;
#27472 = CIRCLE('',#72822,0.1) ;
#27473 = CIRCLE('',#72824,0.1) ;
#27474 = CIRCLE('',#72825,0.1) ;
#27475 = CIRCLE('',#72827,0.1) ;
#27476 = CIRCLE('',#72828,0.1) ;
#27477 = CIRCLE('',#72830,0.1) ;
#27478 = CIRCLE('',#72831,0.1) ;
#27479 = CIRCLE('',#72833,0.1) ;
#27480 = CIRCLE('',#72835,0.1) ;
#27481 = CIRCLE('',#72837,0.1) ;
#27482 = CIRCLE('',#72839,0.1) ;
#27483 = CIRCLE('',#72840,0.1) ;
#27484 = CIRCLE('',#72842,0.1) ;
#27485 = CIRCLE('',#72844,0.1) ;
#27486 = CIRCLE('',#72846,0.1) ;
#27487 = CIRCLE('',#72848,0.1) ;
#27488 = CIRCLE('',#72850,0.1) ;
#27489 = CIRCLE('',#72851,0.1) ;
#27490 = CIRCLE('',#72853,0.1) ;
#27491 = CIRCLE('',#72855,0.1) ;
#27492 = CIRCLE('',#72857,0.1) ;
#27493 = CIRCLE('',#72859,0.1) ;
#27494 = CIRCLE('',#72861,0.1) ;
#27495 = CIRCLE('',#72863,0.1) ;
#27496 = CIRCLE('',#72865,0.1) ;
#27497 = CIRCLE('',#72868,0.1) ;
#27498 = CIRCLE('',#72870,0.1) ;
#27499 = CIRCLE('',#72872,0.1) ;
#27500 = CIRCLE('',#72874,0.1) ;
#27501 = CIRCLE('',#72876,0.1) ;
#27502 = CIRCLE('',#72878,0.1) ;
#27503 = CIRCLE('',#72881,0.1) ;
#27504 = CIRCLE('',#72883,0.1) ;
#27505 = CIRCLE('',#72885,0.1) ;
#27506 = CIRCLE('',#72887,0.1) ;
#27507 = CIRCLE('',#72890,0.1) ;
#27508 = CIRCLE('',#72892,0.1) ;
#27509 = CIRCLE('',#72894,0.1) ;
#27510 = CIRCLE('',#72896,0.1) ;
#27511 = CIRCLE('',#72899,0.2) ;
#27512 = CIRCLE('',#72900,0.2) ;
#27513 = CIRCLE('',#72902,0.2) ;
#27514 = CIRCLE('',#72903,0.2) ;
#27515 = CIRCLE('',#72905,0.2) ;
#27516 = CIRCLE('',#72906,0.2) ;
#27517 = CIRCLE('',#72908,0.2) ;
#27518 = CIRCLE('',#72909,0.2) ;
#27519 = CIRCLE('',#72911,0.2) ;
#27520 = CIRCLE('',#72912,0.2) ;
#27521 = CIRCLE('',#72914,0.2) ;
#27522 = CIRCLE('',#72915,0.2) ;
#27523 = CIRCLE('',#72917,0.2) ;
#27524 = CIRCLE('',#72918,0.2) ;
#27525 = CIRCLE('',#72920,0.2) ;
#27526 = CIRCLE('',#72921,0.2) ;
#27527 = CIRCLE('',#72923,0.2) ;
#27528 = CIRCLE('',#72924,0.2) ;
#27529 = CIRCLE('',#72971,0.100000000000003) ;
#27530 = CIRCLE('',#72972,0.100000000000003) ;
#27531 = CIRCLE('',#72975,0.100000000000003) ;
#27532 = CIRCLE('',#72976,0.100000000000003) ;
#27533 = CIRCLE('',#72979,0.0999999999999959) ;
#27534 = CIRCLE('',#72980,0.0999999999999959) ;
#27535 = CIRCLE('',#72983,0.100000000000003) ;
#27536 = CIRCLE('',#72987,0.100000000000003) ;
#27537 = CIRCLE('',#72988,0.100000000000003) ;
#27538 = CIRCLE('',#72991,0.100000000000003) ;
#27539 = CIRCLE('',#72992,0.100000000000003) ;
#27540 = CIRCLE('',#72995,0.100000000000003) ;
#27541 = CIRCLE('',#72996,0.100000000000003) ;
#27542 = CIRCLE('',#72999,0.100000000000003) ;
#27543 = CIRCLE('',#73000,0.100000000000003) ;
#27544 = CIRCLE('',#73003,0.100000000000003) ;
#27545 = CIRCLE('',#73004,0.100000000000003) ;
#27546 = CIRCLE('',#73007,0.100000000000003) ;
#27547 = CIRCLE('',#73008,0.100000000000003) ;
#27548 = CIRCLE('',#73010,1.65625) ;
#27549 = CIRCLE('',#73011,1.65625) ;
#27550 = CIRCLE('',#73013,0.100000000000003) ;
#27551 = CIRCLE('',#73014,0.100000000000003) ;
#27552 = CIRCLE('',#73017,0.100000000000003) ;
#27553 = CIRCLE('',#73018,0.100000000000003) ;
#27554 = CIRCLE('',#73021,0.100000000000003) ;
#27555 = CIRCLE('',#73022,0.100000000000003) ;
#27556 = CIRCLE('',#73025,0.199999999999999) ;
#27557 = CIRCLE('',#73026,0.199999999999999) ;
#27558 = CIRCLE('',#73027,1.75625) ;
#27559 = CIRCLE('',#73028,0.199999999999999) ;
#27560 = CIRCLE('',#73029,0.199999999999999) ;
#27561 = CIRCLE('',#73031,0.0999999999999994) ;
#27562 = CIRCLE('',#73032,0.0999999999999994) ;
#27563 = CIRCLE('',#73035,0.0999999999999994) ;
#27564 = CIRCLE('',#73036,0.0999999999999994) ;
#27565 = CIRCLE('',#73039,0.0999999999999994) ;
#27566 = CIRCLE('',#73040,0.0999999999999994) ;
#27567 = CIRCLE('',#73043,0.0999999999999994) ;
#27568 = CIRCLE('',#73047,0.100000000000003) ;
#27569 = CIRCLE('',#73048,0.100000000000003) ;
#27570 = CIRCLE('',#73051,0.0999999999999994) ;
#27571 = CIRCLE('',#73052,0.0999999999999994) ;
#27572 = CIRCLE('',#73055,0.0999999999999994) ;
#27573 = CIRCLE('',#73056,0.0999999999999994) ;
#27574 = CIRCLE('',#73059,0.100000000000003) ;
#27575 = CIRCLE('',#73060,0.100000000000003) ;
#27576 = CIRCLE('',#73063,0.100000000000003) ;
#27577 = CIRCLE('',#73064,0.100000000000003) ;
#27578 = CIRCLE('',#73067,0.100000000000003) ;
#27579 = CIRCLE('',#73068,0.100000000000003) ;
#27580 = CIRCLE('',#73070,1.65625) ;
#27581 = CIRCLE('',#73071,1.65625) ;
#27582 = CIRCLE('',#73073,0.0999999999999994) ;
#27583 = CIRCLE('',#73074,0.0999999999999994) ;
#27584 = CIRCLE('',#73077,0.0999999999999994) ;
#27585 = CIRCLE('',#73078,0.0999999999999994) ;
#27586 = CIRCLE('',#73081,0.0999999999999994) ;
#27587 = CIRCLE('',#73082,0.0999999999999994) ;
#27588 = CIRCLE('',#73085,0.199999999999999) ;
#27589 = CIRCLE('',#73086,0.199999999999999) ;
#27590 = CIRCLE('',#73087,1.75625) ;
#27591 = CIRCLE('',#73088,0.199999999999999) ;
#27592 = CIRCLE('',#73089,0.199999999999999) ;
#27593 = CIRCLE('',#73091,0.0999999999999994) ;
#27594 = CIRCLE('',#73092,0.0999999999999994) ;
#27595 = CIRCLE('',#73095,0.0999999999999994) ;
#27596 = CIRCLE('',#73096,0.0999999999999994) ;
#27597 = CIRCLE('',#73099,0.0999999999999994) ;
#27598 = CIRCLE('',#73100,0.0999999999999994) ;
#27599 = CIRCLE('',#73103,0.0999999999999994) ;
#27600 = CIRCLE('',#73107,0.0999999999999994) ;
#27601 = CIRCLE('',#73108,0.0999999999999994) ;
#27602 = CIRCLE('',#73111,0.0999999999999994) ;
#27603 = CIRCLE('',#73112,0.0999999999999994) ;
#27604 = CIRCLE('',#73115,0.0999999999999994) ;
#27605 = CIRCLE('',#73116,0.0999999999999994) ;
#27606 = CIRCLE('',#73119,0.0999999999999994) ;
#27607 = CIRCLE('',#73120,0.0999999999999994) ;
#27608 = CIRCLE('',#73123,0.0999999999999994) ;
#27609 = CIRCLE('',#73124,0.0999999999999994) ;
#27610 = CIRCLE('',#73127,0.0999999999999994) ;
#27611 = CIRCLE('',#73128,0.0999999999999994) ;
#27612 = CIRCLE('',#73130,1.65625) ;
#27613 = CIRCLE('',#73131,1.65625) ;
#27614 = CIRCLE('',#73133,0.0999999999999994) ;
#27615 = CIRCLE('',#73134,0.0999999999999994) ;
#27616 = CIRCLE('',#73137,0.0999999999999994) ;
#27617 = CIRCLE('',#73138,0.0999999999999994) ;
#27618 = CIRCLE('',#73141,0.0999999999999994) ;
#27619 = CIRCLE('',#73142,0.0999999999999994) ;
#27620 = CIRCLE('',#73145,0.199999999999999) ;
#27621 = CIRCLE('',#73146,0.199999999999999) ;
#27622 = CIRCLE('',#73147,1.75625) ;
#27623 = CIRCLE('',#73148,0.199999999999999) ;
#27624 = CIRCLE('',#73149,0.199999999999999) ;
#27625 = CIRCLE('',#73151,0.0999999999999994) ;
#27626 = CIRCLE('',#73152,0.0999999999999994) ;
#27627 = CIRCLE('',#73155,0.0999999999999994) ;
#27628 = CIRCLE('',#73156,0.0999999999999994) ;
#27629 = CIRCLE('',#73159,0.0999999999999994) ;
#27630 = CIRCLE('',#73160,0.0999999999999994) ;
#27631 = CIRCLE('',#73163,0.0999999999999994) ;
#27632 = CIRCLE('',#73167,0.0999999999999994) ;
#27633 = CIRCLE('',#73168,0.0999999999999994) ;
#27634 = CIRCLE('',#73171,0.0999999999999994) ;
#27635 = CIRCLE('',#73172,0.0999999999999994) ;
#27636 = CIRCLE('',#73175,0.0999999999999994) ;
#27637 = CIRCLE('',#73176,0.0999999999999994) ;
#27638 = CIRCLE('',#73179,0.0999999999999994) ;
#27639 = CIRCLE('',#73180,0.0999999999999994) ;
#27640 = CIRCLE('',#73183,0.0999999999999994) ;
#27641 = CIRCLE('',#73184,0.0999999999999994) ;
#27642 = CIRCLE('',#73187,0.0999999999999994) ;
#27643 = CIRCLE('',#73188,0.0999999999999994) ;
#27644 = CIRCLE('',#73190,1.65625) ;
#27645 = CIRCLE('',#73191,1.65625) ;
#27646 = CIRCLE('',#73193,0.0999999999999994) ;
#27647 = CIRCLE('',#73194,0.0999999999999994) ;
#27648 = CIRCLE('',#73197,0.0999999999999994) ;
#27649 = CIRCLE('',#73198,0.0999999999999994) ;
#27650 = CIRCLE('',#73201,0.0999999999999994) ;
#27651 = CIRCLE('',#73202,0.0999999999999994) ;
#27652 = CIRCLE('',#73205,0.199999999999999) ;
#27653 = CIRCLE('',#73206,0.199999999999999) ;
#27654 = CIRCLE('',#73207,1.75625) ;
#27655 = CIRCLE('',#73208,0.199999999999999) ;
#27656 = CIRCLE('',#73209,0.199999999999999) ;
#27657 = CIRCLE('',#73211,0.0999999999999994) ;
#27658 = CIRCLE('',#73212,0.0999999999999994) ;
#27659 = CIRCLE('',#73215,0.0999999999999994) ;
#27660 = CIRCLE('',#73216,0.0999999999999994) ;
#27661 = CIRCLE('',#73219,0.0999999999999994) ;
#27662 = CIRCLE('',#73220,0.0999999999999994) ;
#27663 = CIRCLE('',#73223,0.0999999999999994) ;
#27664 = CIRCLE('',#73227,0.0999999999999994) ;
#27665 = CIRCLE('',#73228,0.0999999999999994) ;
#27666 = CIRCLE('',#73231,0.0999999999999994) ;
#27667 = CIRCLE('',#73232,0.0999999999999994) ;
#27668 = CIRCLE('',#73235,0.0999999999999994) ;
#27669 = CIRCLE('',#73236,0.0999999999999994) ;
#27670 = CIRCLE('',#73239,0.0999999999999994) ;
#27671 = CIRCLE('',#73240,0.0999999999999994) ;
#27672 = CIRCLE('',#73243,0.0999999999999994) ;
#27673 = CIRCLE('',#73244,0.0999999999999994) ;
#27674 = CIRCLE('',#73247,0.0999999999999994) ;
#27675 = CIRCLE('',#73248,0.0999999999999994) ;
#27676 = CIRCLE('',#73250,1.65625) ;
#27677 = CIRCLE('',#73251,1.65625) ;
#27678 = CIRCLE('',#73253,0.0999999999999994) ;
#27679 = CIRCLE('',#73254,0.0999999999999994) ;
#27680 = CIRCLE('',#73257,0.0999999999999994) ;
#27681 = CIRCLE('',#73258,0.0999999999999994) ;
#27682 = CIRCLE('',#73261,0.0999999999999994) ;
#27683 = CIRCLE('',#73262,0.0999999999999994) ;
#27684 = CIRCLE('',#73265,0.199999999999999) ;
#27685 = CIRCLE('',#73266,0.199999999999999) ;
#27686 = CIRCLE('',#73267,1.75625) ;
#27687 = CIRCLE('',#73268,0.199999999999999) ;
#27688 = CIRCLE('',#73269,0.199999999999999) ;
#27689 = CIRCLE('',#73271,0.0999999999999994) ;
#27690 = CIRCLE('',#73272,0.0999999999999994) ;
#27691 = CIRCLE('',#73275,0.0999999999999994) ;
#27692 = CIRCLE('',#73276,0.0999999999999994) ;
#27693 = CIRCLE('',#73279,0.0999999999999994) ;
#27694 = CIRCLE('',#73280,0.0999999999999994) ;
#27695 = CIRCLE('',#73283,0.100000000000001) ;
#27696 = CIRCLE('',#73287,0.0999999999999994) ;
#27697 = CIRCLE('',#73288,0.0999999999999994) ;
#27698 = CIRCLE('',#73291,0.0999999999999994) ;
#27699 = CIRCLE('',#73292,0.0999999999999994) ;
#27700 = CIRCLE('',#73295,0.0999999999999994) ;
#27701 = CIRCLE('',#73296,0.0999999999999994) ;
#27702 = CIRCLE('',#73299,0.0999999999999994) ;
#27703 = CIRCLE('',#73300,0.0999999999999994) ;
#27704 = CIRCLE('',#73303,0.0999999999999994) ;
#27705 = CIRCLE('',#73304,0.0999999999999994) ;
#27706 = CIRCLE('',#73307,0.0999999999999994) ;
#27707 = CIRCLE('',#73308,0.0999999999999994) ;
#27708 = CIRCLE('',#73310,1.65625) ;
#27709 = CIRCLE('',#73311,1.65625) ;
#27710 = CIRCLE('',#73313,0.0999999999999994) ;
#27711 = CIRCLE('',#73314,0.0999999999999994) ;
#27712 = CIRCLE('',#73317,0.0999999999999994) ;
#27713 = CIRCLE('',#73318,0.0999999999999994) ;
#27714 = CIRCLE('',#73321,0.0999999999999994) ;
#27715 = CIRCLE('',#73322,0.0999999999999994) ;
#27716 = CIRCLE('',#73325,0.200000000000001) ;
#27717 = CIRCLE('',#73326,0.200000000000001) ;
#27718 = CIRCLE('',#73327,1.75625) ;
#27719 = CIRCLE('',#73328,0.199999999999999) ;
#27720 = CIRCLE('',#73329,0.199999999999999) ;
#27721 = CIRCLE('',#73331,0.0999999999999994) ;
#27722 = CIRCLE('',#73332,0.0999999999999994) ;
#27723 = CIRCLE('',#73335,0.0999999999999994) ;
#27724 = CIRCLE('',#73336,0.0999999999999994) ;
#27725 = CIRCLE('',#73339,0.0999999999999994) ;
#27726 = CIRCLE('',#73340,0.0999999999999994) ;
#27727 = CIRCLE('',#73343,0.100000000000001) ;
#27728 = CIRCLE('',#73347,0.100000000000001) ;
#27729 = CIRCLE('',#73348,0.100000000000001) ;
#27730 = CIRCLE('',#73351,0.0999999999999994) ;
#27731 = CIRCLE('',#73352,0.0999999999999994) ;
#27732 = CIRCLE('',#73355,0.0999999999999994) ;
#27733 = CIRCLE('',#73356,0.0999999999999994) ;
#27734 = CIRCLE('',#73359,0.0999999999999994) ;
#27735 = CIRCLE('',#73360,0.0999999999999994) ;
#27736 = CIRCLE('',#73363,0.0999999999999994) ;
#27737 = CIRCLE('',#73364,0.0999999999999994) ;
#27738 = CIRCLE('',#73367,0.0999999999999994) ;
#27739 = CIRCLE('',#73368,0.0999999999999994) ;
#27740 = CIRCLE('',#73370,1.65625) ;
#27741 = CIRCLE('',#73371,1.65625) ;
#27742 = CIRCLE('',#73373,0.0999999999999994) ;
#27743 = CIRCLE('',#73374,0.0999999999999994) ;
#27744 = CIRCLE('',#73377,0.0999999999999994) ;
#27745 = CIRCLE('',#73378,0.0999999999999994) ;
#27746 = CIRCLE('',#73381,0.0999999999999994) ;
#27747 = CIRCLE('',#73382,0.0999999999999994) ;
#27748 = CIRCLE('',#73385,0.200000000000001) ;
#27749 = CIRCLE('',#73386,0.200000000000001) ;
#27750 = CIRCLE('',#73387,1.75625) ;
#27751 = CIRCLE('',#73388,0.200000000000001) ;
#27752 = CIRCLE('',#73389,0.200000000000001) ;
#27753 = CIRCLE('',#73391,0.1) ;
#27754 = CIRCLE('',#73392,0.1) ;
#27755 = CIRCLE('',#73395,0.1) ;
#27756 = CIRCLE('',#73396,0.1) ;
#27757 = CIRCLE('',#73399,0.0999999999999994) ;
#27758 = CIRCLE('',#73400,0.0999999999999994) ;
#27759 = CIRCLE('',#73403,0.1) ;
#27760 = CIRCLE('',#73407,0.100000000000001) ;
#27761 = CIRCLE('',#73408,0.100000000000001) ;
#27762 = CIRCLE('',#73411,0.0999999999999994) ;
#27763 = CIRCLE('',#73412,0.0999999999999994) ;
#27764 = CIRCLE('',#73415,0.0999999999999994) ;
#27765 = CIRCLE('',#73416,0.0999999999999994) ;
#27766 = CIRCLE('',#73419,0.0999999999999994) ;
#27767 = CIRCLE('',#73420,0.0999999999999994) ;
#27768 = CIRCLE('',#73423,0.0999999999999994) ;
#27769 = CIRCLE('',#73424,0.0999999999999994) ;
#27770 = CIRCLE('',#73427,0.0999999999999994) ;
#27771 = CIRCLE('',#73428,0.0999999999999994) ;
#27772 = CIRCLE('',#73430,1.65625) ;
#27773 = CIRCLE('',#73431,1.65625) ;
#27774 = CIRCLE('',#73433,0.1) ;
#27775 = CIRCLE('',#73434,0.1) ;
#27776 = CIRCLE('',#73437,0.1) ;
#27777 = CIRCLE('',#73438,0.1) ;
#27778 = CIRCLE('',#73441,0.1) ;
#27779 = CIRCLE('',#73442,0.1) ;
#27780 = CIRCLE('',#73445,0.2) ;
#27781 = CIRCLE('',#73446,0.2) ;
#27782 = CIRCLE('',#73447,1.75625) ;
#27783 = CIRCLE('',#73448,0.200000000000001) ;
#27784 = CIRCLE('',#73449,0.200000000000001) ;
#27785 = CIRCLE('',#73451,0.0999999999999998) ;
#27786 = CIRCLE('',#73452,0.0999999999999998) ;
#27787 = CIRCLE('',#73455,0.0999999999999998) ;
#27788 = CIRCLE('',#73456,0.0999999999999998) ;
#27789 = CIRCLE('',#73459,0.0999999999999994) ;
#27790 = CIRCLE('',#73460,0.0999999999999994) ;
#27791 = CIRCLE('',#73463,0.100000000000001) ;
#27792 = CIRCLE('',#73467,0.1) ;
#27793 = CIRCLE('',#73468,0.1) ;
#27794 = CIRCLE('',#73471,0.1) ;
#27795 = CIRCLE('',#73472,0.1) ;
#27796 = CIRCLE('',#73475,0.1) ;
#27797 = CIRCLE('',#73476,0.1) ;
#27798 = CIRCLE('',#73479,0.1) ;
#27799 = CIRCLE('',#73480,0.1) ;
#27800 = CIRCLE('',#73483,0.1) ;
#27801 = CIRCLE('',#73484,0.1) ;
#27802 = CIRCLE('',#73487,0.1) ;
#27803 = CIRCLE('',#73488,0.1) ;
#27804 = CIRCLE('',#73490,1.65625) ;
#27805 = CIRCLE('',#73491,1.65625) ;
#27806 = CIRCLE('',#73493,0.0999999999999998) ;
#27807 = CIRCLE('',#73494,0.0999999999999998) ;
#27808 = CIRCLE('',#73497,0.0999999999999998) ;
#27809 = CIRCLE('',#73498,0.0999999999999998) ;
#27810 = CIRCLE('',#73501,0.1) ;
#27811 = CIRCLE('',#73502,0.1) ;
#27812 = CIRCLE('',#73505,0.2) ;
#27813 = CIRCLE('',#73506,0.2) ;
#27814 = CIRCLE('',#73507,1.75625) ;
#27815 = CIRCLE('',#73508,0.2) ;
#27816 = CIRCLE('',#73509,0.2) ;
#27817 = CIRCLE('',#73511,0.0999999999999998) ;
#27818 = CIRCLE('',#73512,0.1) ;
#27819 = CIRCLE('',#73513,0.1) ;
#27820 = CIRCLE('',#73514,0.0999999999999998) ;
#27821 = CIRCLE('',#73516,0.1) ;
#27822 = CIRCLE('',#73517,0.0999999999999994) ;
#27823 = CIRCLE('',#73518,0.0999999999999994) ;
#27824 = CIRCLE('',#73519,0.1) ;
#27825 = CIRCLE('',#73521,0.0999999999999994) ;
#27826 = CIRCLE('',#73522,0.0999999999999994) ;
#27827 = CIRCLE('',#73523,0.0999999999999994) ;
#27828 = CIRCLE('',#73524,0.0999999999999994) ;
#27829 = CIRCLE('',#73526,0.0999999999999994) ;
#27830 = CIRCLE('',#73527,0.0999999999999994) ;
#27831 = CIRCLE('',#73528,0.0999999999999994) ;
#27832 = CIRCLE('',#73529,0.0999999999999994) ;
#27833 = CIRCLE('',#73531,0.0999999999999994) ;
#27834 = CIRCLE('',#73532,0.0999999999999994) ;
#27835 = CIRCLE('',#73533,0.0999999999999994) ;
#27836 = CIRCLE('',#73534,0.0999999999999994) ;
#27837 = CIRCLE('',#73536,0.0999999999999994) ;
#27838 = CIRCLE('',#73537,0.0999999999999994) ;
#27839 = CIRCLE('',#73538,0.0999999999999994) ;
#27840 = CIRCLE('',#73539,0.0999999999999994) ;
#27841 = CIRCLE('',#73541,0.0999999999999994) ;
#27842 = CIRCLE('',#73542,0.0999999999999994) ;
#27843 = CIRCLE('',#73543,0.0999999999999994) ;
#27844 = CIRCLE('',#73544,0.0999999999999994) ;
#27845 = CIRCLE('',#73546,0.0999999999999994) ;
#27846 = CIRCLE('',#73547,0.0999999999999994) ;
#27847 = CIRCLE('',#73548,0.0999999999999994) ;
#27848 = CIRCLE('',#73549,0.0999999999999994) ;
#27849 = CIRCLE('',#73551,0.100000000000003) ;
#27850 = CIRCLE('',#73552,0.100000000000003) ;
#27851 = CIRCLE('',#73553,0.100000000000003) ;
#27852 = CIRCLE('',#73554,0.100000000000003) ;
#27853 = CIRCLE('',#73556,0.0999999999999998) ;
#27854 = CIRCLE('',#73557,0.0999999999999998) ;
#27855 = CIRCLE('',#73559,0.0999999999999998) ;
#27856 = CIRCLE('',#73560,0.1) ;
#27857 = CIRCLE('',#73562,0.0999999999999998) ;
#27858 = CIRCLE('',#73563,0.1) ;
#27859 = CIRCLE('',#73565,0.1) ;
#27860 = CIRCLE('',#73566,0.0999999999999998) ;
#27861 = CIRCLE('',#73568,0.1) ;
#27862 = CIRCLE('',#73570,0.1) ;
#27863 = CIRCLE('',#73572,0.0999999999999998) ;
#27864 = CIRCLE('',#73574,0.1) ;
#27865 = CIRCLE('',#73576,0.0999999999999998) ;
#27866 = CIRCLE('',#73578,0.1) ;
#27867 = CIRCLE('',#73580,0.1) ;
#27868 = CIRCLE('',#73581,0.1) ;
#27869 = CIRCLE('',#73584,0.1) ;
#27870 = CIRCLE('',#73586,0.0999999999999998) ;
#27871 = CIRCLE('',#73587,0.0999999999999998) ;
#27872 = CIRCLE('',#73589,0.1) ;
#27873 = CIRCLE('',#73591,0.1) ;
#27874 = CIRCLE('',#73593,0.0999999999999998) ;
#27875 = CIRCLE('',#73595,0.0999999999999998) ;
#27876 = CIRCLE('',#73597,0.1) ;
#27877 = CIRCLE('',#73599,0.1) ;
#27878 = CIRCLE('',#73600,0.1) ;
#27879 = CIRCLE('',#73602,0.1) ;
#27880 = CIRCLE('',#73604,0.0999999999999998) ;
#27881 = CIRCLE('',#73606,0.0999999999999998) ;
#27882 = CIRCLE('',#73607,0.1) ;
#27883 = CIRCLE('',#73609,0.0999999999999998) ;
#27884 = CIRCLE('',#73611,0.1) ;
#27885 = CIRCLE('',#73612,0.1) ;
#27886 = CIRCLE('',#73614,0.1) ;
#27887 = CIRCLE('',#73616,0.1) ;
#27888 = CIRCLE('',#73618,0.0999999999999998) ;
#27889 = CIRCLE('',#73620,0.0999999999999998) ;
#27890 = CIRCLE('',#73622,0.1) ;
#27891 = CIRCLE('',#73624,0.1) ;
#27892 = CIRCLE('',#73626,0.1) ;
#27893 = CIRCLE('',#73628,0.1) ;
#27894 = CIRCLE('',#73629,0.1) ;
#27895 = CIRCLE('',#73631,0.1) ;
#27896 = CIRCLE('',#73633,0.1) ;
#27897 = CIRCLE('',#73635,0.1) ;
#27898 = CIRCLE('',#73637,0.1) ;
#27899 = CIRCLE('',#73638,0.1) ;
#27900 = CIRCLE('',#73640,0.1) ;
#27901 = CIRCLE('',#73642,0.1) ;
#27902 = CIRCLE('',#73644,0.1) ;
#27903 = CIRCLE('',#73646,0.1) ;
#27904 = CIRCLE('',#73649,0.1) ;
#27905 = CIRCLE('',#73651,0.1) ;
#27906 = CIRCLE('',#73653,0.1) ;
#27907 = CIRCLE('',#73656,0.1) ;
#27908 = CIRCLE('',#73657,0.1) ;
#27909 = CIRCLE('',#73659,0.1) ;
#27910 = CIRCLE('',#73661,0.1) ;
#27911 = CIRCLE('',#73663,0.1) ;
#27912 = CIRCLE('',#73665,0.1) ;
#27913 = CIRCLE('',#73667,0.1) ;
#27914 = CIRCLE('',#73669,0.1) ;
#27915 = CIRCLE('',#73671,0.1) ;
#27916 = CIRCLE('',#73673,0.1) ;
#27917 = CIRCLE('',#73675,0.1) ;
#27918 = CIRCLE('',#73677,0.1) ;
#27919 = CIRCLE('',#73679,0.0999999999999998) ;
#27920 = CIRCLE('',#73681,0.1) ;
#27921 = CIRCLE('',#73683,0.1) ;
#27922 = CIRCLE('',#73685,0.1) ;
#27923 = CIRCLE('',#73688,0.1) ;
#27924 = CIRCLE('',#73690,0.0999999999999998) ;
#27925 = CIRCLE('',#73692,0.0999999999999998) ;
#27926 = CIRCLE('',#73694,0.0999999999999998) ;
#27927 = CIRCLE('',#73696,0.1) ;
#27928 = CIRCLE('',#73698,0.1) ;
#27929 = CIRCLE('',#73700,0.1) ;
#27930 = CIRCLE('',#73702,0.1) ;
#27931 = CIRCLE('',#73704,0.0999999999999998) ;
#27932 = CIRCLE('',#73706,0.0999999999999998) ;
#27933 = CIRCLE('',#73709,0.100000000000003) ;
#27934 = CIRCLE('',#73710,0.100000000000003) ;
#27935 = CIRCLE('',#73712,0.1) ;
#27936 = CIRCLE('',#73714,0.1) ;
#27937 = CIRCLE('',#73716,0.1) ;
#27938 = CIRCLE('',#73718,0.0999999999999998) ;
#27939 = CIRCLE('',#73720,0.0999999999999998) ;
#27940 = CIRCLE('',#73722,0.100000000000003) ;
#27941 = CIRCLE('',#73725,0.100000000000003) ;
#27942 = CIRCLE('',#73727,0.0999999999999994) ;
#27943 = CIRCLE('',#73729,0.0999999999999994) ;
#27944 = CIRCLE('',#73731,0.0999999999999994) ;
#27945 = CIRCLE('',#73733,0.0999999999999998) ;
#27946 = CIRCLE('',#73735,0.1) ;
#27947 = CIRCLE('',#73737,0.0999999999999995) ;
#27948 = CIRCLE('',#73739,0.1) ;
#27949 = CIRCLE('',#73741,0.1) ;
#27950 = CIRCLE('',#73743,0.0999999999999994) ;
#27951 = CIRCLE('',#73745,0.1) ;
#27952 = CIRCLE('',#73747,0.0999999999999998) ;
#27953 = CIRCLE('',#73749,0.100000000000003) ;
#27954 = CIRCLE('',#73751,0.100000000000003) ;
#27955 = CIRCLE('',#73753,0.100000000000003) ;
#27956 = CIRCLE('',#73755,0.100000000000003) ;
#27957 = CIRCLE('',#73757,0.0999999999999994) ;
#27958 = CIRCLE('',#73759,0.1) ;
#27959 = CIRCLE('',#73762,0.0999999999999994) ;
#27960 = CIRCLE('',#73763,0.0999999999999994) ;
#27961 = CIRCLE('',#73765,0.1) ;
#27962 = CIRCLE('',#73767,0.1) ;
#27963 = CIRCLE('',#73769,0.1) ;
#27964 = CIRCLE('',#73771,0.1) ;
#27965 = CIRCLE('',#73773,0.0999999999999998) ;
#27966 = CIRCLE('',#73775,0.100000000000003) ;
#27967 = CIRCLE('',#73778,0.100000000000003) ;
#27968 = CIRCLE('',#73780,0.0999999999999994) ;
#27969 = CIRCLE('',#73782,0.0999999999999994) ;
#27970 = CIRCLE('',#73784,0.0999999999999994) ;
#27971 = CIRCLE('',#73786,0.1) ;
#27972 = CIRCLE('',#73788,0.1) ;
#27973 = CIRCLE('',#73790,0.0999999999999995) ;
#27974 = CIRCLE('',#73792,0.1) ;
#27975 = CIRCLE('',#73794,0.1) ;
#27976 = CIRCLE('',#73796,0.0999999999999994) ;
#27977 = CIRCLE('',#73798,0.1) ;
#27978 = CIRCLE('',#73800,0.0999999999999994) ;
#27979 = CIRCLE('',#73802,0.0999999999999994) ;
#27980 = CIRCLE('',#73804,0.0999999999999994) ;
#27981 = CIRCLE('',#73806,0.0999999999999994) ;
#27982 = CIRCLE('',#73808,0.0999999999999994) ;
#27983 = CIRCLE('',#73810,0.0999999999999994) ;
#27984 = CIRCLE('',#73812,0.1) ;
#27985 = CIRCLE('',#73815,0.0999999999999994) ;
#27986 = CIRCLE('',#73816,0.0999999999999994) ;
#27987 = CIRCLE('',#73818,0.1) ;
#27988 = CIRCLE('',#73820,0.1) ;
#27989 = CIRCLE('',#73822,0.1) ;
#27990 = CIRCLE('',#73824,0.1) ;
#27991 = CIRCLE('',#73826,0.1) ;
#27992 = CIRCLE('',#73828,0.0999999999999994) ;
#27993 = CIRCLE('',#73831,0.0999999999999994) ;
#27994 = CIRCLE('',#73833,0.0999999999999994) ;
#27995 = CIRCLE('',#73835,0.0999999999999994) ;
#27996 = CIRCLE('',#73837,0.0999999999999994) ;
#27997 = CIRCLE('',#73839,0.1) ;
#27998 = CIRCLE('',#73841,0.1) ;
#27999 = CIRCLE('',#73843,0.0999999999999995) ;
#28000 = CIRCLE('',#73845,0.1) ;
#28001 = CIRCLE('',#73847,0.1) ;
#28002 = CIRCLE('',#73849,0.0999999999999994) ;
#28003 = CIRCLE('',#73851,0.1) ;
#28004 = CIRCLE('',#73853,0.0999999999999994) ;
#28005 = CIRCLE('',#73855,0.0999999999999994) ;
#28006 = CIRCLE('',#73857,0.0999999999999994) ;
#28007 = CIRCLE('',#73859,0.0999999999999994) ;
#28008 = CIRCLE('',#73861,0.0999999999999994) ;
#28009 = CIRCLE('',#73863,0.0999999999999994) ;
#28010 = CIRCLE('',#73865,0.1) ;
#28011 = CIRCLE('',#73868,0.0999999999999994) ;
#28012 = CIRCLE('',#73869,0.0999999999999994) ;
#28013 = CIRCLE('',#73871,0.1) ;
#28014 = CIRCLE('',#73873,0.1) ;
#28015 = CIRCLE('',#73875,0.1) ;
#28016 = CIRCLE('',#73877,0.1) ;
#28017 = CIRCLE('',#73879,0.1) ;
#28018 = CIRCLE('',#73881,0.0999999999999994) ;
#28019 = CIRCLE('',#73884,0.0999999999999994) ;
#28020 = CIRCLE('',#73886,0.0999999999999994) ;
#28021 = CIRCLE('',#73888,0.0999999999999994) ;
#28022 = CIRCLE('',#73890,0.0999999999999994) ;
#28023 = CIRCLE('',#73892,0.1) ;
#28024 = CIRCLE('',#73894,0.1) ;
#28025 = CIRCLE('',#73896,0.0999999999999995) ;
#28026 = CIRCLE('',#73898,0.1) ;
#28027 = CIRCLE('',#73900,0.1) ;
#28028 = CIRCLE('',#73902,0.0999999999999994) ;
#28029 = CIRCLE('',#73904,0.1) ;
#28030 = CIRCLE('',#73906,0.0999999999999994) ;
#28031 = CIRCLE('',#73908,0.0999999999999994) ;
#28032 = CIRCLE('',#73910,0.0999999999999994) ;
#28033 = CIRCLE('',#73912,0.0999999999999994) ;
#28034 = CIRCLE('',#73914,0.0999999999999994) ;
#28035 = CIRCLE('',#73916,0.0999999999999994) ;
#28036 = CIRCLE('',#73918,0.1) ;
#28037 = CIRCLE('',#73921,0.0999999999999994) ;
#28038 = CIRCLE('',#73922,0.0999999999999994) ;
#28039 = CIRCLE('',#73924,0.1) ;
#28040 = CIRCLE('',#73926,0.1) ;
#28041 = CIRCLE('',#73928,0.1) ;
#28042 = CIRCLE('',#73930,0.1) ;
#28043 = CIRCLE('',#73932,0.1) ;
#28044 = CIRCLE('',#73934,0.0999999999999994) ;
#28045 = CIRCLE('',#73937,0.0999999999999994) ;
#28046 = CIRCLE('',#73939,0.0999999999999994) ;
#28047 = CIRCLE('',#73941,0.0999999999999994) ;
#28048 = CIRCLE('',#73943,0.0999999999999994) ;
#28049 = CIRCLE('',#73945,0.1) ;
#28050 = CIRCLE('',#73947,0.1) ;
#28051 = CIRCLE('',#73949,0.0999999999999995) ;
#28052 = CIRCLE('',#73951,0.1) ;
#28053 = CIRCLE('',#73953,0.1) ;
#28054 = CIRCLE('',#73955,0.0999999999999994) ;
#28055 = CIRCLE('',#73957,0.1) ;
#28056 = CIRCLE('',#73959,0.0999999999999994) ;
#28057 = CIRCLE('',#73961,0.0999999999999994) ;
#28058 = CIRCLE('',#73963,0.0999999999999994) ;
#28059 = CIRCLE('',#73965,0.0999999999999994) ;
#28060 = CIRCLE('',#73967,0.0999999999999994) ;
#28061 = CIRCLE('',#73969,0.0999999999999994) ;
#28062 = CIRCLE('',#73971,0.1) ;
#28063 = CIRCLE('',#73974,0.0999999999999994) ;
#28064 = CIRCLE('',#73975,0.0999999999999994) ;
#28065 = CIRCLE('',#73977,0.1) ;
#28066 = CIRCLE('',#73979,0.1) ;
#28067 = CIRCLE('',#73981,0.1) ;
#28068 = CIRCLE('',#73983,0.1) ;
#28069 = CIRCLE('',#73985,0.1) ;
#28070 = CIRCLE('',#73987,0.0999999999999994) ;
#28071 = CIRCLE('',#73990,0.0999999999999994) ;
#28072 = CIRCLE('',#73992,0.0999999999999994) ;
#28073 = CIRCLE('',#73994,0.0999999999999994) ;
#28074 = CIRCLE('',#73996,0.0999999999999994) ;
#28075 = CIRCLE('',#73998,0.1) ;
#28076 = CIRCLE('',#74000,0.1) ;
#28077 = CIRCLE('',#74002,0.1) ;
#28078 = CIRCLE('',#74004,0.1) ;
#28079 = CIRCLE('',#74006,0.1) ;
#28080 = CIRCLE('',#74008,0.0999999999999994) ;
#28081 = CIRCLE('',#74010,0.1) ;
#28082 = CIRCLE('',#74012,0.0999999999999994) ;
#28083 = CIRCLE('',#74014,0.0999999999999994) ;
#28084 = CIRCLE('',#74016,0.0999999999999994) ;
#28085 = CIRCLE('',#74018,0.0999999999999994) ;
#28086 = CIRCLE('',#74020,0.0999999999999994) ;
#28087 = CIRCLE('',#74022,0.0999999999999994) ;
#28088 = CIRCLE('',#74024,0.1) ;
#28089 = CIRCLE('',#74027,0.0999999999999994) ;
#28090 = CIRCLE('',#74028,0.0999999999999994) ;
#28091 = CIRCLE('',#74030,0.1) ;
#28092 = CIRCLE('',#74032,0.1) ;
#28093 = CIRCLE('',#74034,0.1) ;
#28094 = CIRCLE('',#74036,0.1) ;
#28095 = CIRCLE('',#74038,0.1) ;
#28096 = CIRCLE('',#74040,0.0999999999999994) ;
#28097 = CIRCLE('',#74043,0.0999999999999994) ;
#28098 = CIRCLE('',#74045,0.0999999999999994) ;
#28099 = CIRCLE('',#74047,0.0999999999999994) ;
#28100 = CIRCLE('',#74049,0.0999999999999994) ;
#28101 = CIRCLE('',#74051,0.1) ;
#28102 = CIRCLE('',#74053,0.1) ;
#28103 = CIRCLE('',#74055,0.1) ;
#28104 = CIRCLE('',#74057,0.1) ;
#28105 = CIRCLE('',#74059,0.1) ;
#28106 = CIRCLE('',#74061,0.0999999999999994) ;
#28107 = CIRCLE('',#74063,0.1) ;
#28108 = CIRCLE('',#74065,0.0999999999999994) ;
#28109 = CIRCLE('',#74067,0.0999999999999994) ;
#28110 = CIRCLE('',#74069,0.0999999999999994) ;
#28111 = CIRCLE('',#74071,0.0999999999999994) ;
#28112 = CIRCLE('',#74073,0.0999999999999994) ;
#28113 = CIRCLE('',#74075,0.0999999999999994) ;
#28114 = CIRCLE('',#74077,0.1) ;
#28115 = CIRCLE('',#74080,0.0999999999999994) ;
#28116 = CIRCLE('',#74081,0.0999999999999994) ;
#28117 = CIRCLE('',#74083,0.1) ;
#28118 = CIRCLE('',#74085,0.1) ;
#28119 = CIRCLE('',#74087,0.1) ;
#28120 = CIRCLE('',#74089,0.1) ;
#28121 = CIRCLE('',#74091,0.1) ;
#28122 = CIRCLE('',#74093,0.0999999999999994) ;
#28123 = CIRCLE('',#74096,0.0999999999999994) ;
#28124 = CIRCLE('',#74098,0.0999999999999994) ;
#28125 = CIRCLE('',#74100,0.0999999999999994) ;
#28126 = CIRCLE('',#74102,0.0999999999999994) ;
#28127 = CIRCLE('',#74104,0.1) ;
#28128 = CIRCLE('',#74106,0.1) ;
#28129 = CIRCLE('',#74108,0.1) ;
#28130 = CIRCLE('',#74110,0.1) ;
#28131 = CIRCLE('',#74112,0.0999999999999998) ;
#28132 = CIRCLE('',#74114,0.0999999999999994) ;
#28133 = CIRCLE('',#74116,0.1) ;
#28134 = CIRCLE('',#74118,0.0999999999999994) ;
#28135 = CIRCLE('',#74120,0.1) ;
#28136 = CIRCLE('',#74122,0.1) ;
#28137 = CIRCLE('',#74124,0.1) ;
#28138 = CIRCLE('',#74126,0.1) ;
#28139 = CIRCLE('',#74128,0.0999999999999994) ;
#28140 = CIRCLE('',#74130,0.1) ;
#28141 = CIRCLE('',#74133,0.1) ;
#28142 = CIRCLE('',#74134,0.1) ;
#28143 = CIRCLE('',#74136,0.1) ;
#28144 = CIRCLE('',#74138,0.1) ;
#28145 = CIRCLE('',#74140,0.1) ;
#28146 = CIRCLE('',#74142,0.0999999999999998) ;
#28147 = CIRCLE('',#74144,0.1) ;
#28148 = CIRCLE('',#74146,0.1) ;
#28149 = CIRCLE('',#74149,0.1) ;
#28150 = CIRCLE('',#74151,0.0999999999999994) ;
#28151 = CIRCLE('',#74153,0.0999999999999994) ;
#28152 = CIRCLE('',#74155,0.0999999999999994) ;
#28153 = CIRCLE('',#74157,0.0999999999999998) ;
#28154 = CIRCLE('',#74159,0.1) ;
#28155 = CIRCLE('',#74161,0.0999999999999998) ;
#28156 = CIRCLE('',#74163,0.1) ;
#28157 = CIRCLE('',#74165,0.1) ;
#28158 = CIRCLE('',#74167,0.0999999999999994) ;
#28159 = CIRCLE('',#74169,0.0999999999999998) ;
#28160 = CIRCLE('',#74171,0.0999999999999998) ;
#28161 = CIRCLE('',#74173,0.0999999999999998) ;
#28162 = CIRCLE('',#74175,0.0999999999999998) ;
#28163 = CIRCLE('',#74177,0.0999999999999998) ;
#28164 = CIRCLE('',#74179,0.0999999999999998) ;
#28165 = CIRCLE('',#74181,0.0999999999999994) ;
#28166 = CIRCLE('',#74183,0.1) ;
#28167 = CIRCLE('',#74186,0.1) ;
#28168 = CIRCLE('',#74187,0.1) ;
#28169 = CIRCLE('',#74189,0.1) ;
#28170 = CIRCLE('',#74190,0.1) ;
#28171 = CIRCLE('',#74192,0.1) ;
#28172 = CIRCLE('',#74193,0.1) ;
#28173 = CIRCLE('',#74195,0.1) ;
#28174 = CIRCLE('',#74196,0.0999999999999998) ;
#28175 = CIRCLE('',#74198,0.1) ;
#28176 = CIRCLE('',#74200,0.1) ;
#28177 = CIRCLE('',#74202,0.1) ;
#28178 = CIRCLE('',#74204,0.1) ;
#28179 = CIRCLE('',#74206,0.0999999999999998) ;
#28180 = CIRCLE('',#74208,0.1) ;
#28181 = CIRCLE('',#74210,0.0999999999999994) ;
#28182 = CIRCLE('',#74211,0.1) ;
#28183 = CIRCLE('',#74214,0.1) ;
#28184 = CIRCLE('',#74216,0.1) ;
#28185 = CIRCLE('',#74217,0.1) ;
#28186 = CIRCLE('',#74219,0.0999999999999994) ;
#28187 = CIRCLE('',#74221,0.1) ;
#28188 = CIRCLE('',#74223,0.1) ;
#28189 = CIRCLE('',#74225,0.1) ;
#28190 = CIRCLE('',#74227,0.0999999999999994) ;
#28191 = CIRCLE('',#74229,0.1) ;
#28192 = CIRCLE('',#74230,0.0999999999999994) ;
#28193 = CIRCLE('',#74232,0.1) ;
#28194 = CIRCLE('',#74234,0.1) ;
#28195 = CIRCLE('',#74236,0.0999999999999998) ;
#28196 = CIRCLE('',#74237,0.1) ;
#28197 = CIRCLE('',#74239,0.1) ;
#28198 = CIRCLE('',#74241,0.1) ;
#28199 = CIRCLE('',#74242,0.1) ;
#28200 = CIRCLE('',#74244,0.1) ;
#28201 = CIRCLE('',#74246,0.1) ;
#28202 = CIRCLE('',#74248,0.1) ;
#28203 = CIRCLE('',#74250,0.1) ;
#28204 = CIRCLE('',#74252,0.1) ;
#28205 = CIRCLE('',#74254,0.1) ;
#28206 = CIRCLE('',#74256,0.1) ;
#28207 = CIRCLE('',#74258,0.0999999999999994) ;
#28208 = CIRCLE('',#74259,0.0999999999999994) ;
#28209 = CIRCLE('',#74261,0.1) ;
#28210 = CIRCLE('',#74263,0.1) ;
#28211 = CIRCLE('',#74265,0.1) ;
#28212 = CIRCLE('',#74267,0.1) ;
#28213 = CIRCLE('',#74268,0.0999999999999994) ;
#28214 = CIRCLE('',#74270,0.0999999999999994) ;
#28215 = CIRCLE('',#74272,0.0999999999999994) ;
#28216 = CIRCLE('',#74274,0.1) ;
#28217 = CIRCLE('',#74276,0.0999999999999994) ;
#28218 = CIRCLE('',#74279,0.0999999999999994) ;
#28219 = CIRCLE('',#74281,0.1) ;
#28220 = CIRCLE('',#74283,0.0999999999999994) ;
#28221 = CIRCLE('',#74286,0.1) ;
#28222 = CIRCLE('',#74287,0.1) ;
#28223 = CIRCLE('',#74289,0.0999999999999994) ;
#28224 = CIRCLE('',#74291,0.0999999999999994) ;
#28225 = CIRCLE('',#74293,0.0999999999999994) ;
#28226 = CIRCLE('',#74295,0.0999999999999994) ;
#28227 = CIRCLE('',#74297,0.1) ;
#28228 = CIRCLE('',#74299,0.0999999999999998) ;
#28229 = CIRCLE('',#74301,0.1) ;
#28230 = CIRCLE('',#74303,0.1) ;
#28231 = CIRCLE('',#74305,0.1) ;
#28232 = CIRCLE('',#74307,0.1) ;
#28233 = CIRCLE('',#74309,0.1) ;
#28234 = CIRCLE('',#74311,0.1) ;
#28235 = CIRCLE('',#74313,0.1) ;
#28236 = CIRCLE('',#74315,0.1) ;
#28237 = CIRCLE('',#74318,0.1) ;
#28238 = CIRCLE('',#74320,0.1) ;
#28239 = CIRCLE('',#74322,0.1) ;
#28240 = CIRCLE('',#74324,0.1) ;
#28241 = CIRCLE('',#74326,0.0999999999999998) ;
#28242 = CIRCLE('',#74328,0.1) ;
#28243 = CIRCLE('',#74330,0.1) ;
#28244 = CIRCLE('',#74332,0.1) ;
#28245 = CIRCLE('',#74334,0.1) ;
#28246 = CIRCLE('',#74336,0.1) ;
#28247 = CIRCLE('',#74339,0.0999999999999994) ;
#28248 = CIRCLE('',#74340,0.0999999999999994) ;
#28249 = CIRCLE('',#74342,0.0999999999999994) ;
#28250 = CIRCLE('',#74343,0.1) ;
#28251 = CIRCLE('',#74345,0.0999999999999994) ;
#28252 = CIRCLE('',#74346,0.1) ;
#28253 = CIRCLE('',#74348,0.1) ;
#28254 = CIRCLE('',#74349,0.0999999999999998) ;
#28255 = CIRCLE('',#74351,0.1) ;
#28256 = CIRCLE('',#74353,0.1) ;
#28257 = CIRCLE('',#74355,0.0999999999999994) ;
#28258 = CIRCLE('',#74357,0.1) ;
#28259 = CIRCLE('',#74359,0.0999999999999998) ;
#28260 = CIRCLE('',#74361,0.1) ;
#28261 = CIRCLE('',#74363,0.0999999999999994) ;
#28262 = CIRCLE('',#74364,0.1) ;
#28263 = CIRCLE('',#74367,0.1) ;
#28264 = CIRCLE('',#74369,0.0999999999999994) ;
#28265 = CIRCLE('',#74370,0.0999999999999994) ;
#28266 = CIRCLE('',#74372,0.0999999999999994) ;
#28267 = CIRCLE('',#74374,0.1) ;
#28268 = CIRCLE('',#74376,0.0999999999999994) ;
#28269 = CIRCLE('',#74378,0.0999999999999994) ;
#28270 = CIRCLE('',#74380,0.0999999999999994) ;
#28271 = CIRCLE('',#74382,0.1) ;
#28272 = CIRCLE('',#74383,0.0999999999999994) ;
#28273 = CIRCLE('',#74385,0.1) ;
#28274 = CIRCLE('',#74387,0.0999999999999994) ;
#28275 = CIRCLE('',#74389,0.0999999999999998) ;
#28276 = CIRCLE('',#74390,0.1) ;
#28277 = CIRCLE('',#74392,0.0999999999999994) ;
#28278 = CIRCLE('',#74394,0.1) ;
#28279 = CIRCLE('',#74395,0.1) ;
#28280 = CIRCLE('',#74397,0.1) ;
#28281 = CIRCLE('',#74399,0.1) ;
#28282 = CIRCLE('',#74401,0.0999999999999994) ;
#28283 = CIRCLE('',#74403,0.0999999999999994) ;
#28284 = CIRCLE('',#74405,0.1) ;
#28285 = CIRCLE('',#74407,0.1) ;
#28286 = CIRCLE('',#74409,0.1) ;
#28287 = CIRCLE('',#74411,0.0999999999999994) ;
#28288 = CIRCLE('',#74412,0.0999999999999994) ;
#28289 = CIRCLE('',#74414,0.1) ;
#28290 = CIRCLE('',#74416,0.1) ;
#28291 = CIRCLE('',#74418,0.1) ;
#28292 = CIRCLE('',#74420,0.1) ;
#28293 = CIRCLE('',#74421,0.0999999999999994) ;
#28294 = CIRCLE('',#74423,0.0999999999999994) ;
#28295 = CIRCLE('',#74425,0.0999999999999994) ;
#28296 = CIRCLE('',#74427,0.1) ;
#28297 = CIRCLE('',#74429,0.0999999999999994) ;
#28298 = CIRCLE('',#74432,0.0999999999999994) ;
#28299 = CIRCLE('',#74434,0.1) ;
#28300 = CIRCLE('',#74436,0.0999999999999994) ;
#28301 = CIRCLE('',#74439,0.1) ;
#28302 = CIRCLE('',#74440,0.1) ;
#28303 = CIRCLE('',#74442,0.0999999999999994) ;
#28304 = CIRCLE('',#74444,0.0999999999999994) ;
#28305 = CIRCLE('',#74446,0.0999999999999994) ;
#28306 = CIRCLE('',#74448,0.0999999999999994) ;
#28307 = CIRCLE('',#74450,0.1) ;
#28308 = CIRCLE('',#74452,0.0999999999999998) ;
#28309 = CIRCLE('',#74454,0.1) ;
#28310 = CIRCLE('',#74456,0.1) ;
#28311 = CIRCLE('',#74458,0.1) ;
#28312 = CIRCLE('',#74460,0.1) ;
#28313 = CIRCLE('',#74462,0.1) ;
#28314 = CIRCLE('',#74464,0.1) ;
#28315 = CIRCLE('',#74466,0.1) ;
#28316 = CIRCLE('',#74468,0.1) ;
#28317 = CIRCLE('',#74471,0.1) ;
#28318 = CIRCLE('',#74473,0.0999999999999994) ;
#28319 = CIRCLE('',#74475,0.1) ;
#28320 = CIRCLE('',#74477,0.0999999999999994) ;
#28321 = CIRCLE('',#74479,0.1) ;
#28322 = CIRCLE('',#74481,0.1) ;
#28323 = CIRCLE('',#74483,0.1) ;
#28324 = CIRCLE('',#74485,0.1) ;
#28325 = CIRCLE('',#74487,0.0999999999999994) ;
#28326 = CIRCLE('',#74489,0.0999999999999994) ;
#28327 = CIRCLE('',#74492,0.0999999999999994) ;
#28328 = CIRCLE('',#74493,0.0999999999999994) ;
#28329 = CIRCLE('',#74495,0.0999999999999994) ;
#28330 = CIRCLE('',#74496,0.1) ;
#28331 = CIRCLE('',#74498,0.0999999999999994) ;
#28332 = CIRCLE('',#74499,0.1) ;
#28333 = CIRCLE('',#74501,0.1) ;
#28334 = CIRCLE('',#74502,0.0999999999999998) ;
#28335 = CIRCLE('',#74504,0.1) ;
#28336 = CIRCLE('',#74506,0.1) ;
#28337 = CIRCLE('',#74508,0.0999999999999994) ;
#28338 = CIRCLE('',#74510,0.1) ;
#28339 = CIRCLE('',#74512,0.0999999999999998) ;
#28340 = CIRCLE('',#74514,0.1) ;
#28341 = CIRCLE('',#74516,0.0999999999999994) ;
#28342 = CIRCLE('',#74517,0.1) ;
#28343 = CIRCLE('',#74520,0.1) ;
#28344 = CIRCLE('',#74522,0.0999999999999994) ;
#28345 = CIRCLE('',#74523,0.0999999999999994) ;
#28346 = CIRCLE('',#74525,0.0999999999999994) ;
#28347 = CIRCLE('',#74527,0.1) ;
#28348 = CIRCLE('',#74529,0.0999999999999994) ;
#28349 = CIRCLE('',#74531,0.0999999999999994) ;
#28350 = CIRCLE('',#74533,0.0999999999999994) ;
#28351 = CIRCLE('',#74535,0.1) ;
#28352 = CIRCLE('',#74536,0.0999999999999994) ;
#28353 = CIRCLE('',#74538,0.1) ;
#28354 = CIRCLE('',#74540,0.0999999999999994) ;
#28355 = CIRCLE('',#74542,0.0999999999999998) ;
#28356 = CIRCLE('',#74543,0.1) ;
#28357 = CIRCLE('',#74545,0.0999999999999994) ;
#28358 = CIRCLE('',#74547,0.1) ;
#28359 = CIRCLE('',#74548,0.1) ;
#28360 = CIRCLE('',#74550,0.1) ;
#28361 = CIRCLE('',#74552,0.1) ;
#28362 = CIRCLE('',#74554,0.0999999999999994) ;
#28363 = CIRCLE('',#74556,0.0999999999999994) ;
#28364 = CIRCLE('',#74558,0.1) ;
#28365 = CIRCLE('',#74560,0.1) ;
#28366 = CIRCLE('',#74562,0.1) ;
#28367 = CIRCLE('',#74564,0.0999999999999994) ;
#28368 = CIRCLE('',#74565,0.0999999999999994) ;
#28369 = CIRCLE('',#74567,0.1) ;
#28370 = CIRCLE('',#74569,0.1) ;
#28371 = CIRCLE('',#74571,0.1) ;
#28372 = CIRCLE('',#74573,0.1) ;
#28373 = CIRCLE('',#74574,0.0999999999999994) ;
#28374 = CIRCLE('',#74576,0.0999999999999994) ;
#28375 = CIRCLE('',#74578,0.0999999999999994) ;
#28376 = CIRCLE('',#74580,0.1) ;
#28377 = CIRCLE('',#74582,0.0999999999999994) ;
#28378 = CIRCLE('',#74585,0.0999999999999994) ;
#28379 = CIRCLE('',#74587,0.1) ;
#28380 = CIRCLE('',#74589,0.0999999999999994) ;
#28381 = CIRCLE('',#74592,0.1) ;
#28382 = CIRCLE('',#74593,0.1) ;
#28383 = CIRCLE('',#74595,0.0999999999999994) ;
#28384 = CIRCLE('',#74597,0.0999999999999994) ;
#28385 = CIRCLE('',#74599,0.0999999999999994) ;
#28386 = CIRCLE('',#74601,0.0999999999999994) ;
#28387 = CIRCLE('',#74603,0.1) ;
#28388 = CIRCLE('',#74605,0.1) ;
#28389 = CIRCLE('',#74607,0.1) ;
#28390 = CIRCLE('',#74609,0.1) ;
#28391 = CIRCLE('',#74611,0.1) ;
#28392 = CIRCLE('',#74613,0.1) ;
#28393 = CIRCLE('',#74615,0.100000000000001) ;
#28394 = CIRCLE('',#74617,0.1) ;
#28395 = CIRCLE('',#74619,0.1) ;
#28396 = CIRCLE('',#74621,0.1) ;
#28397 = CIRCLE('',#74624,0.1) ;
#28398 = CIRCLE('',#74626,0.0999999999999994) ;
#28399 = CIRCLE('',#74628,0.1) ;
#28400 = CIRCLE('',#74630,0.0999999999999994) ;
#28401 = CIRCLE('',#74632,0.1) ;
#28402 = CIRCLE('',#74634,0.1) ;
#28403 = CIRCLE('',#74636,0.1) ;
#28404 = CIRCLE('',#74638,0.1) ;
#28405 = CIRCLE('',#74640,0.0999999999999994) ;
#28406 = CIRCLE('',#74642,0.0999999999999994) ;
#28407 = CIRCLE('',#74645,0.0999999999999994) ;
#28408 = CIRCLE('',#74646,0.0999999999999994) ;
#28409 = CIRCLE('',#74648,0.0999999999999994) ;
#28410 = CIRCLE('',#74649,0.1) ;
#28411 = CIRCLE('',#74651,0.0999999999999994) ;
#28412 = CIRCLE('',#74652,0.1) ;
#28413 = CIRCLE('',#74654,0.1) ;
#28414 = CIRCLE('',#74655,0.0999999999999998) ;
#28415 = CIRCLE('',#74657,0.1) ;
#28416 = CIRCLE('',#74659,0.1) ;
#28417 = CIRCLE('',#74661,0.0999999999999994) ;
#28418 = CIRCLE('',#74663,0.1) ;
#28419 = CIRCLE('',#74665,0.0999999999999998) ;
#28420 = CIRCLE('',#74667,0.1) ;
#28421 = CIRCLE('',#74669,0.0999999999999994) ;
#28422 = CIRCLE('',#74670,0.1) ;
#28423 = CIRCLE('',#74673,0.1) ;
#28424 = CIRCLE('',#74675,0.0999999999999994) ;
#28425 = CIRCLE('',#74676,0.0999999999999994) ;
#28426 = CIRCLE('',#74678,0.0999999999999994) ;
#28427 = CIRCLE('',#74680,0.1) ;
#28428 = CIRCLE('',#74682,0.0999999999999994) ;
#28429 = CIRCLE('',#74684,0.0999999999999994) ;
#28430 = CIRCLE('',#74686,0.0999999999999994) ;
#28431 = CIRCLE('',#74688,0.1) ;
#28432 = CIRCLE('',#74689,0.0999999999999994) ;
#28433 = CIRCLE('',#74691,0.1) ;
#28434 = CIRCLE('',#74693,0.0999999999999994) ;
#28435 = CIRCLE('',#74695,0.0999999999999998) ;
#28436 = CIRCLE('',#74696,0.1) ;
#28437 = CIRCLE('',#74698,0.0999999999999994) ;
#28438 = CIRCLE('',#74700,0.1) ;
#28439 = CIRCLE('',#74701,0.1) ;
#28440 = CIRCLE('',#74703,0.1) ;
#28441 = CIRCLE('',#74705,0.1) ;
#28442 = CIRCLE('',#74707,0.0999999999999994) ;
#28443 = CIRCLE('',#74709,0.0999999999999994) ;
#28444 = CIRCLE('',#74711,0.1) ;
#28445 = CIRCLE('',#74713,0.1) ;
#28446 = CIRCLE('',#74715,0.1) ;
#28447 = CIRCLE('',#74717,0.0999999999999994) ;
#28448 = CIRCLE('',#74718,0.0999999999999994) ;
#28449 = CIRCLE('',#74720,0.1) ;
#28450 = CIRCLE('',#74722,0.1) ;
#28451 = CIRCLE('',#74724,0.1) ;
#28452 = CIRCLE('',#74726,0.1) ;
#28453 = CIRCLE('',#74727,0.0999999999999994) ;
#28454 = CIRCLE('',#74729,0.0999999999999994) ;
#28455 = CIRCLE('',#74731,0.0999999999999994) ;
#28456 = CIRCLE('',#74733,0.1) ;
#28457 = CIRCLE('',#74735,0.0999999999999994) ;
#28458 = CIRCLE('',#74738,0.0999999999999994) ;
#28459 = CIRCLE('',#74740,0.1) ;
#28460 = CIRCLE('',#74742,0.0999999999999994) ;
#28461 = CIRCLE('',#74745,0.1) ;
#28462 = CIRCLE('',#74746,0.1) ;
#28463 = CIRCLE('',#74748,0.0999999999999994) ;
#28464 = CIRCLE('',#74750,0.0999999999999994) ;
#28465 = CIRCLE('',#74752,0.0999999999999994) ;
#28466 = CIRCLE('',#74754,0.0999999999999994) ;
#28467 = CIRCLE('',#74756,0.1) ;
#28468 = CIRCLE('',#74758,0.1) ;
#28469 = CIRCLE('',#74760,0.1) ;
#28470 = CIRCLE('',#74762,0.1) ;
#28471 = CIRCLE('',#74764,0.1) ;
#28472 = CIRCLE('',#74766,0.1) ;
#28473 = CIRCLE('',#74768,0.0999999999999989) ;
#28474 = CIRCLE('',#74770,0.1) ;
#28475 = CIRCLE('',#74772,0.1) ;
#28476 = CIRCLE('',#74774,0.1) ;
#28477 = CIRCLE('',#74777,0.1) ;
#28478 = CIRCLE('',#74779,0.0999999999999994) ;
#28479 = CIRCLE('',#74781,0.0999999999999995) ;
#28480 = CIRCLE('',#74783,0.0999999999999994) ;
#28481 = CIRCLE('',#74785,0.1) ;
#28482 = CIRCLE('',#74787,0.1) ;
#28483 = CIRCLE('',#74789,0.1) ;
#28484 = CIRCLE('',#74791,0.1) ;
#28485 = CIRCLE('',#74793,0.0999999999999994) ;
#28486 = CIRCLE('',#74795,0.0999999999999994) ;
#28487 = CIRCLE('',#74798,0.0999999999999994) ;
#28488 = CIRCLE('',#74799,0.0999999999999994) ;
#28489 = CIRCLE('',#74801,0.0999999999999994) ;
#28490 = CIRCLE('',#74802,0.1) ;
#28491 = CIRCLE('',#74804,0.0999999999999994) ;
#28492 = CIRCLE('',#74805,0.1) ;
#28493 = CIRCLE('',#74807,0.1) ;
#28494 = CIRCLE('',#74808,0.0999999999999998) ;
#28495 = CIRCLE('',#74810,0.1) ;
#28496 = CIRCLE('',#74812,0.1) ;
#28497 = CIRCLE('',#74814,0.0999999999999994) ;
#28498 = CIRCLE('',#74816,0.1) ;
#28499 = CIRCLE('',#74818,0.0999999999999998) ;
#28500 = CIRCLE('',#74820,0.1) ;
#28501 = CIRCLE('',#74822,0.0999999999999994) ;
#28502 = CIRCLE('',#74823,0.1) ;
#28503 = CIRCLE('',#74826,0.1) ;
#28504 = CIRCLE('',#74828,0.0999999999999994) ;
#28505 = CIRCLE('',#74829,0.0999999999999994) ;
#28506 = CIRCLE('',#74831,0.0999999999999994) ;
#28507 = CIRCLE('',#74833,0.1) ;
#28508 = CIRCLE('',#74835,0.0999999999999994) ;
#28509 = CIRCLE('',#74837,0.0999999999999994) ;
#28510 = CIRCLE('',#74839,0.0999999999999994) ;
#28511 = CIRCLE('',#74841,0.1) ;
#28512 = CIRCLE('',#74842,0.0999999999999994) ;
#28513 = CIRCLE('',#74844,0.1) ;
#28514 = CIRCLE('',#74846,0.0999999999999994) ;
#28515 = CIRCLE('',#74848,0.0999999999999998) ;
#28516 = CIRCLE('',#74849,0.1) ;
#28517 = CIRCLE('',#74851,0.0999999999999994) ;
#28518 = CIRCLE('',#74853,0.1) ;
#28519 = CIRCLE('',#74854,0.1) ;
#28520 = CIRCLE('',#74856,0.1) ;
#28521 = CIRCLE('',#74858,0.1) ;
#28522 = CIRCLE('',#74860,0.0999999999999994) ;
#28523 = CIRCLE('',#74862,0.0999999999999994) ;
#28524 = CIRCLE('',#74864,0.1) ;
#28525 = CIRCLE('',#74866,0.1) ;
#28526 = CIRCLE('',#74868,0.1) ;
#28527 = CIRCLE('',#74870,0.0999999999999994) ;
#28528 = CIRCLE('',#74871,0.0999999999999994) ;
#28529 = CIRCLE('',#74873,0.1) ;
#28530 = CIRCLE('',#74875,0.1) ;
#28531 = CIRCLE('',#74877,0.1) ;
#28532 = CIRCLE('',#74879,0.1) ;
#28533 = CIRCLE('',#74880,0.0999999999999994) ;
#28534 = CIRCLE('',#74882,0.0999999999999994) ;
#28535 = CIRCLE('',#74884,0.0999999999999994) ;
#28536 = CIRCLE('',#74886,0.1) ;
#28537 = CIRCLE('',#74888,0.0999999999999994) ;
#28538 = CIRCLE('',#74891,0.0999999999999994) ;
#28539 = CIRCLE('',#74893,0.1) ;
#28540 = CIRCLE('',#74895,0.0999999999999994) ;
#28541 = CIRCLE('',#74898,0.1) ;
#28542 = CIRCLE('',#74899,0.1) ;
#28543 = CIRCLE('',#74901,0.0999999999999994) ;
#28544 = CIRCLE('',#74903,0.0999999999999994) ;
#28545 = CIRCLE('',#74905,0.0999999999999994) ;
#28546 = CIRCLE('',#74907,0.0999999999999994) ;
#28547 = CIRCLE('',#74909,0.1) ;
#28548 = CIRCLE('',#74911,0.1) ;
#28549 = CIRCLE('',#74913,0.1) ;
#28550 = CIRCLE('',#74915,0.1) ;
#28551 = CIRCLE('',#74917,0.1) ;
#28552 = CIRCLE('',#74919,0.1) ;
#28553 = CIRCLE('',#74921,0.0999999999999989) ;
#28554 = CIRCLE('',#74923,0.1) ;
#28555 = CIRCLE('',#74925,0.1) ;
#28556 = CIRCLE('',#74927,0.1) ;
#28557 = CIRCLE('',#74930,0.1) ;
#28558 = CIRCLE('',#74932,0.0999999999999994) ;
#28559 = CIRCLE('',#74934,0.0999999999999995) ;
#28560 = CIRCLE('',#74936,0.0999999999999994) ;
#28561 = CIRCLE('',#74938,0.1) ;
#28562 = CIRCLE('',#74940,0.1) ;
#28563 = CIRCLE('',#74942,0.1) ;
#28564 = CIRCLE('',#74944,0.1) ;
#28565 = CIRCLE('',#74946,0.0999999999999994) ;
#28566 = CIRCLE('',#74948,0.0999999999999994) ;
#28567 = CIRCLE('',#74951,0.0999999999999994) ;
#28568 = CIRCLE('',#74952,0.0999999999999994) ;
#28569 = CIRCLE('',#74954,0.0999999999999994) ;
#28570 = CIRCLE('',#74955,0.1) ;
#28571 = CIRCLE('',#74957,0.0999999999999994) ;
#28572 = CIRCLE('',#74958,0.1) ;
#28573 = CIRCLE('',#74960,0.1) ;
#28574 = CIRCLE('',#74961,0.0999999999999998) ;
#28575 = CIRCLE('',#74963,0.1) ;
#28576 = CIRCLE('',#74965,0.1) ;
#28577 = CIRCLE('',#74967,0.0999999999999994) ;
#28578 = CIRCLE('',#74969,0.1) ;
#28579 = CIRCLE('',#74971,0.0999999999999998) ;
#28580 = CIRCLE('',#74973,0.1) ;
#28581 = CIRCLE('',#74975,0.0999999999999994) ;
#28582 = CIRCLE('',#74976,0.1) ;
#28583 = CIRCLE('',#74979,0.1) ;
#28584 = CIRCLE('',#74981,0.0999999999999994) ;
#28585 = CIRCLE('',#74982,0.0999999999999994) ;
#28586 = CIRCLE('',#74984,0.0999999999999994) ;
#28587 = CIRCLE('',#74986,0.1) ;
#28588 = CIRCLE('',#74988,0.0999999999999994) ;
#28589 = CIRCLE('',#74990,0.0999999999999994) ;
#28590 = CIRCLE('',#74992,0.0999999999999994) ;
#28591 = CIRCLE('',#74994,0.1) ;
#28592 = CIRCLE('',#74995,0.0999999999999994) ;
#28593 = CIRCLE('',#74997,0.1) ;
#28594 = CIRCLE('',#74999,0.0999999999999994) ;
#28595 = CIRCLE('',#75001,0.0999999999999998) ;
#28596 = CIRCLE('',#75002,0.1) ;
#28597 = CIRCLE('',#75004,0.0999999999999994) ;
#28598 = CIRCLE('',#75006,0.1) ;
#28599 = CIRCLE('',#75007,0.1) ;
#28600 = CIRCLE('',#75009,0.1) ;
#28601 = CIRCLE('',#75011,0.1) ;
#28602 = CIRCLE('',#75013,0.0999999999999994) ;
#28603 = CIRCLE('',#75015,0.0999999999999994) ;
#28604 = CIRCLE('',#75017,0.1) ;
#28605 = CIRCLE('',#75019,0.1) ;
#28606 = CIRCLE('',#75021,0.1) ;
#28607 = CIRCLE('',#75023,0.0999999999999994) ;
#28608 = CIRCLE('',#75024,0.0999999999999994) ;
#28609 = CIRCLE('',#75026,0.1) ;
#28610 = CIRCLE('',#75028,0.1) ;
#28611 = CIRCLE('',#75030,0.1) ;
#28612 = CIRCLE('',#75032,0.1) ;
#28613 = CIRCLE('',#75033,0.0999999999999994) ;
#28614 = CIRCLE('',#75035,0.0999999999999994) ;
#28615 = CIRCLE('',#75037,0.0999999999999994) ;
#28616 = CIRCLE('',#75039,0.1) ;
#28617 = CIRCLE('',#75041,0.0999999999999994) ;
#28618 = CIRCLE('',#75044,0.0999999999999994) ;
#28619 = CIRCLE('',#75046,0.1) ;
#28620 = CIRCLE('',#75048,0.0999999999999994) ;
#28621 = CIRCLE('',#75051,0.1) ;
#28622 = CIRCLE('',#75052,0.1) ;
#28623 = CIRCLE('',#75054,0.0999999999999994) ;
#28624 = CIRCLE('',#75056,0.0999999999999994) ;
#28625 = CIRCLE('',#75058,0.0999999999999994) ;
#28626 = CIRCLE('',#75060,0.0999999999999994) ;
#28627 = CIRCLE('',#75062,0.1) ;
#28628 = CIRCLE('',#75064,0.1) ;
#28629 = CIRCLE('',#75066,0.1) ;
#28630 = CIRCLE('',#75068,0.1) ;
#28631 = CIRCLE('',#75070,0.1) ;
#28632 = CIRCLE('',#75072,0.1) ;
#28633 = CIRCLE('',#75074,0.0999999999999989) ;
#28634 = CIRCLE('',#75076,0.1) ;
#28635 = CIRCLE('',#75078,0.1) ;
#28636 = CIRCLE('',#75080,0.1) ;
#28637 = CIRCLE('',#75083,0.1) ;
#28638 = CIRCLE('',#75085,0.0999999999999994) ;
#28639 = CIRCLE('',#75087,0.0999999999999995) ;
#28640 = CIRCLE('',#75089,0.0999999999999994) ;
#28641 = CIRCLE('',#75091,0.1) ;
#28642 = CIRCLE('',#75093,0.1) ;
#28643 = CIRCLE('',#75095,0.1) ;
#28644 = CIRCLE('',#75097,0.1) ;
#28645 = CIRCLE('',#75099,0.0999999999999994) ;
#28646 = CIRCLE('',#75101,0.0999999999999994) ;
#28647 = CIRCLE('',#75104,0.0999999999999994) ;
#28648 = CIRCLE('',#75105,0.0999999999999994) ;
#28649 = CIRCLE('',#75107,0.0999999999999994) ;
#28650 = CIRCLE('',#75108,0.1) ;
#28651 = CIRCLE('',#75110,0.0999999999999994) ;
#28652 = CIRCLE('',#75111,0.1) ;
#28653 = CIRCLE('',#75113,0.1) ;
#28654 = CIRCLE('',#75114,0.0999999999999998) ;
#28655 = CIRCLE('',#75116,0.1) ;
#28656 = CIRCLE('',#75118,0.1) ;
#28657 = CIRCLE('',#75120,0.0999999999999994) ;
#28658 = CIRCLE('',#75122,0.1) ;
#28659 = CIRCLE('',#75124,0.0999999999999998) ;
#28660 = CIRCLE('',#75126,0.1) ;
#28661 = CIRCLE('',#75128,0.0999999999999994) ;
#28662 = CIRCLE('',#75129,0.1) ;
#28663 = CIRCLE('',#75132,0.1) ;
#28664 = CIRCLE('',#75134,0.0999999999999994) ;
#28665 = CIRCLE('',#75135,0.0999999999999994) ;
#28666 = CIRCLE('',#75137,0.0999999999999994) ;
#28667 = CIRCLE('',#75139,0.1) ;
#28668 = CIRCLE('',#75141,0.0999999999999994) ;
#28669 = CIRCLE('',#75143,0.0999999999999994) ;
#28670 = CIRCLE('',#75145,0.0999999999999994) ;
#28671 = CIRCLE('',#75147,0.1) ;
#28672 = CIRCLE('',#75148,0.0999999999999994) ;
#28673 = CIRCLE('',#75150,0.1) ;
#28674 = CIRCLE('',#75152,0.0999999999999994) ;
#28675 = CIRCLE('',#75154,0.0999999999999998) ;
#28676 = CIRCLE('',#75155,0.1) ;
#28677 = CIRCLE('',#75157,0.0999999999999994) ;
#28678 = CIRCLE('',#75159,0.1) ;
#28679 = CIRCLE('',#75160,0.1) ;
#28680 = CIRCLE('',#75162,0.1) ;
#28681 = CIRCLE('',#75164,0.1) ;
#28682 = CIRCLE('',#75166,0.0999999999999994) ;
#28683 = CIRCLE('',#75168,0.0999999999999994) ;
#28684 = CIRCLE('',#75170,0.1) ;
#28685 = CIRCLE('',#75172,0.1) ;
#28686 = CIRCLE('',#75174,0.1) ;
#28687 = CIRCLE('',#75176,0.100000000000003) ;
#28688 = CIRCLE('',#75177,0.100000000000003) ;
#28689 = CIRCLE('',#75179,0.1) ;
#28690 = CIRCLE('',#75181,0.1) ;
#28691 = CIRCLE('',#75183,0.1) ;
#28692 = CIRCLE('',#75185,0.1) ;
#28693 = CIRCLE('',#75186,0.100000000000003) ;
#28694 = CIRCLE('',#75188,0.100000000000003) ;
#28695 = CIRCLE('',#75190,0.100000000000003) ;
#28696 = CIRCLE('',#75192,0.1) ;
#28697 = CIRCLE('',#75194,0.100000000000003) ;
#28698 = CIRCLE('',#75197,0.100000000000003) ;
#28699 = CIRCLE('',#75199,0.1) ;
#28700 = CIRCLE('',#75201,0.100000000000003) ;
#28701 = CIRCLE('',#75204,0.1) ;
#28702 = CIRCLE('',#75205,0.1) ;
#28703 = CIRCLE('',#75207,0.0999999999999994) ;
#28704 = CIRCLE('',#75209,0.100000000000003) ;
#28705 = CIRCLE('',#75211,0.0999999999999994) ;
#28706 = CIRCLE('',#75213,0.100000000000003) ;
#28707 = CIRCLE('',#75215,0.1) ;
#28708 = CIRCLE('',#75217,0.1) ;
#28709 = CIRCLE('',#75219,0.1) ;
#28710 = CIRCLE('',#75221,0.1) ;
#28711 = CIRCLE('',#75223,0.0999999999999999) ;
#28712 = CIRCLE('',#75225,0.1) ;
#28713 = CIRCLE('',#75227,0.0999999999999992) ;
#28714 = CIRCLE('',#75229,0.1) ;
#28715 = CIRCLE('',#75231,0.1) ;
#28716 = CIRCLE('',#75233,0.1) ;
#28717 = CIRCLE('',#75236,0.1) ;
#28718 = CIRCLE('',#75238,0.0999999999999994) ;
#28719 = CIRCLE('',#75240,0.0999999999999995) ;
#28720 = CIRCLE('',#75242,0.0999999999999994) ;
#28721 = CIRCLE('',#75244,0.1) ;
#28722 = CIRCLE('',#75246,0.1) ;
#28723 = CIRCLE('',#75248,0.1) ;
#28724 = CIRCLE('',#75250,0.1) ;
#28725 = CIRCLE('',#75252,0.0999999999999994) ;
#28726 = CIRCLE('',#75254,0.0999999999999994) ;
#28727 = CIRCLE('',#75257,0.100000000000003) ;
#28728 = CIRCLE('',#75258,0.100000000000003) ;
#28729 = CIRCLE('',#75260,0.100000000000003) ;
#28730 = CIRCLE('',#75261,0.1) ;
#28731 = CIRCLE('',#75263,0.100000000000003) ;
#28732 = CIRCLE('',#75264,0.1) ;
#28733 = CIRCLE('',#75266,0.1) ;
#28734 = CIRCLE('',#75267,0.0999999999999998) ;
#28735 = CIRCLE('',#75269,0.1) ;
#28736 = CIRCLE('',#75271,0.1) ;
#28737 = CIRCLE('',#75273,0.100000000000003) ;
#28738 = CIRCLE('',#75275,0.1) ;
#28739 = CIRCLE('',#75277,0.0999999999999998) ;
#28740 = CIRCLE('',#75279,0.1) ;
#28741 = CIRCLE('',#75281,0.100000000000003) ;
#28742 = CIRCLE('',#75282,0.1) ;
#28743 = CIRCLE('',#75285,0.1) ;
#28744 = CIRCLE('',#75287,0.100000000000003) ;
#28745 = CIRCLE('',#75288,0.100000000000003) ;
#28746 = CIRCLE('',#75290,0.100000000000003) ;
#28747 = CIRCLE('',#75292,0.1) ;
#28748 = CIRCLE('',#75294,0.100000000000003) ;
#28749 = CIRCLE('',#75296,0.100000000000003) ;
#28750 = CIRCLE('',#75298,0.100000000000003) ;
#28751 = CIRCLE('',#75300,0.1) ;
#28752 = CIRCLE('',#75301,0.100000000000003) ;
#28753 = CIRCLE('',#75303,0.1) ;
#28754 = CIRCLE('',#75305,0.100000000000003) ;
#28755 = CIRCLE('',#75307,0.0999999999999998) ;
#28756 = CIRCLE('',#75308,0.1) ;
#28757 = CIRCLE('',#75310,0.100000000000003) ;
#28758 = CIRCLE('',#75312,0.1) ;
#28759 = CIRCLE('',#75313,0.1) ;
#28760 = CIRCLE('',#75315,0.1) ;
#28761 = CIRCLE('',#75317,0.1) ;
#28762 = CIRCLE('',#75319,0.100000000000003) ;
#28763 = CIRCLE('',#75321,0.100000000000003) ;
#28764 = CIRCLE('',#75323,0.1) ;
#28765 = CIRCLE('',#75325,0.1) ;
#28766 = CIRCLE('',#75327,0.1) ;
#28767 = CIRCLE('',#75329,0.100000000000003) ;
#28768 = CIRCLE('',#75330,0.100000000000003) ;
#28769 = CIRCLE('',#75332,0.1) ;
#28770 = CIRCLE('',#75334,0.1) ;
#28771 = CIRCLE('',#75336,0.1) ;
#28772 = CIRCLE('',#75338,0.1) ;
#28773 = CIRCLE('',#75339,0.100000000000003) ;
#28774 = CIRCLE('',#75341,0.100000000000003) ;
#28775 = CIRCLE('',#75343,0.100000000000003) ;
#28776 = CIRCLE('',#75345,0.1) ;
#28777 = CIRCLE('',#75347,0.100000000000003) ;
#28778 = CIRCLE('',#75350,0.100000000000003) ;
#28779 = CIRCLE('',#75352,0.1) ;
#28780 = CIRCLE('',#75354,0.100000000000003) ;
#28781 = CIRCLE('',#75357,0.1) ;
#28782 = CIRCLE('',#75358,0.1) ;
#28783 = CIRCLE('',#75360,0.100000000000003) ;
#28784 = CIRCLE('',#75362,0.100000000000003) ;
#28785 = CIRCLE('',#75364,0.100000000000003) ;
#28786 = CIRCLE('',#75366,0.100000000000003) ;
#28787 = CIRCLE('',#75368,0.1) ;
#28788 = CIRCLE('',#75370,0.1) ;
#28789 = CIRCLE('',#75372,0.1) ;
#28790 = CIRCLE('',#75374,0.1) ;
#28791 = CIRCLE('',#75376,0.0999999999999999) ;
#28792 = CIRCLE('',#75378,0.1) ;
#28793 = CIRCLE('',#75380,0.0999999999999992) ;
#28794 = CIRCLE('',#75382,0.1) ;
#28795 = CIRCLE('',#75384,0.1) ;
#28796 = CIRCLE('',#75386,0.1) ;
#28797 = CIRCLE('',#75389,0.1) ;
#28798 = CIRCLE('',#75391,0.100000000000003) ;
#28799 = CIRCLE('',#75393,0.0999999999999998) ;
#28800 = CIRCLE('',#75395,0.100000000000003) ;
#28801 = CIRCLE('',#75397,0.1) ;
#28802 = CIRCLE('',#75399,0.1) ;
#28803 = CIRCLE('',#75401,0.1) ;
#28804 = CIRCLE('',#75403,0.1) ;
#28805 = CIRCLE('',#75405,0.100000000000003) ;
#28806 = CIRCLE('',#75407,0.100000000000003) ;
#28807 = CIRCLE('',#75415,0.3) ;
#28808 = CIRCLE('',#75416,0.9) ;
#28809 = CIRCLE('',#75418,0.9) ;
#28810 = CIRCLE('',#75419,0.3) ;
#28811 = CIRCLE('',#75421,1.) ;
#28812 = CIRCLE('',#75422,1.) ;
#28813 = CIRCLE('',#75424,0.2) ;
#28814 = CIRCLE('',#75425,0.2) ;
#28815 = CIRCLE('',#75439,0.3) ;
#28816 = CIRCLE('',#75440,0.9) ;
#28817 = CIRCLE('',#75442,0.9) ;
#28818 = CIRCLE('',#75443,0.3) ;
#28819 = CIRCLE('',#75445,1.) ;
#28820 = CIRCLE('',#75446,1.) ;
#28821 = CIRCLE('',#75448,0.2) ;
#28822 = CIRCLE('',#75449,0.2) ;
#28823 = CIRCLE('',#75463,0.3) ;
#28824 = CIRCLE('',#75464,0.9) ;
#28825 = CIRCLE('',#75466,0.9) ;
#28826 = CIRCLE('',#75467,0.3) ;
#28827 = CIRCLE('',#75469,1.) ;
#28828 = CIRCLE('',#75470,1.) ;
#28829 = CIRCLE('',#75472,0.2) ;
#28830 = CIRCLE('',#75473,0.2) ;
#28831 = CIRCLE('',#75487,0.3) ;
#28832 = CIRCLE('',#75488,0.9) ;
#28833 = CIRCLE('',#75490,0.9) ;
#28834 = CIRCLE('',#75491,0.3) ;
#28835 = CIRCLE('',#75493,1.) ;
#28836 = CIRCLE('',#75494,1.) ;
#28837 = CIRCLE('',#75496,0.2) ;
#28838 = CIRCLE('',#75497,0.2) ;
#28839 = CIRCLE('',#75511,0.3) ;
#28840 = CIRCLE('',#75512,0.9) ;
#28841 = CIRCLE('',#75514,0.9) ;
#28842 = CIRCLE('',#75515,0.3) ;
#28843 = CIRCLE('',#75517,1.) ;
#28844 = CIRCLE('',#75518,1.) ;
#28845 = CIRCLE('',#75520,0.2) ;
#28846 = CIRCLE('',#75521,0.2) ;
#28847 = CIRCLE('',#75535,0.3) ;
#28848 = CIRCLE('',#75536,0.9) ;
#28849 = CIRCLE('',#75538,0.9) ;
#28850 = CIRCLE('',#75539,0.3) ;
#28851 = CIRCLE('',#75541,1.) ;
#28852 = CIRCLE('',#75542,1.) ;
#28853 = CIRCLE('',#75544,0.2) ;
#28854 = CIRCLE('',#75545,0.2) ;
#28855 = CIRCLE('',#75559,0.3) ;
#28856 = CIRCLE('',#75560,0.9) ;
#28857 = CIRCLE('',#75562,0.9) ;
#28858 = CIRCLE('',#75563,0.3) ;
#28859 = CIRCLE('',#75565,1.) ;
#28860 = CIRCLE('',#75566,1.) ;
#28861 = CIRCLE('',#75568,0.2) ;
#28862 = CIRCLE('',#75569,0.2) ;
#28863 = CIRCLE('',#75583,0.3) ;
#28864 = CIRCLE('',#75584,0.9) ;
#28865 = CIRCLE('',#75586,0.9) ;
#28866 = CIRCLE('',#75587,0.3) ;
#28867 = CIRCLE('',#75589,1.) ;
#28868 = CIRCLE('',#75590,1.) ;
#28869 = CIRCLE('',#75592,0.2) ;
#28870 = CIRCLE('',#75593,0.2) ;
#28871 = CIRCLE('',#75607,0.3) ;
#28872 = CIRCLE('',#75608,0.9) ;
#28873 = CIRCLE('',#75610,0.9) ;
#28874 = CIRCLE('',#75611,0.3) ;
#28875 = CIRCLE('',#75613,1.) ;
#28876 = CIRCLE('',#75614,1.) ;
#28877 = CIRCLE('',#75616,0.2) ;
#28878 = CIRCLE('',#75617,0.2) ;
#28879 = CIRCLE('',#75662,0.1) ;
#28880 = CIRCLE('',#75663,0.0999999999999998) ;
#28881 = CIRCLE('',#75665,0.1) ;
#28882 = CIRCLE('',#75666,0.1) ;
#28883 = CIRCLE('',#75668,0.0999999999999998) ;
#28884 = CIRCLE('',#75669,0.1) ;
#28885 = CIRCLE('',#75671,0.0999999999999999) ;
#28886 = CIRCLE('',#75672,0.1) ;
#28887 = CIRCLE('',#75674,0.1) ;
#28888 = CIRCLE('',#75676,0.0999999999999998) ;
#28889 = CIRCLE('',#75678,0.0999999999999998) ;
#28890 = CIRCLE('',#75680,0.0999999999999999) ;
#28891 = CIRCLE('',#75681,0.1) ;
#28892 = CIRCLE('',#75683,0.0999999999999998) ;
#28893 = CIRCLE('',#75685,0.1) ;
#28894 = CIRCLE('',#75687,0.1) ;
#28895 = CIRCLE('',#75689,0.0999999999999999) ;
#28896 = CIRCLE('',#75691,0.1) ;
#28897 = CIRCLE('',#75692,0.1) ;
#28898 = CIRCLE('',#75694,0.1) ;
#28899 = CIRCLE('',#75696,0.1) ;
#28900 = CIRCLE('',#75697,0.0999999999999998) ;
#28901 = CIRCLE('',#75699,0.1) ;
#28902 = CIRCLE('',#75700,0.1) ;
#28903 = CIRCLE('',#75702,0.0999999999999998) ;
#28904 = CIRCLE('',#75703,0.1) ;
#28905 = CIRCLE('',#75705,0.1) ;
#28906 = CIRCLE('',#75706,0.1) ;
#28907 = CIRCLE('',#75708,0.1) ;
#28908 = CIRCLE('',#75710,0.1) ;
#28909 = CIRCLE('',#75712,0.0999999999999998) ;
#28910 = CIRCLE('',#75714,0.1) ;
#28911 = CIRCLE('',#75715,0.1) ;
#28912 = CIRCLE('',#75717,0.0999999999999998) ;
#28913 = CIRCLE('',#75719,0.1) ;
#28914 = CIRCLE('',#75721,0.1) ;
#28915 = CIRCLE('',#75723,0.1) ;
#28916 = CIRCLE('',#75725,0.1) ;
#28917 = CIRCLE('',#75726,0.1) ;
#28918 = CIRCLE('',#75728,0.1) ;
#28919 = CIRCLE('',#75730,0.0999999999999997) ;
#28920 = CIRCLE('',#75731,0.0999999999999999) ;
#28921 = CIRCLE('',#75733,0.1) ;
#28922 = CIRCLE('',#75734,0.1) ;
#28923 = CIRCLE('',#75736,0.1) ;
#28924 = CIRCLE('',#75737,0.1) ;
#28925 = CIRCLE('',#75739,0.1) ;
#28926 = CIRCLE('',#75740,0.1) ;
#28927 = CIRCLE('',#75742,0.1) ;
#28928 = CIRCLE('',#75744,0.1) ;
#28929 = CIRCLE('',#75746,0.1) ;
#28930 = CIRCLE('',#75748,0.1) ;
#28931 = CIRCLE('',#75749,0.1) ;
#28932 = CIRCLE('',#75751,0.1) ;
#28933 = CIRCLE('',#75753,0.1) ;
#28934 = CIRCLE('',#75755,0.1) ;
#28935 = CIRCLE('',#75757,0.1) ;
#28936 = CIRCLE('',#75759,0.1) ;
#28937 = CIRCLE('',#75760,0.1) ;
#28938 = CIRCLE('',#75762,0.1) ;
#28939 = CIRCLE('',#75764,0.0999999999999999) ;
#28940 = CIRCLE('',#75765,0.1) ;
#28941 = CIRCLE('',#75767,0.1) ;
#28942 = CIRCLE('',#75768,0.1) ;
#28943 = CIRCLE('',#75770,0.1) ;
#28944 = CIRCLE('',#75771,0.1) ;
#28945 = CIRCLE('',#75773,0.1) ;
#28946 = CIRCLE('',#75774,0.1) ;
#28947 = CIRCLE('',#75776,0.1) ;
#28948 = CIRCLE('',#75778,0.1) ;
#28949 = CIRCLE('',#75780,0.1) ;
#28950 = CIRCLE('',#75782,0.0999999999999999) ;
#28951 = CIRCLE('',#75783,0.1) ;
#28952 = CIRCLE('',#75785,0.1) ;
#28953 = CIRCLE('',#75787,0.1) ;
#28954 = CIRCLE('',#75789,0.1) ;
#28955 = CIRCLE('',#75791,0.1) ;
#28956 = CIRCLE('',#75793,0.1) ;
#28957 = CIRCLE('',#75794,0.1) ;
#28958 = CIRCLE('',#75796,0.0999999999999997) ;
#28959 = CIRCLE('',#75798,0.0999999999999999) ;
#28960 = CIRCLE('',#75799,0.1) ;
#28961 = CIRCLE('',#75801,0.1) ;
#28962 = CIRCLE('',#75802,0.1) ;
#28963 = CIRCLE('',#75804,0.0999999999999994) ;
#28964 = CIRCLE('',#75805,0.1) ;
#28965 = CIRCLE('',#75807,0.1) ;
#28966 = CIRCLE('',#75808,0.1) ;
#28967 = CIRCLE('',#75810,0.1) ;
#28968 = CIRCLE('',#75812,0.0999999999999994) ;
#28969 = CIRCLE('',#75814,0.0999999999999994) ;
#28970 = CIRCLE('',#75816,0.1) ;
#28971 = CIRCLE('',#75817,0.1) ;
#28972 = CIRCLE('',#75819,0.0999999999999994) ;
#28973 = CIRCLE('',#75821,0.1) ;
#28974 = CIRCLE('',#75823,0.1) ;
#28975 = CIRCLE('',#75825,0.0999999999999998) ;
#28976 = CIRCLE('',#75827,0.1) ;
#28977 = CIRCLE('',#75828,0.1) ;
#28978 = CIRCLE('',#75830,0.1) ;
#28979 = CIRCLE('',#75832,0.1) ;
#28980 = CIRCLE('',#75833,0.1) ;
#28981 = CIRCLE('',#75835,0.1) ;
#28982 = CIRCLE('',#75836,0.1) ;
#28983 = CIRCLE('',#75838,0.0999999999999994) ;
#28984 = CIRCLE('',#75839,0.1) ;
#28985 = CIRCLE('',#75841,0.1) ;
#28986 = CIRCLE('',#75842,0.1) ;
#28987 = CIRCLE('',#75844,0.1) ;
#28988 = CIRCLE('',#75846,0.1) ;
#28989 = CIRCLE('',#75848,0.0999999999999994) ;
#28990 = CIRCLE('',#75850,0.1) ;
#28991 = CIRCLE('',#75851,0.1) ;
#28992 = CIRCLE('',#75853,0.0999999999999994) ;
#28993 = CIRCLE('',#75855,0.1) ;
#28994 = CIRCLE('',#75857,0.1) ;
#28995 = CIRCLE('',#75859,0.1) ;
#28996 = CIRCLE('',#75861,0.1) ;
#28997 = CIRCLE('',#75862,0.1) ;
#28998 = CIRCLE('',#75864,0.100000000000001) ;
#28999 = CIRCLE('',#75866,0.0999999999999999) ;
#29000 = CIRCLE('',#75867,0.0999999999999999) ;
#29001 = CIRCLE('',#75869,0.1) ;
#29002 = CIRCLE('',#75870,0.1) ;
#29003 = CIRCLE('',#75872,0.0999999999999994) ;
#29004 = CIRCLE('',#75873,0.1) ;
#29005 = CIRCLE('',#75875,0.1) ;
#29006 = CIRCLE('',#75876,0.1) ;
#29007 = CIRCLE('',#75878,0.1) ;
#29008 = CIRCLE('',#75880,0.0999999999999994) ;
#29009 = CIRCLE('',#75882,0.0999999999999994) ;
#29010 = CIRCLE('',#75884,0.1) ;
#29011 = CIRCLE('',#75885,0.1) ;
#29012 = CIRCLE('',#75887,0.0999999999999994) ;
#29013 = CIRCLE('',#75889,0.1) ;
#29014 = CIRCLE('',#75891,0.1) ;
#29015 = CIRCLE('',#75893,0.0999999999999999) ;
#29016 = CIRCLE('',#75895,0.1) ;
#29017 = CIRCLE('',#75896,0.1) ;
#29018 = CIRCLE('',#75898,0.0999999999999998) ;
#29019 = CIRCLE('',#75900,0.0999999999999999) ;
#29020 = CIRCLE('',#75901,0.0999999999999998) ;
#29021 = CIRCLE('',#75903,0.1) ;
#29022 = CIRCLE('',#75904,0.1) ;
#29023 = CIRCLE('',#75906,0.0999999999999994) ;
#29024 = CIRCLE('',#75907,0.1) ;
#29025 = CIRCLE('',#75909,0.1) ;
#29026 = CIRCLE('',#75910,0.1) ;
#29027 = CIRCLE('',#75912,0.1) ;
#29028 = CIRCLE('',#75914,0.1) ;
#29029 = CIRCLE('',#75916,0.0999999999999994) ;
#29030 = CIRCLE('',#75918,0.1) ;
#29031 = CIRCLE('',#75919,0.1) ;
#29032 = CIRCLE('',#75921,0.0999999999999994) ;
#29033 = CIRCLE('',#75923,0.1) ;
#29034 = CIRCLE('',#75925,0.1) ;
#29035 = CIRCLE('',#75927,0.0999999999999995) ;
#29036 = CIRCLE('',#75929,0.1) ;
#29037 = CIRCLE('',#75930,0.1) ;
#29038 = CIRCLE('',#75932,0.1) ;
#29039 = CIRCLE('',#75934,0.1) ;
#29040 = CIRCLE('',#75935,0.0999999999999999) ;
#29041 = CIRCLE('',#75937,0.1) ;
#29042 = CIRCLE('',#75938,0.1) ;
#29043 = CIRCLE('',#75940,0.0999999999999994) ;
#29044 = CIRCLE('',#75941,0.1) ;
#29045 = CIRCLE('',#75943,0.099999999999999) ;
#29046 = CIRCLE('',#75944,0.1) ;
#29047 = CIRCLE('',#75946,0.1) ;
#29048 = CIRCLE('',#75948,0.0999999999999994) ;
#29049 = CIRCLE('',#75950,0.0999999999999994) ;
#29050 = CIRCLE('',#75952,0.0999999999999999) ;
#29051 = CIRCLE('',#75953,0.1) ;
#29052 = CIRCLE('',#75955,0.0999999999999994) ;
#29053 = CIRCLE('',#75957,0.1) ;
#29054 = CIRCLE('',#75959,0.099999999999999) ;
#29055 = CIRCLE('',#75961,0.1) ;
#29056 = CIRCLE('',#75963,0.1) ;
#29057 = CIRCLE('',#75964,0.1) ;
#29058 = CIRCLE('',#75966,0.0999999999999995) ;
#29059 = CIRCLE('',#75968,0.0999999999999991) ;
#29060 = CIRCLE('',#75969,0.0999999999999995) ;
#29061 = CIRCLE('',#75971,0.1) ;
#29062 = CIRCLE('',#75972,0.1) ;
#29063 = CIRCLE('',#75974,0.0999999999999994) ;
#29064 = CIRCLE('',#75975,0.1) ;
#29065 = CIRCLE('',#75977,0.0999999999999989) ;
#29066 = CIRCLE('',#75978,0.099999999999999) ;
#29067 = CIRCLE('',#75980,0.1) ;
#29068 = CIRCLE('',#75982,0.0999999999999994) ;
#29069 = CIRCLE('',#75984,0.0999999999999994) ;
#29070 = CIRCLE('',#75986,0.1) ;
#29071 = CIRCLE('',#75987,0.1) ;
#29072 = CIRCLE('',#75989,0.0999999999999994) ;
#29073 = CIRCLE('',#75991,0.1) ;
#29074 = CIRCLE('',#75993,0.0999999999999989) ;
#29075 = CIRCLE('',#75995,0.0999999999999999) ;
#29076 = CIRCLE('',#75997,0.1) ;
#29077 = CIRCLE('',#75998,0.1) ;
#29078 = CIRCLE('',#76000,0.0999999999999989) ;
#29079 = CIRCLE('',#76002,0.1) ;
#29080 = CIRCLE('',#76003,0.0999999999999999) ;
#29081 = CIRCLE('',#76005,0.1) ;
#29082 = CIRCLE('',#76006,0.1) ;
#29083 = CIRCLE('',#76008,0.0999999999999994) ;
#29084 = CIRCLE('',#76009,0.1) ;
#29085 = CIRCLE('',#76011,0.099999999999999) ;
#29086 = CIRCLE('',#76012,0.1) ;
#29087 = CIRCLE('',#76014,0.1) ;
#29088 = CIRCLE('',#76016,0.0999999999999994) ;
#29089 = CIRCLE('',#76018,0.0999999999999994) ;
#29090 = CIRCLE('',#76020,0.0999999999999999) ;
#29091 = CIRCLE('',#76021,0.1) ;
#29092 = CIRCLE('',#76023,0.0999999999999994) ;
#29093 = CIRCLE('',#76025,0.1) ;
#29094 = CIRCLE('',#76027,0.099999999999999) ;
#29095 = CIRCLE('',#76029,0.1) ;
#29096 = CIRCLE('',#76031,0.1) ;
#29097 = CIRCLE('',#76032,0.1) ;
#29098 = CIRCLE('',#76034,0.0999999999999995) ;
#29099 = CIRCLE('',#76036,0.0999999999999991) ;
#29100 = CIRCLE('',#76037,0.0999999999999995) ;
#29101 = CIRCLE('',#76039,0.1) ;
#29102 = CIRCLE('',#76040,0.1) ;
#29103 = CIRCLE('',#76042,0.0999999999999994) ;
#29104 = CIRCLE('',#76043,0.1) ;
#29105 = CIRCLE('',#76045,0.0999999999999989) ;
#29106 = CIRCLE('',#76046,0.099999999999999) ;
#29107 = CIRCLE('',#76048,0.1) ;
#29108 = CIRCLE('',#76050,0.0999999999999994) ;
#29109 = CIRCLE('',#76052,0.0999999999999994) ;
#29110 = CIRCLE('',#76054,0.1) ;
#29111 = CIRCLE('',#76055,0.1) ;
#29112 = CIRCLE('',#76057,0.0999999999999994) ;
#29113 = CIRCLE('',#76059,0.1) ;
#29114 = CIRCLE('',#76061,0.0999999999999989) ;
#29115 = CIRCLE('',#76063,0.0999999999999999) ;
#29116 = CIRCLE('',#76065,0.1) ;
#29117 = CIRCLE('',#76066,0.1) ;
#29118 = CIRCLE('',#76068,0.0999999999999989) ;
#29119 = CIRCLE('',#76070,0.1) ;
#29120 = CIRCLE('',#76071,0.0999999999999999) ;
#29121 = CIRCLE('',#76073,0.1) ;
#29122 = CIRCLE('',#76074,0.1) ;
#29123 = CIRCLE('',#76076,0.0999999999999994) ;
#29124 = CIRCLE('',#76077,0.1) ;
#29125 = CIRCLE('',#76079,0.099999999999999) ;
#29126 = CIRCLE('',#76080,0.1) ;
#29127 = CIRCLE('',#76082,0.1) ;
#29128 = CIRCLE('',#76084,0.0999999999999994) ;
#29129 = CIRCLE('',#76086,0.0999999999999994) ;
#29130 = CIRCLE('',#76088,0.0999999999999999) ;
#29131 = CIRCLE('',#76089,0.1) ;
#29132 = CIRCLE('',#76091,0.0999999999999994) ;
#29133 = CIRCLE('',#76093,0.1) ;
#29134 = CIRCLE('',#76095,0.099999999999999) ;
#29135 = CIRCLE('',#76097,0.1) ;
#29136 = CIRCLE('',#76099,0.1) ;
#29137 = CIRCLE('',#76100,0.1) ;
#29138 = CIRCLE('',#76102,0.0999999999999995) ;
#29139 = CIRCLE('',#76104,0.0999999999999991) ;
#29140 = CIRCLE('',#76105,0.0999999999999995) ;
#29141 = CIRCLE('',#76107,0.1) ;
#29142 = CIRCLE('',#76108,0.1) ;
#29143 = CIRCLE('',#76110,0.0999999999999994) ;
#29144 = CIRCLE('',#76111,0.1) ;
#29145 = CIRCLE('',#76113,0.0999999999999989) ;
#29146 = CIRCLE('',#76114,0.099999999999999) ;
#29147 = CIRCLE('',#76116,0.1) ;
#29148 = CIRCLE('',#76118,0.0999999999999994) ;
#29149 = CIRCLE('',#76120,0.0999999999999994) ;
#29150 = CIRCLE('',#76122,0.1) ;
#29151 = CIRCLE('',#76123,0.1) ;
#29152 = CIRCLE('',#76125,0.0999999999999994) ;
#29153 = CIRCLE('',#76127,0.1) ;
#29154 = CIRCLE('',#76129,0.0999999999999989) ;
#29155 = CIRCLE('',#76131,0.0999999999999999) ;
#29156 = CIRCLE('',#76133,0.1) ;
#29157 = CIRCLE('',#76134,0.1) ;
#29158 = CIRCLE('',#76136,0.0999999999999989) ;
#29159 = CIRCLE('',#76138,0.1) ;
#29160 = CIRCLE('',#76139,0.0999999999999999) ;
#29161 = CIRCLE('',#76141,0.1) ;
#29162 = CIRCLE('',#76142,0.1) ;
#29163 = CIRCLE('',#76144,0.0999999999999994) ;
#29164 = CIRCLE('',#76145,0.1) ;
#29165 = CIRCLE('',#76147,0.099999999999999) ;
#29166 = CIRCLE('',#76148,0.1) ;
#29167 = CIRCLE('',#76150,0.1) ;
#29168 = CIRCLE('',#76152,0.0999999999999994) ;
#29169 = CIRCLE('',#76154,0.0999999999999994) ;
#29170 = CIRCLE('',#76156,0.0999999999999999) ;
#29171 = CIRCLE('',#76157,0.1) ;
#29172 = CIRCLE('',#76159,0.0999999999999994) ;
#29173 = CIRCLE('',#76161,0.1) ;
#29174 = CIRCLE('',#76163,0.099999999999999) ;
#29175 = CIRCLE('',#76165,0.1) ;
#29176 = CIRCLE('',#76167,0.1) ;
#29177 = CIRCLE('',#76168,0.1) ;
#29178 = CIRCLE('',#76170,0.0999999999999995) ;
#29179 = CIRCLE('',#76172,0.0999999999999991) ;
#29180 = CIRCLE('',#76173,0.0999999999999995) ;
#29181 = CIRCLE('',#76175,0.1) ;
#29182 = CIRCLE('',#76176,0.1) ;
#29183 = CIRCLE('',#76178,0.0999999999999994) ;
#29184 = CIRCLE('',#76179,0.1) ;
#29185 = CIRCLE('',#76181,0.0999999999999989) ;
#29186 = CIRCLE('',#76182,0.099999999999999) ;
#29187 = CIRCLE('',#76184,0.1) ;
#29188 = CIRCLE('',#76186,0.0999999999999994) ;
#29189 = CIRCLE('',#76188,0.0999999999999994) ;
#29190 = CIRCLE('',#76190,0.1) ;
#29191 = CIRCLE('',#76191,0.1) ;
#29192 = CIRCLE('',#76193,0.0999999999999994) ;
#29193 = CIRCLE('',#76195,0.1) ;
#29194 = CIRCLE('',#76197,0.0999999999999989) ;
#29195 = CIRCLE('',#76199,0.0999999999999999) ;
#29196 = CIRCLE('',#76201,0.1) ;
#29197 = CIRCLE('',#76202,0.1) ;
#29198 = CIRCLE('',#76204,0.0999999999999989) ;
#29199 = CIRCLE('',#76206,0.0999999999999997) ;
#29200 = CIRCLE('',#76207,0.0999999999999995) ;
#29201 = CIRCLE('',#76209,0.1) ;
#29202 = CIRCLE('',#76210,0.1) ;
#29203 = CIRCLE('',#76212,0.100000000000003) ;
#29204 = CIRCLE('',#76213,0.1) ;
#29205 = CIRCLE('',#76215,0.099999999999999) ;
#29206 = CIRCLE('',#76216,0.100000000000001) ;
#29207 = CIRCLE('',#76218,0.1) ;
#29208 = CIRCLE('',#76220,0.100000000000003) ;
#29209 = CIRCLE('',#76222,0.100000000000003) ;
#29210 = CIRCLE('',#76224,0.0999999999999995) ;
#29211 = CIRCLE('',#76225,0.1) ;
#29212 = CIRCLE('',#76227,0.100000000000003) ;
#29213 = CIRCLE('',#76229,0.1) ;
#29214 = CIRCLE('',#76231,0.099999999999999) ;
#29215 = CIRCLE('',#76233,0.1) ;
#29216 = CIRCLE('',#76235,0.1) ;
#29217 = CIRCLE('',#76236,0.1) ;
#29218 = CIRCLE('',#76238,0.0999999999999999) ;
#29219 = CIRCLE('',#76240,0.1) ;
#29220 = CIRCLE('',#76241,0.0999999999999983) ;
#29221 = CIRCLE('',#76243,0.1) ;
#29222 = CIRCLE('',#76244,0.1) ;
#29223 = CIRCLE('',#76246,0.100000000000003) ;
#29224 = CIRCLE('',#76247,0.1) ;
#29225 = CIRCLE('',#76249,0.0999999999999989) ;
#29226 = CIRCLE('',#76250,0.0999999999999998) ;
#29227 = CIRCLE('',#76252,0.1) ;
#29228 = CIRCLE('',#76254,0.1) ;
#29229 = CIRCLE('',#76256,0.100000000000003) ;
#29230 = CIRCLE('',#76258,0.0999999999999998) ;
#29231 = CIRCLE('',#76259,0.1) ;
#29232 = CIRCLE('',#76261,0.100000000000003) ;
#29233 = CIRCLE('',#76263,0.1) ;
#29234 = CIRCLE('',#76265,0.0999999999999989) ;
#29235 = CIRCLE('',#76267,0.1) ;
#29236 = CIRCLE('',#76269,0.1) ;
#29237 = CIRCLE('',#76270,0.1) ;
#29238 = CIRCLE('',#76272,0.100000000000001) ;
#29239 = CIRCLE('',#76274,0.1) ;
#29240 = CIRCLE('',#76276,0.1) ;
#29241 = CIRCLE('',#76278,0.1) ;
#29242 = CIRCLE('',#76280,0.1) ;
#29243 = CIRCLE('',#76282,0.1) ;
#29244 = CIRCLE('',#76284,0.1) ;
#29245 = CIRCLE('',#76287,0.0999999999999998) ;
#29246 = CIRCLE('',#76289,0.0999999999999998) ;
#29247 = CIRCLE('',#76291,0.1) ;
#29248 = CIRCLE('',#76293,0.0999999999999998) ;
#29249 = CIRCLE('',#76295,0.0999999999999998) ;
#29250 = CIRCLE('',#76297,0.0999999999999998) ;
#29251 = CIRCLE('',#76300,0.1) ;
#29252 = CIRCLE('',#76302,0.1) ;
#29253 = CIRCLE('',#76304,0.1) ;
#29254 = CIRCLE('',#76306,0.1) ;
#29255 = CIRCLE('',#76309,0.0999999999999998) ;
#29256 = CIRCLE('',#76311,0.1) ;
#29257 = CIRCLE('',#76313,0.0999999999999998) ;
#29258 = CIRCLE('',#76315,0.0999999999999998) ;
#29259 = CIRCLE('',#76318,0.0999999999999994) ;
#29260 = CIRCLE('',#76320,0.0999999999999994) ;
#29261 = CIRCLE('',#76322,0.1) ;
#29262 = CIRCLE('',#76324,0.0999999999999994) ;
#29263 = CIRCLE('',#76326,0.0999999999999994) ;
#29264 = CIRCLE('',#76328,0.0999999999999994) ;
#29265 = CIRCLE('',#76331,0.1) ;
#29266 = CIRCLE('',#76333,0.1) ;
#29267 = CIRCLE('',#76335,0.1) ;
#29268 = CIRCLE('',#76337,0.1) ;
#29269 = CIRCLE('',#76339,0.1) ;
#29270 = CIRCLE('',#76341,0.1) ;
#29271 = CIRCLE('',#76344,0.0999999999999994) ;
#29272 = CIRCLE('',#76346,0.1) ;
#29273 = CIRCLE('',#76348,0.0999999999999994) ;
#29274 = CIRCLE('',#76350,0.0999999999999994) ;
#29275 = CIRCLE('',#76353,0.1) ;
#29276 = CIRCLE('',#76355,0.1) ;
#29277 = CIRCLE('',#76357,0.1) ;
#29278 = CIRCLE('',#76359,0.1) ;
#29279 = CIRCLE('',#76362,0.0999999999999994) ;
#29280 = CIRCLE('',#76364,0.0999999999999994) ;
#29281 = CIRCLE('',#76366,0.1) ;
#29282 = CIRCLE('',#76368,0.0999999999999994) ;
#29283 = CIRCLE('',#76370,0.0999999999999994) ;
#29284 = CIRCLE('',#76372,0.0999999999999994) ;
#29285 = CIRCLE('',#76375,0.0999999999999994) ;
#29286 = CIRCLE('',#76377,0.0999999999999994) ;
#29287 = CIRCLE('',#76379,0.1) ;
#29288 = CIRCLE('',#76381,0.0999999999999994) ;
#29289 = CIRCLE('',#76383,0.0999999999999994) ;
#29290 = CIRCLE('',#76385,0.0999999999999994) ;
#29291 = CIRCLE('',#76388,0.0999999999999994) ;
#29292 = CIRCLE('',#76390,0.1) ;
#29293 = CIRCLE('',#76392,0.0999999999999994) ;
#29294 = CIRCLE('',#76394,0.0999999999999994) ;
#29295 = CIRCLE('',#76397,0.0999999999999994) ;
#29296 = CIRCLE('',#76399,0.1) ;
#29297 = CIRCLE('',#76401,0.0999999999999994) ;
#29298 = CIRCLE('',#76403,0.0999999999999994) ;
#29299 = CIRCLE('',#76406,0.0999999999999994) ;
#29300 = CIRCLE('',#76408,0.0999999999999994) ;
#29301 = CIRCLE('',#76410,0.0999999999999994) ;
#29302 = CIRCLE('',#76412,0.0999999999999994) ;
#29303 = CIRCLE('',#76414,0.0999999999999994) ;
#29304 = CIRCLE('',#76416,0.0999999999999994) ;
#29305 = CIRCLE('',#76419,0.0999999999999994) ;
#29306 = CIRCLE('',#76421,0.0999999999999994) ;
#29307 = CIRCLE('',#76423,0.1) ;
#29308 = CIRCLE('',#76425,0.0999999999999994) ;
#29309 = CIRCLE('',#76427,0.0999999999999994) ;
#29310 = CIRCLE('',#76429,0.0999999999999994) ;
#29311 = CIRCLE('',#76432,0.100000000000001) ;
#29312 = CIRCLE('',#76434,0.1) ;
#29313 = CIRCLE('',#76436,0.100000000000001) ;
#29314 = CIRCLE('',#76438,0.0999999999999994) ;
#29315 = CIRCLE('',#76441,0.0999999999999994) ;
#29316 = CIRCLE('',#76443,0.1) ;
#29317 = CIRCLE('',#76445,0.0999999999999994) ;
#29318 = CIRCLE('',#76447,0.0999999999999994) ;
#29319 = CIRCLE('',#76450,0.0999999999999994) ;
#29320 = CIRCLE('',#76452,0.0999999999999994) ;
#29321 = CIRCLE('',#76454,0.1) ;
#29322 = CIRCLE('',#76456,0.0999999999999994) ;
#29323 = CIRCLE('',#76458,0.0999999999999994) ;
#29324 = CIRCLE('',#76460,0.0999999999999994) ;
#29325 = CIRCLE('',#76463,0.0999999999999994) ;
#29326 = CIRCLE('',#76465,0.0999999999999994) ;
#29327 = CIRCLE('',#76467,0.1) ;
#29328 = CIRCLE('',#76469,0.0999999999999994) ;
#29329 = CIRCLE('',#76471,0.0999999999999994) ;
#29330 = CIRCLE('',#76473,0.0999999999999994) ;
#29331 = CIRCLE('',#76476,0.0999999999999994) ;
#29332 = CIRCLE('',#76478,0.1) ;
#29333 = CIRCLE('',#76480,0.0999999999999994) ;
#29334 = CIRCLE('',#76482,0.0999999999999994) ;
#29335 = CIRCLE('',#76485,0.0999999999999994) ;
#29336 = CIRCLE('',#76487,0.1) ;
#29337 = CIRCLE('',#76489,0.0999999999999994) ;
#29338 = CIRCLE('',#76491,0.0999999999999994) ;
#29339 = CIRCLE('',#76494,0.0999999999999994) ;
#29340 = CIRCLE('',#76496,0.0999999999999994) ;
#29341 = CIRCLE('',#76498,0.1) ;
#29342 = CIRCLE('',#76500,0.0999999999999994) ;
#29343 = CIRCLE('',#76502,0.0999999999999994) ;
#29344 = CIRCLE('',#76504,0.0999999999999994) ;
#29345 = CIRCLE('',#76507,0.0999999999999994) ;
#29346 = CIRCLE('',#76509,0.0999999999999994) ;
#29347 = CIRCLE('',#76511,0.1) ;
#29348 = CIRCLE('',#76513,0.0999999999999994) ;
#29349 = CIRCLE('',#76515,0.0999999999999994) ;
#29350 = CIRCLE('',#76517,0.0999999999999994) ;
#29351 = CIRCLE('',#76520,0.0999999999999994) ;
#29352 = CIRCLE('',#76522,0.1) ;
#29353 = CIRCLE('',#76524,0.0999999999999994) ;
#29354 = CIRCLE('',#76526,0.0999999999999994) ;
#29355 = CIRCLE('',#76529,0.0999999999999994) ;
#29356 = CIRCLE('',#76531,0.1) ;
#29357 = CIRCLE('',#76533,0.0999999999999994) ;
#29358 = CIRCLE('',#76535,0.0999999999999994) ;
#29359 = CIRCLE('',#76538,0.0999999999999994) ;
#29360 = CIRCLE('',#76540,0.0999999999999994) ;
#29361 = CIRCLE('',#76542,0.1) ;
#29362 = CIRCLE('',#76544,0.0999999999999994) ;
#29363 = CIRCLE('',#76546,0.0999999999999994) ;
#29364 = CIRCLE('',#76548,0.0999999999999994) ;
#29365 = CIRCLE('',#76551,0.0999999999999994) ;
#29366 = CIRCLE('',#76553,0.0999999999999994) ;
#29367 = CIRCLE('',#76555,0.1) ;
#29368 = CIRCLE('',#76557,0.0999999999999994) ;
#29369 = CIRCLE('',#76559,0.0999999999999994) ;
#29370 = CIRCLE('',#76561,0.0999999999999994) ;
#29371 = CIRCLE('',#76564,0.0999999999999994) ;
#29372 = CIRCLE('',#76566,0.1) ;
#29373 = CIRCLE('',#76568,0.0999999999999994) ;
#29374 = CIRCLE('',#76570,0.0999999999999994) ;
#29375 = CIRCLE('',#76573,0.0999999999999994) ;
#29376 = CIRCLE('',#76575,0.1) ;
#29377 = CIRCLE('',#76577,0.0999999999999994) ;
#29378 = CIRCLE('',#76579,0.0999999999999994) ;
#29379 = CIRCLE('',#76582,0.0999999999999994) ;
#29380 = CIRCLE('',#76584,0.0999999999999994) ;
#29381 = CIRCLE('',#76586,0.1) ;
#29382 = CIRCLE('',#76588,0.0999999999999994) ;
#29383 = CIRCLE('',#76590,0.0999999999999994) ;
#29384 = CIRCLE('',#76592,0.0999999999999994) ;
#29385 = CIRCLE('',#76595,0.0999999999999994) ;
#29386 = CIRCLE('',#76597,0.0999999999999994) ;
#29387 = CIRCLE('',#76599,0.1) ;
#29388 = CIRCLE('',#76601,0.0999999999999994) ;
#29389 = CIRCLE('',#76603,0.0999999999999994) ;
#29390 = CIRCLE('',#76605,0.0999999999999994) ;
#29391 = CIRCLE('',#76608,0.0999999999999994) ;
#29392 = CIRCLE('',#76610,0.1) ;
#29393 = CIRCLE('',#76612,0.0999999999999994) ;
#29394 = CIRCLE('',#76614,0.0999999999999994) ;
#29395 = CIRCLE('',#76617,0.0999999999999994) ;
#29396 = CIRCLE('',#76619,0.1) ;
#29397 = CIRCLE('',#76621,0.0999999999999994) ;
#29398 = CIRCLE('',#76623,0.0999999999999994) ;
#29399 = CIRCLE('',#76626,0.100000000000003) ;
#29400 = CIRCLE('',#76628,0.100000000000003) ;
#29401 = CIRCLE('',#76630,0.1) ;
#29402 = CIRCLE('',#76632,0.100000000000003) ;
#29403 = CIRCLE('',#76634,0.100000000000003) ;
#29404 = CIRCLE('',#76636,0.100000000000003) ;
#29405 = CIRCLE('',#76639,0.100000000000003) ;
#29406 = CIRCLE('',#76641,0.100000000000003) ;
#29407 = CIRCLE('',#76643,0.1) ;
#29408 = CIRCLE('',#76645,0.100000000000003) ;
#29409 = CIRCLE('',#76647,0.100000000000003) ;
#29410 = CIRCLE('',#76649,0.100000000000003) ;
#29411 = CIRCLE('',#76652,0.100000000000003) ;
#29412 = CIRCLE('',#76654,0.1) ;
#29413 = CIRCLE('',#76656,0.100000000000003) ;
#29414 = CIRCLE('',#76658,0.100000000000003) ;
#29415 = CIRCLE('',#76661,0.100000000000003) ;
#29416 = CIRCLE('',#76663,0.1) ;
#29417 = CIRCLE('',#76665,0.100000000000003) ;
#29418 = CIRCLE('',#76667,0.100000000000003) ;
#29419 = CIRCLE('',#76681,1.5) ;
#29420 = CIRCLE('',#76690,1.5) ;
#29421 = CIRCLE('',#76695,1.22936706250017) ;
#29422 = CIRCLE('',#76697,1.25) ;
#29423 = CIRCLE('',#76698,1.6) ;
#29424 = CIRCLE('',#76700,1.25) ;
#29425 = CIRCLE('',#76703,1.6) ;
#29426 = CIRCLE('',#76704,0.1) ;
#29427 = CIRCLE('',#76706,0.999999999999998) ;
#29428 = CIRCLE('',#76708,2.49807621135332) ;
#29429 = CIRCLE('',#76709,2.49807621135332) ;
#29430 = CIRCLE('',#76711,2.49807621135332) ;
#29431 = CIRCLE('',#76712,2.49807621135332) ;
#29432 = CIRCLE('',#76714,2.49807621135332) ;
#29433 = CIRCLE('',#76715,2.49807621135332) ;
#29434 = CIRCLE('',#76717,2.49807621135332) ;
#29435 = CIRCLE('',#76718,2.49807621135332) ;
#29436 = CIRCLE('',#76720,2.49807621135332) ;
#29437 = CIRCLE('',#76721,2.49807621135332) ;
#29438 = CIRCLE('',#76723,2.49807621135332) ;
#29439 = CIRCLE('',#76724,2.49807621135332) ;
#29440 = CIRCLE('',#76726,2.25) ;
#29441 = CIRCLE('',#76728,2.25) ;
#29442 = CIRCLE('',#76730,2.25) ;
#29443 = CIRCLE('',#76732,2.25) ;
#29444 = CIRCLE('',#76734,2.25) ;
#29445 = CIRCLE('',#76736,2.25) ;
#29446 = CIRCLE('',#76738,2.25) ;
#29447 = CIRCLE('',#76740,2.25) ;
#29448 = CIRCLE('',#76742,2.25) ;
#29449 = CIRCLE('',#76744,2.25) ;
#29450 = CIRCLE('',#76746,2.25) ;
#29451 = CIRCLE('',#76748,2.25) ;
#29452 = CIRCLE('',#76758,2.37313871770562) ;
#29453 = CIRCLE('',#76764,0.556) ;
#29454 = CIRCLE('',#76765,0.556) ;
#29455 = CIRCLE('',#76766,0.556) ;
#29456 = CIRCLE('',#76767,0.556) ;
#29457 = CIRCLE('',#76768,0.556) ;
#29458 = CIRCLE('',#76769,0.556) ;
#29459 = CIRCLE('',#76770,0.556) ;
#29460 = CIRCLE('',#76771,0.556) ;
#29461 = CIRCLE('',#76772,0.556) ;
#29462 = CIRCLE('',#76773,0.556) ;
#29463 = CIRCLE('',#76774,0.556) ;
#29464 = CIRCLE('',#76775,0.556) ;
#29465 = CIRCLE('',#76776,0.556) ;
#29466 = CIRCLE('',#76777,0.556) ;
#29467 = CIRCLE('',#76778,0.556) ;
#29468 = CIRCLE('',#76779,0.556) ;
#29469 = CIRCLE('',#76780,0.556) ;
#29470 = CIRCLE('',#76784,1.6) ;
#29471 = CIRCLE('',#76785,0.1) ;
#29472 = CIRCLE('',#76786,1.5) ;
#29473 = CIRCLE('',#76788,2.67441860465116) ;
#29474 = CIRCLE('',#76789,0.27) ;
#29475 = CIRCLE('',#76790,2.8) ;
#29476 = CIRCLE('',#76792,2.8) ;
#29477 = CIRCLE('',#76794,1.5) ;
#29478 = CIRCLE('',#76796,4.90340272700175) ;
#29479 = CIRCLE('',#76797,4.98629120689917) ;
#29480 = CIRCLE('',#76798,0.675169614150692) ;
#29481 = CIRCLE('',#76799,4.98629120689917) ;
#29482 = CIRCLE('',#76800,4.90340272700175) ;
#29483 = CIRCLE('',#76801,4.98629120689917) ;
#29484 = CIRCLE('',#76802,0.675169614150692) ;
#29485 = CIRCLE('',#76803,4.98629120689917) ;
#29486 = CIRCLE('',#76804,4.90340272700175) ;
#29487 = CIRCLE('',#76805,4.98629120689917) ;
#29488 = CIRCLE('',#76806,0.675169614150692) ;
#29489 = CIRCLE('',#76807,4.98629120689917) ;
#29490 = CIRCLE('',#76808,4.90340272700175) ;
#29491 = CIRCLE('',#76809,4.98629120689917) ;
#29492 = CIRCLE('',#76810,0.675169614150692) ;
#29493 = CIRCLE('',#76811,4.98629120689917) ;
#29494 = VERTEX_POINT('',#99149) ;
#29495 = VERTEX_POINT('',#99150) ;
#29496 = VERTEX_POINT('',#99153) ;
#29497 = VERTEX_POINT('',#99157) ;
#29498 = VERTEX_POINT('',#99159) ;
#29499 = VERTEX_POINT('',#99161) ;
#29500 = VERTEX_POINT('',#99165) ;
#29501 = VERTEX_POINT('',#99166) ;
#29502 = VERTEX_POINT('',#99169) ;
#29503 = VERTEX_POINT('',#99171) ;
#29504 = VERTEX_POINT('',#99175) ;
#29505 = VERTEX_POINT('',#99177) ;
#29506 = VERTEX_POINT('',#99181) ;
#29507 = VERTEX_POINT('',#99182) ;
#29508 = VERTEX_POINT('',#99185) ;
#29509 = VERTEX_POINT('',#99187) ;
#29510 = VERTEX_POINT('',#99191) ;
#29511 = VERTEX_POINT('',#99193) ;
#29512 = VERTEX_POINT('',#99197) ;
#29513 = VERTEX_POINT('',#99203) ;
#29514 = VERTEX_POINT('',#99211) ;
#29515 = VERTEX_POINT('',#99212) ;
#29516 = VERTEX_POINT('',#99214) ;
#29517 = VERTEX_POINT('',#99216) ;
#29518 = VERTEX_POINT('',#99218) ;
#29519 = VERTEX_POINT('',#99220) ;
#29520 = VERTEX_POINT('',#99223) ;
#29521 = VERTEX_POINT('',#99224) ;
#29522 = VERTEX_POINT('',#99226) ;
#29523 = VERTEX_POINT('',#99228) ;
#29524 = VERTEX_POINT('',#99230) ;
#29525 = VERTEX_POINT('',#99232) ;
#29526 = VERTEX_POINT('',#99234) ;
#29527 = VERTEX_POINT('',#99236) ;
#29528 = VERTEX_POINT('',#99240) ;
#29529 = VERTEX_POINT('',#99241) ;
#29530 = VERTEX_POINT('',#99243) ;
#29531 = VERTEX_POINT('',#99245) ;
#29532 = VERTEX_POINT('',#99247) ;
#29533 = VERTEX_POINT('',#99249) ;
#29534 = VERTEX_POINT('',#99252) ;
#29535 = VERTEX_POINT('',#99253) ;
#29536 = VERTEX_POINT('',#99255) ;
#29537 = VERTEX_POINT('',#99257) ;
#29538 = VERTEX_POINT('',#99259) ;
#29539 = VERTEX_POINT('',#99261) ;
#29540 = VERTEX_POINT('',#99263) ;
#29541 = VERTEX_POINT('',#99265) ;
#29542 = VERTEX_POINT('',#99269) ;
#29543 = VERTEX_POINT('',#99270) ;
#29544 = VERTEX_POINT('',#99272) ;
#29545 = VERTEX_POINT('',#99274) ;
#29546 = VERTEX_POINT('',#99276) ;
#29547 = VERTEX_POINT('',#99278) ;
#29548 = VERTEX_POINT('',#99280) ;
#29549 = VERTEX_POINT('',#99282) ;
#29550 = VERTEX_POINT('',#99284) ;
#29551 = VERTEX_POINT('',#99286) ;
#29552 = VERTEX_POINT('',#99288) ;
#29553 = VERTEX_POINT('',#99291) ;
#29554 = VERTEX_POINT('',#99292) ;
#29555 = VERTEX_POINT('',#99294) ;
#29556 = VERTEX_POINT('',#99296) ;
#29557 = VERTEX_POINT('',#99298) ;
#29558 = VERTEX_POINT('',#99300) ;
#29559 = VERTEX_POINT('',#99302) ;
#29560 = VERTEX_POINT('',#99304) ;
#29561 = VERTEX_POINT('',#99307) ;
#29562 = VERTEX_POINT('',#99308) ;
#29563 = VERTEX_POINT('',#99310) ;
#29564 = VERTEX_POINT('',#99312) ;
#29565 = VERTEX_POINT('',#99314) ;
#29566 = VERTEX_POINT('',#99316) ;
#29567 = VERTEX_POINT('',#99318) ;
#29568 = VERTEX_POINT('',#99320) ;
#29569 = VERTEX_POINT('',#99323) ;
#29570 = VERTEX_POINT('',#99324) ;
#29571 = VERTEX_POINT('',#99326) ;
#29572 = VERTEX_POINT('',#99328) ;
#29573 = VERTEX_POINT('',#99330) ;
#29574 = VERTEX_POINT('',#99332) ;
#29575 = VERTEX_POINT('',#99334) ;
#29576 = VERTEX_POINT('',#99336) ;
#29577 = VERTEX_POINT('',#99339) ;
#29578 = VERTEX_POINT('',#99340) ;
#29579 = VERTEX_POINT('',#99342) ;
#29580 = VERTEX_POINT('',#99344) ;
#29581 = VERTEX_POINT('',#99346) ;
#29582 = VERTEX_POINT('',#99348) ;
#29583 = VERTEX_POINT('',#99350) ;
#29584 = VERTEX_POINT('',#99352) ;
#29585 = VERTEX_POINT('',#99356) ;
#29586 = VERTEX_POINT('',#99357) ;
#29587 = VERTEX_POINT('',#99359) ;
#29588 = VERTEX_POINT('',#99361) ;
#29589 = VERTEX_POINT('',#99363) ;
#29590 = VERTEX_POINT('',#99365) ;
#29591 = VERTEX_POINT('',#99367) ;
#29592 = VERTEX_POINT('',#99369) ;
#29593 = VERTEX_POINT('',#99371) ;
#29594 = VERTEX_POINT('',#99373) ;
#29595 = VERTEX_POINT('',#99375) ;
#29596 = VERTEX_POINT('',#99378) ;
#29597 = VERTEX_POINT('',#99379) ;
#29598 = VERTEX_POINT('',#99381) ;
#29599 = VERTEX_POINT('',#99383) ;
#29600 = VERTEX_POINT('',#99385) ;
#29601 = VERTEX_POINT('',#99387) ;
#29602 = VERTEX_POINT('',#99389) ;
#29603 = VERTEX_POINT('',#99391) ;
#29604 = VERTEX_POINT('',#99394) ;
#29605 = VERTEX_POINT('',#99395) ;
#29606 = VERTEX_POINT('',#99397) ;
#29607 = VERTEX_POINT('',#99399) ;
#29608 = VERTEX_POINT('',#99401) ;
#29609 = VERTEX_POINT('',#99403) ;
#29610 = VERTEX_POINT('',#99405) ;
#29611 = VERTEX_POINT('',#99407) ;
#29612 = VERTEX_POINT('',#99410) ;
#29613 = VERTEX_POINT('',#99411) ;
#29614 = VERTEX_POINT('',#99413) ;
#29615 = VERTEX_POINT('',#99415) ;
#29616 = VERTEX_POINT('',#99417) ;
#29617 = VERTEX_POINT('',#99419) ;
#29618 = VERTEX_POINT('',#99421) ;
#29619 = VERTEX_POINT('',#99423) ;
#29620 = VERTEX_POINT('',#99426) ;
#29621 = VERTEX_POINT('',#99427) ;
#29622 = VERTEX_POINT('',#99429) ;
#29623 = VERTEX_POINT('',#99431) ;
#29624 = VERTEX_POINT('',#99433) ;
#29625 = VERTEX_POINT('',#99435) ;
#29626 = VERTEX_POINT('',#99437) ;
#29627 = VERTEX_POINT('',#99439) ;
#29628 = VERTEX_POINT('',#99443) ;
#29629 = VERTEX_POINT('',#99444) ;
#29630 = VERTEX_POINT('',#99446) ;
#29631 = VERTEX_POINT('',#99448) ;
#29632 = VERTEX_POINT('',#99450) ;
#29633 = VERTEX_POINT('',#99452) ;
#29634 = VERTEX_POINT('',#99454) ;
#29635 = VERTEX_POINT('',#99456) ;
#29636 = VERTEX_POINT('',#99458) ;
#29637 = VERTEX_POINT('',#99460) ;
#29638 = VERTEX_POINT('',#99462) ;
#29639 = VERTEX_POINT('',#99465) ;
#29640 = VERTEX_POINT('',#99466) ;
#29641 = VERTEX_POINT('',#99468) ;
#29642 = VERTEX_POINT('',#99470) ;
#29643 = VERTEX_POINT('',#99472) ;
#29644 = VERTEX_POINT('',#99474) ;
#29645 = VERTEX_POINT('',#99476) ;
#29646 = VERTEX_POINT('',#99478) ;
#29647 = VERTEX_POINT('',#99481) ;
#29648 = VERTEX_POINT('',#99482) ;
#29649 = VERTEX_POINT('',#99484) ;
#29650 = VERTEX_POINT('',#99486) ;
#29651 = VERTEX_POINT('',#99488) ;
#29652 = VERTEX_POINT('',#99490) ;
#29653 = VERTEX_POINT('',#99492) ;
#29654 = VERTEX_POINT('',#99494) ;
#29655 = VERTEX_POINT('',#99497) ;
#29656 = VERTEX_POINT('',#99498) ;
#29657 = VERTEX_POINT('',#99500) ;
#29658 = VERTEX_POINT('',#99502) ;
#29659 = VERTEX_POINT('',#99504) ;
#29660 = VERTEX_POINT('',#99506) ;
#29661 = VERTEX_POINT('',#99508) ;
#29662 = VERTEX_POINT('',#99510) ;
#29663 = VERTEX_POINT('',#99513) ;
#29664 = VERTEX_POINT('',#99514) ;
#29665 = VERTEX_POINT('',#99516) ;
#29666 = VERTEX_POINT('',#99518) ;
#29667 = VERTEX_POINT('',#99520) ;
#29668 = VERTEX_POINT('',#99522) ;
#29669 = VERTEX_POINT('',#99524) ;
#29670 = VERTEX_POINT('',#99526) ;
#29671 = VERTEX_POINT('',#99529) ;
#29672 = VERTEX_POINT('',#99530) ;
#29673 = VERTEX_POINT('',#99532) ;
#29674 = VERTEX_POINT('',#99534) ;
#29675 = VERTEX_POINT('',#99536) ;
#29676 = VERTEX_POINT('',#99538) ;
#29677 = VERTEX_POINT('',#99540) ;
#29678 = VERTEX_POINT('',#99542) ;
#29679 = VERTEX_POINT('',#99545) ;
#29680 = VERTEX_POINT('',#99546) ;
#29681 = VERTEX_POINT('',#99548) ;
#29682 = VERTEX_POINT('',#99550) ;
#29683 = VERTEX_POINT('',#99552) ;
#29684 = VERTEX_POINT('',#99554) ;
#29685 = VERTEX_POINT('',#99556) ;
#29686 = VERTEX_POINT('',#99558) ;
#29687 = VERTEX_POINT('',#99561) ;
#29688 = VERTEX_POINT('',#99562) ;
#29689 = VERTEX_POINT('',#99564) ;
#29690 = VERTEX_POINT('',#99566) ;
#29691 = VERTEX_POINT('',#99568) ;
#29692 = VERTEX_POINT('',#99570) ;
#29693 = VERTEX_POINT('',#99572) ;
#29694 = VERTEX_POINT('',#99574) ;
#29695 = VERTEX_POINT('',#99578) ;
#29696 = VERTEX_POINT('',#99579) ;
#29697 = VERTEX_POINT('',#99581) ;
#29698 = VERTEX_POINT('',#99583) ;
#29699 = VERTEX_POINT('',#99585) ;
#29700 = VERTEX_POINT('',#99587) ;
#29701 = VERTEX_POINT('',#99589) ;
#29702 = VERTEX_POINT('',#99591) ;
#29703 = VERTEX_POINT('',#99593) ;
#29704 = VERTEX_POINT('',#99595) ;
#29705 = VERTEX_POINT('',#99597) ;
#29706 = VERTEX_POINT('',#99600) ;
#29707 = VERTEX_POINT('',#99601) ;
#29708 = VERTEX_POINT('',#99603) ;
#29709 = VERTEX_POINT('',#99605) ;
#29710 = VERTEX_POINT('',#99607) ;
#29711 = VERTEX_POINT('',#99609) ;
#29712 = VERTEX_POINT('',#99611) ;
#29713 = VERTEX_POINT('',#99613) ;
#29714 = VERTEX_POINT('',#99616) ;
#29715 = VERTEX_POINT('',#99617) ;
#29716 = VERTEX_POINT('',#99619) ;
#29717 = VERTEX_POINT('',#99621) ;
#29718 = VERTEX_POINT('',#99623) ;
#29719 = VERTEX_POINT('',#99625) ;
#29720 = VERTEX_POINT('',#99627) ;
#29721 = VERTEX_POINT('',#99629) ;
#29722 = VERTEX_POINT('',#99632) ;
#29723 = VERTEX_POINT('',#99633) ;
#29724 = VERTEX_POINT('',#99635) ;
#29725 = VERTEX_POINT('',#99637) ;
#29726 = VERTEX_POINT('',#99639) ;
#29727 = VERTEX_POINT('',#99641) ;
#29728 = VERTEX_POINT('',#99643) ;
#29729 = VERTEX_POINT('',#99645) ;
#29730 = VERTEX_POINT('',#99648) ;
#29731 = VERTEX_POINT('',#99649) ;
#29732 = VERTEX_POINT('',#99651) ;
#29733 = VERTEX_POINT('',#99653) ;
#29734 = VERTEX_POINT('',#99655) ;
#29735 = VERTEX_POINT('',#99657) ;
#29736 = VERTEX_POINT('',#99659) ;
#29737 = VERTEX_POINT('',#99661) ;
#29738 = VERTEX_POINT('',#99664) ;
#29739 = VERTEX_POINT('',#99665) ;
#29740 = VERTEX_POINT('',#99667) ;
#29741 = VERTEX_POINT('',#99669) ;
#29742 = VERTEX_POINT('',#99671) ;
#29743 = VERTEX_POINT('',#99673) ;
#29744 = VERTEX_POINT('',#99675) ;
#29745 = VERTEX_POINT('',#99677) ;
#29746 = VERTEX_POINT('',#99680) ;
#29747 = VERTEX_POINT('',#99681) ;
#29748 = VERTEX_POINT('',#99683) ;
#29749 = VERTEX_POINT('',#99685) ;
#29750 = VERTEX_POINT('',#99687) ;
#29751 = VERTEX_POINT('',#99689) ;
#29752 = VERTEX_POINT('',#99691) ;
#29753 = VERTEX_POINT('',#99693) ;
#29754 = VERTEX_POINT('',#99696) ;
#29755 = VERTEX_POINT('',#99697) ;
#29756 = VERTEX_POINT('',#99699) ;
#29757 = VERTEX_POINT('',#99701) ;
#29758 = VERTEX_POINT('',#99703) ;
#29759 = VERTEX_POINT('',#99705) ;
#29760 = VERTEX_POINT('',#99707) ;
#29761 = VERTEX_POINT('',#99709) ;
#29762 = VERTEX_POINT('',#99713) ;
#29763 = VERTEX_POINT('',#99714) ;
#29764 = VERTEX_POINT('',#99716) ;
#29765 = VERTEX_POINT('',#99718) ;
#29766 = VERTEX_POINT('',#99720) ;
#29767 = VERTEX_POINT('',#99722) ;
#29768 = VERTEX_POINT('',#99724) ;
#29769 = VERTEX_POINT('',#99726) ;
#29770 = VERTEX_POINT('',#99728) ;
#29771 = VERTEX_POINT('',#99730) ;
#29772 = VERTEX_POINT('',#99734) ;
#29773 = VERTEX_POINT('',#99735) ;
#29774 = VERTEX_POINT('',#99737) ;
#29775 = VERTEX_POINT('',#99739) ;
#29776 = VERTEX_POINT('',#99741) ;
#29777 = VERTEX_POINT('',#99743) ;
#29778 = VERTEX_POINT('',#99745) ;
#29779 = VERTEX_POINT('',#99747) ;
#29780 = VERTEX_POINT('',#99749) ;
#29781 = VERTEX_POINT('',#99751) ;
#29782 = VERTEX_POINT('',#99755) ;
#29783 = VERTEX_POINT('',#99756) ;
#29784 = VERTEX_POINT('',#99758) ;
#29785 = VERTEX_POINT('',#99760) ;
#29786 = VERTEX_POINT('',#99764) ;
#29787 = VERTEX_POINT('',#99765) ;
#29788 = VERTEX_POINT('',#99767) ;
#29789 = VERTEX_POINT('',#99769) ;
#29790 = VERTEX_POINT('',#99773) ;
#29791 = VERTEX_POINT('',#99774) ;
#29792 = VERTEX_POINT('',#99776) ;
#29793 = VERTEX_POINT('',#99778) ;
#29794 = VERTEX_POINT('',#99782) ;
#29795 = VERTEX_POINT('',#99783) ;
#29796 = VERTEX_POINT('',#99785) ;
#29797 = VERTEX_POINT('',#99787) ;
#29798 = VERTEX_POINT('',#99791) ;
#29799 = VERTEX_POINT('',#99792) ;
#29800 = VERTEX_POINT('',#99794) ;
#29801 = VERTEX_POINT('',#99796) ;
#29802 = VERTEX_POINT('',#99800) ;
#29803 = VERTEX_POINT('',#99802) ;
#29804 = VERTEX_POINT('',#99815) ;
#29805 = VERTEX_POINT('',#99816) ;
#29806 = VERTEX_POINT('',#99818) ;
#29807 = VERTEX_POINT('',#99820) ;
#29808 = VERTEX_POINT('',#99824) ;
#29809 = VERTEX_POINT('',#99825) ;
#29810 = VERTEX_POINT('',#99827) ;
#29811 = VERTEX_POINT('',#99829) ;
#29812 = VERTEX_POINT('',#99833) ;
#29813 = VERTEX_POINT('',#99834) ;
#29814 = VERTEX_POINT('',#99836) ;
#29815 = VERTEX_POINT('',#99838) ;
#29816 = VERTEX_POINT('',#99842) ;
#29817 = VERTEX_POINT('',#99843) ;
#29818 = VERTEX_POINT('',#99845) ;
#29819 = VERTEX_POINT('',#99847) ;
#29820 = VERTEX_POINT('',#99851) ;
#29821 = VERTEX_POINT('',#99852) ;
#29822 = VERTEX_POINT('',#99854) ;
#29823 = VERTEX_POINT('',#99856) ;
#29824 = VERTEX_POINT('',#99860) ;
#29825 = VERTEX_POINT('',#99861) ;
#29826 = VERTEX_POINT('',#99863) ;
#29827 = VERTEX_POINT('',#99865) ;
#29828 = VERTEX_POINT('',#99869) ;
#29829 = VERTEX_POINT('',#99871) ;
#29830 = VERTEX_POINT('',#99877) ;
#29831 = VERTEX_POINT('',#99878) ;
#29832 = VERTEX_POINT('',#99880) ;
#29833 = VERTEX_POINT('',#99882) ;
#29834 = VERTEX_POINT('',#99886) ;
#29835 = VERTEX_POINT('',#99887) ;
#29836 = VERTEX_POINT('',#99889) ;
#29837 = VERTEX_POINT('',#99891) ;
#29838 = VERTEX_POINT('',#99895) ;
#29839 = VERTEX_POINT('',#99896) ;
#29840 = VERTEX_POINT('',#99898) ;
#29841 = VERTEX_POINT('',#99900) ;
#29842 = VERTEX_POINT('',#99919) ;
#29843 = VERTEX_POINT('',#99920) ;
#29844 = VERTEX_POINT('',#99933) ;
#29845 = VERTEX_POINT('',#99934) ;
#29846 = VERTEX_POINT('',#99936) ;
#29847 = VERTEX_POINT('',#99938) ;
#29848 = VERTEX_POINT('',#99942) ;
#29849 = VERTEX_POINT('',#99943) ;
#29850 = VERTEX_POINT('',#99945) ;
#29851 = VERTEX_POINT('',#99947) ;
#29852 = VERTEX_POINT('',#99951) ;
#29853 = VERTEX_POINT('',#99952) ;
#29854 = VERTEX_POINT('',#99954) ;
#29855 = VERTEX_POINT('',#99956) ;
#29856 = VERTEX_POINT('',#99960) ;
#29857 = VERTEX_POINT('',#99961) ;
#29858 = VERTEX_POINT('',#99963) ;
#29859 = VERTEX_POINT('',#99965) ;
#29860 = VERTEX_POINT('',#99969) ;
#29861 = VERTEX_POINT('',#99970) ;
#29862 = VERTEX_POINT('',#99972) ;
#29863 = VERTEX_POINT('',#99974) ;
#29864 = VERTEX_POINT('',#99978) ;
#29865 = VERTEX_POINT('',#99979) ;
#29866 = VERTEX_POINT('',#99981) ;
#29867 = VERTEX_POINT('',#99983) ;
#29868 = VERTEX_POINT('',#99989) ;
#29869 = VERTEX_POINT('',#99990) ;
#29870 = VERTEX_POINT('',#99995) ;
#29871 = VERTEX_POINT('',#99996) ;
#29872 = VERTEX_POINT('',#99998) ;
#29873 = VERTEX_POINT('',#100000) ;
#29874 = VERTEX_POINT('',#100004) ;
#29875 = VERTEX_POINT('',#100005) ;
#29876 = VERTEX_POINT('',#100007) ;
#29877 = VERTEX_POINT('',#100009) ;
#29878 = VERTEX_POINT('',#100013) ;
#29879 = VERTEX_POINT('',#100014) ;
#29880 = VERTEX_POINT('',#100016) ;
#29881 = VERTEX_POINT('',#100018) ;
#29882 = VERTEX_POINT('',#100022) ;
#29883 = VERTEX_POINT('',#100023) ;
#29884 = VERTEX_POINT('',#100025) ;
#29885 = VERTEX_POINT('',#100027) ;
#29886 = VERTEX_POINT('',#100031) ;
#29887 = VERTEX_POINT('',#100032) ;
#29888 = VERTEX_POINT('',#100034) ;
#29889 = VERTEX_POINT('',#100036) ;
#29890 = VERTEX_POINT('',#100040) ;
#29891 = VERTEX_POINT('',#100041) ;
#29892 = VERTEX_POINT('',#100043) ;
#29893 = VERTEX_POINT('',#100045) ;
#29894 = VERTEX_POINT('',#100049) ;
#29895 = VERTEX_POINT('',#100050) ;
#29896 = VERTEX_POINT('',#100052) ;
#29897 = VERTEX_POINT('',#100054) ;
#29898 = VERTEX_POINT('',#100058) ;
#29899 = VERTEX_POINT('',#100059) ;
#29900 = VERTEX_POINT('',#100061) ;
#29901 = VERTEX_POINT('',#100063) ;
#29902 = VERTEX_POINT('',#100067) ;
#29903 = VERTEX_POINT('',#100068) ;
#29904 = VERTEX_POINT('',#100070) ;
#29905 = VERTEX_POINT('',#100072) ;
#29906 = VERTEX_POINT('',#100076) ;
#29907 = VERTEX_POINT('',#100077) ;
#29908 = VERTEX_POINT('',#100079) ;
#29909 = VERTEX_POINT('',#100081) ;
#29910 = VERTEX_POINT('',#100085) ;
#29911 = VERTEX_POINT('',#100086) ;
#29912 = VERTEX_POINT('',#100088) ;
#29913 = VERTEX_POINT('',#100090) ;
#29914 = VERTEX_POINT('',#100094) ;
#29915 = VERTEX_POINT('',#100095) ;
#29916 = VERTEX_POINT('',#100097) ;
#29917 = VERTEX_POINT('',#100099) ;
#29918 = VERTEX_POINT('',#100103) ;
#29919 = VERTEX_POINT('',#100104) ;
#29920 = VERTEX_POINT('',#100106) ;
#29921 = VERTEX_POINT('',#100108) ;
#29922 = VERTEX_POINT('',#100112) ;
#29923 = VERTEX_POINT('',#100113) ;
#29924 = VERTEX_POINT('',#100115) ;
#29925 = VERTEX_POINT('',#100117) ;
#29926 = VERTEX_POINT('',#100121) ;
#29927 = VERTEX_POINT('',#100122) ;
#29928 = VERTEX_POINT('',#100124) ;
#29929 = VERTEX_POINT('',#100126) ;
#29930 = VERTEX_POINT('',#100130) ;
#29931 = VERTEX_POINT('',#100131) ;
#29932 = VERTEX_POINT('',#100133) ;
#29933 = VERTEX_POINT('',#100135) ;
#29934 = VERTEX_POINT('',#100139) ;
#29935 = VERTEX_POINT('',#100140) ;
#29936 = VERTEX_POINT('',#100142) ;
#29937 = VERTEX_POINT('',#100144) ;
#29938 = VERTEX_POINT('',#100148) ;
#29939 = VERTEX_POINT('',#100149) ;
#29940 = VERTEX_POINT('',#100151) ;
#29941 = VERTEX_POINT('',#100153) ;
#29942 = VERTEX_POINT('',#100157) ;
#29943 = VERTEX_POINT('',#100158) ;
#29944 = VERTEX_POINT('',#100160) ;
#29945 = VERTEX_POINT('',#100162) ;
#29946 = VERTEX_POINT('',#100166) ;
#29947 = VERTEX_POINT('',#100167) ;
#29948 = VERTEX_POINT('',#100169) ;
#29949 = VERTEX_POINT('',#100171) ;
#29950 = VERTEX_POINT('',#100175) ;
#29951 = VERTEX_POINT('',#100176) ;
#29952 = VERTEX_POINT('',#100178) ;
#29953 = VERTEX_POINT('',#100180) ;
#29954 = VERTEX_POINT('',#100184) ;
#29955 = VERTEX_POINT('',#100185) ;
#29956 = VERTEX_POINT('',#100187) ;
#29957 = VERTEX_POINT('',#100189) ;
#29958 = VERTEX_POINT('',#100193) ;
#29959 = VERTEX_POINT('',#100194) ;
#29960 = VERTEX_POINT('',#100196) ;
#29961 = VERTEX_POINT('',#100198) ;
#29962 = VERTEX_POINT('',#100202) ;
#29963 = VERTEX_POINT('',#100203) ;
#29964 = VERTEX_POINT('',#100205) ;
#29965 = VERTEX_POINT('',#100207) ;
#29966 = VERTEX_POINT('',#100211) ;
#29967 = VERTEX_POINT('',#100212) ;
#29968 = VERTEX_POINT('',#100214) ;
#29969 = VERTEX_POINT('',#100216) ;
#29970 = VERTEX_POINT('',#100220) ;
#29971 = VERTEX_POINT('',#100221) ;
#29972 = VERTEX_POINT('',#100223) ;
#29973 = VERTEX_POINT('',#100225) ;
#29974 = VERTEX_POINT('',#100229) ;
#29975 = VERTEX_POINT('',#100230) ;
#29976 = VERTEX_POINT('',#100232) ;
#29977 = VERTEX_POINT('',#100234) ;
#29978 = VERTEX_POINT('',#100238) ;
#29979 = VERTEX_POINT('',#100239) ;
#29980 = VERTEX_POINT('',#100241) ;
#29981 = VERTEX_POINT('',#100243) ;
#29982 = VERTEX_POINT('',#100247) ;
#29983 = VERTEX_POINT('',#100248) ;
#29984 = VERTEX_POINT('',#100250) ;
#29985 = VERTEX_POINT('',#100252) ;
#29986 = VERTEX_POINT('',#100256) ;
#29987 = VERTEX_POINT('',#100257) ;
#29988 = VERTEX_POINT('',#100259) ;
#29989 = VERTEX_POINT('',#100261) ;
#29990 = VERTEX_POINT('',#100265) ;
#29991 = VERTEX_POINT('',#100266) ;
#29992 = VERTEX_POINT('',#100268) ;
#29993 = VERTEX_POINT('',#100270) ;
#29994 = VERTEX_POINT('',#100274) ;
#29995 = VERTEX_POINT('',#100275) ;
#29996 = VERTEX_POINT('',#100277) ;
#29997 = VERTEX_POINT('',#100279) ;
#29998 = VERTEX_POINT('',#100283) ;
#29999 = VERTEX_POINT('',#100284) ;
#30000 = VERTEX_POINT('',#100286) ;
#30001 = VERTEX_POINT('',#100288) ;
#30002 = VERTEX_POINT('',#100292) ;
#30003 = VERTEX_POINT('',#100293) ;
#30004 = VERTEX_POINT('',#100295) ;
#30005 = VERTEX_POINT('',#100297) ;
#30006 = VERTEX_POINT('',#100301) ;
#30007 = VERTEX_POINT('',#100302) ;
#30008 = VERTEX_POINT('',#100304) ;
#30009 = VERTEX_POINT('',#100306) ;
#30010 = VERTEX_POINT('',#100310) ;
#30011 = VERTEX_POINT('',#100311) ;
#30012 = VERTEX_POINT('',#100313) ;
#30013 = VERTEX_POINT('',#100315) ;
#30014 = VERTEX_POINT('',#100319) ;
#30015 = VERTEX_POINT('',#100320) ;
#30016 = VERTEX_POINT('',#100322) ;
#30017 = VERTEX_POINT('',#100324) ;
#30018 = VERTEX_POINT('',#100328) ;
#30019 = VERTEX_POINT('',#100329) ;
#30020 = VERTEX_POINT('',#100331) ;
#30021 = VERTEX_POINT('',#100333) ;
#30022 = VERTEX_POINT('',#100337) ;
#30023 = VERTEX_POINT('',#100338) ;
#30024 = VERTEX_POINT('',#100340) ;
#30025 = VERTEX_POINT('',#100342) ;
#30026 = VERTEX_POINT('',#100346) ;
#30027 = VERTEX_POINT('',#100347) ;
#30028 = VERTEX_POINT('',#100349) ;
#30029 = VERTEX_POINT('',#100351) ;
#30030 = VERTEX_POINT('',#100355) ;
#30031 = VERTEX_POINT('',#100356) ;
#30032 = VERTEX_POINT('',#100358) ;
#30033 = VERTEX_POINT('',#100360) ;
#30034 = VERTEX_POINT('',#100364) ;
#30035 = VERTEX_POINT('',#100365) ;
#30036 = VERTEX_POINT('',#100367) ;
#30037 = VERTEX_POINT('',#100369) ;
#30038 = VERTEX_POINT('',#100373) ;
#30039 = VERTEX_POINT('',#100374) ;
#30040 = VERTEX_POINT('',#100376) ;
#30041 = VERTEX_POINT('',#100378) ;
#30042 = VERTEX_POINT('',#100382) ;
#30043 = VERTEX_POINT('',#100383) ;
#30044 = VERTEX_POINT('',#100385) ;
#30045 = VERTEX_POINT('',#100387) ;
#30046 = VERTEX_POINT('',#100391) ;
#30047 = VERTEX_POINT('',#100392) ;
#30048 = VERTEX_POINT('',#100394) ;
#30049 = VERTEX_POINT('',#100396) ;
#30050 = VERTEX_POINT('',#100400) ;
#30051 = VERTEX_POINT('',#100401) ;
#30052 = VERTEX_POINT('',#100403) ;
#30053 = VERTEX_POINT('',#100405) ;
#30054 = VERTEX_POINT('',#100409) ;
#30055 = VERTEX_POINT('',#100410) ;
#30056 = VERTEX_POINT('',#100412) ;
#30057 = VERTEX_POINT('',#100414) ;
#30058 = VERTEX_POINT('',#100418) ;
#30059 = VERTEX_POINT('',#100419) ;
#30060 = VERTEX_POINT('',#100421) ;
#30061 = VERTEX_POINT('',#100423) ;
#30062 = VERTEX_POINT('',#101197) ;
#30063 = VERTEX_POINT('',#101198) ;
#30064 = VERTEX_POINT('',#101209) ;
#30065 = VERTEX_POINT('',#101211) ;
#30066 = VERTEX_POINT('',#101213) ;
#30067 = VERTEX_POINT('',#101234) ;
#30068 = VERTEX_POINT('',#101235) ;
#30069 = VERTEX_POINT('',#101252) ;
#30070 = VERTEX_POINT('',#101254) ;
#30071 = VERTEX_POINT('',#101256) ;
#30072 = VERTEX_POINT('',#101260) ;
#30073 = VERTEX_POINT('',#101262) ;
#30074 = VERTEX_POINT('',#101266) ;
#30075 = VERTEX_POINT('',#101268) ;
#30076 = VERTEX_POINT('',#101272) ;
#30077 = VERTEX_POINT('',#101273) ;
#30078 = VERTEX_POINT('',#101275) ;
#30079 = VERTEX_POINT('',#101277) ;
#30080 = VERTEX_POINT('',#101279) ;
#30081 = VERTEX_POINT('',#101283) ;
#30082 = VERTEX_POINT('',#101284) ;
#30083 = VERTEX_POINT('',#101286) ;
#30084 = VERTEX_POINT('',#101288) ;
#30085 = VERTEX_POINT('',#101292) ;
#30086 = VERTEX_POINT('',#101293) ;
#30087 = VERTEX_POINT('',#101295) ;
#30088 = VERTEX_POINT('',#101297) ;
#30089 = VERTEX_POINT('',#101303) ;
#30090 = VERTEX_POINT('',#101306) ;
#30091 = VERTEX_POINT('',#101313) ;
#30092 = VERTEX_POINT('',#101321) ;
#30093 = VERTEX_POINT('',#101325) ;
#30094 = VERTEX_POINT('',#101326) ;
#30095 = VERTEX_POINT('',#101328) ;
#30096 = VERTEX_POINT('',#101330) ;
#30097 = VERTEX_POINT('',#101337) ;
#30098 = VERTEX_POINT('',#101339) ;
#30099 = VERTEX_POINT('',#101343) ;
#30100 = VERTEX_POINT('',#101344) ;
#30101 = VERTEX_POINT('',#101346) ;
#30102 = VERTEX_POINT('',#101348) ;
#30103 = VERTEX_POINT('',#101377) ;
#30104 = VERTEX_POINT('',#101388) ;
#30105 = VERTEX_POINT('',#101392) ;
#30106 = VERTEX_POINT('',#101393) ;
#30107 = VERTEX_POINT('',#101395) ;
#30108 = VERTEX_POINT('',#101397) ;
#30109 = VERTEX_POINT('',#101401) ;
#30110 = VERTEX_POINT('',#101402) ;
#30111 = VERTEX_POINT('',#101404) ;
#30112 = VERTEX_POINT('',#101412) ;
#30113 = VERTEX_POINT('',#101425) ;
#30114 = VERTEX_POINT('',#101427) ;
#30115 = VERTEX_POINT('',#101431) ;
#30116 = VERTEX_POINT('',#101432) ;
#30117 = VERTEX_POINT('',#101434) ;
#30118 = VERTEX_POINT('',#101436) ;
#30119 = VERTEX_POINT('',#101440) ;
#30120 = VERTEX_POINT('',#101441) ;
#30121 = VERTEX_POINT('',#101443) ;
#30122 = VERTEX_POINT('',#101445) ;
#30123 = VERTEX_POINT('',#101449) ;
#30124 = VERTEX_POINT('',#101450) ;
#30125 = VERTEX_POINT('',#101452) ;
#30126 = VERTEX_POINT('',#101454) ;
#30127 = VERTEX_POINT('',#101456) ;
#30128 = VERTEX_POINT('',#101458) ;
#30129 = VERTEX_POINT('',#101462) ;
#30130 = VERTEX_POINT('',#101463) ;
#30131 = VERTEX_POINT('',#101468) ;
#30132 = VERTEX_POINT('',#101470) ;
#30133 = VERTEX_POINT('',#101472) ;
#30134 = VERTEX_POINT('',#101474) ;
#30135 = VERTEX_POINT('',#101476) ;
#30136 = VERTEX_POINT('',#101478) ;
#30137 = VERTEX_POINT('',#101480) ;
#30138 = VERTEX_POINT('',#101482) ;
#30139 = VERTEX_POINT('',#101484) ;
#30140 = VERTEX_POINT('',#101486) ;
#30141 = VERTEX_POINT('',#101488) ;
#30142 = VERTEX_POINT('',#101490) ;
#30143 = VERTEX_POINT('',#101493) ;
#30144 = VERTEX_POINT('',#101495) ;
#30145 = VERTEX_POINT('',#101498) ;
#30146 = VERTEX_POINT('',#101500) ;
#30147 = VERTEX_POINT('',#101502) ;
#30148 = VERTEX_POINT('',#101504) ;
#30149 = VERTEX_POINT('',#101506) ;
#30150 = VERTEX_POINT('',#101508) ;
#30151 = VERTEX_POINT('',#101510) ;
#30152 = VERTEX_POINT('',#101514) ;
#30153 = VERTEX_POINT('',#101515) ;
#30154 = VERTEX_POINT('',#101517) ;
#30155 = VERTEX_POINT('',#101519) ;
#30156 = VERTEX_POINT('',#101521) ;
#30157 = VERTEX_POINT('',#101523) ;
#30158 = VERTEX_POINT('',#101525) ;
#30159 = VERTEX_POINT('',#101527) ;
#30160 = VERTEX_POINT('',#101529) ;
#30161 = VERTEX_POINT('',#101531) ;
#30162 = VERTEX_POINT('',#101533) ;
#30163 = VERTEX_POINT('',#101536) ;
#30164 = VERTEX_POINT('',#101538) ;
#30165 = VERTEX_POINT('',#101541) ;
#30166 = VERTEX_POINT('',#101543) ;
#30167 = VERTEX_POINT('',#101545) ;
#30168 = VERTEX_POINT('',#101547) ;
#30169 = VERTEX_POINT('',#101549) ;
#30170 = VERTEX_POINT('',#101551) ;
#30171 = VERTEX_POINT('',#101553) ;
#30172 = VERTEX_POINT('',#101555) ;
#30173 = VERTEX_POINT('',#101557) ;
#30174 = VERTEX_POINT('',#101559) ;
#30175 = VERTEX_POINT('',#101561) ;
#30176 = VERTEX_POINT('',#101563) ;
#30177 = VERTEX_POINT('',#101565) ;
#30178 = VERTEX_POINT('',#101567) ;
#30179 = VERTEX_POINT('',#101569) ;
#30180 = VERTEX_POINT('',#101571) ;
#30181 = VERTEX_POINT('',#101581) ;
#30182 = VERTEX_POINT('',#101582) ;
#30183 = VERTEX_POINT('',#101625) ;
#30184 = VERTEX_POINT('',#101627) ;
#30185 = VERTEX_POINT('',#101670) ;
#30186 = VERTEX_POINT('',#101671) ;
#30187 = VERTEX_POINT('',#101679) ;
#30188 = VERTEX_POINT('',#101682) ;
#30189 = VERTEX_POINT('',#101686) ;
#30190 = VERTEX_POINT('',#101687) ;
#30191 = VERTEX_POINT('',#101692) ;
#30192 = VERTEX_POINT('',#101707) ;
#30193 = VERTEX_POINT('',#101712) ;
#30194 = VERTEX_POINT('',#101714) ;
#30195 = VERTEX_POINT('',#101749) ;
#30196 = VERTEX_POINT('',#101751) ;
#30197 = VERTEX_POINT('',#101805) ;
#30198 = VERTEX_POINT('',#101807) ;
#30199 = VERTEX_POINT('',#101809) ;
#30200 = VERTEX_POINT('',#101811) ;
#30201 = VERTEX_POINT('',#101813) ;
#30202 = VERTEX_POINT('',#101815) ;
#30203 = VERTEX_POINT('',#101819) ;
#30204 = VERTEX_POINT('',#101820) ;
#30205 = VERTEX_POINT('',#101823) ;
#30206 = VERTEX_POINT('',#101825) ;
#30207 = VERTEX_POINT('',#101827) ;
#30208 = VERTEX_POINT('',#101829) ;
#30209 = VERTEX_POINT('',#101831) ;
#30210 = VERTEX_POINT('',#101833) ;
#30211 = VERTEX_POINT('',#101835) ;
#30212 = VERTEX_POINT('',#101837) ;
#30213 = VERTEX_POINT('',#101839) ;
#30214 = VERTEX_POINT('',#101841) ;
#30215 = VERTEX_POINT('',#101844) ;
#30216 = VERTEX_POINT('',#101846) ;
#30217 = VERTEX_POINT('',#101848) ;
#30218 = VERTEX_POINT('',#101850) ;
#30219 = VERTEX_POINT('',#101852) ;
#30220 = VERTEX_POINT('',#101854) ;
#30221 = VERTEX_POINT('',#101856) ;
#30222 = VERTEX_POINT('',#101858) ;
#30223 = VERTEX_POINT('',#101862) ;
#30224 = VERTEX_POINT('',#101863) ;
#30225 = VERTEX_POINT('',#101865) ;
#30226 = VERTEX_POINT('',#101869) ;
#30227 = VERTEX_POINT('',#101871) ;
#30228 = VERTEX_POINT('',#101873) ;
#30229 = VERTEX_POINT('',#101877) ;
#30230 = VERTEX_POINT('',#101878) ;
#30231 = VERTEX_POINT('',#101882) ;
#30232 = VERTEX_POINT('',#101884) ;
#30233 = VERTEX_POINT('',#101888) ;
#30234 = VERTEX_POINT('',#101889) ;
#30235 = VERTEX_POINT('',#101891) ;
#30236 = VERTEX_POINT('',#101895) ;
#30237 = VERTEX_POINT('',#101896) ;
#30238 = VERTEX_POINT('',#101898) ;
#30239 = VERTEX_POINT('',#101902) ;
#30240 = VERTEX_POINT('',#101903) ;
#30241 = VERTEX_POINT('',#101905) ;
#30242 = VERTEX_POINT('',#101907) ;
#30243 = VERTEX_POINT('',#101909) ;
#30244 = VERTEX_POINT('',#101911) ;
#30245 = VERTEX_POINT('',#101913) ;
#30246 = VERTEX_POINT('',#101915) ;
#30247 = VERTEX_POINT('',#101919) ;
#30248 = VERTEX_POINT('',#101920) ;
#30249 = VERTEX_POINT('',#101922) ;
#30250 = VERTEX_POINT('',#101924) ;
#30251 = VERTEX_POINT('',#101928) ;
#30252 = VERTEX_POINT('',#101929) ;
#30253 = VERTEX_POINT('',#101931) ;
#30254 = VERTEX_POINT('',#101933) ;
#30255 = VERTEX_POINT('',#101937) ;
#30256 = VERTEX_POINT('',#101938) ;
#30257 = VERTEX_POINT('',#101940) ;
#30258 = VERTEX_POINT('',#101942) ;
#30259 = VERTEX_POINT('',#101946) ;
#30260 = VERTEX_POINT('',#101947) ;
#30261 = VERTEX_POINT('',#101956) ;
#30262 = VERTEX_POINT('',#101958) ;
#30263 = VERTEX_POINT('',#101960) ;
#30264 = VERTEX_POINT('',#101962) ;
#30265 = VERTEX_POINT('',#101973) ;
#30266 = VERTEX_POINT('',#101974) ;
#30267 = VERTEX_POINT('',#101976) ;
#30268 = VERTEX_POINT('',#101978) ;
#30269 = VERTEX_POINT('',#101980) ;
#30270 = VERTEX_POINT('',#101982) ;
#30271 = VERTEX_POINT('',#101984) ;
#30272 = VERTEX_POINT('',#101986) ;
#30273 = VERTEX_POINT('',#101990) ;
#30274 = VERTEX_POINT('',#101991) ;
#30275 = VERTEX_POINT('',#101993) ;
#30276 = VERTEX_POINT('',#101995) ;
#30277 = VERTEX_POINT('',#101997) ;
#30278 = VERTEX_POINT('',#101999) ;
#30279 = VERTEX_POINT('',#102001) ;
#30280 = VERTEX_POINT('',#102003) ;
#30281 = VERTEX_POINT('',#102007) ;
#30282 = VERTEX_POINT('',#102008) ;
#30283 = VERTEX_POINT('',#102011) ;
#30284 = VERTEX_POINT('',#102013) ;
#30285 = VERTEX_POINT('',#102015) ;
#30286 = VERTEX_POINT('',#102019) ;
#30287 = VERTEX_POINT('',#102021) ;
#30288 = VERTEX_POINT('',#102025) ;
#30289 = VERTEX_POINT('',#102026) ;
#30290 = VERTEX_POINT('',#102031) ;
#30291 = VERTEX_POINT('',#102032) ;
#30292 = VERTEX_POINT('',#102034) ;
#30293 = VERTEX_POINT('',#102036) ;
#30294 = VERTEX_POINT('',#102040) ;
#30295 = VERTEX_POINT('',#102041) ;
#30296 = VERTEX_POINT('',#102043) ;
#30297 = VERTEX_POINT('',#102045) ;
#30298 = VERTEX_POINT('',#102049) ;
#30299 = VERTEX_POINT('',#102051) ;
#30300 = VERTEX_POINT('',#102055) ;
#30301 = VERTEX_POINT('',#102056) ;
#30302 = VERTEX_POINT('',#102061) ;
#30303 = VERTEX_POINT('',#102062) ;
#30304 = VERTEX_POINT('',#102065) ;
#30305 = VERTEX_POINT('',#102067) ;
#30306 = VERTEX_POINT('',#102069) ;
#30307 = VERTEX_POINT('',#102073) ;
#30308 = VERTEX_POINT('',#102074) ;
#30309 = VERTEX_POINT('',#102077) ;
#30310 = VERTEX_POINT('',#102081) ;
#30311 = VERTEX_POINT('',#102082) ;
#30312 = VERTEX_POINT('',#102087) ;
#30313 = VERTEX_POINT('',#102088) ;
#30314 = VERTEX_POINT('',#102090) ;
#30315 = VERTEX_POINT('',#102092) ;
#30316 = VERTEX_POINT('',#102096) ;
#30317 = VERTEX_POINT('',#102097) ;
#30318 = VERTEX_POINT('',#102099) ;
#30319 = VERTEX_POINT('',#102101) ;
#30320 = VERTEX_POINT('',#102105) ;
#30321 = VERTEX_POINT('',#102106) ;
#30322 = VERTEX_POINT('',#102108) ;
#30323 = VERTEX_POINT('',#102110) ;
#30324 = VERTEX_POINT('',#102114) ;
#30325 = VERTEX_POINT('',#102116) ;
#30326 = VERTEX_POINT('',#102120) ;
#30327 = VERTEX_POINT('',#102121) ;
#30328 = VERTEX_POINT('',#102123) ;
#30329 = VERTEX_POINT('',#102125) ;
#30330 = VERTEX_POINT('',#102129) ;
#30331 = VERTEX_POINT('',#102130) ;
#30332 = VERTEX_POINT('',#102133) ;
#30333 = VERTEX_POINT('',#102137) ;
#30334 = VERTEX_POINT('',#102138) ;
#30335 = VERTEX_POINT('',#102140) ;
#30336 = VERTEX_POINT('',#102142) ;
#30337 = VERTEX_POINT('',#102146) ;
#30338 = VERTEX_POINT('',#102147) ;
#30339 = VERTEX_POINT('',#102150) ;
#30340 = VERTEX_POINT('',#102152) ;
#30341 = VERTEX_POINT('',#102154) ;
#30342 = VERTEX_POINT('',#102156) ;
#30343 = VERTEX_POINT('',#102160) ;
#30344 = VERTEX_POINT('',#102161) ;
#30345 = VERTEX_POINT('',#102164) ;
#30346 = VERTEX_POINT('',#102168) ;
#30347 = VERTEX_POINT('',#102169) ;
#30348 = VERTEX_POINT('',#102171) ;
#30349 = VERTEX_POINT('',#102173) ;
#30350 = VERTEX_POINT('',#102177) ;
#30351 = VERTEX_POINT('',#102178) ;
#30352 = VERTEX_POINT('',#102180) ;
#30353 = VERTEX_POINT('',#102182) ;
#30354 = VERTEX_POINT('',#102186) ;
#30355 = VERTEX_POINT('',#102187) ;
#30356 = VERTEX_POINT('',#102189) ;
#30357 = VERTEX_POINT('',#102191) ;
#30358 = VERTEX_POINT('',#102195) ;
#30359 = VERTEX_POINT('',#102197) ;
#30360 = VERTEX_POINT('',#102201) ;
#30361 = VERTEX_POINT('',#102203) ;
#30362 = VERTEX_POINT('',#102207) ;
#30363 = VERTEX_POINT('',#102209) ;
#30364 = VERTEX_POINT('',#102213) ;
#30365 = VERTEX_POINT('',#102215) ;
#30366 = VERTEX_POINT('',#102219) ;
#30367 = VERTEX_POINT('',#102220) ;
#30368 = VERTEX_POINT('',#102222) ;
#30369 = VERTEX_POINT('',#102224) ;
#30370 = VERTEX_POINT('',#102226) ;
#30371 = VERTEX_POINT('',#102228) ;
#30372 = VERTEX_POINT('',#102232) ;
#30373 = VERTEX_POINT('',#102233) ;
#30374 = VERTEX_POINT('',#102235) ;
#30375 = VERTEX_POINT('',#102237) ;
#30376 = VERTEX_POINT('',#102239) ;
#30377 = VERTEX_POINT('',#102241) ;
#30378 = VERTEX_POINT('',#102245) ;
#30379 = VERTEX_POINT('',#102246) ;
#30380 = VERTEX_POINT('',#102251) ;
#30381 = VERTEX_POINT('',#102253) ;
#30382 = VERTEX_POINT('',#102257) ;
#30383 = VERTEX_POINT('',#102258) ;
#30384 = VERTEX_POINT('',#102260) ;
#30385 = VERTEX_POINT('',#102262) ;
#30386 = VERTEX_POINT('',#102266) ;
#30387 = VERTEX_POINT('',#102267) ;
#30388 = VERTEX_POINT('',#102269) ;
#30389 = VERTEX_POINT('',#102271) ;
#30390 = VERTEX_POINT('',#102275) ;
#30391 = VERTEX_POINT('',#102276) ;
#30392 = VERTEX_POINT('',#102278) ;
#30393 = VERTEX_POINT('',#102280) ;
#30394 = VERTEX_POINT('',#102284) ;
#30395 = VERTEX_POINT('',#102285) ;
#30396 = VERTEX_POINT('',#102287) ;
#30397 = VERTEX_POINT('',#102289) ;
#30398 = VERTEX_POINT('',#102296) ;
#30399 = VERTEX_POINT('',#102297) ;
#30400 = VERTEX_POINT('',#102299) ;
#30401 = VERTEX_POINT('',#102301) ;
#30402 = VERTEX_POINT('',#102305) ;
#30403 = VERTEX_POINT('',#102306) ;
#30404 = VERTEX_POINT('',#102308) ;
#30405 = VERTEX_POINT('',#102310) ;
#30406 = VERTEX_POINT('',#102314) ;
#30407 = VERTEX_POINT('',#102315) ;
#30408 = VERTEX_POINT('',#102317) ;
#30409 = VERTEX_POINT('',#102319) ;
#30410 = VERTEX_POINT('',#102323) ;
#30411 = VERTEX_POINT('',#102324) ;
#30412 = VERTEX_POINT('',#102326) ;
#30413 = VERTEX_POINT('',#102328) ;
#30414 = VERTEX_POINT('',#102332) ;
#30415 = VERTEX_POINT('',#102334) ;
#30416 = VERTEX_POINT('',#102338) ;
#30417 = VERTEX_POINT('',#102339) ;
#30418 = VERTEX_POINT('',#102344) ;
#30419 = VERTEX_POINT('',#102346) ;
#30420 = VERTEX_POINT('',#102423) ;
#30421 = VERTEX_POINT('',#102440) ;
#30422 = VERTEX_POINT('',#102459) ;
#30423 = VERTEX_POINT('',#102475) ;
#30424 = VERTEX_POINT('',#102492) ;
#30425 = VERTEX_POINT('',#102508) ;
#30426 = VERTEX_POINT('',#102528) ;
#30427 = VERTEX_POINT('',#102532) ;
#30428 = VERTEX_POINT('',#102536) ;
#30429 = VERTEX_POINT('',#102554) ;
#30430 = VERTEX_POINT('',#102572) ;
#30431 = VERTEX_POINT('',#102581) ;
#30432 = VERTEX_POINT('',#102587) ;
#30433 = VERTEX_POINT('',#102595) ;
#30434 = VERTEX_POINT('',#102601) ;
#30435 = VERTEX_POINT('',#102614) ;
#30436 = VERTEX_POINT('',#102720) ;
#30437 = VERTEX_POINT('',#103147) ;
#30438 = VERTEX_POINT('',#103227) ;
#30439 = VERTEX_POINT('',#103238) ;
#30440 = VERTEX_POINT('',#103464) ;
#30441 = VERTEX_POINT('',#103481) ;
#30442 = VERTEX_POINT('',#103709) ;
#30443 = VERTEX_POINT('',#103710) ;
#30444 = VERTEX_POINT('',#103721) ;
#30445 = VERTEX_POINT('',#103723) ;
#30446 = VERTEX_POINT('',#103725) ;
#30447 = VERTEX_POINT('',#103746) ;
#30448 = VERTEX_POINT('',#103747) ;
#30449 = VERTEX_POINT('',#103764) ;
#30450 = VERTEX_POINT('',#103766) ;
#30451 = VERTEX_POINT('',#103768) ;
#30452 = VERTEX_POINT('',#103772) ;
#30453 = VERTEX_POINT('',#103774) ;
#30454 = VERTEX_POINT('',#103778) ;
#30455 = VERTEX_POINT('',#103780) ;
#30456 = VERTEX_POINT('',#103784) ;
#30457 = VERTEX_POINT('',#103785) ;
#30458 = VERTEX_POINT('',#103787) ;
#30459 = VERTEX_POINT('',#103789) ;
#30460 = VERTEX_POINT('',#103791) ;
#30461 = VERTEX_POINT('',#103795) ;
#30462 = VERTEX_POINT('',#103796) ;
#30463 = VERTEX_POINT('',#103798) ;
#30464 = VERTEX_POINT('',#103800) ;
#30465 = VERTEX_POINT('',#103804) ;
#30466 = VERTEX_POINT('',#103805) ;
#30467 = VERTEX_POINT('',#103807) ;
#30468 = VERTEX_POINT('',#103809) ;
#30469 = VERTEX_POINT('',#103815) ;
#30470 = VERTEX_POINT('',#103818) ;
#30471 = VERTEX_POINT('',#103825) ;
#30472 = VERTEX_POINT('',#103833) ;
#30473 = VERTEX_POINT('',#103837) ;
#30474 = VERTEX_POINT('',#103838) ;
#30475 = VERTEX_POINT('',#103840) ;
#30476 = VERTEX_POINT('',#103842) ;
#30477 = VERTEX_POINT('',#103849) ;
#30478 = VERTEX_POINT('',#103851) ;
#30479 = VERTEX_POINT('',#103855) ;
#30480 = VERTEX_POINT('',#103856) ;
#30481 = VERTEX_POINT('',#103858) ;
#30482 = VERTEX_POINT('',#103860) ;
#30483 = VERTEX_POINT('',#103889) ;
#30484 = VERTEX_POINT('',#103900) ;
#30485 = VERTEX_POINT('',#103904) ;
#30486 = VERTEX_POINT('',#103905) ;
#30487 = VERTEX_POINT('',#103907) ;
#30488 = VERTEX_POINT('',#103909) ;
#30489 = VERTEX_POINT('',#103913) ;
#30490 = VERTEX_POINT('',#103914) ;
#30491 = VERTEX_POINT('',#103916) ;
#30492 = VERTEX_POINT('',#103924) ;
#30493 = VERTEX_POINT('',#103937) ;
#30494 = VERTEX_POINT('',#103939) ;
#30495 = VERTEX_POINT('',#103943) ;
#30496 = VERTEX_POINT('',#103944) ;
#30497 = VERTEX_POINT('',#103946) ;
#30498 = VERTEX_POINT('',#103948) ;
#30499 = VERTEX_POINT('',#103952) ;
#30500 = VERTEX_POINT('',#103953) ;
#30501 = VERTEX_POINT('',#103955) ;
#30502 = VERTEX_POINT('',#103957) ;
#30503 = VERTEX_POINT('',#103961) ;
#30504 = VERTEX_POINT('',#103962) ;
#30505 = VERTEX_POINT('',#103964) ;
#30506 = VERTEX_POINT('',#103966) ;
#30507 = VERTEX_POINT('',#103968) ;
#30508 = VERTEX_POINT('',#103970) ;
#30509 = VERTEX_POINT('',#103974) ;
#30510 = VERTEX_POINT('',#103975) ;
#30511 = VERTEX_POINT('',#103980) ;
#30512 = VERTEX_POINT('',#103982) ;
#30513 = VERTEX_POINT('',#103984) ;
#30514 = VERTEX_POINT('',#103986) ;
#30515 = VERTEX_POINT('',#103988) ;
#30516 = VERTEX_POINT('',#103990) ;
#30517 = VERTEX_POINT('',#103992) ;
#30518 = VERTEX_POINT('',#103994) ;
#30519 = VERTEX_POINT('',#103996) ;
#30520 = VERTEX_POINT('',#103998) ;
#30521 = VERTEX_POINT('',#104000) ;
#30522 = VERTEX_POINT('',#104002) ;
#30523 = VERTEX_POINT('',#104005) ;
#30524 = VERTEX_POINT('',#104007) ;
#30525 = VERTEX_POINT('',#104010) ;
#30526 = VERTEX_POINT('',#104012) ;
#30527 = VERTEX_POINT('',#104014) ;
#30528 = VERTEX_POINT('',#104016) ;
#30529 = VERTEX_POINT('',#104018) ;
#30530 = VERTEX_POINT('',#104020) ;
#30531 = VERTEX_POINT('',#104022) ;
#30532 = VERTEX_POINT('',#104026) ;
#30533 = VERTEX_POINT('',#104027) ;
#30534 = VERTEX_POINT('',#104029) ;
#30535 = VERTEX_POINT('',#104031) ;
#30536 = VERTEX_POINT('',#104033) ;
#30537 = VERTEX_POINT('',#104035) ;
#30538 = VERTEX_POINT('',#104037) ;
#30539 = VERTEX_POINT('',#104039) ;
#30540 = VERTEX_POINT('',#104041) ;
#30541 = VERTEX_POINT('',#104043) ;
#30542 = VERTEX_POINT('',#104045) ;
#30543 = VERTEX_POINT('',#104048) ;
#30544 = VERTEX_POINT('',#104050) ;
#30545 = VERTEX_POINT('',#104053) ;
#30546 = VERTEX_POINT('',#104055) ;
#30547 = VERTEX_POINT('',#104057) ;
#30548 = VERTEX_POINT('',#104059) ;
#30549 = VERTEX_POINT('',#104061) ;
#30550 = VERTEX_POINT('',#104063) ;
#30551 = VERTEX_POINT('',#104065) ;
#30552 = VERTEX_POINT('',#104067) ;
#30553 = VERTEX_POINT('',#104069) ;
#30554 = VERTEX_POINT('',#104071) ;
#30555 = VERTEX_POINT('',#104073) ;
#30556 = VERTEX_POINT('',#104075) ;
#30557 = VERTEX_POINT('',#104077) ;
#30558 = VERTEX_POINT('',#104079) ;
#30559 = VERTEX_POINT('',#104081) ;
#30560 = VERTEX_POINT('',#104083) ;
#30561 = VERTEX_POINT('',#104093) ;
#30562 = VERTEX_POINT('',#104094) ;
#30563 = VERTEX_POINT('',#104137) ;
#30564 = VERTEX_POINT('',#104139) ;
#30565 = VERTEX_POINT('',#104182) ;
#30566 = VERTEX_POINT('',#104183) ;
#30567 = VERTEX_POINT('',#104191) ;
#30568 = VERTEX_POINT('',#104194) ;
#30569 = VERTEX_POINT('',#104198) ;
#30570 = VERTEX_POINT('',#104199) ;
#30571 = VERTEX_POINT('',#104204) ;
#30572 = VERTEX_POINT('',#104219) ;
#30573 = VERTEX_POINT('',#104224) ;
#30574 = VERTEX_POINT('',#104226) ;
#30575 = VERTEX_POINT('',#104261) ;
#30576 = VERTEX_POINT('',#104263) ;
#30577 = VERTEX_POINT('',#104317) ;
#30578 = VERTEX_POINT('',#104319) ;
#30579 = VERTEX_POINT('',#104321) ;
#30580 = VERTEX_POINT('',#104323) ;
#30581 = VERTEX_POINT('',#104325) ;
#30582 = VERTEX_POINT('',#104327) ;
#30583 = VERTEX_POINT('',#104331) ;
#30584 = VERTEX_POINT('',#104332) ;
#30585 = VERTEX_POINT('',#104335) ;
#30586 = VERTEX_POINT('',#104337) ;
#30587 = VERTEX_POINT('',#104339) ;
#30588 = VERTEX_POINT('',#104341) ;
#30589 = VERTEX_POINT('',#104343) ;
#30590 = VERTEX_POINT('',#104345) ;
#30591 = VERTEX_POINT('',#104347) ;
#30592 = VERTEX_POINT('',#104349) ;
#30593 = VERTEX_POINT('',#104351) ;
#30594 = VERTEX_POINT('',#104353) ;
#30595 = VERTEX_POINT('',#104356) ;
#30596 = VERTEX_POINT('',#104358) ;
#30597 = VERTEX_POINT('',#104360) ;
#30598 = VERTEX_POINT('',#104362) ;
#30599 = VERTEX_POINT('',#104364) ;
#30600 = VERTEX_POINT('',#104366) ;
#30601 = VERTEX_POINT('',#104368) ;
#30602 = VERTEX_POINT('',#104370) ;
#30603 = VERTEX_POINT('',#104374) ;
#30604 = VERTEX_POINT('',#104375) ;
#30605 = VERTEX_POINT('',#104377) ;
#30606 = VERTEX_POINT('',#104381) ;
#30607 = VERTEX_POINT('',#104383) ;
#30608 = VERTEX_POINT('',#104385) ;
#30609 = VERTEX_POINT('',#104389) ;
#30610 = VERTEX_POINT('',#104390) ;
#30611 = VERTEX_POINT('',#104394) ;
#30612 = VERTEX_POINT('',#104396) ;
#30613 = VERTEX_POINT('',#104400) ;
#30614 = VERTEX_POINT('',#104401) ;
#30615 = VERTEX_POINT('',#104403) ;
#30616 = VERTEX_POINT('',#104407) ;
#30617 = VERTEX_POINT('',#104408) ;
#30618 = VERTEX_POINT('',#104410) ;
#30619 = VERTEX_POINT('',#104414) ;
#30620 = VERTEX_POINT('',#104415) ;
#30621 = VERTEX_POINT('',#104417) ;
#30622 = VERTEX_POINT('',#104419) ;
#30623 = VERTEX_POINT('',#104421) ;
#30624 = VERTEX_POINT('',#104423) ;
#30625 = VERTEX_POINT('',#104425) ;
#30626 = VERTEX_POINT('',#104427) ;
#30627 = VERTEX_POINT('',#104431) ;
#30628 = VERTEX_POINT('',#104432) ;
#30629 = VERTEX_POINT('',#104434) ;
#30630 = VERTEX_POINT('',#104436) ;
#30631 = VERTEX_POINT('',#104440) ;
#30632 = VERTEX_POINT('',#104441) ;
#30633 = VERTEX_POINT('',#104443) ;
#30634 = VERTEX_POINT('',#104445) ;
#30635 = VERTEX_POINT('',#104449) ;
#30636 = VERTEX_POINT('',#104450) ;
#30637 = VERTEX_POINT('',#104452) ;
#30638 = VERTEX_POINT('',#104454) ;
#30639 = VERTEX_POINT('',#104458) ;
#30640 = VERTEX_POINT('',#104459) ;
#30641 = VERTEX_POINT('',#104468) ;
#30642 = VERTEX_POINT('',#104470) ;
#30643 = VERTEX_POINT('',#104472) ;
#30644 = VERTEX_POINT('',#104474) ;
#30645 = VERTEX_POINT('',#104485) ;
#30646 = VERTEX_POINT('',#104486) ;
#30647 = VERTEX_POINT('',#104488) ;
#30648 = VERTEX_POINT('',#104490) ;
#30649 = VERTEX_POINT('',#104492) ;
#30650 = VERTEX_POINT('',#104494) ;
#30651 = VERTEX_POINT('',#104496) ;
#30652 = VERTEX_POINT('',#104498) ;
#30653 = VERTEX_POINT('',#104502) ;
#30654 = VERTEX_POINT('',#104503) ;
#30655 = VERTEX_POINT('',#104505) ;
#30656 = VERTEX_POINT('',#104507) ;
#30657 = VERTEX_POINT('',#104509) ;
#30658 = VERTEX_POINT('',#104511) ;
#30659 = VERTEX_POINT('',#104513) ;
#30660 = VERTEX_POINT('',#104515) ;
#30661 = VERTEX_POINT('',#104519) ;
#30662 = VERTEX_POINT('',#104520) ;
#30663 = VERTEX_POINT('',#104523) ;
#30664 = VERTEX_POINT('',#104525) ;
#30665 = VERTEX_POINT('',#104527) ;
#30666 = VERTEX_POINT('',#104531) ;
#30667 = VERTEX_POINT('',#104533) ;
#30668 = VERTEX_POINT('',#104537) ;
#30669 = VERTEX_POINT('',#104538) ;
#30670 = VERTEX_POINT('',#104543) ;
#30671 = VERTEX_POINT('',#104544) ;
#30672 = VERTEX_POINT('',#104546) ;
#30673 = VERTEX_POINT('',#104548) ;
#30674 = VERTEX_POINT('',#104552) ;
#30675 = VERTEX_POINT('',#104553) ;
#30676 = VERTEX_POINT('',#104555) ;
#30677 = VERTEX_POINT('',#104557) ;
#30678 = VERTEX_POINT('',#104561) ;
#30679 = VERTEX_POINT('',#104563) ;
#30680 = VERTEX_POINT('',#104567) ;
#30681 = VERTEX_POINT('',#104568) ;
#30682 = VERTEX_POINT('',#104573) ;
#30683 = VERTEX_POINT('',#104574) ;
#30684 = VERTEX_POINT('',#104577) ;
#30685 = VERTEX_POINT('',#104579) ;
#30686 = VERTEX_POINT('',#104581) ;
#30687 = VERTEX_POINT('',#104585) ;
#30688 = VERTEX_POINT('',#104586) ;
#30689 = VERTEX_POINT('',#104589) ;
#30690 = VERTEX_POINT('',#104593) ;
#30691 = VERTEX_POINT('',#104594) ;
#30692 = VERTEX_POINT('',#104599) ;
#30693 = VERTEX_POINT('',#104600) ;
#30694 = VERTEX_POINT('',#104602) ;
#30695 = VERTEX_POINT('',#104604) ;
#30696 = VERTEX_POINT('',#104608) ;
#30697 = VERTEX_POINT('',#104609) ;
#30698 = VERTEX_POINT('',#104611) ;
#30699 = VERTEX_POINT('',#104613) ;
#30700 = VERTEX_POINT('',#104617) ;
#30701 = VERTEX_POINT('',#104618) ;
#30702 = VERTEX_POINT('',#104620) ;
#30703 = VERTEX_POINT('',#104622) ;
#30704 = VERTEX_POINT('',#104626) ;
#30705 = VERTEX_POINT('',#104628) ;
#30706 = VERTEX_POINT('',#104632) ;
#30707 = VERTEX_POINT('',#104633) ;
#30708 = VERTEX_POINT('',#104635) ;
#30709 = VERTEX_POINT('',#104637) ;
#30710 = VERTEX_POINT('',#104641) ;
#30711 = VERTEX_POINT('',#104642) ;
#30712 = VERTEX_POINT('',#104645) ;
#30713 = VERTEX_POINT('',#104649) ;
#30714 = VERTEX_POINT('',#104650) ;
#30715 = VERTEX_POINT('',#104652) ;
#30716 = VERTEX_POINT('',#104654) ;
#30717 = VERTEX_POINT('',#104658) ;
#30718 = VERTEX_POINT('',#104659) ;
#30719 = VERTEX_POINT('',#104662) ;
#30720 = VERTEX_POINT('',#104664) ;
#30721 = VERTEX_POINT('',#104666) ;
#30722 = VERTEX_POINT('',#104668) ;
#30723 = VERTEX_POINT('',#104672) ;
#30724 = VERTEX_POINT('',#104673) ;
#30725 = VERTEX_POINT('',#104676) ;
#30726 = VERTEX_POINT('',#104680) ;
#30727 = VERTEX_POINT('',#104681) ;
#30728 = VERTEX_POINT('',#104683) ;
#30729 = VERTEX_POINT('',#104685) ;
#30730 = VERTEX_POINT('',#104689) ;
#30731 = VERTEX_POINT('',#104690) ;
#30732 = VERTEX_POINT('',#104692) ;
#30733 = VERTEX_POINT('',#104694) ;
#30734 = VERTEX_POINT('',#104698) ;
#30735 = VERTEX_POINT('',#104699) ;
#30736 = VERTEX_POINT('',#104701) ;
#30737 = VERTEX_POINT('',#104703) ;
#30738 = VERTEX_POINT('',#104707) ;
#30739 = VERTEX_POINT('',#104709) ;
#30740 = VERTEX_POINT('',#104713) ;
#30741 = VERTEX_POINT('',#104715) ;
#30742 = VERTEX_POINT('',#104719) ;
#30743 = VERTEX_POINT('',#104721) ;
#30744 = VERTEX_POINT('',#104725) ;
#30745 = VERTEX_POINT('',#104727) ;
#30746 = VERTEX_POINT('',#104731) ;
#30747 = VERTEX_POINT('',#104732) ;
#30748 = VERTEX_POINT('',#104734) ;
#30749 = VERTEX_POINT('',#104736) ;
#30750 = VERTEX_POINT('',#104738) ;
#30751 = VERTEX_POINT('',#104740) ;
#30752 = VERTEX_POINT('',#104744) ;
#30753 = VERTEX_POINT('',#104745) ;
#30754 = VERTEX_POINT('',#104747) ;
#30755 = VERTEX_POINT('',#104749) ;
#30756 = VERTEX_POINT('',#104751) ;
#30757 = VERTEX_POINT('',#104753) ;
#30758 = VERTEX_POINT('',#104757) ;
#30759 = VERTEX_POINT('',#104758) ;
#30760 = VERTEX_POINT('',#104763) ;
#30761 = VERTEX_POINT('',#104765) ;
#30762 = VERTEX_POINT('',#104769) ;
#30763 = VERTEX_POINT('',#104770) ;
#30764 = VERTEX_POINT('',#104772) ;
#30765 = VERTEX_POINT('',#104774) ;
#30766 = VERTEX_POINT('',#104778) ;
#30767 = VERTEX_POINT('',#104779) ;
#30768 = VERTEX_POINT('',#104781) ;
#30769 = VERTEX_POINT('',#104783) ;
#30770 = VERTEX_POINT('',#104787) ;
#30771 = VERTEX_POINT('',#104788) ;
#30772 = VERTEX_POINT('',#104790) ;
#30773 = VERTEX_POINT('',#104792) ;
#30774 = VERTEX_POINT('',#104796) ;
#30775 = VERTEX_POINT('',#104797) ;
#30776 = VERTEX_POINT('',#104799) ;
#30777 = VERTEX_POINT('',#104801) ;
#30778 = VERTEX_POINT('',#104808) ;
#30779 = VERTEX_POINT('',#104809) ;
#30780 = VERTEX_POINT('',#104811) ;
#30781 = VERTEX_POINT('',#104813) ;
#30782 = VERTEX_POINT('',#104817) ;
#30783 = VERTEX_POINT('',#104818) ;
#30784 = VERTEX_POINT('',#104820) ;
#30785 = VERTEX_POINT('',#104822) ;
#30786 = VERTEX_POINT('',#104826) ;
#30787 = VERTEX_POINT('',#104827) ;
#30788 = VERTEX_POINT('',#104829) ;
#30789 = VERTEX_POINT('',#104831) ;
#30790 = VERTEX_POINT('',#104835) ;
#30791 = VERTEX_POINT('',#104836) ;
#30792 = VERTEX_POINT('',#104838) ;
#30793 = VERTEX_POINT('',#104840) ;
#30794 = VERTEX_POINT('',#104844) ;
#30795 = VERTEX_POINT('',#104846) ;
#30796 = VERTEX_POINT('',#104850) ;
#30797 = VERTEX_POINT('',#104851) ;
#30798 = VERTEX_POINT('',#104856) ;
#30799 = VERTEX_POINT('',#104858) ;
#30800 = VERTEX_POINT('',#104935) ;
#30801 = VERTEX_POINT('',#104952) ;
#30802 = VERTEX_POINT('',#104971) ;
#30803 = VERTEX_POINT('',#104987) ;
#30804 = VERTEX_POINT('',#105004) ;
#30805 = VERTEX_POINT('',#105020) ;
#30806 = VERTEX_POINT('',#105040) ;
#30807 = VERTEX_POINT('',#105044) ;
#30808 = VERTEX_POINT('',#105048) ;
#30809 = VERTEX_POINT('',#105066) ;
#30810 = VERTEX_POINT('',#105084) ;
#30811 = VERTEX_POINT('',#105093) ;
#30812 = VERTEX_POINT('',#105099) ;
#30813 = VERTEX_POINT('',#105107) ;
#30814 = VERTEX_POINT('',#105113) ;
#30815 = VERTEX_POINT('',#105126) ;
#30816 = VERTEX_POINT('',#105232) ;
#30817 = VERTEX_POINT('',#105659) ;
#30818 = VERTEX_POINT('',#105739) ;
#30819 = VERTEX_POINT('',#105750) ;
#30820 = VERTEX_POINT('',#105976) ;
#30821 = VERTEX_POINT('',#105993) ;
#30822 = VERTEX_POINT('',#106221) ;
#30823 = VERTEX_POINT('',#106222) ;
#30824 = VERTEX_POINT('',#106233) ;
#30825 = VERTEX_POINT('',#106235) ;
#30826 = VERTEX_POINT('',#106237) ;
#30827 = VERTEX_POINT('',#106258) ;
#30828 = VERTEX_POINT('',#106259) ;
#30829 = VERTEX_POINT('',#106276) ;
#30830 = VERTEX_POINT('',#106278) ;
#30831 = VERTEX_POINT('',#106280) ;
#30832 = VERTEX_POINT('',#106284) ;
#30833 = VERTEX_POINT('',#106286) ;
#30834 = VERTEX_POINT('',#106290) ;
#30835 = VERTEX_POINT('',#106292) ;
#30836 = VERTEX_POINT('',#106296) ;
#30837 = VERTEX_POINT('',#106297) ;
#30838 = VERTEX_POINT('',#106299) ;
#30839 = VERTEX_POINT('',#106301) ;
#30840 = VERTEX_POINT('',#106303) ;
#30841 = VERTEX_POINT('',#106307) ;
#30842 = VERTEX_POINT('',#106308) ;
#30843 = VERTEX_POINT('',#106310) ;
#30844 = VERTEX_POINT('',#106312) ;
#30845 = VERTEX_POINT('',#106316) ;
#30846 = VERTEX_POINT('',#106317) ;
#30847 = VERTEX_POINT('',#106319) ;
#30848 = VERTEX_POINT('',#106321) ;
#30849 = VERTEX_POINT('',#106327) ;
#30850 = VERTEX_POINT('',#106330) ;
#30851 = VERTEX_POINT('',#106337) ;
#30852 = VERTEX_POINT('',#106345) ;
#30853 = VERTEX_POINT('',#106349) ;
#30854 = VERTEX_POINT('',#106350) ;
#30855 = VERTEX_POINT('',#106352) ;
#30856 = VERTEX_POINT('',#106354) ;
#30857 = VERTEX_POINT('',#106361) ;
#30858 = VERTEX_POINT('',#106363) ;
#30859 = VERTEX_POINT('',#106367) ;
#30860 = VERTEX_POINT('',#106368) ;
#30861 = VERTEX_POINT('',#106370) ;
#30862 = VERTEX_POINT('',#106372) ;
#30863 = VERTEX_POINT('',#106401) ;
#30864 = VERTEX_POINT('',#106412) ;
#30865 = VERTEX_POINT('',#106416) ;
#30866 = VERTEX_POINT('',#106417) ;
#30867 = VERTEX_POINT('',#106419) ;
#30868 = VERTEX_POINT('',#106421) ;
#30869 = VERTEX_POINT('',#106425) ;
#30870 = VERTEX_POINT('',#106426) ;
#30871 = VERTEX_POINT('',#106428) ;
#30872 = VERTEX_POINT('',#106436) ;
#30873 = VERTEX_POINT('',#106449) ;
#30874 = VERTEX_POINT('',#106451) ;
#30875 = VERTEX_POINT('',#106455) ;
#30876 = VERTEX_POINT('',#106456) ;
#30877 = VERTEX_POINT('',#106458) ;
#30878 = VERTEX_POINT('',#106460) ;
#30879 = VERTEX_POINT('',#106464) ;
#30880 = VERTEX_POINT('',#106465) ;
#30881 = VERTEX_POINT('',#106467) ;
#30882 = VERTEX_POINT('',#106469) ;
#30883 = VERTEX_POINT('',#106473) ;
#30884 = VERTEX_POINT('',#106474) ;
#30885 = VERTEX_POINT('',#106476) ;
#30886 = VERTEX_POINT('',#106478) ;
#30887 = VERTEX_POINT('',#106480) ;
#30888 = VERTEX_POINT('',#106482) ;
#30889 = VERTEX_POINT('',#106486) ;
#30890 = VERTEX_POINT('',#106487) ;
#30891 = VERTEX_POINT('',#106492) ;
#30892 = VERTEX_POINT('',#106494) ;
#30893 = VERTEX_POINT('',#106496) ;
#30894 = VERTEX_POINT('',#106498) ;
#30895 = VERTEX_POINT('',#106500) ;
#30896 = VERTEX_POINT('',#106502) ;
#30897 = VERTEX_POINT('',#106504) ;
#30898 = VERTEX_POINT('',#106506) ;
#30899 = VERTEX_POINT('',#106508) ;
#30900 = VERTEX_POINT('',#106510) ;
#30901 = VERTEX_POINT('',#106512) ;
#30902 = VERTEX_POINT('',#106514) ;
#30903 = VERTEX_POINT('',#106517) ;
#30904 = VERTEX_POINT('',#106519) ;
#30905 = VERTEX_POINT('',#106522) ;
#30906 = VERTEX_POINT('',#106524) ;
#30907 = VERTEX_POINT('',#106526) ;
#30908 = VERTEX_POINT('',#106528) ;
#30909 = VERTEX_POINT('',#106530) ;
#30910 = VERTEX_POINT('',#106532) ;
#30911 = VERTEX_POINT('',#106534) ;
#30912 = VERTEX_POINT('',#106538) ;
#30913 = VERTEX_POINT('',#106539) ;
#30914 = VERTEX_POINT('',#106541) ;
#30915 = VERTEX_POINT('',#106543) ;
#30916 = VERTEX_POINT('',#106545) ;
#30917 = VERTEX_POINT('',#106547) ;
#30918 = VERTEX_POINT('',#106549) ;
#30919 = VERTEX_POINT('',#106551) ;
#30920 = VERTEX_POINT('',#106553) ;
#30921 = VERTEX_POINT('',#106555) ;
#30922 = VERTEX_POINT('',#106557) ;
#30923 = VERTEX_POINT('',#106560) ;
#30924 = VERTEX_POINT('',#106562) ;
#30925 = VERTEX_POINT('',#106565) ;
#30926 = VERTEX_POINT('',#106567) ;
#30927 = VERTEX_POINT('',#106569) ;
#30928 = VERTEX_POINT('',#106571) ;
#30929 = VERTEX_POINT('',#106573) ;
#30930 = VERTEX_POINT('',#106575) ;
#30931 = VERTEX_POINT('',#106577) ;
#30932 = VERTEX_POINT('',#106579) ;
#30933 = VERTEX_POINT('',#106581) ;
#30934 = VERTEX_POINT('',#106583) ;
#30935 = VERTEX_POINT('',#106585) ;
#30936 = VERTEX_POINT('',#106587) ;
#30937 = VERTEX_POINT('',#106589) ;
#30938 = VERTEX_POINT('',#106591) ;
#30939 = VERTEX_POINT('',#106593) ;
#30940 = VERTEX_POINT('',#106595) ;
#30941 = VERTEX_POINT('',#106605) ;
#30942 = VERTEX_POINT('',#106606) ;
#30943 = VERTEX_POINT('',#106649) ;
#30944 = VERTEX_POINT('',#106651) ;
#30945 = VERTEX_POINT('',#106694) ;
#30946 = VERTEX_POINT('',#106695) ;
#30947 = VERTEX_POINT('',#106703) ;
#30948 = VERTEX_POINT('',#106706) ;
#30949 = VERTEX_POINT('',#106710) ;
#30950 = VERTEX_POINT('',#106711) ;
#30951 = VERTEX_POINT('',#106716) ;
#30952 = VERTEX_POINT('',#106731) ;
#30953 = VERTEX_POINT('',#106736) ;
#30954 = VERTEX_POINT('',#106738) ;
#30955 = VERTEX_POINT('',#106773) ;
#30956 = VERTEX_POINT('',#106775) ;
#30957 = VERTEX_POINT('',#106829) ;
#30958 = VERTEX_POINT('',#106831) ;
#30959 = VERTEX_POINT('',#106833) ;
#30960 = VERTEX_POINT('',#106835) ;
#30961 = VERTEX_POINT('',#106837) ;
#30962 = VERTEX_POINT('',#106839) ;
#30963 = VERTEX_POINT('',#106843) ;
#30964 = VERTEX_POINT('',#106844) ;
#30965 = VERTEX_POINT('',#106847) ;
#30966 = VERTEX_POINT('',#106849) ;
#30967 = VERTEX_POINT('',#106851) ;
#30968 = VERTEX_POINT('',#106853) ;
#30969 = VERTEX_POINT('',#106855) ;
#30970 = VERTEX_POINT('',#106857) ;
#30971 = VERTEX_POINT('',#106859) ;
#30972 = VERTEX_POINT('',#106861) ;
#30973 = VERTEX_POINT('',#106863) ;
#30974 = VERTEX_POINT('',#106865) ;
#30975 = VERTEX_POINT('',#106868) ;
#30976 = VERTEX_POINT('',#106870) ;
#30977 = VERTEX_POINT('',#106872) ;
#30978 = VERTEX_POINT('',#106874) ;
#30979 = VERTEX_POINT('',#106876) ;
#30980 = VERTEX_POINT('',#106878) ;
#30981 = VERTEX_POINT('',#106880) ;
#30982 = VERTEX_POINT('',#106882) ;
#30983 = VERTEX_POINT('',#106886) ;
#30984 = VERTEX_POINT('',#106887) ;
#30985 = VERTEX_POINT('',#106889) ;
#30986 = VERTEX_POINT('',#106893) ;
#30987 = VERTEX_POINT('',#106895) ;
#30988 = VERTEX_POINT('',#106897) ;
#30989 = VERTEX_POINT('',#106901) ;
#30990 = VERTEX_POINT('',#106902) ;
#30991 = VERTEX_POINT('',#106906) ;
#30992 = VERTEX_POINT('',#106908) ;
#30993 = VERTEX_POINT('',#106912) ;
#30994 = VERTEX_POINT('',#106913) ;
#30995 = VERTEX_POINT('',#106915) ;
#30996 = VERTEX_POINT('',#106919) ;
#30997 = VERTEX_POINT('',#106920) ;
#30998 = VERTEX_POINT('',#106922) ;
#30999 = VERTEX_POINT('',#106926) ;
#31000 = VERTEX_POINT('',#106927) ;
#31001 = VERTEX_POINT('',#106929) ;
#31002 = VERTEX_POINT('',#106931) ;
#31003 = VERTEX_POINT('',#106933) ;
#31004 = VERTEX_POINT('',#106935) ;
#31005 = VERTEX_POINT('',#106937) ;
#31006 = VERTEX_POINT('',#106939) ;
#31007 = VERTEX_POINT('',#106943) ;
#31008 = VERTEX_POINT('',#106944) ;
#31009 = VERTEX_POINT('',#106946) ;
#31010 = VERTEX_POINT('',#106948) ;
#31011 = VERTEX_POINT('',#106952) ;
#31012 = VERTEX_POINT('',#106953) ;
#31013 = VERTEX_POINT('',#106955) ;
#31014 = VERTEX_POINT('',#106957) ;
#31015 = VERTEX_POINT('',#106961) ;
#31016 = VERTEX_POINT('',#106962) ;
#31017 = VERTEX_POINT('',#106964) ;
#31018 = VERTEX_POINT('',#106966) ;
#31019 = VERTEX_POINT('',#106970) ;
#31020 = VERTEX_POINT('',#106971) ;
#31021 = VERTEX_POINT('',#106980) ;
#31022 = VERTEX_POINT('',#106982) ;
#31023 = VERTEX_POINT('',#106984) ;
#31024 = VERTEX_POINT('',#106986) ;
#31025 = VERTEX_POINT('',#106997) ;
#31026 = VERTEX_POINT('',#106998) ;
#31027 = VERTEX_POINT('',#107000) ;
#31028 = VERTEX_POINT('',#107002) ;
#31029 = VERTEX_POINT('',#107004) ;
#31030 = VERTEX_POINT('',#107006) ;
#31031 = VERTEX_POINT('',#107008) ;
#31032 = VERTEX_POINT('',#107010) ;
#31033 = VERTEX_POINT('',#107014) ;
#31034 = VERTEX_POINT('',#107015) ;
#31035 = VERTEX_POINT('',#107017) ;
#31036 = VERTEX_POINT('',#107019) ;
#31037 = VERTEX_POINT('',#107021) ;
#31038 = VERTEX_POINT('',#107023) ;
#31039 = VERTEX_POINT('',#107025) ;
#31040 = VERTEX_POINT('',#107027) ;
#31041 = VERTEX_POINT('',#107031) ;
#31042 = VERTEX_POINT('',#107032) ;
#31043 = VERTEX_POINT('',#107035) ;
#31044 = VERTEX_POINT('',#107037) ;
#31045 = VERTEX_POINT('',#107039) ;
#31046 = VERTEX_POINT('',#107043) ;
#31047 = VERTEX_POINT('',#107045) ;
#31048 = VERTEX_POINT('',#107049) ;
#31049 = VERTEX_POINT('',#107050) ;
#31050 = VERTEX_POINT('',#107055) ;
#31051 = VERTEX_POINT('',#107056) ;
#31052 = VERTEX_POINT('',#107058) ;
#31053 = VERTEX_POINT('',#107060) ;
#31054 = VERTEX_POINT('',#107064) ;
#31055 = VERTEX_POINT('',#107065) ;
#31056 = VERTEX_POINT('',#107067) ;
#31057 = VERTEX_POINT('',#107069) ;
#31058 = VERTEX_POINT('',#107073) ;
#31059 = VERTEX_POINT('',#107075) ;
#31060 = VERTEX_POINT('',#107079) ;
#31061 = VERTEX_POINT('',#107080) ;
#31062 = VERTEX_POINT('',#107085) ;
#31063 = VERTEX_POINT('',#107086) ;
#31064 = VERTEX_POINT('',#107089) ;
#31065 = VERTEX_POINT('',#107091) ;
#31066 = VERTEX_POINT('',#107093) ;
#31067 = VERTEX_POINT('',#107097) ;
#31068 = VERTEX_POINT('',#107098) ;
#31069 = VERTEX_POINT('',#107101) ;
#31070 = VERTEX_POINT('',#107105) ;
#31071 = VERTEX_POINT('',#107106) ;
#31072 = VERTEX_POINT('',#107111) ;
#31073 = VERTEX_POINT('',#107112) ;
#31074 = VERTEX_POINT('',#107114) ;
#31075 = VERTEX_POINT('',#107116) ;
#31076 = VERTEX_POINT('',#107120) ;
#31077 = VERTEX_POINT('',#107121) ;
#31078 = VERTEX_POINT('',#107123) ;
#31079 = VERTEX_POINT('',#107125) ;
#31080 = VERTEX_POINT('',#107129) ;
#31081 = VERTEX_POINT('',#107130) ;
#31082 = VERTEX_POINT('',#107132) ;
#31083 = VERTEX_POINT('',#107134) ;
#31084 = VERTEX_POINT('',#107138) ;
#31085 = VERTEX_POINT('',#107140) ;
#31086 = VERTEX_POINT('',#107144) ;
#31087 = VERTEX_POINT('',#107145) ;
#31088 = VERTEX_POINT('',#107147) ;
#31089 = VERTEX_POINT('',#107149) ;
#31090 = VERTEX_POINT('',#107153) ;
#31091 = VERTEX_POINT('',#107154) ;
#31092 = VERTEX_POINT('',#107157) ;
#31093 = VERTEX_POINT('',#107161) ;
#31094 = VERTEX_POINT('',#107162) ;
#31095 = VERTEX_POINT('',#107164) ;
#31096 = VERTEX_POINT('',#107166) ;
#31097 = VERTEX_POINT('',#107170) ;
#31098 = VERTEX_POINT('',#107171) ;
#31099 = VERTEX_POINT('',#107174) ;
#31100 = VERTEX_POINT('',#107176) ;
#31101 = VERTEX_POINT('',#107178) ;
#31102 = VERTEX_POINT('',#107180) ;
#31103 = VERTEX_POINT('',#107184) ;
#31104 = VERTEX_POINT('',#107185) ;
#31105 = VERTEX_POINT('',#107188) ;
#31106 = VERTEX_POINT('',#107192) ;
#31107 = VERTEX_POINT('',#107193) ;
#31108 = VERTEX_POINT('',#107195) ;
#31109 = VERTEX_POINT('',#107197) ;
#31110 = VERTEX_POINT('',#107201) ;
#31111 = VERTEX_POINT('',#107202) ;
#31112 = VERTEX_POINT('',#107204) ;
#31113 = VERTEX_POINT('',#107206) ;
#31114 = VERTEX_POINT('',#107210) ;
#31115 = VERTEX_POINT('',#107211) ;
#31116 = VERTEX_POINT('',#107213) ;
#31117 = VERTEX_POINT('',#107215) ;
#31118 = VERTEX_POINT('',#107219) ;
#31119 = VERTEX_POINT('',#107221) ;
#31120 = VERTEX_POINT('',#107225) ;
#31121 = VERTEX_POINT('',#107227) ;
#31122 = VERTEX_POINT('',#107231) ;
#31123 = VERTEX_POINT('',#107233) ;
#31124 = VERTEX_POINT('',#107237) ;
#31125 = VERTEX_POINT('',#107239) ;
#31126 = VERTEX_POINT('',#107243) ;
#31127 = VERTEX_POINT('',#107244) ;
#31128 = VERTEX_POINT('',#107246) ;
#31129 = VERTEX_POINT('',#107248) ;
#31130 = VERTEX_POINT('',#107250) ;
#31131 = VERTEX_POINT('',#107252) ;
#31132 = VERTEX_POINT('',#107256) ;
#31133 = VERTEX_POINT('',#107257) ;
#31134 = VERTEX_POINT('',#107259) ;
#31135 = VERTEX_POINT('',#107261) ;
#31136 = VERTEX_POINT('',#107263) ;
#31137 = VERTEX_POINT('',#107265) ;
#31138 = VERTEX_POINT('',#107269) ;
#31139 = VERTEX_POINT('',#107270) ;
#31140 = VERTEX_POINT('',#107275) ;
#31141 = VERTEX_POINT('',#107277) ;
#31142 = VERTEX_POINT('',#107281) ;
#31143 = VERTEX_POINT('',#107282) ;
#31144 = VERTEX_POINT('',#107284) ;
#31145 = VERTEX_POINT('',#107286) ;
#31146 = VERTEX_POINT('',#107290) ;
#31147 = VERTEX_POINT('',#107291) ;
#31148 = VERTEX_POINT('',#107293) ;
#31149 = VERTEX_POINT('',#107295) ;
#31150 = VERTEX_POINT('',#107299) ;
#31151 = VERTEX_POINT('',#107300) ;
#31152 = VERTEX_POINT('',#107302) ;
#31153 = VERTEX_POINT('',#107304) ;
#31154 = VERTEX_POINT('',#107308) ;
#31155 = VERTEX_POINT('',#107309) ;
#31156 = VERTEX_POINT('',#107311) ;
#31157 = VERTEX_POINT('',#107313) ;
#31158 = VERTEX_POINT('',#107320) ;
#31159 = VERTEX_POINT('',#107321) ;
#31160 = VERTEX_POINT('',#107323) ;
#31161 = VERTEX_POINT('',#107325) ;
#31162 = VERTEX_POINT('',#107329) ;
#31163 = VERTEX_POINT('',#107330) ;
#31164 = VERTEX_POINT('',#107332) ;
#31165 = VERTEX_POINT('',#107334) ;
#31166 = VERTEX_POINT('',#107338) ;
#31167 = VERTEX_POINT('',#107339) ;
#31168 = VERTEX_POINT('',#107341) ;
#31169 = VERTEX_POINT('',#107343) ;
#31170 = VERTEX_POINT('',#107347) ;
#31171 = VERTEX_POINT('',#107348) ;
#31172 = VERTEX_POINT('',#107350) ;
#31173 = VERTEX_POINT('',#107352) ;
#31174 = VERTEX_POINT('',#107356) ;
#31175 = VERTEX_POINT('',#107358) ;
#31176 = VERTEX_POINT('',#107362) ;
#31177 = VERTEX_POINT('',#107363) ;
#31178 = VERTEX_POINT('',#107368) ;
#31179 = VERTEX_POINT('',#107370) ;
#31180 = VERTEX_POINT('',#107447) ;
#31181 = VERTEX_POINT('',#107464) ;
#31182 = VERTEX_POINT('',#107483) ;
#31183 = VERTEX_POINT('',#107499) ;
#31184 = VERTEX_POINT('',#107516) ;
#31185 = VERTEX_POINT('',#107532) ;
#31186 = VERTEX_POINT('',#107552) ;
#31187 = VERTEX_POINT('',#107556) ;
#31188 = VERTEX_POINT('',#107560) ;
#31189 = VERTEX_POINT('',#107578) ;
#31190 = VERTEX_POINT('',#107596) ;
#31191 = VERTEX_POINT('',#107605) ;
#31192 = VERTEX_POINT('',#107611) ;
#31193 = VERTEX_POINT('',#107619) ;
#31194 = VERTEX_POINT('',#107625) ;
#31195 = VERTEX_POINT('',#107638) ;
#31196 = VERTEX_POINT('',#107744) ;
#31197 = VERTEX_POINT('',#108171) ;
#31198 = VERTEX_POINT('',#108251) ;
#31199 = VERTEX_POINT('',#108262) ;
#31200 = VERTEX_POINT('',#108488) ;
#31201 = VERTEX_POINT('',#108505) ;
#31202 = VERTEX_POINT('',#108733) ;
#31203 = VERTEX_POINT('',#108734) ;
#31204 = VERTEX_POINT('',#108745) ;
#31205 = VERTEX_POINT('',#108747) ;
#31206 = VERTEX_POINT('',#108749) ;
#31207 = VERTEX_POINT('',#108770) ;
#31208 = VERTEX_POINT('',#108771) ;
#31209 = VERTEX_POINT('',#108788) ;
#31210 = VERTEX_POINT('',#108790) ;
#31211 = VERTEX_POINT('',#108792) ;
#31212 = VERTEX_POINT('',#108796) ;
#31213 = VERTEX_POINT('',#108798) ;
#31214 = VERTEX_POINT('',#108802) ;
#31215 = VERTEX_POINT('',#108804) ;
#31216 = VERTEX_POINT('',#108808) ;
#31217 = VERTEX_POINT('',#108809) ;
#31218 = VERTEX_POINT('',#108811) ;
#31219 = VERTEX_POINT('',#108813) ;
#31220 = VERTEX_POINT('',#108815) ;
#31221 = VERTEX_POINT('',#108819) ;
#31222 = VERTEX_POINT('',#108820) ;
#31223 = VERTEX_POINT('',#108822) ;
#31224 = VERTEX_POINT('',#108824) ;
#31225 = VERTEX_POINT('',#108828) ;
#31226 = VERTEX_POINT('',#108829) ;
#31227 = VERTEX_POINT('',#108831) ;
#31228 = VERTEX_POINT('',#108833) ;
#31229 = VERTEX_POINT('',#108839) ;
#31230 = VERTEX_POINT('',#108842) ;
#31231 = VERTEX_POINT('',#108849) ;
#31232 = VERTEX_POINT('',#108857) ;
#31233 = VERTEX_POINT('',#108861) ;
#31234 = VERTEX_POINT('',#108862) ;
#31235 = VERTEX_POINT('',#108864) ;
#31236 = VERTEX_POINT('',#108866) ;
#31237 = VERTEX_POINT('',#108873) ;
#31238 = VERTEX_POINT('',#108875) ;
#31239 = VERTEX_POINT('',#108879) ;
#31240 = VERTEX_POINT('',#108880) ;
#31241 = VERTEX_POINT('',#108882) ;
#31242 = VERTEX_POINT('',#108884) ;
#31243 = VERTEX_POINT('',#108913) ;
#31244 = VERTEX_POINT('',#108924) ;
#31245 = VERTEX_POINT('',#108928) ;
#31246 = VERTEX_POINT('',#108929) ;
#31247 = VERTEX_POINT('',#108931) ;
#31248 = VERTEX_POINT('',#108933) ;
#31249 = VERTEX_POINT('',#108937) ;
#31250 = VERTEX_POINT('',#108938) ;
#31251 = VERTEX_POINT('',#108940) ;
#31252 = VERTEX_POINT('',#108948) ;
#31253 = VERTEX_POINT('',#108961) ;
#31254 = VERTEX_POINT('',#108963) ;
#31255 = VERTEX_POINT('',#108967) ;
#31256 = VERTEX_POINT('',#108968) ;
#31257 = VERTEX_POINT('',#108970) ;
#31258 = VERTEX_POINT('',#108972) ;
#31259 = VERTEX_POINT('',#108976) ;
#31260 = VERTEX_POINT('',#108977) ;
#31261 = VERTEX_POINT('',#108979) ;
#31262 = VERTEX_POINT('',#108981) ;
#31263 = VERTEX_POINT('',#108985) ;
#31264 = VERTEX_POINT('',#108986) ;
#31265 = VERTEX_POINT('',#108988) ;
#31266 = VERTEX_POINT('',#108990) ;
#31267 = VERTEX_POINT('',#108992) ;
#31268 = VERTEX_POINT('',#108994) ;
#31269 = VERTEX_POINT('',#108998) ;
#31270 = VERTEX_POINT('',#108999) ;
#31271 = VERTEX_POINT('',#109004) ;
#31272 = VERTEX_POINT('',#109006) ;
#31273 = VERTEX_POINT('',#109008) ;
#31274 = VERTEX_POINT('',#109010) ;
#31275 = VERTEX_POINT('',#109012) ;
#31276 = VERTEX_POINT('',#109014) ;
#31277 = VERTEX_POINT('',#109016) ;
#31278 = VERTEX_POINT('',#109018) ;
#31279 = VERTEX_POINT('',#109020) ;
#31280 = VERTEX_POINT('',#109022) ;
#31281 = VERTEX_POINT('',#109024) ;
#31282 = VERTEX_POINT('',#109026) ;
#31283 = VERTEX_POINT('',#109029) ;
#31284 = VERTEX_POINT('',#109031) ;
#31285 = VERTEX_POINT('',#109034) ;
#31286 = VERTEX_POINT('',#109036) ;
#31287 = VERTEX_POINT('',#109038) ;
#31288 = VERTEX_POINT('',#109040) ;
#31289 = VERTEX_POINT('',#109042) ;
#31290 = VERTEX_POINT('',#109044) ;
#31291 = VERTEX_POINT('',#109046) ;
#31292 = VERTEX_POINT('',#109050) ;
#31293 = VERTEX_POINT('',#109051) ;
#31294 = VERTEX_POINT('',#109053) ;
#31295 = VERTEX_POINT('',#109055) ;
#31296 = VERTEX_POINT('',#109057) ;
#31297 = VERTEX_POINT('',#109059) ;
#31298 = VERTEX_POINT('',#109061) ;
#31299 = VERTEX_POINT('',#109063) ;
#31300 = VERTEX_POINT('',#109065) ;
#31301 = VERTEX_POINT('',#109067) ;
#31302 = VERTEX_POINT('',#109069) ;
#31303 = VERTEX_POINT('',#109072) ;
#31304 = VERTEX_POINT('',#109074) ;
#31305 = VERTEX_POINT('',#109077) ;
#31306 = VERTEX_POINT('',#109079) ;
#31307 = VERTEX_POINT('',#109081) ;
#31308 = VERTEX_POINT('',#109083) ;
#31309 = VERTEX_POINT('',#109085) ;
#31310 = VERTEX_POINT('',#109087) ;
#31311 = VERTEX_POINT('',#109089) ;
#31312 = VERTEX_POINT('',#109091) ;
#31313 = VERTEX_POINT('',#109093) ;
#31314 = VERTEX_POINT('',#109095) ;
#31315 = VERTEX_POINT('',#109097) ;
#31316 = VERTEX_POINT('',#109099) ;
#31317 = VERTEX_POINT('',#109101) ;
#31318 = VERTEX_POINT('',#109103) ;
#31319 = VERTEX_POINT('',#109105) ;
#31320 = VERTEX_POINT('',#109107) ;
#31321 = VERTEX_POINT('',#109117) ;
#31322 = VERTEX_POINT('',#109118) ;
#31323 = VERTEX_POINT('',#109161) ;
#31324 = VERTEX_POINT('',#109163) ;
#31325 = VERTEX_POINT('',#109206) ;
#31326 = VERTEX_POINT('',#109207) ;
#31327 = VERTEX_POINT('',#109215) ;
#31328 = VERTEX_POINT('',#109218) ;
#31329 = VERTEX_POINT('',#109222) ;
#31330 = VERTEX_POINT('',#109223) ;
#31331 = VERTEX_POINT('',#109228) ;
#31332 = VERTEX_POINT('',#109243) ;
#31333 = VERTEX_POINT('',#109248) ;
#31334 = VERTEX_POINT('',#109250) ;
#31335 = VERTEX_POINT('',#109285) ;
#31336 = VERTEX_POINT('',#109287) ;
#31337 = VERTEX_POINT('',#109341) ;
#31338 = VERTEX_POINT('',#109343) ;
#31339 = VERTEX_POINT('',#109345) ;
#31340 = VERTEX_POINT('',#109347) ;
#31341 = VERTEX_POINT('',#109349) ;
#31342 = VERTEX_POINT('',#109351) ;
#31343 = VERTEX_POINT('',#109355) ;
#31344 = VERTEX_POINT('',#109356) ;
#31345 = VERTEX_POINT('',#109359) ;
#31346 = VERTEX_POINT('',#109361) ;
#31347 = VERTEX_POINT('',#109363) ;
#31348 = VERTEX_POINT('',#109365) ;
#31349 = VERTEX_POINT('',#109367) ;
#31350 = VERTEX_POINT('',#109369) ;
#31351 = VERTEX_POINT('',#109371) ;
#31352 = VERTEX_POINT('',#109373) ;
#31353 = VERTEX_POINT('',#109375) ;
#31354 = VERTEX_POINT('',#109377) ;
#31355 = VERTEX_POINT('',#109380) ;
#31356 = VERTEX_POINT('',#109382) ;
#31357 = VERTEX_POINT('',#109384) ;
#31358 = VERTEX_POINT('',#109386) ;
#31359 = VERTEX_POINT('',#109388) ;
#31360 = VERTEX_POINT('',#109390) ;
#31361 = VERTEX_POINT('',#109392) ;
#31362 = VERTEX_POINT('',#109394) ;
#31363 = VERTEX_POINT('',#109398) ;
#31364 = VERTEX_POINT('',#109399) ;
#31365 = VERTEX_POINT('',#109401) ;
#31366 = VERTEX_POINT('',#109405) ;
#31367 = VERTEX_POINT('',#109407) ;
#31368 = VERTEX_POINT('',#109409) ;
#31369 = VERTEX_POINT('',#109413) ;
#31370 = VERTEX_POINT('',#109414) ;
#31371 = VERTEX_POINT('',#109418) ;
#31372 = VERTEX_POINT('',#109420) ;
#31373 = VERTEX_POINT('',#109424) ;
#31374 = VERTEX_POINT('',#109425) ;
#31375 = VERTEX_POINT('',#109427) ;
#31376 = VERTEX_POINT('',#109431) ;
#31377 = VERTEX_POINT('',#109432) ;
#31378 = VERTEX_POINT('',#109434) ;
#31379 = VERTEX_POINT('',#109438) ;
#31380 = VERTEX_POINT('',#109439) ;
#31381 = VERTEX_POINT('',#109441) ;
#31382 = VERTEX_POINT('',#109443) ;
#31383 = VERTEX_POINT('',#109445) ;
#31384 = VERTEX_POINT('',#109447) ;
#31385 = VERTEX_POINT('',#109449) ;
#31386 = VERTEX_POINT('',#109451) ;
#31387 = VERTEX_POINT('',#109455) ;
#31388 = VERTEX_POINT('',#109456) ;
#31389 = VERTEX_POINT('',#109458) ;
#31390 = VERTEX_POINT('',#109460) ;
#31391 = VERTEX_POINT('',#109464) ;
#31392 = VERTEX_POINT('',#109465) ;
#31393 = VERTEX_POINT('',#109467) ;
#31394 = VERTEX_POINT('',#109469) ;
#31395 = VERTEX_POINT('',#109473) ;
#31396 = VERTEX_POINT('',#109474) ;
#31397 = VERTEX_POINT('',#109476) ;
#31398 = VERTEX_POINT('',#109478) ;
#31399 = VERTEX_POINT('',#109482) ;
#31400 = VERTEX_POINT('',#109483) ;
#31401 = VERTEX_POINT('',#109492) ;
#31402 = VERTEX_POINT('',#109494) ;
#31403 = VERTEX_POINT('',#109496) ;
#31404 = VERTEX_POINT('',#109498) ;
#31405 = VERTEX_POINT('',#109509) ;
#31406 = VERTEX_POINT('',#109510) ;
#31407 = VERTEX_POINT('',#109512) ;
#31408 = VERTEX_POINT('',#109514) ;
#31409 = VERTEX_POINT('',#109516) ;
#31410 = VERTEX_POINT('',#109518) ;
#31411 = VERTEX_POINT('',#109520) ;
#31412 = VERTEX_POINT('',#109522) ;
#31413 = VERTEX_POINT('',#109526) ;
#31414 = VERTEX_POINT('',#109527) ;
#31415 = VERTEX_POINT('',#109529) ;
#31416 = VERTEX_POINT('',#109531) ;
#31417 = VERTEX_POINT('',#109533) ;
#31418 = VERTEX_POINT('',#109535) ;
#31419 = VERTEX_POINT('',#109537) ;
#31420 = VERTEX_POINT('',#109539) ;
#31421 = VERTEX_POINT('',#109543) ;
#31422 = VERTEX_POINT('',#109544) ;
#31423 = VERTEX_POINT('',#109547) ;
#31424 = VERTEX_POINT('',#109549) ;
#31425 = VERTEX_POINT('',#109551) ;
#31426 = VERTEX_POINT('',#109555) ;
#31427 = VERTEX_POINT('',#109557) ;
#31428 = VERTEX_POINT('',#109561) ;
#31429 = VERTEX_POINT('',#109562) ;
#31430 = VERTEX_POINT('',#109567) ;
#31431 = VERTEX_POINT('',#109568) ;
#31432 = VERTEX_POINT('',#109570) ;
#31433 = VERTEX_POINT('',#109572) ;
#31434 = VERTEX_POINT('',#109576) ;
#31435 = VERTEX_POINT('',#109577) ;
#31436 = VERTEX_POINT('',#109579) ;
#31437 = VERTEX_POINT('',#109581) ;
#31438 = VERTEX_POINT('',#109585) ;
#31439 = VERTEX_POINT('',#109587) ;
#31440 = VERTEX_POINT('',#109591) ;
#31441 = VERTEX_POINT('',#109592) ;
#31442 = VERTEX_POINT('',#109597) ;
#31443 = VERTEX_POINT('',#109598) ;
#31444 = VERTEX_POINT('',#109601) ;
#31445 = VERTEX_POINT('',#109603) ;
#31446 = VERTEX_POINT('',#109605) ;
#31447 = VERTEX_POINT('',#109609) ;
#31448 = VERTEX_POINT('',#109610) ;
#31449 = VERTEX_POINT('',#109613) ;
#31450 = VERTEX_POINT('',#109617) ;
#31451 = VERTEX_POINT('',#109618) ;
#31452 = VERTEX_POINT('',#109623) ;
#31453 = VERTEX_POINT('',#109624) ;
#31454 = VERTEX_POINT('',#109626) ;
#31455 = VERTEX_POINT('',#109628) ;
#31456 = VERTEX_POINT('',#109632) ;
#31457 = VERTEX_POINT('',#109633) ;
#31458 = VERTEX_POINT('',#109635) ;
#31459 = VERTEX_POINT('',#109637) ;
#31460 = VERTEX_POINT('',#109641) ;
#31461 = VERTEX_POINT('',#109642) ;
#31462 = VERTEX_POINT('',#109644) ;
#31463 = VERTEX_POINT('',#109646) ;
#31464 = VERTEX_POINT('',#109650) ;
#31465 = VERTEX_POINT('',#109652) ;
#31466 = VERTEX_POINT('',#109656) ;
#31467 = VERTEX_POINT('',#109657) ;
#31468 = VERTEX_POINT('',#109659) ;
#31469 = VERTEX_POINT('',#109661) ;
#31470 = VERTEX_POINT('',#109665) ;
#31471 = VERTEX_POINT('',#109666) ;
#31472 = VERTEX_POINT('',#109669) ;
#31473 = VERTEX_POINT('',#109673) ;
#31474 = VERTEX_POINT('',#109674) ;
#31475 = VERTEX_POINT('',#109676) ;
#31476 = VERTEX_POINT('',#109678) ;
#31477 = VERTEX_POINT('',#109682) ;
#31478 = VERTEX_POINT('',#109683) ;
#31479 = VERTEX_POINT('',#109686) ;
#31480 = VERTEX_POINT('',#109688) ;
#31481 = VERTEX_POINT('',#109690) ;
#31482 = VERTEX_POINT('',#109692) ;
#31483 = VERTEX_POINT('',#109696) ;
#31484 = VERTEX_POINT('',#109697) ;
#31485 = VERTEX_POINT('',#109700) ;
#31486 = VERTEX_POINT('',#109704) ;
#31487 = VERTEX_POINT('',#109705) ;
#31488 = VERTEX_POINT('',#109707) ;
#31489 = VERTEX_POINT('',#109709) ;
#31490 = VERTEX_POINT('',#109713) ;
#31491 = VERTEX_POINT('',#109714) ;
#31492 = VERTEX_POINT('',#109716) ;
#31493 = VERTEX_POINT('',#109718) ;
#31494 = VERTEX_POINT('',#109722) ;
#31495 = VERTEX_POINT('',#109723) ;
#31496 = VERTEX_POINT('',#109725) ;
#31497 = VERTEX_POINT('',#109727) ;
#31498 = VERTEX_POINT('',#109731) ;
#31499 = VERTEX_POINT('',#109733) ;
#31500 = VERTEX_POINT('',#109737) ;
#31501 = VERTEX_POINT('',#109739) ;
#31502 = VERTEX_POINT('',#109743) ;
#31503 = VERTEX_POINT('',#109745) ;
#31504 = VERTEX_POINT('',#109749) ;
#31505 = VERTEX_POINT('',#109751) ;
#31506 = VERTEX_POINT('',#109755) ;
#31507 = VERTEX_POINT('',#109756) ;
#31508 = VERTEX_POINT('',#109758) ;
#31509 = VERTEX_POINT('',#109760) ;
#31510 = VERTEX_POINT('',#109762) ;
#31511 = VERTEX_POINT('',#109764) ;
#31512 = VERTEX_POINT('',#109768) ;
#31513 = VERTEX_POINT('',#109769) ;
#31514 = VERTEX_POINT('',#109771) ;
#31515 = VERTEX_POINT('',#109773) ;
#31516 = VERTEX_POINT('',#109775) ;
#31517 = VERTEX_POINT('',#109777) ;
#31518 = VERTEX_POINT('',#109781) ;
#31519 = VERTEX_POINT('',#109782) ;
#31520 = VERTEX_POINT('',#109787) ;
#31521 = VERTEX_POINT('',#109789) ;
#31522 = VERTEX_POINT('',#109793) ;
#31523 = VERTEX_POINT('',#109794) ;
#31524 = VERTEX_POINT('',#109796) ;
#31525 = VERTEX_POINT('',#109798) ;
#31526 = VERTEX_POINT('',#109802) ;
#31527 = VERTEX_POINT('',#109803) ;
#31528 = VERTEX_POINT('',#109805) ;
#31529 = VERTEX_POINT('',#109807) ;
#31530 = VERTEX_POINT('',#109811) ;
#31531 = VERTEX_POINT('',#109812) ;
#31532 = VERTEX_POINT('',#109814) ;
#31533 = VERTEX_POINT('',#109816) ;
#31534 = VERTEX_POINT('',#109820) ;
#31535 = VERTEX_POINT('',#109821) ;
#31536 = VERTEX_POINT('',#109823) ;
#31537 = VERTEX_POINT('',#109825) ;
#31538 = VERTEX_POINT('',#109832) ;
#31539 = VERTEX_POINT('',#109833) ;
#31540 = VERTEX_POINT('',#109835) ;
#31541 = VERTEX_POINT('',#109837) ;
#31542 = VERTEX_POINT('',#109841) ;
#31543 = VERTEX_POINT('',#109842) ;
#31544 = VERTEX_POINT('',#109844) ;
#31545 = VERTEX_POINT('',#109846) ;
#31546 = VERTEX_POINT('',#109850) ;
#31547 = VERTEX_POINT('',#109851) ;
#31548 = VERTEX_POINT('',#109853) ;
#31549 = VERTEX_POINT('',#109855) ;
#31550 = VERTEX_POINT('',#109859) ;
#31551 = VERTEX_POINT('',#109860) ;
#31552 = VERTEX_POINT('',#109862) ;
#31553 = VERTEX_POINT('',#109864) ;
#31554 = VERTEX_POINT('',#109868) ;
#31555 = VERTEX_POINT('',#109870) ;
#31556 = VERTEX_POINT('',#109874) ;
#31557 = VERTEX_POINT('',#109875) ;
#31558 = VERTEX_POINT('',#109880) ;
#31559 = VERTEX_POINT('',#109882) ;
#31560 = VERTEX_POINT('',#109959) ;
#31561 = VERTEX_POINT('',#109976) ;
#31562 = VERTEX_POINT('',#109995) ;
#31563 = VERTEX_POINT('',#110011) ;
#31564 = VERTEX_POINT('',#110028) ;
#31565 = VERTEX_POINT('',#110044) ;
#31566 = VERTEX_POINT('',#110064) ;
#31567 = VERTEX_POINT('',#110068) ;
#31568 = VERTEX_POINT('',#110072) ;
#31569 = VERTEX_POINT('',#110090) ;
#31570 = VERTEX_POINT('',#110108) ;
#31571 = VERTEX_POINT('',#110117) ;
#31572 = VERTEX_POINT('',#110123) ;
#31573 = VERTEX_POINT('',#110131) ;
#31574 = VERTEX_POINT('',#110137) ;
#31575 = VERTEX_POINT('',#110150) ;
#31576 = VERTEX_POINT('',#110256) ;
#31577 = VERTEX_POINT('',#110683) ;
#31578 = VERTEX_POINT('',#110763) ;
#31579 = VERTEX_POINT('',#110774) ;
#31580 = VERTEX_POINT('',#111000) ;
#31581 = VERTEX_POINT('',#111017) ;
#31582 = VERTEX_POINT('',#111245) ;
#31583 = VERTEX_POINT('',#111246) ;
#31584 = VERTEX_POINT('',#111257) ;
#31585 = VERTEX_POINT('',#111259) ;
#31586 = VERTEX_POINT('',#111261) ;
#31587 = VERTEX_POINT('',#111282) ;
#31588 = VERTEX_POINT('',#111283) ;
#31589 = VERTEX_POINT('',#111300) ;
#31590 = VERTEX_POINT('',#111302) ;
#31591 = VERTEX_POINT('',#111304) ;
#31592 = VERTEX_POINT('',#111308) ;
#31593 = VERTEX_POINT('',#111310) ;
#31594 = VERTEX_POINT('',#111314) ;
#31595 = VERTEX_POINT('',#111316) ;
#31596 = VERTEX_POINT('',#111320) ;
#31597 = VERTEX_POINT('',#111321) ;
#31598 = VERTEX_POINT('',#111323) ;
#31599 = VERTEX_POINT('',#111325) ;
#31600 = VERTEX_POINT('',#111327) ;
#31601 = VERTEX_POINT('',#111331) ;
#31602 = VERTEX_POINT('',#111332) ;
#31603 = VERTEX_POINT('',#111334) ;
#31604 = VERTEX_POINT('',#111336) ;
#31605 = VERTEX_POINT('',#111340) ;
#31606 = VERTEX_POINT('',#111341) ;
#31607 = VERTEX_POINT('',#111343) ;
#31608 = VERTEX_POINT('',#111345) ;
#31609 = VERTEX_POINT('',#111351) ;
#31610 = VERTEX_POINT('',#111354) ;
#31611 = VERTEX_POINT('',#111361) ;
#31612 = VERTEX_POINT('',#111369) ;
#31613 = VERTEX_POINT('',#111373) ;
#31614 = VERTEX_POINT('',#111374) ;
#31615 = VERTEX_POINT('',#111376) ;
#31616 = VERTEX_POINT('',#111378) ;
#31617 = VERTEX_POINT('',#111385) ;
#31618 = VERTEX_POINT('',#111387) ;
#31619 = VERTEX_POINT('',#111391) ;
#31620 = VERTEX_POINT('',#111392) ;
#31621 = VERTEX_POINT('',#111394) ;
#31622 = VERTEX_POINT('',#111396) ;
#31623 = VERTEX_POINT('',#111425) ;
#31624 = VERTEX_POINT('',#111436) ;
#31625 = VERTEX_POINT('',#111440) ;
#31626 = VERTEX_POINT('',#111441) ;
#31627 = VERTEX_POINT('',#111443) ;
#31628 = VERTEX_POINT('',#111445) ;
#31629 = VERTEX_POINT('',#111449) ;
#31630 = VERTEX_POINT('',#111450) ;
#31631 = VERTEX_POINT('',#111452) ;
#31632 = VERTEX_POINT('',#111460) ;
#31633 = VERTEX_POINT('',#111473) ;
#31634 = VERTEX_POINT('',#111475) ;
#31635 = VERTEX_POINT('',#111479) ;
#31636 = VERTEX_POINT('',#111480) ;
#31637 = VERTEX_POINT('',#111482) ;
#31638 = VERTEX_POINT('',#111484) ;
#31639 = VERTEX_POINT('',#111488) ;
#31640 = VERTEX_POINT('',#111489) ;
#31641 = VERTEX_POINT('',#111491) ;
#31642 = VERTEX_POINT('',#111493) ;
#31643 = VERTEX_POINT('',#111497) ;
#31644 = VERTEX_POINT('',#111498) ;
#31645 = VERTEX_POINT('',#111500) ;
#31646 = VERTEX_POINT('',#111502) ;
#31647 = VERTEX_POINT('',#111504) ;
#31648 = VERTEX_POINT('',#111506) ;
#31649 = VERTEX_POINT('',#111510) ;
#31650 = VERTEX_POINT('',#111511) ;
#31651 = VERTEX_POINT('',#111516) ;
#31652 = VERTEX_POINT('',#111518) ;
#31653 = VERTEX_POINT('',#111520) ;
#31654 = VERTEX_POINT('',#111522) ;
#31655 = VERTEX_POINT('',#111524) ;
#31656 = VERTEX_POINT('',#111526) ;
#31657 = VERTEX_POINT('',#111528) ;
#31658 = VERTEX_POINT('',#111530) ;
#31659 = VERTEX_POINT('',#111532) ;
#31660 = VERTEX_POINT('',#111534) ;
#31661 = VERTEX_POINT('',#111536) ;
#31662 = VERTEX_POINT('',#111538) ;
#31663 = VERTEX_POINT('',#111541) ;
#31664 = VERTEX_POINT('',#111543) ;
#31665 = VERTEX_POINT('',#111546) ;
#31666 = VERTEX_POINT('',#111548) ;
#31667 = VERTEX_POINT('',#111550) ;
#31668 = VERTEX_POINT('',#111552) ;
#31669 = VERTEX_POINT('',#111554) ;
#31670 = VERTEX_POINT('',#111556) ;
#31671 = VERTEX_POINT('',#111558) ;
#31672 = VERTEX_POINT('',#111562) ;
#31673 = VERTEX_POINT('',#111563) ;
#31674 = VERTEX_POINT('',#111565) ;
#31675 = VERTEX_POINT('',#111567) ;
#31676 = VERTEX_POINT('',#111569) ;
#31677 = VERTEX_POINT('',#111571) ;
#31678 = VERTEX_POINT('',#111573) ;
#31679 = VERTEX_POINT('',#111575) ;
#31680 = VERTEX_POINT('',#111577) ;
#31681 = VERTEX_POINT('',#111579) ;
#31682 = VERTEX_POINT('',#111581) ;
#31683 = VERTEX_POINT('',#111584) ;
#31684 = VERTEX_POINT('',#111586) ;
#31685 = VERTEX_POINT('',#111589) ;
#31686 = VERTEX_POINT('',#111591) ;
#31687 = VERTEX_POINT('',#111593) ;
#31688 = VERTEX_POINT('',#111595) ;
#31689 = VERTEX_POINT('',#111597) ;
#31690 = VERTEX_POINT('',#111599) ;
#31691 = VERTEX_POINT('',#111601) ;
#31692 = VERTEX_POINT('',#111603) ;
#31693 = VERTEX_POINT('',#111605) ;
#31694 = VERTEX_POINT('',#111607) ;
#31695 = VERTEX_POINT('',#111609) ;
#31696 = VERTEX_POINT('',#111611) ;
#31697 = VERTEX_POINT('',#111613) ;
#31698 = VERTEX_POINT('',#111615) ;
#31699 = VERTEX_POINT('',#111617) ;
#31700 = VERTEX_POINT('',#111619) ;
#31701 = VERTEX_POINT('',#111629) ;
#31702 = VERTEX_POINT('',#111630) ;
#31703 = VERTEX_POINT('',#111673) ;
#31704 = VERTEX_POINT('',#111675) ;
#31705 = VERTEX_POINT('',#111718) ;
#31706 = VERTEX_POINT('',#111719) ;
#31707 = VERTEX_POINT('',#111727) ;
#31708 = VERTEX_POINT('',#111730) ;
#31709 = VERTEX_POINT('',#111734) ;
#31710 = VERTEX_POINT('',#111735) ;
#31711 = VERTEX_POINT('',#111740) ;
#31712 = VERTEX_POINT('',#111755) ;
#31713 = VERTEX_POINT('',#111760) ;
#31714 = VERTEX_POINT('',#111762) ;
#31715 = VERTEX_POINT('',#111797) ;
#31716 = VERTEX_POINT('',#111799) ;
#31717 = VERTEX_POINT('',#111853) ;
#31718 = VERTEX_POINT('',#111855) ;
#31719 = VERTEX_POINT('',#111857) ;
#31720 = VERTEX_POINT('',#111859) ;
#31721 = VERTEX_POINT('',#111861) ;
#31722 = VERTEX_POINT('',#111863) ;
#31723 = VERTEX_POINT('',#111867) ;
#31724 = VERTEX_POINT('',#111868) ;
#31725 = VERTEX_POINT('',#111871) ;
#31726 = VERTEX_POINT('',#111873) ;
#31727 = VERTEX_POINT('',#111875) ;
#31728 = VERTEX_POINT('',#111877) ;
#31729 = VERTEX_POINT('',#111879) ;
#31730 = VERTEX_POINT('',#111881) ;
#31731 = VERTEX_POINT('',#111883) ;
#31732 = VERTEX_POINT('',#111885) ;
#31733 = VERTEX_POINT('',#111887) ;
#31734 = VERTEX_POINT('',#111889) ;
#31735 = VERTEX_POINT('',#111892) ;
#31736 = VERTEX_POINT('',#111894) ;
#31737 = VERTEX_POINT('',#111896) ;
#31738 = VERTEX_POINT('',#111898) ;
#31739 = VERTEX_POINT('',#111900) ;
#31740 = VERTEX_POINT('',#111902) ;
#31741 = VERTEX_POINT('',#111904) ;
#31742 = VERTEX_POINT('',#111906) ;
#31743 = VERTEX_POINT('',#111910) ;
#31744 = VERTEX_POINT('',#111911) ;
#31745 = VERTEX_POINT('',#111913) ;
#31746 = VERTEX_POINT('',#111917) ;
#31747 = VERTEX_POINT('',#111919) ;
#31748 = VERTEX_POINT('',#111921) ;
#31749 = VERTEX_POINT('',#111925) ;
#31750 = VERTEX_POINT('',#111926) ;
#31751 = VERTEX_POINT('',#111930) ;
#31752 = VERTEX_POINT('',#111932) ;
#31753 = VERTEX_POINT('',#111936) ;
#31754 = VERTEX_POINT('',#111937) ;
#31755 = VERTEX_POINT('',#111939) ;
#31756 = VERTEX_POINT('',#111943) ;
#31757 = VERTEX_POINT('',#111944) ;
#31758 = VERTEX_POINT('',#111946) ;
#31759 = VERTEX_POINT('',#111950) ;
#31760 = VERTEX_POINT('',#111951) ;
#31761 = VERTEX_POINT('',#111953) ;
#31762 = VERTEX_POINT('',#111955) ;
#31763 = VERTEX_POINT('',#111957) ;
#31764 = VERTEX_POINT('',#111959) ;
#31765 = VERTEX_POINT('',#111961) ;
#31766 = VERTEX_POINT('',#111963) ;
#31767 = VERTEX_POINT('',#111967) ;
#31768 = VERTEX_POINT('',#111968) ;
#31769 = VERTEX_POINT('',#111970) ;
#31770 = VERTEX_POINT('',#111972) ;
#31771 = VERTEX_POINT('',#111976) ;
#31772 = VERTEX_POINT('',#111977) ;
#31773 = VERTEX_POINT('',#111979) ;
#31774 = VERTEX_POINT('',#111981) ;
#31775 = VERTEX_POINT('',#111985) ;
#31776 = VERTEX_POINT('',#111986) ;
#31777 = VERTEX_POINT('',#111988) ;
#31778 = VERTEX_POINT('',#111990) ;
#31779 = VERTEX_POINT('',#111994) ;
#31780 = VERTEX_POINT('',#111995) ;
#31781 = VERTEX_POINT('',#112004) ;
#31782 = VERTEX_POINT('',#112006) ;
#31783 = VERTEX_POINT('',#112008) ;
#31784 = VERTEX_POINT('',#112010) ;
#31785 = VERTEX_POINT('',#112021) ;
#31786 = VERTEX_POINT('',#112022) ;
#31787 = VERTEX_POINT('',#112024) ;
#31788 = VERTEX_POINT('',#112026) ;
#31789 = VERTEX_POINT('',#112028) ;
#31790 = VERTEX_POINT('',#112030) ;
#31791 = VERTEX_POINT('',#112032) ;
#31792 = VERTEX_POINT('',#112034) ;
#31793 = VERTEX_POINT('',#112038) ;
#31794 = VERTEX_POINT('',#112039) ;
#31795 = VERTEX_POINT('',#112041) ;
#31796 = VERTEX_POINT('',#112043) ;
#31797 = VERTEX_POINT('',#112045) ;
#31798 = VERTEX_POINT('',#112047) ;
#31799 = VERTEX_POINT('',#112049) ;
#31800 = VERTEX_POINT('',#112051) ;
#31801 = VERTEX_POINT('',#112055) ;
#31802 = VERTEX_POINT('',#112056) ;
#31803 = VERTEX_POINT('',#112059) ;
#31804 = VERTEX_POINT('',#112061) ;
#31805 = VERTEX_POINT('',#112063) ;
#31806 = VERTEX_POINT('',#112067) ;
#31807 = VERTEX_POINT('',#112069) ;
#31808 = VERTEX_POINT('',#112073) ;
#31809 = VERTEX_POINT('',#112074) ;
#31810 = VERTEX_POINT('',#112079) ;
#31811 = VERTEX_POINT('',#112080) ;
#31812 = VERTEX_POINT('',#112082) ;
#31813 = VERTEX_POINT('',#112084) ;
#31814 = VERTEX_POINT('',#112088) ;
#31815 = VERTEX_POINT('',#112089) ;
#31816 = VERTEX_POINT('',#112091) ;
#31817 = VERTEX_POINT('',#112093) ;
#31818 = VERTEX_POINT('',#112097) ;
#31819 = VERTEX_POINT('',#112099) ;
#31820 = VERTEX_POINT('',#112103) ;
#31821 = VERTEX_POINT('',#112104) ;
#31822 = VERTEX_POINT('',#112109) ;
#31823 = VERTEX_POINT('',#112110) ;
#31824 = VERTEX_POINT('',#112113) ;
#31825 = VERTEX_POINT('',#112115) ;
#31826 = VERTEX_POINT('',#112117) ;
#31827 = VERTEX_POINT('',#112121) ;
#31828 = VERTEX_POINT('',#112122) ;
#31829 = VERTEX_POINT('',#112125) ;
#31830 = VERTEX_POINT('',#112129) ;
#31831 = VERTEX_POINT('',#112130) ;
#31832 = VERTEX_POINT('',#112135) ;
#31833 = VERTEX_POINT('',#112136) ;
#31834 = VERTEX_POINT('',#112138) ;
#31835 = VERTEX_POINT('',#112140) ;
#31836 = VERTEX_POINT('',#112144) ;
#31837 = VERTEX_POINT('',#112145) ;
#31838 = VERTEX_POINT('',#112147) ;
#31839 = VERTEX_POINT('',#112149) ;
#31840 = VERTEX_POINT('',#112153) ;
#31841 = VERTEX_POINT('',#112154) ;
#31842 = VERTEX_POINT('',#112156) ;
#31843 = VERTEX_POINT('',#112158) ;
#31844 = VERTEX_POINT('',#112162) ;
#31845 = VERTEX_POINT('',#112164) ;
#31846 = VERTEX_POINT('',#112168) ;
#31847 = VERTEX_POINT('',#112169) ;
#31848 = VERTEX_POINT('',#112171) ;
#31849 = VERTEX_POINT('',#112173) ;
#31850 = VERTEX_POINT('',#112177) ;
#31851 = VERTEX_POINT('',#112178) ;
#31852 = VERTEX_POINT('',#112181) ;
#31853 = VERTEX_POINT('',#112185) ;
#31854 = VERTEX_POINT('',#112186) ;
#31855 = VERTEX_POINT('',#112188) ;
#31856 = VERTEX_POINT('',#112190) ;
#31857 = VERTEX_POINT('',#112194) ;
#31858 = VERTEX_POINT('',#112195) ;
#31859 = VERTEX_POINT('',#112198) ;
#31860 = VERTEX_POINT('',#112200) ;
#31861 = VERTEX_POINT('',#112202) ;
#31862 = VERTEX_POINT('',#112204) ;
#31863 = VERTEX_POINT('',#112208) ;
#31864 = VERTEX_POINT('',#112209) ;
#31865 = VERTEX_POINT('',#112212) ;
#31866 = VERTEX_POINT('',#112216) ;
#31867 = VERTEX_POINT('',#112217) ;
#31868 = VERTEX_POINT('',#112219) ;
#31869 = VERTEX_POINT('',#112221) ;
#31870 = VERTEX_POINT('',#112225) ;
#31871 = VERTEX_POINT('',#112226) ;
#31872 = VERTEX_POINT('',#112228) ;
#31873 = VERTEX_POINT('',#112230) ;
#31874 = VERTEX_POINT('',#112234) ;
#31875 = VERTEX_POINT('',#112235) ;
#31876 = VERTEX_POINT('',#112237) ;
#31877 = VERTEX_POINT('',#112239) ;
#31878 = VERTEX_POINT('',#112243) ;
#31879 = VERTEX_POINT('',#112245) ;
#31880 = VERTEX_POINT('',#112249) ;
#31881 = VERTEX_POINT('',#112251) ;
#31882 = VERTEX_POINT('',#112255) ;
#31883 = VERTEX_POINT('',#112257) ;
#31884 = VERTEX_POINT('',#112261) ;
#31885 = VERTEX_POINT('',#112263) ;
#31886 = VERTEX_POINT('',#112267) ;
#31887 = VERTEX_POINT('',#112268) ;
#31888 = VERTEX_POINT('',#112270) ;
#31889 = VERTEX_POINT('',#112272) ;
#31890 = VERTEX_POINT('',#112274) ;
#31891 = VERTEX_POINT('',#112276) ;
#31892 = VERTEX_POINT('',#112280) ;
#31893 = VERTEX_POINT('',#112281) ;
#31894 = VERTEX_POINT('',#112283) ;
#31895 = VERTEX_POINT('',#112285) ;
#31896 = VERTEX_POINT('',#112287) ;
#31897 = VERTEX_POINT('',#112289) ;
#31898 = VERTEX_POINT('',#112293) ;
#31899 = VERTEX_POINT('',#112294) ;
#31900 = VERTEX_POINT('',#112299) ;
#31901 = VERTEX_POINT('',#112301) ;
#31902 = VERTEX_POINT('',#112305) ;
#31903 = VERTEX_POINT('',#112306) ;
#31904 = VERTEX_POINT('',#112308) ;
#31905 = VERTEX_POINT('',#112310) ;
#31906 = VERTEX_POINT('',#112314) ;
#31907 = VERTEX_POINT('',#112315) ;
#31908 = VERTEX_POINT('',#112317) ;
#31909 = VERTEX_POINT('',#112319) ;
#31910 = VERTEX_POINT('',#112323) ;
#31911 = VERTEX_POINT('',#112324) ;
#31912 = VERTEX_POINT('',#112326) ;
#31913 = VERTEX_POINT('',#112328) ;
#31914 = VERTEX_POINT('',#112332) ;
#31915 = VERTEX_POINT('',#112333) ;
#31916 = VERTEX_POINT('',#112335) ;
#31917 = VERTEX_POINT('',#112337) ;
#31918 = VERTEX_POINT('',#112344) ;
#31919 = VERTEX_POINT('',#112345) ;
#31920 = VERTEX_POINT('',#112347) ;
#31921 = VERTEX_POINT('',#112349) ;
#31922 = VERTEX_POINT('',#112353) ;
#31923 = VERTEX_POINT('',#112354) ;
#31924 = VERTEX_POINT('',#112356) ;
#31925 = VERTEX_POINT('',#112358) ;
#31926 = VERTEX_POINT('',#112362) ;
#31927 = VERTEX_POINT('',#112363) ;
#31928 = VERTEX_POINT('',#112365) ;
#31929 = VERTEX_POINT('',#112367) ;
#31930 = VERTEX_POINT('',#112371) ;
#31931 = VERTEX_POINT('',#112372) ;
#31932 = VERTEX_POINT('',#112374) ;
#31933 = VERTEX_POINT('',#112376) ;
#31934 = VERTEX_POINT('',#112380) ;
#31935 = VERTEX_POINT('',#112382) ;
#31936 = VERTEX_POINT('',#112386) ;
#31937 = VERTEX_POINT('',#112387) ;
#31938 = VERTEX_POINT('',#112392) ;
#31939 = VERTEX_POINT('',#112394) ;
#31940 = VERTEX_POINT('',#112471) ;
#31941 = VERTEX_POINT('',#112488) ;
#31942 = VERTEX_POINT('',#112507) ;
#31943 = VERTEX_POINT('',#112523) ;
#31944 = VERTEX_POINT('',#112540) ;
#31945 = VERTEX_POINT('',#112556) ;
#31946 = VERTEX_POINT('',#112576) ;
#31947 = VERTEX_POINT('',#112580) ;
#31948 = VERTEX_POINT('',#112584) ;
#31949 = VERTEX_POINT('',#112602) ;
#31950 = VERTEX_POINT('',#112620) ;
#31951 = VERTEX_POINT('',#112629) ;
#31952 = VERTEX_POINT('',#112635) ;
#31953 = VERTEX_POINT('',#112643) ;
#31954 = VERTEX_POINT('',#112649) ;
#31955 = VERTEX_POINT('',#112662) ;
#31956 = VERTEX_POINT('',#112768) ;
#31957 = VERTEX_POINT('',#113195) ;
#31958 = VERTEX_POINT('',#113275) ;
#31959 = VERTEX_POINT('',#113286) ;
#31960 = VERTEX_POINT('',#113512) ;
#31961 = VERTEX_POINT('',#113529) ;
#31962 = VERTEX_POINT('',#113747) ;
#31963 = VERTEX_POINT('',#113749) ;
#31964 = VERTEX_POINT('',#113751) ;
#31965 = VERTEX_POINT('',#113755) ;
#31966 = VERTEX_POINT('',#113756) ;
#31967 = VERTEX_POINT('',#113758) ;
#31968 = VERTEX_POINT('',#113760) ;
#31969 = VERTEX_POINT('',#113764) ;
#31970 = VERTEX_POINT('',#113765) ;
#31971 = VERTEX_POINT('',#113767) ;
#31972 = VERTEX_POINT('',#113769) ;
#31973 = VERTEX_POINT('',#113771) ;
#31974 = VERTEX_POINT('',#113773) ;
#31975 = VERTEX_POINT('',#113775) ;
#31976 = VERTEX_POINT('',#113779) ;
#31977 = VERTEX_POINT('',#113780) ;
#31978 = VERTEX_POINT('',#113782) ;
#31979 = VERTEX_POINT('',#113784) ;
#31980 = VERTEX_POINT('',#113786) ;
#31981 = VERTEX_POINT('',#113788) ;
#31982 = VERTEX_POINT('',#113790) ;
#31983 = VERTEX_POINT('',#113797) ;
#31984 = VERTEX_POINT('',#113798) ;
#31985 = VERTEX_POINT('',#113800) ;
#31986 = VERTEX_POINT('',#113802) ;
#31987 = VERTEX_POINT('',#113804) ;
#31988 = VERTEX_POINT('',#113806) ;
#31989 = VERTEX_POINT('',#113808) ;
#31990 = VERTEX_POINT('',#113812) ;
#31991 = VERTEX_POINT('',#113813) ;
#31992 = VERTEX_POINT('',#113818) ;
#31993 = VERTEX_POINT('',#113819) ;
#31994 = VERTEX_POINT('',#113821) ;
#31995 = VERTEX_POINT('',#113823) ;
#31996 = VERTEX_POINT('',#113826) ;
#31997 = VERTEX_POINT('',#113854) ;
#31998 = VERTEX_POINT('',#113860) ;
#31999 = VERTEX_POINT('',#113862) ;
#32000 = VERTEX_POINT('',#113864) ;
#32001 = VERTEX_POINT('',#113868) ;
#32002 = VERTEX_POINT('',#113870) ;
#32003 = VERTEX_POINT('',#113874) ;
#32004 = VERTEX_POINT('',#113875) ;
#32005 = VERTEX_POINT('',#113877) ;
#32006 = VERTEX_POINT('',#113881) ;
#32007 = VERTEX_POINT('',#113882) ;
#32008 = VERTEX_POINT('',#113884) ;
#32009 = VERTEX_POINT('',#113886) ;
#32010 = VERTEX_POINT('',#113888) ;
#32011 = VERTEX_POINT('',#113890) ;
#32012 = VERTEX_POINT('',#113892) ;
#32013 = VERTEX_POINT('',#113903) ;
#32014 = VERTEX_POINT('',#113905) ;
#32015 = VERTEX_POINT('',#113907) ;
#32016 = VERTEX_POINT('',#113911) ;
#32017 = VERTEX_POINT('',#113913) ;
#32018 = VERTEX_POINT('',#113917) ;
#32019 = VERTEX_POINT('',#113918) ;
#32020 = VERTEX_POINT('',#113920) ;
#32021 = VERTEX_POINT('',#113924) ;
#32022 = VERTEX_POINT('',#113925) ;
#32023 = VERTEX_POINT('',#113927) ;
#32024 = VERTEX_POINT('',#113929) ;
#32025 = VERTEX_POINT('',#113931) ;
#32026 = VERTEX_POINT('',#113933) ;
#32027 = VERTEX_POINT('',#113935) ;
#32028 = VERTEX_POINT('',#113946) ;
#32029 = VERTEX_POINT('',#113948) ;
#32030 = VERTEX_POINT('',#113950) ;
#32031 = VERTEX_POINT('',#113954) ;
#32032 = VERTEX_POINT('',#113956) ;
#32033 = VERTEX_POINT('',#113960) ;
#32034 = VERTEX_POINT('',#113961) ;
#32035 = VERTEX_POINT('',#113963) ;
#32036 = VERTEX_POINT('',#113967) ;
#32037 = VERTEX_POINT('',#113968) ;
#32038 = VERTEX_POINT('',#113970) ;
#32039 = VERTEX_POINT('',#113972) ;
#32040 = VERTEX_POINT('',#113974) ;
#32041 = VERTEX_POINT('',#113976) ;
#32042 = VERTEX_POINT('',#113978) ;
#32043 = VERTEX_POINT('',#113989) ;
#32044 = VERTEX_POINT('',#113991) ;
#32045 = VERTEX_POINT('',#113993) ;
#32046 = VERTEX_POINT('',#113997) ;
#32047 = VERTEX_POINT('',#113999) ;
#32048 = VERTEX_POINT('',#114003) ;
#32049 = VERTEX_POINT('',#114004) ;
#32050 = VERTEX_POINT('',#114006) ;
#32051 = VERTEX_POINT('',#114010) ;
#32052 = VERTEX_POINT('',#114011) ;
#32053 = VERTEX_POINT('',#114013) ;
#32054 = VERTEX_POINT('',#114015) ;
#32055 = VERTEX_POINT('',#114017) ;
#32056 = VERTEX_POINT('',#114019) ;
#32057 = VERTEX_POINT('',#114021) ;
#32058 = VERTEX_POINT('',#114032) ;
#32059 = VERTEX_POINT('',#114034) ;
#32060 = VERTEX_POINT('',#114036) ;
#32061 = VERTEX_POINT('',#114040) ;
#32062 = VERTEX_POINT('',#114042) ;
#32063 = VERTEX_POINT('',#114046) ;
#32064 = VERTEX_POINT('',#114047) ;
#32065 = VERTEX_POINT('',#114049) ;
#32066 = VERTEX_POINT('',#114053) ;
#32067 = VERTEX_POINT('',#114054) ;
#32068 = VERTEX_POINT('',#114056) ;
#32069 = VERTEX_POINT('',#114058) ;
#32070 = VERTEX_POINT('',#114060) ;
#32071 = VERTEX_POINT('',#114062) ;
#32072 = VERTEX_POINT('',#114064) ;
#32073 = VERTEX_POINT('',#114075) ;
#32074 = VERTEX_POINT('',#114077) ;
#32075 = VERTEX_POINT('',#114079) ;
#32076 = VERTEX_POINT('',#114083) ;
#32077 = VERTEX_POINT('',#114085) ;
#32078 = VERTEX_POINT('',#114089) ;
#32079 = VERTEX_POINT('',#114090) ;
#32080 = VERTEX_POINT('',#114092) ;
#32081 = VERTEX_POINT('',#114096) ;
#32082 = VERTEX_POINT('',#114097) ;
#32083 = VERTEX_POINT('',#114099) ;
#32084 = VERTEX_POINT('',#114101) ;
#32085 = VERTEX_POINT('',#114103) ;
#32086 = VERTEX_POINT('',#114105) ;
#32087 = VERTEX_POINT('',#114107) ;
#32088 = VERTEX_POINT('',#114118) ;
#32089 = VERTEX_POINT('',#114120) ;
#32090 = VERTEX_POINT('',#114122) ;
#32091 = VERTEX_POINT('',#114126) ;
#32092 = VERTEX_POINT('',#114128) ;
#32093 = VERTEX_POINT('',#114132) ;
#32094 = VERTEX_POINT('',#114133) ;
#32095 = VERTEX_POINT('',#114135) ;
#32096 = VERTEX_POINT('',#114139) ;
#32097 = VERTEX_POINT('',#114140) ;
#32098 = VERTEX_POINT('',#114142) ;
#32099 = VERTEX_POINT('',#114144) ;
#32100 = VERTEX_POINT('',#114146) ;
#32101 = VERTEX_POINT('',#114148) ;
#32102 = VERTEX_POINT('',#114150) ;
#32103 = VERTEX_POINT('',#114161) ;
#32104 = VERTEX_POINT('',#114163) ;
#32105 = VERTEX_POINT('',#114165) ;
#32106 = VERTEX_POINT('',#114169) ;
#32107 = VERTEX_POINT('',#114171) ;
#32108 = VERTEX_POINT('',#114175) ;
#32109 = VERTEX_POINT('',#114176) ;
#32110 = VERTEX_POINT('',#114178) ;
#32111 = VERTEX_POINT('',#114182) ;
#32112 = VERTEX_POINT('',#114183) ;
#32113 = VERTEX_POINT('',#114185) ;
#32114 = VERTEX_POINT('',#114187) ;
#32115 = VERTEX_POINT('',#114189) ;
#32116 = VERTEX_POINT('',#114191) ;
#32117 = VERTEX_POINT('',#114193) ;
#32118 = VERTEX_POINT('',#114204) ;
#32119 = VERTEX_POINT('',#114206) ;
#32120 = VERTEX_POINT('',#114208) ;
#32121 = VERTEX_POINT('',#114212) ;
#32122 = VERTEX_POINT('',#114213) ;
#32123 = VERTEX_POINT('',#114215) ;
#32124 = VERTEX_POINT('',#114217) ;
#32125 = VERTEX_POINT('',#114221) ;
#32126 = VERTEX_POINT('',#114222) ;
#32127 = VERTEX_POINT('',#114224) ;
#32128 = VERTEX_POINT('',#114226) ;
#32129 = VERTEX_POINT('',#114230) ;
#32130 = VERTEX_POINT('',#114231) ;
#32131 = VERTEX_POINT('',#114233) ;
#32132 = VERTEX_POINT('',#114235) ;
#32133 = VERTEX_POINT('',#114239) ;
#32134 = VERTEX_POINT('',#114240) ;
#32135 = VERTEX_POINT('',#114242) ;
#32136 = VERTEX_POINT('',#114244) ;
#32137 = VERTEX_POINT('',#114248) ;
#32138 = VERTEX_POINT('',#114249) ;
#32139 = VERTEX_POINT('',#114251) ;
#32140 = VERTEX_POINT('',#114253) ;
#32141 = VERTEX_POINT('',#114257) ;
#32142 = VERTEX_POINT('',#114258) ;
#32143 = VERTEX_POINT('',#114260) ;
#32144 = VERTEX_POINT('',#114262) ;
#32145 = VERTEX_POINT('',#114266) ;
#32146 = VERTEX_POINT('',#114267) ;
#32147 = VERTEX_POINT('',#114269) ;
#32148 = VERTEX_POINT('',#114271) ;
#32149 = VERTEX_POINT('',#114275) ;
#32150 = VERTEX_POINT('',#114276) ;
#32151 = VERTEX_POINT('',#114278) ;
#32152 = VERTEX_POINT('',#114280) ;
#32153 = VERTEX_POINT('',#114284) ;
#32154 = VERTEX_POINT('',#114285) ;
#32155 = VERTEX_POINT('',#114287) ;
#32156 = VERTEX_POINT('',#114289) ;
#32157 = VERTEX_POINT('',#114293) ;
#32158 = VERTEX_POINT('',#114295) ;
#32159 = VERTEX_POINT('',#114299) ;
#32160 = VERTEX_POINT('',#114300) ;
#32161 = VERTEX_POINT('',#114302) ;
#32162 = VERTEX_POINT('',#114306) ;
#32163 = VERTEX_POINT('',#114307) ;
#32164 = VERTEX_POINT('',#114309) ;
#32165 = VERTEX_POINT('',#114311) ;
#32166 = VERTEX_POINT('',#114313) ;
#32167 = VERTEX_POINT('',#114315) ;
#32168 = VERTEX_POINT('',#114317) ;
#32169 = VERTEX_POINT('',#114346) ;
#32170 = VERTEX_POINT('',#114347) ;
#32171 = VERTEX_POINT('',#114352) ;
#32172 = VERTEX_POINT('',#114353) ;
#32173 = VERTEX_POINT('',#114358) ;
#32174 = VERTEX_POINT('',#114359) ;
#32175 = VERTEX_POINT('',#114364) ;
#32176 = VERTEX_POINT('',#114365) ;
#32177 = VERTEX_POINT('',#114370) ;
#32178 = VERTEX_POINT('',#114371) ;
#32179 = VERTEX_POINT('',#114376) ;
#32180 = VERTEX_POINT('',#114377) ;
#32181 = VERTEX_POINT('',#114382) ;
#32182 = VERTEX_POINT('',#114383) ;
#32183 = VERTEX_POINT('',#114388) ;
#32184 = VERTEX_POINT('',#114389) ;
#32185 = VERTEX_POINT('',#114394) ;
#32186 = VERTEX_POINT('',#114395) ;
#32187 = VERTEX_POINT('',#114400) ;
#32188 = VERTEX_POINT('',#114402) ;
#32189 = VERTEX_POINT('',#114404) ;
#32190 = VERTEX_POINT('',#114408) ;
#32191 = VERTEX_POINT('',#114409) ;
#32192 = VERTEX_POINT('',#114411) ;
#32193 = VERTEX_POINT('',#114413) ;
#32194 = VERTEX_POINT('',#114417) ;
#32195 = VERTEX_POINT('',#114419) ;
#32196 = VERTEX_POINT('',#114423) ;
#32197 = VERTEX_POINT('',#114424) ;
#32198 = VERTEX_POINT('',#114426) ;
#32199 = VERTEX_POINT('',#114430) ;
#32200 = VERTEX_POINT('',#114431) ;
#32201 = VERTEX_POINT('',#114433) ;
#32202 = VERTEX_POINT('',#114435) ;
#32203 = VERTEX_POINT('',#114437) ;
#32204 = VERTEX_POINT('',#114439) ;
#32205 = VERTEX_POINT('',#114441) ;
#32206 = VERTEX_POINT('',#114454) ;
#32207 = VERTEX_POINT('',#114455) ;
#32208 = VERTEX_POINT('',#114460) ;
#32209 = VERTEX_POINT('',#114461) ;
#32210 = VERTEX_POINT('',#114463) ;
#32211 = VERTEX_POINT('',#114465) ;
#32212 = VERTEX_POINT('',#114468) ;
#32213 = VERTEX_POINT('',#114470) ;
#32214 = VERTEX_POINT('',#114472) ;
#32215 = VERTEX_POINT('',#114474) ;
#32216 = VERTEX_POINT('',#114476) ;
#32217 = VERTEX_POINT('',#114478) ;
#32218 = VERTEX_POINT('',#114482) ;
#32219 = VERTEX_POINT('',#114483) ;
#32220 = VERTEX_POINT('',#114485) ;
#32221 = VERTEX_POINT('',#114487) ;
#32222 = VERTEX_POINT('',#114490) ;
#32223 = VERTEX_POINT('',#114492) ;
#32224 = VERTEX_POINT('',#114494) ;
#32225 = VERTEX_POINT('',#114496) ;
#32226 = VERTEX_POINT('',#114498) ;
#32227 = VERTEX_POINT('',#114500) ;
#32228 = VERTEX_POINT('',#114504) ;
#32229 = VERTEX_POINT('',#114505) ;
#32230 = VERTEX_POINT('',#114507) ;
#32231 = VERTEX_POINT('',#114509) ;
#32232 = VERTEX_POINT('',#114512) ;
#32233 = VERTEX_POINT('',#114514) ;
#32234 = VERTEX_POINT('',#114516) ;
#32235 = VERTEX_POINT('',#114518) ;
#32236 = VERTEX_POINT('',#114520) ;
#32237 = VERTEX_POINT('',#114522) ;
#32238 = VERTEX_POINT('',#114526) ;
#32239 = VERTEX_POINT('',#114527) ;
#32240 = VERTEX_POINT('',#114529) ;
#32241 = VERTEX_POINT('',#114531) ;
#32242 = VERTEX_POINT('',#114534) ;
#32243 = VERTEX_POINT('',#114536) ;
#32244 = VERTEX_POINT('',#114538) ;
#32245 = VERTEX_POINT('',#114540) ;
#32246 = VERTEX_POINT('',#114542) ;
#32247 = VERTEX_POINT('',#114544) ;
#32248 = VERTEX_POINT('',#114548) ;
#32249 = VERTEX_POINT('',#114549) ;
#32250 = VERTEX_POINT('',#114551) ;
#32251 = VERTEX_POINT('',#114553) ;
#32252 = VERTEX_POINT('',#114556) ;
#32253 = VERTEX_POINT('',#114558) ;
#32254 = VERTEX_POINT('',#114560) ;
#32255 = VERTEX_POINT('',#114562) ;
#32256 = VERTEX_POINT('',#114564) ;
#32257 = VERTEX_POINT('',#114566) ;
#32258 = VERTEX_POINT('',#114570) ;
#32259 = VERTEX_POINT('',#114571) ;
#32260 = VERTEX_POINT('',#114573) ;
#32261 = VERTEX_POINT('',#114575) ;
#32262 = VERTEX_POINT('',#114578) ;
#32263 = VERTEX_POINT('',#114580) ;
#32264 = VERTEX_POINT('',#114582) ;
#32265 = VERTEX_POINT('',#114584) ;
#32266 = VERTEX_POINT('',#114586) ;
#32267 = VERTEX_POINT('',#114588) ;
#32268 = VERTEX_POINT('',#114592) ;
#32269 = VERTEX_POINT('',#114593) ;
#32270 = VERTEX_POINT('',#114595) ;
#32271 = VERTEX_POINT('',#114597) ;
#32272 = VERTEX_POINT('',#114600) ;
#32273 = VERTEX_POINT('',#114602) ;
#32274 = VERTEX_POINT('',#114604) ;
#32275 = VERTEX_POINT('',#114606) ;
#32276 = VERTEX_POINT('',#114608) ;
#32277 = VERTEX_POINT('',#114610) ;
#32278 = VERTEX_POINT('',#114614) ;
#32279 = VERTEX_POINT('',#114615) ;
#32280 = VERTEX_POINT('',#114617) ;
#32281 = VERTEX_POINT('',#114619) ;
#32282 = VERTEX_POINT('',#114622) ;
#32283 = VERTEX_POINT('',#114624) ;
#32284 = VERTEX_POINT('',#114626) ;
#32285 = VERTEX_POINT('',#114628) ;
#32286 = VERTEX_POINT('',#114630) ;
#32287 = VERTEX_POINT('',#114632) ;
#32288 = VERTEX_POINT('',#114636) ;
#32289 = VERTEX_POINT('',#114637) ;
#32290 = VERTEX_POINT('',#114639) ;
#32291 = VERTEX_POINT('',#114641) ;
#32292 = VERTEX_POINT('',#114644) ;
#32293 = VERTEX_POINT('',#114646) ;
#32294 = VERTEX_POINT('',#114648) ;
#32295 = VERTEX_POINT('',#114650) ;
#32296 = VERTEX_POINT('',#114652) ;
#32297 = VERTEX_POINT('',#114654) ;
#32298 = VERTEX_POINT('',#114658) ;
#32299 = VERTEX_POINT('',#114659) ;
#32300 = VERTEX_POINT('',#114661) ;
#32301 = VERTEX_POINT('',#114663) ;
#32302 = VERTEX_POINT('',#114665) ;
#32303 = VERTEX_POINT('',#114669) ;
#32304 = VERTEX_POINT('',#114670) ;
#32305 = VERTEX_POINT('',#114672) ;
#32306 = VERTEX_POINT('',#114674) ;
#32307 = VERTEX_POINT('',#114676) ;
#32308 = VERTEX_POINT('',#114680) ;
#32309 = VERTEX_POINT('',#114681) ;
#32310 = VERTEX_POINT('',#114683) ;
#32311 = VERTEX_POINT('',#114685) ;
#32312 = VERTEX_POINT('',#114687) ;
#32313 = VERTEX_POINT('',#114691) ;
#32314 = VERTEX_POINT('',#114692) ;
#32315 = VERTEX_POINT('',#114694) ;
#32316 = VERTEX_POINT('',#114696) ;
#32317 = VERTEX_POINT('',#114698) ;
#32318 = VERTEX_POINT('',#114702) ;
#32319 = VERTEX_POINT('',#114703) ;
#32320 = VERTEX_POINT('',#114705) ;
#32321 = VERTEX_POINT('',#114707) ;
#32322 = VERTEX_POINT('',#114709) ;
#32323 = VERTEX_POINT('',#114713) ;
#32324 = VERTEX_POINT('',#114714) ;
#32325 = VERTEX_POINT('',#114716) ;
#32326 = VERTEX_POINT('',#114718) ;
#32327 = VERTEX_POINT('',#114720) ;
#32328 = VERTEX_POINT('',#114724) ;
#32329 = VERTEX_POINT('',#114725) ;
#32330 = VERTEX_POINT('',#114727) ;
#32331 = VERTEX_POINT('',#114729) ;
#32332 = VERTEX_POINT('',#114731) ;
#32333 = VERTEX_POINT('',#114735) ;
#32334 = VERTEX_POINT('',#114736) ;
#32335 = VERTEX_POINT('',#114738) ;
#32336 = VERTEX_POINT('',#114740) ;
#32337 = VERTEX_POINT('',#114742) ;
#32338 = VERTEX_POINT('',#114746) ;
#32339 = VERTEX_POINT('',#114747) ;
#32340 = VERTEX_POINT('',#114749) ;
#32341 = VERTEX_POINT('',#114751) ;
#32342 = VERTEX_POINT('',#114753) ;
#32343 = VERTEX_POINT('',#114757) ;
#32344 = VERTEX_POINT('',#114758) ;
#32345 = VERTEX_POINT('',#114760) ;
#32346 = VERTEX_POINT('',#114762) ;
#32347 = VERTEX_POINT('',#114764) ;
#32348 = VERTEX_POINT('',#114768) ;
#32349 = VERTEX_POINT('',#114769) ;
#32350 = VERTEX_POINT('',#114771) ;
#32351 = VERTEX_POINT('',#114773) ;
#32352 = VERTEX_POINT('',#114775) ;
#32353 = VERTEX_POINT('',#114779) ;
#32354 = VERTEX_POINT('',#114780) ;
#32355 = VERTEX_POINT('',#114782) ;
#32356 = VERTEX_POINT('',#114784) ;
#32357 = VERTEX_POINT('',#114786) ;
#32358 = VERTEX_POINT('',#114790) ;
#32359 = VERTEX_POINT('',#114791) ;
#32360 = VERTEX_POINT('',#114793) ;
#32361 = VERTEX_POINT('',#114795) ;
#32362 = VERTEX_POINT('',#114797) ;
#32363 = VERTEX_POINT('',#114801) ;
#32364 = VERTEX_POINT('',#114802) ;
#32365 = VERTEX_POINT('',#114804) ;
#32366 = VERTEX_POINT('',#114806) ;
#32367 = VERTEX_POINT('',#114808) ;
#32368 = VERTEX_POINT('',#114812) ;
#32369 = VERTEX_POINT('',#114813) ;
#32370 = VERTEX_POINT('',#114815) ;
#32371 = VERTEX_POINT('',#114817) ;
#32372 = VERTEX_POINT('',#114819) ;
#32373 = VERTEX_POINT('',#114823) ;
#32374 = VERTEX_POINT('',#114824) ;
#32375 = VERTEX_POINT('',#114826) ;
#32376 = VERTEX_POINT('',#114828) ;
#32377 = VERTEX_POINT('',#114830) ;
#32378 = VERTEX_POINT('',#114834) ;
#32379 = VERTEX_POINT('',#114835) ;
#32380 = VERTEX_POINT('',#114837) ;
#32381 = VERTEX_POINT('',#114839) ;
#32382 = VERTEX_POINT('',#114841) ;
#32383 = VERTEX_POINT('',#114845) ;
#32384 = VERTEX_POINT('',#114846) ;
#32385 = VERTEX_POINT('',#114848) ;
#32386 = VERTEX_POINT('',#114850) ;
#32387 = VERTEX_POINT('',#114852) ;
#32388 = VERTEX_POINT('',#114856) ;
#32389 = VERTEX_POINT('',#114857) ;
#32390 = VERTEX_POINT('',#114859) ;
#32391 = VERTEX_POINT('',#114861) ;
#32392 = VERTEX_POINT('',#114865) ;
#32393 = VERTEX_POINT('',#114866) ;
#32394 = VERTEX_POINT('',#114868) ;
#32395 = VERTEX_POINT('',#114870) ;
#32396 = VERTEX_POINT('',#114874) ;
#32397 = VERTEX_POINT('',#114875) ;
#32398 = VERTEX_POINT('',#114877) ;
#32399 = VERTEX_POINT('',#114879) ;
#32400 = VERTEX_POINT('',#114883) ;
#32401 = VERTEX_POINT('',#114884) ;
#32402 = VERTEX_POINT('',#114886) ;
#32403 = VERTEX_POINT('',#114888) ;
#32404 = VERTEX_POINT('',#114892) ;
#32405 = VERTEX_POINT('',#114893) ;
#32406 = VERTEX_POINT('',#114895) ;
#32407 = VERTEX_POINT('',#114897) ;
#32408 = VERTEX_POINT('',#114901) ;
#32409 = VERTEX_POINT('',#114902) ;
#32410 = VERTEX_POINT('',#114904) ;
#32411 = VERTEX_POINT('',#114906) ;
#32412 = VERTEX_POINT('',#114910) ;
#32413 = VERTEX_POINT('',#114911) ;
#32414 = VERTEX_POINT('',#114913) ;
#32415 = VERTEX_POINT('',#114915) ;
#32416 = VERTEX_POINT('',#114919) ;
#32417 = VERTEX_POINT('',#114920) ;
#32418 = VERTEX_POINT('',#114922) ;
#32419 = VERTEX_POINT('',#114924) ;
#32420 = VERTEX_POINT('',#114928) ;
#32421 = VERTEX_POINT('',#114929) ;
#32422 = VERTEX_POINT('',#114931) ;
#32423 = VERTEX_POINT('',#114933) ;
#32424 = VERTEX_POINT('',#114937) ;
#32425 = VERTEX_POINT('',#114938) ;
#32426 = VERTEX_POINT('',#114940) ;
#32427 = VERTEX_POINT('',#114942) ;
#32428 = VERTEX_POINT('',#114945) ;
#32429 = VERTEX_POINT('',#114947) ;
#32430 = VERTEX_POINT('',#114949) ;
#32431 = VERTEX_POINT('',#114951) ;
#32432 = VERTEX_POINT('',#114953) ;
#32433 = VERTEX_POINT('',#114955) ;
#32434 = VERTEX_POINT('',#114959) ;
#32435 = VERTEX_POINT('',#114960) ;
#32436 = VERTEX_POINT('',#114962) ;
#32437 = VERTEX_POINT('',#114964) ;
#32438 = VERTEX_POINT('',#114966) ;
#32439 = VERTEX_POINT('',#114970) ;
#32440 = VERTEX_POINT('',#114971) ;
#32441 = VERTEX_POINT('',#114973) ;
#32442 = VERTEX_POINT('',#114975) ;
#32443 = VERTEX_POINT('',#114977) ;
#32444 = VERTEX_POINT('',#114981) ;
#32445 = VERTEX_POINT('',#114982) ;
#32446 = VERTEX_POINT('',#114984) ;
#32447 = VERTEX_POINT('',#114986) ;
#32448 = VERTEX_POINT('',#114990) ;
#32449 = VERTEX_POINT('',#114991) ;
#32450 = VERTEX_POINT('',#114993) ;
#32451 = VERTEX_POINT('',#114995) ;
#32452 = VERTEX_POINT('',#114999) ;
#32453 = VERTEX_POINT('',#115000) ;
#32454 = VERTEX_POINT('',#115002) ;
#32455 = VERTEX_POINT('',#115004) ;
#32456 = VERTEX_POINT('',#115008) ;
#32457 = VERTEX_POINT('',#115010) ;
#32458 = VERTEX_POINT('',#115012) ;
#32459 = VERTEX_POINT('',#115014) ;
#32460 = VERTEX_POINT('',#115017) ;
#32461 = VERTEX_POINT('',#115019) ;
#32462 = VERTEX_POINT('',#115021) ;
#32463 = VERTEX_POINT('',#115023) ;
#32464 = VERTEX_POINT('',#115026) ;
#32465 = VERTEX_POINT('',#115028) ;
#32466 = VERTEX_POINT('',#115030) ;
#32467 = VERTEX_POINT('',#115032) ;
#32468 = VERTEX_POINT('',#115035) ;
#32469 = VERTEX_POINT('',#115037) ;
#32470 = VERTEX_POINT('',#115039) ;
#32471 = VERTEX_POINT('',#115041) ;
#32472 = VERTEX_POINT('',#115044) ;
#32473 = VERTEX_POINT('',#115046) ;
#32474 = VERTEX_POINT('',#115048) ;
#32475 = VERTEX_POINT('',#115050) ;
#32476 = VERTEX_POINT('',#115053) ;
#32477 = VERTEX_POINT('',#115055) ;
#32478 = VERTEX_POINT('',#115057) ;
#32479 = VERTEX_POINT('',#115059) ;
#32480 = VERTEX_POINT('',#115062) ;
#32481 = VERTEX_POINT('',#115064) ;
#32482 = VERTEX_POINT('',#115066) ;
#32483 = VERTEX_POINT('',#115068) ;
#32484 = VERTEX_POINT('',#115071) ;
#32485 = VERTEX_POINT('',#115073) ;
#32486 = VERTEX_POINT('',#115075) ;
#32487 = VERTEX_POINT('',#115077) ;
#32488 = VERTEX_POINT('',#115080) ;
#32489 = VERTEX_POINT('',#115082) ;
#32490 = VERTEX_POINT('',#115084) ;
#32491 = VERTEX_POINT('',#115086) ;
#32492 = VERTEX_POINT('',#115089) ;
#32493 = VERTEX_POINT('',#115091) ;
#32494 = VERTEX_POINT('',#115095) ;
#32495 = VERTEX_POINT('',#115097) ;
#32496 = VERTEX_POINT('',#115101) ;
#32497 = VERTEX_POINT('',#115102) ;
#32498 = VERTEX_POINT('',#115105) ;
#32499 = VERTEX_POINT('',#115107) ;
#32500 = VERTEX_POINT('',#115109) ;
#32501 = VERTEX_POINT('',#115111) ;
#32502 = VERTEX_POINT('',#115114) ;
#32503 = VERTEX_POINT('',#115116) ;
#32504 = VERTEX_POINT('',#115118) ;
#32505 = VERTEX_POINT('',#115120) ;
#32506 = VERTEX_POINT('',#115123) ;
#32507 = VERTEX_POINT('',#115125) ;
#32508 = VERTEX_POINT('',#115127) ;
#32509 = VERTEX_POINT('',#115129) ;
#32510 = VERTEX_POINT('',#115132) ;
#32511 = VERTEX_POINT('',#115134) ;
#32512 = VERTEX_POINT('',#115136) ;
#32513 = VERTEX_POINT('',#115138) ;
#32514 = VERTEX_POINT('',#115141) ;
#32515 = VERTEX_POINT('',#115143) ;
#32516 = VERTEX_POINT('',#115145) ;
#32517 = VERTEX_POINT('',#115147) ;
#32518 = VERTEX_POINT('',#115150) ;
#32519 = VERTEX_POINT('',#115152) ;
#32520 = VERTEX_POINT('',#115154) ;
#32521 = VERTEX_POINT('',#115156) ;
#32522 = VERTEX_POINT('',#115159) ;
#32523 = VERTEX_POINT('',#115161) ;
#32524 = VERTEX_POINT('',#115163) ;
#32525 = VERTEX_POINT('',#115165) ;
#32526 = VERTEX_POINT('',#115168) ;
#32527 = VERTEX_POINT('',#115170) ;
#32528 = VERTEX_POINT('',#115172) ;
#32529 = VERTEX_POINT('',#115174) ;
#32530 = VERTEX_POINT('',#115177) ;
#32531 = VERTEX_POINT('',#115179) ;
#32532 = VERTEX_POINT('',#115181) ;
#32533 = VERTEX_POINT('',#115183) ;
#32534 = VERTEX_POINT('',#115186) ;
#32535 = VERTEX_POINT('',#115188) ;
#32536 = VERTEX_POINT('',#115191) ;
#32537 = VERTEX_POINT('',#115193) ;
#32538 = VERTEX_POINT('',#115197) ;
#32539 = VERTEX_POINT('',#115198) ;
#32540 = VERTEX_POINT('',#115203) ;
#32541 = VERTEX_POINT('',#115204) ;
#32542 = VERTEX_POINT('',#115209) ;
#32543 = VERTEX_POINT('',#115210) ;
#32544 = VERTEX_POINT('',#115215) ;
#32545 = VERTEX_POINT('',#115216) ;
#32546 = VERTEX_POINT('',#115221) ;
#32547 = VERTEX_POINT('',#115222) ;
#32548 = VERTEX_POINT('',#115227) ;
#32549 = VERTEX_POINT('',#115228) ;
#32550 = VERTEX_POINT('',#115233) ;
#32551 = VERTEX_POINT('',#115234) ;
#32552 = VERTEX_POINT('',#115239) ;
#32553 = VERTEX_POINT('',#115240) ;
#32554 = VERTEX_POINT('',#115245) ;
#32555 = VERTEX_POINT('',#115246) ;
#32556 = VERTEX_POINT('',#115251) ;
#32557 = VERTEX_POINT('',#115252) ;
#32558 = VERTEX_POINT('',#115257) ;
#32559 = VERTEX_POINT('',#115258) ;
#32560 = VERTEX_POINT('',#115265) ;
#32561 = VERTEX_POINT('',#115266) ;
#32562 = VERTEX_POINT('',#115268) ;
#32563 = VERTEX_POINT('',#115270) ;
#32564 = VERTEX_POINT('',#115272) ;
#32565 = VERTEX_POINT('',#115274) ;
#32566 = VERTEX_POINT('',#115276) ;
#32567 = VERTEX_POINT('',#115278) ;
#32568 = VERTEX_POINT('',#115281) ;
#32569 = VERTEX_POINT('',#115283) ;
#32570 = VERTEX_POINT('',#115285) ;
#32571 = VERTEX_POINT('',#115287) ;
#32572 = VERTEX_POINT('',#115289) ;
#32573 = VERTEX_POINT('',#115291) ;
#32574 = VERTEX_POINT('',#115293) ;
#32575 = VERTEX_POINT('',#115295) ;
#32576 = VERTEX_POINT('',#115297) ;
#32577 = VERTEX_POINT('',#115299) ;
#32578 = VERTEX_POINT('',#115301) ;
#32579 = VERTEX_POINT('',#115303) ;
#32580 = VERTEX_POINT('',#115305) ;
#32581 = VERTEX_POINT('',#115307) ;
#32582 = VERTEX_POINT('',#115310) ;
#32583 = VERTEX_POINT('',#115311) ;
#32584 = VERTEX_POINT('',#115313) ;
#32585 = VERTEX_POINT('',#115315) ;
#32586 = VERTEX_POINT('',#115317) ;
#32587 = VERTEX_POINT('',#115319) ;
#32588 = VERTEX_POINT('',#115321) ;
#32589 = VERTEX_POINT('',#115323) ;
#32590 = VERTEX_POINT('',#115326) ;
#32591 = VERTEX_POINT('',#115328) ;
#32592 = VERTEX_POINT('',#115330) ;
#32593 = VERTEX_POINT('',#115332) ;
#32594 = VERTEX_POINT('',#115334) ;
#32595 = VERTEX_POINT('',#115336) ;
#32596 = VERTEX_POINT('',#115338) ;
#32597 = VERTEX_POINT('',#115340) ;
#32598 = VERTEX_POINT('',#115342) ;
#32599 = VERTEX_POINT('',#115344) ;
#32600 = VERTEX_POINT('',#115346) ;
#32601 = VERTEX_POINT('',#115348) ;
#32602 = VERTEX_POINT('',#115350) ;
#32603 = VERTEX_POINT('',#115352) ;
#32604 = VERTEX_POINT('',#115355) ;
#32605 = VERTEX_POINT('',#115356) ;
#32606 = VERTEX_POINT('',#115358) ;
#32607 = VERTEX_POINT('',#115360) ;
#32608 = VERTEX_POINT('',#115362) ;
#32609 = VERTEX_POINT('',#115364) ;
#32610 = VERTEX_POINT('',#115366) ;
#32611 = VERTEX_POINT('',#115368) ;
#32612 = VERTEX_POINT('',#115371) ;
#32613 = VERTEX_POINT('',#115373) ;
#32614 = VERTEX_POINT('',#115375) ;
#32615 = VERTEX_POINT('',#115377) ;
#32616 = VERTEX_POINT('',#115379) ;
#32617 = VERTEX_POINT('',#115381) ;
#32618 = VERTEX_POINT('',#115383) ;
#32619 = VERTEX_POINT('',#115385) ;
#32620 = VERTEX_POINT('',#115387) ;
#32621 = VERTEX_POINT('',#115389) ;
#32622 = VERTEX_POINT('',#115391) ;
#32623 = VERTEX_POINT('',#115393) ;
#32624 = VERTEX_POINT('',#115395) ;
#32625 = VERTEX_POINT('',#115397) ;
#32626 = VERTEX_POINT('',#115400) ;
#32627 = VERTEX_POINT('',#115401) ;
#32628 = VERTEX_POINT('',#115403) ;
#32629 = VERTEX_POINT('',#115405) ;
#32630 = VERTEX_POINT('',#115407) ;
#32631 = VERTEX_POINT('',#115409) ;
#32632 = VERTEX_POINT('',#115411) ;
#32633 = VERTEX_POINT('',#115413) ;
#32634 = VERTEX_POINT('',#115416) ;
#32635 = VERTEX_POINT('',#115418) ;
#32636 = VERTEX_POINT('',#115420) ;
#32637 = VERTEX_POINT('',#115422) ;
#32638 = VERTEX_POINT('',#115424) ;
#32639 = VERTEX_POINT('',#115426) ;
#32640 = VERTEX_POINT('',#115428) ;
#32641 = VERTEX_POINT('',#115430) ;
#32642 = VERTEX_POINT('',#115432) ;
#32643 = VERTEX_POINT('',#115434) ;
#32644 = VERTEX_POINT('',#115436) ;
#32645 = VERTEX_POINT('',#115438) ;
#32646 = VERTEX_POINT('',#115440) ;
#32647 = VERTEX_POINT('',#115442) ;
#32648 = VERTEX_POINT('',#115445) ;
#32649 = VERTEX_POINT('',#115446) ;
#32650 = VERTEX_POINT('',#115448) ;
#32651 = VERTEX_POINT('',#115450) ;
#32652 = VERTEX_POINT('',#115452) ;
#32653 = VERTEX_POINT('',#115454) ;
#32654 = VERTEX_POINT('',#115456) ;
#32655 = VERTEX_POINT('',#115458) ;
#32656 = VERTEX_POINT('',#115461) ;
#32657 = VERTEX_POINT('',#115463) ;
#32658 = VERTEX_POINT('',#115465) ;
#32659 = VERTEX_POINT('',#115467) ;
#32660 = VERTEX_POINT('',#115469) ;
#32661 = VERTEX_POINT('',#115471) ;
#32662 = VERTEX_POINT('',#115473) ;
#32663 = VERTEX_POINT('',#115475) ;
#32664 = VERTEX_POINT('',#115477) ;
#32665 = VERTEX_POINT('',#115479) ;
#32666 = VERTEX_POINT('',#115481) ;
#32667 = VERTEX_POINT('',#115483) ;
#32668 = VERTEX_POINT('',#115485) ;
#32669 = VERTEX_POINT('',#115487) ;
#32670 = VERTEX_POINT('',#115490) ;
#32671 = VERTEX_POINT('',#115491) ;
#32672 = VERTEX_POINT('',#115493) ;
#32673 = VERTEX_POINT('',#115495) ;
#32674 = VERTEX_POINT('',#115497) ;
#32675 = VERTEX_POINT('',#115499) ;
#32676 = VERTEX_POINT('',#115501) ;
#32677 = VERTEX_POINT('',#115503) ;
#32678 = VERTEX_POINT('',#115506) ;
#32679 = VERTEX_POINT('',#115508) ;
#32680 = VERTEX_POINT('',#115510) ;
#32681 = VERTEX_POINT('',#115512) ;
#32682 = VERTEX_POINT('',#115514) ;
#32683 = VERTEX_POINT('',#115516) ;
#32684 = VERTEX_POINT('',#115518) ;
#32685 = VERTEX_POINT('',#115520) ;
#32686 = VERTEX_POINT('',#115522) ;
#32687 = VERTEX_POINT('',#115524) ;
#32688 = VERTEX_POINT('',#115526) ;
#32689 = VERTEX_POINT('',#115528) ;
#32690 = VERTEX_POINT('',#115530) ;
#32691 = VERTEX_POINT('',#115532) ;
#32692 = VERTEX_POINT('',#115535) ;
#32693 = VERTEX_POINT('',#115536) ;
#32694 = VERTEX_POINT('',#115538) ;
#32695 = VERTEX_POINT('',#115540) ;
#32696 = VERTEX_POINT('',#115542) ;
#32697 = VERTEX_POINT('',#115544) ;
#32698 = VERTEX_POINT('',#115546) ;
#32699 = VERTEX_POINT('',#115548) ;
#32700 = VERTEX_POINT('',#115551) ;
#32701 = VERTEX_POINT('',#115553) ;
#32702 = VERTEX_POINT('',#115555) ;
#32703 = VERTEX_POINT('',#115557) ;
#32704 = VERTEX_POINT('',#115559) ;
#32705 = VERTEX_POINT('',#115561) ;
#32706 = VERTEX_POINT('',#115563) ;
#32707 = VERTEX_POINT('',#115565) ;
#32708 = VERTEX_POINT('',#115567) ;
#32709 = VERTEX_POINT('',#115569) ;
#32710 = VERTEX_POINT('',#115571) ;
#32711 = VERTEX_POINT('',#115573) ;
#32712 = VERTEX_POINT('',#115575) ;
#32713 = VERTEX_POINT('',#115577) ;
#32714 = VERTEX_POINT('',#115580) ;
#32715 = VERTEX_POINT('',#115581) ;
#32716 = VERTEX_POINT('',#115583) ;
#32717 = VERTEX_POINT('',#115585) ;
#32718 = VERTEX_POINT('',#115587) ;
#32719 = VERTEX_POINT('',#115589) ;
#32720 = VERTEX_POINT('',#115591) ;
#32721 = VERTEX_POINT('',#115593) ;
#32722 = VERTEX_POINT('',#115596) ;
#32723 = VERTEX_POINT('',#115598) ;
#32724 = VERTEX_POINT('',#115600) ;
#32725 = VERTEX_POINT('',#115602) ;
#32726 = VERTEX_POINT('',#115604) ;
#32727 = VERTEX_POINT('',#115606) ;
#32728 = VERTEX_POINT('',#115608) ;
#32729 = VERTEX_POINT('',#115610) ;
#32730 = VERTEX_POINT('',#115612) ;
#32731 = VERTEX_POINT('',#115614) ;
#32732 = VERTEX_POINT('',#115616) ;
#32733 = VERTEX_POINT('',#115618) ;
#32734 = VERTEX_POINT('',#115620) ;
#32735 = VERTEX_POINT('',#115622) ;
#32736 = VERTEX_POINT('',#115625) ;
#32737 = VERTEX_POINT('',#115626) ;
#32738 = VERTEX_POINT('',#115628) ;
#32739 = VERTEX_POINT('',#115630) ;
#32740 = VERTEX_POINT('',#115632) ;
#32741 = VERTEX_POINT('',#115634) ;
#32742 = VERTEX_POINT('',#115636) ;
#32743 = VERTEX_POINT('',#115638) ;
#32744 = VERTEX_POINT('',#115641) ;
#32745 = VERTEX_POINT('',#115643) ;
#32746 = VERTEX_POINT('',#115645) ;
#32747 = VERTEX_POINT('',#115647) ;
#32748 = VERTEX_POINT('',#115649) ;
#32749 = VERTEX_POINT('',#115651) ;
#32750 = VERTEX_POINT('',#115653) ;
#32751 = VERTEX_POINT('',#115655) ;
#32752 = VERTEX_POINT('',#115657) ;
#32753 = VERTEX_POINT('',#115659) ;
#32754 = VERTEX_POINT('',#115661) ;
#32755 = VERTEX_POINT('',#115663) ;
#32756 = VERTEX_POINT('',#115665) ;
#32757 = VERTEX_POINT('',#115667) ;
#32758 = VERTEX_POINT('',#115670) ;
#32759 = VERTEX_POINT('',#115671) ;
#32760 = VERTEX_POINT('',#115673) ;
#32761 = VERTEX_POINT('',#115675) ;
#32762 = VERTEX_POINT('',#115677) ;
#32763 = VERTEX_POINT('',#115679) ;
#32764 = VERTEX_POINT('',#115681) ;
#32765 = VERTEX_POINT('',#115683) ;
#32766 = VERTEX_POINT('',#115686) ;
#32767 = VERTEX_POINT('',#115688) ;
#32768 = VERTEX_POINT('',#115690) ;
#32769 = VERTEX_POINT('',#115692) ;
#32770 = VERTEX_POINT('',#115694) ;
#32771 = VERTEX_POINT('',#115696) ;
#32772 = VERTEX_POINT('',#115698) ;
#32773 = VERTEX_POINT('',#115700) ;
#32774 = VERTEX_POINT('',#115702) ;
#32775 = VERTEX_POINT('',#115704) ;
#32776 = VERTEX_POINT('',#115706) ;
#32777 = VERTEX_POINT('',#115708) ;
#32778 = VERTEX_POINT('',#115710) ;
#32779 = VERTEX_POINT('',#115712) ;
#32780 = VERTEX_POINT('',#115716) ;
#32781 = VERTEX_POINT('',#115717) ;
#32782 = VERTEX_POINT('',#115719) ;
#32783 = VERTEX_POINT('',#115721) ;
#32784 = VERTEX_POINT('',#115723) ;
#32785 = VERTEX_POINT('',#115725) ;
#32786 = VERTEX_POINT('',#115727) ;
#32787 = VERTEX_POINT('',#115729) ;
#32788 = VERTEX_POINT('',#115731) ;
#32789 = VERTEX_POINT('',#115733) ;
#32790 = VERTEX_POINT('',#115737) ;
#32791 = VERTEX_POINT('',#115738) ;
#32792 = VERTEX_POINT('',#115740) ;
#32793 = VERTEX_POINT('',#115742) ;
#32794 = VERTEX_POINT('',#115744) ;
#32795 = VERTEX_POINT('',#115746) ;
#32796 = VERTEX_POINT('',#115748) ;
#32797 = VERTEX_POINT('',#115750) ;
#32798 = VERTEX_POINT('',#115752) ;
#32799 = VERTEX_POINT('',#115754) ;
#32800 = VERTEX_POINT('',#115758) ;
#32801 = VERTEX_POINT('',#115759) ;
#32802 = VERTEX_POINT('',#115761) ;
#32803 = VERTEX_POINT('',#115763) ;
#32804 = VERTEX_POINT('',#115765) ;
#32805 = VERTEX_POINT('',#115767) ;
#32806 = VERTEX_POINT('',#115769) ;
#32807 = VERTEX_POINT('',#115771) ;
#32808 = VERTEX_POINT('',#115773) ;
#32809 = VERTEX_POINT('',#115775) ;
#32810 = VERTEX_POINT('',#115779) ;
#32811 = VERTEX_POINT('',#115780) ;
#32812 = VERTEX_POINT('',#115782) ;
#32813 = VERTEX_POINT('',#115784) ;
#32814 = VERTEX_POINT('',#115788) ;
#32815 = VERTEX_POINT('',#115790) ;
#32816 = VERTEX_POINT('',#115794) ;
#32817 = VERTEX_POINT('',#115795) ;
#32818 = VERTEX_POINT('',#115797) ;
#32819 = VERTEX_POINT('',#115799) ;
#32820 = VERTEX_POINT('',#115803) ;
#32821 = VERTEX_POINT('',#115804) ;
#32822 = VERTEX_POINT('',#115806) ;
#32823 = VERTEX_POINT('',#115808) ;
#32824 = VERTEX_POINT('',#115812) ;
#32825 = VERTEX_POINT('',#115813) ;
#32826 = VERTEX_POINT('',#115815) ;
#32827 = VERTEX_POINT('',#115817) ;
#32828 = VERTEX_POINT('',#115821) ;
#32829 = VERTEX_POINT('',#115822) ;
#32830 = VERTEX_POINT('',#115824) ;
#32831 = VERTEX_POINT('',#115826) ;
#32832 = VERTEX_POINT('',#115830) ;
#32833 = VERTEX_POINT('',#115832) ;
#32834 = VERTEX_POINT('',#115836) ;
#32835 = VERTEX_POINT('',#115838) ;
#32836 = VERTEX_POINT('',#115842) ;
#32837 = VERTEX_POINT('',#115844) ;
#32838 = VERTEX_POINT('',#115848) ;
#32839 = VERTEX_POINT('',#115850) ;
#32840 = VERTEX_POINT('',#115855) ;
#32841 = VERTEX_POINT('',#115859) ;
#32842 = VERTEX_POINT('',#115866) ;
#32843 = VERTEX_POINT('',#115868) ;
#32844 = VERTEX_POINT('',#115872) ;
#32845 = VERTEX_POINT('',#115874) ;
#32846 = VERTEX_POINT('',#115878) ;
#32847 = VERTEX_POINT('',#115880) ;
#32848 = VERTEX_POINT('',#115884) ;
#32849 = VERTEX_POINT('',#115886) ;
#32850 = VERTEX_POINT('',#115890) ;
#32851 = VERTEX_POINT('',#115892) ;
#32852 = VERTEX_POINT('',#115896) ;
#32853 = VERTEX_POINT('',#115898) ;
#32854 = VERTEX_POINT('',#115902) ;
#32855 = VERTEX_POINT('',#115904) ;
#32856 = VERTEX_POINT('',#115908) ;
#32857 = VERTEX_POINT('',#115910) ;
#32858 = VERTEX_POINT('',#115914) ;
#32859 = VERTEX_POINT('',#115916) ;
#32860 = VERTEX_POINT('',#115920) ;
#32861 = VERTEX_POINT('',#115922) ;
#32862 = VERTEX_POINT('',#115926) ;
#32863 = VERTEX_POINT('',#115928) ;
#32864 = VERTEX_POINT('',#115932) ;
#32865 = VERTEX_POINT('',#115934) ;
#32866 = VERTEX_POINT('',#115938) ;
#32867 = VERTEX_POINT('',#115940) ;
#32868 = VERTEX_POINT('',#115944) ;
#32869 = VERTEX_POINT('',#115946) ;
#32870 = VERTEX_POINT('',#115950) ;
#32871 = VERTEX_POINT('',#115952) ;
#32872 = VERTEX_POINT('',#115956) ;
#32873 = VERTEX_POINT('',#115958) ;
#32874 = VERTEX_POINT('',#115962) ;
#32875 = VERTEX_POINT('',#115964) ;
#32876 = VERTEX_POINT('',#115968) ;
#32877 = VERTEX_POINT('',#115970) ;
#32878 = VERTEX_POINT('',#115977) ;
#32879 = VERTEX_POINT('',#115978) ;
#32880 = VERTEX_POINT('',#115980) ;
#32881 = VERTEX_POINT('',#115982) ;
#32882 = VERTEX_POINT('',#115984) ;
#32883 = VERTEX_POINT('',#115986) ;
#32884 = VERTEX_POINT('',#115988) ;
#32885 = VERTEX_POINT('',#115990) ;
#32886 = VERTEX_POINT('',#115992) ;
#32887 = VERTEX_POINT('',#115994) ;
#32888 = VERTEX_POINT('',#115996) ;
#32889 = VERTEX_POINT('',#115998) ;
#32890 = VERTEX_POINT('',#116000) ;
#32891 = VERTEX_POINT('',#116002) ;
#32892 = VERTEX_POINT('',#116004) ;
#32893 = VERTEX_POINT('',#116006) ;
#32894 = VERTEX_POINT('',#116009) ;
#32895 = VERTEX_POINT('',#116013) ;
#32896 = VERTEX_POINT('',#116014) ;
#32897 = VERTEX_POINT('',#116016) ;
#32898 = VERTEX_POINT('',#116018) ;
#32899 = VERTEX_POINT('',#116020) ;
#32900 = VERTEX_POINT('',#116022) ;
#32901 = VERTEX_POINT('',#116024) ;
#32902 = VERTEX_POINT('',#116026) ;
#32903 = VERTEX_POINT('',#116036) ;
#32904 = VERTEX_POINT('',#116046) ;
#32905 = VERTEX_POINT('',#116057) ;
#32906 = VERTEX_POINT('',#116089) ;
#32907 = VERTEX_POINT('',#116136) ;
#32908 = VERTEX_POINT('',#116154) ;
#32909 = VERTEX_POINT('',#116168) ;
#32910 = VERTEX_POINT('',#116183) ;
#32911 = VERTEX_POINT('',#116374) ;
#32912 = VERTEX_POINT('',#116375) ;
#32913 = VERTEX_POINT('',#116377) ;
#32914 = VERTEX_POINT('',#116379) ;
#32915 = VERTEX_POINT('',#116383) ;
#32916 = VERTEX_POINT('',#116384) ;
#32917 = VERTEX_POINT('',#116386) ;
#32918 = VERTEX_POINT('',#116388) ;
#32919 = VERTEX_POINT('',#116392) ;
#32920 = VERTEX_POINT('',#116393) ;
#32921 = VERTEX_POINT('',#116395) ;
#32922 = VERTEX_POINT('',#116397) ;
#32923 = VERTEX_POINT('',#116401) ;
#32924 = VERTEX_POINT('',#116402) ;
#32925 = VERTEX_POINT('',#116404) ;
#32926 = VERTEX_POINT('',#116406) ;
#32927 = VERTEX_POINT('',#116410) ;
#32928 = VERTEX_POINT('',#116411) ;
#32929 = VERTEX_POINT('',#116413) ;
#32930 = VERTEX_POINT('',#116415) ;
#32931 = VERTEX_POINT('',#116419) ;
#32932 = VERTEX_POINT('',#116420) ;
#32933 = VERTEX_POINT('',#116423) ;
#32934 = VERTEX_POINT('',#116425) ;
#32935 = VERTEX_POINT('',#116429) ;
#32936 = VERTEX_POINT('',#116430) ;
#32937 = VERTEX_POINT('',#116433) ;
#32938 = VERTEX_POINT('',#116435) ;
#32939 = VERTEX_POINT('',#116445) ;
#32940 = VERTEX_POINT('',#116446) ;
#32941 = VERTEX_POINT('',#116448) ;
#32942 = VERTEX_POINT('',#116450) ;
#32943 = VERTEX_POINT('',#116454) ;
#32944 = VERTEX_POINT('',#116455) ;
#32945 = VERTEX_POINT('',#116460) ;
#32946 = VERTEX_POINT('',#116462) ;
#32947 = VERTEX_POINT('',#116466) ;
#32948 = VERTEX_POINT('',#116467) ;
#32949 = VERTEX_POINT('',#116469) ;
#32950 = VERTEX_POINT('',#116471) ;
#32951 = VERTEX_POINT('',#116475) ;
#32952 = VERTEX_POINT('',#116476) ;
#32953 = VERTEX_POINT('',#116478) ;
#32954 = VERTEX_POINT('',#116480) ;
#32955 = VERTEX_POINT('',#116484) ;
#32956 = VERTEX_POINT('',#116485) ;
#32957 = VERTEX_POINT('',#116490) ;
#32958 = VERTEX_POINT('',#116492) ;
#32959 = VERTEX_POINT('',#116496) ;
#32960 = VERTEX_POINT('',#116497) ;
#32961 = VERTEX_POINT('',#116499) ;
#32962 = VERTEX_POINT('',#116501) ;
#32963 = VERTEX_POINT('',#116505) ;
#32964 = VERTEX_POINT('',#116506) ;
#32965 = VERTEX_POINT('',#116508) ;
#32966 = VERTEX_POINT('',#116510) ;
#32967 = VERTEX_POINT('',#116514) ;
#32968 = VERTEX_POINT('',#116515) ;
#32969 = VERTEX_POINT('',#116517) ;
#32970 = VERTEX_POINT('',#116519) ;
#32971 = VERTEX_POINT('',#116523) ;
#32972 = VERTEX_POINT('',#116524) ;
#32973 = VERTEX_POINT('',#116526) ;
#32974 = VERTEX_POINT('',#116528) ;
#32975 = VERTEX_POINT('',#116644) ;
#32976 = VERTEX_POINT('',#116645) ;
#32977 = VERTEX_POINT('',#116647) ;
#32978 = VERTEX_POINT('',#116649) ;
#32979 = VERTEX_POINT('',#116651) ;
#32980 = VERTEX_POINT('',#116653) ;
#32981 = VERTEX_POINT('',#116655) ;
#32982 = VERTEX_POINT('',#116657) ;
#32983 = VERTEX_POINT('',#116659) ;
#32984 = VERTEX_POINT('',#116661) ;
#32985 = VERTEX_POINT('',#116665) ;
#32986 = VERTEX_POINT('',#116666) ;
#32987 = VERTEX_POINT('',#116668) ;
#32988 = VERTEX_POINT('',#116670) ;
#32989 = VERTEX_POINT('',#116672) ;
#32990 = VERTEX_POINT('',#116674) ;
#32991 = VERTEX_POINT('',#116676) ;
#32992 = VERTEX_POINT('',#116678) ;
#32993 = VERTEX_POINT('',#116680) ;
#32994 = VERTEX_POINT('',#116682) ;
#32995 = VERTEX_POINT('',#116686) ;
#32996 = VERTEX_POINT('',#116687) ;
#32997 = VERTEX_POINT('',#116689) ;
#32998 = VERTEX_POINT('',#116691) ;
#32999 = VERTEX_POINT('',#116693) ;
#33000 = VERTEX_POINT('',#116695) ;
#33001 = VERTEX_POINT('',#116697) ;
#33002 = VERTEX_POINT('',#116699) ;
#33003 = VERTEX_POINT('',#116701) ;
#33004 = VERTEX_POINT('',#116703) ;
#33005 = VERTEX_POINT('',#116707) ;
#33006 = VERTEX_POINT('',#116708) ;
#33007 = VERTEX_POINT('',#116710) ;
#33008 = VERTEX_POINT('',#116712) ;
#33009 = VERTEX_POINT('',#116714) ;
#33010 = VERTEX_POINT('',#116716) ;
#33011 = VERTEX_POINT('',#116718) ;
#33012 = VERTEX_POINT('',#116720) ;
#33013 = VERTEX_POINT('',#116722) ;
#33014 = VERTEX_POINT('',#116724) ;
#33015 = VERTEX_POINT('',#116728) ;
#33016 = VERTEX_POINT('',#116729) ;
#33017 = VERTEX_POINT('',#116731) ;
#33018 = VERTEX_POINT('',#116733) ;
#33019 = VERTEX_POINT('',#116735) ;
#33020 = VERTEX_POINT('',#116737) ;
#33021 = VERTEX_POINT('',#116739) ;
#33022 = VERTEX_POINT('',#116741) ;
#33023 = VERTEX_POINT('',#116743) ;
#33024 = VERTEX_POINT('',#116745) ;
#33025 = VERTEX_POINT('',#116749) ;
#33026 = VERTEX_POINT('',#116750) ;
#33027 = VERTEX_POINT('',#116752) ;
#33028 = VERTEX_POINT('',#116754) ;
#33029 = VERTEX_POINT('',#116756) ;
#33030 = VERTEX_POINT('',#116758) ;
#33031 = VERTEX_POINT('',#116760) ;
#33032 = VERTEX_POINT('',#116762) ;
#33033 = VERTEX_POINT('',#116764) ;
#33034 = VERTEX_POINT('',#116766) ;
#33035 = VERTEX_POINT('',#116770) ;
#33036 = VERTEX_POINT('',#116771) ;
#33037 = VERTEX_POINT('',#116773) ;
#33038 = VERTEX_POINT('',#116775) ;
#33039 = VERTEX_POINT('',#116777) ;
#33040 = VERTEX_POINT('',#116779) ;
#33041 = VERTEX_POINT('',#116781) ;
#33042 = VERTEX_POINT('',#116783) ;
#33043 = VERTEX_POINT('',#116785) ;
#33044 = VERTEX_POINT('',#116787) ;
#33045 = VERTEX_POINT('',#116791) ;
#33046 = VERTEX_POINT('',#116792) ;
#33047 = VERTEX_POINT('',#116794) ;
#33048 = VERTEX_POINT('',#116796) ;
#33049 = VERTEX_POINT('',#116798) ;
#33050 = VERTEX_POINT('',#116800) ;
#33051 = VERTEX_POINT('',#116802) ;
#33052 = VERTEX_POINT('',#116804) ;
#33053 = VERTEX_POINT('',#116806) ;
#33054 = VERTEX_POINT('',#116808) ;
#33055 = VERTEX_POINT('',#116812) ;
#33056 = VERTEX_POINT('',#116813) ;
#33057 = VERTEX_POINT('',#116815) ;
#33058 = VERTEX_POINT('',#116817) ;
#33059 = VERTEX_POINT('',#116819) ;
#33060 = VERTEX_POINT('',#116821) ;
#33061 = VERTEX_POINT('',#116823) ;
#33062 = VERTEX_POINT('',#116825) ;
#33063 = VERTEX_POINT('',#116827) ;
#33064 = VERTEX_POINT('',#116829) ;
#33065 = VERTEX_POINT('',#116833) ;
#33066 = VERTEX_POINT('',#116834) ;
#33067 = VERTEX_POINT('',#116836) ;
#33068 = VERTEX_POINT('',#116838) ;
#33069 = VERTEX_POINT('',#116842) ;
#33070 = VERTEX_POINT('',#116844) ;
#33071 = VERTEX_POINT('',#116848) ;
#33072 = VERTEX_POINT('',#116849) ;
#33073 = VERTEX_POINT('',#116851) ;
#33074 = VERTEX_POINT('',#116853) ;
#33075 = VERTEX_POINT('',#116857) ;
#33076 = VERTEX_POINT('',#116858) ;
#33077 = VERTEX_POINT('',#116860) ;
#33078 = VERTEX_POINT('',#116862) ;
#33079 = VERTEX_POINT('',#116866) ;
#33080 = VERTEX_POINT('',#116867) ;
#33081 = VERTEX_POINT('',#116869) ;
#33082 = VERTEX_POINT('',#116871) ;
#33083 = VERTEX_POINT('',#116875) ;
#33084 = VERTEX_POINT('',#116876) ;
#33085 = VERTEX_POINT('',#116878) ;
#33086 = VERTEX_POINT('',#116880) ;
#33087 = VERTEX_POINT('',#116884) ;
#33088 = VERTEX_POINT('',#116886) ;
#33089 = VERTEX_POINT('',#116890) ;
#33090 = VERTEX_POINT('',#116891) ;
#33091 = VERTEX_POINT('',#116893) ;
#33092 = VERTEX_POINT('',#116895) ;
#33093 = VERTEX_POINT('',#116899) ;
#33094 = VERTEX_POINT('',#116900) ;
#33095 = VERTEX_POINT('',#116902) ;
#33096 = VERTEX_POINT('',#116904) ;
#33097 = VERTEX_POINT('',#116908) ;
#33098 = VERTEX_POINT('',#116909) ;
#33099 = VERTEX_POINT('',#116911) ;
#33100 = VERTEX_POINT('',#116913) ;
#33101 = VERTEX_POINT('',#116917) ;
#33102 = VERTEX_POINT('',#116918) ;
#33103 = VERTEX_POINT('',#116920) ;
#33104 = VERTEX_POINT('',#116922) ;
#33105 = VERTEX_POINT('',#116926) ;
#33106 = VERTEX_POINT('',#116928) ;
#33107 = VERTEX_POINT('',#116932) ;
#33108 = VERTEX_POINT('',#116933) ;
#33109 = VERTEX_POINT('',#116935) ;
#33110 = VERTEX_POINT('',#116937) ;
#33111 = VERTEX_POINT('',#116941) ;
#33112 = VERTEX_POINT('',#116942) ;
#33113 = VERTEX_POINT('',#116944) ;
#33114 = VERTEX_POINT('',#116946) ;
#33115 = VERTEX_POINT('',#116950) ;
#33116 = VERTEX_POINT('',#116951) ;
#33117 = VERTEX_POINT('',#116953) ;
#33118 = VERTEX_POINT('',#116955) ;
#33119 = VERTEX_POINT('',#116959) ;
#33120 = VERTEX_POINT('',#116960) ;
#33121 = VERTEX_POINT('',#116962) ;
#33122 = VERTEX_POINT('',#116964) ;
#33123 = VERTEX_POINT('',#116968) ;
#33124 = VERTEX_POINT('',#116970) ;
#33125 = VERTEX_POINT('',#116974) ;
#33126 = VERTEX_POINT('',#116975) ;
#33127 = VERTEX_POINT('',#116977) ;
#33128 = VERTEX_POINT('',#116979) ;
#33129 = VERTEX_POINT('',#116983) ;
#33130 = VERTEX_POINT('',#116984) ;
#33131 = VERTEX_POINT('',#116986) ;
#33132 = VERTEX_POINT('',#116988) ;
#33133 = VERTEX_POINT('',#116992) ;
#33134 = VERTEX_POINT('',#116993) ;
#33135 = VERTEX_POINT('',#116995) ;
#33136 = VERTEX_POINT('',#116997) ;
#33137 = VERTEX_POINT('',#117001) ;
#33138 = VERTEX_POINT('',#117002) ;
#33139 = VERTEX_POINT('',#117004) ;
#33140 = VERTEX_POINT('',#117006) ;
#33141 = VERTEX_POINT('',#117010) ;
#33142 = VERTEX_POINT('',#117012) ;
#33143 = VERTEX_POINT('',#117016) ;
#33144 = VERTEX_POINT('',#117017) ;
#33145 = VERTEX_POINT('',#117019) ;
#33146 = VERTEX_POINT('',#117021) ;
#33147 = VERTEX_POINT('',#117025) ;
#33148 = VERTEX_POINT('',#117026) ;
#33149 = VERTEX_POINT('',#117028) ;
#33150 = VERTEX_POINT('',#117030) ;
#33151 = VERTEX_POINT('',#117034) ;
#33152 = VERTEX_POINT('',#117035) ;
#33153 = VERTEX_POINT('',#117037) ;
#33154 = VERTEX_POINT('',#117039) ;
#33155 = VERTEX_POINT('',#117043) ;
#33156 = VERTEX_POINT('',#117044) ;
#33157 = VERTEX_POINT('',#117046) ;
#33158 = VERTEX_POINT('',#117048) ;
#33159 = VERTEX_POINT('',#117052) ;
#33160 = VERTEX_POINT('',#117054) ;
#33161 = VERTEX_POINT('',#117058) ;
#33162 = VERTEX_POINT('',#117059) ;
#33163 = VERTEX_POINT('',#117061) ;
#33164 = VERTEX_POINT('',#117063) ;
#33165 = VERTEX_POINT('',#117067) ;
#33166 = VERTEX_POINT('',#117068) ;
#33167 = VERTEX_POINT('',#117070) ;
#33168 = VERTEX_POINT('',#117072) ;
#33169 = VERTEX_POINT('',#117076) ;
#33170 = VERTEX_POINT('',#117077) ;
#33171 = VERTEX_POINT('',#117079) ;
#33172 = VERTEX_POINT('',#117081) ;
#33173 = VERTEX_POINT('',#117085) ;
#33174 = VERTEX_POINT('',#117086) ;
#33175 = VERTEX_POINT('',#117088) ;
#33176 = VERTEX_POINT('',#117090) ;
#33177 = VERTEX_POINT('',#117094) ;
#33178 = VERTEX_POINT('',#117096) ;
#33179 = VERTEX_POINT('',#117100) ;
#33180 = VERTEX_POINT('',#117101) ;
#33181 = VERTEX_POINT('',#117103) ;
#33182 = VERTEX_POINT('',#117105) ;
#33183 = VERTEX_POINT('',#117109) ;
#33184 = VERTEX_POINT('',#117110) ;
#33185 = VERTEX_POINT('',#117112) ;
#33186 = VERTEX_POINT('',#117114) ;
#33187 = VERTEX_POINT('',#117118) ;
#33188 = VERTEX_POINT('',#117119) ;
#33189 = VERTEX_POINT('',#117121) ;
#33190 = VERTEX_POINT('',#117123) ;
#33191 = VERTEX_POINT('',#117127) ;
#33192 = VERTEX_POINT('',#117128) ;
#33193 = VERTEX_POINT('',#117130) ;
#33194 = VERTEX_POINT('',#117132) ;
#33195 = VERTEX_POINT('',#117136) ;
#33196 = VERTEX_POINT('',#117138) ;
#33197 = VERTEX_POINT('',#117142) ;
#33198 = VERTEX_POINT('',#117143) ;
#33199 = VERTEX_POINT('',#117145) ;
#33200 = VERTEX_POINT('',#117147) ;
#33201 = VERTEX_POINT('',#117151) ;
#33202 = VERTEX_POINT('',#117152) ;
#33203 = VERTEX_POINT('',#117154) ;
#33204 = VERTEX_POINT('',#117156) ;
#33205 = VERTEX_POINT('',#117160) ;
#33206 = VERTEX_POINT('',#117161) ;
#33207 = VERTEX_POINT('',#117163) ;
#33208 = VERTEX_POINT('',#117165) ;
#33209 = VERTEX_POINT('',#117169) ;
#33210 = VERTEX_POINT('',#117170) ;
#33211 = VERTEX_POINT('',#117172) ;
#33212 = VERTEX_POINT('',#117174) ;
#33213 = VERTEX_POINT('',#117178) ;
#33214 = VERTEX_POINT('',#117180) ;
#33215 = VERTEX_POINT('',#117184) ;
#33216 = VERTEX_POINT('',#117185) ;
#33217 = VERTEX_POINT('',#117187) ;
#33218 = VERTEX_POINT('',#117189) ;
#33219 = VERTEX_POINT('',#117193) ;
#33220 = VERTEX_POINT('',#117194) ;
#33221 = VERTEX_POINT('',#117196) ;
#33222 = VERTEX_POINT('',#117198) ;
#33223 = VERTEX_POINT('',#117202) ;
#33224 = VERTEX_POINT('',#117203) ;
#33225 = VERTEX_POINT('',#117205) ;
#33226 = VERTEX_POINT('',#117207) ;
#33227 = VERTEX_POINT('',#117211) ;
#33228 = VERTEX_POINT('',#117212) ;
#33229 = VERTEX_POINT('',#117214) ;
#33230 = VERTEX_POINT('',#117216) ;
#33231 = VERTEX_POINT('',#117220) ;
#33232 = VERTEX_POINT('',#117222) ;
#33233 = VERTEX_POINT('',#117226) ;
#33234 = VERTEX_POINT('',#117228) ;
#33235 = VERTEX_POINT('',#117232) ;
#33236 = VERTEX_POINT('',#117234) ;
#33237 = VERTEX_POINT('',#117238) ;
#33238 = VERTEX_POINT('',#117240) ;
#33239 = VERTEX_POINT('',#117245) ;
#33240 = VERTEX_POINT('',#117249) ;
#33241 = VERTEX_POINT('',#117256) ;
#33242 = VERTEX_POINT('',#117258) ;
#33243 = VERTEX_POINT('',#117262) ;
#33244 = VERTEX_POINT('',#117264) ;
#33245 = VERTEX_POINT('',#117268) ;
#33246 = VERTEX_POINT('',#117270) ;
#33247 = VERTEX_POINT('',#117274) ;
#33248 = VERTEX_POINT('',#117276) ;
#33249 = VERTEX_POINT('',#117280) ;
#33250 = VERTEX_POINT('',#117282) ;
#33251 = VERTEX_POINT('',#117286) ;
#33252 = VERTEX_POINT('',#117288) ;
#33253 = VERTEX_POINT('',#117292) ;
#33254 = VERTEX_POINT('',#117294) ;
#33255 = VERTEX_POINT('',#117298) ;
#33256 = VERTEX_POINT('',#117300) ;
#33257 = VERTEX_POINT('',#117304) ;
#33258 = VERTEX_POINT('',#117306) ;
#33259 = VERTEX_POINT('',#117310) ;
#33260 = VERTEX_POINT('',#117312) ;
#33261 = VERTEX_POINT('',#117316) ;
#33262 = VERTEX_POINT('',#117318) ;
#33263 = VERTEX_POINT('',#117322) ;
#33264 = VERTEX_POINT('',#117324) ;
#33265 = VERTEX_POINT('',#117328) ;
#33266 = VERTEX_POINT('',#117330) ;
#33267 = VERTEX_POINT('',#117334) ;
#33268 = VERTEX_POINT('',#117336) ;
#33269 = VERTEX_POINT('',#117340) ;
#33270 = VERTEX_POINT('',#117342) ;
#33271 = VERTEX_POINT('',#117346) ;
#33272 = VERTEX_POINT('',#117348) ;
#33273 = VERTEX_POINT('',#117352) ;
#33274 = VERTEX_POINT('',#117354) ;
#33275 = VERTEX_POINT('',#117358) ;
#33276 = VERTEX_POINT('',#117360) ;
#33277 = VERTEX_POINT('',#117367) ;
#33278 = VERTEX_POINT('',#117368) ;
#33279 = VERTEX_POINT('',#117370) ;
#33280 = VERTEX_POINT('',#117372) ;
#33281 = VERTEX_POINT('',#117374) ;
#33282 = VERTEX_POINT('',#117376) ;
#33283 = VERTEX_POINT('',#117378) ;
#33284 = VERTEX_POINT('',#117380) ;
#33285 = VERTEX_POINT('',#117382) ;
#33286 = VERTEX_POINT('',#117384) ;
#33287 = VERTEX_POINT('',#117386) ;
#33288 = VERTEX_POINT('',#117388) ;
#33289 = VERTEX_POINT('',#117390) ;
#33290 = VERTEX_POINT('',#117392) ;
#33291 = VERTEX_POINT('',#117394) ;
#33292 = VERTEX_POINT('',#117396) ;
#33293 = VERTEX_POINT('',#117399) ;
#33294 = VERTEX_POINT('',#117403) ;
#33295 = VERTEX_POINT('',#117404) ;
#33296 = VERTEX_POINT('',#117406) ;
#33297 = VERTEX_POINT('',#117408) ;
#33298 = VERTEX_POINT('',#117412) ;
#33299 = VERTEX_POINT('',#117414) ;
#33300 = VERTEX_POINT('',#117418) ;
#33301 = VERTEX_POINT('',#117420) ;
#33302 = VERTEX_POINT('',#117424) ;
#33303 = VERTEX_POINT('',#117426) ;
#33304 = VERTEX_POINT('',#117430) ;
#33305 = VERTEX_POINT('',#117432) ;
#33306 = VERTEX_POINT('',#117437) ;
#33307 = VERTEX_POINT('',#117441) ;
#33308 = VERTEX_POINT('',#117448) ;
#33309 = VERTEX_POINT('',#117450) ;
#33310 = VERTEX_POINT('',#117454) ;
#33311 = VERTEX_POINT('',#117456) ;
#33312 = VERTEX_POINT('',#117460) ;
#33313 = VERTEX_POINT('',#117462) ;
#33314 = VERTEX_POINT('',#117466) ;
#33315 = VERTEX_POINT('',#117468) ;
#33316 = VERTEX_POINT('',#117472) ;
#33317 = VERTEX_POINT('',#117474) ;
#33318 = VERTEX_POINT('',#117478) ;
#33319 = VERTEX_POINT('',#117480) ;
#33320 = VERTEX_POINT('',#117484) ;
#33321 = VERTEX_POINT('',#117486) ;
#33322 = VERTEX_POINT('',#117490) ;
#33323 = VERTEX_POINT('',#117492) ;
#33324 = VERTEX_POINT('',#117496) ;
#33325 = VERTEX_POINT('',#117498) ;
#33326 = VERTEX_POINT('',#117502) ;
#33327 = VERTEX_POINT('',#117504) ;
#33328 = VERTEX_POINT('',#117508) ;
#33329 = VERTEX_POINT('',#117510) ;
#33330 = VERTEX_POINT('',#117514) ;
#33331 = VERTEX_POINT('',#117516) ;
#33332 = VERTEX_POINT('',#117520) ;
#33333 = VERTEX_POINT('',#117522) ;
#33334 = VERTEX_POINT('',#117526) ;
#33335 = VERTEX_POINT('',#117528) ;
#33336 = VERTEX_POINT('',#117532) ;
#33337 = VERTEX_POINT('',#117534) ;
#33338 = VERTEX_POINT('',#117538) ;
#33339 = VERTEX_POINT('',#117540) ;
#33340 = VERTEX_POINT('',#117544) ;
#33341 = VERTEX_POINT('',#117546) ;
#33342 = VERTEX_POINT('',#117550) ;
#33343 = VERTEX_POINT('',#117552) ;
#33344 = VERTEX_POINT('',#117559) ;
#33345 = VERTEX_POINT('',#117560) ;
#33346 = VERTEX_POINT('',#117562) ;
#33347 = VERTEX_POINT('',#117564) ;
#33348 = VERTEX_POINT('',#117566) ;
#33349 = VERTEX_POINT('',#117568) ;
#33350 = VERTEX_POINT('',#117570) ;
#33351 = VERTEX_POINT('',#117572) ;
#33352 = VERTEX_POINT('',#117574) ;
#33353 = VERTEX_POINT('',#117576) ;
#33354 = VERTEX_POINT('',#117578) ;
#33355 = VERTEX_POINT('',#117580) ;
#33356 = VERTEX_POINT('',#117582) ;
#33357 = VERTEX_POINT('',#117584) ;
#33358 = VERTEX_POINT('',#117586) ;
#33359 = VERTEX_POINT('',#117588) ;
#33360 = VERTEX_POINT('',#117591) ;
#33361 = VERTEX_POINT('',#117595) ;
#33362 = VERTEX_POINT('',#117596) ;
#33363 = VERTEX_POINT('',#117598) ;
#33364 = VERTEX_POINT('',#117600) ;
#33365 = VERTEX_POINT('',#117604) ;
#33366 = VERTEX_POINT('',#117606) ;
#33367 = VERTEX_POINT('',#117610) ;
#33368 = VERTEX_POINT('',#117612) ;
#33369 = VERTEX_POINT('',#117616) ;
#33370 = VERTEX_POINT('',#117618) ;
#33371 = VERTEX_POINT('',#117622) ;
#33372 = VERTEX_POINT('',#117624) ;
#33373 = VERTEX_POINT('',#117629) ;
#33374 = VERTEX_POINT('',#117633) ;
#33375 = VERTEX_POINT('',#117640) ;
#33376 = VERTEX_POINT('',#117642) ;
#33377 = VERTEX_POINT('',#117646) ;
#33378 = VERTEX_POINT('',#117648) ;
#33379 = VERTEX_POINT('',#117652) ;
#33380 = VERTEX_POINT('',#117654) ;
#33381 = VERTEX_POINT('',#117658) ;
#33382 = VERTEX_POINT('',#117660) ;
#33383 = VERTEX_POINT('',#117664) ;
#33384 = VERTEX_POINT('',#117666) ;
#33385 = VERTEX_POINT('',#117670) ;
#33386 = VERTEX_POINT('',#117672) ;
#33387 = VERTEX_POINT('',#117676) ;
#33388 = VERTEX_POINT('',#117678) ;
#33389 = VERTEX_POINT('',#117682) ;
#33390 = VERTEX_POINT('',#117684) ;
#33391 = VERTEX_POINT('',#117688) ;
#33392 = VERTEX_POINT('',#117690) ;
#33393 = VERTEX_POINT('',#117694) ;
#33394 = VERTEX_POINT('',#117696) ;
#33395 = VERTEX_POINT('',#117700) ;
#33396 = VERTEX_POINT('',#117702) ;
#33397 = VERTEX_POINT('',#117706) ;
#33398 = VERTEX_POINT('',#117708) ;
#33399 = VERTEX_POINT('',#117712) ;
#33400 = VERTEX_POINT('',#117714) ;
#33401 = VERTEX_POINT('',#117718) ;
#33402 = VERTEX_POINT('',#117720) ;
#33403 = VERTEX_POINT('',#117724) ;
#33404 = VERTEX_POINT('',#117726) ;
#33405 = VERTEX_POINT('',#117730) ;
#33406 = VERTEX_POINT('',#117732) ;
#33407 = VERTEX_POINT('',#117736) ;
#33408 = VERTEX_POINT('',#117738) ;
#33409 = VERTEX_POINT('',#117742) ;
#33410 = VERTEX_POINT('',#117744) ;
#33411 = VERTEX_POINT('',#117751) ;
#33412 = VERTEX_POINT('',#117752) ;
#33413 = VERTEX_POINT('',#117754) ;
#33414 = VERTEX_POINT('',#117756) ;
#33415 = VERTEX_POINT('',#117758) ;
#33416 = VERTEX_POINT('',#117760) ;
#33417 = VERTEX_POINT('',#117762) ;
#33418 = VERTEX_POINT('',#117764) ;
#33419 = VERTEX_POINT('',#117766) ;
#33420 = VERTEX_POINT('',#117768) ;
#33421 = VERTEX_POINT('',#117770) ;
#33422 = VERTEX_POINT('',#117772) ;
#33423 = VERTEX_POINT('',#117774) ;
#33424 = VERTEX_POINT('',#117776) ;
#33425 = VERTEX_POINT('',#117778) ;
#33426 = VERTEX_POINT('',#117780) ;
#33427 = VERTEX_POINT('',#117783) ;
#33428 = VERTEX_POINT('',#117787) ;
#33429 = VERTEX_POINT('',#117788) ;
#33430 = VERTEX_POINT('',#117790) ;
#33431 = VERTEX_POINT('',#117792) ;
#33432 = VERTEX_POINT('',#117796) ;
#33433 = VERTEX_POINT('',#117798) ;
#33434 = VERTEX_POINT('',#117802) ;
#33435 = VERTEX_POINT('',#117804) ;
#33436 = VERTEX_POINT('',#117808) ;
#33437 = VERTEX_POINT('',#117810) ;
#33438 = VERTEX_POINT('',#117814) ;
#33439 = VERTEX_POINT('',#117816) ;
#33440 = VERTEX_POINT('',#117821) ;
#33441 = VERTEX_POINT('',#117825) ;
#33442 = VERTEX_POINT('',#117832) ;
#33443 = VERTEX_POINT('',#117834) ;
#33444 = VERTEX_POINT('',#117838) ;
#33445 = VERTEX_POINT('',#117840) ;
#33446 = VERTEX_POINT('',#117844) ;
#33447 = VERTEX_POINT('',#117846) ;
#33448 = VERTEX_POINT('',#117850) ;
#33449 = VERTEX_POINT('',#117852) ;
#33450 = VERTEX_POINT('',#117856) ;
#33451 = VERTEX_POINT('',#117858) ;
#33452 = VERTEX_POINT('',#117862) ;
#33453 = VERTEX_POINT('',#117864) ;
#33454 = VERTEX_POINT('',#117868) ;
#33455 = VERTEX_POINT('',#117870) ;
#33456 = VERTEX_POINT('',#117874) ;
#33457 = VERTEX_POINT('',#117876) ;
#33458 = VERTEX_POINT('',#117880) ;
#33459 = VERTEX_POINT('',#117882) ;
#33460 = VERTEX_POINT('',#117886) ;
#33461 = VERTEX_POINT('',#117888) ;
#33462 = VERTEX_POINT('',#117892) ;
#33463 = VERTEX_POINT('',#117894) ;
#33464 = VERTEX_POINT('',#117898) ;
#33465 = VERTEX_POINT('',#117900) ;
#33466 = VERTEX_POINT('',#117904) ;
#33467 = VERTEX_POINT('',#117906) ;
#33468 = VERTEX_POINT('',#117910) ;
#33469 = VERTEX_POINT('',#117912) ;
#33470 = VERTEX_POINT('',#117916) ;
#33471 = VERTEX_POINT('',#117918) ;
#33472 = VERTEX_POINT('',#117922) ;
#33473 = VERTEX_POINT('',#117924) ;
#33474 = VERTEX_POINT('',#117928) ;
#33475 = VERTEX_POINT('',#117930) ;
#33476 = VERTEX_POINT('',#117934) ;
#33477 = VERTEX_POINT('',#117936) ;
#33478 = VERTEX_POINT('',#117943) ;
#33479 = VERTEX_POINT('',#117944) ;
#33480 = VERTEX_POINT('',#117946) ;
#33481 = VERTEX_POINT('',#117948) ;
#33482 = VERTEX_POINT('',#117950) ;
#33483 = VERTEX_POINT('',#117952) ;
#33484 = VERTEX_POINT('',#117954) ;
#33485 = VERTEX_POINT('',#117956) ;
#33486 = VERTEX_POINT('',#117958) ;
#33487 = VERTEX_POINT('',#117960) ;
#33488 = VERTEX_POINT('',#117962) ;
#33489 = VERTEX_POINT('',#117964) ;
#33490 = VERTEX_POINT('',#117966) ;
#33491 = VERTEX_POINT('',#117968) ;
#33492 = VERTEX_POINT('',#117970) ;
#33493 = VERTEX_POINT('',#117972) ;
#33494 = VERTEX_POINT('',#117975) ;
#33495 = VERTEX_POINT('',#117979) ;
#33496 = VERTEX_POINT('',#117980) ;
#33497 = VERTEX_POINT('',#117982) ;
#33498 = VERTEX_POINT('',#117984) ;
#33499 = VERTEX_POINT('',#117988) ;
#33500 = VERTEX_POINT('',#117990) ;
#33501 = VERTEX_POINT('',#117994) ;
#33502 = VERTEX_POINT('',#117996) ;
#33503 = VERTEX_POINT('',#118000) ;
#33504 = VERTEX_POINT('',#118002) ;
#33505 = VERTEX_POINT('',#118006) ;
#33506 = VERTEX_POINT('',#118008) ;
#33507 = VERTEX_POINT('',#118013) ;
#33508 = VERTEX_POINT('',#118017) ;
#33509 = VERTEX_POINT('',#118024) ;
#33510 = VERTEX_POINT('',#118026) ;
#33511 = VERTEX_POINT('',#118030) ;
#33512 = VERTEX_POINT('',#118032) ;
#33513 = VERTEX_POINT('',#118036) ;
#33514 = VERTEX_POINT('',#118038) ;
#33515 = VERTEX_POINT('',#118042) ;
#33516 = VERTEX_POINT('',#118044) ;
#33517 = VERTEX_POINT('',#118048) ;
#33518 = VERTEX_POINT('',#118050) ;
#33519 = VERTEX_POINT('',#118054) ;
#33520 = VERTEX_POINT('',#118056) ;
#33521 = VERTEX_POINT('',#118060) ;
#33522 = VERTEX_POINT('',#118062) ;
#33523 = VERTEX_POINT('',#118066) ;
#33524 = VERTEX_POINT('',#118068) ;
#33525 = VERTEX_POINT('',#118072) ;
#33526 = VERTEX_POINT('',#118074) ;
#33527 = VERTEX_POINT('',#118078) ;
#33528 = VERTEX_POINT('',#118080) ;
#33529 = VERTEX_POINT('',#118084) ;
#33530 = VERTEX_POINT('',#118086) ;
#33531 = VERTEX_POINT('',#118090) ;
#33532 = VERTEX_POINT('',#118092) ;
#33533 = VERTEX_POINT('',#118096) ;
#33534 = VERTEX_POINT('',#118098) ;
#33535 = VERTEX_POINT('',#118102) ;
#33536 = VERTEX_POINT('',#118104) ;
#33537 = VERTEX_POINT('',#118108) ;
#33538 = VERTEX_POINT('',#118110) ;
#33539 = VERTEX_POINT('',#118114) ;
#33540 = VERTEX_POINT('',#118116) ;
#33541 = VERTEX_POINT('',#118120) ;
#33542 = VERTEX_POINT('',#118122) ;
#33543 = VERTEX_POINT('',#118126) ;
#33544 = VERTEX_POINT('',#118128) ;
#33545 = VERTEX_POINT('',#118135) ;
#33546 = VERTEX_POINT('',#118136) ;
#33547 = VERTEX_POINT('',#118138) ;
#33548 = VERTEX_POINT('',#118140) ;
#33549 = VERTEX_POINT('',#118142) ;
#33550 = VERTEX_POINT('',#118144) ;
#33551 = VERTEX_POINT('',#118146) ;
#33552 = VERTEX_POINT('',#118148) ;
#33553 = VERTEX_POINT('',#118150) ;
#33554 = VERTEX_POINT('',#118152) ;
#33555 = VERTEX_POINT('',#118154) ;
#33556 = VERTEX_POINT('',#118156) ;
#33557 = VERTEX_POINT('',#118158) ;
#33558 = VERTEX_POINT('',#118160) ;
#33559 = VERTEX_POINT('',#118162) ;
#33560 = VERTEX_POINT('',#118164) ;
#33561 = VERTEX_POINT('',#118167) ;
#33562 = VERTEX_POINT('',#118171) ;
#33563 = VERTEX_POINT('',#118172) ;
#33564 = VERTEX_POINT('',#118174) ;
#33565 = VERTEX_POINT('',#118176) ;
#33566 = VERTEX_POINT('',#118180) ;
#33567 = VERTEX_POINT('',#118182) ;
#33568 = VERTEX_POINT('',#118186) ;
#33569 = VERTEX_POINT('',#118188) ;
#33570 = VERTEX_POINT('',#118192) ;
#33571 = VERTEX_POINT('',#118194) ;
#33572 = VERTEX_POINT('',#118198) ;
#33573 = VERTEX_POINT('',#118200) ;
#33574 = VERTEX_POINT('',#118205) ;
#33575 = VERTEX_POINT('',#118209) ;
#33576 = VERTEX_POINT('',#118216) ;
#33577 = VERTEX_POINT('',#118218) ;
#33578 = VERTEX_POINT('',#118222) ;
#33579 = VERTEX_POINT('',#118224) ;
#33580 = VERTEX_POINT('',#118228) ;
#33581 = VERTEX_POINT('',#118230) ;
#33582 = VERTEX_POINT('',#118234) ;
#33583 = VERTEX_POINT('',#118236) ;
#33584 = VERTEX_POINT('',#118240) ;
#33585 = VERTEX_POINT('',#118242) ;
#33586 = VERTEX_POINT('',#118246) ;
#33587 = VERTEX_POINT('',#118248) ;
#33588 = VERTEX_POINT('',#118252) ;
#33589 = VERTEX_POINT('',#118254) ;
#33590 = VERTEX_POINT('',#118258) ;
#33591 = VERTEX_POINT('',#118260) ;
#33592 = VERTEX_POINT('',#118264) ;
#33593 = VERTEX_POINT('',#118266) ;
#33594 = VERTEX_POINT('',#118270) ;
#33595 = VERTEX_POINT('',#118272) ;
#33596 = VERTEX_POINT('',#118276) ;
#33597 = VERTEX_POINT('',#118278) ;
#33598 = VERTEX_POINT('',#118282) ;
#33599 = VERTEX_POINT('',#118284) ;
#33600 = VERTEX_POINT('',#118288) ;
#33601 = VERTEX_POINT('',#118290) ;
#33602 = VERTEX_POINT('',#118294) ;
#33603 = VERTEX_POINT('',#118296) ;
#33604 = VERTEX_POINT('',#118300) ;
#33605 = VERTEX_POINT('',#118302) ;
#33606 = VERTEX_POINT('',#118306) ;
#33607 = VERTEX_POINT('',#118308) ;
#33608 = VERTEX_POINT('',#118312) ;
#33609 = VERTEX_POINT('',#118314) ;
#33610 = VERTEX_POINT('',#118318) ;
#33611 = VERTEX_POINT('',#118320) ;
#33612 = VERTEX_POINT('',#118327) ;
#33613 = VERTEX_POINT('',#118328) ;
#33614 = VERTEX_POINT('',#118330) ;
#33615 = VERTEX_POINT('',#118332) ;
#33616 = VERTEX_POINT('',#118334) ;
#33617 = VERTEX_POINT('',#118336) ;
#33618 = VERTEX_POINT('',#118338) ;
#33619 = VERTEX_POINT('',#118340) ;
#33620 = VERTEX_POINT('',#118342) ;
#33621 = VERTEX_POINT('',#118344) ;
#33622 = VERTEX_POINT('',#118346) ;
#33623 = VERTEX_POINT('',#118348) ;
#33624 = VERTEX_POINT('',#118350) ;
#33625 = VERTEX_POINT('',#118352) ;
#33626 = VERTEX_POINT('',#118354) ;
#33627 = VERTEX_POINT('',#118356) ;
#33628 = VERTEX_POINT('',#118359) ;
#33629 = VERTEX_POINT('',#118363) ;
#33630 = VERTEX_POINT('',#118364) ;
#33631 = VERTEX_POINT('',#118366) ;
#33632 = VERTEX_POINT('',#118368) ;
#33633 = VERTEX_POINT('',#118372) ;
#33634 = VERTEX_POINT('',#118374) ;
#33635 = VERTEX_POINT('',#118378) ;
#33636 = VERTEX_POINT('',#118380) ;
#33637 = VERTEX_POINT('',#118384) ;
#33638 = VERTEX_POINT('',#118386) ;
#33639 = VERTEX_POINT('',#118390) ;
#33640 = VERTEX_POINT('',#118392) ;
#33641 = VERTEX_POINT('',#118397) ;
#33642 = VERTEX_POINT('',#118401) ;
#33643 = VERTEX_POINT('',#118408) ;
#33644 = VERTEX_POINT('',#118410) ;
#33645 = VERTEX_POINT('',#118414) ;
#33646 = VERTEX_POINT('',#118416) ;
#33647 = VERTEX_POINT('',#118420) ;
#33648 = VERTEX_POINT('',#118422) ;
#33649 = VERTEX_POINT('',#118426) ;
#33650 = VERTEX_POINT('',#118428) ;
#33651 = VERTEX_POINT('',#118432) ;
#33652 = VERTEX_POINT('',#118434) ;
#33653 = VERTEX_POINT('',#118438) ;
#33654 = VERTEX_POINT('',#118440) ;
#33655 = VERTEX_POINT('',#118444) ;
#33656 = VERTEX_POINT('',#118446) ;
#33657 = VERTEX_POINT('',#118450) ;
#33658 = VERTEX_POINT('',#118452) ;
#33659 = VERTEX_POINT('',#118456) ;
#33660 = VERTEX_POINT('',#118458) ;
#33661 = VERTEX_POINT('',#118462) ;
#33662 = VERTEX_POINT('',#118464) ;
#33663 = VERTEX_POINT('',#118468) ;
#33664 = VERTEX_POINT('',#118470) ;
#33665 = VERTEX_POINT('',#118474) ;
#33666 = VERTEX_POINT('',#118476) ;
#33667 = VERTEX_POINT('',#118480) ;
#33668 = VERTEX_POINT('',#118482) ;
#33669 = VERTEX_POINT('',#118486) ;
#33670 = VERTEX_POINT('',#118488) ;
#33671 = VERTEX_POINT('',#118492) ;
#33672 = VERTEX_POINT('',#118494) ;
#33673 = VERTEX_POINT('',#118498) ;
#33674 = VERTEX_POINT('',#118500) ;
#33675 = VERTEX_POINT('',#118504) ;
#33676 = VERTEX_POINT('',#118506) ;
#33677 = VERTEX_POINT('',#118510) ;
#33678 = VERTEX_POINT('',#118512) ;
#33679 = VERTEX_POINT('',#118519) ;
#33680 = VERTEX_POINT('',#118520) ;
#33681 = VERTEX_POINT('',#118522) ;
#33682 = VERTEX_POINT('',#118524) ;
#33683 = VERTEX_POINT('',#118526) ;
#33684 = VERTEX_POINT('',#118528) ;
#33685 = VERTEX_POINT('',#118530) ;
#33686 = VERTEX_POINT('',#118532) ;
#33687 = VERTEX_POINT('',#118534) ;
#33688 = VERTEX_POINT('',#118536) ;
#33689 = VERTEX_POINT('',#118538) ;
#33690 = VERTEX_POINT('',#118540) ;
#33691 = VERTEX_POINT('',#118542) ;
#33692 = VERTEX_POINT('',#118544) ;
#33693 = VERTEX_POINT('',#118546) ;
#33694 = VERTEX_POINT('',#118548) ;
#33695 = VERTEX_POINT('',#118551) ;
#33696 = VERTEX_POINT('',#118555) ;
#33697 = VERTEX_POINT('',#118556) ;
#33698 = VERTEX_POINT('',#118558) ;
#33699 = VERTEX_POINT('',#118560) ;
#33700 = VERTEX_POINT('',#118564) ;
#33701 = VERTEX_POINT('',#118566) ;
#33702 = VERTEX_POINT('',#118570) ;
#33703 = VERTEX_POINT('',#118572) ;
#33704 = VERTEX_POINT('',#118576) ;
#33705 = VERTEX_POINT('',#118578) ;
#33706 = VERTEX_POINT('',#118582) ;
#33707 = VERTEX_POINT('',#118584) ;
#33708 = VERTEX_POINT('',#118589) ;
#33709 = VERTEX_POINT('',#118593) ;
#33710 = VERTEX_POINT('',#118600) ;
#33711 = VERTEX_POINT('',#118602) ;
#33712 = VERTEX_POINT('',#118606) ;
#33713 = VERTEX_POINT('',#118608) ;
#33714 = VERTEX_POINT('',#118612) ;
#33715 = VERTEX_POINT('',#118614) ;
#33716 = VERTEX_POINT('',#118618) ;
#33717 = VERTEX_POINT('',#118620) ;
#33718 = VERTEX_POINT('',#118624) ;
#33719 = VERTEX_POINT('',#118626) ;
#33720 = VERTEX_POINT('',#118630) ;
#33721 = VERTEX_POINT('',#118632) ;
#33722 = VERTEX_POINT('',#118636) ;
#33723 = VERTEX_POINT('',#118638) ;
#33724 = VERTEX_POINT('',#118642) ;
#33725 = VERTEX_POINT('',#118644) ;
#33726 = VERTEX_POINT('',#118648) ;
#33727 = VERTEX_POINT('',#118650) ;
#33728 = VERTEX_POINT('',#118654) ;
#33729 = VERTEX_POINT('',#118656) ;
#33730 = VERTEX_POINT('',#118660) ;
#33731 = VERTEX_POINT('',#118662) ;
#33732 = VERTEX_POINT('',#118666) ;
#33733 = VERTEX_POINT('',#118668) ;
#33734 = VERTEX_POINT('',#118672) ;
#33735 = VERTEX_POINT('',#118674) ;
#33736 = VERTEX_POINT('',#118678) ;
#33737 = VERTEX_POINT('',#118680) ;
#33738 = VERTEX_POINT('',#118684) ;
#33739 = VERTEX_POINT('',#118686) ;
#33740 = VERTEX_POINT('',#118690) ;
#33741 = VERTEX_POINT('',#118692) ;
#33742 = VERTEX_POINT('',#118696) ;
#33743 = VERTEX_POINT('',#118698) ;
#33744 = VERTEX_POINT('',#118702) ;
#33745 = VERTEX_POINT('',#118704) ;
#33746 = VERTEX_POINT('',#118711) ;
#33747 = VERTEX_POINT('',#118712) ;
#33748 = VERTEX_POINT('',#118714) ;
#33749 = VERTEX_POINT('',#118716) ;
#33750 = VERTEX_POINT('',#118718) ;
#33751 = VERTEX_POINT('',#118720) ;
#33752 = VERTEX_POINT('',#118722) ;
#33753 = VERTEX_POINT('',#118724) ;
#33754 = VERTEX_POINT('',#118726) ;
#33755 = VERTEX_POINT('',#118728) ;
#33756 = VERTEX_POINT('',#118730) ;
#33757 = VERTEX_POINT('',#118732) ;
#33758 = VERTEX_POINT('',#118734) ;
#33759 = VERTEX_POINT('',#118736) ;
#33760 = VERTEX_POINT('',#118738) ;
#33761 = VERTEX_POINT('',#118740) ;
#33762 = VERTEX_POINT('',#118743) ;
#33763 = VERTEX_POINT('',#118747) ;
#33764 = VERTEX_POINT('',#118748) ;
#33765 = VERTEX_POINT('',#118750) ;
#33766 = VERTEX_POINT('',#118752) ;
#33767 = VERTEX_POINT('',#118756) ;
#33768 = VERTEX_POINT('',#118758) ;
#33769 = VERTEX_POINT('',#118762) ;
#33770 = VERTEX_POINT('',#118764) ;
#33771 = VERTEX_POINT('',#118768) ;
#33772 = VERTEX_POINT('',#118770) ;
#33773 = VERTEX_POINT('',#118774) ;
#33774 = VERTEX_POINT('',#118776) ;
#33775 = VERTEX_POINT('',#118781) ;
#33776 = VERTEX_POINT('',#118785) ;
#33777 = VERTEX_POINT('',#118792) ;
#33778 = VERTEX_POINT('',#118794) ;
#33779 = VERTEX_POINT('',#118798) ;
#33780 = VERTEX_POINT('',#118800) ;
#33781 = VERTEX_POINT('',#118804) ;
#33782 = VERTEX_POINT('',#118806) ;
#33783 = VERTEX_POINT('',#118810) ;
#33784 = VERTEX_POINT('',#118812) ;
#33785 = VERTEX_POINT('',#118816) ;
#33786 = VERTEX_POINT('',#118818) ;
#33787 = VERTEX_POINT('',#118822) ;
#33788 = VERTEX_POINT('',#118824) ;
#33789 = VERTEX_POINT('',#118828) ;
#33790 = VERTEX_POINT('',#118830) ;
#33791 = VERTEX_POINT('',#118834) ;
#33792 = VERTEX_POINT('',#118836) ;
#33793 = VERTEX_POINT('',#118840) ;
#33794 = VERTEX_POINT('',#118842) ;
#33795 = VERTEX_POINT('',#118846) ;
#33796 = VERTEX_POINT('',#118848) ;
#33797 = VERTEX_POINT('',#118852) ;
#33798 = VERTEX_POINT('',#118854) ;
#33799 = VERTEX_POINT('',#118858) ;
#33800 = VERTEX_POINT('',#118860) ;
#33801 = VERTEX_POINT('',#118864) ;
#33802 = VERTEX_POINT('',#118866) ;
#33803 = VERTEX_POINT('',#118870) ;
#33804 = VERTEX_POINT('',#118872) ;
#33805 = VERTEX_POINT('',#118876) ;
#33806 = VERTEX_POINT('',#118878) ;
#33807 = VERTEX_POINT('',#118882) ;
#33808 = VERTEX_POINT('',#118884) ;
#33809 = VERTEX_POINT('',#118888) ;
#33810 = VERTEX_POINT('',#118890) ;
#33811 = VERTEX_POINT('',#118894) ;
#33812 = VERTEX_POINT('',#118896) ;
#33813 = VERTEX_POINT('',#118903) ;
#33814 = VERTEX_POINT('',#118904) ;
#33815 = VERTEX_POINT('',#118906) ;
#33816 = VERTEX_POINT('',#118908) ;
#33817 = VERTEX_POINT('',#118910) ;
#33818 = VERTEX_POINT('',#118912) ;
#33819 = VERTEX_POINT('',#118914) ;
#33820 = VERTEX_POINT('',#118916) ;
#33821 = VERTEX_POINT('',#118918) ;
#33822 = VERTEX_POINT('',#118920) ;
#33823 = VERTEX_POINT('',#118922) ;
#33824 = VERTEX_POINT('',#118924) ;
#33825 = VERTEX_POINT('',#118926) ;
#33826 = VERTEX_POINT('',#118928) ;
#33827 = VERTEX_POINT('',#118930) ;
#33828 = VERTEX_POINT('',#118932) ;
#33829 = VERTEX_POINT('',#118935) ;
#33830 = VERTEX_POINT('',#118939) ;
#33831 = VERTEX_POINT('',#118940) ;
#33832 = VERTEX_POINT('',#118942) ;
#33833 = VERTEX_POINT('',#118944) ;
#33834 = VERTEX_POINT('',#118946) ;
#33835 = VERTEX_POINT('',#118948) ;
#33836 = VERTEX_POINT('',#118950) ;
#33837 = VERTEX_POINT('',#118952) ;
#33838 = VERTEX_POINT('',#118956) ;
#33839 = VERTEX_POINT('',#118957) ;
#33840 = VERTEX_POINT('',#118959) ;
#33841 = VERTEX_POINT('',#118961) ;
#33842 = VERTEX_POINT('',#118963) ;
#33843 = VERTEX_POINT('',#118965) ;
#33844 = VERTEX_POINT('',#118967) ;
#33845 = VERTEX_POINT('',#118969) ;
#33846 = VERTEX_POINT('',#118973) ;
#33847 = VERTEX_POINT('',#118974) ;
#33848 = VERTEX_POINT('',#118976) ;
#33849 = VERTEX_POINT('',#118978) ;
#33850 = VERTEX_POINT('',#118980) ;
#33851 = VERTEX_POINT('',#118982) ;
#33852 = VERTEX_POINT('',#118984) ;
#33853 = VERTEX_POINT('',#118986) ;
#33854 = VERTEX_POINT('',#118990) ;
#33855 = VERTEX_POINT('',#118991) ;
#33856 = VERTEX_POINT('',#118993) ;
#33857 = VERTEX_POINT('',#118995) ;
#33858 = VERTEX_POINT('',#118997) ;
#33859 = VERTEX_POINT('',#118999) ;
#33860 = VERTEX_POINT('',#119001) ;
#33861 = VERTEX_POINT('',#119003) ;
#33862 = VERTEX_POINT('',#119007) ;
#33863 = VERTEX_POINT('',#119008) ;
#33864 = VERTEX_POINT('',#119010) ;
#33865 = VERTEX_POINT('',#119012) ;
#33866 = VERTEX_POINT('',#119014) ;
#33867 = VERTEX_POINT('',#119016) ;
#33868 = VERTEX_POINT('',#119018) ;
#33869 = VERTEX_POINT('',#119020) ;
#33870 = VERTEX_POINT('',#119024) ;
#33871 = VERTEX_POINT('',#119025) ;
#33872 = VERTEX_POINT('',#119027) ;
#33873 = VERTEX_POINT('',#119029) ;
#33874 = VERTEX_POINT('',#119031) ;
#33875 = VERTEX_POINT('',#119033) ;
#33876 = VERTEX_POINT('',#119035) ;
#33877 = VERTEX_POINT('',#119037) ;
#33878 = VERTEX_POINT('',#119041) ;
#33879 = VERTEX_POINT('',#119042) ;
#33880 = VERTEX_POINT('',#119044) ;
#33881 = VERTEX_POINT('',#119046) ;
#33882 = VERTEX_POINT('',#119048) ;
#33883 = VERTEX_POINT('',#119050) ;
#33884 = VERTEX_POINT('',#119052) ;
#33885 = VERTEX_POINT('',#119054) ;
#33886 = VERTEX_POINT('',#119058) ;
#33887 = VERTEX_POINT('',#119059) ;
#33888 = VERTEX_POINT('',#119061) ;
#33889 = VERTEX_POINT('',#119063) ;
#33890 = VERTEX_POINT('',#119065) ;
#33891 = VERTEX_POINT('',#119067) ;
#33892 = VERTEX_POINT('',#119069) ;
#33893 = VERTEX_POINT('',#119071) ;
#33894 = VERTEX_POINT('',#119075) ;
#33895 = VERTEX_POINT('',#119076) ;
#33896 = VERTEX_POINT('',#119078) ;
#33897 = VERTEX_POINT('',#119080) ;
#33898 = VERTEX_POINT('',#119082) ;
#33899 = VERTEX_POINT('',#119084) ;
#33900 = VERTEX_POINT('',#119086) ;
#33901 = VERTEX_POINT('',#119088) ;
#33902 = VERTEX_POINT('',#119098) ;
#33903 = VERTEX_POINT('',#119108) ;
#33904 = VERTEX_POINT('',#119119) ;
#33905 = VERTEX_POINT('',#119151) ;
#33906 = VERTEX_POINT('',#119198) ;
#33907 = VERTEX_POINT('',#119216) ;
#33908 = VERTEX_POINT('',#119230) ;
#33909 = VERTEX_POINT('',#119245) ;
#33910 = VERTEX_POINT('',#119802) ;
#33911 = VERTEX_POINT('',#119812) ;
#33912 = VERTEX_POINT('',#119823) ;
#33913 = VERTEX_POINT('',#119855) ;
#33914 = VERTEX_POINT('',#119902) ;
#33915 = VERTEX_POINT('',#119920) ;
#33916 = VERTEX_POINT('',#119934) ;
#33917 = VERTEX_POINT('',#119949) ;
#33918 = VERTEX_POINT('',#120029) ;
#33919 = VERTEX_POINT('',#120039) ;
#33920 = VERTEX_POINT('',#120050) ;
#33921 = VERTEX_POINT('',#120082) ;
#33922 = VERTEX_POINT('',#120129) ;
#33923 = VERTEX_POINT('',#120147) ;
#33924 = VERTEX_POINT('',#120161) ;
#33925 = VERTEX_POINT('',#120176) ;
#33926 = VERTEX_POINT('',#120256) ;
#33927 = VERTEX_POINT('',#120266) ;
#33928 = VERTEX_POINT('',#120277) ;
#33929 = VERTEX_POINT('',#120309) ;
#33930 = VERTEX_POINT('',#120356) ;
#33931 = VERTEX_POINT('',#120374) ;
#33932 = VERTEX_POINT('',#120388) ;
#33933 = VERTEX_POINT('',#120403) ;
#33934 = VERTEX_POINT('',#120483) ;
#33935 = VERTEX_POINT('',#120493) ;
#33936 = VERTEX_POINT('',#120504) ;
#33937 = VERTEX_POINT('',#120536) ;
#33938 = VERTEX_POINT('',#120583) ;
#33939 = VERTEX_POINT('',#120601) ;
#33940 = VERTEX_POINT('',#120615) ;
#33941 = VERTEX_POINT('',#120630) ;
#33942 = VERTEX_POINT('',#120710) ;
#33943 = VERTEX_POINT('',#120720) ;
#33944 = VERTEX_POINT('',#120731) ;
#33945 = VERTEX_POINT('',#120763) ;
#33946 = VERTEX_POINT('',#120810) ;
#33947 = VERTEX_POINT('',#120828) ;
#33948 = VERTEX_POINT('',#120842) ;
#33949 = VERTEX_POINT('',#120857) ;
#33950 = VERTEX_POINT('',#120937) ;
#33951 = VERTEX_POINT('',#120947) ;
#33952 = VERTEX_POINT('',#120958) ;
#33953 = VERTEX_POINT('',#120990) ;
#33954 = VERTEX_POINT('',#121037) ;
#33955 = VERTEX_POINT('',#121055) ;
#33956 = VERTEX_POINT('',#121069) ;
#33957 = VERTEX_POINT('',#121084) ;
#33958 = VERTEX_POINT('',#121164) ;
#33959 = VERTEX_POINT('',#121174) ;
#33960 = VERTEX_POINT('',#121185) ;
#33961 = VERTEX_POINT('',#121217) ;
#33962 = VERTEX_POINT('',#121264) ;
#33963 = VERTEX_POINT('',#121282) ;
#33964 = VERTEX_POINT('',#121296) ;
#33965 = VERTEX_POINT('',#121311) ;
#33966 = VERTEX_POINT('',#121391) ;
#33967 = VERTEX_POINT('',#121401) ;
#33968 = VERTEX_POINT('',#121412) ;
#33969 = VERTEX_POINT('',#121444) ;
#33970 = VERTEX_POINT('',#121491) ;
#33971 = VERTEX_POINT('',#121509) ;
#33972 = VERTEX_POINT('',#121523) ;
#33973 = VERTEX_POINT('',#121538) ;
#33974 = VERTEX_POINT('',#121612) ;
#33975 = VERTEX_POINT('',#121613) ;
#33976 = VERTEX_POINT('',#121615) ;
#33977 = VERTEX_POINT('',#121617) ;
#33978 = VERTEX_POINT('',#121621) ;
#33979 = VERTEX_POINT('',#121622) ;
#33980 = VERTEX_POINT('',#121624) ;
#33981 = VERTEX_POINT('',#121626) ;
#33982 = VERTEX_POINT('',#121630) ;
#33983 = VERTEX_POINT('',#121631) ;
#33984 = VERTEX_POINT('',#121633) ;
#33985 = VERTEX_POINT('',#121635) ;
#33986 = VERTEX_POINT('',#121639) ;
#33987 = VERTEX_POINT('',#121640) ;
#33988 = VERTEX_POINT('',#121642) ;
#33989 = VERTEX_POINT('',#121644) ;
#33990 = VERTEX_POINT('',#121648) ;
#33991 = VERTEX_POINT('',#121649) ;
#33992 = VERTEX_POINT('',#121651) ;
#33993 = VERTEX_POINT('',#121653) ;
#33994 = VERTEX_POINT('',#121657) ;
#33995 = VERTEX_POINT('',#121658) ;
#33996 = VERTEX_POINT('',#121661) ;
#33997 = VERTEX_POINT('',#121663) ;
#33998 = VERTEX_POINT('',#121667) ;
#33999 = VERTEX_POINT('',#121668) ;
#34000 = VERTEX_POINT('',#121671) ;
#34001 = VERTEX_POINT('',#121673) ;
#34002 = VERTEX_POINT('',#121683) ;
#34003 = VERTEX_POINT('',#121684) ;
#34004 = VERTEX_POINT('',#121686) ;
#34005 = VERTEX_POINT('',#121688) ;
#34006 = VERTEX_POINT('',#121692) ;
#34007 = VERTEX_POINT('',#121693) ;
#34008 = VERTEX_POINT('',#121698) ;
#34009 = VERTEX_POINT('',#121700) ;
#34010 = VERTEX_POINT('',#121704) ;
#34011 = VERTEX_POINT('',#121705) ;
#34012 = VERTEX_POINT('',#121707) ;
#34013 = VERTEX_POINT('',#121709) ;
#34014 = VERTEX_POINT('',#121713) ;
#34015 = VERTEX_POINT('',#121714) ;
#34016 = VERTEX_POINT('',#121716) ;
#34017 = VERTEX_POINT('',#121718) ;
#34018 = VERTEX_POINT('',#121722) ;
#34019 = VERTEX_POINT('',#121723) ;
#34020 = VERTEX_POINT('',#121728) ;
#34021 = VERTEX_POINT('',#121730) ;
#34022 = VERTEX_POINT('',#121734) ;
#34023 = VERTEX_POINT('',#121735) ;
#34024 = VERTEX_POINT('',#121737) ;
#34025 = VERTEX_POINT('',#121739) ;
#34026 = VERTEX_POINT('',#121743) ;
#34027 = VERTEX_POINT('',#121744) ;
#34028 = VERTEX_POINT('',#121746) ;
#34029 = VERTEX_POINT('',#121748) ;
#34030 = VERTEX_POINT('',#121752) ;
#34031 = VERTEX_POINT('',#121753) ;
#34032 = VERTEX_POINT('',#121755) ;
#34033 = VERTEX_POINT('',#121757) ;
#34034 = VERTEX_POINT('',#121761) ;
#34035 = VERTEX_POINT('',#121762) ;
#34036 = VERTEX_POINT('',#121764) ;
#34037 = VERTEX_POINT('',#121766) ;
#34038 = VERTEX_POINT('',#121770) ;
#34039 = VERTEX_POINT('',#121771) ;
#34040 = VERTEX_POINT('',#121773) ;
#34041 = VERTEX_POINT('',#121775) ;
#34042 = VERTEX_POINT('',#121779) ;
#34043 = VERTEX_POINT('',#121780) ;
#34044 = VERTEX_POINT('',#121783) ;
#34045 = VERTEX_POINT('',#121785) ;
#34046 = VERTEX_POINT('',#121789) ;
#34047 = VERTEX_POINT('',#121790) ;
#34048 = VERTEX_POINT('',#121793) ;
#34049 = VERTEX_POINT('',#121795) ;
#34050 = VERTEX_POINT('',#121805) ;
#34051 = VERTEX_POINT('',#121806) ;
#34052 = VERTEX_POINT('',#121808) ;
#34053 = VERTEX_POINT('',#121810) ;
#34054 = VERTEX_POINT('',#121814) ;
#34055 = VERTEX_POINT('',#121815) ;
#34056 = VERTEX_POINT('',#121820) ;
#34057 = VERTEX_POINT('',#121822) ;
#34058 = VERTEX_POINT('',#121826) ;
#34059 = VERTEX_POINT('',#121827) ;
#34060 = VERTEX_POINT('',#121829) ;
#34061 = VERTEX_POINT('',#121831) ;
#34062 = VERTEX_POINT('',#121835) ;
#34063 = VERTEX_POINT('',#121836) ;
#34064 = VERTEX_POINT('',#121838) ;
#34065 = VERTEX_POINT('',#121840) ;
#34066 = VERTEX_POINT('',#121844) ;
#34067 = VERTEX_POINT('',#121845) ;
#34068 = VERTEX_POINT('',#121850) ;
#34069 = VERTEX_POINT('',#121852) ;
#34070 = VERTEX_POINT('',#121856) ;
#34071 = VERTEX_POINT('',#121857) ;
#34072 = VERTEX_POINT('',#121859) ;
#34073 = VERTEX_POINT('',#121861) ;
#34074 = VERTEX_POINT('',#121865) ;
#34075 = VERTEX_POINT('',#121866) ;
#34076 = VERTEX_POINT('',#121868) ;
#34077 = VERTEX_POINT('',#121870) ;
#34078 = VERTEX_POINT('',#121874) ;
#34079 = VERTEX_POINT('',#121875) ;
#34080 = VERTEX_POINT('',#121877) ;
#34081 = VERTEX_POINT('',#121879) ;
#34082 = VERTEX_POINT('',#121883) ;
#34083 = VERTEX_POINT('',#121884) ;
#34084 = VERTEX_POINT('',#121886) ;
#34085 = VERTEX_POINT('',#121888) ;
#34086 = VERTEX_POINT('',#121892) ;
#34087 = VERTEX_POINT('',#121893) ;
#34088 = VERTEX_POINT('',#121895) ;
#34089 = VERTEX_POINT('',#121897) ;
#34090 = VERTEX_POINT('',#121901) ;
#34091 = VERTEX_POINT('',#121902) ;
#34092 = VERTEX_POINT('',#121905) ;
#34093 = VERTEX_POINT('',#121907) ;
#34094 = VERTEX_POINT('',#121911) ;
#34095 = VERTEX_POINT('',#121912) ;
#34096 = VERTEX_POINT('',#121915) ;
#34097 = VERTEX_POINT('',#121917) ;
#34098 = VERTEX_POINT('',#121927) ;
#34099 = VERTEX_POINT('',#121928) ;
#34100 = VERTEX_POINT('',#121930) ;
#34101 = VERTEX_POINT('',#121932) ;
#34102 = VERTEX_POINT('',#121936) ;
#34103 = VERTEX_POINT('',#121937) ;
#34104 = VERTEX_POINT('',#121942) ;
#34105 = VERTEX_POINT('',#121944) ;
#34106 = VERTEX_POINT('',#121948) ;
#34107 = VERTEX_POINT('',#121949) ;
#34108 = VERTEX_POINT('',#121951) ;
#34109 = VERTEX_POINT('',#121953) ;
#34110 = VERTEX_POINT('',#121957) ;
#34111 = VERTEX_POINT('',#121958) ;
#34112 = VERTEX_POINT('',#121960) ;
#34113 = VERTEX_POINT('',#121962) ;
#34114 = VERTEX_POINT('',#121966) ;
#34115 = VERTEX_POINT('',#121967) ;
#34116 = VERTEX_POINT('',#121972) ;
#34117 = VERTEX_POINT('',#121974) ;
#34118 = VERTEX_POINT('',#121978) ;
#34119 = VERTEX_POINT('',#121979) ;
#34120 = VERTEX_POINT('',#121981) ;
#34121 = VERTEX_POINT('',#121983) ;
#34122 = VERTEX_POINT('',#121987) ;
#34123 = VERTEX_POINT('',#121988) ;
#34124 = VERTEX_POINT('',#121990) ;
#34125 = VERTEX_POINT('',#121992) ;
#34126 = VERTEX_POINT('',#121996) ;
#34127 = VERTEX_POINT('',#121997) ;
#34128 = VERTEX_POINT('',#121999) ;
#34129 = VERTEX_POINT('',#122001) ;
#34130 = VERTEX_POINT('',#122005) ;
#34131 = VERTEX_POINT('',#122006) ;
#34132 = VERTEX_POINT('',#122008) ;
#34133 = VERTEX_POINT('',#122010) ;
#34134 = VERTEX_POINT('',#122014) ;
#34135 = VERTEX_POINT('',#122015) ;
#34136 = VERTEX_POINT('',#122017) ;
#34137 = VERTEX_POINT('',#122019) ;
#34138 = VERTEX_POINT('',#122023) ;
#34139 = VERTEX_POINT('',#122024) ;
#34140 = VERTEX_POINT('',#122027) ;
#34141 = VERTEX_POINT('',#122029) ;
#34142 = VERTEX_POINT('',#122033) ;
#34143 = VERTEX_POINT('',#122034) ;
#34144 = VERTEX_POINT('',#122037) ;
#34145 = VERTEX_POINT('',#122039) ;
#34146 = VERTEX_POINT('',#122049) ;
#34147 = VERTEX_POINT('',#122050) ;
#34148 = VERTEX_POINT('',#122052) ;
#34149 = VERTEX_POINT('',#122054) ;
#34150 = VERTEX_POINT('',#122058) ;
#34151 = VERTEX_POINT('',#122059) ;
#34152 = VERTEX_POINT('',#122064) ;
#34153 = VERTEX_POINT('',#122066) ;
#34154 = VERTEX_POINT('',#122070) ;
#34155 = VERTEX_POINT('',#122071) ;
#34156 = VERTEX_POINT('',#122073) ;
#34157 = VERTEX_POINT('',#122075) ;
#34158 = VERTEX_POINT('',#122079) ;
#34159 = VERTEX_POINT('',#122080) ;
#34160 = VERTEX_POINT('',#122082) ;
#34161 = VERTEX_POINT('',#122084) ;
#34162 = VERTEX_POINT('',#122088) ;
#34163 = VERTEX_POINT('',#122089) ;
#34164 = VERTEX_POINT('',#122094) ;
#34165 = VERTEX_POINT('',#122096) ;
#34166 = VERTEX_POINT('',#122100) ;
#34167 = VERTEX_POINT('',#122101) ;
#34168 = VERTEX_POINT('',#122103) ;
#34169 = VERTEX_POINT('',#122105) ;
#34170 = VERTEX_POINT('',#122109) ;
#34171 = VERTEX_POINT('',#122110) ;
#34172 = VERTEX_POINT('',#122112) ;
#34173 = VERTEX_POINT('',#122114) ;
#34174 = VERTEX_POINT('',#122118) ;
#34175 = VERTEX_POINT('',#122119) ;
#34176 = VERTEX_POINT('',#122121) ;
#34177 = VERTEX_POINT('',#122123) ;
#34178 = VERTEX_POINT('',#122127) ;
#34179 = VERTEX_POINT('',#122128) ;
#34180 = VERTEX_POINT('',#122130) ;
#34181 = VERTEX_POINT('',#122132) ;
#34182 = VERTEX_POINT('',#122136) ;
#34183 = VERTEX_POINT('',#122137) ;
#34184 = VERTEX_POINT('',#122139) ;
#34185 = VERTEX_POINT('',#122141) ;
#34186 = VERTEX_POINT('',#122145) ;
#34187 = VERTEX_POINT('',#122146) ;
#34188 = VERTEX_POINT('',#122149) ;
#34189 = VERTEX_POINT('',#122151) ;
#34190 = VERTEX_POINT('',#122155) ;
#34191 = VERTEX_POINT('',#122156) ;
#34192 = VERTEX_POINT('',#122159) ;
#34193 = VERTEX_POINT('',#122161) ;
#34194 = VERTEX_POINT('',#122171) ;
#34195 = VERTEX_POINT('',#122172) ;
#34196 = VERTEX_POINT('',#122174) ;
#34197 = VERTEX_POINT('',#122176) ;
#34198 = VERTEX_POINT('',#122180) ;
#34199 = VERTEX_POINT('',#122181) ;
#34200 = VERTEX_POINT('',#122186) ;
#34201 = VERTEX_POINT('',#122188) ;
#34202 = VERTEX_POINT('',#122192) ;
#34203 = VERTEX_POINT('',#122193) ;
#34204 = VERTEX_POINT('',#122195) ;
#34205 = VERTEX_POINT('',#122197) ;
#34206 = VERTEX_POINT('',#122201) ;
#34207 = VERTEX_POINT('',#122202) ;
#34208 = VERTEX_POINT('',#122204) ;
#34209 = VERTEX_POINT('',#122206) ;
#34210 = VERTEX_POINT('',#122210) ;
#34211 = VERTEX_POINT('',#122211) ;
#34212 = VERTEX_POINT('',#122216) ;
#34213 = VERTEX_POINT('',#122218) ;
#34214 = VERTEX_POINT('',#122222) ;
#34215 = VERTEX_POINT('',#122223) ;
#34216 = VERTEX_POINT('',#122225) ;
#34217 = VERTEX_POINT('',#122227) ;
#34218 = VERTEX_POINT('',#122231) ;
#34219 = VERTEX_POINT('',#122232) ;
#34220 = VERTEX_POINT('',#122234) ;
#34221 = VERTEX_POINT('',#122236) ;
#34222 = VERTEX_POINT('',#122240) ;
#34223 = VERTEX_POINT('',#122241) ;
#34224 = VERTEX_POINT('',#122243) ;
#34225 = VERTEX_POINT('',#122245) ;
#34226 = VERTEX_POINT('',#122249) ;
#34227 = VERTEX_POINT('',#122250) ;
#34228 = VERTEX_POINT('',#122252) ;
#34229 = VERTEX_POINT('',#122254) ;
#34230 = VERTEX_POINT('',#122258) ;
#34231 = VERTEX_POINT('',#122259) ;
#34232 = VERTEX_POINT('',#122261) ;
#34233 = VERTEX_POINT('',#122263) ;
#34234 = VERTEX_POINT('',#122267) ;
#34235 = VERTEX_POINT('',#122268) ;
#34236 = VERTEX_POINT('',#122271) ;
#34237 = VERTEX_POINT('',#122273) ;
#34238 = VERTEX_POINT('',#122277) ;
#34239 = VERTEX_POINT('',#122278) ;
#34240 = VERTEX_POINT('',#122281) ;
#34241 = VERTEX_POINT('',#122283) ;
#34242 = VERTEX_POINT('',#122293) ;
#34243 = VERTEX_POINT('',#122294) ;
#34244 = VERTEX_POINT('',#122296) ;
#34245 = VERTEX_POINT('',#122298) ;
#34246 = VERTEX_POINT('',#122302) ;
#34247 = VERTEX_POINT('',#122303) ;
#34248 = VERTEX_POINT('',#122308) ;
#34249 = VERTEX_POINT('',#122310) ;
#34250 = VERTEX_POINT('',#122314) ;
#34251 = VERTEX_POINT('',#122315) ;
#34252 = VERTEX_POINT('',#122317) ;
#34253 = VERTEX_POINT('',#122319) ;
#34254 = VERTEX_POINT('',#122323) ;
#34255 = VERTEX_POINT('',#122324) ;
#34256 = VERTEX_POINT('',#122326) ;
#34257 = VERTEX_POINT('',#122328) ;
#34258 = VERTEX_POINT('',#122332) ;
#34259 = VERTEX_POINT('',#122333) ;
#34260 = VERTEX_POINT('',#122338) ;
#34261 = VERTEX_POINT('',#122340) ;
#34262 = VERTEX_POINT('',#122344) ;
#34263 = VERTEX_POINT('',#122345) ;
#34264 = VERTEX_POINT('',#122347) ;
#34265 = VERTEX_POINT('',#122349) ;
#34266 = VERTEX_POINT('',#122353) ;
#34267 = VERTEX_POINT('',#122354) ;
#34268 = VERTEX_POINT('',#122356) ;
#34269 = VERTEX_POINT('',#122358) ;
#34270 = VERTEX_POINT('',#122362) ;
#34271 = VERTEX_POINT('',#122363) ;
#34272 = VERTEX_POINT('',#122365) ;
#34273 = VERTEX_POINT('',#122367) ;
#34274 = VERTEX_POINT('',#122371) ;
#34275 = VERTEX_POINT('',#122372) ;
#34276 = VERTEX_POINT('',#122374) ;
#34277 = VERTEX_POINT('',#122376) ;
#34278 = VERTEX_POINT('',#122380) ;
#34279 = VERTEX_POINT('',#122381) ;
#34280 = VERTEX_POINT('',#122383) ;
#34281 = VERTEX_POINT('',#122385) ;
#34282 = VERTEX_POINT('',#122389) ;
#34283 = VERTEX_POINT('',#122390) ;
#34284 = VERTEX_POINT('',#122393) ;
#34285 = VERTEX_POINT('',#122395) ;
#34286 = VERTEX_POINT('',#122399) ;
#34287 = VERTEX_POINT('',#122400) ;
#34288 = VERTEX_POINT('',#122403) ;
#34289 = VERTEX_POINT('',#122405) ;
#34290 = VERTEX_POINT('',#122415) ;
#34291 = VERTEX_POINT('',#122416) ;
#34292 = VERTEX_POINT('',#122418) ;
#34293 = VERTEX_POINT('',#122420) ;
#34294 = VERTEX_POINT('',#122424) ;
#34295 = VERTEX_POINT('',#122425) ;
#34296 = VERTEX_POINT('',#122430) ;
#34297 = VERTEX_POINT('',#122432) ;
#34298 = VERTEX_POINT('',#122436) ;
#34299 = VERTEX_POINT('',#122437) ;
#34300 = VERTEX_POINT('',#122439) ;
#34301 = VERTEX_POINT('',#122441) ;
#34302 = VERTEX_POINT('',#122445) ;
#34303 = VERTEX_POINT('',#122446) ;
#34304 = VERTEX_POINT('',#122448) ;
#34305 = VERTEX_POINT('',#122450) ;
#34306 = VERTEX_POINT('',#122454) ;
#34307 = VERTEX_POINT('',#122455) ;
#34308 = VERTEX_POINT('',#122460) ;
#34309 = VERTEX_POINT('',#122462) ;
#34310 = VERTEX_POINT('',#122466) ;
#34311 = VERTEX_POINT('',#122467) ;
#34312 = VERTEX_POINT('',#122469) ;
#34313 = VERTEX_POINT('',#122471) ;
#34314 = VERTEX_POINT('',#122475) ;
#34315 = VERTEX_POINT('',#122476) ;
#34316 = VERTEX_POINT('',#122478) ;
#34317 = VERTEX_POINT('',#122480) ;
#34318 = VERTEX_POINT('',#122484) ;
#34319 = VERTEX_POINT('',#122485) ;
#34320 = VERTEX_POINT('',#122487) ;
#34321 = VERTEX_POINT('',#122489) ;
#34322 = VERTEX_POINT('',#122493) ;
#34323 = VERTEX_POINT('',#122494) ;
#34324 = VERTEX_POINT('',#122496) ;
#34325 = VERTEX_POINT('',#122498) ;
#34326 = VERTEX_POINT('',#122502) ;
#34327 = VERTEX_POINT('',#122503) ;
#34328 = VERTEX_POINT('',#122505) ;
#34329 = VERTEX_POINT('',#122507) ;
#34330 = VERTEX_POINT('',#122511) ;
#34331 = VERTEX_POINT('',#122512) ;
#34332 = VERTEX_POINT('',#122515) ;
#34333 = VERTEX_POINT('',#122517) ;
#34334 = VERTEX_POINT('',#122521) ;
#34335 = VERTEX_POINT('',#122522) ;
#34336 = VERTEX_POINT('',#122525) ;
#34337 = VERTEX_POINT('',#122527) ;
#34338 = VERTEX_POINT('',#122537) ;
#34339 = VERTEX_POINT('',#122538) ;
#34340 = VERTEX_POINT('',#122540) ;
#34341 = VERTEX_POINT('',#122542) ;
#34342 = VERTEX_POINT('',#122546) ;
#34343 = VERTEX_POINT('',#122547) ;
#34344 = VERTEX_POINT('',#122552) ;
#34345 = VERTEX_POINT('',#122554) ;
#34346 = VERTEX_POINT('',#122558) ;
#34347 = VERTEX_POINT('',#122559) ;
#34348 = VERTEX_POINT('',#122561) ;
#34349 = VERTEX_POINT('',#122563) ;
#34350 = VERTEX_POINT('',#122567) ;
#34351 = VERTEX_POINT('',#122568) ;
#34352 = VERTEX_POINT('',#122570) ;
#34353 = VERTEX_POINT('',#122572) ;
#34354 = VERTEX_POINT('',#122576) ;
#34355 = VERTEX_POINT('',#122577) ;
#34356 = VERTEX_POINT('',#122582) ;
#34357 = VERTEX_POINT('',#122584) ;
#34358 = VERTEX_POINT('',#122588) ;
#34359 = VERTEX_POINT('',#122589) ;
#34360 = VERTEX_POINT('',#122591) ;
#34361 = VERTEX_POINT('',#122593) ;
#34362 = VERTEX_POINT('',#122597) ;
#34363 = VERTEX_POINT('',#122598) ;
#34364 = VERTEX_POINT('',#122600) ;
#34365 = VERTEX_POINT('',#122602) ;
#34366 = VERTEX_POINT('',#122606) ;
#34367 = VERTEX_POINT('',#122607) ;
#34368 = VERTEX_POINT('',#122609) ;
#34369 = VERTEX_POINT('',#122611) ;
#34370 = VERTEX_POINT('',#122615) ;
#34371 = VERTEX_POINT('',#122616) ;
#34372 = VERTEX_POINT('',#122618) ;
#34373 = VERTEX_POINT('',#122620) ;
#34374 = VERTEX_POINT('',#122624) ;
#34375 = VERTEX_POINT('',#122625) ;
#34376 = VERTEX_POINT('',#122627) ;
#34377 = VERTEX_POINT('',#122629) ;
#34378 = VERTEX_POINT('',#122633) ;
#34379 = VERTEX_POINT('',#122634) ;
#34380 = VERTEX_POINT('',#122637) ;
#34381 = VERTEX_POINT('',#122639) ;
#34382 = VERTEX_POINT('',#122643) ;
#34383 = VERTEX_POINT('',#122644) ;
#34384 = VERTEX_POINT('',#122647) ;
#34385 = VERTEX_POINT('',#122649) ;
#34386 = VERTEX_POINT('',#122659) ;
#34387 = VERTEX_POINT('',#122660) ;
#34388 = VERTEX_POINT('',#122662) ;
#34389 = VERTEX_POINT('',#122664) ;
#34390 = VERTEX_POINT('',#122668) ;
#34391 = VERTEX_POINT('',#122669) ;
#34392 = VERTEX_POINT('',#122674) ;
#34393 = VERTEX_POINT('',#122676) ;
#34394 = VERTEX_POINT('',#122680) ;
#34395 = VERTEX_POINT('',#122681) ;
#34396 = VERTEX_POINT('',#122683) ;
#34397 = VERTEX_POINT('',#122685) ;
#34398 = VERTEX_POINT('',#122689) ;
#34399 = VERTEX_POINT('',#122690) ;
#34400 = VERTEX_POINT('',#122692) ;
#34401 = VERTEX_POINT('',#122694) ;
#34402 = VERTEX_POINT('',#122698) ;
#34403 = VERTEX_POINT('',#122699) ;
#34404 = VERTEX_POINT('',#122704) ;
#34405 = VERTEX_POINT('',#122706) ;
#34406 = VERTEX_POINT('',#122710) ;
#34407 = VERTEX_POINT('',#122711) ;
#34408 = VERTEX_POINT('',#122713) ;
#34409 = VERTEX_POINT('',#122715) ;
#34410 = VERTEX_POINT('',#122719) ;
#34411 = VERTEX_POINT('',#122720) ;
#34412 = VERTEX_POINT('',#122722) ;
#34413 = VERTEX_POINT('',#122724) ;
#34414 = VERTEX_POINT('',#122728) ;
#34415 = VERTEX_POINT('',#122729) ;
#34416 = VERTEX_POINT('',#122731) ;
#34417 = VERTEX_POINT('',#122733) ;
#34418 = VERTEX_POINT('',#122737) ;
#34419 = VERTEX_POINT('',#122738) ;
#34420 = VERTEX_POINT('',#122740) ;
#34421 = VERTEX_POINT('',#122742) ;
#34422 = VERTEX_POINT('',#122746) ;
#34423 = VERTEX_POINT('',#122747) ;
#34424 = VERTEX_POINT('',#122749) ;
#34425 = VERTEX_POINT('',#122751) ;
#34426 = VERTEX_POINT('',#122755) ;
#34427 = VERTEX_POINT('',#122756) ;
#34428 = VERTEX_POINT('',#122758) ;
#34429 = VERTEX_POINT('',#122760) ;
#34430 = VERTEX_POINT('',#122764) ;
#34431 = VERTEX_POINT('',#122765) ;
#34432 = VERTEX_POINT('',#122767) ;
#34433 = VERTEX_POINT('',#122769) ;
#34434 = VERTEX_POINT('',#122773) ;
#34435 = VERTEX_POINT('',#122774) ;
#34436 = VERTEX_POINT('',#122776) ;
#34437 = VERTEX_POINT('',#122778) ;
#34438 = VERTEX_POINT('',#122782) ;
#34439 = VERTEX_POINT('',#122783) ;
#34440 = VERTEX_POINT('',#122785) ;
#34441 = VERTEX_POINT('',#122787) ;
#34442 = VERTEX_POINT('',#122791) ;
#34443 = VERTEX_POINT('',#122792) ;
#34444 = VERTEX_POINT('',#122794) ;
#34445 = VERTEX_POINT('',#122796) ;
#34446 = VERTEX_POINT('',#122800) ;
#34447 = VERTEX_POINT('',#122801) ;
#34448 = VERTEX_POINT('',#122803) ;
#34449 = VERTEX_POINT('',#122805) ;
#34450 = VERTEX_POINT('',#122809) ;
#34451 = VERTEX_POINT('',#122810) ;
#34452 = VERTEX_POINT('',#122812) ;
#34453 = VERTEX_POINT('',#122814) ;
#34454 = VERTEX_POINT('',#122818) ;
#34455 = VERTEX_POINT('',#122819) ;
#34456 = VERTEX_POINT('',#122821) ;
#34457 = VERTEX_POINT('',#122823) ;
#34458 = VERTEX_POINT('',#122827) ;
#34459 = VERTEX_POINT('',#122828) ;
#34460 = VERTEX_POINT('',#122830) ;
#34461 = VERTEX_POINT('',#122832) ;
#34462 = VERTEX_POINT('',#122836) ;
#34463 = VERTEX_POINT('',#122837) ;
#34464 = VERTEX_POINT('',#122839) ;
#34465 = VERTEX_POINT('',#122841) ;
#34466 = VERTEX_POINT('',#122845) ;
#34467 = VERTEX_POINT('',#122846) ;
#34468 = VERTEX_POINT('',#122848) ;
#34469 = VERTEX_POINT('',#122850) ;
#34470 = VERTEX_POINT('',#122854) ;
#34471 = VERTEX_POINT('',#122855) ;
#34472 = VERTEX_POINT('',#122857) ;
#34473 = VERTEX_POINT('',#122859) ;
#34474 = VERTEX_POINT('',#122863) ;
#34475 = VERTEX_POINT('',#122864) ;
#34476 = VERTEX_POINT('',#122866) ;
#34477 = VERTEX_POINT('',#122868) ;
#34478 = VERTEX_POINT('',#122872) ;
#34479 = VERTEX_POINT('',#122873) ;
#34480 = VERTEX_POINT('',#122875) ;
#34481 = VERTEX_POINT('',#122877) ;
#34482 = VERTEX_POINT('',#122881) ;
#34483 = VERTEX_POINT('',#122882) ;
#34484 = VERTEX_POINT('',#122884) ;
#34485 = VERTEX_POINT('',#122886) ;
#34486 = VERTEX_POINT('',#122890) ;
#34487 = VERTEX_POINT('',#122891) ;
#34488 = VERTEX_POINT('',#122893) ;
#34489 = VERTEX_POINT('',#122895) ;
#34490 = VERTEX_POINT('',#122899) ;
#34491 = VERTEX_POINT('',#122900) ;
#34492 = VERTEX_POINT('',#122902) ;
#34493 = VERTEX_POINT('',#122904) ;
#34494 = VERTEX_POINT('',#122908) ;
#34495 = VERTEX_POINT('',#122909) ;
#34496 = VERTEX_POINT('',#122911) ;
#34497 = VERTEX_POINT('',#122913) ;
#34498 = VERTEX_POINT('',#122917) ;
#34499 = VERTEX_POINT('',#122918) ;
#34500 = VERTEX_POINT('',#122920) ;
#34501 = VERTEX_POINT('',#122922) ;
#34502 = VERTEX_POINT('',#122926) ;
#34503 = VERTEX_POINT('',#122927) ;
#34504 = VERTEX_POINT('',#122929) ;
#34505 = VERTEX_POINT('',#122931) ;
#34506 = VERTEX_POINT('',#122935) ;
#34507 = VERTEX_POINT('',#122936) ;
#34508 = VERTEX_POINT('',#122938) ;
#34509 = VERTEX_POINT('',#122940) ;
#34510 = VERTEX_POINT('',#122944) ;
#34511 = VERTEX_POINT('',#122945) ;
#34512 = VERTEX_POINT('',#122947) ;
#34513 = VERTEX_POINT('',#122949) ;
#34514 = VERTEX_POINT('',#122953) ;
#34515 = VERTEX_POINT('',#122954) ;
#34516 = VERTEX_POINT('',#122956) ;
#34517 = VERTEX_POINT('',#122958) ;
#34518 = VERTEX_POINT('',#122962) ;
#34519 = VERTEX_POINT('',#122963) ;
#34520 = VERTEX_POINT('',#122965) ;
#34521 = VERTEX_POINT('',#122967) ;
#34522 = VERTEX_POINT('',#122971) ;
#34523 = VERTEX_POINT('',#122972) ;
#34524 = VERTEX_POINT('',#122974) ;
#34525 = VERTEX_POINT('',#122976) ;
#34526 = VERTEX_POINT('',#122980) ;
#34527 = VERTEX_POINT('',#122981) ;
#34528 = VERTEX_POINT('',#122983) ;
#34529 = VERTEX_POINT('',#122985) ;
#34530 = VERTEX_POINT('',#122989) ;
#34531 = VERTEX_POINT('',#122990) ;
#34532 = VERTEX_POINT('',#122992) ;
#34533 = VERTEX_POINT('',#122994) ;
#34534 = VERTEX_POINT('',#122998) ;
#34535 = VERTEX_POINT('',#122999) ;
#34536 = VERTEX_POINT('',#123001) ;
#34537 = VERTEX_POINT('',#123003) ;
#34538 = VERTEX_POINT('',#123007) ;
#34539 = VERTEX_POINT('',#123008) ;
#34540 = VERTEX_POINT('',#123010) ;
#34541 = VERTEX_POINT('',#123012) ;
#34542 = VERTEX_POINT('',#123016) ;
#34543 = VERTEX_POINT('',#123017) ;
#34544 = VERTEX_POINT('',#123019) ;
#34545 = VERTEX_POINT('',#123021) ;
#34546 = VERTEX_POINT('',#123025) ;
#34547 = VERTEX_POINT('',#123026) ;
#34548 = VERTEX_POINT('',#123028) ;
#34549 = VERTEX_POINT('',#123030) ;
#34550 = VERTEX_POINT('',#124043) ;
#34551 = VERTEX_POINT('',#124044) ;
#34552 = VERTEX_POINT('',#124046) ;
#34553 = VERTEX_POINT('',#124067) ;
#34554 = VERTEX_POINT('',#124090) ;
#34555 = VERTEX_POINT('',#124091) ;
#34556 = VERTEX_POINT('',#124170) ;
#34557 = VERTEX_POINT('',#124171) ;
#34558 = VERTEX_POINT('',#124246) ;
#34559 = VERTEX_POINT('',#124247) ;
#34560 = VERTEX_POINT('',#124322) ;
#34561 = VERTEX_POINT('',#124323) ;
#34562 = VERTEX_POINT('',#124398) ;
#34563 = VERTEX_POINT('',#124399) ;
#34564 = VERTEX_POINT('',#124474) ;
#34565 = VERTEX_POINT('',#124475) ;
#34566 = VERTEX_POINT('',#124550) ;
#34567 = VERTEX_POINT('',#124551) ;
#34568 = VERTEX_POINT('',#124626) ;
#34569 = VERTEX_POINT('',#124627) ;
#34570 = VERTEX_POINT('',#124706) ;
#34571 = VERTEX_POINT('',#124707) ;
#34572 = VERTEX_POINT('',#124782) ;
#34573 = VERTEX_POINT('',#124783) ;
#34574 = VERTEX_POINT('',#124785) ;
#34575 = VERTEX_POINT('',#124798) ;
#34576 = VERTEX_POINT('',#124809) ;
#34577 = VERTEX_POINT('',#124810) ;
#34578 = VERTEX_POINT('',#124885) ;
#34579 = VERTEX_POINT('',#124886) ;
#34580 = VERTEX_POINT('',#124961) ;
#34581 = VERTEX_POINT('',#124962) ;
#34582 = VERTEX_POINT('',#125037) ;
#34583 = VERTEX_POINT('',#125038) ;
#34584 = VERTEX_POINT('',#125113) ;
#34585 = VERTEX_POINT('',#125114) ;
#34586 = VERTEX_POINT('',#125189) ;
#34587 = VERTEX_POINT('',#125190) ;
#34588 = VERTEX_POINT('',#125267) ;
#34589 = VERTEX_POINT('',#125268) ;
#34590 = VERTEX_POINT('',#125345) ;
#34591 = VERTEX_POINT('',#125347) ;
#34592 = VERTEX_POINT('',#125349) ;
#34593 = VERTEX_POINT('',#125378) ;
#34594 = VERTEX_POINT('',#125380) ;
#34595 = VERTEX_POINT('',#125382) ;
#34596 = VERTEX_POINT('',#125384) ;
#34597 = VERTEX_POINT('',#125415) ;
#34598 = VERTEX_POINT('',#125527) ;
#34599 = VERTEX_POINT('',#125550) ;
#34600 = VERTEX_POINT('',#125567) ;
#34601 = VERTEX_POINT('',#125569) ;
#34602 = VERTEX_POINT('',#125573) ;
#34603 = VERTEX_POINT('',#125577) ;
#34604 = VERTEX_POINT('',#125580) ;
#34605 = VERTEX_POINT('',#125584) ;
#34606 = VERTEX_POINT('',#125615) ;
#34607 = VERTEX_POINT('',#125639) ;
#34608 = VERTEX_POINT('',#125640) ;
#34609 = VERTEX_POINT('',#125642) ;
#34610 = VERTEX_POINT('',#125644) ;
#34611 = VERTEX_POINT('',#125648) ;
#34612 = VERTEX_POINT('',#125649) ;
#34613 = VERTEX_POINT('',#125651) ;
#34614 = VERTEX_POINT('',#125653) ;
#34615 = VERTEX_POINT('',#125657) ;
#34616 = VERTEX_POINT('',#125658) ;
#34617 = VERTEX_POINT('',#125660) ;
#34618 = VERTEX_POINT('',#125662) ;
#34619 = VERTEX_POINT('',#125666) ;
#34620 = VERTEX_POINT('',#125667) ;
#34621 = VERTEX_POINT('',#125669) ;
#34622 = VERTEX_POINT('',#125671) ;
#34623 = VERTEX_POINT('',#125675) ;
#34624 = VERTEX_POINT('',#125676) ;
#34625 = VERTEX_POINT('',#125678) ;
#34626 = VERTEX_POINT('',#125680) ;
#34627 = VERTEX_POINT('',#125684) ;
#34628 = VERTEX_POINT('',#125685) ;
#34629 = VERTEX_POINT('',#125687) ;
#34630 = VERTEX_POINT('',#125689) ;
#34631 = VERTEX_POINT('',#125693) ;
#34632 = VERTEX_POINT('',#125697) ;
#34633 = VERTEX_POINT('',#125703) ;
#34634 = VERTEX_POINT('',#125712) ;
#34635 = VERTEX_POINT('',#125721) ;
#34636 = VERTEX_POINT('',#125730) ;
#34637 = VERTEX_POINT('',#125747) ;
#34638 = VERTEX_POINT('',#125751) ;
#34639 = VERTEX_POINT('',#125757) ;
#34640 = VERTEX_POINT('',#125769) ;
#34641 = VERTEX_POINT('',#125778) ;
#34642 = VERTEX_POINT('',#125787) ;
#34643 = VERTEX_POINT('',#126350) ;
#34644 = VERTEX_POINT('',#126369) ;
#34645 = VERTEX_POINT('',#126370) ;
#34646 = VERTEX_POINT('',#126372) ;
#34647 = VERTEX_POINT('',#126374) ;
#34648 = VERTEX_POINT('',#126376) ;
#34649 = VERTEX_POINT('',#126378) ;
#34650 = VERTEX_POINT('',#126380) ;
#34651 = VERTEX_POINT('',#126382) ;
#34652 = VERTEX_POINT('',#126384) ;
#34653 = VERTEX_POINT('',#126386) ;
#34654 = VERTEX_POINT('',#126388) ;
#34655 = VERTEX_POINT('',#126390) ;
#34656 = VERTEX_POINT('',#126392) ;
#34657 = VERTEX_POINT('',#126394) ;
#34658 = VERTEX_POINT('',#126396) ;
#34659 = VERTEX_POINT('',#126398) ;
#34660 = VERTEX_POINT('',#126400) ;
#34661 = VERTEX_POINT('',#126402) ;
#34662 = VERTEX_POINT('',#126408) ;
#34663 = VERTEX_POINT('',#126410) ;
#34664 = VERTEX_POINT('',#126414) ;
#34665 = VERTEX_POINT('',#126416) ;
#34666 = VERTEX_POINT('',#126420) ;
#34667 = VERTEX_POINT('',#126424) ;
#34668 = VERTEX_POINT('',#126428) ;
#34669 = VERTEX_POINT('',#126429) ;
#34670 = VERTEX_POINT('',#126431) ;
#34671 = VERTEX_POINT('',#126433) ;
#34672 = VERTEX_POINT('',#126435) ;
#34673 = VERTEX_POINT('',#126437) ;
#34674 = VERTEX_POINT('',#126439) ;
#34675 = VERTEX_POINT('',#126441) ;
#34676 = VERTEX_POINT('',#126443) ;
#34677 = VERTEX_POINT('',#126445) ;
#34678 = VERTEX_POINT('',#126447) ;
#34679 = VERTEX_POINT('',#126449) ;
#34680 = VERTEX_POINT('',#126451) ;
#34681 = VERTEX_POINT('',#126453) ;
#34682 = VERTEX_POINT('',#126455) ;
#34683 = VERTEX_POINT('',#126457) ;
#34684 = VERTEX_POINT('',#126464) ;
#34685 = VERTEX_POINT('',#126468) ;
#34686 = VERTEX_POINT('',#126475) ;
#34687 = VERTEX_POINT('',#126485) ;
#34688 = VERTEX_POINT('',#126497) ;
#34689 = VERTEX_POINT('',#126503) ;
#34690 = VERTEX_POINT('',#126507) ;
#34691 = VERTEX_POINT('',#126516) ;
#34692 = EDGE_CURVE('',#29494,#29495,#24719,.T.) ;
#34693 = EDGE_CURVE('',#29495,#29494,#24720,.T.) ;
#34694 = EDGE_CURVE('',#29495,#29496,#24721,.T.) ;
#34695 = EDGE_CURVE('',#29496,#29496,#24722,.T.) ;
#34696 = EDGE_CURVE('',#29497,#29497,#24723,.T.) ;
#34697 = EDGE_CURVE('',#29497,#29498,#24724,.T.) ;
#34698 = EDGE_CURVE('',#29499,#29498,#24725,.T.) ;
#34699 = EDGE_CURVE('',#29498,#29499,#24726,.T.) ;
#34700 = EDGE_CURVE('',#29500,#29501,#24727,.T.) ;
#34701 = EDGE_CURVE('',#29501,#29500,#24728,.T.) ;
#34702 = EDGE_CURVE('',#29501,#29502,#24729,.T.) ;
#34703 = EDGE_CURVE('',#29503,#29502,#24730,.T.) ;
#34704 = EDGE_CURVE('',#29502,#29503,#24731,.T.) ;
#34705 = EDGE_CURVE('',#29504,#29504,#24732,.T.) ;
#34706 = EDGE_CURVE('',#29504,#29505,#24733,.T.) ;
#34707 = EDGE_CURVE('',#29505,#29505,#24734,.T.) ;
#34708 = EDGE_CURVE('',#29506,#29507,#24735,.T.) ;
#34709 = EDGE_CURVE('',#29507,#29506,#24736,.T.) ;
#34710 = EDGE_CURVE('',#29507,#29508,#24737,.T.) ;
#34711 = EDGE_CURVE('',#29509,#29508,#24738,.T.) ;
#34712 = EDGE_CURVE('',#29508,#29509,#24739,.T.) ;
#34713 = EDGE_CURVE('',#29510,#29510,#24740,.T.) ;
#34714 = EDGE_CURVE('',#29510,#29511,#24741,.T.) ;
#34715 = EDGE_CURVE('',#29511,#29511,#24742,.T.) ;
#34716 = EDGE_CURVE('',#29506,#29512,#7896,.T.) ;
#34717 = EDGE_CURVE('',#29512,#29512,#24743,.T.) ;
#34718 = EDGE_CURVE('',#29511,#29509,#7897,.T.) ;
#34719 = EDGE_CURVE('',#29500,#29513,#7898,.T.) ;
#34720 = EDGE_CURVE('',#29513,#29513,#24744,.T.) ;
#34721 = EDGE_CURVE('',#29505,#29503,#7899,.T.) ;
#34722 = EDGE_CURVE('',#29494,#29499,#7900,.T.) ;
#34723 = EDGE_CURVE('',#29514,#29515,#7901,.T.) ;
#34724 = EDGE_CURVE('',#29515,#29516,#7902,.T.) ;
#34725 = EDGE_CURVE('',#29516,#29517,#7903,.T.) ;
#34726 = EDGE_CURVE('',#29517,#29518,#7904,.T.) ;
#34727 = EDGE_CURVE('',#29519,#29518,#7905,.T.) ;
#34728 = EDGE_CURVE('',#29514,#29519,#7906,.T.) ;
#34729 = EDGE_CURVE('',#29520,#29521,#24745,.T.) ;
#34730 = EDGE_CURVE('',#29520,#29522,#7907,.T.) ;
#34731 = EDGE_CURVE('',#29523,#29522,#24746,.T.) ;
#34732 = EDGE_CURVE('',#29523,#29524,#7908,.T.) ;
#34733 = EDGE_CURVE('',#29525,#29524,#24747,.T.) ;
#34734 = EDGE_CURVE('',#29525,#29526,#7909,.T.) ;
#34735 = EDGE_CURVE('',#29527,#29526,#24748,.T.) ;
#34736 = EDGE_CURVE('',#29527,#29521,#7910,.T.) ;
#34737 = EDGE_CURVE('',#29528,#29529,#7911,.T.) ;
#34738 = EDGE_CURVE('',#29529,#29530,#7912,.T.) ;
#34739 = EDGE_CURVE('',#29531,#29530,#7913,.T.) ;
#34740 = EDGE_CURVE('',#29532,#29531,#7914,.T.) ;
#34741 = EDGE_CURVE('',#29532,#29533,#7915,.T.) ;
#34742 = EDGE_CURVE('',#29533,#29528,#7916,.T.) ;
#34743 = EDGE_CURVE('',#29534,#29535,#24749,.T.) ;
#34744 = EDGE_CURVE('',#29534,#29536,#7917,.T.) ;
#34745 = EDGE_CURVE('',#29537,#29536,#24750,.T.) ;
#34746 = EDGE_CURVE('',#29537,#29538,#7918,.T.) ;
#34747 = EDGE_CURVE('',#29539,#29538,#24751,.T.) ;
#34748 = EDGE_CURVE('',#29539,#29540,#7919,.T.) ;
#34749 = EDGE_CURVE('',#29541,#29540,#24752,.T.) ;
#34750 = EDGE_CURVE('',#29541,#29535,#7920,.T.) ;
#34751 = EDGE_CURVE('',#29542,#29543,#24753,.T.) ;
#34752 = EDGE_CURVE('',#29542,#29544,#7921,.T.) ;
#34753 = EDGE_CURVE('',#29545,#29544,#7922,.T.) ;
#34754 = EDGE_CURVE('',#29546,#29545,#7923,.T.) ;
#34755 = EDGE_CURVE('',#29546,#29547,#7924,.T.) ;
#34756 = EDGE_CURVE('',#29547,#29548,#7925,.T.) ;
#34757 = EDGE_CURVE('',#29548,#29549,#7926,.T.) ;
#34758 = EDGE_CURVE('',#29550,#29549,#24754,.T.) ;
#34759 = EDGE_CURVE('',#29550,#29551,#7927,.T.) ;
#34760 = EDGE_CURVE('',#29551,#29552,#7928,.T.) ;
#34761 = EDGE_CURVE('',#29552,#29543,#7929,.T.) ;
#34762 = EDGE_CURVE('',#29553,#29554,#24755,.T.) ;
#34763 = EDGE_CURVE('',#29553,#29555,#7930,.T.) ;
#34764 = EDGE_CURVE('',#29556,#29555,#24756,.T.) ;
#34765 = EDGE_CURVE('',#29556,#29557,#7931,.T.) ;
#34766 = EDGE_CURVE('',#29558,#29557,#24757,.T.) ;
#34767 = EDGE_CURVE('',#29558,#29559,#7932,.T.) ;
#34768 = EDGE_CURVE('',#29560,#29559,#24758,.T.) ;
#34769 = EDGE_CURVE('',#29560,#29554,#7933,.T.) ;
#34770 = EDGE_CURVE('',#29561,#29562,#24759,.T.) ;
#34771 = EDGE_CURVE('',#29561,#29563,#7934,.T.) ;
#34772 = EDGE_CURVE('',#29564,#29563,#24760,.T.) ;
#34773 = EDGE_CURVE('',#29564,#29565,#7935,.T.) ;
#34774 = EDGE_CURVE('',#29566,#29565,#24761,.T.) ;
#34775 = EDGE_CURVE('',#29566,#29567,#7936,.T.) ;
#34776 = EDGE_CURVE('',#29568,#29567,#24762,.T.) ;
#34777 = EDGE_CURVE('',#29568,#29562,#7937,.T.) ;
#34778 = EDGE_CURVE('',#29569,#29570,#24763,.T.) ;
#34779 = EDGE_CURVE('',#29569,#29571,#7938,.T.) ;
#34780 = EDGE_CURVE('',#29572,#29571,#24764,.T.) ;
#34781 = EDGE_CURVE('',#29572,#29573,#7939,.T.) ;
#34782 = EDGE_CURVE('',#29574,#29573,#24765,.T.) ;
#34783 = EDGE_CURVE('',#29574,#29575,#7940,.T.) ;
#34784 = EDGE_CURVE('',#29576,#29575,#24766,.T.) ;
#34785 = EDGE_CURVE('',#29576,#29570,#7941,.T.) ;
#34786 = EDGE_CURVE('',#29577,#29578,#24767,.T.) ;
#34787 = EDGE_CURVE('',#29577,#29579,#7942,.T.) ;
#34788 = EDGE_CURVE('',#29580,#29579,#24768,.T.) ;
#34789 = EDGE_CURVE('',#29580,#29581,#7943,.T.) ;
#34790 = EDGE_CURVE('',#29582,#29581,#24769,.T.) ;
#34791 = EDGE_CURVE('',#29582,#29583,#7944,.T.) ;
#34792 = EDGE_CURVE('',#29584,#29583,#24770,.T.) ;
#34793 = EDGE_CURVE('',#29584,#29578,#7945,.T.) ;
#34794 = EDGE_CURVE('',#29585,#29586,#7946,.T.) ;
#34795 = EDGE_CURVE('',#29586,#29587,#7947,.T.) ;
#34796 = EDGE_CURVE('',#29588,#29587,#24771,.T.) ;
#34797 = EDGE_CURVE('',#29588,#29589,#7948,.T.) ;
#34798 = EDGE_CURVE('',#29589,#29590,#7949,.T.) ;
#34799 = EDGE_CURVE('',#29590,#29591,#7950,.T.) ;
#34800 = EDGE_CURVE('',#29592,#29591,#24772,.T.) ;
#34801 = EDGE_CURVE('',#29592,#29593,#7951,.T.) ;
#34802 = EDGE_CURVE('',#29593,#29594,#7952,.T.) ;
#34803 = EDGE_CURVE('',#29594,#29595,#7953,.T.) ;
#34804 = EDGE_CURVE('',#29595,#29585,#7954,.T.) ;
#34805 = EDGE_CURVE('',#29596,#29597,#24773,.T.) ;
#34806 = EDGE_CURVE('',#29596,#29598,#7955,.T.) ;
#34807 = EDGE_CURVE('',#29599,#29598,#24774,.T.) ;
#34808 = EDGE_CURVE('',#29599,#29600,#7956,.T.) ;
#34809 = EDGE_CURVE('',#29601,#29600,#24775,.T.) ;
#34810 = EDGE_CURVE('',#29601,#29602,#7957,.T.) ;
#34811 = EDGE_CURVE('',#29603,#29602,#24776,.T.) ;
#34812 = EDGE_CURVE('',#29603,#29597,#7958,.T.) ;
#34813 = EDGE_CURVE('',#29604,#29605,#24777,.T.) ;
#34814 = EDGE_CURVE('',#29604,#29606,#7959,.T.) ;
#34815 = EDGE_CURVE('',#29607,#29606,#24778,.T.) ;
#34816 = EDGE_CURVE('',#29607,#29608,#7960,.T.) ;
#34817 = EDGE_CURVE('',#29609,#29608,#24779,.T.) ;
#34818 = EDGE_CURVE('',#29609,#29610,#7961,.T.) ;
#34819 = EDGE_CURVE('',#29611,#29610,#24780,.T.) ;
#34820 = EDGE_CURVE('',#29611,#29605,#7962,.T.) ;
#34821 = EDGE_CURVE('',#29612,#29613,#24781,.T.) ;
#34822 = EDGE_CURVE('',#29612,#29614,#7963,.T.) ;
#34823 = EDGE_CURVE('',#29615,#29614,#24782,.T.) ;
#34824 = EDGE_CURVE('',#29615,#29616,#7964,.T.) ;
#34825 = EDGE_CURVE('',#29617,#29616,#24783,.T.) ;
#34826 = EDGE_CURVE('',#29617,#29618,#7965,.T.) ;
#34827 = EDGE_CURVE('',#29619,#29618,#24784,.T.) ;
#34828 = EDGE_CURVE('',#29619,#29613,#7966,.T.) ;
#34829 = EDGE_CURVE('',#29620,#29621,#24785,.T.) ;
#34830 = EDGE_CURVE('',#29620,#29622,#7967,.T.) ;
#34831 = EDGE_CURVE('',#29623,#29622,#24786,.T.) ;
#34832 = EDGE_CURVE('',#29623,#29624,#7968,.T.) ;
#34833 = EDGE_CURVE('',#29625,#29624,#24787,.T.) ;
#34834 = EDGE_CURVE('',#29625,#29626,#7969,.T.) ;
#34835 = EDGE_CURVE('',#29627,#29626,#24788,.T.) ;
#34836 = EDGE_CURVE('',#29627,#29621,#7970,.T.) ;
#34837 = EDGE_CURVE('',#29628,#29629,#7971,.T.) ;
#34838 = EDGE_CURVE('',#29629,#29630,#7972,.T.) ;
#34839 = EDGE_CURVE('',#29631,#29630,#24789,.T.) ;
#34840 = EDGE_CURVE('',#29631,#29632,#7973,.T.) ;
#34841 = EDGE_CURVE('',#29632,#29633,#7974,.T.) ;
#34842 = EDGE_CURVE('',#29633,#29634,#7975,.T.) ;
#34843 = EDGE_CURVE('',#29635,#29634,#24790,.T.) ;
#34844 = EDGE_CURVE('',#29635,#29636,#7976,.T.) ;
#34845 = EDGE_CURVE('',#29636,#29637,#7977,.T.) ;
#34846 = EDGE_CURVE('',#29637,#29638,#7978,.T.) ;
#34847 = EDGE_CURVE('',#29638,#29628,#7979,.T.) ;
#34848 = EDGE_CURVE('',#29639,#29640,#24791,.T.) ;
#34849 = EDGE_CURVE('',#29639,#29641,#7980,.T.) ;
#34850 = EDGE_CURVE('',#29642,#29641,#24792,.T.) ;
#34851 = EDGE_CURVE('',#29642,#29643,#7981,.T.) ;
#34852 = EDGE_CURVE('',#29644,#29643,#24793,.T.) ;
#34853 = EDGE_CURVE('',#29644,#29645,#7982,.T.) ;
#34854 = EDGE_CURVE('',#29646,#29645,#24794,.T.) ;
#34855 = EDGE_CURVE('',#29646,#29640,#7983,.T.) ;
#34856 = EDGE_CURVE('',#29647,#29648,#24795,.T.) ;
#34857 = EDGE_CURVE('',#29647,#29649,#7984,.T.) ;
#34858 = EDGE_CURVE('',#29650,#29649,#24796,.T.) ;
#34859 = EDGE_CURVE('',#29650,#29651,#7985,.T.) ;
#34860 = EDGE_CURVE('',#29652,#29651,#24797,.T.) ;
#34861 = EDGE_CURVE('',#29652,#29653,#7986,.T.) ;
#34862 = EDGE_CURVE('',#29654,#29653,#24798,.T.) ;
#34863 = EDGE_CURVE('',#29654,#29648,#7987,.T.) ;
#34864 = EDGE_CURVE('',#29655,#29656,#24799,.T.) ;
#34865 = EDGE_CURVE('',#29655,#29657,#7988,.T.) ;
#34866 = EDGE_CURVE('',#29658,#29657,#24800,.T.) ;
#34867 = EDGE_CURVE('',#29658,#29659,#7989,.T.) ;
#34868 = EDGE_CURVE('',#29660,#29659,#24801,.T.) ;
#34869 = EDGE_CURVE('',#29660,#29661,#7990,.T.) ;
#34870 = EDGE_CURVE('',#29662,#29661,#24802,.T.) ;
#34871 = EDGE_CURVE('',#29662,#29656,#7991,.T.) ;
#34872 = EDGE_CURVE('',#29663,#29664,#24803,.T.) ;
#34873 = EDGE_CURVE('',#29663,#29665,#7992,.T.) ;
#34874 = EDGE_CURVE('',#29666,#29665,#24804,.T.) ;
#34875 = EDGE_CURVE('',#29666,#29667,#7993,.T.) ;
#34876 = EDGE_CURVE('',#29668,#29667,#24805,.T.) ;
#34877 = EDGE_CURVE('',#29668,#29669,#7994,.T.) ;
#34878 = EDGE_CURVE('',#29670,#29669,#24806,.T.) ;
#34879 = EDGE_CURVE('',#29670,#29664,#7995,.T.) ;
#34880 = EDGE_CURVE('',#29671,#29672,#24807,.T.) ;
#34881 = EDGE_CURVE('',#29671,#29673,#7996,.T.) ;
#34882 = EDGE_CURVE('',#29674,#29673,#24808,.T.) ;
#34883 = EDGE_CURVE('',#29674,#29675,#7997,.T.) ;
#34884 = EDGE_CURVE('',#29676,#29675,#24809,.T.) ;
#34885 = EDGE_CURVE('',#29676,#29677,#7998,.T.) ;
#34886 = EDGE_CURVE('',#29678,#29677,#24810,.T.) ;
#34887 = EDGE_CURVE('',#29678,#29672,#7999,.T.) ;
#34888 = EDGE_CURVE('',#29679,#29680,#24811,.T.) ;
#34889 = EDGE_CURVE('',#29679,#29681,#8000,.T.) ;
#34890 = EDGE_CURVE('',#29682,#29681,#24812,.T.) ;
#34891 = EDGE_CURVE('',#29682,#29683,#8001,.T.) ;
#34892 = EDGE_CURVE('',#29684,#29683,#24813,.T.) ;
#34893 = EDGE_CURVE('',#29684,#29685,#8002,.T.) ;
#34894 = EDGE_CURVE('',#29686,#29685,#24814,.T.) ;
#34895 = EDGE_CURVE('',#29686,#29680,#8003,.T.) ;
#34896 = EDGE_CURVE('',#29687,#29688,#24815,.T.) ;
#34897 = EDGE_CURVE('',#29687,#29689,#8004,.T.) ;
#34898 = EDGE_CURVE('',#29690,#29689,#24816,.T.) ;
#34899 = EDGE_CURVE('',#29690,#29691,#8005,.T.) ;
#34900 = EDGE_CURVE('',#29692,#29691,#24817,.T.) ;
#34901 = EDGE_CURVE('',#29692,#29693,#8006,.T.) ;
#34902 = EDGE_CURVE('',#29694,#29693,#24818,.T.) ;
#34903 = EDGE_CURVE('',#29694,#29688,#8007,.T.) ;
#34904 = EDGE_CURVE('',#29695,#29696,#24819,.T.) ;
#34905 = EDGE_CURVE('',#29695,#29697,#8008,.T.) ;
#34906 = EDGE_CURVE('',#29698,#29697,#8009,.T.) ;
#34907 = EDGE_CURVE('',#29699,#29698,#8010,.T.) ;
#34908 = EDGE_CURVE('',#29699,#29700,#8011,.T.) ;
#34909 = EDGE_CURVE('',#29700,#29701,#8012,.T.) ;
#34910 = EDGE_CURVE('',#29701,#29702,#8013,.T.) ;
#34911 = EDGE_CURVE('',#29703,#29702,#24820,.T.) ;
#34912 = EDGE_CURVE('',#29703,#29704,#8014,.T.) ;
#34913 = EDGE_CURVE('',#29704,#29705,#8015,.T.) ;
#34914 = EDGE_CURVE('',#29705,#29696,#8016,.T.) ;
#34915 = EDGE_CURVE('',#29706,#29707,#24821,.T.) ;
#34916 = EDGE_CURVE('',#29706,#29708,#8017,.T.) ;
#34917 = EDGE_CURVE('',#29709,#29708,#24822,.T.) ;
#34918 = EDGE_CURVE('',#29709,#29710,#8018,.T.) ;
#34919 = EDGE_CURVE('',#29711,#29710,#24823,.T.) ;
#34920 = EDGE_CURVE('',#29711,#29712,#8019,.T.) ;
#34921 = EDGE_CURVE('',#29713,#29712,#24824,.T.) ;
#34922 = EDGE_CURVE('',#29713,#29707,#8020,.T.) ;
#34923 = EDGE_CURVE('',#29714,#29715,#24825,.T.) ;
#34924 = EDGE_CURVE('',#29714,#29716,#8021,.T.) ;
#34925 = EDGE_CURVE('',#29717,#29716,#24826,.T.) ;
#34926 = EDGE_CURVE('',#29717,#29718,#8022,.T.) ;
#34927 = EDGE_CURVE('',#29719,#29718,#24827,.T.) ;
#34928 = EDGE_CURVE('',#29719,#29720,#8023,.T.) ;
#34929 = EDGE_CURVE('',#29721,#29720,#24828,.T.) ;
#34930 = EDGE_CURVE('',#29721,#29715,#8024,.T.) ;
#34931 = EDGE_CURVE('',#29722,#29723,#24829,.T.) ;
#34932 = EDGE_CURVE('',#29722,#29724,#8025,.T.) ;
#34933 = EDGE_CURVE('',#29725,#29724,#24830,.T.) ;
#34934 = EDGE_CURVE('',#29725,#29726,#8026,.T.) ;
#34935 = EDGE_CURVE('',#29727,#29726,#24831,.T.) ;
#34936 = EDGE_CURVE('',#29727,#29728,#8027,.T.) ;
#34937 = EDGE_CURVE('',#29729,#29728,#24832,.T.) ;
#34938 = EDGE_CURVE('',#29729,#29723,#8028,.T.) ;
#34939 = EDGE_CURVE('',#29730,#29731,#24833,.T.) ;
#34940 = EDGE_CURVE('',#29730,#29732,#8029,.T.) ;
#34941 = EDGE_CURVE('',#29733,#29732,#24834,.T.) ;
#34942 = EDGE_CURVE('',#29733,#29734,#8030,.T.) ;
#34943 = EDGE_CURVE('',#29735,#29734,#24835,.T.) ;
#34944 = EDGE_CURVE('',#29735,#29736,#8031,.T.) ;
#34945 = EDGE_CURVE('',#29737,#29736,#24836,.T.) ;
#34946 = EDGE_CURVE('',#29737,#29731,#8032,.T.) ;
#34947 = EDGE_CURVE('',#29738,#29739,#24837,.T.) ;
#34948 = EDGE_CURVE('',#29738,#29740,#8033,.T.) ;
#34949 = EDGE_CURVE('',#29741,#29740,#24838,.T.) ;
#34950 = EDGE_CURVE('',#29741,#29742,#8034,.T.) ;
#34951 = EDGE_CURVE('',#29743,#29742,#24839,.T.) ;
#34952 = EDGE_CURVE('',#29743,#29744,#8035,.T.) ;
#34953 = EDGE_CURVE('',#29745,#29744,#24840,.T.) ;
#34954 = EDGE_CURVE('',#29745,#29739,#8036,.T.) ;
#34955 = EDGE_CURVE('',#29746,#29747,#24841,.T.) ;
#34956 = EDGE_CURVE('',#29746,#29748,#8037,.T.) ;
#34957 = EDGE_CURVE('',#29749,#29748,#24842,.T.) ;
#34958 = EDGE_CURVE('',#29749,#29750,#8038,.T.) ;
#34959 = EDGE_CURVE('',#29751,#29750,#24843,.T.) ;
#34960 = EDGE_CURVE('',#29751,#29752,#8039,.T.) ;
#34961 = EDGE_CURVE('',#29753,#29752,#24844,.T.) ;
#34962 = EDGE_CURVE('',#29753,#29747,#8040,.T.) ;
#34963 = EDGE_CURVE('',#29754,#29755,#24845,.T.) ;
#34964 = EDGE_CURVE('',#29754,#29756,#8041,.T.) ;
#34965 = EDGE_CURVE('',#29757,#29756,#24846,.T.) ;
#34966 = EDGE_CURVE('',#29757,#29758,#8042,.T.) ;
#34967 = EDGE_CURVE('',#29759,#29758,#24847,.T.) ;
#34968 = EDGE_CURVE('',#29759,#29760,#8043,.T.) ;
#34969 = EDGE_CURVE('',#29761,#29760,#24848,.T.) ;
#34970 = EDGE_CURVE('',#29761,#29755,#8044,.T.) ;
#34971 = EDGE_CURVE('',#29762,#29763,#24849,.T.) ;
#34972 = EDGE_CURVE('',#29762,#29764,#8045,.T.) ;
#34973 = EDGE_CURVE('',#29765,#29764,#8046,.T.) ;
#34974 = EDGE_CURVE('',#29765,#29766,#8047,.T.) ;
#34975 = EDGE_CURVE('',#29766,#29767,#8048,.T.) ;
#34976 = EDGE_CURVE('',#29767,#29768,#8049,.T.) ;
#34977 = EDGE_CURVE('',#29769,#29768,#24850,.T.) ;
#34978 = EDGE_CURVE('',#29769,#29770,#8050,.T.) ;
#34979 = EDGE_CURVE('',#29770,#29771,#8051,.T.) ;
#34980 = EDGE_CURVE('',#29771,#29763,#8052,.T.) ;
#34981 = EDGE_CURVE('',#29772,#29773,#8053,.T.) ;
#34982 = EDGE_CURVE('',#29773,#29774,#8054,.T.) ;
#34983 = EDGE_CURVE('',#29775,#29774,#24851,.T.) ;
#34984 = EDGE_CURVE('',#29775,#29776,#8055,.T.) ;
#34985 = EDGE_CURVE('',#29776,#29777,#8056,.T.) ;
#34986 = EDGE_CURVE('',#29777,#29778,#8057,.T.) ;
#34987 = EDGE_CURVE('',#29779,#29778,#24852,.T.) ;
#34988 = EDGE_CURVE('',#29779,#29780,#8058,.T.) ;
#34989 = EDGE_CURVE('',#29781,#29780,#8059,.T.) ;
#34990 = EDGE_CURVE('',#29772,#29781,#8060,.T.) ;
#34991 = EDGE_CURVE('',#29782,#29783,#8061,.T.) ;
#34992 = EDGE_CURVE('',#29783,#29784,#8062,.T.) ;
#34993 = EDGE_CURVE('',#29784,#29785,#8063,.T.) ;
#34994 = EDGE_CURVE('',#29785,#29782,#8064,.T.) ;
#34995 = EDGE_CURVE('',#29786,#29787,#8065,.T.) ;
#34996 = EDGE_CURVE('',#29787,#29788,#8066,.T.) ;
#34997 = EDGE_CURVE('',#29788,#29789,#8067,.T.) ;
#34998 = EDGE_CURVE('',#29789,#29786,#8068,.T.) ;
#34999 = EDGE_CURVE('',#29790,#29791,#8069,.T.) ;
#35000 = EDGE_CURVE('',#29791,#29792,#8070,.T.) ;
#35001 = EDGE_CURVE('',#29792,#29793,#8071,.T.) ;
#35002 = EDGE_CURVE('',#29793,#29790,#8072,.T.) ;
#35003 = EDGE_CURVE('',#29794,#29795,#8073,.T.) ;
#35004 = EDGE_CURVE('',#29795,#29796,#8074,.T.) ;
#35005 = EDGE_CURVE('',#29796,#29797,#8075,.T.) ;
#35006 = EDGE_CURVE('',#29797,#29794,#8076,.T.) ;
#35007 = EDGE_CURVE('',#29798,#29799,#8077,.T.) ;
#35008 = EDGE_CURVE('',#29799,#29800,#8078,.T.) ;
#35009 = EDGE_CURVE('',#29800,#29801,#8079,.T.) ;
#35010 = EDGE_CURVE('',#29801,#29798,#8080,.T.) ;
#35011 = EDGE_CURVE('',#29788,#29802,#24853,.T.) ;
#35012 = EDGE_CURVE('',#29803,#29802,#8081,.T.) ;
#35013 = EDGE_CURVE('',#29803,#29789,#24854,.T.) ;
#35014 = EDGE_CURVE('',#29698,#29772,#24855,.T.) ;
#35015 = EDGE_CURVE('',#29772,#29765,#8082,.T.) ;
#35016 = EDGE_CURVE('',#29628,#29765,#24856,.T.) ;
#35017 = EDGE_CURVE('',#29628,#29698,#8083,.T.) ;
#35018 = EDGE_CURVE('',#29764,#29629,#24857,.T.) ;
#35019 = EDGE_CURVE('',#29697,#29773,#24858,.T.) ;
#35020 = EDGE_CURVE('',#29804,#29805,#8084,.T.) ;
#35021 = EDGE_CURVE('',#29805,#29806,#8085,.T.) ;
#35022 = EDGE_CURVE('',#29806,#29807,#8086,.T.) ;
#35023 = EDGE_CURVE('',#29807,#29804,#8087,.T.) ;
#35024 = EDGE_CURVE('',#29808,#29809,#8088,.T.) ;
#35025 = EDGE_CURVE('',#29809,#29810,#8089,.T.) ;
#35026 = EDGE_CURVE('',#29810,#29811,#8090,.T.) ;
#35027 = EDGE_CURVE('',#29811,#29808,#8091,.T.) ;
#35028 = EDGE_CURVE('',#29812,#29813,#8092,.T.) ;
#35029 = EDGE_CURVE('',#29813,#29814,#8093,.T.) ;
#35030 = EDGE_CURVE('',#29814,#29815,#8094,.T.) ;
#35031 = EDGE_CURVE('',#29815,#29812,#8095,.T.) ;
#35032 = EDGE_CURVE('',#29816,#29817,#8096,.T.) ;
#35033 = EDGE_CURVE('',#29817,#29818,#8097,.T.) ;
#35034 = EDGE_CURVE('',#29818,#29819,#8098,.T.) ;
#35035 = EDGE_CURVE('',#29819,#29816,#8099,.T.) ;
#35036 = EDGE_CURVE('',#29820,#29821,#8100,.T.) ;
#35037 = EDGE_CURVE('',#29821,#29822,#8101,.T.) ;
#35038 = EDGE_CURVE('',#29822,#29823,#8102,.T.) ;
#35039 = EDGE_CURVE('',#29823,#29820,#8103,.T.) ;
#35040 = EDGE_CURVE('',#29824,#29825,#8104,.T.) ;
#35041 = EDGE_CURVE('',#29825,#29826,#8105,.T.) ;
#35042 = EDGE_CURVE('',#29826,#29827,#8106,.T.) ;
#35043 = EDGE_CURVE('',#29827,#29824,#8107,.T.) ;
#35044 = EDGE_CURVE('',#29802,#29828,#8108,.T.) ;
#35045 = EDGE_CURVE('',#29828,#29829,#8109,.T.) ;
#35046 = EDGE_CURVE('',#29829,#29803,#8110,.T.) ;
#35047 = EDGE_CURVE('',#29638,#29699,#8111,.T.) ;
#35048 = EDGE_CURVE('',#29830,#29831,#8112,.T.) ;
#35049 = EDGE_CURVE('',#29831,#29832,#8113,.T.) ;
#35050 = EDGE_CURVE('',#29832,#29833,#8114,.T.) ;
#35051 = EDGE_CURVE('',#29833,#29830,#8115,.T.) ;
#35052 = EDGE_CURVE('',#29834,#29835,#8116,.T.) ;
#35053 = EDGE_CURVE('',#29835,#29836,#8117,.T.) ;
#35054 = EDGE_CURVE('',#29836,#29837,#8118,.T.) ;
#35055 = EDGE_CURVE('',#29837,#29834,#8119,.T.) ;
#35056 = EDGE_CURVE('',#29838,#29839,#8120,.T.) ;
#35057 = EDGE_CURVE('',#29839,#29840,#8121,.T.) ;
#35058 = EDGE_CURVE('',#29840,#29841,#8122,.T.) ;
#35059 = EDGE_CURVE('',#29841,#29838,#8123,.T.) ;
#35060 = EDGE_CURVE('',#29530,#29515,#8124,.T.) ;
#35061 = EDGE_CURVE('',#29531,#29514,#8125,.T.) ;
#35062 = EDGE_CURVE('',#29518,#29533,#8126,.T.) ;
#35063 = EDGE_CURVE('',#29532,#29519,#8127,.T.) ;
#35064 = EDGE_CURVE('',#29532,#29781,#24859,.T.) ;
#35065 = EDGE_CURVE('',#29781,#29766,#8128,.T.) ;
#35066 = EDGE_CURVE('',#29519,#29766,#24860,.T.) ;
#35067 = EDGE_CURVE('',#29772,#29531,#24861,.T.) ;
#35068 = EDGE_CURVE('',#29765,#29514,#24862,.T.) ;
#35069 = EDGE_CURVE('',#29842,#29843,#8129,.T.) ;
#35070 = EDGE_CURVE('',#29842,#29783,#24863,.T.) ;
#35071 = EDGE_CURVE('',#29782,#29843,#24864,.T.) ;
#35072 = EDGE_CURVE('',#29781,#29585,#24865,.T.) ;
#35073 = EDGE_CURVE('',#29585,#29545,#8130,.T.) ;
#35074 = EDGE_CURVE('',#29766,#29545,#24866,.T.) ;
#35075 = EDGE_CURVE('',#29544,#29767,#24867,.T.) ;
#35076 = EDGE_CURVE('',#29780,#29586,#24868,.T.) ;
#35077 = EDGE_CURVE('',#29844,#29845,#8131,.T.) ;
#35078 = EDGE_CURVE('',#29845,#29846,#8132,.T.) ;
#35079 = EDGE_CURVE('',#29846,#29847,#8133,.T.) ;
#35080 = EDGE_CURVE('',#29847,#29844,#8134,.T.) ;
#35081 = EDGE_CURVE('',#29848,#29849,#8135,.T.) ;
#35082 = EDGE_CURVE('',#29849,#29850,#8136,.T.) ;
#35083 = EDGE_CURVE('',#29850,#29851,#8137,.T.) ;
#35084 = EDGE_CURVE('',#29851,#29848,#8138,.T.) ;
#35085 = EDGE_CURVE('',#29852,#29853,#8139,.T.) ;
#35086 = EDGE_CURVE('',#29853,#29854,#8140,.T.) ;
#35087 = EDGE_CURVE('',#29854,#29855,#8141,.T.) ;
#35088 = EDGE_CURVE('',#29855,#29852,#8142,.T.) ;
#35089 = EDGE_CURVE('',#29856,#29857,#8143,.T.) ;
#35090 = EDGE_CURVE('',#29857,#29858,#8144,.T.) ;
#35091 = EDGE_CURVE('',#29858,#29859,#8145,.T.) ;
#35092 = EDGE_CURVE('',#29859,#29856,#8146,.T.) ;
#35093 = EDGE_CURVE('',#29860,#29861,#8147,.T.) ;
#35094 = EDGE_CURVE('',#29861,#29862,#8148,.T.) ;
#35095 = EDGE_CURVE('',#29862,#29863,#8149,.T.) ;
#35096 = EDGE_CURVE('',#29863,#29860,#8150,.T.) ;
#35097 = EDGE_CURVE('',#29864,#29865,#8151,.T.) ;
#35098 = EDGE_CURVE('',#29865,#29866,#8152,.T.) ;
#35099 = EDGE_CURVE('',#29866,#29867,#8153,.T.) ;
#35100 = EDGE_CURVE('',#29867,#29864,#8154,.T.) ;
#35101 = EDGE_CURVE('',#29595,#29546,#8155,.T.) ;
#35102 = EDGE_CURVE('',#29868,#29869,#8156,.T.) ;
#35103 = EDGE_CURVE('',#29869,#29842,#8157,.T.) ;
#35104 = EDGE_CURVE('',#29843,#29868,#8158,.T.) ;
#35105 = EDGE_CURVE('',#29870,#29871,#8159,.T.) ;
#35106 = EDGE_CURVE('',#29871,#29872,#8160,.T.) ;
#35107 = EDGE_CURVE('',#29872,#29873,#8161,.T.) ;
#35108 = EDGE_CURVE('',#29873,#29870,#8162,.T.) ;
#35109 = EDGE_CURVE('',#29874,#29875,#8163,.T.) ;
#35110 = EDGE_CURVE('',#29875,#29876,#8164,.T.) ;
#35111 = EDGE_CURVE('',#29876,#29877,#8165,.T.) ;
#35112 = EDGE_CURVE('',#29877,#29874,#8166,.T.) ;
#35113 = EDGE_CURVE('',#29878,#29879,#8167,.T.) ;
#35114 = EDGE_CURVE('',#29879,#29880,#8168,.T.) ;
#35115 = EDGE_CURVE('',#29880,#29881,#8169,.T.) ;
#35116 = EDGE_CURVE('',#29881,#29878,#8170,.T.) ;
#35117 = EDGE_CURVE('',#29882,#29883,#8171,.T.) ;
#35118 = EDGE_CURVE('',#29883,#29884,#8172,.T.) ;
#35119 = EDGE_CURVE('',#29884,#29885,#8173,.T.) ;
#35120 = EDGE_CURVE('',#29885,#29882,#8174,.T.) ;
#35121 = EDGE_CURVE('',#29886,#29887,#8175,.T.) ;
#35122 = EDGE_CURVE('',#29887,#29888,#8176,.T.) ;
#35123 = EDGE_CURVE('',#29888,#29889,#8177,.T.) ;
#35124 = EDGE_CURVE('',#29889,#29886,#8178,.T.) ;
#35125 = EDGE_CURVE('',#29890,#29891,#8179,.T.) ;
#35126 = EDGE_CURVE('',#29891,#29892,#8180,.T.) ;
#35127 = EDGE_CURVE('',#29892,#29893,#8181,.T.) ;
#35128 = EDGE_CURVE('',#29893,#29890,#8182,.T.) ;
#35129 = EDGE_CURVE('',#29894,#29895,#8183,.T.) ;
#35130 = EDGE_CURVE('',#29895,#29896,#8184,.T.) ;
#35131 = EDGE_CURVE('',#29896,#29897,#8185,.T.) ;
#35132 = EDGE_CURVE('',#29897,#29894,#8186,.T.) ;
#35133 = EDGE_CURVE('',#29898,#29899,#8187,.T.) ;
#35134 = EDGE_CURVE('',#29899,#29900,#8188,.T.) ;
#35135 = EDGE_CURVE('',#29900,#29901,#8189,.T.) ;
#35136 = EDGE_CURVE('',#29901,#29898,#8190,.T.) ;
#35137 = EDGE_CURVE('',#29902,#29903,#8191,.T.) ;
#35138 = EDGE_CURVE('',#29903,#29904,#8192,.T.) ;
#35139 = EDGE_CURVE('',#29904,#29905,#8193,.T.) ;
#35140 = EDGE_CURVE('',#29905,#29902,#8194,.T.) ;
#35141 = EDGE_CURVE('',#29906,#29907,#8195,.T.) ;
#35142 = EDGE_CURVE('',#29907,#29908,#8196,.T.) ;
#35143 = EDGE_CURVE('',#29908,#29909,#8197,.T.) ;
#35144 = EDGE_CURVE('',#29909,#29906,#8198,.T.) ;
#35145 = EDGE_CURVE('',#29910,#29911,#8199,.T.) ;
#35146 = EDGE_CURVE('',#29911,#29912,#8200,.T.) ;
#35147 = EDGE_CURVE('',#29912,#29913,#8201,.T.) ;
#35148 = EDGE_CURVE('',#29913,#29910,#8202,.T.) ;
#35149 = EDGE_CURVE('',#29914,#29915,#8203,.T.) ;
#35150 = EDGE_CURVE('',#29915,#29916,#8204,.T.) ;
#35151 = EDGE_CURVE('',#29916,#29917,#8205,.T.) ;
#35152 = EDGE_CURVE('',#29917,#29914,#8206,.T.) ;
#35153 = EDGE_CURVE('',#29918,#29919,#8207,.T.) ;
#35154 = EDGE_CURVE('',#29919,#29920,#8208,.T.) ;
#35155 = EDGE_CURVE('',#29920,#29921,#8209,.T.) ;
#35156 = EDGE_CURVE('',#29921,#29918,#8210,.T.) ;
#35157 = EDGE_CURVE('',#29922,#29923,#8211,.T.) ;
#35158 = EDGE_CURVE('',#29923,#29924,#8212,.T.) ;
#35159 = EDGE_CURVE('',#29924,#29925,#8213,.T.) ;
#35160 = EDGE_CURVE('',#29925,#29922,#8214,.T.) ;
#35161 = EDGE_CURVE('',#29926,#29927,#8215,.T.) ;
#35162 = EDGE_CURVE('',#29927,#29928,#8216,.T.) ;
#35163 = EDGE_CURVE('',#29928,#29929,#8217,.T.) ;
#35164 = EDGE_CURVE('',#29929,#29926,#8218,.T.) ;
#35165 = EDGE_CURVE('',#29930,#29931,#8219,.T.) ;
#35166 = EDGE_CURVE('',#29931,#29932,#8220,.T.) ;
#35167 = EDGE_CURVE('',#29932,#29933,#8221,.T.) ;
#35168 = EDGE_CURVE('',#29933,#29930,#8222,.T.) ;
#35169 = EDGE_CURVE('',#29934,#29935,#8223,.T.) ;
#35170 = EDGE_CURVE('',#29935,#29936,#8224,.T.) ;
#35171 = EDGE_CURVE('',#29936,#29937,#8225,.T.) ;
#35172 = EDGE_CURVE('',#29937,#29934,#8226,.T.) ;
#35173 = EDGE_CURVE('',#29938,#29939,#8227,.T.) ;
#35174 = EDGE_CURVE('',#29939,#29940,#8228,.T.) ;
#35175 = EDGE_CURVE('',#29940,#29941,#8229,.T.) ;
#35176 = EDGE_CURVE('',#29941,#29938,#8230,.T.) ;
#35177 = EDGE_CURVE('',#29942,#29943,#8231,.T.) ;
#35178 = EDGE_CURVE('',#29943,#29944,#8232,.T.) ;
#35179 = EDGE_CURVE('',#29944,#29945,#8233,.T.) ;
#35180 = EDGE_CURVE('',#29945,#29942,#8234,.T.) ;
#35181 = EDGE_CURVE('',#29946,#29947,#8235,.T.) ;
#35182 = EDGE_CURVE('',#29947,#29948,#8236,.T.) ;
#35183 = EDGE_CURVE('',#29948,#29949,#8237,.T.) ;
#35184 = EDGE_CURVE('',#29949,#29946,#8238,.T.) ;
#35185 = EDGE_CURVE('',#29950,#29951,#8239,.T.) ;
#35186 = EDGE_CURVE('',#29951,#29952,#8240,.T.) ;
#35187 = EDGE_CURVE('',#29952,#29953,#8241,.T.) ;
#35188 = EDGE_CURVE('',#29953,#29950,#8242,.T.) ;
#35189 = EDGE_CURVE('',#29954,#29955,#8243,.T.) ;
#35190 = EDGE_CURVE('',#29955,#29956,#8244,.T.) ;
#35191 = EDGE_CURVE('',#29956,#29957,#8245,.T.) ;
#35192 = EDGE_CURVE('',#29957,#29954,#8246,.T.) ;
#35193 = EDGE_CURVE('',#29958,#29959,#8247,.T.) ;
#35194 = EDGE_CURVE('',#29959,#29960,#8248,.T.) ;
#35195 = EDGE_CURVE('',#29960,#29961,#8249,.T.) ;
#35196 = EDGE_CURVE('',#29961,#29958,#8250,.T.) ;
#35197 = EDGE_CURVE('',#29962,#29963,#8251,.T.) ;
#35198 = EDGE_CURVE('',#29963,#29964,#8252,.T.) ;
#35199 = EDGE_CURVE('',#29964,#29965,#8253,.T.) ;
#35200 = EDGE_CURVE('',#29965,#29962,#8254,.T.) ;
#35201 = EDGE_CURVE('',#29966,#29967,#8255,.T.) ;
#35202 = EDGE_CURVE('',#29967,#29968,#8256,.T.) ;
#35203 = EDGE_CURVE('',#29968,#29969,#8257,.T.) ;
#35204 = EDGE_CURVE('',#29969,#29966,#8258,.T.) ;
#35205 = EDGE_CURVE('',#29970,#29971,#8259,.T.) ;
#35206 = EDGE_CURVE('',#29971,#29972,#8260,.T.) ;
#35207 = EDGE_CURVE('',#29972,#29973,#8261,.T.) ;
#35208 = EDGE_CURVE('',#29973,#29970,#8262,.T.) ;
#35209 = EDGE_CURVE('',#29974,#29975,#8263,.T.) ;
#35210 = EDGE_CURVE('',#29975,#29976,#8264,.T.) ;
#35211 = EDGE_CURVE('',#29976,#29977,#8265,.T.) ;
#35212 = EDGE_CURVE('',#29977,#29974,#8266,.T.) ;
#35213 = EDGE_CURVE('',#29978,#29979,#8267,.T.) ;
#35214 = EDGE_CURVE('',#29979,#29980,#8268,.T.) ;
#35215 = EDGE_CURVE('',#29980,#29981,#8269,.T.) ;
#35216 = EDGE_CURVE('',#29981,#29978,#8270,.T.) ;
#35217 = EDGE_CURVE('',#29982,#29983,#8271,.T.) ;
#35218 = EDGE_CURVE('',#29983,#29984,#8272,.T.) ;
#35219 = EDGE_CURVE('',#29984,#29985,#8273,.T.) ;
#35220 = EDGE_CURVE('',#29985,#29982,#8274,.T.) ;
#35221 = EDGE_CURVE('',#29986,#29987,#8275,.T.) ;
#35222 = EDGE_CURVE('',#29987,#29988,#8276,.T.) ;
#35223 = EDGE_CURVE('',#29988,#29989,#8277,.T.) ;
#35224 = EDGE_CURVE('',#29989,#29986,#8278,.T.) ;
#35225 = EDGE_CURVE('',#29990,#29991,#8279,.T.) ;
#35226 = EDGE_CURVE('',#29991,#29992,#8280,.T.) ;
#35227 = EDGE_CURVE('',#29992,#29993,#8281,.T.) ;
#35228 = EDGE_CURVE('',#29993,#29990,#8282,.T.) ;
#35229 = EDGE_CURVE('',#29994,#29995,#8283,.T.) ;
#35230 = EDGE_CURVE('',#29995,#29996,#8284,.T.) ;
#35231 = EDGE_CURVE('',#29996,#29997,#8285,.T.) ;
#35232 = EDGE_CURVE('',#29997,#29994,#8286,.T.) ;
#35233 = EDGE_CURVE('',#29998,#29999,#8287,.T.) ;
#35234 = EDGE_CURVE('',#29999,#30000,#8288,.T.) ;
#35235 = EDGE_CURVE('',#30000,#30001,#8289,.T.) ;
#35236 = EDGE_CURVE('',#30001,#29998,#8290,.T.) ;
#35237 = EDGE_CURVE('',#30002,#30003,#8291,.T.) ;
#35238 = EDGE_CURVE('',#30003,#30004,#8292,.T.) ;
#35239 = EDGE_CURVE('',#30004,#30005,#8293,.T.) ;
#35240 = EDGE_CURVE('',#30005,#30002,#8294,.T.) ;
#35241 = EDGE_CURVE('',#30006,#30007,#8295,.T.) ;
#35242 = EDGE_CURVE('',#30007,#30008,#8296,.T.) ;
#35243 = EDGE_CURVE('',#30008,#30009,#8297,.T.) ;
#35244 = EDGE_CURVE('',#30009,#30006,#8298,.T.) ;
#35245 = EDGE_CURVE('',#30010,#30011,#8299,.T.) ;
#35246 = EDGE_CURVE('',#30011,#30012,#8300,.T.) ;
#35247 = EDGE_CURVE('',#30012,#30013,#8301,.T.) ;
#35248 = EDGE_CURVE('',#30013,#30010,#8302,.T.) ;
#35249 = EDGE_CURVE('',#30014,#30015,#8303,.T.) ;
#35250 = EDGE_CURVE('',#30015,#30016,#8304,.T.) ;
#35251 = EDGE_CURVE('',#30016,#30017,#8305,.T.) ;
#35252 = EDGE_CURVE('',#30017,#30014,#8306,.T.) ;
#35253 = EDGE_CURVE('',#30018,#30019,#8307,.T.) ;
#35254 = EDGE_CURVE('',#30019,#30020,#8308,.T.) ;
#35255 = EDGE_CURVE('',#30020,#30021,#8309,.T.) ;
#35256 = EDGE_CURVE('',#30021,#30018,#8310,.T.) ;
#35257 = EDGE_CURVE('',#30022,#30023,#8311,.T.) ;
#35258 = EDGE_CURVE('',#30023,#30024,#8312,.T.) ;
#35259 = EDGE_CURVE('',#30024,#30025,#8313,.T.) ;
#35260 = EDGE_CURVE('',#30025,#30022,#8314,.T.) ;
#35261 = EDGE_CURVE('',#30026,#30027,#8315,.T.) ;
#35262 = EDGE_CURVE('',#30027,#30028,#8316,.T.) ;
#35263 = EDGE_CURVE('',#30028,#30029,#8317,.T.) ;
#35264 = EDGE_CURVE('',#30029,#30026,#8318,.T.) ;
#35265 = EDGE_CURVE('',#30030,#30031,#8319,.T.) ;
#35266 = EDGE_CURVE('',#30031,#30032,#8320,.T.) ;
#35267 = EDGE_CURVE('',#30032,#30033,#8321,.T.) ;
#35268 = EDGE_CURVE('',#30033,#30030,#8322,.T.) ;
#35269 = EDGE_CURVE('',#30034,#30035,#8323,.T.) ;
#35270 = EDGE_CURVE('',#30035,#30036,#8324,.T.) ;
#35271 = EDGE_CURVE('',#30036,#30037,#8325,.T.) ;
#35272 = EDGE_CURVE('',#30037,#30034,#8326,.T.) ;
#35273 = EDGE_CURVE('',#30038,#30039,#8327,.T.) ;
#35274 = EDGE_CURVE('',#30039,#30040,#8328,.T.) ;
#35275 = EDGE_CURVE('',#30040,#30041,#8329,.T.) ;
#35276 = EDGE_CURVE('',#30041,#30038,#8330,.T.) ;
#35277 = EDGE_CURVE('',#30042,#30043,#8331,.T.) ;
#35278 = EDGE_CURVE('',#30043,#30044,#8332,.T.) ;
#35279 = EDGE_CURVE('',#30044,#30045,#8333,.T.) ;
#35280 = EDGE_CURVE('',#30045,#30042,#8334,.T.) ;
#35281 = EDGE_CURVE('',#30046,#30047,#8335,.T.) ;
#35282 = EDGE_CURVE('',#30047,#30048,#8336,.T.) ;
#35283 = EDGE_CURVE('',#30048,#30049,#8337,.T.) ;
#35284 = EDGE_CURVE('',#30049,#30046,#8338,.T.) ;
#35285 = EDGE_CURVE('',#30050,#30051,#8339,.T.) ;
#35286 = EDGE_CURVE('',#30051,#30052,#8340,.T.) ;
#35287 = EDGE_CURVE('',#30052,#30053,#8341,.T.) ;
#35288 = EDGE_CURVE('',#30053,#30050,#8342,.T.) ;
#35289 = EDGE_CURVE('',#30054,#30055,#8343,.T.) ;
#35290 = EDGE_CURVE('',#30055,#30056,#8344,.T.) ;
#35291 = EDGE_CURVE('',#30056,#30057,#8345,.T.) ;
#35292 = EDGE_CURVE('',#30057,#30054,#8346,.T.) ;
#35293 = EDGE_CURVE('',#30058,#30059,#8347,.T.) ;
#35294 = EDGE_CURVE('',#30059,#30060,#8348,.T.) ;
#35295 = EDGE_CURVE('',#30060,#30061,#8349,.T.) ;
#35296 = EDGE_CURVE('',#30061,#30058,#8350,.T.) ;
#35297 = EDGE_CURVE('',#29547,#29865,#24869,.T.) ;
#35298 = EDGE_CURVE('',#29866,#29546,#4840,.T.) ;
#35299 = EDGE_CURVE('',#29867,#29595,#4841,.T.) ;
#35300 = EDGE_CURVE('',#29547,#29863,#24870,.T.) ;
#35301 = EDGE_CURVE('',#29863,#29865,#24871,.T.) ;
#35302 = EDGE_CURVE('',#29864,#29594,#24872,.T.) ;
#35303 = EDGE_CURVE('',#29860,#29864,#24873,.T.) ;
#35304 = EDGE_CURVE('',#29548,#29862,#24874,.T.) ;
#35305 = EDGE_CURVE('',#29860,#29594,#24875,.T.) ;
#35306 = EDGE_CURVE('',#29548,#29859,#24876,.T.) ;
#35307 = EDGE_CURVE('',#29859,#29862,#24877,.T.) ;
#35308 = EDGE_CURVE('',#29861,#29593,#24878,.T.) ;
#35309 = EDGE_CURVE('',#29856,#29861,#24879,.T.) ;
#35310 = EDGE_CURVE('',#29549,#29858,#24880,.T.) ;
#35311 = EDGE_CURVE('',#29856,#29593,#24881,.T.) ;
#35312 = EDGE_CURVE('',#29855,#29858,#24882,.T.) ;
#35313 = EDGE_CURVE('',#29550,#29855,#24883,.T.) ;
#35314 = EDGE_CURVE('',#29857,#29592,#24884,.T.) ;
#35315 = EDGE_CURVE('',#29852,#29857,#24885,.T.) ;
#35316 = EDGE_CURVE('',#29551,#29854,#24886,.T.) ;
#35317 = EDGE_CURVE('',#29852,#29591,#24887,.T.) ;
#35318 = EDGE_CURVE('',#29551,#29851,#24888,.T.) ;
#35319 = EDGE_CURVE('',#29851,#29854,#24889,.T.) ;
#35320 = EDGE_CURVE('',#29853,#29590,#24890,.T.) ;
#35321 = EDGE_CURVE('',#29848,#29853,#24891,.T.) ;
#35322 = EDGE_CURVE('',#29552,#29850,#24892,.T.) ;
#35323 = EDGE_CURVE('',#29848,#29590,#24893,.T.) ;
#35324 = EDGE_CURVE('',#29552,#29847,#24894,.T.) ;
#35325 = EDGE_CURVE('',#29847,#29850,#24895,.T.) ;
#35326 = EDGE_CURVE('',#29849,#29589,#24896,.T.) ;
#35327 = EDGE_CURVE('',#29844,#29849,#24897,.T.) ;
#35328 = EDGE_CURVE('',#29543,#29846,#24898,.T.) ;
#35329 = EDGE_CURVE('',#29638,#29824,#4842,.T.) ;
#35330 = EDGE_CURVE('',#29825,#29637,#24899,.T.) ;
#35331 = EDGE_CURVE('',#29844,#29589,#24900,.T.) ;
#35332 = EDGE_CURVE('',#29868,#29846,#24901,.T.) ;
#35333 = EDGE_CURVE('',#29542,#29868,#24902,.T.) ;
#35334 = EDGE_CURVE('',#29825,#29807,#24903,.T.) ;
#35335 = EDGE_CURVE('',#29807,#29637,#24904,.T.) ;
#35336 = EDGE_CURVE('',#29699,#29827,#4843,.T.) ;
#35337 = EDGE_CURVE('',#29845,#29588,#24905,.T.) ;
#35338 = EDGE_CURVE('',#29869,#29845,#24906,.T.) ;
#35339 = EDGE_CURVE('',#29544,#29843,#24907,.T.) ;
#35340 = EDGE_CURVE('',#29804,#29636,#24908,.T.) ;
#35341 = EDGE_CURVE('',#29826,#29806,#24909,.T.) ;
#35342 = EDGE_CURVE('',#29700,#29826,#24910,.T.) ;
#35343 = EDGE_CURVE('',#29869,#29587,#24911,.T.) ;
#35344 = EDGE_CURVE('',#29767,#29782,#24912,.T.) ;
#35345 = EDGE_CURVE('',#29804,#29810,#24913,.T.) ;
#35346 = EDGE_CURVE('',#29810,#29636,#24914,.T.) ;
#35347 = EDGE_CURVE('',#29700,#29806,#24915,.T.) ;
#35348 = EDGE_CURVE('',#29842,#29586,#24916,.T.) ;
#35349 = EDGE_CURVE('',#29768,#29785,#24917,.T.) ;
#35350 = EDGE_CURVE('',#29811,#29635,#24918,.T.) ;
#35351 = EDGE_CURVE('',#29805,#29809,#24919,.T.) ;
#35352 = EDGE_CURVE('',#29701,#29805,#24920,.T.) ;
#35353 = EDGE_CURVE('',#29783,#29780,#24921,.T.) ;
#35354 = EDGE_CURVE('',#29797,#29785,#24922,.T.) ;
#35355 = EDGE_CURVE('',#29769,#29797,#24923,.T.) ;
#35356 = EDGE_CURVE('',#29814,#29634,#24924,.T.) ;
#35357 = EDGE_CURVE('',#29811,#29814,#24925,.T.) ;
#35358 = EDGE_CURVE('',#29701,#29809,#24926,.T.) ;
#35359 = EDGE_CURVE('',#29784,#29779,#24927,.T.) ;
#35360 = EDGE_CURVE('',#29794,#29784,#24928,.T.) ;
#35361 = EDGE_CURVE('',#29770,#29796,#24929,.T.) ;
#35362 = EDGE_CURVE('',#29815,#29633,#24930,.T.) ;
#35363 = EDGE_CURVE('',#29808,#29813,#24931,.T.) ;
#35364 = EDGE_CURVE('',#29702,#29808,#24932,.T.) ;
#35365 = EDGE_CURVE('',#29794,#29778,#24933,.T.) ;
#35366 = EDGE_CURVE('',#29770,#29793,#24934,.T.) ;
#35367 = EDGE_CURVE('',#29793,#29796,#24935,.T.) ;
#35368 = EDGE_CURVE('',#29815,#29818,#24936,.T.) ;
#35369 = EDGE_CURVE('',#29818,#29633,#24937,.T.) ;
#35370 = EDGE_CURVE('',#29703,#29813,#24938,.T.) ;
#35371 = EDGE_CURVE('',#29795,#29777,#24939,.T.) ;
#35372 = EDGE_CURVE('',#29790,#29795,#24940,.T.) ;
#35373 = EDGE_CURVE('',#29771,#29792,#24941,.T.) ;
#35374 = EDGE_CURVE('',#29819,#29632,#24942,.T.) ;
#35375 = EDGE_CURVE('',#29812,#29817,#24943,.T.) ;
#35376 = EDGE_CURVE('',#29704,#29812,#24944,.T.) ;
#35377 = EDGE_CURVE('',#29790,#29777,#24945,.T.) ;
#35378 = EDGE_CURVE('',#29771,#29801,#24946,.T.) ;
#35379 = EDGE_CURVE('',#29801,#29792,#24947,.T.) ;
#35380 = EDGE_CURVE('',#29629,#29803,#24948,.T.) ;
#35381 = EDGE_CURVE('',#29789,#29764,#24949,.T.) ;
#35382 = EDGE_CURVE('',#29819,#29822,#24950,.T.) ;
#35383 = EDGE_CURVE('',#29822,#29632,#24951,.T.) ;
#35384 = EDGE_CURVE('',#29704,#29817,#24952,.T.) ;
#35385 = EDGE_CURVE('',#29791,#29776,#24953,.T.) ;
#35386 = EDGE_CURVE('',#29798,#29791,#24954,.T.) ;
#35387 = EDGE_CURVE('',#29763,#29800,#24955,.T.) ;
#35388 = EDGE_CURVE('',#29786,#29762,#24956,.T.) ;
#35389 = EDGE_CURVE('',#29630,#29829,#24957,.T.) ;
#35390 = EDGE_CURVE('',#29823,#29631,#24958,.T.) ;
#35391 = EDGE_CURVE('',#29816,#29821,#24959,.T.) ;
#35392 = EDGE_CURVE('',#29705,#29816,#24960,.T.) ;
#35393 = EDGE_CURVE('',#29798,#29776,#24961,.T.) ;
#35394 = EDGE_CURVE('',#29786,#29800,#24962,.T.) ;
#35395 = EDGE_CURVE('',#29823,#29829,#24963,.T.) ;
#35396 = EDGE_CURVE('',#29705,#29821,#24964,.T.) ;
#35397 = EDGE_CURVE('',#29799,#29775,#24965,.T.) ;
#35398 = EDGE_CURVE('',#29787,#29799,#24966,.T.) ;
#35399 = EDGE_CURVE('',#29820,#29828,#24967,.T.) ;
#35400 = EDGE_CURVE('',#29696,#29820,#24968,.T.) ;
#35401 = EDGE_CURVE('',#29787,#29774,#24969,.T.) ;
#35402 = EDGE_CURVE('',#29695,#29828,#24970,.T.) ;
#35403 = EDGE_CURVE('',#29788,#29773,#24971,.T.) ;
#35404 = EDGE_CURVE('',#29697,#29802,#24972,.T.) ;
#35405 = EDGE_CURVE('',#29562,#30044,#24973,.T.) ;
#35406 = EDGE_CURVE('',#30045,#29568,#24974,.T.) ;
#35407 = EDGE_CURVE('',#30031,#30044,#24975,.T.) ;
#35408 = EDGE_CURVE('',#29561,#30031,#24976,.T.) ;
#35409 = EDGE_CURVE('',#30038,#29567,#24977,.T.) ;
#35410 = EDGE_CURVE('',#30045,#30038,#24978,.T.) ;
#35411 = EDGE_CURVE('',#30032,#30043,#24979,.T.) ;
#35412 = EDGE_CURVE('',#29563,#30030,#24980,.T.) ;
#35413 = EDGE_CURVE('',#29565,#30034,#24981,.T.) ;
#35414 = EDGE_CURVE('',#30035,#29564,#24982,.T.) ;
#35415 = EDGE_CURVE('',#30039,#29566,#24983,.T.) ;
#35416 = EDGE_CURVE('',#30042,#30041,#24984,.T.) ;
#35417 = EDGE_CURVE('',#29608,#30042,#24985,.T.) ;
#35418 = EDGE_CURVE('',#30043,#29607,#24986,.T.) ;
#35419 = EDGE_CURVE('',#30032,#29606,#24987,.T.) ;
#35420 = EDGE_CURVE('',#30035,#30030,#24988,.T.) ;
#35421 = EDGE_CURVE('',#30039,#30034,#24989,.T.) ;
#35422 = EDGE_CURVE('',#29609,#30041,#24990,.T.) ;
#35423 = EDGE_CURVE('',#30033,#29604,#24991,.T.) ;
#35424 = EDGE_CURVE('',#30036,#30033,#24992,.T.) ;
#35425 = EDGE_CURVE('',#30040,#30037,#24993,.T.) ;
#35426 = EDGE_CURVE('',#29610,#30040,#24994,.T.) ;
#35427 = EDGE_CURVE('',#30036,#29605,#24995,.T.) ;
#35428 = EDGE_CURVE('',#29611,#30037,#24996,.T.) ;
#35429 = EDGE_CURVE('',#29570,#30016,#24997,.T.) ;
#35430 = EDGE_CURVE('',#30017,#29576,#24998,.T.) ;
#35431 = EDGE_CURVE('',#30019,#30016,#24999,.T.) ;
#35432 = EDGE_CURVE('',#29569,#30019,#25000,.T.) ;
#35433 = EDGE_CURVE('',#30026,#29575,#25001,.T.) ;
#35434 = EDGE_CURVE('',#30017,#30026,#25002,.T.) ;
#35435 = EDGE_CURVE('',#30020,#30015,#25003,.T.) ;
#35436 = EDGE_CURVE('',#29571,#30018,#25004,.T.) ;
#35437 = EDGE_CURVE('',#29573,#30022,#25005,.T.) ;
#35438 = EDGE_CURVE('',#30023,#29572,#25006,.T.) ;
#35439 = EDGE_CURVE('',#30027,#29574,#25007,.T.) ;
#35440 = EDGE_CURVE('',#30014,#30029,#25008,.T.) ;
#35441 = EDGE_CURVE('',#29616,#30014,#25009,.T.) ;
#35442 = EDGE_CURVE('',#30015,#29615,#25010,.T.) ;
#35443 = EDGE_CURVE('',#30020,#29614,#25011,.T.) ;
#35444 = EDGE_CURVE('',#30023,#30018,#25012,.T.) ;
#35445 = EDGE_CURVE('',#30027,#30022,#25013,.T.) ;
#35446 = EDGE_CURVE('',#29617,#30029,#25014,.T.) ;
#35447 = EDGE_CURVE('',#30021,#29612,#25015,.T.) ;
#35448 = EDGE_CURVE('',#30024,#30021,#25016,.T.) ;
#35449 = EDGE_CURVE('',#30028,#30025,#25017,.T.) ;
#35450 = EDGE_CURVE('',#29618,#30028,#25018,.T.) ;
#35451 = EDGE_CURVE('',#30024,#29613,#25019,.T.) ;
#35452 = EDGE_CURVE('',#29619,#30025,#25020,.T.) ;
#35453 = EDGE_CURVE('',#29554,#30000,#25021,.T.) ;
#35454 = EDGE_CURVE('',#30001,#29560,#25022,.T.) ;
#35455 = EDGE_CURVE('',#30011,#30000,#25023,.T.) ;
#35456 = EDGE_CURVE('',#29553,#30011,#25024,.T.) ;
#35457 = EDGE_CURVE('',#30002,#29559,#25025,.T.) ;
#35458 = EDGE_CURVE('',#30001,#30002,#25026,.T.) ;
#35459 = EDGE_CURVE('',#30012,#29999,#25027,.T.) ;
#35460 = EDGE_CURVE('',#29555,#30010,#25028,.T.) ;
#35461 = EDGE_CURVE('',#29557,#30006,#25029,.T.) ;
#35462 = EDGE_CURVE('',#30007,#29556,#25030,.T.) ;
#35463 = EDGE_CURVE('',#30003,#29558,#25031,.T.) ;
#35464 = EDGE_CURVE('',#29998,#30005,#25032,.T.) ;
#35465 = EDGE_CURVE('',#29600,#29998,#25033,.T.) ;
#35466 = EDGE_CURVE('',#29999,#29599,#25034,.T.) ;
#35467 = EDGE_CURVE('',#30012,#29598,#25035,.T.) ;
#35468 = EDGE_CURVE('',#30007,#30010,#25036,.T.) ;
#35469 = EDGE_CURVE('',#30003,#30006,#25037,.T.) ;
#35470 = EDGE_CURVE('',#29601,#30005,#25038,.T.) ;
#35471 = EDGE_CURVE('',#30013,#29596,#25039,.T.) ;
#35472 = EDGE_CURVE('',#30008,#30013,#25040,.T.) ;
#35473 = EDGE_CURVE('',#30004,#30009,#25041,.T.) ;
#35474 = EDGE_CURVE('',#29602,#30004,#25042,.T.) ;
#35475 = EDGE_CURVE('',#30008,#29597,#25043,.T.) ;
#35476 = EDGE_CURVE('',#29603,#30009,#25044,.T.) ;
#35477 = EDGE_CURVE('',#29578,#29984,#25045,.T.) ;
#35478 = EDGE_CURVE('',#29985,#29584,#25046,.T.) ;
#35479 = EDGE_CURVE('',#29987,#29984,#25047,.T.) ;
#35480 = EDGE_CURVE('',#29577,#29987,#25048,.T.) ;
#35481 = EDGE_CURVE('',#29994,#29583,#25049,.T.) ;
#35482 = EDGE_CURVE('',#29985,#29994,#25050,.T.) ;
#35483 = EDGE_CURVE('',#29988,#29983,#25051,.T.) ;
#35484 = EDGE_CURVE('',#29579,#29986,#25052,.T.) ;
#35485 = EDGE_CURVE('',#29581,#29990,#25053,.T.) ;
#35486 = EDGE_CURVE('',#29991,#29580,#25054,.T.) ;
#35487 = EDGE_CURVE('',#29995,#29582,#25055,.T.) ;
#35488 = EDGE_CURVE('',#29982,#29997,#25056,.T.) ;
#35489 = EDGE_CURVE('',#29624,#29982,#25057,.T.) ;
#35490 = EDGE_CURVE('',#29983,#29623,#25058,.T.) ;
#35491 = EDGE_CURVE('',#29988,#29622,#25059,.T.) ;
#35492 = EDGE_CURVE('',#29991,#29986,#25060,.T.) ;
#35493 = EDGE_CURVE('',#29995,#29990,#25061,.T.) ;
#35494 = EDGE_CURVE('',#29625,#29997,#25062,.T.) ;
#35495 = EDGE_CURVE('',#29989,#29620,#25063,.T.) ;
#35496 = EDGE_CURVE('',#29992,#29989,#25064,.T.) ;
#35497 = EDGE_CURVE('',#29996,#29993,#25065,.T.) ;
#35498 = EDGE_CURVE('',#29626,#29996,#25066,.T.) ;
#35499 = EDGE_CURVE('',#29992,#29621,#25067,.T.) ;
#35500 = EDGE_CURVE('',#29627,#29993,#25068,.T.) ;
#35501 = EDGE_CURVE('',#29524,#30050,#25069,.T.) ;
#35502 = EDGE_CURVE('',#30051,#29523,#25070,.T.) ;
#35503 = EDGE_CURVE('',#30049,#29522,#25071,.T.) ;
#35504 = EDGE_CURVE('',#30051,#30049,#25072,.T.) ;
#35505 = EDGE_CURVE('',#30054,#30050,#25073,.T.) ;
#35506 = EDGE_CURVE('',#29525,#30054,#25074,.T.) ;
#35507 = EDGE_CURVE('',#30046,#29520,#25075,.T.) ;
#35508 = EDGE_CURVE('',#30052,#30048,#25076,.T.) ;
#35509 = EDGE_CURVE('',#30053,#29541,#25077,.T.) ;
#35510 = EDGE_CURVE('',#29535,#30052,#25078,.T.) ;
#35511 = EDGE_CURVE('',#30055,#30053,#25079,.T.) ;
#35512 = EDGE_CURVE('',#29526,#30057,#25080,.T.) ;
#35513 = EDGE_CURVE('',#29521,#30060,#25081,.T.) ;
#35514 = EDGE_CURVE('',#30061,#29527,#25082,.T.) ;
#35515 = EDGE_CURVE('',#30046,#30060,#25083,.T.) ;
#35516 = EDGE_CURVE('',#29534,#30048,#25084,.T.) ;
#35517 = EDGE_CURVE('',#30055,#29540,#25085,.T.) ;
#35518 = EDGE_CURVE('',#30061,#30057,#25086,.T.) ;
#35519 = EDGE_CURVE('',#30047,#30059,#25087,.T.) ;
#35520 = EDGE_CURVE('',#29536,#30047,#25088,.T.) ;
#35521 = EDGE_CURVE('',#30056,#29539,#25089,.T.) ;
#35522 = EDGE_CURVE('',#30058,#30056,#25090,.T.) ;
#35523 = EDGE_CURVE('',#29537,#30059,#25091,.T.) ;
#35524 = EDGE_CURVE('',#30058,#29538,#25092,.T.) ;
#35525 = EDGE_CURVE('',#29664,#29880,#25093,.T.) ;
#35526 = EDGE_CURVE('',#29881,#29670,#25094,.T.) ;
#35527 = EDGE_CURVE('',#29883,#29880,#25095,.T.) ;
#35528 = EDGE_CURVE('',#29663,#29883,#25096,.T.) ;
#35529 = EDGE_CURVE('',#29874,#29669,#25097,.T.) ;
#35530 = EDGE_CURVE('',#29881,#29874,#25098,.T.) ;
#35531 = EDGE_CURVE('',#29884,#29879,#25099,.T.) ;
#35532 = EDGE_CURVE('',#29665,#29882,#25100,.T.) ;
#35533 = EDGE_CURVE('',#29667,#29870,#25101,.T.) ;
#35534 = EDGE_CURVE('',#29871,#29666,#25102,.T.) ;
#35535 = EDGE_CURVE('',#29875,#29668,#25103,.T.) ;
#35536 = EDGE_CURVE('',#29878,#29877,#25104,.T.) ;
#35537 = EDGE_CURVE('',#29734,#29878,#25105,.T.) ;
#35538 = EDGE_CURVE('',#29879,#29733,#25106,.T.) ;
#35539 = EDGE_CURVE('',#29884,#29732,#25107,.T.) ;
#35540 = EDGE_CURVE('',#29871,#29882,#25108,.T.) ;
#35541 = EDGE_CURVE('',#29875,#29870,#25109,.T.) ;
#35542 = EDGE_CURVE('',#29735,#29877,#25110,.T.) ;
#35543 = EDGE_CURVE('',#29885,#29730,#25111,.T.) ;
#35544 = EDGE_CURVE('',#29872,#29885,#25112,.T.) ;
#35545 = EDGE_CURVE('',#29876,#29873,#25113,.T.) ;
#35546 = EDGE_CURVE('',#29736,#29876,#25114,.T.) ;
#35547 = EDGE_CURVE('',#29872,#29731,#25115,.T.) ;
#35548 = EDGE_CURVE('',#29737,#29873,#25116,.T.) ;
#35549 = EDGE_CURVE('',#29672,#29896,#25117,.T.) ;
#35550 = EDGE_CURVE('',#29897,#29678,#25118,.T.) ;
#35551 = EDGE_CURVE('',#29899,#29896,#25119,.T.) ;
#35552 = EDGE_CURVE('',#29671,#29899,#25120,.T.) ;
#35553 = EDGE_CURVE('',#29890,#29677,#25121,.T.) ;
#35554 = EDGE_CURVE('',#29897,#29890,#25122,.T.) ;
#35555 = EDGE_CURVE('',#29900,#29895,#25123,.T.) ;
#35556 = EDGE_CURVE('',#29673,#29898,#25124,.T.) ;
#35557 = EDGE_CURVE('',#29675,#29886,#25125,.T.) ;
#35558 = EDGE_CURVE('',#29887,#29674,#25126,.T.) ;
#35559 = EDGE_CURVE('',#29891,#29676,#25127,.T.) ;
#35560 = EDGE_CURVE('',#29894,#29893,#25128,.T.) ;
#35561 = EDGE_CURVE('',#29742,#29894,#25129,.T.) ;
#35562 = EDGE_CURVE('',#29895,#29741,#25130,.T.) ;
#35563 = EDGE_CURVE('',#29900,#29740,#25131,.T.) ;
#35564 = EDGE_CURVE('',#29887,#29898,#25132,.T.) ;
#35565 = EDGE_CURVE('',#29891,#29886,#25133,.T.) ;
#35566 = EDGE_CURVE('',#29743,#29893,#25134,.T.) ;
#35567 = EDGE_CURVE('',#29901,#29738,#25135,.T.) ;
#35568 = EDGE_CURVE('',#29888,#29901,#25136,.T.) ;
#35569 = EDGE_CURVE('',#29892,#29889,#25137,.T.) ;
#35570 = EDGE_CURVE('',#29744,#29892,#25138,.T.) ;
#35571 = EDGE_CURVE('',#29888,#29739,#25139,.T.) ;
#35572 = EDGE_CURVE('',#29745,#29889,#25140,.T.) ;
#35573 = EDGE_CURVE('',#29656,#29912,#25141,.T.) ;
#35574 = EDGE_CURVE('',#29913,#29662,#25142,.T.) ;
#35575 = EDGE_CURVE('',#29915,#29912,#25143,.T.) ;
#35576 = EDGE_CURVE('',#29655,#29915,#25144,.T.) ;
#35577 = EDGE_CURVE('',#29906,#29661,#25145,.T.) ;
#35578 = EDGE_CURVE('',#29913,#29906,#25146,.T.) ;
#35579 = EDGE_CURVE('',#29916,#29911,#25147,.T.) ;
#35580 = EDGE_CURVE('',#29657,#29914,#25148,.T.) ;
#35581 = EDGE_CURVE('',#29659,#29902,#25149,.T.) ;
#35582 = EDGE_CURVE('',#29903,#29658,#25150,.T.) ;
#35583 = EDGE_CURVE('',#29907,#29660,#25151,.T.) ;
#35584 = EDGE_CURVE('',#29910,#29909,#25152,.T.) ;
#35585 = EDGE_CURVE('',#29726,#29910,#25153,.T.) ;
#35586 = EDGE_CURVE('',#29911,#29725,#25154,.T.) ;
#35587 = EDGE_CURVE('',#29916,#29724,#25155,.T.) ;
#35588 = EDGE_CURVE('',#29903,#29914,#25156,.T.) ;
#35589 = EDGE_CURVE('',#29907,#29902,#25157,.T.) ;
#35590 = EDGE_CURVE('',#29727,#29909,#25158,.T.) ;
#35591 = EDGE_CURVE('',#29917,#29722,#25159,.T.) ;
#35592 = EDGE_CURVE('',#29904,#29917,#25160,.T.) ;
#35593 = EDGE_CURVE('',#29908,#29905,#25161,.T.) ;
#35594 = EDGE_CURVE('',#29728,#29908,#25162,.T.) ;
#35595 = EDGE_CURVE('',#29904,#29723,#25163,.T.) ;
#35596 = EDGE_CURVE('',#29729,#29905,#25164,.T.) ;
#35597 = EDGE_CURVE('',#29680,#29928,#25165,.T.) ;
#35598 = EDGE_CURVE('',#29929,#29686,#25166,.T.) ;
#35599 = EDGE_CURVE('',#29931,#29928,#25167,.T.) ;
#35600 = EDGE_CURVE('',#29679,#29931,#25168,.T.) ;
#35601 = EDGE_CURVE('',#29922,#29685,#25169,.T.) ;
#35602 = EDGE_CURVE('',#29929,#29922,#25170,.T.) ;
#35603 = EDGE_CURVE('',#29932,#29927,#25171,.T.) ;
#35604 = EDGE_CURVE('',#29681,#29930,#25172,.T.) ;
#35605 = EDGE_CURVE('',#29683,#29918,#25173,.T.) ;
#35606 = EDGE_CURVE('',#29919,#29682,#25174,.T.) ;
#35607 = EDGE_CURVE('',#29923,#29684,#25175,.T.) ;
#35608 = EDGE_CURVE('',#29926,#29925,#25176,.T.) ;
#35609 = EDGE_CURVE('',#29750,#29926,#25177,.T.) ;
#35610 = EDGE_CURVE('',#29927,#29749,#25178,.T.) ;
#35611 = EDGE_CURVE('',#29932,#29748,#25179,.T.) ;
#35612 = EDGE_CURVE('',#29919,#29930,#25180,.T.) ;
#35613 = EDGE_CURVE('',#29923,#29918,#25181,.T.) ;
#35614 = EDGE_CURVE('',#29751,#29925,#25182,.T.) ;
#35615 = EDGE_CURVE('',#29933,#29746,#25183,.T.) ;
#35616 = EDGE_CURVE('',#29920,#29933,#25184,.T.) ;
#35617 = EDGE_CURVE('',#29924,#29921,#25185,.T.) ;
#35618 = EDGE_CURVE('',#29752,#29924,#25186,.T.) ;
#35619 = EDGE_CURVE('',#29920,#29747,#25187,.T.) ;
#35620 = EDGE_CURVE('',#29753,#29921,#25188,.T.) ;
#35621 = EDGE_CURVE('',#29648,#29944,#25189,.T.) ;
#35622 = EDGE_CURVE('',#29945,#29654,#25190,.T.) ;
#35623 = EDGE_CURVE('',#29947,#29944,#25191,.T.) ;
#35624 = EDGE_CURVE('',#29647,#29947,#25192,.T.) ;
#35625 = EDGE_CURVE('',#29938,#29653,#25193,.T.) ;
#35626 = EDGE_CURVE('',#29945,#29938,#25194,.T.) ;
#35627 = EDGE_CURVE('',#29948,#29943,#25195,.T.) ;
#35628 = EDGE_CURVE('',#29649,#29946,#25196,.T.) ;
#35629 = EDGE_CURVE('',#29651,#29934,#25197,.T.) ;
#35630 = EDGE_CURVE('',#29935,#29650,#25198,.T.) ;
#35631 = EDGE_CURVE('',#29939,#29652,#25199,.T.) ;
#35632 = EDGE_CURVE('',#29942,#29941,#25200,.T.) ;
#35633 = EDGE_CURVE('',#29718,#29942,#25201,.T.) ;
#35634 = EDGE_CURVE('',#29943,#29717,#25202,.T.) ;
#35635 = EDGE_CURVE('',#29948,#29716,#25203,.T.) ;
#35636 = EDGE_CURVE('',#29935,#29946,#25204,.T.) ;
#35637 = EDGE_CURVE('',#29939,#29934,#25205,.T.) ;
#35638 = EDGE_CURVE('',#29719,#29941,#25206,.T.) ;
#35639 = EDGE_CURVE('',#29949,#29714,#25207,.T.) ;
#35640 = EDGE_CURVE('',#29936,#29949,#25208,.T.) ;
#35641 = EDGE_CURVE('',#29940,#29937,#25209,.T.) ;
#35642 = EDGE_CURVE('',#29720,#29940,#25210,.T.) ;
#35643 = EDGE_CURVE('',#29936,#29715,#25211,.T.) ;
#35644 = EDGE_CURVE('',#29721,#29937,#25212,.T.) ;
#35645 = EDGE_CURVE('',#29688,#29952,#25213,.T.) ;
#35646 = EDGE_CURVE('',#29953,#29694,#25214,.T.) ;
#35647 = EDGE_CURVE('',#29955,#29952,#25215,.T.) ;
#35648 = EDGE_CURVE('',#29687,#29955,#25216,.T.) ;
#35649 = EDGE_CURVE('',#29962,#29693,#25217,.T.) ;
#35650 = EDGE_CURVE('',#29953,#29962,#25218,.T.) ;
#35651 = EDGE_CURVE('',#29956,#29951,#25219,.T.) ;
#35652 = EDGE_CURVE('',#29689,#29954,#25220,.T.) ;
#35653 = EDGE_CURVE('',#29691,#29958,#25221,.T.) ;
#35654 = EDGE_CURVE('',#29959,#29690,#25222,.T.) ;
#35655 = EDGE_CURVE('',#29963,#29692,#25223,.T.) ;
#35656 = EDGE_CURVE('',#29950,#29965,#25224,.T.) ;
#35657 = EDGE_CURVE('',#29758,#29950,#25225,.T.) ;
#35658 = EDGE_CURVE('',#29951,#29757,#25226,.T.) ;
#35659 = EDGE_CURVE('',#29956,#29756,#25227,.T.) ;
#35660 = EDGE_CURVE('',#29959,#29954,#25228,.T.) ;
#35661 = EDGE_CURVE('',#29963,#29958,#25229,.T.) ;
#35662 = EDGE_CURVE('',#29759,#29965,#25230,.T.) ;
#35663 = EDGE_CURVE('',#29957,#29754,#25231,.T.) ;
#35664 = EDGE_CURVE('',#29960,#29957,#25232,.T.) ;
#35665 = EDGE_CURVE('',#29964,#29961,#25233,.T.) ;
#35666 = EDGE_CURVE('',#29760,#29964,#25234,.T.) ;
#35667 = EDGE_CURVE('',#29960,#29755,#25235,.T.) ;
#35668 = EDGE_CURVE('',#29761,#29961,#25236,.T.) ;
#35669 = EDGE_CURVE('',#29640,#29980,#25237,.T.) ;
#35670 = EDGE_CURVE('',#29981,#29646,#25238,.T.) ;
#35671 = EDGE_CURVE('',#29967,#29980,#25239,.T.) ;
#35672 = EDGE_CURVE('',#29639,#29967,#25240,.T.) ;
#35673 = EDGE_CURVE('',#29974,#29645,#25241,.T.) ;
#35674 = EDGE_CURVE('',#29981,#29974,#25242,.T.) ;
#35675 = EDGE_CURVE('',#29968,#29979,#25243,.T.) ;
#35676 = EDGE_CURVE('',#29641,#29966,#25244,.T.) ;
#35677 = EDGE_CURVE('',#29643,#29970,#25245,.T.) ;
#35678 = EDGE_CURVE('',#29971,#29642,#25246,.T.) ;
#35679 = EDGE_CURVE('',#29975,#29644,#25247,.T.) ;
#35680 = EDGE_CURVE('',#29978,#29977,#25248,.T.) ;
#35681 = EDGE_CURVE('',#29710,#29978,#25249,.T.) ;
#35682 = EDGE_CURVE('',#29979,#29709,#25250,.T.) ;
#35683 = EDGE_CURVE('',#29968,#29708,#25251,.T.) ;
#35684 = EDGE_CURVE('',#29971,#29966,#25252,.T.) ;
#35685 = EDGE_CURVE('',#29975,#29970,#25253,.T.) ;
#35686 = EDGE_CURVE('',#29711,#29977,#25254,.T.) ;
#35687 = EDGE_CURVE('',#29969,#29706,#25255,.T.) ;
#35688 = EDGE_CURVE('',#29972,#29969,#25256,.T.) ;
#35689 = EDGE_CURVE('',#29976,#29973,#25257,.T.) ;
#35690 = EDGE_CURVE('',#29712,#29976,#25258,.T.) ;
#35691 = EDGE_CURVE('',#29972,#29707,#25259,.T.) ;
#35692 = EDGE_CURVE('',#29713,#29973,#25260,.T.) ;
#35693 = EDGE_CURVE('',#29530,#29840,#4844,.T.) ;
#35694 = EDGE_CURVE('',#29841,#29529,#25261,.T.) ;
#35695 = EDGE_CURVE('',#29528,#29832,#25262,.T.) ;
#35696 = EDGE_CURVE('',#29833,#29533,#4845,.T.) ;
#35697 = EDGE_CURVE('',#29529,#29836,#25263,.T.) ;
#35698 = EDGE_CURVE('',#29837,#29528,#25264,.T.) ;
#35699 = EDGE_CURVE('',#29841,#29836,#25265,.T.) ;
#35700 = EDGE_CURVE('',#29515,#29839,#4846,.T.) ;
#35701 = EDGE_CURVE('',#29830,#29518,#4847,.T.) ;
#35702 = EDGE_CURVE('',#29837,#29832,#25266,.T.) ;
#35703 = EDGE_CURVE('',#29838,#29835,#25267,.T.) ;
#35704 = EDGE_CURVE('',#29516,#29838,#25268,.T.) ;
#35705 = EDGE_CURVE('',#29831,#29517,#25269,.T.) ;
#35706 = EDGE_CURVE('',#29834,#29831,#25270,.T.) ;
#35707 = EDGE_CURVE('',#29516,#29835,#25271,.T.) ;
#35708 = EDGE_CURVE('',#29834,#29517,#25272,.T.) ;
#35709 = EDGE_CURVE('',#30062,#30063,#75,.T.) ;
#35710 = EDGE_CURVE('',#30063,#30064,#4848,.T.) ;
#35711 = EDGE_CURVE('',#30064,#30065,#25273,.T.) ;
#35712 = EDGE_CURVE('',#30066,#30065,#4849,.T.) ;
#35713 = EDGE_CURVE('',#30062,#30066,#76,.T.) ;
#35714 = EDGE_CURVE('',#30067,#30068,#77,.T.) ;
#35715 = EDGE_CURVE('',#30068,#30069,#25274,.T.) ;
#35716 = EDGE_CURVE('',#30070,#30069,#4850,.T.) ;
#35717 = EDGE_CURVE('',#30071,#30070,#25275,.T.) ;
#35718 = EDGE_CURVE('',#30067,#30071,#4851,.T.) ;
#35719 = EDGE_CURVE('',#30072,#30072,#25276,.T.) ;
#35720 = EDGE_CURVE('',#30072,#30073,#25277,.T.) ;
#35721 = EDGE_CURVE('',#30073,#30073,#25278,.T.) ;
#35722 = EDGE_CURVE('',#30074,#30074,#25279,.T.) ;
#35723 = EDGE_CURVE('',#30074,#30075,#25280,.T.) ;
#35724 = EDGE_CURVE('',#30075,#30075,#25281,.T.) ;
#35725 = EDGE_CURVE('',#30076,#30077,#25282,.T.) ;
#35726 = EDGE_CURVE('',#30078,#30076,#8351,.T.) ;
#35727 = EDGE_CURVE('',#30078,#30079,#25283,.T.) ;
#35728 = EDGE_CURVE('',#30079,#30080,#25284,.T.) ;
#35729 = EDGE_CURVE('',#30077,#30080,#8352,.T.) ;
#35730 = EDGE_CURVE('',#30081,#30082,#25285,.T.) ;
#35731 = EDGE_CURVE('',#30083,#30081,#8353,.T.) ;
#35732 = EDGE_CURVE('',#30083,#30084,#25286,.T.) ;
#35733 = EDGE_CURVE('',#30082,#30084,#8354,.T.) ;
#35734 = EDGE_CURVE('',#30085,#30086,#25287,.T.) ;
#35735 = EDGE_CURVE('',#30085,#30087,#25288,.T.) ;
#35736 = EDGE_CURVE('',#30088,#30087,#25289,.T.) ;
#35737 = EDGE_CURVE('',#30088,#30086,#25290,.T.) ;
#35738 = EDGE_CURVE('',#30073,#30074,#8355,.T.) ;
#35739 = EDGE_CURVE('',#30086,#30089,#8356,.T.) ;
#35740 = EDGE_CURVE('',#30089,#30083,#25291,.T.) ;
#35741 = EDGE_CURVE('',#30090,#30081,#78,.T.) ;
#35742 = EDGE_CURVE('',#30090,#30091,#25292,.T.) ;
#35743 = EDGE_CURVE('',#30077,#30091,#79,.T.) ;
#35744 = EDGE_CURVE('',#30080,#30092,#25293,.T.) ;
#35745 = EDGE_CURVE('',#30092,#30085,#8357,.T.) ;
#35746 = EDGE_CURVE('',#30093,#30094,#8358,.T.) ;
#35747 = EDGE_CURVE('',#30094,#30095,#8359,.T.) ;
#35748 = EDGE_CURVE('',#30095,#30096,#80,.T.) ;
#35749 = EDGE_CURVE('',#30096,#30097,#8360,.T.) ;
#35750 = EDGE_CURVE('',#30097,#30098,#4852,.T.) ;
#35751 = EDGE_CURVE('',#30098,#30093,#8361,.T.) ;
#35752 = EDGE_CURVE('',#30099,#30100,#8362,.T.) ;
#35753 = EDGE_CURVE('',#30100,#30101,#8363,.T.) ;
#35754 = EDGE_CURVE('',#30101,#30102,#81,.T.) ;
#35755 = EDGE_CURVE('',#30102,#30103,#82,.T.) ;
#35756 = EDGE_CURVE('',#30103,#30104,#8364,.T.) ;
#35757 = EDGE_CURVE('',#30104,#30099,#8365,.T.) ;
#35758 = EDGE_CURVE('',#30105,#30106,#8366,.T.) ;
#35759 = EDGE_CURVE('',#30106,#30107,#8367,.T.) ;
#35760 = EDGE_CURVE('',#30107,#30108,#8368,.T.) ;
#35761 = EDGE_CURVE('',#30108,#30105,#8369,.T.) ;
#35762 = EDGE_CURVE('',#30109,#30110,#8370,.T.) ;
#35763 = EDGE_CURVE('',#30110,#30111,#83,.T.) ;
#35764 = EDGE_CURVE('',#30111,#30112,#84,.T.) ;
#35765 = EDGE_CURVE('',#30112,#30113,#8371,.T.) ;
#35766 = EDGE_CURVE('',#30113,#30114,#8372,.T.) ;
#35767 = EDGE_CURVE('',#30114,#30109,#8373,.T.) ;
#35768 = EDGE_CURVE('',#30115,#30116,#8374,.T.) ;
#35769 = EDGE_CURVE('',#30116,#30117,#8375,.T.) ;
#35770 = EDGE_CURVE('',#30117,#30118,#8376,.T.) ;
#35771 = EDGE_CURVE('',#30118,#30115,#8377,.T.) ;
#35772 = EDGE_CURVE('',#30119,#30120,#8378,.T.) ;
#35773 = EDGE_CURVE('',#30119,#30121,#8379,.T.) ;
#35774 = EDGE_CURVE('',#30121,#30122,#8380,.T.) ;
#35775 = EDGE_CURVE('',#30122,#30120,#8381,.T.) ;
#35776 = EDGE_CURVE('',#30123,#30124,#8382,.T.) ;
#35777 = EDGE_CURVE('',#30123,#30125,#8383,.T.) ;
#35778 = EDGE_CURVE('',#30125,#30126,#8384,.T.) ;
#35779 = EDGE_CURVE('',#30126,#30127,#8385,.T.) ;
#35780 = EDGE_CURVE('',#30127,#30128,#25294,.T.) ;
#35781 = EDGE_CURVE('',#30128,#30124,#8386,.T.) ;
#35782 = EDGE_CURVE('',#30129,#30130,#8387,.T.) ;
#35783 = EDGE_CURVE('',#30129,#30100,#25295,.T.) ;
#35784 = EDGE_CURVE('',#30099,#30106,#25296,.T.) ;
#35785 = EDGE_CURVE('',#30105,#30114,#25297,.T.) ;
#35786 = EDGE_CURVE('',#30113,#30131,#25298,.T.) ;
#35787 = EDGE_CURVE('',#30132,#30131,#8388,.T.) ;
#35788 = EDGE_CURVE('',#30132,#30133,#25299,.T.) ;
#35789 = EDGE_CURVE('',#30134,#30133,#8389,.T.) ;
#35790 = EDGE_CURVE('',#30134,#30135,#25300,.T.) ;
#35791 = EDGE_CURVE('',#30135,#30136,#8390,.T.) ;
#35792 = EDGE_CURVE('',#30136,#30137,#25301,.T.) ;
#35793 = EDGE_CURVE('',#30138,#30137,#8391,.T.) ;
#35794 = EDGE_CURVE('',#30138,#30139,#25302,.T.) ;
#35795 = EDGE_CURVE('',#30139,#30140,#8392,.T.) ;
#35796 = EDGE_CURVE('',#30140,#30141,#25303,.T.) ;
#35797 = EDGE_CURVE('',#30142,#30141,#8393,.T.) ;
#35798 = EDGE_CURVE('',#30142,#30118,#25304,.T.) ;
#35799 = EDGE_CURVE('',#30117,#30143,#25305,.T.) ;
#35800 = EDGE_CURVE('',#30143,#30144,#8394,.T.) ;
#35801 = EDGE_CURVE('',#30144,#30126,#25306,.T.) ;
#35802 = EDGE_CURVE('',#30125,#30145,#25307,.T.) ;
#35803 = EDGE_CURVE('',#30146,#30145,#8395,.T.) ;
#35804 = EDGE_CURVE('',#30147,#30146,#8396,.T.) ;
#35805 = EDGE_CURVE('',#30147,#30148,#25308,.T.) ;
#35806 = EDGE_CURVE('',#30149,#30148,#8397,.T.) ;
#35807 = EDGE_CURVE('',#30149,#30150,#25309,.T.) ;
#35808 = EDGE_CURVE('',#30151,#30150,#8398,.T.) ;
#35809 = EDGE_CURVE('',#30151,#30130,#25310,.T.) ;
#35810 = EDGE_CURVE('',#30152,#30153,#8399,.T.) ;
#35811 = EDGE_CURVE('',#30153,#30154,#25311,.T.) ;
#35812 = EDGE_CURVE('',#30154,#30155,#8400,.T.) ;
#35813 = EDGE_CURVE('',#30155,#30156,#25312,.T.) ;
#35814 = EDGE_CURVE('',#30156,#30157,#8401,.T.) ;
#35815 = EDGE_CURVE('',#30157,#30158,#25313,.T.) ;
#35816 = EDGE_CURVE('',#30158,#30159,#8402,.T.) ;
#35817 = EDGE_CURVE('',#30159,#30160,#25314,.T.) ;
#35818 = EDGE_CURVE('',#30160,#30161,#8403,.T.) ;
#35819 = EDGE_CURVE('',#30161,#30162,#8404,.T.) ;
#35820 = EDGE_CURVE('',#30162,#30123,#25315,.T.) ;
#35821 = EDGE_CURVE('',#30124,#30163,#25316,.T.) ;
#35822 = EDGE_CURVE('',#30163,#30164,#8405,.T.) ;
#35823 = EDGE_CURVE('',#30164,#30119,#25317,.T.) ;
#35824 = EDGE_CURVE('',#30120,#30165,#25318,.T.) ;
#35825 = EDGE_CURVE('',#30166,#30165,#8406,.T.) ;
#35826 = EDGE_CURVE('',#30166,#30167,#25319,.T.) ;
#35827 = EDGE_CURVE('',#30168,#30167,#8407,.T.) ;
#35828 = EDGE_CURVE('',#30168,#30169,#25320,.T.) ;
#35829 = EDGE_CURVE('',#30169,#30170,#8408,.T.) ;
#35830 = EDGE_CURVE('',#30170,#30171,#25321,.T.) ;
#35831 = EDGE_CURVE('',#30172,#30171,#8409,.T.) ;
#35832 = EDGE_CURVE('',#30172,#30173,#25322,.T.) ;
#35833 = EDGE_CURVE('',#30174,#30173,#8410,.T.) ;
#35834 = EDGE_CURVE('',#30174,#30175,#25323,.T.) ;
#35835 = EDGE_CURVE('',#30175,#30176,#8411,.T.) ;
#35836 = EDGE_CURVE('',#30176,#30177,#25324,.T.) ;
#35837 = EDGE_CURVE('',#30177,#30178,#8412,.T.) ;
#35838 = EDGE_CURVE('',#30178,#30179,#25325,.T.) ;
#35839 = EDGE_CURVE('',#30179,#30180,#8413,.T.) ;
#35840 = EDGE_CURVE('',#30180,#30152,#25326,.T.) ;
#35841 = EDGE_CURVE('',#30148,#30159,#8414,.T.) ;
#35842 = EDGE_CURVE('',#30158,#30149,#8415,.T.) ;
#35843 = EDGE_CURVE('',#30150,#30157,#8416,.T.) ;
#35844 = EDGE_CURVE('',#30156,#30151,#8417,.T.) ;
#35845 = EDGE_CURVE('',#30181,#30182,#85,.T.) ;
#35846 = EDGE_CURVE('',#30182,#30129,#8418,.T.) ;
#35847 = EDGE_CURVE('',#30130,#30155,#8419,.T.) ;
#35848 = EDGE_CURVE('',#30154,#30183,#8420,.T.) ;
#35849 = EDGE_CURVE('',#30183,#30184,#86,.T.) ;
#35850 = EDGE_CURVE('',#30184,#30181,#8421,.T.) ;
#35851 = EDGE_CURVE('',#30185,#30186,#87,.T.) ;
#35852 = EDGE_CURVE('',#30186,#30187,#4853,.T.) ;
#35853 = EDGE_CURVE('',#30187,#30153,#8422,.T.) ;
#35854 = EDGE_CURVE('',#30152,#30188,#8423,.T.) ;
#35855 = EDGE_CURVE('',#30188,#30185,#8424,.T.) ;
#35856 = EDGE_CURVE('',#30189,#30190,#8425,.T.) ;
#35857 = EDGE_CURVE('',#30190,#30180,#8426,.T.) ;
#35858 = EDGE_CURVE('',#30179,#30189,#8427,.T.) ;
#35859 = EDGE_CURVE('',#30191,#30062,#88,.T.) ;
#35860 = EDGE_CURVE('',#30066,#30192,#8428,.T.) ;
#35861 = EDGE_CURVE('',#30192,#30178,#8429,.T.) ;
#35862 = EDGE_CURVE('',#30177,#30191,#8430,.T.) ;
#35863 = EDGE_CURVE('',#30131,#30193,#8431,.T.) ;
#35864 = EDGE_CURVE('',#30193,#30194,#89,.T.) ;
#35865 = EDGE_CURVE('',#30194,#30195,#8432,.T.) ;
#35866 = EDGE_CURVE('',#30195,#30196,#90,.T.) ;
#35867 = EDGE_CURVE('',#30196,#30176,#8433,.T.) ;
#35868 = EDGE_CURVE('',#30175,#30197,#8434,.T.) ;
#35869 = EDGE_CURVE('',#30197,#30198,#8435,.T.) ;
#35870 = EDGE_CURVE('',#30199,#30198,#25327,.T.) ;
#35871 = EDGE_CURVE('',#30199,#30200,#8436,.T.) ;
#35872 = EDGE_CURVE('',#30201,#30200,#25328,.T.) ;
#35873 = EDGE_CURVE('',#30201,#30202,#8437,.T.) ;
#35874 = EDGE_CURVE('',#30202,#30132,#8438,.T.) ;
#35875 = EDGE_CURVE('',#30203,#30204,#25329,.T.) ;
#35876 = EDGE_CURVE('',#30203,#30138,#8439,.T.) ;
#35877 = EDGE_CURVE('',#30137,#30205,#8440,.T.) ;
#35878 = EDGE_CURVE('',#30206,#30205,#25330,.T.) ;
#35879 = EDGE_CURVE('',#30206,#30207,#25331,.T.) ;
#35880 = EDGE_CURVE('',#30208,#30207,#25332,.T.) ;
#35881 = EDGE_CURVE('',#30208,#30209,#8441,.T.) ;
#35882 = EDGE_CURVE('',#30209,#30210,#8442,.T.) ;
#35883 = EDGE_CURVE('',#30210,#30211,#8443,.T.) ;
#35884 = EDGE_CURVE('',#30212,#30211,#25333,.T.) ;
#35885 = EDGE_CURVE('',#30212,#30213,#25334,.T.) ;
#35886 = EDGE_CURVE('',#30214,#30213,#25335,.T.) ;
#35887 = EDGE_CURVE('',#30214,#30170,#8444,.T.) ;
#35888 = EDGE_CURVE('',#30169,#30215,#8445,.T.) ;
#35889 = EDGE_CURVE('',#30216,#30215,#25336,.T.) ;
#35890 = EDGE_CURVE('',#30216,#30217,#25337,.T.) ;
#35891 = EDGE_CURVE('',#30218,#30217,#25338,.T.) ;
#35892 = EDGE_CURVE('',#30218,#30219,#8446,.T.) ;
#35893 = EDGE_CURVE('',#30219,#30220,#25339,.T.) ;
#35894 = EDGE_CURVE('',#30220,#30221,#8447,.T.) ;
#35895 = EDGE_CURVE('',#30222,#30221,#25340,.T.) ;
#35896 = EDGE_CURVE('',#30222,#30204,#25341,.T.) ;
#35897 = EDGE_CURVE('',#30223,#30224,#25342,.T.) ;
#35898 = EDGE_CURVE('',#30223,#30225,#8448,.T.) ;
#35899 = EDGE_CURVE('',#30146,#30225,#8449,.T.) ;
#35900 = EDGE_CURVE('',#30145,#30162,#8450,.T.) ;
#35901 = EDGE_CURVE('',#30226,#30161,#8451,.T.) ;
#35902 = EDGE_CURVE('',#30226,#30227,#8452,.T.) ;
#35903 = EDGE_CURVE('',#30228,#30227,#25343,.T.) ;
#35904 = EDGE_CURVE('',#30228,#30224,#8453,.T.) ;
#35905 = EDGE_CURVE('',#30229,#30230,#25344,.T.) ;
#35906 = EDGE_CURVE('',#30229,#30226,#8454,.T.) ;
#35907 = EDGE_CURVE('',#30160,#30147,#8455,.T.) ;
#35908 = EDGE_CURVE('',#30225,#30231,#8456,.T.) ;
#35909 = EDGE_CURVE('',#30232,#30231,#25345,.T.) ;
#35910 = EDGE_CURVE('',#30232,#30230,#8457,.T.) ;
#35911 = EDGE_CURVE('',#30233,#30234,#8458,.T.) ;
#35912 = EDGE_CURVE('',#30234,#30235,#8459,.T.) ;
#35913 = EDGE_CURVE('',#30233,#30235,#25346,.T.) ;
#35914 = EDGE_CURVE('',#30236,#30237,#25347,.T.) ;
#35915 = EDGE_CURVE('',#30236,#30238,#8460,.T.) ;
#35916 = EDGE_CURVE('',#30238,#30237,#8461,.T.) ;
#35917 = EDGE_CURVE('',#30239,#30240,#8462,.T.) ;
#35918 = EDGE_CURVE('',#30240,#30241,#8463,.T.) ;
#35919 = EDGE_CURVE('',#30241,#30242,#8464,.T.) ;
#35920 = EDGE_CURVE('',#30242,#30243,#8465,.T.) ;
#35921 = EDGE_CURVE('',#30243,#30244,#8466,.T.) ;
#35922 = EDGE_CURVE('',#30244,#30245,#8467,.T.) ;
#35923 = EDGE_CURVE('',#30245,#30246,#8468,.T.) ;
#35924 = EDGE_CURVE('',#30246,#30239,#8469,.T.) ;
#35925 = EDGE_CURVE('',#30247,#30248,#8470,.T.) ;
#35926 = EDGE_CURVE('',#30248,#30249,#8471,.T.) ;
#35927 = EDGE_CURVE('',#30249,#30250,#8472,.T.) ;
#35928 = EDGE_CURVE('',#30250,#30247,#8473,.T.) ;
#35929 = EDGE_CURVE('',#30251,#30252,#8474,.T.) ;
#35930 = EDGE_CURVE('',#30252,#30253,#8475,.T.) ;
#35931 = EDGE_CURVE('',#30253,#30254,#8476,.T.) ;
#35932 = EDGE_CURVE('',#30254,#30251,#8477,.T.) ;
#35933 = EDGE_CURVE('',#30255,#30256,#8478,.T.) ;
#35934 = EDGE_CURVE('',#30256,#30257,#8479,.T.) ;
#35935 = EDGE_CURVE('',#30257,#30258,#8480,.T.) ;
#35936 = EDGE_CURVE('',#30258,#30255,#8481,.T.) ;
#35937 = EDGE_CURVE('',#30259,#30260,#91,.T.) ;
#35938 = EDGE_CURVE('',#30260,#30261,#8482,.T.) ;
#35939 = EDGE_CURVE('',#30261,#30262,#8483,.T.) ;
#35940 = EDGE_CURVE('',#30262,#30263,#8484,.T.) ;
#35941 = EDGE_CURVE('',#30263,#30264,#92,.T.) ;
#35942 = EDGE_CURVE('',#30264,#30259,#8485,.T.) ;
#35943 = EDGE_CURVE('',#30265,#30266,#8486,.T.) ;
#35944 = EDGE_CURVE('',#30266,#30267,#8487,.T.) ;
#35945 = EDGE_CURVE('',#30267,#30268,#8488,.T.) ;
#35946 = EDGE_CURVE('',#30268,#30269,#8489,.T.) ;
#35947 = EDGE_CURVE('',#30269,#30270,#8490,.T.) ;
#35948 = EDGE_CURVE('',#30270,#30271,#8491,.T.) ;
#35949 = EDGE_CURVE('',#30271,#30272,#8492,.T.) ;
#35950 = EDGE_CURVE('',#30272,#30265,#8493,.T.) ;
#35951 = EDGE_CURVE('',#30273,#30274,#8494,.T.) ;
#35952 = EDGE_CURVE('',#30273,#30275,#25348,.T.) ;
#35953 = EDGE_CURVE('',#30275,#30276,#8495,.T.) ;
#35954 = EDGE_CURVE('',#30276,#30277,#25349,.T.) ;
#35955 = EDGE_CURVE('',#30277,#30278,#8496,.T.) ;
#35956 = EDGE_CURVE('',#30278,#30279,#25350,.T.) ;
#35957 = EDGE_CURVE('',#30279,#30280,#8497,.T.) ;
#35958 = EDGE_CURVE('',#30280,#30274,#25351,.T.) ;
#35959 = EDGE_CURVE('',#30281,#30282,#25352,.T.) ;
#35960 = EDGE_CURVE('',#30281,#30142,#8498,.T.) ;
#35961 = EDGE_CURVE('',#30141,#30283,#8499,.T.) ;
#35962 = EDGE_CURVE('',#30283,#30284,#25353,.T.) ;
#35963 = EDGE_CURVE('',#30284,#30285,#8500,.T.) ;
#35964 = EDGE_CURVE('',#30285,#30282,#25354,.T.) ;
#35965 = EDGE_CURVE('',#30139,#30286,#8501,.T.) ;
#35966 = EDGE_CURVE('',#30286,#30287,#8502,.T.) ;
#35967 = EDGE_CURVE('',#30287,#30140,#8503,.T.) ;
#35968 = EDGE_CURVE('',#30288,#30289,#8504,.T.) ;
#35969 = EDGE_CURVE('',#30289,#30082,#8505,.T.) ;
#35970 = EDGE_CURVE('',#30084,#30288,#8506,.T.) ;
#35971 = EDGE_CURVE('',#30290,#30291,#25355,.T.) ;
#35972 = EDGE_CURVE('',#30291,#30292,#8507,.T.) ;
#35973 = EDGE_CURVE('',#30292,#30293,#25356,.T.) ;
#35974 = EDGE_CURVE('',#30293,#30290,#8508,.T.) ;
#35975 = EDGE_CURVE('',#30294,#30295,#25357,.T.) ;
#35976 = EDGE_CURVE('',#30295,#30296,#8509,.T.) ;
#35977 = EDGE_CURVE('',#30296,#30297,#25358,.T.) ;
#35978 = EDGE_CURVE('',#30297,#30294,#8510,.T.) ;
#35979 = EDGE_CURVE('',#30076,#30298,#8511,.T.) ;
#35980 = EDGE_CURVE('',#30298,#30299,#8512,.T.) ;
#35981 = EDGE_CURVE('',#30299,#30078,#8513,.T.) ;
#35982 = EDGE_CURVE('',#30300,#30301,#8514,.T.) ;
#35983 = EDGE_CURVE('',#30301,#30168,#8515,.T.) ;
#35984 = EDGE_CURVE('',#30167,#30300,#8516,.T.) ;
#35985 = EDGE_CURVE('',#30302,#30303,#25359,.T.) ;
#35986 = EDGE_CURVE('',#30303,#30166,#8517,.T.) ;
#35987 = EDGE_CURVE('',#30165,#30304,#8518,.T.) ;
#35988 = EDGE_CURVE('',#30305,#30304,#25360,.T.) ;
#35989 = EDGE_CURVE('',#30305,#30306,#25361,.T.) ;
#35990 = EDGE_CURVE('',#30306,#30302,#8519,.T.) ;
#35991 = EDGE_CURVE('',#30307,#30308,#25362,.T.) ;
#35992 = EDGE_CURVE('',#30308,#30134,#8520,.T.) ;
#35993 = EDGE_CURVE('',#30133,#30309,#8521,.T.) ;
#35994 = EDGE_CURVE('',#30309,#30307,#8522,.T.) ;
#35995 = EDGE_CURVE('',#30310,#30311,#8523,.T.) ;
#35996 = EDGE_CURVE('',#30311,#30136,#8524,.T.) ;
#35997 = EDGE_CURVE('',#30135,#30310,#8525,.T.) ;
#35998 = EDGE_CURVE('',#30312,#30313,#25363,.T.) ;
#35999 = EDGE_CURVE('',#30313,#30314,#8526,.T.) ;
#36000 = EDGE_CURVE('',#30314,#30315,#25364,.T.) ;
#36001 = EDGE_CURVE('',#30315,#30312,#8527,.T.) ;
#36002 = EDGE_CURVE('',#30316,#30317,#8528,.T.) ;
#36003 = EDGE_CURVE('',#30317,#30318,#8529,.T.) ;
#36004 = EDGE_CURVE('',#30318,#30319,#8530,.T.) ;
#36005 = EDGE_CURVE('',#30319,#30316,#8531,.T.) ;
#36006 = EDGE_CURVE('',#30320,#30321,#25365,.T.) ;
#36007 = EDGE_CURVE('',#30321,#30322,#8532,.T.) ;
#36008 = EDGE_CURVE('',#30322,#30323,#25366,.T.) ;
#36009 = EDGE_CURVE('',#30323,#30320,#8533,.T.) ;
#36010 = EDGE_CURVE('',#30171,#30324,#8534,.T.) ;
#36011 = EDGE_CURVE('',#30324,#30325,#8535,.T.) ;
#36012 = EDGE_CURVE('',#30325,#30172,#8536,.T.) ;
#36013 = EDGE_CURVE('',#30326,#30327,#8537,.T.) ;
#36014 = EDGE_CURVE('',#30327,#30328,#8538,.T.) ;
#36015 = EDGE_CURVE('',#30328,#30329,#8539,.T.) ;
#36016 = EDGE_CURVE('',#30329,#30326,#8540,.T.) ;
#36017 = EDGE_CURVE('',#30330,#30331,#8541,.T.) ;
#36018 = EDGE_CURVE('',#30331,#30174,#8542,.T.) ;
#36019 = EDGE_CURVE('',#30173,#30332,#8543,.T.) ;
#36020 = EDGE_CURVE('',#30332,#30330,#25367,.T.) ;
#36021 = EDGE_CURVE('',#30333,#30334,#8544,.T.) ;
#36022 = EDGE_CURVE('',#30334,#30335,#8545,.T.) ;
#36023 = EDGE_CURVE('',#30335,#30336,#8546,.T.) ;
#36024 = EDGE_CURVE('',#30336,#30333,#8547,.T.) ;
#36025 = EDGE_CURVE('',#30337,#30338,#4854,.T.) ;
#36026 = EDGE_CURVE('',#30338,#30067,#8548,.T.) ;
#36027 = EDGE_CURVE('',#30071,#30339,#8549,.T.) ;
#36028 = EDGE_CURVE('',#30339,#30340,#4855,.T.) ;
#36029 = EDGE_CURVE('',#30340,#30341,#8550,.T.) ;
#36030 = EDGE_CURVE('',#30341,#30342,#4856,.T.) ;
#36031 = EDGE_CURVE('',#30342,#30337,#8551,.T.) ;
#36032 = EDGE_CURVE('',#30343,#30344,#8552,.T.) ;
#36033 = EDGE_CURVE('',#30344,#30070,#8553,.T.) ;
#36034 = EDGE_CURVE('',#30070,#30345,#8554,.T.) ;
#36035 = EDGE_CURVE('',#30345,#30343,#8555,.T.) ;
#36036 = EDGE_CURVE('',#30346,#30347,#8556,.T.) ;
#36037 = EDGE_CURVE('',#30347,#30348,#8557,.T.) ;
#36038 = EDGE_CURVE('',#30348,#30349,#8558,.T.) ;
#36039 = EDGE_CURVE('',#30349,#30346,#8559,.T.) ;
#36040 = EDGE_CURVE('',#30350,#30351,#8560,.T.) ;
#36041 = EDGE_CURVE('',#30351,#30352,#8561,.T.) ;
#36042 = EDGE_CURVE('',#30352,#30353,#8562,.T.) ;
#36043 = EDGE_CURVE('',#30353,#30350,#8563,.T.) ;
#36044 = EDGE_CURVE('',#30354,#30355,#8564,.T.) ;
#36045 = EDGE_CURVE('',#30355,#30356,#8565,.T.) ;
#36046 = EDGE_CURVE('',#30356,#30357,#8566,.T.) ;
#36047 = EDGE_CURVE('',#30357,#30354,#8567,.T.) ;
#36048 = EDGE_CURVE('',#30274,#30358,#8568,.T.) ;
#36049 = EDGE_CURVE('',#30358,#30359,#8569,.T.) ;
#36050 = EDGE_CURVE('',#30359,#30273,#8570,.T.) ;
#36051 = EDGE_CURVE('',#30277,#30360,#8571,.T.) ;
#36052 = EDGE_CURVE('',#30360,#30361,#8572,.T.) ;
#36053 = EDGE_CURVE('',#30361,#30278,#8573,.T.) ;
#36054 = EDGE_CURVE('',#30279,#30362,#8574,.T.) ;
#36055 = EDGE_CURVE('',#30362,#30363,#8575,.T.) ;
#36056 = EDGE_CURVE('',#30363,#30280,#8576,.T.) ;
#36057 = EDGE_CURVE('',#30275,#30364,#8577,.T.) ;
#36058 = EDGE_CURVE('',#30364,#30365,#8578,.T.) ;
#36059 = EDGE_CURVE('',#30365,#30276,#8579,.T.) ;
#36060 = EDGE_CURVE('',#30366,#30367,#8580,.T.) ;
#36061 = EDGE_CURVE('',#30367,#30368,#8581,.T.) ;
#36062 = EDGE_CURVE('',#30368,#30369,#8582,.T.) ;
#36063 = EDGE_CURVE('',#30369,#30370,#25368,.T.) ;
#36064 = EDGE_CURVE('',#30370,#30371,#8583,.T.) ;
#36065 = EDGE_CURVE('',#30371,#30366,#25369,.T.) ;
#36066 = EDGE_CURVE('',#30372,#30373,#8584,.T.) ;
#36067 = EDGE_CURVE('',#30373,#30374,#8585,.T.) ;
#36068 = EDGE_CURVE('',#30374,#30375,#8586,.T.) ;
#36069 = EDGE_CURVE('',#30375,#30376,#25370,.T.) ;
#36070 = EDGE_CURVE('',#30376,#30377,#8587,.T.) ;
#36071 = EDGE_CURVE('',#30377,#30372,#25371,.T.) ;
#36072 = EDGE_CURVE('',#30378,#30379,#8588,.T.) ;
#36073 = EDGE_CURVE('',#30378,#30097,#25372,.T.) ;
#36074 = EDGE_CURVE('',#30096,#30379,#25373,.T.) ;
#36075 = EDGE_CURVE('',#30379,#30380,#8589,.T.) ;
#36076 = EDGE_CURVE('',#30380,#30381,#8590,.T.) ;
#36077 = EDGE_CURVE('',#30381,#30378,#8591,.T.) ;
#36078 = EDGE_CURVE('',#30382,#30383,#8592,.T.) ;
#36079 = EDGE_CURVE('',#30383,#30384,#8593,.T.) ;
#36080 = EDGE_CURVE('',#30384,#30385,#8594,.T.) ;
#36081 = EDGE_CURVE('',#30385,#30382,#8595,.T.) ;
#36082 = EDGE_CURVE('',#30386,#30387,#8596,.T.) ;
#36083 = EDGE_CURVE('',#30387,#30388,#8597,.T.) ;
#36084 = EDGE_CURVE('',#30388,#30389,#8598,.T.) ;
#36085 = EDGE_CURVE('',#30389,#30386,#8599,.T.) ;
#36086 = EDGE_CURVE('',#30390,#30391,#8600,.T.) ;
#36087 = EDGE_CURVE('',#30391,#30392,#8601,.T.) ;
#36088 = EDGE_CURVE('',#30392,#30393,#8602,.T.) ;
#36089 = EDGE_CURVE('',#30393,#30390,#8603,.T.) ;
#36090 = EDGE_CURVE('',#30394,#30395,#8604,.T.) ;
#36091 = EDGE_CURVE('',#30395,#30396,#8605,.T.) ;
#36092 = EDGE_CURVE('',#30396,#30397,#8606,.T.) ;
#36093 = EDGE_CURVE('',#30394,#30397,#8607,.T.) ;
#36094 = EDGE_CURVE('',#30264,#30394,#25374,.T.) ;
#36095 = EDGE_CURVE('',#30397,#30259,#25375,.T.) ;
#36096 = EDGE_CURVE('',#30398,#30399,#8608,.T.) ;
#36097 = EDGE_CURVE('',#30399,#30400,#8609,.T.) ;
#36098 = EDGE_CURVE('',#30400,#30401,#8610,.T.) ;
#36099 = EDGE_CURVE('',#30401,#30398,#8611,.T.) ;
#36100 = EDGE_CURVE('',#30402,#30403,#8612,.T.) ;
#36101 = EDGE_CURVE('',#30403,#30404,#8613,.T.) ;
#36102 = EDGE_CURVE('',#30404,#30405,#8614,.T.) ;
#36103 = EDGE_CURVE('',#30405,#30402,#8615,.T.) ;
#36104 = EDGE_CURVE('',#30406,#30407,#8616,.T.) ;
#36105 = EDGE_CURVE('',#30407,#30408,#8617,.T.) ;
#36106 = EDGE_CURVE('',#30408,#30409,#8618,.T.) ;
#36107 = EDGE_CURVE('',#30409,#30406,#8619,.T.) ;
#36108 = EDGE_CURVE('',#30410,#30411,#8620,.T.) ;
#36109 = EDGE_CURVE('',#30411,#30412,#8621,.T.) ;
#36110 = EDGE_CURVE('',#30412,#30413,#8622,.T.) ;
#36111 = EDGE_CURVE('',#30413,#30410,#8623,.T.) ;
#36112 = EDGE_CURVE('',#30163,#30414,#8624,.T.) ;
#36113 = EDGE_CURVE('',#30414,#30415,#25376,.T.) ;
#36114 = EDGE_CURVE('',#30415,#30164,#8625,.T.) ;
#36115 = EDGE_CURVE('',#30416,#30417,#25377,.T.) ;
#36116 = EDGE_CURVE('',#30417,#30088,#25378,.T.) ;
#36117 = EDGE_CURVE('',#30087,#30416,#25379,.T.) ;
#36118 = EDGE_CURVE('',#30143,#30418,#8626,.T.) ;
#36119 = EDGE_CURVE('',#30418,#30419,#25380,.T.) ;
#36120 = EDGE_CURVE('',#30419,#30144,#8627,.T.) ;
#36121 = EDGE_CURVE('',#30332,#30325,#25381,.T.) ;
#36122 = EDGE_CURVE('',#30332,#30321,#25382,.T.) ;
#36123 = EDGE_CURVE('',#30321,#30325,#25383,.T.) ;
#36124 = EDGE_CURVE('',#30324,#30214,#25384,.T.) ;
#36125 = EDGE_CURVE('',#30322,#30324,#25385,.T.) ;
#36126 = EDGE_CURVE('',#30330,#30320,#25386,.T.) ;
#36127 = EDGE_CURVE('',#30322,#30213,#25387,.T.) ;
#36128 = EDGE_CURVE('',#30330,#30329,#25388,.T.) ;
#36129 = EDGE_CURVE('',#30329,#30320,#25389,.T.) ;
#36130 = EDGE_CURVE('',#30310,#30308,#25390,.T.) ;
#36131 = EDGE_CURVE('',#30311,#30315,#25391,.T.) ;
#36132 = EDGE_CURVE('',#30312,#30310,#25392,.T.) ;
#36133 = EDGE_CURVE('',#30205,#30311,#25393,.T.) ;
#36134 = EDGE_CURVE('',#30323,#30212,#25394,.T.) ;
#36135 = EDGE_CURVE('',#30326,#30323,#25395,.T.) ;
#36136 = EDGE_CURVE('',#30331,#30328,#25396,.T.) ;
#36137 = EDGE_CURVE('',#30197,#30331,#25397,.T.) ;
#36138 = EDGE_CURVE('',#30312,#30308,#25398,.T.) ;
#36139 = EDGE_CURVE('',#30206,#30315,#25399,.T.) ;
#36140 = EDGE_CURVE('',#30326,#30211,#25400,.T.) ;
#36141 = EDGE_CURVE('',#30197,#30328,#25401,.T.) ;
#36142 = EDGE_CURVE('',#30313,#30307,#25402,.T.) ;
#36143 = EDGE_CURVE('',#30314,#30319,#25403,.T.) ;
#36144 = EDGE_CURVE('',#30316,#30313,#25404,.T.) ;
#36145 = EDGE_CURVE('',#30207,#30314,#25405,.T.) ;
#36146 = EDGE_CURVE('',#30327,#30210,#25406,.T.) ;
#36147 = EDGE_CURVE('',#30198,#30327,#25407,.T.) ;
#36148 = EDGE_CURVE('',#30316,#30307,#25408,.T.) ;
#36149 = EDGE_CURVE('',#30208,#30319,#25409,.T.) ;
#36150 = EDGE_CURVE('',#30199,#30210,#25410,.T.) ;
#36151 = EDGE_CURVE('',#30309,#30202,#25411,.T.) ;
#36152 = EDGE_CURVE('',#30317,#30309,#25412,.T.) ;
#36153 = EDGE_CURVE('',#30209,#30318,#25413,.T.) ;
#36154 = EDGE_CURVE('',#30200,#30209,#25414,.T.) ;
#36155 = EDGE_CURVE('',#30317,#30202,#25415,.T.) ;
#36156 = EDGE_CURVE('',#30201,#30318,#25416,.T.) ;
#36157 = EDGE_CURVE('',#30265,#30246,#25417,.T.) ;
#36158 = EDGE_CURVE('',#30254,#30265,#25418,.T.) ;
#36159 = EDGE_CURVE('',#30246,#30254,#25419,.T.) ;
#36160 = EDGE_CURVE('',#30272,#30420,#93,.T.) ;
#36161 = EDGE_CURVE('',#30420,#30251,#4857,.T.) ;
#36162 = EDGE_CURVE('',#30253,#30421,#4858,.T.) ;
#36163 = EDGE_CURVE('',#30421,#30239,#94,.T.) ;
#36164 = EDGE_CURVE('',#30266,#30245,#25420,.T.) ;
#36165 = EDGE_CURVE('',#30261,#30422,#4859,.T.) ;
#36166 = EDGE_CURVE('',#30422,#30272,#95,.T.) ;
#36167 = EDGE_CURVE('',#30271,#30423,#96,.T.) ;
#36168 = EDGE_CURVE('',#30423,#30262,#4860,.T.) ;
#36169 = EDGE_CURVE('',#30239,#30424,#97,.T.) ;
#36170 = EDGE_CURVE('',#30424,#30256,#4861,.T.) ;
#36171 = EDGE_CURVE('',#30255,#30425,#4862,.T.) ;
#36172 = EDGE_CURVE('',#30425,#30240,#98,.T.) ;
#36173 = EDGE_CURVE('',#30266,#30237,#25421,.T.) ;
#36174 = EDGE_CURVE('',#30236,#30245,#25422,.T.) ;
#36175 = EDGE_CURVE('',#30426,#30237,#8628,.T.) ;
#36176 = EDGE_CURVE('',#30267,#30426,#25423,.T.) ;
#36177 = EDGE_CURVE('',#30427,#30426,#25424,.T.) ;
#36178 = EDGE_CURVE('',#30267,#30427,#25425,.T.) ;
#36179 = EDGE_CURVE('',#30250,#30428,#4863,.T.) ;
#36180 = EDGE_CURVE('',#30428,#30271,#99,.T.) ;
#36181 = EDGE_CURVE('',#30247,#30270,#25426,.T.) ;
#36182 = EDGE_CURVE('',#30240,#30429,#100,.T.) ;
#36183 = EDGE_CURVE('',#30429,#30248,#4864,.T.) ;
#36184 = EDGE_CURVE('',#30241,#30247,#25427,.T.) ;
#36185 = EDGE_CURVE('',#30430,#30244,#25428,.T.) ;
#36186 = EDGE_CURVE('',#30236,#30430,#8629,.T.) ;
#36187 = EDGE_CURVE('',#30225,#30238,#4865,.T.) ;
#36188 = EDGE_CURVE('',#30426,#30223,#25429,.T.) ;
#36189 = EDGE_CURVE('',#30427,#30224,#25430,.T.) ;
#36190 = EDGE_CURVE('',#30431,#30427,#8630,.T.) ;
#36191 = EDGE_CURVE('',#30268,#30431,#25431,.T.) ;
#36192 = EDGE_CURVE('',#30241,#30270,#25432,.T.) ;
#36193 = EDGE_CURVE('',#30430,#30432,#25433,.T.) ;
#36194 = EDGE_CURVE('',#30432,#30244,#25434,.T.) ;
#36195 = EDGE_CURVE('',#30231,#30430,#25435,.T.) ;
#36196 = EDGE_CURVE('',#30431,#30228,#25436,.T.) ;
#36197 = EDGE_CURVE('',#30433,#30431,#25437,.T.) ;
#36198 = EDGE_CURVE('',#30268,#30433,#25438,.T.) ;
#36199 = EDGE_CURVE('',#30242,#30269,#25439,.T.) ;
#36200 = EDGE_CURVE('',#30434,#30243,#25440,.T.) ;
#36201 = EDGE_CURVE('',#30432,#30434,#8631,.T.) ;
#36202 = EDGE_CURVE('',#30232,#30432,#25441,.T.) ;
#36203 = EDGE_CURVE('',#30433,#30227,#25442,.T.) ;
#36204 = EDGE_CURVE('',#30233,#30433,#8632,.T.) ;
#36205 = EDGE_CURVE('',#30269,#30233,#25443,.T.) ;
#36206 = EDGE_CURVE('',#30242,#30235,#25444,.T.) ;
#36207 = EDGE_CURVE('',#30434,#30435,#25445,.T.) ;
#36208 = EDGE_CURVE('',#30435,#30243,#25446,.T.) ;
#36209 = EDGE_CURVE('',#30230,#30434,#25447,.T.) ;
#36210 = EDGE_CURVE('',#30234,#30226,#4866,.T.) ;
#36211 = EDGE_CURVE('',#30435,#30235,#8633,.T.) ;
#36212 = EDGE_CURVE('',#30229,#30435,#25448,.T.) ;
#36213 = EDGE_CURVE('',#30283,#30287,#25449,.T.) ;
#36214 = EDGE_CURVE('',#30283,#30291,#25450,.T.) ;
#36215 = EDGE_CURVE('',#30291,#30287,#25451,.T.) ;
#36216 = EDGE_CURVE('',#30286,#30203,#25452,.T.) ;
#36217 = EDGE_CURVE('',#30292,#30286,#25453,.T.) ;
#36218 = EDGE_CURVE('',#30284,#30290,#25454,.T.) ;
#36219 = EDGE_CURVE('',#30115,#30281,#25455,.T.) ;
#36220 = EDGE_CURVE('',#30086,#30116,#25456,.T.) ;
#36221 = EDGE_CURVE('',#30089,#30115,#25457,.T.) ;
#36222 = EDGE_CURVE('',#30292,#30204,#25458,.T.) ;
#36223 = EDGE_CURVE('',#30284,#30288,#25459,.T.) ;
#36224 = EDGE_CURVE('',#30288,#30290,#25460,.T.) ;
#36225 = EDGE_CURVE('',#30089,#30282,#25461,.T.) ;
#36226 = EDGE_CURVE('',#30293,#30222,#25462,.T.) ;
#36227 = EDGE_CURVE('',#30289,#30293,#25463,.T.) ;
#36228 = EDGE_CURVE('',#30285,#30084,#25464,.T.) ;
#36229 = EDGE_CURVE('',#30083,#30285,#25465,.T.) ;
#36230 = EDGE_CURVE('',#30121,#30085,#25466,.T.) ;
#36231 = EDGE_CURVE('',#30122,#30092,#25467,.T.) ;
#36232 = EDGE_CURVE('',#30304,#30122,#25468,.T.) ;
#36233 = EDGE_CURVE('',#30300,#30303,#25469,.T.) ;
#36234 = EDGE_CURVE('',#30289,#30221,#25470,.T.) ;
#36235 = EDGE_CURVE('',#30305,#30092,#25471,.T.) ;
#36236 = EDGE_CURVE('',#30300,#30294,#25472,.T.) ;
#36237 = EDGE_CURVE('',#30294,#30303,#25473,.T.) ;
#36238 = EDGE_CURVE('',#30082,#30220,#101,.T.) ;
#36239 = EDGE_CURVE('',#30306,#30080,#25474,.T.) ;
#36240 = EDGE_CURVE('',#30302,#30299,#25475,.T.) ;
#36241 = EDGE_CURVE('',#30078,#30306,#25476,.T.) ;
#36242 = EDGE_CURVE('',#30295,#30302,#25477,.T.) ;
#36243 = EDGE_CURVE('',#30301,#30297,#25478,.T.) ;
#36244 = EDGE_CURVE('',#30215,#30301,#25479,.T.) ;
#36245 = EDGE_CURVE('',#30090,#30220,#25480,.T.) ;
#36246 = EDGE_CURVE('',#30436,#30079,#25481,.T.) ;
#36247 = EDGE_CURVE('',#30295,#30299,#25482,.T.) ;
#36248 = EDGE_CURVE('',#30216,#30297,#25483,.T.) ;
#36249 = EDGE_CURVE('',#30091,#30219,#25484,.T.) ;
#36250 = EDGE_CURVE('',#30296,#30298,#25485,.T.) ;
#36251 = EDGE_CURVE('',#30217,#30296,#25486,.T.) ;
#36252 = EDGE_CURVE('',#30076,#30219,#102,.T.) ;
#36253 = EDGE_CURVE('',#30218,#30298,#25487,.T.) ;
#36254 = EDGE_CURVE('',#30095,#30376,#103,.T.) ;
#36255 = EDGE_CURVE('',#30379,#30375,#25488,.T.) ;
#36256 = EDGE_CURVE('',#30374,#30380,#25489,.T.) ;
#36257 = EDGE_CURVE('',#30377,#30260,#104,.T.) ;
#36258 = EDGE_CURVE('',#30372,#30397,#25490,.T.) ;
#36259 = EDGE_CURVE('',#30384,#30411,#25491,.T.) ;
#36260 = EDGE_CURVE('',#30385,#30410,#25492,.T.) ;
#36261 = EDGE_CURVE('',#30371,#30098,#105,.T.) ;
#36262 = EDGE_CURVE('',#30366,#30378,#25493,.T.) ;
#36263 = EDGE_CURVE('',#30396,#30373,#25494,.T.) ;
#36264 = EDGE_CURVE('',#30385,#30389,#25495,.T.) ;
#36265 = EDGE_CURVE('',#30389,#30410,#25496,.T.) ;
#36266 = EDGE_CURVE('',#30381,#30367,#25497,.T.) ;
#36267 = EDGE_CURVE('',#30412,#30391,#25498,.T.) ;
#36268 = EDGE_CURVE('',#30413,#30390,#25499,.T.) ;
#36269 = EDGE_CURVE('',#30386,#30413,#25500,.T.) ;
#36270 = EDGE_CURVE('',#30382,#30388,#25501,.T.) ;
#36271 = EDGE_CURVE('',#30408,#30383,#25502,.T.) ;
#36272 = EDGE_CURVE('',#30409,#30382,#25503,.T.) ;
#36273 = EDGE_CURVE('',#30386,#30390,#25504,.T.) ;
#36274 = EDGE_CURVE('',#30409,#30388,#25505,.T.) ;
#36275 = EDGE_CURVE('',#30387,#30393,#25506,.T.) ;
#36276 = EDGE_CURVE('',#30406,#30387,#25507,.T.) ;
#36277 = EDGE_CURVE('',#30406,#30393,#25508,.T.) ;
#36278 = EDGE_CURVE('',#30392,#30407,#25509,.T.) ;
#36279 = EDGE_CURVE('',#30368,#30395,#25510,.T.) ;
#36280 = EDGE_CURVE('',#30369,#30394,#25511,.T.) ;
#36281 = EDGE_CURVE('',#30263,#30370,#106,.T.) ;
#36282 = EDGE_CURVE('',#30361,#30362,#25512,.T.) ;
#36283 = EDGE_CURVE('',#30365,#30360,#25513,.T.) ;
#36284 = EDGE_CURVE('',#30348,#30399,#25514,.T.) ;
#36285 = EDGE_CURVE('',#30349,#30398,#25515,.T.) ;
#36286 = EDGE_CURVE('',#30400,#30355,#25516,.T.) ;
#36287 = EDGE_CURVE('',#30401,#30354,#25517,.T.) ;
#36288 = EDGE_CURVE('',#30398,#30353,#25518,.T.) ;
#36289 = EDGE_CURVE('',#30350,#30401,#25519,.T.) ;
#36290 = EDGE_CURVE('',#30349,#30353,#25520,.T.) ;
#36291 = EDGE_CURVE('',#30363,#30358,#25521,.T.) ;
#36292 = EDGE_CURVE('',#30359,#30364,#25522,.T.) ;
#36293 = EDGE_CURVE('',#30350,#30354,#25523,.T.) ;
#36294 = EDGE_CURVE('',#30346,#30352,#25524,.T.) ;
#36295 = EDGE_CURVE('',#30404,#30347,#25525,.T.) ;
#36296 = EDGE_CURVE('',#30405,#30346,#25526,.T.) ;
#36297 = EDGE_CURVE('',#30356,#30403,#25527,.T.) ;
#36298 = EDGE_CURVE('',#30357,#30402,#25528,.T.) ;
#36299 = EDGE_CURVE('',#30351,#30357,#25529,.T.) ;
#36300 = EDGE_CURVE('',#30405,#30352,#25530,.T.) ;
#36301 = EDGE_CURVE('',#30351,#30402,#25531,.T.) ;
#36302 = EDGE_CURVE('',#30109,#30108,#25532,.T.) ;
#36303 = EDGE_CURVE('',#30335,#30110,#107,.T.) ;
#36304 = EDGE_CURVE('',#30336,#30109,#25533,.T.) ;
#36305 = EDGE_CURVE('',#30336,#30108,#25534,.T.) ;
#36306 = EDGE_CURVE('',#30107,#30104,#25535,.T.) ;
#36307 = EDGE_CURVE('',#30333,#30107,#25536,.T.) ;
#36308 = EDGE_CURVE('',#30333,#30104,#25537,.T.) ;
#36309 = EDGE_CURVE('',#30103,#30334,#108,.T.) ;
#36310 = EDGE_CURVE('',#30065,#30344,#4867,.T.) ;
#36311 = EDGE_CURVE('',#30192,#30343,#25538,.T.) ;
#36312 = EDGE_CURVE('',#30189,#30192,#25539,.T.) ;
#36313 = EDGE_CURVE('',#30189,#30343,#25540,.T.) ;
#36314 = EDGE_CURVE('',#30190,#30345,#25541,.T.) ;
#36315 = EDGE_CURVE('',#30188,#30190,#25542,.T.) ;
#36316 = EDGE_CURVE('',#30188,#30345,#25543,.T.) ;
#36317 = EDGE_CURVE('',#30069,#30185,#4868,.T.) ;
#36318 = EDGE_CURVE('',#30257,#30094,#25544,.T.) ;
#36319 = EDGE_CURVE('',#30093,#30258,#25545,.T.) ;
#36320 = EDGE_CURVE('',#30419,#30127,#25546,.T.) ;
#36321 = EDGE_CURVE('',#30416,#30128,#25547,.T.) ;
#36322 = EDGE_CURVE('',#30127,#30417,#25548,.T.) ;
#36323 = EDGE_CURVE('',#30128,#30414,#25549,.T.) ;
#36324 = EDGE_CURVE('',#30251,#30261,#25550,.T.) ;
#36325 = EDGE_CURVE('',#30252,#30094,#25551,.T.) ;
#36326 = EDGE_CURVE('',#30252,#30257,#25552,.T.) ;
#36327 = EDGE_CURVE('',#30253,#30256,#25553,.T.) ;
#36328 = EDGE_CURVE('',#30248,#30255,#25554,.T.) ;
#36329 = EDGE_CURVE('',#30249,#30258,#25555,.T.) ;
#36330 = EDGE_CURVE('',#30249,#30093,#25556,.T.) ;
#36331 = EDGE_CURVE('',#30250,#30262,#25557,.T.) ;
#36332 = EDGE_CURVE('',#30102,#30338,#109,.T.) ;
#36333 = EDGE_CURVE('',#30334,#30337,#25558,.T.) ;
#36334 = EDGE_CURVE('',#30335,#30342,#25559,.T.) ;
#36335 = EDGE_CURVE('',#30437,#30341,#110,.T.) ;
#36336 = EDGE_CURVE('',#30438,#30437,#111,.T.) ;
#36337 = EDGE_CURVE('',#30439,#30438,#112,.T.) ;
#36338 = EDGE_CURVE('',#30111,#30439,#113,.T.) ;
#36339 = EDGE_CURVE('',#30193,#30112,#4869,.T.) ;
#36340 = EDGE_CURVE('',#30194,#30341,#25560,.T.) ;
#36341 = EDGE_CURVE('',#30068,#30186,#114,.T.) ;
#36342 = EDGE_CURVE('',#30195,#30340,#25561,.T.) ;
#36343 = EDGE_CURVE('',#30191,#30196,#4870,.T.) ;
#36344 = EDGE_CURVE('',#30339,#30344,#25562,.T.) ;
#36345 = EDGE_CURVE('',#30440,#30340,#115,.T.) ;
#36346 = EDGE_CURVE('',#30441,#30440,#116,.T.) ;
#36347 = EDGE_CURVE('',#30064,#30441,#117,.T.) ;
#36348 = EDGE_CURVE('',#30121,#30415,#25563,.T.) ;
#36349 = EDGE_CURVE('',#30087,#30415,#25564,.T.) ;
#36350 = EDGE_CURVE('',#30416,#30414,#25565,.T.) ;
#36351 = EDGE_CURVE('',#30384,#30380,#25566,.T.) ;
#36352 = EDGE_CURVE('',#30411,#30374,#25567,.T.) ;
#36353 = EDGE_CURVE('',#30381,#30383,#25568,.T.) ;
#36354 = EDGE_CURVE('',#30412,#30373,#25569,.T.) ;
#36355 = EDGE_CURVE('',#30367,#30408,#25570,.T.) ;
#36356 = EDGE_CURVE('',#30391,#30396,#25571,.T.) ;
#36357 = EDGE_CURVE('',#30368,#30407,#25572,.T.) ;
#36358 = EDGE_CURVE('',#30392,#30395,#25573,.T.) ;
#36359 = EDGE_CURVE('',#30348,#30362,#25574,.T.) ;
#36360 = EDGE_CURVE('',#30399,#30361,#25575,.T.) ;
#36361 = EDGE_CURVE('',#30363,#30347,#25576,.T.) ;
#36362 = EDGE_CURVE('',#30400,#30360,#25577,.T.) ;
#36363 = EDGE_CURVE('',#30358,#30404,#25578,.T.) ;
#36364 = EDGE_CURVE('',#30355,#30365,#25579,.T.) ;
#36365 = EDGE_CURVE('',#30359,#30403,#25580,.T.) ;
#36366 = EDGE_CURVE('',#30356,#30364,#25581,.T.) ;
#36367 = EDGE_CURVE('',#30418,#30116,#25582,.T.) ;
#36368 = EDGE_CURVE('',#30418,#30088,#25583,.T.) ;
#36369 = EDGE_CURVE('',#30419,#30417,#25584,.T.) ;
#36370 = EDGE_CURVE('',#30183,#30187,#4871,.T.) ;
#36371 = EDGE_CURVE('',#30184,#30067,#25585,.T.) ;
#36372 = EDGE_CURVE('',#30181,#30338,#25586,.T.) ;
#36373 = EDGE_CURVE('',#30182,#30101,#4872,.T.) ;
#36374 = EDGE_CURVE('',#30442,#30443,#118,.T.) ;
#36375 = EDGE_CURVE('',#30443,#30444,#4873,.T.) ;
#36376 = EDGE_CURVE('',#30444,#30445,#25587,.T.) ;
#36377 = EDGE_CURVE('',#30446,#30445,#4874,.T.) ;
#36378 = EDGE_CURVE('',#30442,#30446,#119,.T.) ;
#36379 = EDGE_CURVE('',#30447,#30448,#120,.T.) ;
#36380 = EDGE_CURVE('',#30448,#30449,#25588,.T.) ;
#36381 = EDGE_CURVE('',#30450,#30449,#4875,.T.) ;
#36382 = EDGE_CURVE('',#30451,#30450,#25589,.T.) ;
#36383 = EDGE_CURVE('',#30447,#30451,#4876,.T.) ;
#36384 = EDGE_CURVE('',#30452,#30452,#25590,.T.) ;
#36385 = EDGE_CURVE('',#30452,#30453,#25591,.T.) ;
#36386 = EDGE_CURVE('',#30453,#30453,#25592,.T.) ;
#36387 = EDGE_CURVE('',#30454,#30454,#25593,.T.) ;
#36388 = EDGE_CURVE('',#30454,#30455,#25594,.T.) ;
#36389 = EDGE_CURVE('',#30455,#30455,#25595,.T.) ;
#36390 = EDGE_CURVE('',#30456,#30457,#25596,.T.) ;
#36391 = EDGE_CURVE('',#30458,#30456,#8634,.T.) ;
#36392 = EDGE_CURVE('',#30458,#30459,#25597,.T.) ;
#36393 = EDGE_CURVE('',#30459,#30460,#25598,.T.) ;
#36394 = EDGE_CURVE('',#30457,#30460,#8635,.T.) ;
#36395 = EDGE_CURVE('',#30461,#30462,#25599,.T.) ;
#36396 = EDGE_CURVE('',#30463,#30461,#8636,.T.) ;
#36397 = EDGE_CURVE('',#30463,#30464,#25600,.T.) ;
#36398 = EDGE_CURVE('',#30462,#30464,#8637,.T.) ;
#36399 = EDGE_CURVE('',#30465,#30466,#25601,.T.) ;
#36400 = EDGE_CURVE('',#30465,#30467,#25602,.T.) ;
#36401 = EDGE_CURVE('',#30468,#30467,#25603,.T.) ;
#36402 = EDGE_CURVE('',#30468,#30466,#25604,.T.) ;
#36403 = EDGE_CURVE('',#30453,#30454,#8638,.T.) ;
#36404 = EDGE_CURVE('',#30466,#30469,#8639,.T.) ;
#36405 = EDGE_CURVE('',#30469,#30463,#25605,.T.) ;
#36406 = EDGE_CURVE('',#30470,#30461,#121,.T.) ;
#36407 = EDGE_CURVE('',#30470,#30471,#25606,.T.) ;
#36408 = EDGE_CURVE('',#30457,#30471,#122,.T.) ;
#36409 = EDGE_CURVE('',#30460,#30472,#25607,.T.) ;
#36410 = EDGE_CURVE('',#30472,#30465,#8640,.T.) ;
#36411 = EDGE_CURVE('',#30473,#30474,#8641,.T.) ;
#36412 = EDGE_CURVE('',#30474,#30475,#8642,.T.) ;
#36413 = EDGE_CURVE('',#30475,#30476,#123,.T.) ;
#36414 = EDGE_CURVE('',#30476,#30477,#8643,.T.) ;
#36415 = EDGE_CURVE('',#30477,#30478,#4877,.T.) ;
#36416 = EDGE_CURVE('',#30478,#30473,#8644,.T.) ;
#36417 = EDGE_CURVE('',#30479,#30480,#8645,.T.) ;
#36418 = EDGE_CURVE('',#30480,#30481,#8646,.T.) ;
#36419 = EDGE_CURVE('',#30481,#30482,#124,.T.) ;
#36420 = EDGE_CURVE('',#30482,#30483,#125,.T.) ;
#36421 = EDGE_CURVE('',#30483,#30484,#8647,.T.) ;
#36422 = EDGE_CURVE('',#30484,#30479,#8648,.T.) ;
#36423 = EDGE_CURVE('',#30485,#30486,#8649,.T.) ;
#36424 = EDGE_CURVE('',#30486,#30487,#8650,.T.) ;
#36425 = EDGE_CURVE('',#30487,#30488,#8651,.T.) ;
#36426 = EDGE_CURVE('',#30488,#30485,#8652,.T.) ;
#36427 = EDGE_CURVE('',#30489,#30490,#8653,.T.) ;
#36428 = EDGE_CURVE('',#30490,#30491,#126,.T.) ;
#36429 = EDGE_CURVE('',#30491,#30492,#127,.T.) ;
#36430 = EDGE_CURVE('',#30492,#30493,#8654,.T.) ;
#36431 = EDGE_CURVE('',#30493,#30494,#8655,.T.) ;
#36432 = EDGE_CURVE('',#30494,#30489,#8656,.T.) ;
#36433 = EDGE_CURVE('',#30495,#30496,#8657,.T.) ;
#36434 = EDGE_CURVE('',#30496,#30497,#8658,.T.) ;
#36435 = EDGE_CURVE('',#30497,#30498,#8659,.T.) ;
#36436 = EDGE_CURVE('',#30498,#30495,#8660,.T.) ;
#36437 = EDGE_CURVE('',#30499,#30500,#8661,.T.) ;
#36438 = EDGE_CURVE('',#30499,#30501,#8662,.T.) ;
#36439 = EDGE_CURVE('',#30501,#30502,#8663,.T.) ;
#36440 = EDGE_CURVE('',#30502,#30500,#8664,.T.) ;
#36441 = EDGE_CURVE('',#30503,#30504,#8665,.T.) ;
#36442 = EDGE_CURVE('',#30503,#30505,#8666,.T.) ;
#36443 = EDGE_CURVE('',#30505,#30506,#8667,.T.) ;
#36444 = EDGE_CURVE('',#30506,#30507,#8668,.T.) ;
#36445 = EDGE_CURVE('',#30507,#30508,#25608,.T.) ;
#36446 = EDGE_CURVE('',#30508,#30504,#8669,.T.) ;
#36447 = EDGE_CURVE('',#30509,#30510,#8670,.T.) ;
#36448 = EDGE_CURVE('',#30509,#30480,#25609,.T.) ;
#36449 = EDGE_CURVE('',#30479,#30486,#25610,.T.) ;
#36450 = EDGE_CURVE('',#30485,#30494,#25611,.T.) ;
#36451 = EDGE_CURVE('',#30493,#30511,#25612,.T.) ;
#36452 = EDGE_CURVE('',#30512,#30511,#8671,.T.) ;
#36453 = EDGE_CURVE('',#30512,#30513,#25613,.T.) ;
#36454 = EDGE_CURVE('',#30514,#30513,#8672,.T.) ;
#36455 = EDGE_CURVE('',#30514,#30515,#25614,.T.) ;
#36456 = EDGE_CURVE('',#30515,#30516,#8673,.T.) ;
#36457 = EDGE_CURVE('',#30516,#30517,#25615,.T.) ;
#36458 = EDGE_CURVE('',#30518,#30517,#8674,.T.) ;
#36459 = EDGE_CURVE('',#30518,#30519,#25616,.T.) ;
#36460 = EDGE_CURVE('',#30519,#30520,#8675,.T.) ;
#36461 = EDGE_CURVE('',#30520,#30521,#25617,.T.) ;
#36462 = EDGE_CURVE('',#30522,#30521,#8676,.T.) ;
#36463 = EDGE_CURVE('',#30522,#30498,#25618,.T.) ;
#36464 = EDGE_CURVE('',#30497,#30523,#25619,.T.) ;
#36465 = EDGE_CURVE('',#30523,#30524,#8677,.T.) ;
#36466 = EDGE_CURVE('',#30524,#30506,#25620,.T.) ;
#36467 = EDGE_CURVE('',#30505,#30525,#25621,.T.) ;
#36468 = EDGE_CURVE('',#30526,#30525,#8678,.T.) ;
#36469 = EDGE_CURVE('',#30527,#30526,#8679,.T.) ;
#36470 = EDGE_CURVE('',#30527,#30528,#25622,.T.) ;
#36471 = EDGE_CURVE('',#30529,#30528,#8680,.T.) ;
#36472 = EDGE_CURVE('',#30529,#30530,#25623,.T.) ;
#36473 = EDGE_CURVE('',#30531,#30530,#8681,.T.) ;
#36474 = EDGE_CURVE('',#30531,#30510,#25624,.T.) ;
#36475 = EDGE_CURVE('',#30532,#30533,#8682,.T.) ;
#36476 = EDGE_CURVE('',#30533,#30534,#25625,.T.) ;
#36477 = EDGE_CURVE('',#30534,#30535,#8683,.T.) ;
#36478 = EDGE_CURVE('',#30535,#30536,#25626,.T.) ;
#36479 = EDGE_CURVE('',#30536,#30537,#8684,.T.) ;
#36480 = EDGE_CURVE('',#30537,#30538,#25627,.T.) ;
#36481 = EDGE_CURVE('',#30538,#30539,#8685,.T.) ;
#36482 = EDGE_CURVE('',#30539,#30540,#25628,.T.) ;
#36483 = EDGE_CURVE('',#30540,#30541,#8686,.T.) ;
#36484 = EDGE_CURVE('',#30541,#30542,#8687,.T.) ;
#36485 = EDGE_CURVE('',#30542,#30503,#25629,.T.) ;
#36486 = EDGE_CURVE('',#30504,#30543,#25630,.T.) ;
#36487 = EDGE_CURVE('',#30543,#30544,#8688,.T.) ;
#36488 = EDGE_CURVE('',#30544,#30499,#25631,.T.) ;
#36489 = EDGE_CURVE('',#30500,#30545,#25632,.T.) ;
#36490 = EDGE_CURVE('',#30546,#30545,#8689,.T.) ;
#36491 = EDGE_CURVE('',#30546,#30547,#25633,.T.) ;
#36492 = EDGE_CURVE('',#30548,#30547,#8690,.T.) ;
#36493 = EDGE_CURVE('',#30548,#30549,#25634,.T.) ;
#36494 = EDGE_CURVE('',#30549,#30550,#8691,.T.) ;
#36495 = EDGE_CURVE('',#30550,#30551,#25635,.T.) ;
#36496 = EDGE_CURVE('',#30552,#30551,#8692,.T.) ;
#36497 = EDGE_CURVE('',#30552,#30553,#25636,.T.) ;
#36498 = EDGE_CURVE('',#30554,#30553,#8693,.T.) ;
#36499 = EDGE_CURVE('',#30554,#30555,#25637,.T.) ;
#36500 = EDGE_CURVE('',#30555,#30556,#8694,.T.) ;
#36501 = EDGE_CURVE('',#30556,#30557,#25638,.T.) ;
#36502 = EDGE_CURVE('',#30557,#30558,#8695,.T.) ;
#36503 = EDGE_CURVE('',#30558,#30559,#25639,.T.) ;
#36504 = EDGE_CURVE('',#30559,#30560,#8696,.T.) ;
#36505 = EDGE_CURVE('',#30560,#30532,#25640,.T.) ;
#36506 = EDGE_CURVE('',#30528,#30539,#8697,.T.) ;
#36507 = EDGE_CURVE('',#30538,#30529,#8698,.T.) ;
#36508 = EDGE_CURVE('',#30530,#30537,#8699,.T.) ;
#36509 = EDGE_CURVE('',#30536,#30531,#8700,.T.) ;
#36510 = EDGE_CURVE('',#30561,#30562,#128,.T.) ;
#36511 = EDGE_CURVE('',#30562,#30509,#8701,.T.) ;
#36512 = EDGE_CURVE('',#30510,#30535,#8702,.T.) ;
#36513 = EDGE_CURVE('',#30534,#30563,#8703,.T.) ;
#36514 = EDGE_CURVE('',#30563,#30564,#129,.T.) ;
#36515 = EDGE_CURVE('',#30564,#30561,#8704,.T.) ;
#36516 = EDGE_CURVE('',#30565,#30566,#130,.T.) ;
#36517 = EDGE_CURVE('',#30566,#30567,#4878,.T.) ;
#36518 = EDGE_CURVE('',#30567,#30533,#8705,.T.) ;
#36519 = EDGE_CURVE('',#30532,#30568,#8706,.T.) ;
#36520 = EDGE_CURVE('',#30568,#30565,#8707,.T.) ;
#36521 = EDGE_CURVE('',#30569,#30570,#8708,.T.) ;
#36522 = EDGE_CURVE('',#30570,#30560,#8709,.T.) ;
#36523 = EDGE_CURVE('',#30559,#30569,#8710,.T.) ;
#36524 = EDGE_CURVE('',#30571,#30442,#131,.T.) ;
#36525 = EDGE_CURVE('',#30446,#30572,#8711,.T.) ;
#36526 = EDGE_CURVE('',#30572,#30558,#8712,.T.) ;
#36527 = EDGE_CURVE('',#30557,#30571,#8713,.T.) ;
#36528 = EDGE_CURVE('',#30511,#30573,#8714,.T.) ;
#36529 = EDGE_CURVE('',#30573,#30574,#132,.T.) ;
#36530 = EDGE_CURVE('',#30574,#30575,#8715,.T.) ;
#36531 = EDGE_CURVE('',#30575,#30576,#133,.T.) ;
#36532 = EDGE_CURVE('',#30576,#30556,#8716,.T.) ;
#36533 = EDGE_CURVE('',#30555,#30577,#8717,.T.) ;
#36534 = EDGE_CURVE('',#30577,#30578,#8718,.T.) ;
#36535 = EDGE_CURVE('',#30579,#30578,#25641,.T.) ;
#36536 = EDGE_CURVE('',#30579,#30580,#8719,.T.) ;
#36537 = EDGE_CURVE('',#30581,#30580,#25642,.T.) ;
#36538 = EDGE_CURVE('',#30581,#30582,#8720,.T.) ;
#36539 = EDGE_CURVE('',#30582,#30512,#8721,.T.) ;
#36540 = EDGE_CURVE('',#30583,#30584,#25643,.T.) ;
#36541 = EDGE_CURVE('',#30583,#30518,#8722,.T.) ;
#36542 = EDGE_CURVE('',#30517,#30585,#8723,.T.) ;
#36543 = EDGE_CURVE('',#30586,#30585,#25644,.T.) ;
#36544 = EDGE_CURVE('',#30586,#30587,#25645,.T.) ;
#36545 = EDGE_CURVE('',#30588,#30587,#25646,.T.) ;
#36546 = EDGE_CURVE('',#30588,#30589,#8724,.T.) ;
#36547 = EDGE_CURVE('',#30589,#30590,#8725,.T.) ;
#36548 = EDGE_CURVE('',#30590,#30591,#8726,.T.) ;
#36549 = EDGE_CURVE('',#30592,#30591,#25647,.T.) ;
#36550 = EDGE_CURVE('',#30592,#30593,#25648,.T.) ;
#36551 = EDGE_CURVE('',#30594,#30593,#25649,.T.) ;
#36552 = EDGE_CURVE('',#30594,#30550,#8727,.T.) ;
#36553 = EDGE_CURVE('',#30549,#30595,#8728,.T.) ;
#36554 = EDGE_CURVE('',#30596,#30595,#25650,.T.) ;
#36555 = EDGE_CURVE('',#30596,#30597,#25651,.T.) ;
#36556 = EDGE_CURVE('',#30598,#30597,#25652,.T.) ;
#36557 = EDGE_CURVE('',#30598,#30599,#8729,.T.) ;
#36558 = EDGE_CURVE('',#30599,#30600,#25653,.T.) ;
#36559 = EDGE_CURVE('',#30600,#30601,#8730,.T.) ;
#36560 = EDGE_CURVE('',#30602,#30601,#25654,.T.) ;
#36561 = EDGE_CURVE('',#30602,#30584,#25655,.T.) ;
#36562 = EDGE_CURVE('',#30603,#30604,#25656,.T.) ;
#36563 = EDGE_CURVE('',#30603,#30605,#8731,.T.) ;
#36564 = EDGE_CURVE('',#30526,#30605,#8732,.T.) ;
#36565 = EDGE_CURVE('',#30525,#30542,#8733,.T.) ;
#36566 = EDGE_CURVE('',#30606,#30541,#8734,.T.) ;
#36567 = EDGE_CURVE('',#30606,#30607,#8735,.T.) ;
#36568 = EDGE_CURVE('',#30608,#30607,#25657,.T.) ;
#36569 = EDGE_CURVE('',#30608,#30604,#8736,.T.) ;
#36570 = EDGE_CURVE('',#30609,#30610,#25658,.T.) ;
#36571 = EDGE_CURVE('',#30609,#30606,#8737,.T.) ;
#36572 = EDGE_CURVE('',#30540,#30527,#8738,.T.) ;
#36573 = EDGE_CURVE('',#30605,#30611,#8739,.T.) ;
#36574 = EDGE_CURVE('',#30612,#30611,#25659,.T.) ;
#36575 = EDGE_CURVE('',#30612,#30610,#8740,.T.) ;
#36576 = EDGE_CURVE('',#30613,#30614,#8741,.T.) ;
#36577 = EDGE_CURVE('',#30614,#30615,#8742,.T.) ;
#36578 = EDGE_CURVE('',#30613,#30615,#25660,.T.) ;
#36579 = EDGE_CURVE('',#30616,#30617,#25661,.T.) ;
#36580 = EDGE_CURVE('',#30616,#30618,#8743,.T.) ;
#36581 = EDGE_CURVE('',#30618,#30617,#8744,.T.) ;
#36582 = EDGE_CURVE('',#30619,#30620,#8745,.T.) ;
#36583 = EDGE_CURVE('',#30620,#30621,#8746,.T.) ;
#36584 = EDGE_CURVE('',#30621,#30622,#8747,.T.) ;
#36585 = EDGE_CURVE('',#30622,#30623,#8748,.T.) ;
#36586 = EDGE_CURVE('',#30623,#30624,#8749,.T.) ;
#36587 = EDGE_CURVE('',#30624,#30625,#8750,.T.) ;
#36588 = EDGE_CURVE('',#30625,#30626,#8751,.T.) ;
#36589 = EDGE_CURVE('',#30626,#30619,#8752,.T.) ;
#36590 = EDGE_CURVE('',#30627,#30628,#8753,.T.) ;
#36591 = EDGE_CURVE('',#30628,#30629,#8754,.T.) ;
#36592 = EDGE_CURVE('',#30629,#30630,#8755,.T.) ;
#36593 = EDGE_CURVE('',#30630,#30627,#8756,.T.) ;
#36594 = EDGE_CURVE('',#30631,#30632,#8757,.T.) ;
#36595 = EDGE_CURVE('',#30632,#30633,#8758,.T.) ;
#36596 = EDGE_CURVE('',#30633,#30634,#8759,.T.) ;
#36597 = EDGE_CURVE('',#30634,#30631,#8760,.T.) ;
#36598 = EDGE_CURVE('',#30635,#30636,#8761,.T.) ;
#36599 = EDGE_CURVE('',#30636,#30637,#8762,.T.) ;
#36600 = EDGE_CURVE('',#30637,#30638,#8763,.T.) ;
#36601 = EDGE_CURVE('',#30638,#30635,#8764,.T.) ;
#36602 = EDGE_CURVE('',#30639,#30640,#134,.T.) ;
#36603 = EDGE_CURVE('',#30640,#30641,#8765,.T.) ;
#36604 = EDGE_CURVE('',#30641,#30642,#8766,.T.) ;
#36605 = EDGE_CURVE('',#30642,#30643,#8767,.T.) ;
#36606 = EDGE_CURVE('',#30643,#30644,#135,.T.) ;
#36607 = EDGE_CURVE('',#30644,#30639,#8768,.T.) ;
#36608 = EDGE_CURVE('',#30645,#30646,#8769,.T.) ;
#36609 = EDGE_CURVE('',#30646,#30647,#8770,.T.) ;
#36610 = EDGE_CURVE('',#30647,#30648,#8771,.T.) ;
#36611 = EDGE_CURVE('',#30648,#30649,#8772,.T.) ;
#36612 = EDGE_CURVE('',#30649,#30650,#8773,.T.) ;
#36613 = EDGE_CURVE('',#30650,#30651,#8774,.T.) ;
#36614 = EDGE_CURVE('',#30651,#30652,#8775,.T.) ;
#36615 = EDGE_CURVE('',#30652,#30645,#8776,.T.) ;
#36616 = EDGE_CURVE('',#30653,#30654,#8777,.T.) ;
#36617 = EDGE_CURVE('',#30653,#30655,#25662,.T.) ;
#36618 = EDGE_CURVE('',#30655,#30656,#8778,.T.) ;
#36619 = EDGE_CURVE('',#30656,#30657,#25663,.T.) ;
#36620 = EDGE_CURVE('',#30657,#30658,#8779,.T.) ;
#36621 = EDGE_CURVE('',#30658,#30659,#25664,.T.) ;
#36622 = EDGE_CURVE('',#30659,#30660,#8780,.T.) ;
#36623 = EDGE_CURVE('',#30660,#30654,#25665,.T.) ;
#36624 = EDGE_CURVE('',#30661,#30662,#25666,.T.) ;
#36625 = EDGE_CURVE('',#30661,#30522,#8781,.T.) ;
#36626 = EDGE_CURVE('',#30521,#30663,#8782,.T.) ;
#36627 = EDGE_CURVE('',#30663,#30664,#25667,.T.) ;
#36628 = EDGE_CURVE('',#30664,#30665,#8783,.T.) ;
#36629 = EDGE_CURVE('',#30665,#30662,#25668,.T.) ;
#36630 = EDGE_CURVE('',#30519,#30666,#8784,.T.) ;
#36631 = EDGE_CURVE('',#30666,#30667,#8785,.T.) ;
#36632 = EDGE_CURVE('',#30667,#30520,#8786,.T.) ;
#36633 = EDGE_CURVE('',#30668,#30669,#8787,.T.) ;
#36634 = EDGE_CURVE('',#30669,#30462,#8788,.T.) ;
#36635 = EDGE_CURVE('',#30464,#30668,#8789,.T.) ;
#36636 = EDGE_CURVE('',#30670,#30671,#25669,.T.) ;
#36637 = EDGE_CURVE('',#30671,#30672,#8790,.T.) ;
#36638 = EDGE_CURVE('',#30672,#30673,#25670,.T.) ;
#36639 = EDGE_CURVE('',#30673,#30670,#8791,.T.) ;
#36640 = EDGE_CURVE('',#30674,#30675,#25671,.T.) ;
#36641 = EDGE_CURVE('',#30675,#30676,#8792,.T.) ;
#36642 = EDGE_CURVE('',#30676,#30677,#25672,.T.) ;
#36643 = EDGE_CURVE('',#30677,#30674,#8793,.T.) ;
#36644 = EDGE_CURVE('',#30456,#30678,#8794,.T.) ;
#36645 = EDGE_CURVE('',#30678,#30679,#8795,.T.) ;
#36646 = EDGE_CURVE('',#30679,#30458,#8796,.T.) ;
#36647 = EDGE_CURVE('',#30680,#30681,#8797,.T.) ;
#36648 = EDGE_CURVE('',#30681,#30548,#8798,.T.) ;
#36649 = EDGE_CURVE('',#30547,#30680,#8799,.T.) ;
#36650 = EDGE_CURVE('',#30682,#30683,#25673,.T.) ;
#36651 = EDGE_CURVE('',#30683,#30546,#8800,.T.) ;
#36652 = EDGE_CURVE('',#30545,#30684,#8801,.T.) ;
#36653 = EDGE_CURVE('',#30685,#30684,#25674,.T.) ;
#36654 = EDGE_CURVE('',#30685,#30686,#25675,.T.) ;
#36655 = EDGE_CURVE('',#30686,#30682,#8802,.T.) ;
#36656 = EDGE_CURVE('',#30687,#30688,#25676,.T.) ;
#36657 = EDGE_CURVE('',#30688,#30514,#8803,.T.) ;
#36658 = EDGE_CURVE('',#30513,#30689,#8804,.T.) ;
#36659 = EDGE_CURVE('',#30689,#30687,#8805,.T.) ;
#36660 = EDGE_CURVE('',#30690,#30691,#8806,.T.) ;
#36661 = EDGE_CURVE('',#30691,#30516,#8807,.T.) ;
#36662 = EDGE_CURVE('',#30515,#30690,#8808,.T.) ;
#36663 = EDGE_CURVE('',#30692,#30693,#25677,.T.) ;
#36664 = EDGE_CURVE('',#30693,#30694,#8809,.T.) ;
#36665 = EDGE_CURVE('',#30694,#30695,#25678,.T.) ;
#36666 = EDGE_CURVE('',#30695,#30692,#8810,.T.) ;
#36667 = EDGE_CURVE('',#30696,#30697,#8811,.T.) ;
#36668 = EDGE_CURVE('',#30697,#30698,#8812,.T.) ;
#36669 = EDGE_CURVE('',#30698,#30699,#8813,.T.) ;
#36670 = EDGE_CURVE('',#30699,#30696,#8814,.T.) ;
#36671 = EDGE_CURVE('',#30700,#30701,#25679,.T.) ;
#36672 = EDGE_CURVE('',#30701,#30702,#8815,.T.) ;
#36673 = EDGE_CURVE('',#30702,#30703,#25680,.T.) ;
#36674 = EDGE_CURVE('',#30703,#30700,#8816,.T.) ;
#36675 = EDGE_CURVE('',#30551,#30704,#8817,.T.) ;
#36676 = EDGE_CURVE('',#30704,#30705,#8818,.T.) ;
#36677 = EDGE_CURVE('',#30705,#30552,#8819,.T.) ;
#36678 = EDGE_CURVE('',#30706,#30707,#8820,.T.) ;
#36679 = EDGE_CURVE('',#30707,#30708,#8821,.T.) ;
#36680 = EDGE_CURVE('',#30708,#30709,#8822,.T.) ;
#36681 = EDGE_CURVE('',#30709,#30706,#8823,.T.) ;
#36682 = EDGE_CURVE('',#30710,#30711,#8824,.T.) ;
#36683 = EDGE_CURVE('',#30711,#30554,#8825,.T.) ;
#36684 = EDGE_CURVE('',#30553,#30712,#8826,.T.) ;
#36685 = EDGE_CURVE('',#30712,#30710,#25681,.T.) ;
#36686 = EDGE_CURVE('',#30713,#30714,#8827,.T.) ;
#36687 = EDGE_CURVE('',#30714,#30715,#8828,.T.) ;
#36688 = EDGE_CURVE('',#30715,#30716,#8829,.T.) ;
#36689 = EDGE_CURVE('',#30716,#30713,#8830,.T.) ;
#36690 = EDGE_CURVE('',#30717,#30718,#4879,.T.) ;
#36691 = EDGE_CURVE('',#30718,#30447,#8831,.T.) ;
#36692 = EDGE_CURVE('',#30451,#30719,#8832,.T.) ;
#36693 = EDGE_CURVE('',#30719,#30720,#4880,.T.) ;
#36694 = EDGE_CURVE('',#30720,#30721,#8833,.T.) ;
#36695 = EDGE_CURVE('',#30721,#30722,#4881,.T.) ;
#36696 = EDGE_CURVE('',#30722,#30717,#8834,.T.) ;
#36697 = EDGE_CURVE('',#30723,#30724,#8835,.T.) ;
#36698 = EDGE_CURVE('',#30724,#30450,#8836,.T.) ;
#36699 = EDGE_CURVE('',#30450,#30725,#8837,.T.) ;
#36700 = EDGE_CURVE('',#30725,#30723,#8838,.T.) ;
#36701 = EDGE_CURVE('',#30726,#30727,#8839,.T.) ;
#36702 = EDGE_CURVE('',#30727,#30728,#8840,.T.) ;
#36703 = EDGE_CURVE('',#30728,#30729,#8841,.T.) ;
#36704 = EDGE_CURVE('',#30729,#30726,#8842,.T.) ;
#36705 = EDGE_CURVE('',#30730,#30731,#8843,.T.) ;
#36706 = EDGE_CURVE('',#30731,#30732,#8844,.T.) ;
#36707 = EDGE_CURVE('',#30732,#30733,#8845,.T.) ;
#36708 = EDGE_CURVE('',#30733,#30730,#8846,.T.) ;
#36709 = EDGE_CURVE('',#30734,#30735,#8847,.T.) ;
#36710 = EDGE_CURVE('',#30735,#30736,#8848,.T.) ;
#36711 = EDGE_CURVE('',#30736,#30737,#8849,.T.) ;
#36712 = EDGE_CURVE('',#30737,#30734,#8850,.T.) ;
#36713 = EDGE_CURVE('',#30654,#30738,#8851,.T.) ;
#36714 = EDGE_CURVE('',#30738,#30739,#8852,.T.) ;
#36715 = EDGE_CURVE('',#30739,#30653,#8853,.T.) ;
#36716 = EDGE_CURVE('',#30657,#30740,#8854,.T.) ;
#36717 = EDGE_CURVE('',#30740,#30741,#8855,.T.) ;
#36718 = EDGE_CURVE('',#30741,#30658,#8856,.T.) ;
#36719 = EDGE_CURVE('',#30659,#30742,#8857,.T.) ;
#36720 = EDGE_CURVE('',#30742,#30743,#8858,.T.) ;
#36721 = EDGE_CURVE('',#30743,#30660,#8859,.T.) ;
#36722 = EDGE_CURVE('',#30655,#30744,#8860,.T.) ;
#36723 = EDGE_CURVE('',#30744,#30745,#8861,.T.) ;
#36724 = EDGE_CURVE('',#30745,#30656,#8862,.T.) ;
#36725 = EDGE_CURVE('',#30746,#30747,#8863,.T.) ;
#36726 = EDGE_CURVE('',#30747,#30748,#8864,.T.) ;
#36727 = EDGE_CURVE('',#30748,#30749,#8865,.T.) ;
#36728 = EDGE_CURVE('',#30749,#30750,#25682,.T.) ;
#36729 = EDGE_CURVE('',#30750,#30751,#8866,.T.) ;
#36730 = EDGE_CURVE('',#30751,#30746,#25683,.T.) ;
#36731 = EDGE_CURVE('',#30752,#30753,#8867,.T.) ;
#36732 = EDGE_CURVE('',#30753,#30754,#8868,.T.) ;
#36733 = EDGE_CURVE('',#30754,#30755,#8869,.T.) ;
#36734 = EDGE_CURVE('',#30755,#30756,#25684,.T.) ;
#36735 = EDGE_CURVE('',#30756,#30757,#8870,.T.) ;
#36736 = EDGE_CURVE('',#30757,#30752,#25685,.T.) ;
#36737 = EDGE_CURVE('',#30758,#30759,#8871,.T.) ;
#36738 = EDGE_CURVE('',#30758,#30477,#25686,.T.) ;
#36739 = EDGE_CURVE('',#30476,#30759,#25687,.T.) ;
#36740 = EDGE_CURVE('',#30759,#30760,#8872,.T.) ;
#36741 = EDGE_CURVE('',#30760,#30761,#8873,.T.) ;
#36742 = EDGE_CURVE('',#30761,#30758,#8874,.T.) ;
#36743 = EDGE_CURVE('',#30762,#30763,#8875,.T.) ;
#36744 = EDGE_CURVE('',#30763,#30764,#8876,.T.) ;
#36745 = EDGE_CURVE('',#30764,#30765,#8877,.T.) ;
#36746 = EDGE_CURVE('',#30765,#30762,#8878,.T.) ;
#36747 = EDGE_CURVE('',#30766,#30767,#8879,.T.) ;
#36748 = EDGE_CURVE('',#30767,#30768,#8880,.T.) ;
#36749 = EDGE_CURVE('',#30768,#30769,#8881,.T.) ;
#36750 = EDGE_CURVE('',#30769,#30766,#8882,.T.) ;
#36751 = EDGE_CURVE('',#30770,#30771,#8883,.T.) ;
#36752 = EDGE_CURVE('',#30771,#30772,#8884,.T.) ;
#36753 = EDGE_CURVE('',#30772,#30773,#8885,.T.) ;
#36754 = EDGE_CURVE('',#30773,#30770,#8886,.T.) ;
#36755 = EDGE_CURVE('',#30774,#30775,#8887,.T.) ;
#36756 = EDGE_CURVE('',#30775,#30776,#8888,.T.) ;
#36757 = EDGE_CURVE('',#30776,#30777,#8889,.T.) ;
#36758 = EDGE_CURVE('',#30774,#30777,#8890,.T.) ;
#36759 = EDGE_CURVE('',#30644,#30774,#25688,.T.) ;
#36760 = EDGE_CURVE('',#30777,#30639,#25689,.T.) ;
#36761 = EDGE_CURVE('',#30778,#30779,#8891,.T.) ;
#36762 = EDGE_CURVE('',#30779,#30780,#8892,.T.) ;
#36763 = EDGE_CURVE('',#30780,#30781,#8893,.T.) ;
#36764 = EDGE_CURVE('',#30781,#30778,#8894,.T.) ;
#36765 = EDGE_CURVE('',#30782,#30783,#8895,.T.) ;
#36766 = EDGE_CURVE('',#30783,#30784,#8896,.T.) ;
#36767 = EDGE_CURVE('',#30784,#30785,#8897,.T.) ;
#36768 = EDGE_CURVE('',#30785,#30782,#8898,.T.) ;
#36769 = EDGE_CURVE('',#30786,#30787,#8899,.T.) ;
#36770 = EDGE_CURVE('',#30787,#30788,#8900,.T.) ;
#36771 = EDGE_CURVE('',#30788,#30789,#8901,.T.) ;
#36772 = EDGE_CURVE('',#30789,#30786,#8902,.T.) ;
#36773 = EDGE_CURVE('',#30790,#30791,#8903,.T.) ;
#36774 = EDGE_CURVE('',#30791,#30792,#8904,.T.) ;
#36775 = EDGE_CURVE('',#30792,#30793,#8905,.T.) ;
#36776 = EDGE_CURVE('',#30793,#30790,#8906,.T.) ;
#36777 = EDGE_CURVE('',#30543,#30794,#8907,.T.) ;
#36778 = EDGE_CURVE('',#30794,#30795,#25690,.T.) ;
#36779 = EDGE_CURVE('',#30795,#30544,#8908,.T.) ;
#36780 = EDGE_CURVE('',#30796,#30797,#25691,.T.) ;
#36781 = EDGE_CURVE('',#30797,#30468,#25692,.T.) ;
#36782 = EDGE_CURVE('',#30467,#30796,#25693,.T.) ;
#36783 = EDGE_CURVE('',#30523,#30798,#8909,.T.) ;
#36784 = EDGE_CURVE('',#30798,#30799,#25694,.T.) ;
#36785 = EDGE_CURVE('',#30799,#30524,#8910,.T.) ;
#36786 = EDGE_CURVE('',#30712,#30705,#25695,.T.) ;
#36787 = EDGE_CURVE('',#30712,#30701,#25696,.T.) ;
#36788 = EDGE_CURVE('',#30701,#30705,#25697,.T.) ;
#36789 = EDGE_CURVE('',#30704,#30594,#25698,.T.) ;
#36790 = EDGE_CURVE('',#30702,#30704,#25699,.T.) ;
#36791 = EDGE_CURVE('',#30710,#30700,#25700,.T.) ;
#36792 = EDGE_CURVE('',#30702,#30593,#25701,.T.) ;
#36793 = EDGE_CURVE('',#30710,#30709,#25702,.T.) ;
#36794 = EDGE_CURVE('',#30709,#30700,#25703,.T.) ;
#36795 = EDGE_CURVE('',#30690,#30688,#25704,.T.) ;
#36796 = EDGE_CURVE('',#30691,#30695,#25705,.T.) ;
#36797 = EDGE_CURVE('',#30692,#30690,#25706,.T.) ;
#36798 = EDGE_CURVE('',#30585,#30691,#25707,.T.) ;
#36799 = EDGE_CURVE('',#30703,#30592,#25708,.T.) ;
#36800 = EDGE_CURVE('',#30706,#30703,#25709,.T.) ;
#36801 = EDGE_CURVE('',#30711,#30708,#25710,.T.) ;
#36802 = EDGE_CURVE('',#30577,#30711,#25711,.T.) ;
#36803 = EDGE_CURVE('',#30692,#30688,#25712,.T.) ;
#36804 = EDGE_CURVE('',#30586,#30695,#25713,.T.) ;
#36805 = EDGE_CURVE('',#30706,#30591,#25714,.T.) ;
#36806 = EDGE_CURVE('',#30577,#30708,#25715,.T.) ;
#36807 = EDGE_CURVE('',#30693,#30687,#25716,.T.) ;
#36808 = EDGE_CURVE('',#30694,#30699,#25717,.T.) ;
#36809 = EDGE_CURVE('',#30696,#30693,#25718,.T.) ;
#36810 = EDGE_CURVE('',#30587,#30694,#25719,.T.) ;
#36811 = EDGE_CURVE('',#30707,#30590,#25720,.T.) ;
#36812 = EDGE_CURVE('',#30578,#30707,#25721,.T.) ;
#36813 = EDGE_CURVE('',#30696,#30687,#25722,.T.) ;
#36814 = EDGE_CURVE('',#30588,#30699,#25723,.T.) ;
#36815 = EDGE_CURVE('',#30579,#30590,#25724,.T.) ;
#36816 = EDGE_CURVE('',#30689,#30582,#25725,.T.) ;
#36817 = EDGE_CURVE('',#30697,#30689,#25726,.T.) ;
#36818 = EDGE_CURVE('',#30589,#30698,#25727,.T.) ;
#36819 = EDGE_CURVE('',#30580,#30589,#25728,.T.) ;
#36820 = EDGE_CURVE('',#30697,#30582,#25729,.T.) ;
#36821 = EDGE_CURVE('',#30581,#30698,#25730,.T.) ;
#36822 = EDGE_CURVE('',#30645,#30626,#25731,.T.) ;
#36823 = EDGE_CURVE('',#30634,#30645,#25732,.T.) ;
#36824 = EDGE_CURVE('',#30626,#30634,#25733,.T.) ;
#36825 = EDGE_CURVE('',#30652,#30800,#136,.T.) ;
#36826 = EDGE_CURVE('',#30800,#30631,#4882,.T.) ;
#36827 = EDGE_CURVE('',#30633,#30801,#4883,.T.) ;
#36828 = EDGE_CURVE('',#30801,#30619,#137,.T.) ;
#36829 = EDGE_CURVE('',#30646,#30625,#25734,.T.) ;
#36830 = EDGE_CURVE('',#30641,#30802,#4884,.T.) ;
#36831 = EDGE_CURVE('',#30802,#30652,#138,.T.) ;
#36832 = EDGE_CURVE('',#30651,#30803,#139,.T.) ;
#36833 = EDGE_CURVE('',#30803,#30642,#4885,.T.) ;
#36834 = EDGE_CURVE('',#30619,#30804,#140,.T.) ;
#36835 = EDGE_CURVE('',#30804,#30636,#4886,.T.) ;
#36836 = EDGE_CURVE('',#30635,#30805,#4887,.T.) ;
#36837 = EDGE_CURVE('',#30805,#30620,#141,.T.) ;
#36838 = EDGE_CURVE('',#30646,#30617,#25735,.T.) ;
#36839 = EDGE_CURVE('',#30616,#30625,#25736,.T.) ;
#36840 = EDGE_CURVE('',#30806,#30617,#8911,.T.) ;
#36841 = EDGE_CURVE('',#30647,#30806,#25737,.T.) ;
#36842 = EDGE_CURVE('',#30807,#30806,#25738,.T.) ;
#36843 = EDGE_CURVE('',#30647,#30807,#25739,.T.) ;
#36844 = EDGE_CURVE('',#30630,#30808,#4888,.T.) ;
#36845 = EDGE_CURVE('',#30808,#30651,#142,.T.) ;
#36846 = EDGE_CURVE('',#30627,#30650,#25740,.T.) ;
#36847 = EDGE_CURVE('',#30620,#30809,#143,.T.) ;
#36848 = EDGE_CURVE('',#30809,#30628,#4889,.T.) ;
#36849 = EDGE_CURVE('',#30621,#30627,#25741,.T.) ;
#36850 = EDGE_CURVE('',#30810,#30624,#25742,.T.) ;
#36851 = EDGE_CURVE('',#30616,#30810,#8912,.T.) ;
#36852 = EDGE_CURVE('',#30605,#30618,#4890,.T.) ;
#36853 = EDGE_CURVE('',#30806,#30603,#25743,.T.) ;
#36854 = EDGE_CURVE('',#30807,#30604,#25744,.T.) ;
#36855 = EDGE_CURVE('',#30811,#30807,#8913,.T.) ;
#36856 = EDGE_CURVE('',#30648,#30811,#25745,.T.) ;
#36857 = EDGE_CURVE('',#30621,#30650,#25746,.T.) ;
#36858 = EDGE_CURVE('',#30810,#30812,#25747,.T.) ;
#36859 = EDGE_CURVE('',#30812,#30624,#25748,.T.) ;
#36860 = EDGE_CURVE('',#30611,#30810,#25749,.T.) ;
#36861 = EDGE_CURVE('',#30811,#30608,#25750,.T.) ;
#36862 = EDGE_CURVE('',#30813,#30811,#25751,.T.) ;
#36863 = EDGE_CURVE('',#30648,#30813,#25752,.T.) ;
#36864 = EDGE_CURVE('',#30622,#30649,#25753,.T.) ;
#36865 = EDGE_CURVE('',#30814,#30623,#25754,.T.) ;
#36866 = EDGE_CURVE('',#30812,#30814,#8914,.T.) ;
#36867 = EDGE_CURVE('',#30612,#30812,#25755,.T.) ;
#36868 = EDGE_CURVE('',#30813,#30607,#25756,.T.) ;
#36869 = EDGE_CURVE('',#30613,#30813,#8915,.T.) ;
#36870 = EDGE_CURVE('',#30649,#30613,#25757,.T.) ;
#36871 = EDGE_CURVE('',#30622,#30615,#25758,.T.) ;
#36872 = EDGE_CURVE('',#30814,#30815,#25759,.T.) ;
#36873 = EDGE_CURVE('',#30815,#30623,#25760,.T.) ;
#36874 = EDGE_CURVE('',#30610,#30814,#25761,.T.) ;
#36875 = EDGE_CURVE('',#30614,#30606,#4891,.T.) ;
#36876 = EDGE_CURVE('',#30815,#30615,#8916,.T.) ;
#36877 = EDGE_CURVE('',#30609,#30815,#25762,.T.) ;
#36878 = EDGE_CURVE('',#30663,#30667,#25763,.T.) ;
#36879 = EDGE_CURVE('',#30663,#30671,#25764,.T.) ;
#36880 = EDGE_CURVE('',#30671,#30667,#25765,.T.) ;
#36881 = EDGE_CURVE('',#30666,#30583,#25766,.T.) ;
#36882 = EDGE_CURVE('',#30672,#30666,#25767,.T.) ;
#36883 = EDGE_CURVE('',#30664,#30670,#25768,.T.) ;
#36884 = EDGE_CURVE('',#30495,#30661,#25769,.T.) ;
#36885 = EDGE_CURVE('',#30466,#30496,#25770,.T.) ;
#36886 = EDGE_CURVE('',#30469,#30495,#25771,.T.) ;
#36887 = EDGE_CURVE('',#30672,#30584,#25772,.T.) ;
#36888 = EDGE_CURVE('',#30664,#30668,#25773,.T.) ;
#36889 = EDGE_CURVE('',#30668,#30670,#25774,.T.) ;
#36890 = EDGE_CURVE('',#30469,#30662,#25775,.T.) ;
#36891 = EDGE_CURVE('',#30673,#30602,#25776,.T.) ;
#36892 = EDGE_CURVE('',#30669,#30673,#25777,.T.) ;
#36893 = EDGE_CURVE('',#30665,#30464,#25778,.T.) ;
#36894 = EDGE_CURVE('',#30463,#30665,#25779,.T.) ;
#36895 = EDGE_CURVE('',#30501,#30465,#25780,.T.) ;
#36896 = EDGE_CURVE('',#30502,#30472,#25781,.T.) ;
#36897 = EDGE_CURVE('',#30684,#30502,#25782,.T.) ;
#36898 = EDGE_CURVE('',#30680,#30683,#25783,.T.) ;
#36899 = EDGE_CURVE('',#30669,#30601,#25784,.T.) ;
#36900 = EDGE_CURVE('',#30685,#30472,#25785,.T.) ;
#36901 = EDGE_CURVE('',#30680,#30674,#25786,.T.) ;
#36902 = EDGE_CURVE('',#30674,#30683,#25787,.T.) ;
#36903 = EDGE_CURVE('',#30462,#30600,#144,.T.) ;
#36904 = EDGE_CURVE('',#30686,#30460,#25788,.T.) ;
#36905 = EDGE_CURVE('',#30682,#30679,#25789,.T.) ;
#36906 = EDGE_CURVE('',#30458,#30686,#25790,.T.) ;
#36907 = EDGE_CURVE('',#30675,#30682,#25791,.T.) ;
#36908 = EDGE_CURVE('',#30681,#30677,#25792,.T.) ;
#36909 = EDGE_CURVE('',#30595,#30681,#25793,.T.) ;
#36910 = EDGE_CURVE('',#30470,#30600,#25794,.T.) ;
#36911 = EDGE_CURVE('',#30816,#30459,#25795,.T.) ;
#36912 = EDGE_CURVE('',#30675,#30679,#25796,.T.) ;
#36913 = EDGE_CURVE('',#30596,#30677,#25797,.T.) ;
#36914 = EDGE_CURVE('',#30471,#30599,#25798,.T.) ;
#36915 = EDGE_CURVE('',#30676,#30678,#25799,.T.) ;
#36916 = EDGE_CURVE('',#30597,#30676,#25800,.T.) ;
#36917 = EDGE_CURVE('',#30456,#30599,#145,.T.) ;
#36918 = EDGE_CURVE('',#30598,#30678,#25801,.T.) ;
#36919 = EDGE_CURVE('',#30475,#30756,#146,.T.) ;
#36920 = EDGE_CURVE('',#30759,#30755,#25802,.T.) ;
#36921 = EDGE_CURVE('',#30754,#30760,#25803,.T.) ;
#36922 = EDGE_CURVE('',#30757,#30640,#147,.T.) ;
#36923 = EDGE_CURVE('',#30752,#30777,#25804,.T.) ;
#36924 = EDGE_CURVE('',#30764,#30791,#25805,.T.) ;
#36925 = EDGE_CURVE('',#30765,#30790,#25806,.T.) ;
#36926 = EDGE_CURVE('',#30751,#30478,#148,.T.) ;
#36927 = EDGE_CURVE('',#30746,#30758,#25807,.T.) ;
#36928 = EDGE_CURVE('',#30776,#30753,#25808,.T.) ;
#36929 = EDGE_CURVE('',#30765,#30769,#25809,.T.) ;
#36930 = EDGE_CURVE('',#30769,#30790,#25810,.T.) ;
#36931 = EDGE_CURVE('',#30761,#30747,#25811,.T.) ;
#36932 = EDGE_CURVE('',#30792,#30771,#25812,.T.) ;
#36933 = EDGE_CURVE('',#30793,#30770,#25813,.T.) ;
#36934 = EDGE_CURVE('',#30766,#30793,#25814,.T.) ;
#36935 = EDGE_CURVE('',#30762,#30768,#25815,.T.) ;
#36936 = EDGE_CURVE('',#30788,#30763,#25816,.T.) ;
#36937 = EDGE_CURVE('',#30789,#30762,#25817,.T.) ;
#36938 = EDGE_CURVE('',#30766,#30770,#25818,.T.) ;
#36939 = EDGE_CURVE('',#30789,#30768,#25819,.T.) ;
#36940 = EDGE_CURVE('',#30767,#30773,#25820,.T.) ;
#36941 = EDGE_CURVE('',#30786,#30767,#25821,.T.) ;
#36942 = EDGE_CURVE('',#30786,#30773,#25822,.T.) ;
#36943 = EDGE_CURVE('',#30772,#30787,#25823,.T.) ;
#36944 = EDGE_CURVE('',#30748,#30775,#25824,.T.) ;
#36945 = EDGE_CURVE('',#30749,#30774,#25825,.T.) ;
#36946 = EDGE_CURVE('',#30643,#30750,#149,.T.) ;
#36947 = EDGE_CURVE('',#30741,#30742,#25826,.T.) ;
#36948 = EDGE_CURVE('',#30745,#30740,#25827,.T.) ;
#36949 = EDGE_CURVE('',#30728,#30779,#25828,.T.) ;
#36950 = EDGE_CURVE('',#30729,#30778,#25829,.T.) ;
#36951 = EDGE_CURVE('',#30780,#30735,#25830,.T.) ;
#36952 = EDGE_CURVE('',#30781,#30734,#25831,.T.) ;
#36953 = EDGE_CURVE('',#30778,#30733,#25832,.T.) ;
#36954 = EDGE_CURVE('',#30730,#30781,#25833,.T.) ;
#36955 = EDGE_CURVE('',#30729,#30733,#25834,.T.) ;
#36956 = EDGE_CURVE('',#30743,#30738,#25835,.T.) ;
#36957 = EDGE_CURVE('',#30739,#30744,#25836,.T.) ;
#36958 = EDGE_CURVE('',#30730,#30734,#25837,.T.) ;
#36959 = EDGE_CURVE('',#30726,#30732,#25838,.T.) ;
#36960 = EDGE_CURVE('',#30784,#30727,#25839,.T.) ;
#36961 = EDGE_CURVE('',#30785,#30726,#25840,.T.) ;
#36962 = EDGE_CURVE('',#30736,#30783,#25841,.T.) ;
#36963 = EDGE_CURVE('',#30737,#30782,#25842,.T.) ;
#36964 = EDGE_CURVE('',#30731,#30737,#25843,.T.) ;
#36965 = EDGE_CURVE('',#30785,#30732,#25844,.T.) ;
#36966 = EDGE_CURVE('',#30731,#30782,#25845,.T.) ;
#36967 = EDGE_CURVE('',#30489,#30488,#25846,.T.) ;
#36968 = EDGE_CURVE('',#30715,#30490,#150,.T.) ;
#36969 = EDGE_CURVE('',#30716,#30489,#25847,.T.) ;
#36970 = EDGE_CURVE('',#30716,#30488,#25848,.T.) ;
#36971 = EDGE_CURVE('',#30487,#30484,#25849,.T.) ;
#36972 = EDGE_CURVE('',#30713,#30487,#25850,.T.) ;
#36973 = EDGE_CURVE('',#30713,#30484,#25851,.T.) ;
#36974 = EDGE_CURVE('',#30483,#30714,#151,.T.) ;
#36975 = EDGE_CURVE('',#30445,#30724,#4892,.T.) ;
#36976 = EDGE_CURVE('',#30572,#30723,#25852,.T.) ;
#36977 = EDGE_CURVE('',#30569,#30572,#25853,.T.) ;
#36978 = EDGE_CURVE('',#30569,#30723,#25854,.T.) ;
#36979 = EDGE_CURVE('',#30570,#30725,#25855,.T.) ;
#36980 = EDGE_CURVE('',#30568,#30570,#25856,.T.) ;
#36981 = EDGE_CURVE('',#30568,#30725,#25857,.T.) ;
#36982 = EDGE_CURVE('',#30449,#30565,#4893,.T.) ;
#36983 = EDGE_CURVE('',#30637,#30474,#25858,.T.) ;
#36984 = EDGE_CURVE('',#30473,#30638,#25859,.T.) ;
#36985 = EDGE_CURVE('',#30799,#30507,#25860,.T.) ;
#36986 = EDGE_CURVE('',#30796,#30508,#25861,.T.) ;
#36987 = EDGE_CURVE('',#30507,#30797,#25862,.T.) ;
#36988 = EDGE_CURVE('',#30508,#30794,#25863,.T.) ;
#36989 = EDGE_CURVE('',#30631,#30641,#25864,.T.) ;
#36990 = EDGE_CURVE('',#30632,#30474,#25865,.T.) ;
#36991 = EDGE_CURVE('',#30632,#30637,#25866,.T.) ;
#36992 = EDGE_CURVE('',#30633,#30636,#25867,.T.) ;
#36993 = EDGE_CURVE('',#30628,#30635,#25868,.T.) ;
#36994 = EDGE_CURVE('',#30629,#30638,#25869,.T.) ;
#36995 = EDGE_CURVE('',#30629,#30473,#25870,.T.) ;
#36996 = EDGE_CURVE('',#30630,#30642,#25871,.T.) ;
#36997 = EDGE_CURVE('',#30482,#30718,#152,.T.) ;
#36998 = EDGE_CURVE('',#30714,#30717,#25872,.T.) ;
#36999 = EDGE_CURVE('',#30715,#30722,#25873,.T.) ;
#37000 = EDGE_CURVE('',#30817,#30721,#153,.T.) ;
#37001 = EDGE_CURVE('',#30818,#30817,#154,.T.) ;
#37002 = EDGE_CURVE('',#30819,#30818,#155,.T.) ;
#37003 = EDGE_CURVE('',#30491,#30819,#156,.T.) ;
#37004 = EDGE_CURVE('',#30573,#30492,#4894,.T.) ;
#37005 = EDGE_CURVE('',#30574,#30721,#25874,.T.) ;
#37006 = EDGE_CURVE('',#30448,#30566,#157,.T.) ;
#37007 = EDGE_CURVE('',#30575,#30720,#25875,.T.) ;
#37008 = EDGE_CURVE('',#30571,#30576,#4895,.T.) ;
#37009 = EDGE_CURVE('',#30719,#30724,#25876,.T.) ;
#37010 = EDGE_CURVE('',#30820,#30720,#158,.T.) ;
#37011 = EDGE_CURVE('',#30821,#30820,#159,.T.) ;
#37012 = EDGE_CURVE('',#30444,#30821,#160,.T.) ;
#37013 = EDGE_CURVE('',#30501,#30795,#25877,.T.) ;
#37014 = EDGE_CURVE('',#30467,#30795,#25878,.T.) ;
#37015 = EDGE_CURVE('',#30796,#30794,#25879,.T.) ;
#37016 = EDGE_CURVE('',#30764,#30760,#25880,.T.) ;
#37017 = EDGE_CURVE('',#30791,#30754,#25881,.T.) ;
#37018 = EDGE_CURVE('',#30761,#30763,#25882,.T.) ;
#37019 = EDGE_CURVE('',#30792,#30753,#25883,.T.) ;
#37020 = EDGE_CURVE('',#30747,#30788,#25884,.T.) ;
#37021 = EDGE_CURVE('',#30771,#30776,#25885,.T.) ;
#37022 = EDGE_CURVE('',#30748,#30787,#25886,.T.) ;
#37023 = EDGE_CURVE('',#30772,#30775,#25887,.T.) ;
#37024 = EDGE_CURVE('',#30728,#30742,#25888,.T.) ;
#37025 = EDGE_CURVE('',#30779,#30741,#25889,.T.) ;
#37026 = EDGE_CURVE('',#30743,#30727,#25890,.T.) ;
#37027 = EDGE_CURVE('',#30780,#30740,#25891,.T.) ;
#37028 = EDGE_CURVE('',#30738,#30784,#25892,.T.) ;
#37029 = EDGE_CURVE('',#30735,#30745,#25893,.T.) ;
#37030 = EDGE_CURVE('',#30739,#30783,#25894,.T.) ;
#37031 = EDGE_CURVE('',#30736,#30744,#25895,.T.) ;
#37032 = EDGE_CURVE('',#30798,#30496,#25896,.T.) ;
#37033 = EDGE_CURVE('',#30798,#30468,#25897,.T.) ;
#37034 = EDGE_CURVE('',#30799,#30797,#25898,.T.) ;
#37035 = EDGE_CURVE('',#30563,#30567,#4896,.T.) ;
#37036 = EDGE_CURVE('',#30564,#30447,#25899,.T.) ;
#37037 = EDGE_CURVE('',#30561,#30718,#25900,.T.) ;
#37038 = EDGE_CURVE('',#30562,#30481,#4897,.T.) ;
#37039 = EDGE_CURVE('',#30822,#30823,#161,.T.) ;
#37040 = EDGE_CURVE('',#30823,#30824,#4898,.T.) ;
#37041 = EDGE_CURVE('',#30824,#30825,#25901,.T.) ;
#37042 = EDGE_CURVE('',#30826,#30825,#4899,.T.) ;
#37043 = EDGE_CURVE('',#30822,#30826,#162,.T.) ;
#37044 = EDGE_CURVE('',#30827,#30828,#163,.T.) ;
#37045 = EDGE_CURVE('',#30828,#30829,#25902,.T.) ;
#37046 = EDGE_CURVE('',#30830,#30829,#4900,.T.) ;
#37047 = EDGE_CURVE('',#30831,#30830,#25903,.T.) ;
#37048 = EDGE_CURVE('',#30827,#30831,#4901,.T.) ;
#37049 = EDGE_CURVE('',#30832,#30832,#25904,.T.) ;
#37050 = EDGE_CURVE('',#30832,#30833,#25905,.T.) ;
#37051 = EDGE_CURVE('',#30833,#30833,#25906,.T.) ;
#37052 = EDGE_CURVE('',#30834,#30834,#25907,.T.) ;
#37053 = EDGE_CURVE('',#30834,#30835,#25908,.T.) ;
#37054 = EDGE_CURVE('',#30835,#30835,#25909,.T.) ;
#37055 = EDGE_CURVE('',#30836,#30837,#25910,.T.) ;
#37056 = EDGE_CURVE('',#30838,#30836,#8917,.T.) ;
#37057 = EDGE_CURVE('',#30838,#30839,#25911,.T.) ;
#37058 = EDGE_CURVE('',#30839,#30840,#25912,.T.) ;
#37059 = EDGE_CURVE('',#30837,#30840,#8918,.T.) ;
#37060 = EDGE_CURVE('',#30841,#30842,#25913,.T.) ;
#37061 = EDGE_CURVE('',#30843,#30841,#8919,.T.) ;
#37062 = EDGE_CURVE('',#30843,#30844,#25914,.T.) ;
#37063 = EDGE_CURVE('',#30842,#30844,#8920,.T.) ;
#37064 = EDGE_CURVE('',#30845,#30846,#25915,.T.) ;
#37065 = EDGE_CURVE('',#30845,#30847,#25916,.T.) ;
#37066 = EDGE_CURVE('',#30848,#30847,#25917,.T.) ;
#37067 = EDGE_CURVE('',#30848,#30846,#25918,.T.) ;
#37068 = EDGE_CURVE('',#30833,#30834,#8921,.T.) ;
#37069 = EDGE_CURVE('',#30846,#30849,#8922,.T.) ;
#37070 = EDGE_CURVE('',#30849,#30843,#25919,.T.) ;
#37071 = EDGE_CURVE('',#30850,#30841,#164,.T.) ;
#37072 = EDGE_CURVE('',#30850,#30851,#25920,.T.) ;
#37073 = EDGE_CURVE('',#30837,#30851,#165,.T.) ;
#37074 = EDGE_CURVE('',#30840,#30852,#25921,.T.) ;
#37075 = EDGE_CURVE('',#30852,#30845,#8923,.T.) ;
#37076 = EDGE_CURVE('',#30853,#30854,#8924,.T.) ;
#37077 = EDGE_CURVE('',#30854,#30855,#8925,.T.) ;
#37078 = EDGE_CURVE('',#30855,#30856,#166,.T.) ;
#37079 = EDGE_CURVE('',#30856,#30857,#8926,.T.) ;
#37080 = EDGE_CURVE('',#30857,#30858,#4902,.T.) ;
#37081 = EDGE_CURVE('',#30858,#30853,#8927,.T.) ;
#37082 = EDGE_CURVE('',#30859,#30860,#8928,.T.) ;
#37083 = EDGE_CURVE('',#30860,#30861,#8929,.T.) ;
#37084 = EDGE_CURVE('',#30861,#30862,#167,.T.) ;
#37085 = EDGE_CURVE('',#30862,#30863,#168,.T.) ;
#37086 = EDGE_CURVE('',#30863,#30864,#8930,.T.) ;
#37087 = EDGE_CURVE('',#30864,#30859,#8931,.T.) ;
#37088 = EDGE_CURVE('',#30865,#30866,#8932,.T.) ;
#37089 = EDGE_CURVE('',#30866,#30867,#8933,.T.) ;
#37090 = EDGE_CURVE('',#30867,#30868,#8934,.T.) ;
#37091 = EDGE_CURVE('',#30868,#30865,#8935,.T.) ;
#37092 = EDGE_CURVE('',#30869,#30870,#8936,.T.) ;
#37093 = EDGE_CURVE('',#30870,#30871,#169,.T.) ;
#37094 = EDGE_CURVE('',#30871,#30872,#170,.T.) ;
#37095 = EDGE_CURVE('',#30872,#30873,#8937,.T.) ;
#37096 = EDGE_CURVE('',#30873,#30874,#8938,.T.) ;
#37097 = EDGE_CURVE('',#30874,#30869,#8939,.T.) ;
#37098 = EDGE_CURVE('',#30875,#30876,#8940,.T.) ;
#37099 = EDGE_CURVE('',#30876,#30877,#8941,.T.) ;
#37100 = EDGE_CURVE('',#30877,#30878,#8942,.T.) ;
#37101 = EDGE_CURVE('',#30878,#30875,#8943,.T.) ;
#37102 = EDGE_CURVE('',#30879,#30880,#8944,.T.) ;
#37103 = EDGE_CURVE('',#30879,#30881,#8945,.T.) ;
#37104 = EDGE_CURVE('',#30881,#30882,#8946,.T.) ;
#37105 = EDGE_CURVE('',#30882,#30880,#8947,.T.) ;
#37106 = EDGE_CURVE('',#30883,#30884,#8948,.T.) ;
#37107 = EDGE_CURVE('',#30883,#30885,#8949,.T.) ;
#37108 = EDGE_CURVE('',#30885,#30886,#8950,.T.) ;
#37109 = EDGE_CURVE('',#30886,#30887,#8951,.T.) ;
#37110 = EDGE_CURVE('',#30887,#30888,#25922,.T.) ;
#37111 = EDGE_CURVE('',#30888,#30884,#8952,.T.) ;
#37112 = EDGE_CURVE('',#30889,#30890,#8953,.T.) ;
#37113 = EDGE_CURVE('',#30889,#30860,#25923,.T.) ;
#37114 = EDGE_CURVE('',#30859,#30866,#25924,.T.) ;
#37115 = EDGE_CURVE('',#30865,#30874,#25925,.T.) ;
#37116 = EDGE_CURVE('',#30873,#30891,#25926,.T.) ;
#37117 = EDGE_CURVE('',#30892,#30891,#8954,.T.) ;
#37118 = EDGE_CURVE('',#30892,#30893,#25927,.T.) ;
#37119 = EDGE_CURVE('',#30894,#30893,#8955,.T.) ;
#37120 = EDGE_CURVE('',#30894,#30895,#25928,.T.) ;
#37121 = EDGE_CURVE('',#30895,#30896,#8956,.T.) ;
#37122 = EDGE_CURVE('',#30896,#30897,#25929,.T.) ;
#37123 = EDGE_CURVE('',#30898,#30897,#8957,.T.) ;
#37124 = EDGE_CURVE('',#30898,#30899,#25930,.T.) ;
#37125 = EDGE_CURVE('',#30899,#30900,#8958,.T.) ;
#37126 = EDGE_CURVE('',#30900,#30901,#25931,.T.) ;
#37127 = EDGE_CURVE('',#30902,#30901,#8959,.T.) ;
#37128 = EDGE_CURVE('',#30902,#30878,#25932,.T.) ;
#37129 = EDGE_CURVE('',#30877,#30903,#25933,.T.) ;
#37130 = EDGE_CURVE('',#30903,#30904,#8960,.T.) ;
#37131 = EDGE_CURVE('',#30904,#30886,#25934,.T.) ;
#37132 = EDGE_CURVE('',#30885,#30905,#25935,.T.) ;
#37133 = EDGE_CURVE('',#30906,#30905,#8961,.T.) ;
#37134 = EDGE_CURVE('',#30907,#30906,#8962,.T.) ;
#37135 = EDGE_CURVE('',#30907,#30908,#25936,.T.) ;
#37136 = EDGE_CURVE('',#30909,#30908,#8963,.T.) ;
#37137 = EDGE_CURVE('',#30909,#30910,#25937,.T.) ;
#37138 = EDGE_CURVE('',#30911,#30910,#8964,.T.) ;
#37139 = EDGE_CURVE('',#30911,#30890,#25938,.T.) ;
#37140 = EDGE_CURVE('',#30912,#30913,#8965,.T.) ;
#37141 = EDGE_CURVE('',#30913,#30914,#25939,.T.) ;
#37142 = EDGE_CURVE('',#30914,#30915,#8966,.T.) ;
#37143 = EDGE_CURVE('',#30915,#30916,#25940,.T.) ;
#37144 = EDGE_CURVE('',#30916,#30917,#8967,.T.) ;
#37145 = EDGE_CURVE('',#30917,#30918,#25941,.T.) ;
#37146 = EDGE_CURVE('',#30918,#30919,#8968,.T.) ;
#37147 = EDGE_CURVE('',#30919,#30920,#25942,.T.) ;
#37148 = EDGE_CURVE('',#30920,#30921,#8969,.T.) ;
#37149 = EDGE_CURVE('',#30921,#30922,#8970,.T.) ;
#37150 = EDGE_CURVE('',#30922,#30883,#25943,.T.) ;
#37151 = EDGE_CURVE('',#30884,#30923,#25944,.T.) ;
#37152 = EDGE_CURVE('',#30923,#30924,#8971,.T.) ;
#37153 = EDGE_CURVE('',#30924,#30879,#25945,.T.) ;
#37154 = EDGE_CURVE('',#30880,#30925,#25946,.T.) ;
#37155 = EDGE_CURVE('',#30926,#30925,#8972,.T.) ;
#37156 = EDGE_CURVE('',#30926,#30927,#25947,.T.) ;
#37157 = EDGE_CURVE('',#30928,#30927,#8973,.T.) ;
#37158 = EDGE_CURVE('',#30928,#30929,#25948,.T.) ;
#37159 = EDGE_CURVE('',#30929,#30930,#8974,.T.) ;
#37160 = EDGE_CURVE('',#30930,#30931,#25949,.T.) ;
#37161 = EDGE_CURVE('',#30932,#30931,#8975,.T.) ;
#37162 = EDGE_CURVE('',#30932,#30933,#25950,.T.) ;
#37163 = EDGE_CURVE('',#30934,#30933,#8976,.T.) ;
#37164 = EDGE_CURVE('',#30934,#30935,#25951,.T.) ;
#37165 = EDGE_CURVE('',#30935,#30936,#8977,.T.) ;
#37166 = EDGE_CURVE('',#30936,#30937,#25952,.T.) ;
#37167 = EDGE_CURVE('',#30937,#30938,#8978,.T.) ;
#37168 = EDGE_CURVE('',#30938,#30939,#25953,.T.) ;
#37169 = EDGE_CURVE('',#30939,#30940,#8979,.T.) ;
#37170 = EDGE_CURVE('',#30940,#30912,#25954,.T.) ;
#37171 = EDGE_CURVE('',#30908,#30919,#8980,.T.) ;
#37172 = EDGE_CURVE('',#30918,#30909,#8981,.T.) ;
#37173 = EDGE_CURVE('',#30910,#30917,#8982,.T.) ;
#37174 = EDGE_CURVE('',#30916,#30911,#8983,.T.) ;
#37175 = EDGE_CURVE('',#30941,#30942,#171,.T.) ;
#37176 = EDGE_CURVE('',#30942,#30889,#8984,.T.) ;
#37177 = EDGE_CURVE('',#30890,#30915,#8985,.T.) ;
#37178 = EDGE_CURVE('',#30914,#30943,#8986,.T.) ;
#37179 = EDGE_CURVE('',#30943,#30944,#172,.T.) ;
#37180 = EDGE_CURVE('',#30944,#30941,#8987,.T.) ;
#37181 = EDGE_CURVE('',#30945,#30946,#173,.T.) ;
#37182 = EDGE_CURVE('',#30946,#30947,#4903,.T.) ;
#37183 = EDGE_CURVE('',#30947,#30913,#8988,.T.) ;
#37184 = EDGE_CURVE('',#30912,#30948,#8989,.T.) ;
#37185 = EDGE_CURVE('',#30948,#30945,#8990,.T.) ;
#37186 = EDGE_CURVE('',#30949,#30950,#8991,.T.) ;
#37187 = EDGE_CURVE('',#30950,#30940,#8992,.T.) ;
#37188 = EDGE_CURVE('',#30939,#30949,#8993,.T.) ;
#37189 = EDGE_CURVE('',#30951,#30822,#174,.T.) ;
#37190 = EDGE_CURVE('',#30826,#30952,#8994,.T.) ;
#37191 = EDGE_CURVE('',#30952,#30938,#8995,.T.) ;
#37192 = EDGE_CURVE('',#30937,#30951,#8996,.T.) ;
#37193 = EDGE_CURVE('',#30891,#30953,#8997,.T.) ;
#37194 = EDGE_CURVE('',#30953,#30954,#175,.T.) ;
#37195 = EDGE_CURVE('',#30954,#30955,#8998,.T.) ;
#37196 = EDGE_CURVE('',#30955,#30956,#176,.T.) ;
#37197 = EDGE_CURVE('',#30956,#30936,#8999,.T.) ;
#37198 = EDGE_CURVE('',#30935,#30957,#9000,.T.) ;
#37199 = EDGE_CURVE('',#30957,#30958,#9001,.T.) ;
#37200 = EDGE_CURVE('',#30959,#30958,#25955,.T.) ;
#37201 = EDGE_CURVE('',#30959,#30960,#9002,.T.) ;
#37202 = EDGE_CURVE('',#30961,#30960,#25956,.T.) ;
#37203 = EDGE_CURVE('',#30961,#30962,#9003,.T.) ;
#37204 = EDGE_CURVE('',#30962,#30892,#9004,.T.) ;
#37205 = EDGE_CURVE('',#30963,#30964,#25957,.T.) ;
#37206 = EDGE_CURVE('',#30963,#30898,#9005,.T.) ;
#37207 = EDGE_CURVE('',#30897,#30965,#9006,.T.) ;
#37208 = EDGE_CURVE('',#30966,#30965,#25958,.T.) ;
#37209 = EDGE_CURVE('',#30966,#30967,#25959,.T.) ;
#37210 = EDGE_CURVE('',#30968,#30967,#25960,.T.) ;
#37211 = EDGE_CURVE('',#30968,#30969,#9007,.T.) ;
#37212 = EDGE_CURVE('',#30969,#30970,#9008,.T.) ;
#37213 = EDGE_CURVE('',#30970,#30971,#9009,.T.) ;
#37214 = EDGE_CURVE('',#30972,#30971,#25961,.T.) ;
#37215 = EDGE_CURVE('',#30972,#30973,#25962,.T.) ;
#37216 = EDGE_CURVE('',#30974,#30973,#25963,.T.) ;
#37217 = EDGE_CURVE('',#30974,#30930,#9010,.T.) ;
#37218 = EDGE_CURVE('',#30929,#30975,#9011,.T.) ;
#37219 = EDGE_CURVE('',#30976,#30975,#25964,.T.) ;
#37220 = EDGE_CURVE('',#30976,#30977,#25965,.T.) ;
#37221 = EDGE_CURVE('',#30978,#30977,#25966,.T.) ;
#37222 = EDGE_CURVE('',#30978,#30979,#9012,.T.) ;
#37223 = EDGE_CURVE('',#30979,#30980,#25967,.T.) ;
#37224 = EDGE_CURVE('',#30980,#30981,#9013,.T.) ;
#37225 = EDGE_CURVE('',#30982,#30981,#25968,.T.) ;
#37226 = EDGE_CURVE('',#30982,#30964,#25969,.T.) ;
#37227 = EDGE_CURVE('',#30983,#30984,#25970,.T.) ;
#37228 = EDGE_CURVE('',#30983,#30985,#9014,.T.) ;
#37229 = EDGE_CURVE('',#30906,#30985,#9015,.T.) ;
#37230 = EDGE_CURVE('',#30905,#30922,#9016,.T.) ;
#37231 = EDGE_CURVE('',#30986,#30921,#9017,.T.) ;
#37232 = EDGE_CURVE('',#30986,#30987,#9018,.T.) ;
#37233 = EDGE_CURVE('',#30988,#30987,#25971,.T.) ;
#37234 = EDGE_CURVE('',#30988,#30984,#9019,.T.) ;
#37235 = EDGE_CURVE('',#30989,#30990,#25972,.T.) ;
#37236 = EDGE_CURVE('',#30989,#30986,#9020,.T.) ;
#37237 = EDGE_CURVE('',#30920,#30907,#9021,.T.) ;
#37238 = EDGE_CURVE('',#30985,#30991,#9022,.T.) ;
#37239 = EDGE_CURVE('',#30992,#30991,#25973,.T.) ;
#37240 = EDGE_CURVE('',#30992,#30990,#9023,.T.) ;
#37241 = EDGE_CURVE('',#30993,#30994,#9024,.T.) ;
#37242 = EDGE_CURVE('',#30994,#30995,#9025,.T.) ;
#37243 = EDGE_CURVE('',#30993,#30995,#25974,.T.) ;
#37244 = EDGE_CURVE('',#30996,#30997,#25975,.T.) ;
#37245 = EDGE_CURVE('',#30996,#30998,#9026,.T.) ;
#37246 = EDGE_CURVE('',#30998,#30997,#9027,.T.) ;
#37247 = EDGE_CURVE('',#30999,#31000,#9028,.T.) ;
#37248 = EDGE_CURVE('',#31000,#31001,#9029,.T.) ;
#37249 = EDGE_CURVE('',#31001,#31002,#9030,.T.) ;
#37250 = EDGE_CURVE('',#31002,#31003,#9031,.T.) ;
#37251 = EDGE_CURVE('',#31003,#31004,#9032,.T.) ;
#37252 = EDGE_CURVE('',#31004,#31005,#9033,.T.) ;
#37253 = EDGE_CURVE('',#31005,#31006,#9034,.T.) ;
#37254 = EDGE_CURVE('',#31006,#30999,#9035,.T.) ;
#37255 = EDGE_CURVE('',#31007,#31008,#9036,.T.) ;
#37256 = EDGE_CURVE('',#31008,#31009,#9037,.T.) ;
#37257 = EDGE_CURVE('',#31009,#31010,#9038,.T.) ;
#37258 = EDGE_CURVE('',#31010,#31007,#9039,.T.) ;
#37259 = EDGE_CURVE('',#31011,#31012,#9040,.T.) ;
#37260 = EDGE_CURVE('',#31012,#31013,#9041,.T.) ;
#37261 = EDGE_CURVE('',#31013,#31014,#9042,.T.) ;
#37262 = EDGE_CURVE('',#31014,#31011,#9043,.T.) ;
#37263 = EDGE_CURVE('',#31015,#31016,#9044,.T.) ;
#37264 = EDGE_CURVE('',#31016,#31017,#9045,.T.) ;
#37265 = EDGE_CURVE('',#31017,#31018,#9046,.T.) ;
#37266 = EDGE_CURVE('',#31018,#31015,#9047,.T.) ;
#37267 = EDGE_CURVE('',#31019,#31020,#177,.T.) ;
#37268 = EDGE_CURVE('',#31020,#31021,#9048,.T.) ;
#37269 = EDGE_CURVE('',#31021,#31022,#9049,.T.) ;
#37270 = EDGE_CURVE('',#31022,#31023,#9050,.T.) ;
#37271 = EDGE_CURVE('',#31023,#31024,#178,.T.) ;
#37272 = EDGE_CURVE('',#31024,#31019,#9051,.T.) ;
#37273 = EDGE_CURVE('',#31025,#31026,#9052,.T.) ;
#37274 = EDGE_CURVE('',#31026,#31027,#9053,.T.) ;
#37275 = EDGE_CURVE('',#31027,#31028,#9054,.T.) ;
#37276 = EDGE_CURVE('',#31028,#31029,#9055,.T.) ;
#37277 = EDGE_CURVE('',#31029,#31030,#9056,.T.) ;
#37278 = EDGE_CURVE('',#31030,#31031,#9057,.T.) ;
#37279 = EDGE_CURVE('',#31031,#31032,#9058,.T.) ;
#37280 = EDGE_CURVE('',#31032,#31025,#9059,.T.) ;
#37281 = EDGE_CURVE('',#31033,#31034,#9060,.T.) ;
#37282 = EDGE_CURVE('',#31033,#31035,#25976,.T.) ;
#37283 = EDGE_CURVE('',#31035,#31036,#9061,.T.) ;
#37284 = EDGE_CURVE('',#31036,#31037,#25977,.T.) ;
#37285 = EDGE_CURVE('',#31037,#31038,#9062,.T.) ;
#37286 = EDGE_CURVE('',#31038,#31039,#25978,.T.) ;
#37287 = EDGE_CURVE('',#31039,#31040,#9063,.T.) ;
#37288 = EDGE_CURVE('',#31040,#31034,#25979,.T.) ;
#37289 = EDGE_CURVE('',#31041,#31042,#25980,.T.) ;
#37290 = EDGE_CURVE('',#31041,#30902,#9064,.T.) ;
#37291 = EDGE_CURVE('',#30901,#31043,#9065,.T.) ;
#37292 = EDGE_CURVE('',#31043,#31044,#25981,.T.) ;
#37293 = EDGE_CURVE('',#31044,#31045,#9066,.T.) ;
#37294 = EDGE_CURVE('',#31045,#31042,#25982,.T.) ;
#37295 = EDGE_CURVE('',#30899,#31046,#9067,.T.) ;
#37296 = EDGE_CURVE('',#31046,#31047,#9068,.T.) ;
#37297 = EDGE_CURVE('',#31047,#30900,#9069,.T.) ;
#37298 = EDGE_CURVE('',#31048,#31049,#9070,.T.) ;
#37299 = EDGE_CURVE('',#31049,#30842,#9071,.T.) ;
#37300 = EDGE_CURVE('',#30844,#31048,#9072,.T.) ;
#37301 = EDGE_CURVE('',#31050,#31051,#25983,.T.) ;
#37302 = EDGE_CURVE('',#31051,#31052,#9073,.T.) ;
#37303 = EDGE_CURVE('',#31052,#31053,#25984,.T.) ;
#37304 = EDGE_CURVE('',#31053,#31050,#9074,.T.) ;
#37305 = EDGE_CURVE('',#31054,#31055,#25985,.T.) ;
#37306 = EDGE_CURVE('',#31055,#31056,#9075,.T.) ;
#37307 = EDGE_CURVE('',#31056,#31057,#25986,.T.) ;
#37308 = EDGE_CURVE('',#31057,#31054,#9076,.T.) ;
#37309 = EDGE_CURVE('',#30836,#31058,#9077,.T.) ;
#37310 = EDGE_CURVE('',#31058,#31059,#9078,.T.) ;
#37311 = EDGE_CURVE('',#31059,#30838,#9079,.T.) ;
#37312 = EDGE_CURVE('',#31060,#31061,#9080,.T.) ;
#37313 = EDGE_CURVE('',#31061,#30928,#9081,.T.) ;
#37314 = EDGE_CURVE('',#30927,#31060,#9082,.T.) ;
#37315 = EDGE_CURVE('',#31062,#31063,#25987,.T.) ;
#37316 = EDGE_CURVE('',#31063,#30926,#9083,.T.) ;
#37317 = EDGE_CURVE('',#30925,#31064,#9084,.T.) ;
#37318 = EDGE_CURVE('',#31065,#31064,#25988,.T.) ;
#37319 = EDGE_CURVE('',#31065,#31066,#25989,.T.) ;
#37320 = EDGE_CURVE('',#31066,#31062,#9085,.T.) ;
#37321 = EDGE_CURVE('',#31067,#31068,#25990,.T.) ;
#37322 = EDGE_CURVE('',#31068,#30894,#9086,.T.) ;
#37323 = EDGE_CURVE('',#30893,#31069,#9087,.T.) ;
#37324 = EDGE_CURVE('',#31069,#31067,#9088,.T.) ;
#37325 = EDGE_CURVE('',#31070,#31071,#9089,.T.) ;
#37326 = EDGE_CURVE('',#31071,#30896,#9090,.T.) ;
#37327 = EDGE_CURVE('',#30895,#31070,#9091,.T.) ;
#37328 = EDGE_CURVE('',#31072,#31073,#25991,.T.) ;
#37329 = EDGE_CURVE('',#31073,#31074,#9092,.T.) ;
#37330 = EDGE_CURVE('',#31074,#31075,#25992,.T.) ;
#37331 = EDGE_CURVE('',#31075,#31072,#9093,.T.) ;
#37332 = EDGE_CURVE('',#31076,#31077,#9094,.T.) ;
#37333 = EDGE_CURVE('',#31077,#31078,#9095,.T.) ;
#37334 = EDGE_CURVE('',#31078,#31079,#9096,.T.) ;
#37335 = EDGE_CURVE('',#31079,#31076,#9097,.T.) ;
#37336 = EDGE_CURVE('',#31080,#31081,#25993,.T.) ;
#37337 = EDGE_CURVE('',#31081,#31082,#9098,.T.) ;
#37338 = EDGE_CURVE('',#31082,#31083,#25994,.T.) ;
#37339 = EDGE_CURVE('',#31083,#31080,#9099,.T.) ;
#37340 = EDGE_CURVE('',#30931,#31084,#9100,.T.) ;
#37341 = EDGE_CURVE('',#31084,#31085,#9101,.T.) ;
#37342 = EDGE_CURVE('',#31085,#30932,#9102,.T.) ;
#37343 = EDGE_CURVE('',#31086,#31087,#9103,.T.) ;
#37344 = EDGE_CURVE('',#31087,#31088,#9104,.T.) ;
#37345 = EDGE_CURVE('',#31088,#31089,#9105,.T.) ;
#37346 = EDGE_CURVE('',#31089,#31086,#9106,.T.) ;
#37347 = EDGE_CURVE('',#31090,#31091,#9107,.T.) ;
#37348 = EDGE_CURVE('',#31091,#30934,#9108,.T.) ;
#37349 = EDGE_CURVE('',#30933,#31092,#9109,.T.) ;
#37350 = EDGE_CURVE('',#31092,#31090,#25995,.T.) ;
#37351 = EDGE_CURVE('',#31093,#31094,#9110,.T.) ;
#37352 = EDGE_CURVE('',#31094,#31095,#9111,.T.) ;
#37353 = EDGE_CURVE('',#31095,#31096,#9112,.T.) ;
#37354 = EDGE_CURVE('',#31096,#31093,#9113,.T.) ;
#37355 = EDGE_CURVE('',#31097,#31098,#4904,.T.) ;
#37356 = EDGE_CURVE('',#31098,#30827,#9114,.T.) ;
#37357 = EDGE_CURVE('',#30831,#31099,#9115,.T.) ;
#37358 = EDGE_CURVE('',#31099,#31100,#4905,.T.) ;
#37359 = EDGE_CURVE('',#31100,#31101,#9116,.T.) ;
#37360 = EDGE_CURVE('',#31101,#31102,#4906,.T.) ;
#37361 = EDGE_CURVE('',#31102,#31097,#9117,.T.) ;
#37362 = EDGE_CURVE('',#31103,#31104,#9118,.T.) ;
#37363 = EDGE_CURVE('',#31104,#30830,#9119,.T.) ;
#37364 = EDGE_CURVE('',#30830,#31105,#9120,.T.) ;
#37365 = EDGE_CURVE('',#31105,#31103,#9121,.T.) ;
#37366 = EDGE_CURVE('',#31106,#31107,#9122,.T.) ;
#37367 = EDGE_CURVE('',#31107,#31108,#9123,.T.) ;
#37368 = EDGE_CURVE('',#31108,#31109,#9124,.T.) ;
#37369 = EDGE_CURVE('',#31109,#31106,#9125,.T.) ;
#37370 = EDGE_CURVE('',#31110,#31111,#9126,.T.) ;
#37371 = EDGE_CURVE('',#31111,#31112,#9127,.T.) ;
#37372 = EDGE_CURVE('',#31112,#31113,#9128,.T.) ;
#37373 = EDGE_CURVE('',#31113,#31110,#9129,.T.) ;
#37374 = EDGE_CURVE('',#31114,#31115,#9130,.T.) ;
#37375 = EDGE_CURVE('',#31115,#31116,#9131,.T.) ;
#37376 = EDGE_CURVE('',#31116,#31117,#9132,.T.) ;
#37377 = EDGE_CURVE('',#31117,#31114,#9133,.T.) ;
#37378 = EDGE_CURVE('',#31034,#31118,#9134,.T.) ;
#37379 = EDGE_CURVE('',#31118,#31119,#9135,.T.) ;
#37380 = EDGE_CURVE('',#31119,#31033,#9136,.T.) ;
#37381 = EDGE_CURVE('',#31037,#31120,#9137,.T.) ;
#37382 = EDGE_CURVE('',#31120,#31121,#9138,.T.) ;
#37383 = EDGE_CURVE('',#31121,#31038,#9139,.T.) ;
#37384 = EDGE_CURVE('',#31039,#31122,#9140,.T.) ;
#37385 = EDGE_CURVE('',#31122,#31123,#9141,.T.) ;
#37386 = EDGE_CURVE('',#31123,#31040,#9142,.T.) ;
#37387 = EDGE_CURVE('',#31035,#31124,#9143,.T.) ;
#37388 = EDGE_CURVE('',#31124,#31125,#9144,.T.) ;
#37389 = EDGE_CURVE('',#31125,#31036,#9145,.T.) ;
#37390 = EDGE_CURVE('',#31126,#31127,#9146,.T.) ;
#37391 = EDGE_CURVE('',#31127,#31128,#9147,.T.) ;
#37392 = EDGE_CURVE('',#31128,#31129,#9148,.T.) ;
#37393 = EDGE_CURVE('',#31129,#31130,#25996,.T.) ;
#37394 = EDGE_CURVE('',#31130,#31131,#9149,.T.) ;
#37395 = EDGE_CURVE('',#31131,#31126,#25997,.T.) ;
#37396 = EDGE_CURVE('',#31132,#31133,#9150,.T.) ;
#37397 = EDGE_CURVE('',#31133,#31134,#9151,.T.) ;
#37398 = EDGE_CURVE('',#31134,#31135,#9152,.T.) ;
#37399 = EDGE_CURVE('',#31135,#31136,#25998,.T.) ;
#37400 = EDGE_CURVE('',#31136,#31137,#9153,.T.) ;
#37401 = EDGE_CURVE('',#31137,#31132,#25999,.T.) ;
#37402 = EDGE_CURVE('',#31138,#31139,#9154,.T.) ;
#37403 = EDGE_CURVE('',#31138,#30857,#26000,.T.) ;
#37404 = EDGE_CURVE('',#30856,#31139,#26001,.T.) ;
#37405 = EDGE_CURVE('',#31139,#31140,#9155,.T.) ;
#37406 = EDGE_CURVE('',#31140,#31141,#9156,.T.) ;
#37407 = EDGE_CURVE('',#31141,#31138,#9157,.T.) ;
#37408 = EDGE_CURVE('',#31142,#31143,#9158,.T.) ;
#37409 = EDGE_CURVE('',#31143,#31144,#9159,.T.) ;
#37410 = EDGE_CURVE('',#31144,#31145,#9160,.T.) ;
#37411 = EDGE_CURVE('',#31145,#31142,#9161,.T.) ;
#37412 = EDGE_CURVE('',#31146,#31147,#9162,.T.) ;
#37413 = EDGE_CURVE('',#31147,#31148,#9163,.T.) ;
#37414 = EDGE_CURVE('',#31148,#31149,#9164,.T.) ;
#37415 = EDGE_CURVE('',#31149,#31146,#9165,.T.) ;
#37416 = EDGE_CURVE('',#31150,#31151,#9166,.T.) ;
#37417 = EDGE_CURVE('',#31151,#31152,#9167,.T.) ;
#37418 = EDGE_CURVE('',#31152,#31153,#9168,.T.) ;
#37419 = EDGE_CURVE('',#31153,#31150,#9169,.T.) ;
#37420 = EDGE_CURVE('',#31154,#31155,#9170,.T.) ;
#37421 = EDGE_CURVE('',#31155,#31156,#9171,.T.) ;
#37422 = EDGE_CURVE('',#31156,#31157,#9172,.T.) ;
#37423 = EDGE_CURVE('',#31154,#31157,#9173,.T.) ;
#37424 = EDGE_CURVE('',#31024,#31154,#26002,.T.) ;
#37425 = EDGE_CURVE('',#31157,#31019,#26003,.T.) ;
#37426 = EDGE_CURVE('',#31158,#31159,#9174,.T.) ;
#37427 = EDGE_CURVE('',#31159,#31160,#9175,.T.) ;
#37428 = EDGE_CURVE('',#31160,#31161,#9176,.T.) ;
#37429 = EDGE_CURVE('',#31161,#31158,#9177,.T.) ;
#37430 = EDGE_CURVE('',#31162,#31163,#9178,.T.) ;
#37431 = EDGE_CURVE('',#31163,#31164,#9179,.T.) ;
#37432 = EDGE_CURVE('',#31164,#31165,#9180,.T.) ;
#37433 = EDGE_CURVE('',#31165,#31162,#9181,.T.) ;
#37434 = EDGE_CURVE('',#31166,#31167,#9182,.T.) ;
#37435 = EDGE_CURVE('',#31167,#31168,#9183,.T.) ;
#37436 = EDGE_CURVE('',#31168,#31169,#9184,.T.) ;
#37437 = EDGE_CURVE('',#31169,#31166,#9185,.T.) ;
#37438 = EDGE_CURVE('',#31170,#31171,#9186,.T.) ;
#37439 = EDGE_CURVE('',#31171,#31172,#9187,.T.) ;
#37440 = EDGE_CURVE('',#31172,#31173,#9188,.T.) ;
#37441 = EDGE_CURVE('',#31173,#31170,#9189,.T.) ;
#37442 = EDGE_CURVE('',#30923,#31174,#9190,.T.) ;
#37443 = EDGE_CURVE('',#31174,#31175,#26004,.T.) ;
#37444 = EDGE_CURVE('',#31175,#30924,#9191,.T.) ;
#37445 = EDGE_CURVE('',#31176,#31177,#26005,.T.) ;
#37446 = EDGE_CURVE('',#31177,#30848,#26006,.T.) ;
#37447 = EDGE_CURVE('',#30847,#31176,#26007,.T.) ;
#37448 = EDGE_CURVE('',#30903,#31178,#9192,.T.) ;
#37449 = EDGE_CURVE('',#31178,#31179,#26008,.T.) ;
#37450 = EDGE_CURVE('',#31179,#30904,#9193,.T.) ;
#37451 = EDGE_CURVE('',#31092,#31085,#26009,.T.) ;
#37452 = EDGE_CURVE('',#31092,#31081,#26010,.T.) ;
#37453 = EDGE_CURVE('',#31081,#31085,#26011,.T.) ;
#37454 = EDGE_CURVE('',#31084,#30974,#26012,.T.) ;
#37455 = EDGE_CURVE('',#31082,#31084,#26013,.T.) ;
#37456 = EDGE_CURVE('',#31090,#31080,#26014,.T.) ;
#37457 = EDGE_CURVE('',#31082,#30973,#26015,.T.) ;
#37458 = EDGE_CURVE('',#31090,#31089,#26016,.T.) ;
#37459 = EDGE_CURVE('',#31089,#31080,#26017,.T.) ;
#37460 = EDGE_CURVE('',#31070,#31068,#26018,.T.) ;
#37461 = EDGE_CURVE('',#31071,#31075,#26019,.T.) ;
#37462 = EDGE_CURVE('',#31072,#31070,#26020,.T.) ;
#37463 = EDGE_CURVE('',#30965,#31071,#26021,.T.) ;
#37464 = EDGE_CURVE('',#31083,#30972,#26022,.T.) ;
#37465 = EDGE_CURVE('',#31086,#31083,#26023,.T.) ;
#37466 = EDGE_CURVE('',#31091,#31088,#26024,.T.) ;
#37467 = EDGE_CURVE('',#30957,#31091,#26025,.T.) ;
#37468 = EDGE_CURVE('',#31072,#31068,#26026,.T.) ;
#37469 = EDGE_CURVE('',#30966,#31075,#26027,.T.) ;
#37470 = EDGE_CURVE('',#31086,#30971,#26028,.T.) ;
#37471 = EDGE_CURVE('',#30957,#31088,#26029,.T.) ;
#37472 = EDGE_CURVE('',#31073,#31067,#26030,.T.) ;
#37473 = EDGE_CURVE('',#31074,#31079,#26031,.T.) ;
#37474 = EDGE_CURVE('',#31076,#31073,#26032,.T.) ;
#37475 = EDGE_CURVE('',#30967,#31074,#26033,.T.) ;
#37476 = EDGE_CURVE('',#31087,#30970,#26034,.T.) ;
#37477 = EDGE_CURVE('',#30958,#31087,#26035,.T.) ;
#37478 = EDGE_CURVE('',#31076,#31067,#26036,.T.) ;
#37479 = EDGE_CURVE('',#30968,#31079,#26037,.T.) ;
#37480 = EDGE_CURVE('',#30959,#30970,#26038,.T.) ;
#37481 = EDGE_CURVE('',#31069,#30962,#26039,.T.) ;
#37482 = EDGE_CURVE('',#31077,#31069,#26040,.T.) ;
#37483 = EDGE_CURVE('',#30969,#31078,#26041,.T.) ;
#37484 = EDGE_CURVE('',#30960,#30969,#26042,.T.) ;
#37485 = EDGE_CURVE('',#31077,#30962,#26043,.T.) ;
#37486 = EDGE_CURVE('',#30961,#31078,#26044,.T.) ;
#37487 = EDGE_CURVE('',#31025,#31006,#26045,.T.) ;
#37488 = EDGE_CURVE('',#31014,#31025,#26046,.T.) ;
#37489 = EDGE_CURVE('',#31006,#31014,#26047,.T.) ;
#37490 = EDGE_CURVE('',#31032,#31180,#179,.T.) ;
#37491 = EDGE_CURVE('',#31180,#31011,#4907,.T.) ;
#37492 = EDGE_CURVE('',#31013,#31181,#4908,.T.) ;
#37493 = EDGE_CURVE('',#31181,#30999,#180,.T.) ;
#37494 = EDGE_CURVE('',#31026,#31005,#26048,.T.) ;
#37495 = EDGE_CURVE('',#31021,#31182,#4909,.T.) ;
#37496 = EDGE_CURVE('',#31182,#31032,#181,.T.) ;
#37497 = EDGE_CURVE('',#31031,#31183,#182,.T.) ;
#37498 = EDGE_CURVE('',#31183,#31022,#4910,.T.) ;
#37499 = EDGE_CURVE('',#30999,#31184,#183,.T.) ;
#37500 = EDGE_CURVE('',#31184,#31016,#4911,.T.) ;
#37501 = EDGE_CURVE('',#31015,#31185,#4912,.T.) ;
#37502 = EDGE_CURVE('',#31185,#31000,#184,.T.) ;
#37503 = EDGE_CURVE('',#31026,#30997,#26049,.T.) ;
#37504 = EDGE_CURVE('',#30996,#31005,#26050,.T.) ;
#37505 = EDGE_CURVE('',#31186,#30997,#9194,.T.) ;
#37506 = EDGE_CURVE('',#31027,#31186,#26051,.T.) ;
#37507 = EDGE_CURVE('',#31187,#31186,#26052,.T.) ;
#37508 = EDGE_CURVE('',#31027,#31187,#26053,.T.) ;
#37509 = EDGE_CURVE('',#31010,#31188,#4913,.T.) ;
#37510 = EDGE_CURVE('',#31188,#31031,#185,.T.) ;
#37511 = EDGE_CURVE('',#31007,#31030,#26054,.T.) ;
#37512 = EDGE_CURVE('',#31000,#31189,#186,.T.) ;
#37513 = EDGE_CURVE('',#31189,#31008,#4914,.T.) ;
#37514 = EDGE_CURVE('',#31001,#31007,#26055,.T.) ;
#37515 = EDGE_CURVE('',#31190,#31004,#26056,.T.) ;
#37516 = EDGE_CURVE('',#30996,#31190,#9195,.T.) ;
#37517 = EDGE_CURVE('',#30985,#30998,#4915,.T.) ;
#37518 = EDGE_CURVE('',#31186,#30983,#26057,.T.) ;
#37519 = EDGE_CURVE('',#31187,#30984,#26058,.T.) ;
#37520 = EDGE_CURVE('',#31191,#31187,#9196,.T.) ;
#37521 = EDGE_CURVE('',#31028,#31191,#26059,.T.) ;
#37522 = EDGE_CURVE('',#31001,#31030,#26060,.T.) ;
#37523 = EDGE_CURVE('',#31190,#31192,#26061,.T.) ;
#37524 = EDGE_CURVE('',#31192,#31004,#26062,.T.) ;
#37525 = EDGE_CURVE('',#30991,#31190,#26063,.T.) ;
#37526 = EDGE_CURVE('',#31191,#30988,#26064,.T.) ;
#37527 = EDGE_CURVE('',#31193,#31191,#26065,.T.) ;
#37528 = EDGE_CURVE('',#31028,#31193,#26066,.T.) ;
#37529 = EDGE_CURVE('',#31002,#31029,#26067,.T.) ;
#37530 = EDGE_CURVE('',#31194,#31003,#26068,.T.) ;
#37531 = EDGE_CURVE('',#31192,#31194,#9197,.T.) ;
#37532 = EDGE_CURVE('',#30992,#31192,#26069,.T.) ;
#37533 = EDGE_CURVE('',#31193,#30987,#26070,.T.) ;
#37534 = EDGE_CURVE('',#30993,#31193,#9198,.T.) ;
#37535 = EDGE_CURVE('',#31029,#30993,#26071,.T.) ;
#37536 = EDGE_CURVE('',#31002,#30995,#26072,.T.) ;
#37537 = EDGE_CURVE('',#31194,#31195,#26073,.T.) ;
#37538 = EDGE_CURVE('',#31195,#31003,#26074,.T.) ;
#37539 = EDGE_CURVE('',#30990,#31194,#26075,.T.) ;
#37540 = EDGE_CURVE('',#30994,#30986,#4916,.T.) ;
#37541 = EDGE_CURVE('',#31195,#30995,#9199,.T.) ;
#37542 = EDGE_CURVE('',#30989,#31195,#26076,.T.) ;
#37543 = EDGE_CURVE('',#31043,#31047,#26077,.T.) ;
#37544 = EDGE_CURVE('',#31043,#31051,#26078,.T.) ;
#37545 = EDGE_CURVE('',#31051,#31047,#26079,.T.) ;
#37546 = EDGE_CURVE('',#31046,#30963,#26080,.T.) ;
#37547 = EDGE_CURVE('',#31052,#31046,#26081,.T.) ;
#37548 = EDGE_CURVE('',#31044,#31050,#26082,.T.) ;
#37549 = EDGE_CURVE('',#30875,#31041,#26083,.T.) ;
#37550 = EDGE_CURVE('',#30846,#30876,#26084,.T.) ;
#37551 = EDGE_CURVE('',#30849,#30875,#26085,.T.) ;
#37552 = EDGE_CURVE('',#31052,#30964,#26086,.T.) ;
#37553 = EDGE_CURVE('',#31044,#31048,#26087,.T.) ;
#37554 = EDGE_CURVE('',#31048,#31050,#26088,.T.) ;
#37555 = EDGE_CURVE('',#30849,#31042,#26089,.T.) ;
#37556 = EDGE_CURVE('',#31053,#30982,#26090,.T.) ;
#37557 = EDGE_CURVE('',#31049,#31053,#26091,.T.) ;
#37558 = EDGE_CURVE('',#31045,#30844,#26092,.T.) ;
#37559 = EDGE_CURVE('',#30843,#31045,#26093,.T.) ;
#37560 = EDGE_CURVE('',#30881,#30845,#26094,.T.) ;
#37561 = EDGE_CURVE('',#30882,#30852,#26095,.T.) ;
#37562 = EDGE_CURVE('',#31064,#30882,#26096,.T.) ;
#37563 = EDGE_CURVE('',#31060,#31063,#26097,.T.) ;
#37564 = EDGE_CURVE('',#31049,#30981,#26098,.T.) ;
#37565 = EDGE_CURVE('',#31065,#30852,#26099,.T.) ;
#37566 = EDGE_CURVE('',#31060,#31054,#26100,.T.) ;
#37567 = EDGE_CURVE('',#31054,#31063,#26101,.T.) ;
#37568 = EDGE_CURVE('',#30842,#30980,#187,.T.) ;
#37569 = EDGE_CURVE('',#31066,#30840,#26102,.T.) ;
#37570 = EDGE_CURVE('',#31062,#31059,#26103,.T.) ;
#37571 = EDGE_CURVE('',#30838,#31066,#26104,.T.) ;
#37572 = EDGE_CURVE('',#31055,#31062,#26105,.T.) ;
#37573 = EDGE_CURVE('',#31061,#31057,#26106,.T.) ;
#37574 = EDGE_CURVE('',#30975,#31061,#26107,.T.) ;
#37575 = EDGE_CURVE('',#30850,#30980,#26108,.T.) ;
#37576 = EDGE_CURVE('',#31196,#30839,#26109,.T.) ;
#37577 = EDGE_CURVE('',#31055,#31059,#26110,.T.) ;
#37578 = EDGE_CURVE('',#30976,#31057,#26111,.T.) ;
#37579 = EDGE_CURVE('',#30851,#30979,#26112,.T.) ;
#37580 = EDGE_CURVE('',#31056,#31058,#26113,.T.) ;
#37581 = EDGE_CURVE('',#30977,#31056,#26114,.T.) ;
#37582 = EDGE_CURVE('',#30836,#30979,#188,.T.) ;
#37583 = EDGE_CURVE('',#30978,#31058,#26115,.T.) ;
#37584 = EDGE_CURVE('',#30855,#31136,#189,.T.) ;
#37585 = EDGE_CURVE('',#31139,#31135,#26116,.T.) ;
#37586 = EDGE_CURVE('',#31134,#31140,#26117,.T.) ;
#37587 = EDGE_CURVE('',#31137,#31020,#190,.T.) ;
#37588 = EDGE_CURVE('',#31132,#31157,#26118,.T.) ;
#37589 = EDGE_CURVE('',#31144,#31171,#26119,.T.) ;
#37590 = EDGE_CURVE('',#31145,#31170,#26120,.T.) ;
#37591 = EDGE_CURVE('',#31131,#30858,#191,.T.) ;
#37592 = EDGE_CURVE('',#31126,#31138,#26121,.T.) ;
#37593 = EDGE_CURVE('',#31156,#31133,#26122,.T.) ;
#37594 = EDGE_CURVE('',#31145,#31149,#26123,.T.) ;
#37595 = EDGE_CURVE('',#31149,#31170,#26124,.T.) ;
#37596 = EDGE_CURVE('',#31141,#31127,#26125,.T.) ;
#37597 = EDGE_CURVE('',#31172,#31151,#26126,.T.) ;
#37598 = EDGE_CURVE('',#31173,#31150,#26127,.T.) ;
#37599 = EDGE_CURVE('',#31146,#31173,#26128,.T.) ;
#37600 = EDGE_CURVE('',#31142,#31148,#26129,.T.) ;
#37601 = EDGE_CURVE('',#31168,#31143,#26130,.T.) ;
#37602 = EDGE_CURVE('',#31169,#31142,#26131,.T.) ;
#37603 = EDGE_CURVE('',#31146,#31150,#26132,.T.) ;
#37604 = EDGE_CURVE('',#31169,#31148,#26133,.T.) ;
#37605 = EDGE_CURVE('',#31147,#31153,#26134,.T.) ;
#37606 = EDGE_CURVE('',#31166,#31147,#26135,.T.) ;
#37607 = EDGE_CURVE('',#31166,#31153,#26136,.T.) ;
#37608 = EDGE_CURVE('',#31152,#31167,#26137,.T.) ;
#37609 = EDGE_CURVE('',#31128,#31155,#26138,.T.) ;
#37610 = EDGE_CURVE('',#31129,#31154,#26139,.T.) ;
#37611 = EDGE_CURVE('',#31023,#31130,#192,.T.) ;
#37612 = EDGE_CURVE('',#31121,#31122,#26140,.T.) ;
#37613 = EDGE_CURVE('',#31125,#31120,#26141,.T.) ;
#37614 = EDGE_CURVE('',#31108,#31159,#26142,.T.) ;
#37615 = EDGE_CURVE('',#31109,#31158,#26143,.T.) ;
#37616 = EDGE_CURVE('',#31160,#31115,#26144,.T.) ;
#37617 = EDGE_CURVE('',#31161,#31114,#26145,.T.) ;
#37618 = EDGE_CURVE('',#31158,#31113,#26146,.T.) ;
#37619 = EDGE_CURVE('',#31110,#31161,#26147,.T.) ;
#37620 = EDGE_CURVE('',#31109,#31113,#26148,.T.) ;
#37621 = EDGE_CURVE('',#31123,#31118,#26149,.T.) ;
#37622 = EDGE_CURVE('',#31119,#31124,#26150,.T.) ;
#37623 = EDGE_CURVE('',#31110,#31114,#26151,.T.) ;
#37624 = EDGE_CURVE('',#31106,#31112,#26152,.T.) ;
#37625 = EDGE_CURVE('',#31164,#31107,#26153,.T.) ;
#37626 = EDGE_CURVE('',#31165,#31106,#26154,.T.) ;
#37627 = EDGE_CURVE('',#31116,#31163,#26155,.T.) ;
#37628 = EDGE_CURVE('',#31117,#31162,#26156,.T.) ;
#37629 = EDGE_CURVE('',#31111,#31117,#26157,.T.) ;
#37630 = EDGE_CURVE('',#31165,#31112,#26158,.T.) ;
#37631 = EDGE_CURVE('',#31111,#31162,#26159,.T.) ;
#37632 = EDGE_CURVE('',#30869,#30868,#26160,.T.) ;
#37633 = EDGE_CURVE('',#31095,#30870,#193,.T.) ;
#37634 = EDGE_CURVE('',#31096,#30869,#26161,.T.) ;
#37635 = EDGE_CURVE('',#31096,#30868,#26162,.T.) ;
#37636 = EDGE_CURVE('',#30867,#30864,#26163,.T.) ;
#37637 = EDGE_CURVE('',#31093,#30867,#26164,.T.) ;
#37638 = EDGE_CURVE('',#31093,#30864,#26165,.T.) ;
#37639 = EDGE_CURVE('',#30863,#31094,#194,.T.) ;
#37640 = EDGE_CURVE('',#30825,#31104,#4917,.T.) ;
#37641 = EDGE_CURVE('',#30952,#31103,#26166,.T.) ;
#37642 = EDGE_CURVE('',#30949,#30952,#26167,.T.) ;
#37643 = EDGE_CURVE('',#30949,#31103,#26168,.T.) ;
#37644 = EDGE_CURVE('',#30950,#31105,#26169,.T.) ;
#37645 = EDGE_CURVE('',#30948,#30950,#26170,.T.) ;
#37646 = EDGE_CURVE('',#30948,#31105,#26171,.T.) ;
#37647 = EDGE_CURVE('',#30829,#30945,#4918,.T.) ;
#37648 = EDGE_CURVE('',#31017,#30854,#26172,.T.) ;
#37649 = EDGE_CURVE('',#30853,#31018,#26173,.T.) ;
#37650 = EDGE_CURVE('',#31179,#30887,#26174,.T.) ;
#37651 = EDGE_CURVE('',#31176,#30888,#26175,.T.) ;
#37652 = EDGE_CURVE('',#30887,#31177,#26176,.T.) ;
#37653 = EDGE_CURVE('',#30888,#31174,#26177,.T.) ;
#37654 = EDGE_CURVE('',#31011,#31021,#26178,.T.) ;
#37655 = EDGE_CURVE('',#31012,#30854,#26179,.T.) ;
#37656 = EDGE_CURVE('',#31012,#31017,#26180,.T.) ;
#37657 = EDGE_CURVE('',#31013,#31016,#26181,.T.) ;
#37658 = EDGE_CURVE('',#31008,#31015,#26182,.T.) ;
#37659 = EDGE_CURVE('',#31009,#31018,#26183,.T.) ;
#37660 = EDGE_CURVE('',#31009,#30853,#26184,.T.) ;
#37661 = EDGE_CURVE('',#31010,#31022,#26185,.T.) ;
#37662 = EDGE_CURVE('',#30862,#31098,#195,.T.) ;
#37663 = EDGE_CURVE('',#31094,#31097,#26186,.T.) ;
#37664 = EDGE_CURVE('',#31095,#31102,#26187,.T.) ;
#37665 = EDGE_CURVE('',#31197,#31101,#196,.T.) ;
#37666 = EDGE_CURVE('',#31198,#31197,#197,.T.) ;
#37667 = EDGE_CURVE('',#31199,#31198,#198,.T.) ;
#37668 = EDGE_CURVE('',#30871,#31199,#199,.T.) ;
#37669 = EDGE_CURVE('',#30953,#30872,#4919,.T.) ;
#37670 = EDGE_CURVE('',#30954,#31101,#26188,.T.) ;
#37671 = EDGE_CURVE('',#30828,#30946,#200,.T.) ;
#37672 = EDGE_CURVE('',#30955,#31100,#26189,.T.) ;
#37673 = EDGE_CURVE('',#30951,#30956,#4920,.T.) ;
#37674 = EDGE_CURVE('',#31099,#31104,#26190,.T.) ;
#37675 = EDGE_CURVE('',#31200,#31100,#201,.T.) ;
#37676 = EDGE_CURVE('',#31201,#31200,#202,.T.) ;
#37677 = EDGE_CURVE('',#30824,#31201,#203,.T.) ;
#37678 = EDGE_CURVE('',#30881,#31175,#26191,.T.) ;
#37679 = EDGE_CURVE('',#30847,#31175,#26192,.T.) ;
#37680 = EDGE_CURVE('',#31176,#31174,#26193,.T.) ;
#37681 = EDGE_CURVE('',#31144,#31140,#26194,.T.) ;
#37682 = EDGE_CURVE('',#31171,#31134,#26195,.T.) ;
#37683 = EDGE_CURVE('',#31141,#31143,#26196,.T.) ;
#37684 = EDGE_CURVE('',#31172,#31133,#26197,.T.) ;
#37685 = EDGE_CURVE('',#31127,#31168,#26198,.T.) ;
#37686 = EDGE_CURVE('',#31151,#31156,#26199,.T.) ;
#37687 = EDGE_CURVE('',#31128,#31167,#26200,.T.) ;
#37688 = EDGE_CURVE('',#31152,#31155,#26201,.T.) ;
#37689 = EDGE_CURVE('',#31108,#31122,#26202,.T.) ;
#37690 = EDGE_CURVE('',#31159,#31121,#26203,.T.) ;
#37691 = EDGE_CURVE('',#31123,#31107,#26204,.T.) ;
#37692 = EDGE_CURVE('',#31160,#31120,#26205,.T.) ;
#37693 = EDGE_CURVE('',#31118,#31164,#26206,.T.) ;
#37694 = EDGE_CURVE('',#31115,#31125,#26207,.T.) ;
#37695 = EDGE_CURVE('',#31119,#31163,#26208,.T.) ;
#37696 = EDGE_CURVE('',#31116,#31124,#26209,.T.) ;
#37697 = EDGE_CURVE('',#31178,#30876,#26210,.T.) ;
#37698 = EDGE_CURVE('',#31178,#30848,#26211,.T.) ;
#37699 = EDGE_CURVE('',#31179,#31177,#26212,.T.) ;
#37700 = EDGE_CURVE('',#30943,#30947,#4921,.T.) ;
#37701 = EDGE_CURVE('',#30944,#30827,#26213,.T.) ;
#37702 = EDGE_CURVE('',#30941,#31098,#26214,.T.) ;
#37703 = EDGE_CURVE('',#30942,#30861,#4922,.T.) ;
#37704 = EDGE_CURVE('',#31202,#31203,#204,.T.) ;
#37705 = EDGE_CURVE('',#31203,#31204,#4923,.T.) ;
#37706 = EDGE_CURVE('',#31204,#31205,#26215,.T.) ;
#37707 = EDGE_CURVE('',#31206,#31205,#4924,.T.) ;
#37708 = EDGE_CURVE('',#31202,#31206,#205,.T.) ;
#37709 = EDGE_CURVE('',#31207,#31208,#206,.T.) ;
#37710 = EDGE_CURVE('',#31208,#31209,#26216,.T.) ;
#37711 = EDGE_CURVE('',#31210,#31209,#4925,.T.) ;
#37712 = EDGE_CURVE('',#31211,#31210,#26217,.T.) ;
#37713 = EDGE_CURVE('',#31207,#31211,#4926,.T.) ;
#37714 = EDGE_CURVE('',#31212,#31212,#26218,.T.) ;
#37715 = EDGE_CURVE('',#31212,#31213,#26219,.T.) ;
#37716 = EDGE_CURVE('',#31213,#31213,#26220,.T.) ;
#37717 = EDGE_CURVE('',#31214,#31214,#26221,.T.) ;
#37718 = EDGE_CURVE('',#31214,#31215,#26222,.T.) ;
#37719 = EDGE_CURVE('',#31215,#31215,#26223,.T.) ;
#37720 = EDGE_CURVE('',#31216,#31217,#26224,.T.) ;
#37721 = EDGE_CURVE('',#31218,#31216,#9200,.T.) ;
#37722 = EDGE_CURVE('',#31218,#31219,#26225,.T.) ;
#37723 = EDGE_CURVE('',#31219,#31220,#26226,.T.) ;
#37724 = EDGE_CURVE('',#31217,#31220,#9201,.T.) ;
#37725 = EDGE_CURVE('',#31221,#31222,#26227,.T.) ;
#37726 = EDGE_CURVE('',#31223,#31221,#9202,.T.) ;
#37727 = EDGE_CURVE('',#31223,#31224,#26228,.T.) ;
#37728 = EDGE_CURVE('',#31222,#31224,#9203,.T.) ;
#37729 = EDGE_CURVE('',#31225,#31226,#26229,.T.) ;
#37730 = EDGE_CURVE('',#31225,#31227,#26230,.T.) ;
#37731 = EDGE_CURVE('',#31228,#31227,#26231,.T.) ;
#37732 = EDGE_CURVE('',#31228,#31226,#26232,.T.) ;
#37733 = EDGE_CURVE('',#31213,#31214,#9204,.T.) ;
#37734 = EDGE_CURVE('',#31226,#31229,#9205,.T.) ;
#37735 = EDGE_CURVE('',#31229,#31223,#26233,.T.) ;
#37736 = EDGE_CURVE('',#31230,#31221,#207,.T.) ;
#37737 = EDGE_CURVE('',#31230,#31231,#26234,.T.) ;
#37738 = EDGE_CURVE('',#31217,#31231,#208,.T.) ;
#37739 = EDGE_CURVE('',#31220,#31232,#26235,.T.) ;
#37740 = EDGE_CURVE('',#31232,#31225,#9206,.T.) ;
#37741 = EDGE_CURVE('',#31233,#31234,#9207,.T.) ;
#37742 = EDGE_CURVE('',#31234,#31235,#9208,.T.) ;
#37743 = EDGE_CURVE('',#31235,#31236,#209,.T.) ;
#37744 = EDGE_CURVE('',#31236,#31237,#9209,.T.) ;
#37745 = EDGE_CURVE('',#31237,#31238,#4927,.T.) ;
#37746 = EDGE_CURVE('',#31238,#31233,#9210,.T.) ;
#37747 = EDGE_CURVE('',#31239,#31240,#9211,.T.) ;
#37748 = EDGE_CURVE('',#31240,#31241,#9212,.T.) ;
#37749 = EDGE_CURVE('',#31241,#31242,#210,.T.) ;
#37750 = EDGE_CURVE('',#31242,#31243,#211,.T.) ;
#37751 = EDGE_CURVE('',#31243,#31244,#9213,.T.) ;
#37752 = EDGE_CURVE('',#31244,#31239,#9214,.T.) ;
#37753 = EDGE_CURVE('',#31245,#31246,#9215,.T.) ;
#37754 = EDGE_CURVE('',#31246,#31247,#9216,.T.) ;
#37755 = EDGE_CURVE('',#31247,#31248,#9217,.T.) ;
#37756 = EDGE_CURVE('',#31248,#31245,#9218,.T.) ;
#37757 = EDGE_CURVE('',#31249,#31250,#9219,.T.) ;
#37758 = EDGE_CURVE('',#31250,#31251,#212,.T.) ;
#37759 = EDGE_CURVE('',#31251,#31252,#213,.T.) ;
#37760 = EDGE_CURVE('',#31252,#31253,#9220,.T.) ;
#37761 = EDGE_CURVE('',#31253,#31254,#9221,.T.) ;
#37762 = EDGE_CURVE('',#31254,#31249,#9222,.T.) ;
#37763 = EDGE_CURVE('',#31255,#31256,#9223,.T.) ;
#37764 = EDGE_CURVE('',#31256,#31257,#9224,.T.) ;
#37765 = EDGE_CURVE('',#31257,#31258,#9225,.T.) ;
#37766 = EDGE_CURVE('',#31258,#31255,#9226,.T.) ;
#37767 = EDGE_CURVE('',#31259,#31260,#9227,.T.) ;
#37768 = EDGE_CURVE('',#31259,#31261,#9228,.T.) ;
#37769 = EDGE_CURVE('',#31261,#31262,#9229,.T.) ;
#37770 = EDGE_CURVE('',#31262,#31260,#9230,.T.) ;
#37771 = EDGE_CURVE('',#31263,#31264,#9231,.T.) ;
#37772 = EDGE_CURVE('',#31263,#31265,#9232,.T.) ;
#37773 = EDGE_CURVE('',#31265,#31266,#9233,.T.) ;
#37774 = EDGE_CURVE('',#31266,#31267,#9234,.T.) ;
#37775 = EDGE_CURVE('',#31267,#31268,#26236,.T.) ;
#37776 = EDGE_CURVE('',#31268,#31264,#9235,.T.) ;
#37777 = EDGE_CURVE('',#31269,#31270,#9236,.T.) ;
#37778 = EDGE_CURVE('',#31269,#31240,#26237,.T.) ;
#37779 = EDGE_CURVE('',#31239,#31246,#26238,.T.) ;
#37780 = EDGE_CURVE('',#31245,#31254,#26239,.T.) ;
#37781 = EDGE_CURVE('',#31253,#31271,#26240,.T.) ;
#37782 = EDGE_CURVE('',#31272,#31271,#9237,.T.) ;
#37783 = EDGE_CURVE('',#31272,#31273,#26241,.T.) ;
#37784 = EDGE_CURVE('',#31274,#31273,#9238,.T.) ;
#37785 = EDGE_CURVE('',#31274,#31275,#26242,.T.) ;
#37786 = EDGE_CURVE('',#31275,#31276,#9239,.T.) ;
#37787 = EDGE_CURVE('',#31276,#31277,#26243,.T.) ;
#37788 = EDGE_CURVE('',#31278,#31277,#9240,.T.) ;
#37789 = EDGE_CURVE('',#31278,#31279,#26244,.T.) ;
#37790 = EDGE_CURVE('',#31279,#31280,#9241,.T.) ;
#37791 = EDGE_CURVE('',#31280,#31281,#26245,.T.) ;
#37792 = EDGE_CURVE('',#31282,#31281,#9242,.T.) ;
#37793 = EDGE_CURVE('',#31282,#31258,#26246,.T.) ;
#37794 = EDGE_CURVE('',#31257,#31283,#26247,.T.) ;
#37795 = EDGE_CURVE('',#31283,#31284,#9243,.T.) ;
#37796 = EDGE_CURVE('',#31284,#31266,#26248,.T.) ;
#37797 = EDGE_CURVE('',#31265,#31285,#26249,.T.) ;
#37798 = EDGE_CURVE('',#31286,#31285,#9244,.T.) ;
#37799 = EDGE_CURVE('',#31287,#31286,#9245,.T.) ;
#37800 = EDGE_CURVE('',#31287,#31288,#26250,.T.) ;
#37801 = EDGE_CURVE('',#31289,#31288,#9246,.T.) ;
#37802 = EDGE_CURVE('',#31289,#31290,#26251,.T.) ;
#37803 = EDGE_CURVE('',#31291,#31290,#9247,.T.) ;
#37804 = EDGE_CURVE('',#31291,#31270,#26252,.T.) ;
#37805 = EDGE_CURVE('',#31292,#31293,#9248,.T.) ;
#37806 = EDGE_CURVE('',#31293,#31294,#26253,.T.) ;
#37807 = EDGE_CURVE('',#31294,#31295,#9249,.T.) ;
#37808 = EDGE_CURVE('',#31295,#31296,#26254,.T.) ;
#37809 = EDGE_CURVE('',#31296,#31297,#9250,.T.) ;
#37810 = EDGE_CURVE('',#31297,#31298,#26255,.T.) ;
#37811 = EDGE_CURVE('',#31298,#31299,#9251,.T.) ;
#37812 = EDGE_CURVE('',#31299,#31300,#26256,.T.) ;
#37813 = EDGE_CURVE('',#31300,#31301,#9252,.T.) ;
#37814 = EDGE_CURVE('',#31301,#31302,#9253,.T.) ;
#37815 = EDGE_CURVE('',#31302,#31263,#26257,.T.) ;
#37816 = EDGE_CURVE('',#31264,#31303,#26258,.T.) ;
#37817 = EDGE_CURVE('',#31303,#31304,#9254,.T.) ;
#37818 = EDGE_CURVE('',#31304,#31259,#26259,.T.) ;
#37819 = EDGE_CURVE('',#31260,#31305,#26260,.T.) ;
#37820 = EDGE_CURVE('',#31306,#31305,#9255,.T.) ;
#37821 = EDGE_CURVE('',#31306,#31307,#26261,.T.) ;
#37822 = EDGE_CURVE('',#31308,#31307,#9256,.T.) ;
#37823 = EDGE_CURVE('',#31308,#31309,#26262,.T.) ;
#37824 = EDGE_CURVE('',#31309,#31310,#9257,.T.) ;
#37825 = EDGE_CURVE('',#31310,#31311,#26263,.T.) ;
#37826 = EDGE_CURVE('',#31312,#31311,#9258,.T.) ;
#37827 = EDGE_CURVE('',#31312,#31313,#26264,.T.) ;
#37828 = EDGE_CURVE('',#31314,#31313,#9259,.T.) ;
#37829 = EDGE_CURVE('',#31314,#31315,#26265,.T.) ;
#37830 = EDGE_CURVE('',#31315,#31316,#9260,.T.) ;
#37831 = EDGE_CURVE('',#31316,#31317,#26266,.T.) ;
#37832 = EDGE_CURVE('',#31317,#31318,#9261,.T.) ;
#37833 = EDGE_CURVE('',#31318,#31319,#26267,.T.) ;
#37834 = EDGE_CURVE('',#31319,#31320,#9262,.T.) ;
#37835 = EDGE_CURVE('',#31320,#31292,#26268,.T.) ;
#37836 = EDGE_CURVE('',#31288,#31299,#9263,.T.) ;
#37837 = EDGE_CURVE('',#31298,#31289,#9264,.T.) ;
#37838 = EDGE_CURVE('',#31290,#31297,#9265,.T.) ;
#37839 = EDGE_CURVE('',#31296,#31291,#9266,.T.) ;
#37840 = EDGE_CURVE('',#31321,#31322,#214,.T.) ;
#37841 = EDGE_CURVE('',#31322,#31269,#9267,.T.) ;
#37842 = EDGE_CURVE('',#31270,#31295,#9268,.T.) ;
#37843 = EDGE_CURVE('',#31294,#31323,#9269,.T.) ;
#37844 = EDGE_CURVE('',#31323,#31324,#215,.T.) ;
#37845 = EDGE_CURVE('',#31324,#31321,#9270,.T.) ;
#37846 = EDGE_CURVE('',#31325,#31326,#216,.T.) ;
#37847 = EDGE_CURVE('',#31326,#31327,#4928,.T.) ;
#37848 = EDGE_CURVE('',#31327,#31293,#9271,.T.) ;
#37849 = EDGE_CURVE('',#31292,#31328,#9272,.T.) ;
#37850 = EDGE_CURVE('',#31328,#31325,#9273,.T.) ;
#37851 = EDGE_CURVE('',#31329,#31330,#9274,.T.) ;
#37852 = EDGE_CURVE('',#31330,#31320,#9275,.T.) ;
#37853 = EDGE_CURVE('',#31319,#31329,#9276,.T.) ;
#37854 = EDGE_CURVE('',#31331,#31202,#217,.T.) ;
#37855 = EDGE_CURVE('',#31206,#31332,#9277,.T.) ;
#37856 = EDGE_CURVE('',#31332,#31318,#9278,.T.) ;
#37857 = EDGE_CURVE('',#31317,#31331,#9279,.T.) ;
#37858 = EDGE_CURVE('',#31271,#31333,#9280,.T.) ;
#37859 = EDGE_CURVE('',#31333,#31334,#218,.T.) ;
#37860 = EDGE_CURVE('',#31334,#31335,#9281,.T.) ;
#37861 = EDGE_CURVE('',#31335,#31336,#219,.T.) ;
#37862 = EDGE_CURVE('',#31336,#31316,#9282,.T.) ;
#37863 = EDGE_CURVE('',#31315,#31337,#9283,.T.) ;
#37864 = EDGE_CURVE('',#31337,#31338,#9284,.T.) ;
#37865 = EDGE_CURVE('',#31339,#31338,#26269,.T.) ;
#37866 = EDGE_CURVE('',#31339,#31340,#9285,.T.) ;
#37867 = EDGE_CURVE('',#31341,#31340,#26270,.T.) ;
#37868 = EDGE_CURVE('',#31341,#31342,#9286,.T.) ;
#37869 = EDGE_CURVE('',#31342,#31272,#9287,.T.) ;
#37870 = EDGE_CURVE('',#31343,#31344,#26271,.T.) ;
#37871 = EDGE_CURVE('',#31343,#31278,#9288,.T.) ;
#37872 = EDGE_CURVE('',#31277,#31345,#9289,.T.) ;
#37873 = EDGE_CURVE('',#31346,#31345,#26272,.T.) ;
#37874 = EDGE_CURVE('',#31346,#31347,#26273,.T.) ;
#37875 = EDGE_CURVE('',#31348,#31347,#26274,.T.) ;
#37876 = EDGE_CURVE('',#31348,#31349,#9290,.T.) ;
#37877 = EDGE_CURVE('',#31349,#31350,#9291,.T.) ;
#37878 = EDGE_CURVE('',#31350,#31351,#9292,.T.) ;
#37879 = EDGE_CURVE('',#31352,#31351,#26275,.T.) ;
#37880 = EDGE_CURVE('',#31352,#31353,#26276,.T.) ;
#37881 = EDGE_CURVE('',#31354,#31353,#26277,.T.) ;
#37882 = EDGE_CURVE('',#31354,#31310,#9293,.T.) ;
#37883 = EDGE_CURVE('',#31309,#31355,#9294,.T.) ;
#37884 = EDGE_CURVE('',#31356,#31355,#26278,.T.) ;
#37885 = EDGE_CURVE('',#31356,#31357,#26279,.T.) ;
#37886 = EDGE_CURVE('',#31358,#31357,#26280,.T.) ;
#37887 = EDGE_CURVE('',#31358,#31359,#9295,.T.) ;
#37888 = EDGE_CURVE('',#31359,#31360,#26281,.T.) ;
#37889 = EDGE_CURVE('',#31360,#31361,#9296,.T.) ;
#37890 = EDGE_CURVE('',#31362,#31361,#26282,.T.) ;
#37891 = EDGE_CURVE('',#31362,#31344,#26283,.T.) ;
#37892 = EDGE_CURVE('',#31363,#31364,#26284,.T.) ;
#37893 = EDGE_CURVE('',#31363,#31365,#9297,.T.) ;
#37894 = EDGE_CURVE('',#31286,#31365,#9298,.T.) ;
#37895 = EDGE_CURVE('',#31285,#31302,#9299,.T.) ;
#37896 = EDGE_CURVE('',#31366,#31301,#9300,.T.) ;
#37897 = EDGE_CURVE('',#31366,#31367,#9301,.T.) ;
#37898 = EDGE_CURVE('',#31368,#31367,#26285,.T.) ;
#37899 = EDGE_CURVE('',#31368,#31364,#9302,.T.) ;
#37900 = EDGE_CURVE('',#31369,#31370,#26286,.T.) ;
#37901 = EDGE_CURVE('',#31369,#31366,#9303,.T.) ;
#37902 = EDGE_CURVE('',#31300,#31287,#9304,.T.) ;
#37903 = EDGE_CURVE('',#31365,#31371,#9305,.T.) ;
#37904 = EDGE_CURVE('',#31372,#31371,#26287,.T.) ;
#37905 = EDGE_CURVE('',#31372,#31370,#9306,.T.) ;
#37906 = EDGE_CURVE('',#31373,#31374,#9307,.T.) ;
#37907 = EDGE_CURVE('',#31374,#31375,#9308,.T.) ;
#37908 = EDGE_CURVE('',#31373,#31375,#26288,.T.) ;
#37909 = EDGE_CURVE('',#31376,#31377,#26289,.T.) ;
#37910 = EDGE_CURVE('',#31376,#31378,#9309,.T.) ;
#37911 = EDGE_CURVE('',#31378,#31377,#9310,.T.) ;
#37912 = EDGE_CURVE('',#31379,#31380,#9311,.T.) ;
#37913 = EDGE_CURVE('',#31380,#31381,#9312,.T.) ;
#37914 = EDGE_CURVE('',#31381,#31382,#9313,.T.) ;
#37915 = EDGE_CURVE('',#31382,#31383,#9314,.T.) ;
#37916 = EDGE_CURVE('',#31383,#31384,#9315,.T.) ;
#37917 = EDGE_CURVE('',#31384,#31385,#9316,.T.) ;
#37918 = EDGE_CURVE('',#31385,#31386,#9317,.T.) ;
#37919 = EDGE_CURVE('',#31386,#31379,#9318,.T.) ;
#37920 = EDGE_CURVE('',#31387,#31388,#9319,.T.) ;
#37921 = EDGE_CURVE('',#31388,#31389,#9320,.T.) ;
#37922 = EDGE_CURVE('',#31389,#31390,#9321,.T.) ;
#37923 = EDGE_CURVE('',#31390,#31387,#9322,.T.) ;
#37924 = EDGE_CURVE('',#31391,#31392,#9323,.T.) ;
#37925 = EDGE_CURVE('',#31392,#31393,#9324,.T.) ;
#37926 = EDGE_CURVE('',#31393,#31394,#9325,.T.) ;
#37927 = EDGE_CURVE('',#31394,#31391,#9326,.T.) ;
#37928 = EDGE_CURVE('',#31395,#31396,#9327,.T.) ;
#37929 = EDGE_CURVE('',#31396,#31397,#9328,.T.) ;
#37930 = EDGE_CURVE('',#31397,#31398,#9329,.T.) ;
#37931 = EDGE_CURVE('',#31398,#31395,#9330,.T.) ;
#37932 = EDGE_CURVE('',#31399,#31400,#220,.T.) ;
#37933 = EDGE_CURVE('',#31400,#31401,#9331,.T.) ;
#37934 = EDGE_CURVE('',#31401,#31402,#9332,.T.) ;
#37935 = EDGE_CURVE('',#31402,#31403,#9333,.T.) ;
#37936 = EDGE_CURVE('',#31403,#31404,#221,.T.) ;
#37937 = EDGE_CURVE('',#31404,#31399,#9334,.T.) ;
#37938 = EDGE_CURVE('',#31405,#31406,#9335,.T.) ;
#37939 = EDGE_CURVE('',#31406,#31407,#9336,.T.) ;
#37940 = EDGE_CURVE('',#31407,#31408,#9337,.T.) ;
#37941 = EDGE_CURVE('',#31408,#31409,#9338,.T.) ;
#37942 = EDGE_CURVE('',#31409,#31410,#9339,.T.) ;
#37943 = EDGE_CURVE('',#31410,#31411,#9340,.T.) ;
#37944 = EDGE_CURVE('',#31411,#31412,#9341,.T.) ;
#37945 = EDGE_CURVE('',#31412,#31405,#9342,.T.) ;
#37946 = EDGE_CURVE('',#31413,#31414,#9343,.T.) ;
#37947 = EDGE_CURVE('',#31413,#31415,#26290,.T.) ;
#37948 = EDGE_CURVE('',#31415,#31416,#9344,.T.) ;
#37949 = EDGE_CURVE('',#31416,#31417,#26291,.T.) ;
#37950 = EDGE_CURVE('',#31417,#31418,#9345,.T.) ;
#37951 = EDGE_CURVE('',#31418,#31419,#26292,.T.) ;
#37952 = EDGE_CURVE('',#31419,#31420,#9346,.T.) ;
#37953 = EDGE_CURVE('',#31420,#31414,#26293,.T.) ;
#37954 = EDGE_CURVE('',#31421,#31422,#26294,.T.) ;
#37955 = EDGE_CURVE('',#31421,#31282,#9347,.T.) ;
#37956 = EDGE_CURVE('',#31281,#31423,#9348,.T.) ;
#37957 = EDGE_CURVE('',#31423,#31424,#26295,.T.) ;
#37958 = EDGE_CURVE('',#31424,#31425,#9349,.T.) ;
#37959 = EDGE_CURVE('',#31425,#31422,#26296,.T.) ;
#37960 = EDGE_CURVE('',#31279,#31426,#9350,.T.) ;
#37961 = EDGE_CURVE('',#31426,#31427,#9351,.T.) ;
#37962 = EDGE_CURVE('',#31427,#31280,#9352,.T.) ;
#37963 = EDGE_CURVE('',#31428,#31429,#9353,.T.) ;
#37964 = EDGE_CURVE('',#31429,#31222,#9354,.T.) ;
#37965 = EDGE_CURVE('',#31224,#31428,#9355,.T.) ;
#37966 = EDGE_CURVE('',#31430,#31431,#26297,.T.) ;
#37967 = EDGE_CURVE('',#31431,#31432,#9356,.T.) ;
#37968 = EDGE_CURVE('',#31432,#31433,#26298,.T.) ;
#37969 = EDGE_CURVE('',#31433,#31430,#9357,.T.) ;
#37970 = EDGE_CURVE('',#31434,#31435,#26299,.T.) ;
#37971 = EDGE_CURVE('',#31435,#31436,#9358,.T.) ;
#37972 = EDGE_CURVE('',#31436,#31437,#26300,.T.) ;
#37973 = EDGE_CURVE('',#31437,#31434,#9359,.T.) ;
#37974 = EDGE_CURVE('',#31216,#31438,#9360,.T.) ;
#37975 = EDGE_CURVE('',#31438,#31439,#9361,.T.) ;
#37976 = EDGE_CURVE('',#31439,#31218,#9362,.T.) ;
#37977 = EDGE_CURVE('',#31440,#31441,#9363,.T.) ;
#37978 = EDGE_CURVE('',#31441,#31308,#9364,.T.) ;
#37979 = EDGE_CURVE('',#31307,#31440,#9365,.T.) ;
#37980 = EDGE_CURVE('',#31442,#31443,#26301,.T.) ;
#37981 = EDGE_CURVE('',#31443,#31306,#9366,.T.) ;
#37982 = EDGE_CURVE('',#31305,#31444,#9367,.T.) ;
#37983 = EDGE_CURVE('',#31445,#31444,#26302,.T.) ;
#37984 = EDGE_CURVE('',#31445,#31446,#26303,.T.) ;
#37985 = EDGE_CURVE('',#31446,#31442,#9368,.T.) ;
#37986 = EDGE_CURVE('',#31447,#31448,#26304,.T.) ;
#37987 = EDGE_CURVE('',#31448,#31274,#9369,.T.) ;
#37988 = EDGE_CURVE('',#31273,#31449,#9370,.T.) ;
#37989 = EDGE_CURVE('',#31449,#31447,#9371,.T.) ;
#37990 = EDGE_CURVE('',#31450,#31451,#9372,.T.) ;
#37991 = EDGE_CURVE('',#31451,#31276,#9373,.T.) ;
#37992 = EDGE_CURVE('',#31275,#31450,#9374,.T.) ;
#37993 = EDGE_CURVE('',#31452,#31453,#26305,.T.) ;
#37994 = EDGE_CURVE('',#31453,#31454,#9375,.T.) ;
#37995 = EDGE_CURVE('',#31454,#31455,#26306,.T.) ;
#37996 = EDGE_CURVE('',#31455,#31452,#9376,.T.) ;
#37997 = EDGE_CURVE('',#31456,#31457,#9377,.T.) ;
#37998 = EDGE_CURVE('',#31457,#31458,#9378,.T.) ;
#37999 = EDGE_CURVE('',#31458,#31459,#9379,.T.) ;
#38000 = EDGE_CURVE('',#31459,#31456,#9380,.T.) ;
#38001 = EDGE_CURVE('',#31460,#31461,#26307,.T.) ;
#38002 = EDGE_CURVE('',#31461,#31462,#9381,.T.) ;
#38003 = EDGE_CURVE('',#31462,#31463,#26308,.T.) ;
#38004 = EDGE_CURVE('',#31463,#31460,#9382,.T.) ;
#38005 = EDGE_CURVE('',#31311,#31464,#9383,.T.) ;
#38006 = EDGE_CURVE('',#31464,#31465,#9384,.T.) ;
#38007 = EDGE_CURVE('',#31465,#31312,#9385,.T.) ;
#38008 = EDGE_CURVE('',#31466,#31467,#9386,.T.) ;
#38009 = EDGE_CURVE('',#31467,#31468,#9387,.T.) ;
#38010 = EDGE_CURVE('',#31468,#31469,#9388,.T.) ;
#38011 = EDGE_CURVE('',#31469,#31466,#9389,.T.) ;
#38012 = EDGE_CURVE('',#31470,#31471,#9390,.T.) ;
#38013 = EDGE_CURVE('',#31471,#31314,#9391,.T.) ;
#38014 = EDGE_CURVE('',#31313,#31472,#9392,.T.) ;
#38015 = EDGE_CURVE('',#31472,#31470,#26309,.T.) ;
#38016 = EDGE_CURVE('',#31473,#31474,#9393,.T.) ;
#38017 = EDGE_CURVE('',#31474,#31475,#9394,.T.) ;
#38018 = EDGE_CURVE('',#31475,#31476,#9395,.T.) ;
#38019 = EDGE_CURVE('',#31476,#31473,#9396,.T.) ;
#38020 = EDGE_CURVE('',#31477,#31478,#4929,.T.) ;
#38021 = EDGE_CURVE('',#31478,#31207,#9397,.T.) ;
#38022 = EDGE_CURVE('',#31211,#31479,#9398,.T.) ;
#38023 = EDGE_CURVE('',#31479,#31480,#4930,.T.) ;
#38024 = EDGE_CURVE('',#31480,#31481,#9399,.T.) ;
#38025 = EDGE_CURVE('',#31481,#31482,#4931,.T.) ;
#38026 = EDGE_CURVE('',#31482,#31477,#9400,.T.) ;
#38027 = EDGE_CURVE('',#31483,#31484,#9401,.T.) ;
#38028 = EDGE_CURVE('',#31484,#31210,#9402,.T.) ;
#38029 = EDGE_CURVE('',#31210,#31485,#9403,.T.) ;
#38030 = EDGE_CURVE('',#31485,#31483,#9404,.T.) ;
#38031 = EDGE_CURVE('',#31486,#31487,#9405,.T.) ;
#38032 = EDGE_CURVE('',#31487,#31488,#9406,.T.) ;
#38033 = EDGE_CURVE('',#31488,#31489,#9407,.T.) ;
#38034 = EDGE_CURVE('',#31489,#31486,#9408,.T.) ;
#38035 = EDGE_CURVE('',#31490,#31491,#9409,.T.) ;
#38036 = EDGE_CURVE('',#31491,#31492,#9410,.T.) ;
#38037 = EDGE_CURVE('',#31492,#31493,#9411,.T.) ;
#38038 = EDGE_CURVE('',#31493,#31490,#9412,.T.) ;
#38039 = EDGE_CURVE('',#31494,#31495,#9413,.T.) ;
#38040 = EDGE_CURVE('',#31495,#31496,#9414,.T.) ;
#38041 = EDGE_CURVE('',#31496,#31497,#9415,.T.) ;
#38042 = EDGE_CURVE('',#31497,#31494,#9416,.T.) ;
#38043 = EDGE_CURVE('',#31414,#31498,#9417,.T.) ;
#38044 = EDGE_CURVE('',#31498,#31499,#9418,.T.) ;
#38045 = EDGE_CURVE('',#31499,#31413,#9419,.T.) ;
#38046 = EDGE_CURVE('',#31417,#31500,#9420,.T.) ;
#38047 = EDGE_CURVE('',#31500,#31501,#9421,.T.) ;
#38048 = EDGE_CURVE('',#31501,#31418,#9422,.T.) ;
#38049 = EDGE_CURVE('',#31419,#31502,#9423,.T.) ;
#38050 = EDGE_CURVE('',#31502,#31503,#9424,.T.) ;
#38051 = EDGE_CURVE('',#31503,#31420,#9425,.T.) ;
#38052 = EDGE_CURVE('',#31415,#31504,#9426,.T.) ;
#38053 = EDGE_CURVE('',#31504,#31505,#9427,.T.) ;
#38054 = EDGE_CURVE('',#31505,#31416,#9428,.T.) ;
#38055 = EDGE_CURVE('',#31506,#31507,#9429,.T.) ;
#38056 = EDGE_CURVE('',#31507,#31508,#9430,.T.) ;
#38057 = EDGE_CURVE('',#31508,#31509,#9431,.T.) ;
#38058 = EDGE_CURVE('',#31509,#31510,#26310,.T.) ;
#38059 = EDGE_CURVE('',#31510,#31511,#9432,.T.) ;
#38060 = EDGE_CURVE('',#31511,#31506,#26311,.T.) ;
#38061 = EDGE_CURVE('',#31512,#31513,#9433,.T.) ;
#38062 = EDGE_CURVE('',#31513,#31514,#9434,.T.) ;
#38063 = EDGE_CURVE('',#31514,#31515,#9435,.T.) ;
#38064 = EDGE_CURVE('',#31515,#31516,#26312,.T.) ;
#38065 = EDGE_CURVE('',#31516,#31517,#9436,.T.) ;
#38066 = EDGE_CURVE('',#31517,#31512,#26313,.T.) ;
#38067 = EDGE_CURVE('',#31518,#31519,#9437,.T.) ;
#38068 = EDGE_CURVE('',#31518,#31237,#26314,.T.) ;
#38069 = EDGE_CURVE('',#31236,#31519,#26315,.T.) ;
#38070 = EDGE_CURVE('',#31519,#31520,#9438,.T.) ;
#38071 = EDGE_CURVE('',#31520,#31521,#9439,.T.) ;
#38072 = EDGE_CURVE('',#31521,#31518,#9440,.T.) ;
#38073 = EDGE_CURVE('',#31522,#31523,#9441,.T.) ;
#38074 = EDGE_CURVE('',#31523,#31524,#9442,.T.) ;
#38075 = EDGE_CURVE('',#31524,#31525,#9443,.T.) ;
#38076 = EDGE_CURVE('',#31525,#31522,#9444,.T.) ;
#38077 = EDGE_CURVE('',#31526,#31527,#9445,.T.) ;
#38078 = EDGE_CURVE('',#31527,#31528,#9446,.T.) ;
#38079 = EDGE_CURVE('',#31528,#31529,#9447,.T.) ;
#38080 = EDGE_CURVE('',#31529,#31526,#9448,.T.) ;
#38081 = EDGE_CURVE('',#31530,#31531,#9449,.T.) ;
#38082 = EDGE_CURVE('',#31531,#31532,#9450,.T.) ;
#38083 = EDGE_CURVE('',#31532,#31533,#9451,.T.) ;
#38084 = EDGE_CURVE('',#31533,#31530,#9452,.T.) ;
#38085 = EDGE_CURVE('',#31534,#31535,#9453,.T.) ;
#38086 = EDGE_CURVE('',#31535,#31536,#9454,.T.) ;
#38087 = EDGE_CURVE('',#31536,#31537,#9455,.T.) ;
#38088 = EDGE_CURVE('',#31534,#31537,#9456,.T.) ;
#38089 = EDGE_CURVE('',#31404,#31534,#26316,.T.) ;
#38090 = EDGE_CURVE('',#31537,#31399,#26317,.T.) ;
#38091 = EDGE_CURVE('',#31538,#31539,#9457,.T.) ;
#38092 = EDGE_CURVE('',#31539,#31540,#9458,.T.) ;
#38093 = EDGE_CURVE('',#31540,#31541,#9459,.T.) ;
#38094 = EDGE_CURVE('',#31541,#31538,#9460,.T.) ;
#38095 = EDGE_CURVE('',#31542,#31543,#9461,.T.) ;
#38096 = EDGE_CURVE('',#31543,#31544,#9462,.T.) ;
#38097 = EDGE_CURVE('',#31544,#31545,#9463,.T.) ;
#38098 = EDGE_CURVE('',#31545,#31542,#9464,.T.) ;
#38099 = EDGE_CURVE('',#31546,#31547,#9465,.T.) ;
#38100 = EDGE_CURVE('',#31547,#31548,#9466,.T.) ;
#38101 = EDGE_CURVE('',#31548,#31549,#9467,.T.) ;
#38102 = EDGE_CURVE('',#31549,#31546,#9468,.T.) ;
#38103 = EDGE_CURVE('',#31550,#31551,#9469,.T.) ;
#38104 = EDGE_CURVE('',#31551,#31552,#9470,.T.) ;
#38105 = EDGE_CURVE('',#31552,#31553,#9471,.T.) ;
#38106 = EDGE_CURVE('',#31553,#31550,#9472,.T.) ;
#38107 = EDGE_CURVE('',#31303,#31554,#9473,.T.) ;
#38108 = EDGE_CURVE('',#31554,#31555,#26318,.T.) ;
#38109 = EDGE_CURVE('',#31555,#31304,#9474,.T.) ;
#38110 = EDGE_CURVE('',#31556,#31557,#26319,.T.) ;
#38111 = EDGE_CURVE('',#31557,#31228,#26320,.T.) ;
#38112 = EDGE_CURVE('',#31227,#31556,#26321,.T.) ;
#38113 = EDGE_CURVE('',#31283,#31558,#9475,.T.) ;
#38114 = EDGE_CURVE('',#31558,#31559,#26322,.T.) ;
#38115 = EDGE_CURVE('',#31559,#31284,#9476,.T.) ;
#38116 = EDGE_CURVE('',#31472,#31465,#26323,.T.) ;
#38117 = EDGE_CURVE('',#31472,#31461,#26324,.T.) ;
#38118 = EDGE_CURVE('',#31461,#31465,#26325,.T.) ;
#38119 = EDGE_CURVE('',#31464,#31354,#26326,.T.) ;
#38120 = EDGE_CURVE('',#31462,#31464,#26327,.T.) ;
#38121 = EDGE_CURVE('',#31470,#31460,#26328,.T.) ;
#38122 = EDGE_CURVE('',#31462,#31353,#26329,.T.) ;
#38123 = EDGE_CURVE('',#31470,#31469,#26330,.T.) ;
#38124 = EDGE_CURVE('',#31469,#31460,#26331,.T.) ;
#38125 = EDGE_CURVE('',#31450,#31448,#26332,.T.) ;
#38126 = EDGE_CURVE('',#31451,#31455,#26333,.T.) ;
#38127 = EDGE_CURVE('',#31452,#31450,#26334,.T.) ;
#38128 = EDGE_CURVE('',#31345,#31451,#26335,.T.) ;
#38129 = EDGE_CURVE('',#31463,#31352,#26336,.T.) ;
#38130 = EDGE_CURVE('',#31466,#31463,#26337,.T.) ;
#38131 = EDGE_CURVE('',#31471,#31468,#26338,.T.) ;
#38132 = EDGE_CURVE('',#31337,#31471,#26339,.T.) ;
#38133 = EDGE_CURVE('',#31452,#31448,#26340,.T.) ;
#38134 = EDGE_CURVE('',#31346,#31455,#26341,.T.) ;
#38135 = EDGE_CURVE('',#31466,#31351,#26342,.T.) ;
#38136 = EDGE_CURVE('',#31337,#31468,#26343,.T.) ;
#38137 = EDGE_CURVE('',#31453,#31447,#26344,.T.) ;
#38138 = EDGE_CURVE('',#31454,#31459,#26345,.T.) ;
#38139 = EDGE_CURVE('',#31456,#31453,#26346,.T.) ;
#38140 = EDGE_CURVE('',#31347,#31454,#26347,.T.) ;
#38141 = EDGE_CURVE('',#31467,#31350,#26348,.T.) ;
#38142 = EDGE_CURVE('',#31338,#31467,#26349,.T.) ;
#38143 = EDGE_CURVE('',#31456,#31447,#26350,.T.) ;
#38144 = EDGE_CURVE('',#31348,#31459,#26351,.T.) ;
#38145 = EDGE_CURVE('',#31339,#31350,#26352,.T.) ;
#38146 = EDGE_CURVE('',#31449,#31342,#26353,.T.) ;
#38147 = EDGE_CURVE('',#31457,#31449,#26354,.T.) ;
#38148 = EDGE_CURVE('',#31349,#31458,#26355,.T.) ;
#38149 = EDGE_CURVE('',#31340,#31349,#26356,.T.) ;
#38150 = EDGE_CURVE('',#31457,#31342,#26357,.T.) ;
#38151 = EDGE_CURVE('',#31341,#31458,#26358,.T.) ;
#38152 = EDGE_CURVE('',#31405,#31386,#26359,.T.) ;
#38153 = EDGE_CURVE('',#31394,#31405,#26360,.T.) ;
#38154 = EDGE_CURVE('',#31386,#31394,#26361,.T.) ;
#38155 = EDGE_CURVE('',#31412,#31560,#222,.T.) ;
#38156 = EDGE_CURVE('',#31560,#31391,#4932,.T.) ;
#38157 = EDGE_CURVE('',#31393,#31561,#4933,.T.) ;
#38158 = EDGE_CURVE('',#31561,#31379,#223,.T.) ;
#38159 = EDGE_CURVE('',#31406,#31385,#26362,.T.) ;
#38160 = EDGE_CURVE('',#31401,#31562,#4934,.T.) ;
#38161 = EDGE_CURVE('',#31562,#31412,#224,.T.) ;
#38162 = EDGE_CURVE('',#31411,#31563,#225,.T.) ;
#38163 = EDGE_CURVE('',#31563,#31402,#4935,.T.) ;
#38164 = EDGE_CURVE('',#31379,#31564,#226,.T.) ;
#38165 = EDGE_CURVE('',#31564,#31396,#4936,.T.) ;
#38166 = EDGE_CURVE('',#31395,#31565,#4937,.T.) ;
#38167 = EDGE_CURVE('',#31565,#31380,#227,.T.) ;
#38168 = EDGE_CURVE('',#31406,#31377,#26363,.T.) ;
#38169 = EDGE_CURVE('',#31376,#31385,#26364,.T.) ;
#38170 = EDGE_CURVE('',#31566,#31377,#9477,.T.) ;
#38171 = EDGE_CURVE('',#31407,#31566,#26365,.T.) ;
#38172 = EDGE_CURVE('',#31567,#31566,#26366,.T.) ;
#38173 = EDGE_CURVE('',#31407,#31567,#26367,.T.) ;
#38174 = EDGE_CURVE('',#31390,#31568,#4938,.T.) ;
#38175 = EDGE_CURVE('',#31568,#31411,#228,.T.) ;
#38176 = EDGE_CURVE('',#31387,#31410,#26368,.T.) ;
#38177 = EDGE_CURVE('',#31380,#31569,#229,.T.) ;
#38178 = EDGE_CURVE('',#31569,#31388,#4939,.T.) ;
#38179 = EDGE_CURVE('',#31381,#31387,#26369,.T.) ;
#38180 = EDGE_CURVE('',#31570,#31384,#26370,.T.) ;
#38181 = EDGE_CURVE('',#31376,#31570,#9478,.T.) ;
#38182 = EDGE_CURVE('',#31365,#31378,#4940,.T.) ;
#38183 = EDGE_CURVE('',#31566,#31363,#26371,.T.) ;
#38184 = EDGE_CURVE('',#31567,#31364,#26372,.T.) ;
#38185 = EDGE_CURVE('',#31571,#31567,#9479,.T.) ;
#38186 = EDGE_CURVE('',#31408,#31571,#26373,.T.) ;
#38187 = EDGE_CURVE('',#31381,#31410,#26374,.T.) ;
#38188 = EDGE_CURVE('',#31570,#31572,#26375,.T.) ;
#38189 = EDGE_CURVE('',#31572,#31384,#26376,.T.) ;
#38190 = EDGE_CURVE('',#31371,#31570,#26377,.T.) ;
#38191 = EDGE_CURVE('',#31571,#31368,#26378,.T.) ;
#38192 = EDGE_CURVE('',#31573,#31571,#26379,.T.) ;
#38193 = EDGE_CURVE('',#31408,#31573,#26380,.T.) ;
#38194 = EDGE_CURVE('',#31382,#31409,#26381,.T.) ;
#38195 = EDGE_CURVE('',#31574,#31383,#26382,.T.) ;
#38196 = EDGE_CURVE('',#31572,#31574,#9480,.T.) ;
#38197 = EDGE_CURVE('',#31372,#31572,#26383,.T.) ;
#38198 = EDGE_CURVE('',#31573,#31367,#26384,.T.) ;
#38199 = EDGE_CURVE('',#31373,#31573,#9481,.T.) ;
#38200 = EDGE_CURVE('',#31409,#31373,#26385,.T.) ;
#38201 = EDGE_CURVE('',#31382,#31375,#26386,.T.) ;
#38202 = EDGE_CURVE('',#31574,#31575,#26387,.T.) ;
#38203 = EDGE_CURVE('',#31575,#31383,#26388,.T.) ;
#38204 = EDGE_CURVE('',#31370,#31574,#26389,.T.) ;
#38205 = EDGE_CURVE('',#31374,#31366,#4941,.T.) ;
#38206 = EDGE_CURVE('',#31575,#31375,#9482,.T.) ;
#38207 = EDGE_CURVE('',#31369,#31575,#26390,.T.) ;
#38208 = EDGE_CURVE('',#31423,#31427,#26391,.T.) ;
#38209 = EDGE_CURVE('',#31423,#31431,#26392,.T.) ;
#38210 = EDGE_CURVE('',#31431,#31427,#26393,.T.) ;
#38211 = EDGE_CURVE('',#31426,#31343,#26394,.T.) ;
#38212 = EDGE_CURVE('',#31432,#31426,#26395,.T.) ;
#38213 = EDGE_CURVE('',#31424,#31430,#26396,.T.) ;
#38214 = EDGE_CURVE('',#31255,#31421,#26397,.T.) ;
#38215 = EDGE_CURVE('',#31226,#31256,#26398,.T.) ;
#38216 = EDGE_CURVE('',#31229,#31255,#26399,.T.) ;
#38217 = EDGE_CURVE('',#31432,#31344,#26400,.T.) ;
#38218 = EDGE_CURVE('',#31424,#31428,#26401,.T.) ;
#38219 = EDGE_CURVE('',#31428,#31430,#26402,.T.) ;
#38220 = EDGE_CURVE('',#31229,#31422,#26403,.T.) ;
#38221 = EDGE_CURVE('',#31433,#31362,#26404,.T.) ;
#38222 = EDGE_CURVE('',#31429,#31433,#26405,.T.) ;
#38223 = EDGE_CURVE('',#31425,#31224,#26406,.T.) ;
#38224 = EDGE_CURVE('',#31223,#31425,#26407,.T.) ;
#38225 = EDGE_CURVE('',#31261,#31225,#26408,.T.) ;
#38226 = EDGE_CURVE('',#31262,#31232,#26409,.T.) ;
#38227 = EDGE_CURVE('',#31444,#31262,#26410,.T.) ;
#38228 = EDGE_CURVE('',#31440,#31443,#26411,.T.) ;
#38229 = EDGE_CURVE('',#31429,#31361,#26412,.T.) ;
#38230 = EDGE_CURVE('',#31445,#31232,#26413,.T.) ;
#38231 = EDGE_CURVE('',#31440,#31434,#26414,.T.) ;
#38232 = EDGE_CURVE('',#31434,#31443,#26415,.T.) ;
#38233 = EDGE_CURVE('',#31222,#31360,#230,.T.) ;
#38234 = EDGE_CURVE('',#31446,#31220,#26416,.T.) ;
#38235 = EDGE_CURVE('',#31442,#31439,#26417,.T.) ;
#38236 = EDGE_CURVE('',#31218,#31446,#26418,.T.) ;
#38237 = EDGE_CURVE('',#31435,#31442,#26419,.T.) ;
#38238 = EDGE_CURVE('',#31441,#31437,#26420,.T.) ;
#38239 = EDGE_CURVE('',#31355,#31441,#26421,.T.) ;
#38240 = EDGE_CURVE('',#31230,#31360,#26422,.T.) ;
#38241 = EDGE_CURVE('',#31576,#31219,#26423,.T.) ;
#38242 = EDGE_CURVE('',#31435,#31439,#26424,.T.) ;
#38243 = EDGE_CURVE('',#31356,#31437,#26425,.T.) ;
#38244 = EDGE_CURVE('',#31231,#31359,#26426,.T.) ;
#38245 = EDGE_CURVE('',#31436,#31438,#26427,.T.) ;
#38246 = EDGE_CURVE('',#31357,#31436,#26428,.T.) ;
#38247 = EDGE_CURVE('',#31216,#31359,#231,.T.) ;
#38248 = EDGE_CURVE('',#31358,#31438,#26429,.T.) ;
#38249 = EDGE_CURVE('',#31235,#31516,#232,.T.) ;
#38250 = EDGE_CURVE('',#31519,#31515,#26430,.T.) ;
#38251 = EDGE_CURVE('',#31514,#31520,#26431,.T.) ;
#38252 = EDGE_CURVE('',#31517,#31400,#233,.T.) ;
#38253 = EDGE_CURVE('',#31512,#31537,#26432,.T.) ;
#38254 = EDGE_CURVE('',#31524,#31551,#26433,.T.) ;
#38255 = EDGE_CURVE('',#31525,#31550,#26434,.T.) ;
#38256 = EDGE_CURVE('',#31511,#31238,#234,.T.) ;
#38257 = EDGE_CURVE('',#31506,#31518,#26435,.T.) ;
#38258 = EDGE_CURVE('',#31536,#31513,#26436,.T.) ;
#38259 = EDGE_CURVE('',#31525,#31529,#26437,.T.) ;
#38260 = EDGE_CURVE('',#31529,#31550,#26438,.T.) ;
#38261 = EDGE_CURVE('',#31521,#31507,#26439,.T.) ;
#38262 = EDGE_CURVE('',#31552,#31531,#26440,.T.) ;
#38263 = EDGE_CURVE('',#31553,#31530,#26441,.T.) ;
#38264 = EDGE_CURVE('',#31526,#31553,#26442,.T.) ;
#38265 = EDGE_CURVE('',#31522,#31528,#26443,.T.) ;
#38266 = EDGE_CURVE('',#31548,#31523,#26444,.T.) ;
#38267 = EDGE_CURVE('',#31549,#31522,#26445,.T.) ;
#38268 = EDGE_CURVE('',#31526,#31530,#26446,.T.) ;
#38269 = EDGE_CURVE('',#31549,#31528,#26447,.T.) ;
#38270 = EDGE_CURVE('',#31527,#31533,#26448,.T.) ;
#38271 = EDGE_CURVE('',#31546,#31527,#26449,.T.) ;
#38272 = EDGE_CURVE('',#31546,#31533,#26450,.T.) ;
#38273 = EDGE_CURVE('',#31532,#31547,#26451,.T.) ;
#38274 = EDGE_CURVE('',#31508,#31535,#26452,.T.) ;
#38275 = EDGE_CURVE('',#31509,#31534,#26453,.T.) ;
#38276 = EDGE_CURVE('',#31403,#31510,#235,.T.) ;
#38277 = EDGE_CURVE('',#31501,#31502,#26454,.T.) ;
#38278 = EDGE_CURVE('',#31505,#31500,#26455,.T.) ;
#38279 = EDGE_CURVE('',#31488,#31539,#26456,.T.) ;
#38280 = EDGE_CURVE('',#31489,#31538,#26457,.T.) ;
#38281 = EDGE_CURVE('',#31540,#31495,#26458,.T.) ;
#38282 = EDGE_CURVE('',#31541,#31494,#26459,.T.) ;
#38283 = EDGE_CURVE('',#31538,#31493,#26460,.T.) ;
#38284 = EDGE_CURVE('',#31490,#31541,#26461,.T.) ;
#38285 = EDGE_CURVE('',#31489,#31493,#26462,.T.) ;
#38286 = EDGE_CURVE('',#31503,#31498,#26463,.T.) ;
#38287 = EDGE_CURVE('',#31499,#31504,#26464,.T.) ;
#38288 = EDGE_CURVE('',#31490,#31494,#26465,.T.) ;
#38289 = EDGE_CURVE('',#31486,#31492,#26466,.T.) ;
#38290 = EDGE_CURVE('',#31544,#31487,#26467,.T.) ;
#38291 = EDGE_CURVE('',#31545,#31486,#26468,.T.) ;
#38292 = EDGE_CURVE('',#31496,#31543,#26469,.T.) ;
#38293 = EDGE_CURVE('',#31497,#31542,#26470,.T.) ;
#38294 = EDGE_CURVE('',#31491,#31497,#26471,.T.) ;
#38295 = EDGE_CURVE('',#31545,#31492,#26472,.T.) ;
#38296 = EDGE_CURVE('',#31491,#31542,#26473,.T.) ;
#38297 = EDGE_CURVE('',#31249,#31248,#26474,.T.) ;
#38298 = EDGE_CURVE('',#31475,#31250,#236,.T.) ;
#38299 = EDGE_CURVE('',#31476,#31249,#26475,.T.) ;
#38300 = EDGE_CURVE('',#31476,#31248,#26476,.T.) ;
#38301 = EDGE_CURVE('',#31247,#31244,#26477,.T.) ;
#38302 = EDGE_CURVE('',#31473,#31247,#26478,.T.) ;
#38303 = EDGE_CURVE('',#31473,#31244,#26479,.T.) ;
#38304 = EDGE_CURVE('',#31243,#31474,#237,.T.) ;
#38305 = EDGE_CURVE('',#31205,#31484,#4942,.T.) ;
#38306 = EDGE_CURVE('',#31332,#31483,#26480,.T.) ;
#38307 = EDGE_CURVE('',#31329,#31332,#26481,.T.) ;
#38308 = EDGE_CURVE('',#31329,#31483,#26482,.T.) ;
#38309 = EDGE_CURVE('',#31330,#31485,#26483,.T.) ;
#38310 = EDGE_CURVE('',#31328,#31330,#26484,.T.) ;
#38311 = EDGE_CURVE('',#31328,#31485,#26485,.T.) ;
#38312 = EDGE_CURVE('',#31209,#31325,#4943,.T.) ;
#38313 = EDGE_CURVE('',#31397,#31234,#26486,.T.) ;
#38314 = EDGE_CURVE('',#31233,#31398,#26487,.T.) ;
#38315 = EDGE_CURVE('',#31559,#31267,#26488,.T.) ;
#38316 = EDGE_CURVE('',#31556,#31268,#26489,.T.) ;
#38317 = EDGE_CURVE('',#31267,#31557,#26490,.T.) ;
#38318 = EDGE_CURVE('',#31268,#31554,#26491,.T.) ;
#38319 = EDGE_CURVE('',#31391,#31401,#26492,.T.) ;
#38320 = EDGE_CURVE('',#31392,#31234,#26493,.T.) ;
#38321 = EDGE_CURVE('',#31392,#31397,#26494,.T.) ;
#38322 = EDGE_CURVE('',#31393,#31396,#26495,.T.) ;
#38323 = EDGE_CURVE('',#31388,#31395,#26496,.T.) ;
#38324 = EDGE_CURVE('',#31389,#31398,#26497,.T.) ;
#38325 = EDGE_CURVE('',#31389,#31233,#26498,.T.) ;
#38326 = EDGE_CURVE('',#31390,#31402,#26499,.T.) ;
#38327 = EDGE_CURVE('',#31242,#31478,#238,.T.) ;
#38328 = EDGE_CURVE('',#31474,#31477,#26500,.T.) ;
#38329 = EDGE_CURVE('',#31475,#31482,#26501,.T.) ;
#38330 = EDGE_CURVE('',#31577,#31481,#239,.T.) ;
#38331 = EDGE_CURVE('',#31578,#31577,#240,.T.) ;
#38332 = EDGE_CURVE('',#31579,#31578,#241,.T.) ;
#38333 = EDGE_CURVE('',#31251,#31579,#242,.T.) ;
#38334 = EDGE_CURVE('',#31333,#31252,#4944,.T.) ;
#38335 = EDGE_CURVE('',#31334,#31481,#26502,.T.) ;
#38336 = EDGE_CURVE('',#31208,#31326,#243,.T.) ;
#38337 = EDGE_CURVE('',#31335,#31480,#26503,.T.) ;
#38338 = EDGE_CURVE('',#31331,#31336,#4945,.T.) ;
#38339 = EDGE_CURVE('',#31479,#31484,#26504,.T.) ;
#38340 = EDGE_CURVE('',#31580,#31480,#244,.T.) ;
#38341 = EDGE_CURVE('',#31581,#31580,#245,.T.) ;
#38342 = EDGE_CURVE('',#31204,#31581,#246,.T.) ;
#38343 = EDGE_CURVE('',#31261,#31555,#26505,.T.) ;
#38344 = EDGE_CURVE('',#31227,#31555,#26506,.T.) ;
#38345 = EDGE_CURVE('',#31556,#31554,#26507,.T.) ;
#38346 = EDGE_CURVE('',#31524,#31520,#26508,.T.) ;
#38347 = EDGE_CURVE('',#31551,#31514,#26509,.T.) ;
#38348 = EDGE_CURVE('',#31521,#31523,#26510,.T.) ;
#38349 = EDGE_CURVE('',#31552,#31513,#26511,.T.) ;
#38350 = EDGE_CURVE('',#31507,#31548,#26512,.T.) ;
#38351 = EDGE_CURVE('',#31531,#31536,#26513,.T.) ;
#38352 = EDGE_CURVE('',#31508,#31547,#26514,.T.) ;
#38353 = EDGE_CURVE('',#31532,#31535,#26515,.T.) ;
#38354 = EDGE_CURVE('',#31488,#31502,#26516,.T.) ;
#38355 = EDGE_CURVE('',#31539,#31501,#26517,.T.) ;
#38356 = EDGE_CURVE('',#31503,#31487,#26518,.T.) ;
#38357 = EDGE_CURVE('',#31540,#31500,#26519,.T.) ;
#38358 = EDGE_CURVE('',#31498,#31544,#26520,.T.) ;
#38359 = EDGE_CURVE('',#31495,#31505,#26521,.T.) ;
#38360 = EDGE_CURVE('',#31499,#31543,#26522,.T.) ;
#38361 = EDGE_CURVE('',#31496,#31504,#26523,.T.) ;
#38362 = EDGE_CURVE('',#31558,#31256,#26524,.T.) ;
#38363 = EDGE_CURVE('',#31558,#31228,#26525,.T.) ;
#38364 = EDGE_CURVE('',#31559,#31557,#26526,.T.) ;
#38365 = EDGE_CURVE('',#31323,#31327,#4946,.T.) ;
#38366 = EDGE_CURVE('',#31324,#31207,#26527,.T.) ;
#38367 = EDGE_CURVE('',#31321,#31478,#26528,.T.) ;
#38368 = EDGE_CURVE('',#31322,#31241,#4947,.T.) ;
#38369 = EDGE_CURVE('',#31582,#31583,#247,.T.) ;
#38370 = EDGE_CURVE('',#31583,#31584,#4948,.T.) ;
#38371 = EDGE_CURVE('',#31584,#31585,#26529,.T.) ;
#38372 = EDGE_CURVE('',#31586,#31585,#4949,.T.) ;
#38373 = EDGE_CURVE('',#31582,#31586,#248,.T.) ;
#38374 = EDGE_CURVE('',#31587,#31588,#249,.T.) ;
#38375 = EDGE_CURVE('',#31588,#31589,#26530,.T.) ;
#38376 = EDGE_CURVE('',#31590,#31589,#4950,.T.) ;
#38377 = EDGE_CURVE('',#31591,#31590,#26531,.T.) ;
#38378 = EDGE_CURVE('',#31587,#31591,#4951,.T.) ;
#38379 = EDGE_CURVE('',#31592,#31592,#26532,.T.) ;
#38380 = EDGE_CURVE('',#31592,#31593,#26533,.T.) ;
#38381 = EDGE_CURVE('',#31593,#31593,#26534,.T.) ;
#38382 = EDGE_CURVE('',#31594,#31594,#26535,.T.) ;
#38383 = EDGE_CURVE('',#31594,#31595,#26536,.T.) ;
#38384 = EDGE_CURVE('',#31595,#31595,#26537,.T.) ;
#38385 = EDGE_CURVE('',#31596,#31597,#26538,.T.) ;
#38386 = EDGE_CURVE('',#31598,#31596,#9483,.T.) ;
#38387 = EDGE_CURVE('',#31598,#31599,#26539,.T.) ;
#38388 = EDGE_CURVE('',#31599,#31600,#26540,.T.) ;
#38389 = EDGE_CURVE('',#31597,#31600,#9484,.T.) ;
#38390 = EDGE_CURVE('',#31601,#31602,#26541,.T.) ;
#38391 = EDGE_CURVE('',#31603,#31601,#9485,.T.) ;
#38392 = EDGE_CURVE('',#31603,#31604,#26542,.T.) ;
#38393 = EDGE_CURVE('',#31602,#31604,#9486,.T.) ;
#38394 = EDGE_CURVE('',#31605,#31606,#26543,.T.) ;
#38395 = EDGE_CURVE('',#31605,#31607,#26544,.T.) ;
#38396 = EDGE_CURVE('',#31608,#31607,#26545,.T.) ;
#38397 = EDGE_CURVE('',#31608,#31606,#26546,.T.) ;
#38398 = EDGE_CURVE('',#31593,#31594,#9487,.T.) ;
#38399 = EDGE_CURVE('',#31606,#31609,#9488,.T.) ;
#38400 = EDGE_CURVE('',#31609,#31603,#26547,.T.) ;
#38401 = EDGE_CURVE('',#31610,#31601,#250,.T.) ;
#38402 = EDGE_CURVE('',#31610,#31611,#26548,.T.) ;
#38403 = EDGE_CURVE('',#31597,#31611,#251,.T.) ;
#38404 = EDGE_CURVE('',#31600,#31612,#26549,.T.) ;
#38405 = EDGE_CURVE('',#31612,#31605,#9489,.T.) ;
#38406 = EDGE_CURVE('',#31613,#31614,#9490,.T.) ;
#38407 = EDGE_CURVE('',#31614,#31615,#9491,.T.) ;
#38408 = EDGE_CURVE('',#31615,#31616,#252,.T.) ;
#38409 = EDGE_CURVE('',#31616,#31617,#9492,.T.) ;
#38410 = EDGE_CURVE('',#31617,#31618,#4952,.T.) ;
#38411 = EDGE_CURVE('',#31618,#31613,#9493,.T.) ;
#38412 = EDGE_CURVE('',#31619,#31620,#9494,.T.) ;
#38413 = EDGE_CURVE('',#31620,#31621,#9495,.T.) ;
#38414 = EDGE_CURVE('',#31621,#31622,#253,.T.) ;
#38415 = EDGE_CURVE('',#31622,#31623,#254,.T.) ;
#38416 = EDGE_CURVE('',#31623,#31624,#9496,.T.) ;
#38417 = EDGE_CURVE('',#31624,#31619,#9497,.T.) ;
#38418 = EDGE_CURVE('',#31625,#31626,#9498,.T.) ;
#38419 = EDGE_CURVE('',#31626,#31627,#9499,.T.) ;
#38420 = EDGE_CURVE('',#31627,#31628,#9500,.T.) ;
#38421 = EDGE_CURVE('',#31628,#31625,#9501,.T.) ;
#38422 = EDGE_CURVE('',#31629,#31630,#9502,.T.) ;
#38423 = EDGE_CURVE('',#31630,#31631,#255,.T.) ;
#38424 = EDGE_CURVE('',#31631,#31632,#256,.T.) ;
#38425 = EDGE_CURVE('',#31632,#31633,#9503,.T.) ;
#38426 = EDGE_CURVE('',#31633,#31634,#9504,.T.) ;
#38427 = EDGE_CURVE('',#31634,#31629,#9505,.T.) ;
#38428 = EDGE_CURVE('',#31635,#31636,#9506,.T.) ;
#38429 = EDGE_CURVE('',#31636,#31637,#9507,.T.) ;
#38430 = EDGE_CURVE('',#31637,#31638,#9508,.T.) ;
#38431 = EDGE_CURVE('',#31638,#31635,#9509,.T.) ;
#38432 = EDGE_CURVE('',#31639,#31640,#9510,.T.) ;
#38433 = EDGE_CURVE('',#31639,#31641,#9511,.T.) ;
#38434 = EDGE_CURVE('',#31641,#31642,#9512,.T.) ;
#38435 = EDGE_CURVE('',#31642,#31640,#9513,.T.) ;
#38436 = EDGE_CURVE('',#31643,#31644,#9514,.T.) ;
#38437 = EDGE_CURVE('',#31643,#31645,#9515,.T.) ;
#38438 = EDGE_CURVE('',#31645,#31646,#9516,.T.) ;
#38439 = EDGE_CURVE('',#31646,#31647,#9517,.T.) ;
#38440 = EDGE_CURVE('',#31647,#31648,#26550,.T.) ;
#38441 = EDGE_CURVE('',#31648,#31644,#9518,.T.) ;
#38442 = EDGE_CURVE('',#31649,#31650,#9519,.T.) ;
#38443 = EDGE_CURVE('',#31649,#31620,#26551,.T.) ;
#38444 = EDGE_CURVE('',#31619,#31626,#26552,.T.) ;
#38445 = EDGE_CURVE('',#31625,#31634,#26553,.T.) ;
#38446 = EDGE_CURVE('',#31633,#31651,#26554,.T.) ;
#38447 = EDGE_CURVE('',#31652,#31651,#9520,.T.) ;
#38448 = EDGE_CURVE('',#31652,#31653,#26555,.T.) ;
#38449 = EDGE_CURVE('',#31654,#31653,#9521,.T.) ;
#38450 = EDGE_CURVE('',#31654,#31655,#26556,.T.) ;
#38451 = EDGE_CURVE('',#31655,#31656,#9522,.T.) ;
#38452 = EDGE_CURVE('',#31656,#31657,#26557,.T.) ;
#38453 = EDGE_CURVE('',#31658,#31657,#9523,.T.) ;
#38454 = EDGE_CURVE('',#31658,#31659,#26558,.T.) ;
#38455 = EDGE_CURVE('',#31659,#31660,#9524,.T.) ;
#38456 = EDGE_CURVE('',#31660,#31661,#26559,.T.) ;
#38457 = EDGE_CURVE('',#31662,#31661,#9525,.T.) ;
#38458 = EDGE_CURVE('',#31662,#31638,#26560,.T.) ;
#38459 = EDGE_CURVE('',#31637,#31663,#26561,.T.) ;
#38460 = EDGE_CURVE('',#31663,#31664,#9526,.T.) ;
#38461 = EDGE_CURVE('',#31664,#31646,#26562,.T.) ;
#38462 = EDGE_CURVE('',#31645,#31665,#26563,.T.) ;
#38463 = EDGE_CURVE('',#31666,#31665,#9527,.T.) ;
#38464 = EDGE_CURVE('',#31667,#31666,#9528,.T.) ;
#38465 = EDGE_CURVE('',#31667,#31668,#26564,.T.) ;
#38466 = EDGE_CURVE('',#31669,#31668,#9529,.T.) ;
#38467 = EDGE_CURVE('',#31669,#31670,#26565,.T.) ;
#38468 = EDGE_CURVE('',#31671,#31670,#9530,.T.) ;
#38469 = EDGE_CURVE('',#31671,#31650,#26566,.T.) ;
#38470 = EDGE_CURVE('',#31672,#31673,#9531,.T.) ;
#38471 = EDGE_CURVE('',#31673,#31674,#26567,.T.) ;
#38472 = EDGE_CURVE('',#31674,#31675,#9532,.T.) ;
#38473 = EDGE_CURVE('',#31675,#31676,#26568,.T.) ;
#38474 = EDGE_CURVE('',#31676,#31677,#9533,.T.) ;
#38475 = EDGE_CURVE('',#31677,#31678,#26569,.T.) ;
#38476 = EDGE_CURVE('',#31678,#31679,#9534,.T.) ;
#38477 = EDGE_CURVE('',#31679,#31680,#26570,.T.) ;
#38478 = EDGE_CURVE('',#31680,#31681,#9535,.T.) ;
#38479 = EDGE_CURVE('',#31681,#31682,#9536,.T.) ;
#38480 = EDGE_CURVE('',#31682,#31643,#26571,.T.) ;
#38481 = EDGE_CURVE('',#31644,#31683,#26572,.T.) ;
#38482 = EDGE_CURVE('',#31683,#31684,#9537,.T.) ;
#38483 = EDGE_CURVE('',#31684,#31639,#26573,.T.) ;
#38484 = EDGE_CURVE('',#31640,#31685,#26574,.T.) ;
#38485 = EDGE_CURVE('',#31686,#31685,#9538,.T.) ;
#38486 = EDGE_CURVE('',#31686,#31687,#26575,.T.) ;
#38487 = EDGE_CURVE('',#31688,#31687,#9539,.T.) ;
#38488 = EDGE_CURVE('',#31688,#31689,#26576,.T.) ;
#38489 = EDGE_CURVE('',#31689,#31690,#9540,.T.) ;
#38490 = EDGE_CURVE('',#31690,#31691,#26577,.T.) ;
#38491 = EDGE_CURVE('',#31692,#31691,#9541,.T.) ;
#38492 = EDGE_CURVE('',#31692,#31693,#26578,.T.) ;
#38493 = EDGE_CURVE('',#31694,#31693,#9542,.T.) ;
#38494 = EDGE_CURVE('',#31694,#31695,#26579,.T.) ;
#38495 = EDGE_CURVE('',#31695,#31696,#9543,.T.) ;
#38496 = EDGE_CURVE('',#31696,#31697,#26580,.T.) ;
#38497 = EDGE_CURVE('',#31697,#31698,#9544,.T.) ;
#38498 = EDGE_CURVE('',#31698,#31699,#26581,.T.) ;
#38499 = EDGE_CURVE('',#31699,#31700,#9545,.T.) ;
#38500 = EDGE_CURVE('',#31700,#31672,#26582,.T.) ;
#38501 = EDGE_CURVE('',#31668,#31679,#9546,.T.) ;
#38502 = EDGE_CURVE('',#31678,#31669,#9547,.T.) ;
#38503 = EDGE_CURVE('',#31670,#31677,#9548,.T.) ;
#38504 = EDGE_CURVE('',#31676,#31671,#9549,.T.) ;
#38505 = EDGE_CURVE('',#31701,#31702,#257,.T.) ;
#38506 = EDGE_CURVE('',#31702,#31649,#9550,.T.) ;
#38507 = EDGE_CURVE('',#31650,#31675,#9551,.T.) ;
#38508 = EDGE_CURVE('',#31674,#31703,#9552,.T.) ;
#38509 = EDGE_CURVE('',#31703,#31704,#258,.T.) ;
#38510 = EDGE_CURVE('',#31704,#31701,#9553,.T.) ;
#38511 = EDGE_CURVE('',#31705,#31706,#259,.T.) ;
#38512 = EDGE_CURVE('',#31706,#31707,#4953,.T.) ;
#38513 = EDGE_CURVE('',#31707,#31673,#9554,.T.) ;
#38514 = EDGE_CURVE('',#31672,#31708,#9555,.T.) ;
#38515 = EDGE_CURVE('',#31708,#31705,#9556,.T.) ;
#38516 = EDGE_CURVE('',#31709,#31710,#9557,.T.) ;
#38517 = EDGE_CURVE('',#31710,#31700,#9558,.T.) ;
#38518 = EDGE_CURVE('',#31699,#31709,#9559,.T.) ;
#38519 = EDGE_CURVE('',#31711,#31582,#260,.T.) ;
#38520 = EDGE_CURVE('',#31586,#31712,#9560,.T.) ;
#38521 = EDGE_CURVE('',#31712,#31698,#9561,.T.) ;
#38522 = EDGE_CURVE('',#31697,#31711,#9562,.T.) ;
#38523 = EDGE_CURVE('',#31651,#31713,#9563,.T.) ;
#38524 = EDGE_CURVE('',#31713,#31714,#261,.T.) ;
#38525 = EDGE_CURVE('',#31714,#31715,#9564,.T.) ;
#38526 = EDGE_CURVE('',#31715,#31716,#262,.T.) ;
#38527 = EDGE_CURVE('',#31716,#31696,#9565,.T.) ;
#38528 = EDGE_CURVE('',#31695,#31717,#9566,.T.) ;
#38529 = EDGE_CURVE('',#31717,#31718,#9567,.T.) ;
#38530 = EDGE_CURVE('',#31719,#31718,#26583,.T.) ;
#38531 = EDGE_CURVE('',#31719,#31720,#9568,.T.) ;
#38532 = EDGE_CURVE('',#31721,#31720,#26584,.T.) ;
#38533 = EDGE_CURVE('',#31721,#31722,#9569,.T.) ;
#38534 = EDGE_CURVE('',#31722,#31652,#9570,.T.) ;
#38535 = EDGE_CURVE('',#31723,#31724,#26585,.T.) ;
#38536 = EDGE_CURVE('',#31723,#31658,#9571,.T.) ;
#38537 = EDGE_CURVE('',#31657,#31725,#9572,.T.) ;
#38538 = EDGE_CURVE('',#31726,#31725,#26586,.T.) ;
#38539 = EDGE_CURVE('',#31726,#31727,#26587,.T.) ;
#38540 = EDGE_CURVE('',#31728,#31727,#26588,.T.) ;
#38541 = EDGE_CURVE('',#31728,#31729,#9573,.T.) ;
#38542 = EDGE_CURVE('',#31729,#31730,#9574,.T.) ;
#38543 = EDGE_CURVE('',#31730,#31731,#9575,.T.) ;
#38544 = EDGE_CURVE('',#31732,#31731,#26589,.T.) ;
#38545 = EDGE_CURVE('',#31732,#31733,#26590,.T.) ;
#38546 = EDGE_CURVE('',#31734,#31733,#26591,.T.) ;
#38547 = EDGE_CURVE('',#31734,#31690,#9576,.T.) ;
#38548 = EDGE_CURVE('',#31689,#31735,#9577,.T.) ;
#38549 = EDGE_CURVE('',#31736,#31735,#26592,.T.) ;
#38550 = EDGE_CURVE('',#31736,#31737,#26593,.T.) ;
#38551 = EDGE_CURVE('',#31738,#31737,#26594,.T.) ;
#38552 = EDGE_CURVE('',#31738,#31739,#9578,.T.) ;
#38553 = EDGE_CURVE('',#31739,#31740,#26595,.T.) ;
#38554 = EDGE_CURVE('',#31740,#31741,#9579,.T.) ;
#38555 = EDGE_CURVE('',#31742,#31741,#26596,.T.) ;
#38556 = EDGE_CURVE('',#31742,#31724,#26597,.T.) ;
#38557 = EDGE_CURVE('',#31743,#31744,#26598,.T.) ;
#38558 = EDGE_CURVE('',#31743,#31745,#9580,.T.) ;
#38559 = EDGE_CURVE('',#31666,#31745,#9581,.T.) ;
#38560 = EDGE_CURVE('',#31665,#31682,#9582,.T.) ;
#38561 = EDGE_CURVE('',#31746,#31681,#9583,.T.) ;
#38562 = EDGE_CURVE('',#31746,#31747,#9584,.T.) ;
#38563 = EDGE_CURVE('',#31748,#31747,#26599,.T.) ;
#38564 = EDGE_CURVE('',#31748,#31744,#9585,.T.) ;
#38565 = EDGE_CURVE('',#31749,#31750,#26600,.T.) ;
#38566 = EDGE_CURVE('',#31749,#31746,#9586,.T.) ;
#38567 = EDGE_CURVE('',#31680,#31667,#9587,.T.) ;
#38568 = EDGE_CURVE('',#31745,#31751,#9588,.T.) ;
#38569 = EDGE_CURVE('',#31752,#31751,#26601,.T.) ;
#38570 = EDGE_CURVE('',#31752,#31750,#9589,.T.) ;
#38571 = EDGE_CURVE('',#31753,#31754,#9590,.T.) ;
#38572 = EDGE_CURVE('',#31754,#31755,#9591,.T.) ;
#38573 = EDGE_CURVE('',#31753,#31755,#26602,.T.) ;
#38574 = EDGE_CURVE('',#31756,#31757,#26603,.T.) ;
#38575 = EDGE_CURVE('',#31756,#31758,#9592,.T.) ;
#38576 = EDGE_CURVE('',#31758,#31757,#9593,.T.) ;
#38577 = EDGE_CURVE('',#31759,#31760,#9594,.T.) ;
#38578 = EDGE_CURVE('',#31760,#31761,#9595,.T.) ;
#38579 = EDGE_CURVE('',#31761,#31762,#9596,.T.) ;
#38580 = EDGE_CURVE('',#31762,#31763,#9597,.T.) ;
#38581 = EDGE_CURVE('',#31763,#31764,#9598,.T.) ;
#38582 = EDGE_CURVE('',#31764,#31765,#9599,.T.) ;
#38583 = EDGE_CURVE('',#31765,#31766,#9600,.T.) ;
#38584 = EDGE_CURVE('',#31766,#31759,#9601,.T.) ;
#38585 = EDGE_CURVE('',#31767,#31768,#9602,.T.) ;
#38586 = EDGE_CURVE('',#31768,#31769,#9603,.T.) ;
#38587 = EDGE_CURVE('',#31769,#31770,#9604,.T.) ;
#38588 = EDGE_CURVE('',#31770,#31767,#9605,.T.) ;
#38589 = EDGE_CURVE('',#31771,#31772,#9606,.T.) ;
#38590 = EDGE_CURVE('',#31772,#31773,#9607,.T.) ;
#38591 = EDGE_CURVE('',#31773,#31774,#9608,.T.) ;
#38592 = EDGE_CURVE('',#31774,#31771,#9609,.T.) ;
#38593 = EDGE_CURVE('',#31775,#31776,#9610,.T.) ;
#38594 = EDGE_CURVE('',#31776,#31777,#9611,.T.) ;
#38595 = EDGE_CURVE('',#31777,#31778,#9612,.T.) ;
#38596 = EDGE_CURVE('',#31778,#31775,#9613,.T.) ;
#38597 = EDGE_CURVE('',#31779,#31780,#263,.T.) ;
#38598 = EDGE_CURVE('',#31780,#31781,#9614,.T.) ;
#38599 = EDGE_CURVE('',#31781,#31782,#9615,.T.) ;
#38600 = EDGE_CURVE('',#31782,#31783,#9616,.T.) ;
#38601 = EDGE_CURVE('',#31783,#31784,#264,.T.) ;
#38602 = EDGE_CURVE('',#31784,#31779,#9617,.T.) ;
#38603 = EDGE_CURVE('',#31785,#31786,#9618,.T.) ;
#38604 = EDGE_CURVE('',#31786,#31787,#9619,.T.) ;
#38605 = EDGE_CURVE('',#31787,#31788,#9620,.T.) ;
#38606 = EDGE_CURVE('',#31788,#31789,#9621,.T.) ;
#38607 = EDGE_CURVE('',#31789,#31790,#9622,.T.) ;
#38608 = EDGE_CURVE('',#31790,#31791,#9623,.T.) ;
#38609 = EDGE_CURVE('',#31791,#31792,#9624,.T.) ;
#38610 = EDGE_CURVE('',#31792,#31785,#9625,.T.) ;
#38611 = EDGE_CURVE('',#31793,#31794,#9626,.T.) ;
#38612 = EDGE_CURVE('',#31793,#31795,#26604,.T.) ;
#38613 = EDGE_CURVE('',#31795,#31796,#9627,.T.) ;
#38614 = EDGE_CURVE('',#31796,#31797,#26605,.T.) ;
#38615 = EDGE_CURVE('',#31797,#31798,#9628,.T.) ;
#38616 = EDGE_CURVE('',#31798,#31799,#26606,.T.) ;
#38617 = EDGE_CURVE('',#31799,#31800,#9629,.T.) ;
#38618 = EDGE_CURVE('',#31800,#31794,#26607,.T.) ;
#38619 = EDGE_CURVE('',#31801,#31802,#26608,.T.) ;
#38620 = EDGE_CURVE('',#31801,#31662,#9630,.T.) ;
#38621 = EDGE_CURVE('',#31661,#31803,#9631,.T.) ;
#38622 = EDGE_CURVE('',#31803,#31804,#26609,.T.) ;
#38623 = EDGE_CURVE('',#31804,#31805,#9632,.T.) ;
#38624 = EDGE_CURVE('',#31805,#31802,#26610,.T.) ;
#38625 = EDGE_CURVE('',#31659,#31806,#9633,.T.) ;
#38626 = EDGE_CURVE('',#31806,#31807,#9634,.T.) ;
#38627 = EDGE_CURVE('',#31807,#31660,#9635,.T.) ;
#38628 = EDGE_CURVE('',#31808,#31809,#9636,.T.) ;
#38629 = EDGE_CURVE('',#31809,#31602,#9637,.T.) ;
#38630 = EDGE_CURVE('',#31604,#31808,#9638,.T.) ;
#38631 = EDGE_CURVE('',#31810,#31811,#26611,.T.) ;
#38632 = EDGE_CURVE('',#31811,#31812,#9639,.T.) ;
#38633 = EDGE_CURVE('',#31812,#31813,#26612,.T.) ;
#38634 = EDGE_CURVE('',#31813,#31810,#9640,.T.) ;
#38635 = EDGE_CURVE('',#31814,#31815,#26613,.T.) ;
#38636 = EDGE_CURVE('',#31815,#31816,#9641,.T.) ;
#38637 = EDGE_CURVE('',#31816,#31817,#26614,.T.) ;
#38638 = EDGE_CURVE('',#31817,#31814,#9642,.T.) ;
#38639 = EDGE_CURVE('',#31596,#31818,#9643,.T.) ;
#38640 = EDGE_CURVE('',#31818,#31819,#9644,.T.) ;
#38641 = EDGE_CURVE('',#31819,#31598,#9645,.T.) ;
#38642 = EDGE_CURVE('',#31820,#31821,#9646,.T.) ;
#38643 = EDGE_CURVE('',#31821,#31688,#9647,.T.) ;
#38644 = EDGE_CURVE('',#31687,#31820,#9648,.T.) ;
#38645 = EDGE_CURVE('',#31822,#31823,#26615,.T.) ;
#38646 = EDGE_CURVE('',#31823,#31686,#9649,.T.) ;
#38647 = EDGE_CURVE('',#31685,#31824,#9650,.T.) ;
#38648 = EDGE_CURVE('',#31825,#31824,#26616,.T.) ;
#38649 = EDGE_CURVE('',#31825,#31826,#26617,.T.) ;
#38650 = EDGE_CURVE('',#31826,#31822,#9651,.T.) ;
#38651 = EDGE_CURVE('',#31827,#31828,#26618,.T.) ;
#38652 = EDGE_CURVE('',#31828,#31654,#9652,.T.) ;
#38653 = EDGE_CURVE('',#31653,#31829,#9653,.T.) ;
#38654 = EDGE_CURVE('',#31829,#31827,#9654,.T.) ;
#38655 = EDGE_CURVE('',#31830,#31831,#9655,.T.) ;
#38656 = EDGE_CURVE('',#31831,#31656,#9656,.T.) ;
#38657 = EDGE_CURVE('',#31655,#31830,#9657,.T.) ;
#38658 = EDGE_CURVE('',#31832,#31833,#26619,.T.) ;
#38659 = EDGE_CURVE('',#31833,#31834,#9658,.T.) ;
#38660 = EDGE_CURVE('',#31834,#31835,#26620,.T.) ;
#38661 = EDGE_CURVE('',#31835,#31832,#9659,.T.) ;
#38662 = EDGE_CURVE('',#31836,#31837,#9660,.T.) ;
#38663 = EDGE_CURVE('',#31837,#31838,#9661,.T.) ;
#38664 = EDGE_CURVE('',#31838,#31839,#9662,.T.) ;
#38665 = EDGE_CURVE('',#31839,#31836,#9663,.T.) ;
#38666 = EDGE_CURVE('',#31840,#31841,#26621,.T.) ;
#38667 = EDGE_CURVE('',#31841,#31842,#9664,.T.) ;
#38668 = EDGE_CURVE('',#31842,#31843,#26622,.T.) ;
#38669 = EDGE_CURVE('',#31843,#31840,#9665,.T.) ;
#38670 = EDGE_CURVE('',#31691,#31844,#9666,.T.) ;
#38671 = EDGE_CURVE('',#31844,#31845,#9667,.T.) ;
#38672 = EDGE_CURVE('',#31845,#31692,#9668,.T.) ;
#38673 = EDGE_CURVE('',#31846,#31847,#9669,.T.) ;
#38674 = EDGE_CURVE('',#31847,#31848,#9670,.T.) ;
#38675 = EDGE_CURVE('',#31848,#31849,#9671,.T.) ;
#38676 = EDGE_CURVE('',#31849,#31846,#9672,.T.) ;
#38677 = EDGE_CURVE('',#31850,#31851,#9673,.T.) ;
#38678 = EDGE_CURVE('',#31851,#31694,#9674,.T.) ;
#38679 = EDGE_CURVE('',#31693,#31852,#9675,.T.) ;
#38680 = EDGE_CURVE('',#31852,#31850,#26623,.T.) ;
#38681 = EDGE_CURVE('',#31853,#31854,#9676,.T.) ;
#38682 = EDGE_CURVE('',#31854,#31855,#9677,.T.) ;
#38683 = EDGE_CURVE('',#31855,#31856,#9678,.T.) ;
#38684 = EDGE_CURVE('',#31856,#31853,#9679,.T.) ;
#38685 = EDGE_CURVE('',#31857,#31858,#4954,.T.) ;
#38686 = EDGE_CURVE('',#31858,#31587,#9680,.T.) ;
#38687 = EDGE_CURVE('',#31591,#31859,#9681,.T.) ;
#38688 = EDGE_CURVE('',#31859,#31860,#4955,.T.) ;
#38689 = EDGE_CURVE('',#31860,#31861,#9682,.T.) ;
#38690 = EDGE_CURVE('',#31861,#31862,#4956,.T.) ;
#38691 = EDGE_CURVE('',#31862,#31857,#9683,.T.) ;
#38692 = EDGE_CURVE('',#31863,#31864,#9684,.T.) ;
#38693 = EDGE_CURVE('',#31864,#31590,#9685,.T.) ;
#38694 = EDGE_CURVE('',#31590,#31865,#9686,.T.) ;
#38695 = EDGE_CURVE('',#31865,#31863,#9687,.T.) ;
#38696 = EDGE_CURVE('',#31866,#31867,#9688,.T.) ;
#38697 = EDGE_CURVE('',#31867,#31868,#9689,.T.) ;
#38698 = EDGE_CURVE('',#31868,#31869,#9690,.T.) ;
#38699 = EDGE_CURVE('',#31869,#31866,#9691,.T.) ;
#38700 = EDGE_CURVE('',#31870,#31871,#9692,.T.) ;
#38701 = EDGE_CURVE('',#31871,#31872,#9693,.T.) ;
#38702 = EDGE_CURVE('',#31872,#31873,#9694,.T.) ;
#38703 = EDGE_CURVE('',#31873,#31870,#9695,.T.) ;
#38704 = EDGE_CURVE('',#31874,#31875,#9696,.T.) ;
#38705 = EDGE_CURVE('',#31875,#31876,#9697,.T.) ;
#38706 = EDGE_CURVE('',#31876,#31877,#9698,.T.) ;
#38707 = EDGE_CURVE('',#31877,#31874,#9699,.T.) ;
#38708 = EDGE_CURVE('',#31794,#31878,#9700,.T.) ;
#38709 = EDGE_CURVE('',#31878,#31879,#9701,.T.) ;
#38710 = EDGE_CURVE('',#31879,#31793,#9702,.T.) ;
#38711 = EDGE_CURVE('',#31797,#31880,#9703,.T.) ;
#38712 = EDGE_CURVE('',#31880,#31881,#9704,.T.) ;
#38713 = EDGE_CURVE('',#31881,#31798,#9705,.T.) ;
#38714 = EDGE_CURVE('',#31799,#31882,#9706,.T.) ;
#38715 = EDGE_CURVE('',#31882,#31883,#9707,.T.) ;
#38716 = EDGE_CURVE('',#31883,#31800,#9708,.T.) ;
#38717 = EDGE_CURVE('',#31795,#31884,#9709,.T.) ;
#38718 = EDGE_CURVE('',#31884,#31885,#9710,.T.) ;
#38719 = EDGE_CURVE('',#31885,#31796,#9711,.T.) ;
#38720 = EDGE_CURVE('',#31886,#31887,#9712,.T.) ;
#38721 = EDGE_CURVE('',#31887,#31888,#9713,.T.) ;
#38722 = EDGE_CURVE('',#31888,#31889,#9714,.T.) ;
#38723 = EDGE_CURVE('',#31889,#31890,#26624,.T.) ;
#38724 = EDGE_CURVE('',#31890,#31891,#9715,.T.) ;
#38725 = EDGE_CURVE('',#31891,#31886,#26625,.T.) ;
#38726 = EDGE_CURVE('',#31892,#31893,#9716,.T.) ;
#38727 = EDGE_CURVE('',#31893,#31894,#9717,.T.) ;
#38728 = EDGE_CURVE('',#31894,#31895,#9718,.T.) ;
#38729 = EDGE_CURVE('',#31895,#31896,#26626,.T.) ;
#38730 = EDGE_CURVE('',#31896,#31897,#9719,.T.) ;
#38731 = EDGE_CURVE('',#31897,#31892,#26627,.T.) ;
#38732 = EDGE_CURVE('',#31898,#31899,#9720,.T.) ;
#38733 = EDGE_CURVE('',#31898,#31617,#26628,.T.) ;
#38734 = EDGE_CURVE('',#31616,#31899,#26629,.T.) ;
#38735 = EDGE_CURVE('',#31899,#31900,#9721,.T.) ;
#38736 = EDGE_CURVE('',#31900,#31901,#9722,.T.) ;
#38737 = EDGE_CURVE('',#31901,#31898,#9723,.T.) ;
#38738 = EDGE_CURVE('',#31902,#31903,#9724,.T.) ;
#38739 = EDGE_CURVE('',#31903,#31904,#9725,.T.) ;
#38740 = EDGE_CURVE('',#31904,#31905,#9726,.T.) ;
#38741 = EDGE_CURVE('',#31905,#31902,#9727,.T.) ;
#38742 = EDGE_CURVE('',#31906,#31907,#9728,.T.) ;
#38743 = EDGE_CURVE('',#31907,#31908,#9729,.T.) ;
#38744 = EDGE_CURVE('',#31908,#31909,#9730,.T.) ;
#38745 = EDGE_CURVE('',#31909,#31906,#9731,.T.) ;
#38746 = EDGE_CURVE('',#31910,#31911,#9732,.T.) ;
#38747 = EDGE_CURVE('',#31911,#31912,#9733,.T.) ;
#38748 = EDGE_CURVE('',#31912,#31913,#9734,.T.) ;
#38749 = EDGE_CURVE('',#31913,#31910,#9735,.T.) ;
#38750 = EDGE_CURVE('',#31914,#31915,#9736,.T.) ;
#38751 = EDGE_CURVE('',#31915,#31916,#9737,.T.) ;
#38752 = EDGE_CURVE('',#31916,#31917,#9738,.T.) ;
#38753 = EDGE_CURVE('',#31914,#31917,#9739,.T.) ;
#38754 = EDGE_CURVE('',#31784,#31914,#26630,.T.) ;
#38755 = EDGE_CURVE('',#31917,#31779,#26631,.T.) ;
#38756 = EDGE_CURVE('',#31918,#31919,#9740,.T.) ;
#38757 = EDGE_CURVE('',#31919,#31920,#9741,.T.) ;
#38758 = EDGE_CURVE('',#31920,#31921,#9742,.T.) ;
#38759 = EDGE_CURVE('',#31921,#31918,#9743,.T.) ;
#38760 = EDGE_CURVE('',#31922,#31923,#9744,.T.) ;
#38761 = EDGE_CURVE('',#31923,#31924,#9745,.T.) ;
#38762 = EDGE_CURVE('',#31924,#31925,#9746,.T.) ;
#38763 = EDGE_CURVE('',#31925,#31922,#9747,.T.) ;
#38764 = EDGE_CURVE('',#31926,#31927,#9748,.T.) ;
#38765 = EDGE_CURVE('',#31927,#31928,#9749,.T.) ;
#38766 = EDGE_CURVE('',#31928,#31929,#9750,.T.) ;
#38767 = EDGE_CURVE('',#31929,#31926,#9751,.T.) ;
#38768 = EDGE_CURVE('',#31930,#31931,#9752,.T.) ;
#38769 = EDGE_CURVE('',#31931,#31932,#9753,.T.) ;
#38770 = EDGE_CURVE('',#31932,#31933,#9754,.T.) ;
#38771 = EDGE_CURVE('',#31933,#31930,#9755,.T.) ;
#38772 = EDGE_CURVE('',#31683,#31934,#9756,.T.) ;
#38773 = EDGE_CURVE('',#31934,#31935,#26632,.T.) ;
#38774 = EDGE_CURVE('',#31935,#31684,#9757,.T.) ;
#38775 = EDGE_CURVE('',#31936,#31937,#26633,.T.) ;
#38776 = EDGE_CURVE('',#31937,#31608,#26634,.T.) ;
#38777 = EDGE_CURVE('',#31607,#31936,#26635,.T.) ;
#38778 = EDGE_CURVE('',#31663,#31938,#9758,.T.) ;
#38779 = EDGE_CURVE('',#31938,#31939,#26636,.T.) ;
#38780 = EDGE_CURVE('',#31939,#31664,#9759,.T.) ;
#38781 = EDGE_CURVE('',#31852,#31845,#26637,.T.) ;
#38782 = EDGE_CURVE('',#31852,#31841,#26638,.T.) ;
#38783 = EDGE_CURVE('',#31841,#31845,#26639,.T.) ;
#38784 = EDGE_CURVE('',#31844,#31734,#26640,.T.) ;
#38785 = EDGE_CURVE('',#31842,#31844,#26641,.T.) ;
#38786 = EDGE_CURVE('',#31850,#31840,#26642,.T.) ;
#38787 = EDGE_CURVE('',#31842,#31733,#26643,.T.) ;
#38788 = EDGE_CURVE('',#31850,#31849,#26644,.T.) ;
#38789 = EDGE_CURVE('',#31849,#31840,#26645,.T.) ;
#38790 = EDGE_CURVE('',#31830,#31828,#26646,.T.) ;
#38791 = EDGE_CURVE('',#31831,#31835,#26647,.T.) ;
#38792 = EDGE_CURVE('',#31832,#31830,#26648,.T.) ;
#38793 = EDGE_CURVE('',#31725,#31831,#26649,.T.) ;
#38794 = EDGE_CURVE('',#31843,#31732,#26650,.T.) ;
#38795 = EDGE_CURVE('',#31846,#31843,#26651,.T.) ;
#38796 = EDGE_CURVE('',#31851,#31848,#26652,.T.) ;
#38797 = EDGE_CURVE('',#31717,#31851,#26653,.T.) ;
#38798 = EDGE_CURVE('',#31832,#31828,#26654,.T.) ;
#38799 = EDGE_CURVE('',#31726,#31835,#26655,.T.) ;
#38800 = EDGE_CURVE('',#31846,#31731,#26656,.T.) ;
#38801 = EDGE_CURVE('',#31717,#31848,#26657,.T.) ;
#38802 = EDGE_CURVE('',#31833,#31827,#26658,.T.) ;
#38803 = EDGE_CURVE('',#31834,#31839,#26659,.T.) ;
#38804 = EDGE_CURVE('',#31836,#31833,#26660,.T.) ;
#38805 = EDGE_CURVE('',#31727,#31834,#26661,.T.) ;
#38806 = EDGE_CURVE('',#31847,#31730,#26662,.T.) ;
#38807 = EDGE_CURVE('',#31718,#31847,#26663,.T.) ;
#38808 = EDGE_CURVE('',#31836,#31827,#26664,.T.) ;
#38809 = EDGE_CURVE('',#31728,#31839,#26665,.T.) ;
#38810 = EDGE_CURVE('',#31719,#31730,#26666,.T.) ;
#38811 = EDGE_CURVE('',#31829,#31722,#26667,.T.) ;
#38812 = EDGE_CURVE('',#31837,#31829,#26668,.T.) ;
#38813 = EDGE_CURVE('',#31729,#31838,#26669,.T.) ;
#38814 = EDGE_CURVE('',#31720,#31729,#26670,.T.) ;
#38815 = EDGE_CURVE('',#31837,#31722,#26671,.T.) ;
#38816 = EDGE_CURVE('',#31721,#31838,#26672,.T.) ;
#38817 = EDGE_CURVE('',#31785,#31766,#26673,.T.) ;
#38818 = EDGE_CURVE('',#31774,#31785,#26674,.T.) ;
#38819 = EDGE_CURVE('',#31766,#31774,#26675,.T.) ;
#38820 = EDGE_CURVE('',#31792,#31940,#265,.T.) ;
#38821 = EDGE_CURVE('',#31940,#31771,#4957,.T.) ;
#38822 = EDGE_CURVE('',#31773,#31941,#4958,.T.) ;
#38823 = EDGE_CURVE('',#31941,#31759,#266,.T.) ;
#38824 = EDGE_CURVE('',#31786,#31765,#26676,.T.) ;
#38825 = EDGE_CURVE('',#31781,#31942,#4959,.T.) ;
#38826 = EDGE_CURVE('',#31942,#31792,#267,.T.) ;
#38827 = EDGE_CURVE('',#31791,#31943,#268,.T.) ;
#38828 = EDGE_CURVE('',#31943,#31782,#4960,.T.) ;
#38829 = EDGE_CURVE('',#31759,#31944,#269,.T.) ;
#38830 = EDGE_CURVE('',#31944,#31776,#4961,.T.) ;
#38831 = EDGE_CURVE('',#31775,#31945,#4962,.T.) ;
#38832 = EDGE_CURVE('',#31945,#31760,#270,.T.) ;
#38833 = EDGE_CURVE('',#31786,#31757,#26677,.T.) ;
#38834 = EDGE_CURVE('',#31756,#31765,#26678,.T.) ;
#38835 = EDGE_CURVE('',#31946,#31757,#9760,.T.) ;
#38836 = EDGE_CURVE('',#31787,#31946,#26679,.T.) ;
#38837 = EDGE_CURVE('',#31947,#31946,#26680,.T.) ;
#38838 = EDGE_CURVE('',#31787,#31947,#26681,.T.) ;
#38839 = EDGE_CURVE('',#31770,#31948,#4963,.T.) ;
#38840 = EDGE_CURVE('',#31948,#31791,#271,.T.) ;
#38841 = EDGE_CURVE('',#31767,#31790,#26682,.T.) ;
#38842 = EDGE_CURVE('',#31760,#31949,#272,.T.) ;
#38843 = EDGE_CURVE('',#31949,#31768,#4964,.T.) ;
#38844 = EDGE_CURVE('',#31761,#31767,#26683,.T.) ;
#38845 = EDGE_CURVE('',#31950,#31764,#26684,.T.) ;
#38846 = EDGE_CURVE('',#31756,#31950,#9761,.T.) ;
#38847 = EDGE_CURVE('',#31745,#31758,#4965,.T.) ;
#38848 = EDGE_CURVE('',#31946,#31743,#26685,.T.) ;
#38849 = EDGE_CURVE('',#31947,#31744,#26686,.T.) ;
#38850 = EDGE_CURVE('',#31951,#31947,#9762,.T.) ;
#38851 = EDGE_CURVE('',#31788,#31951,#26687,.T.) ;
#38852 = EDGE_CURVE('',#31761,#31790,#26688,.T.) ;
#38853 = EDGE_CURVE('',#31950,#31952,#26689,.T.) ;
#38854 = EDGE_CURVE('',#31952,#31764,#26690,.T.) ;
#38855 = EDGE_CURVE('',#31751,#31950,#26691,.T.) ;
#38856 = EDGE_CURVE('',#31951,#31748,#26692,.T.) ;
#38857 = EDGE_CURVE('',#31953,#31951,#26693,.T.) ;
#38858 = EDGE_CURVE('',#31788,#31953,#26694,.T.) ;
#38859 = EDGE_CURVE('',#31762,#31789,#26695,.T.) ;
#38860 = EDGE_CURVE('',#31954,#31763,#26696,.T.) ;
#38861 = EDGE_CURVE('',#31952,#31954,#9763,.T.) ;
#38862 = EDGE_CURVE('',#31752,#31952,#26697,.T.) ;
#38863 = EDGE_CURVE('',#31953,#31747,#26698,.T.) ;
#38864 = EDGE_CURVE('',#31753,#31953,#9764,.T.) ;
#38865 = EDGE_CURVE('',#31789,#31753,#26699,.T.) ;
#38866 = EDGE_CURVE('',#31762,#31755,#26700,.T.) ;
#38867 = EDGE_CURVE('',#31954,#31955,#26701,.T.) ;
#38868 = EDGE_CURVE('',#31955,#31763,#26702,.T.) ;
#38869 = EDGE_CURVE('',#31750,#31954,#26703,.T.) ;
#38870 = EDGE_CURVE('',#31754,#31746,#4966,.T.) ;
#38871 = EDGE_CURVE('',#31955,#31755,#9765,.T.) ;
#38872 = EDGE_CURVE('',#31749,#31955,#26704,.T.) ;
#38873 = EDGE_CURVE('',#31803,#31807,#26705,.T.) ;
#38874 = EDGE_CURVE('',#31803,#31811,#26706,.T.) ;
#38875 = EDGE_CURVE('',#31811,#31807,#26707,.T.) ;
#38876 = EDGE_CURVE('',#31806,#31723,#26708,.T.) ;
#38877 = EDGE_CURVE('',#31812,#31806,#26709,.T.) ;
#38878 = EDGE_CURVE('',#31804,#31810,#26710,.T.) ;
#38879 = EDGE_CURVE('',#31635,#31801,#26711,.T.) ;
#38880 = EDGE_CURVE('',#31606,#31636,#26712,.T.) ;
#38881 = EDGE_CURVE('',#31609,#31635,#26713,.T.) ;
#38882 = EDGE_CURVE('',#31812,#31724,#26714,.T.) ;
#38883 = EDGE_CURVE('',#31804,#31808,#26715,.T.) ;
#38884 = EDGE_CURVE('',#31808,#31810,#26716,.T.) ;
#38885 = EDGE_CURVE('',#31609,#31802,#26717,.T.) ;
#38886 = EDGE_CURVE('',#31813,#31742,#26718,.T.) ;
#38887 = EDGE_CURVE('',#31809,#31813,#26719,.T.) ;
#38888 = EDGE_CURVE('',#31805,#31604,#26720,.T.) ;
#38889 = EDGE_CURVE('',#31603,#31805,#26721,.T.) ;
#38890 = EDGE_CURVE('',#31641,#31605,#26722,.T.) ;
#38891 = EDGE_CURVE('',#31642,#31612,#26723,.T.) ;
#38892 = EDGE_CURVE('',#31824,#31642,#26724,.T.) ;
#38893 = EDGE_CURVE('',#31820,#31823,#26725,.T.) ;
#38894 = EDGE_CURVE('',#31809,#31741,#26726,.T.) ;
#38895 = EDGE_CURVE('',#31825,#31612,#26727,.T.) ;
#38896 = EDGE_CURVE('',#31820,#31814,#26728,.T.) ;
#38897 = EDGE_CURVE('',#31814,#31823,#26729,.T.) ;
#38898 = EDGE_CURVE('',#31602,#31740,#273,.T.) ;
#38899 = EDGE_CURVE('',#31826,#31600,#26730,.T.) ;
#38900 = EDGE_CURVE('',#31822,#31819,#26731,.T.) ;
#38901 = EDGE_CURVE('',#31598,#31826,#26732,.T.) ;
#38902 = EDGE_CURVE('',#31815,#31822,#26733,.T.) ;
#38903 = EDGE_CURVE('',#31821,#31817,#26734,.T.) ;
#38904 = EDGE_CURVE('',#31735,#31821,#26735,.T.) ;
#38905 = EDGE_CURVE('',#31610,#31740,#26736,.T.) ;
#38906 = EDGE_CURVE('',#31956,#31599,#26737,.T.) ;
#38907 = EDGE_CURVE('',#31815,#31819,#26738,.T.) ;
#38908 = EDGE_CURVE('',#31736,#31817,#26739,.T.) ;
#38909 = EDGE_CURVE('',#31611,#31739,#26740,.T.) ;
#38910 = EDGE_CURVE('',#31816,#31818,#26741,.T.) ;
#38911 = EDGE_CURVE('',#31737,#31816,#26742,.T.) ;
#38912 = EDGE_CURVE('',#31596,#31739,#274,.T.) ;
#38913 = EDGE_CURVE('',#31738,#31818,#26743,.T.) ;
#38914 = EDGE_CURVE('',#31615,#31896,#275,.T.) ;
#38915 = EDGE_CURVE('',#31899,#31895,#26744,.T.) ;
#38916 = EDGE_CURVE('',#31894,#31900,#26745,.T.) ;
#38917 = EDGE_CURVE('',#31897,#31780,#276,.T.) ;
#38918 = EDGE_CURVE('',#31892,#31917,#26746,.T.) ;
#38919 = EDGE_CURVE('',#31904,#31931,#26747,.T.) ;
#38920 = EDGE_CURVE('',#31905,#31930,#26748,.T.) ;
#38921 = EDGE_CURVE('',#31891,#31618,#277,.T.) ;
#38922 = EDGE_CURVE('',#31886,#31898,#26749,.T.) ;
#38923 = EDGE_CURVE('',#31916,#31893,#26750,.T.) ;
#38924 = EDGE_CURVE('',#31905,#31909,#26751,.T.) ;
#38925 = EDGE_CURVE('',#31909,#31930,#26752,.T.) ;
#38926 = EDGE_CURVE('',#31901,#31887,#26753,.T.) ;
#38927 = EDGE_CURVE('',#31932,#31911,#26754,.T.) ;
#38928 = EDGE_CURVE('',#31933,#31910,#26755,.T.) ;
#38929 = EDGE_CURVE('',#31906,#31933,#26756,.T.) ;
#38930 = EDGE_CURVE('',#31902,#31908,#26757,.T.) ;
#38931 = EDGE_CURVE('',#31928,#31903,#26758,.T.) ;
#38932 = EDGE_CURVE('',#31929,#31902,#26759,.T.) ;
#38933 = EDGE_CURVE('',#31906,#31910,#26760,.T.) ;
#38934 = EDGE_CURVE('',#31929,#31908,#26761,.T.) ;
#38935 = EDGE_CURVE('',#31907,#31913,#26762,.T.) ;
#38936 = EDGE_CURVE('',#31926,#31907,#26763,.T.) ;
#38937 = EDGE_CURVE('',#31926,#31913,#26764,.T.) ;
#38938 = EDGE_CURVE('',#31912,#31927,#26765,.T.) ;
#38939 = EDGE_CURVE('',#31888,#31915,#26766,.T.) ;
#38940 = EDGE_CURVE('',#31889,#31914,#26767,.T.) ;
#38941 = EDGE_CURVE('',#31783,#31890,#278,.T.) ;
#38942 = EDGE_CURVE('',#31881,#31882,#26768,.T.) ;
#38943 = EDGE_CURVE('',#31885,#31880,#26769,.T.) ;
#38944 = EDGE_CURVE('',#31868,#31919,#26770,.T.) ;
#38945 = EDGE_CURVE('',#31869,#31918,#26771,.T.) ;
#38946 = EDGE_CURVE('',#31920,#31875,#26772,.T.) ;
#38947 = EDGE_CURVE('',#31921,#31874,#26773,.T.) ;
#38948 = EDGE_CURVE('',#31918,#31873,#26774,.T.) ;
#38949 = EDGE_CURVE('',#31870,#31921,#26775,.T.) ;
#38950 = EDGE_CURVE('',#31869,#31873,#26776,.T.) ;
#38951 = EDGE_CURVE('',#31883,#31878,#26777,.T.) ;
#38952 = EDGE_CURVE('',#31879,#31884,#26778,.T.) ;
#38953 = EDGE_CURVE('',#31870,#31874,#26779,.T.) ;
#38954 = EDGE_CURVE('',#31866,#31872,#26780,.T.) ;
#38955 = EDGE_CURVE('',#31924,#31867,#26781,.T.) ;
#38956 = EDGE_CURVE('',#31925,#31866,#26782,.T.) ;
#38957 = EDGE_CURVE('',#31876,#31923,#26783,.T.) ;
#38958 = EDGE_CURVE('',#31877,#31922,#26784,.T.) ;
#38959 = EDGE_CURVE('',#31871,#31877,#26785,.T.) ;
#38960 = EDGE_CURVE('',#31925,#31872,#26786,.T.) ;
#38961 = EDGE_CURVE('',#31871,#31922,#26787,.T.) ;
#38962 = EDGE_CURVE('',#31629,#31628,#26788,.T.) ;
#38963 = EDGE_CURVE('',#31855,#31630,#279,.T.) ;
#38964 = EDGE_CURVE('',#31856,#31629,#26789,.T.) ;
#38965 = EDGE_CURVE('',#31856,#31628,#26790,.T.) ;
#38966 = EDGE_CURVE('',#31627,#31624,#26791,.T.) ;
#38967 = EDGE_CURVE('',#31853,#31627,#26792,.T.) ;
#38968 = EDGE_CURVE('',#31853,#31624,#26793,.T.) ;
#38969 = EDGE_CURVE('',#31623,#31854,#280,.T.) ;
#38970 = EDGE_CURVE('',#31585,#31864,#4967,.T.) ;
#38971 = EDGE_CURVE('',#31712,#31863,#26794,.T.) ;
#38972 = EDGE_CURVE('',#31709,#31712,#26795,.T.) ;
#38973 = EDGE_CURVE('',#31709,#31863,#26796,.T.) ;
#38974 = EDGE_CURVE('',#31710,#31865,#26797,.T.) ;
#38975 = EDGE_CURVE('',#31708,#31710,#26798,.T.) ;
#38976 = EDGE_CURVE('',#31708,#31865,#26799,.T.) ;
#38977 = EDGE_CURVE('',#31589,#31705,#4968,.T.) ;
#38978 = EDGE_CURVE('',#31777,#31614,#26800,.T.) ;
#38979 = EDGE_CURVE('',#31613,#31778,#26801,.T.) ;
#38980 = EDGE_CURVE('',#31939,#31647,#26802,.T.) ;
#38981 = EDGE_CURVE('',#31936,#31648,#26803,.T.) ;
#38982 = EDGE_CURVE('',#31647,#31937,#26804,.T.) ;
#38983 = EDGE_CURVE('',#31648,#31934,#26805,.T.) ;
#38984 = EDGE_CURVE('',#31771,#31781,#26806,.T.) ;
#38985 = EDGE_CURVE('',#31772,#31614,#26807,.T.) ;
#38986 = EDGE_CURVE('',#31772,#31777,#26808,.T.) ;
#38987 = EDGE_CURVE('',#31773,#31776,#26809,.T.) ;
#38988 = EDGE_CURVE('',#31768,#31775,#26810,.T.) ;
#38989 = EDGE_CURVE('',#31769,#31778,#26811,.T.) ;
#38990 = EDGE_CURVE('',#31769,#31613,#26812,.T.) ;
#38991 = EDGE_CURVE('',#31770,#31782,#26813,.T.) ;
#38992 = EDGE_CURVE('',#31622,#31858,#281,.T.) ;
#38993 = EDGE_CURVE('',#31854,#31857,#26814,.T.) ;
#38994 = EDGE_CURVE('',#31855,#31862,#26815,.T.) ;
#38995 = EDGE_CURVE('',#31957,#31861,#282,.T.) ;
#38996 = EDGE_CURVE('',#31958,#31957,#283,.T.) ;
#38997 = EDGE_CURVE('',#31959,#31958,#284,.T.) ;
#38998 = EDGE_CURVE('',#31631,#31959,#285,.T.) ;
#38999 = EDGE_CURVE('',#31713,#31632,#4969,.T.) ;
#39000 = EDGE_CURVE('',#31714,#31861,#26816,.T.) ;
#39001 = EDGE_CURVE('',#31588,#31706,#286,.T.) ;
#39002 = EDGE_CURVE('',#31715,#31860,#26817,.T.) ;
#39003 = EDGE_CURVE('',#31711,#31716,#4970,.T.) ;
#39004 = EDGE_CURVE('',#31859,#31864,#26818,.T.) ;
#39005 = EDGE_CURVE('',#31960,#31860,#287,.T.) ;
#39006 = EDGE_CURVE('',#31961,#31960,#288,.T.) ;
#39007 = EDGE_CURVE('',#31584,#31961,#289,.T.) ;
#39008 = EDGE_CURVE('',#31641,#31935,#26819,.T.) ;
#39009 = EDGE_CURVE('',#31607,#31935,#26820,.T.) ;
#39010 = EDGE_CURVE('',#31936,#31934,#26821,.T.) ;
#39011 = EDGE_CURVE('',#31904,#31900,#26822,.T.) ;
#39012 = EDGE_CURVE('',#31931,#31894,#26823,.T.) ;
#39013 = EDGE_CURVE('',#31901,#31903,#26824,.T.) ;
#39014 = EDGE_CURVE('',#31932,#31893,#26825,.T.) ;
#39015 = EDGE_CURVE('',#31887,#31928,#26826,.T.) ;
#39016 = EDGE_CURVE('',#31911,#31916,#26827,.T.) ;
#39017 = EDGE_CURVE('',#31888,#31927,#26828,.T.) ;
#39018 = EDGE_CURVE('',#31912,#31915,#26829,.T.) ;
#39019 = EDGE_CURVE('',#31868,#31882,#26830,.T.) ;
#39020 = EDGE_CURVE('',#31919,#31881,#26831,.T.) ;
#39021 = EDGE_CURVE('',#31883,#31867,#26832,.T.) ;
#39022 = EDGE_CURVE('',#31920,#31880,#26833,.T.) ;
#39023 = EDGE_CURVE('',#31878,#31924,#26834,.T.) ;
#39024 = EDGE_CURVE('',#31875,#31885,#26835,.T.) ;
#39025 = EDGE_CURVE('',#31879,#31923,#26836,.T.) ;
#39026 = EDGE_CURVE('',#31876,#31884,#26837,.T.) ;
#39027 = EDGE_CURVE('',#31938,#31636,#26838,.T.) ;
#39028 = EDGE_CURVE('',#31938,#31608,#26839,.T.) ;
#39029 = EDGE_CURVE('',#31939,#31937,#26840,.T.) ;
#39030 = EDGE_CURVE('',#31703,#31707,#4971,.T.) ;
#39031 = EDGE_CURVE('',#31704,#31587,#26841,.T.) ;
#39032 = EDGE_CURVE('',#31701,#31858,#26842,.T.) ;
#39033 = EDGE_CURVE('',#31702,#31621,#4972,.T.) ;
#39034 = EDGE_CURVE('',#31962,#31962,#26843,.T.) ;
#39035 = EDGE_CURVE('',#31962,#31963,#9766,.T.) ;
#39036 = EDGE_CURVE('',#31963,#31964,#26844,.T.) ;
#39037 = EDGE_CURVE('',#31964,#31963,#26845,.T.) ;
#39038 = EDGE_CURVE('',#31965,#31966,#26846,.T.) ;
#39039 = EDGE_CURVE('',#31965,#31967,#9767,.T.) ;
#39040 = EDGE_CURVE('',#31967,#31968,#26847,.T.) ;
#39041 = EDGE_CURVE('',#31966,#31968,#9768,.T.) ;
#39042 = EDGE_CURVE('',#31969,#31970,#26848,.T.) ;
#39043 = EDGE_CURVE('',#31971,#31970,#9769,.T.) ;
#39044 = EDGE_CURVE('',#31972,#31971,#9770,.T.) ;
#39045 = EDGE_CURVE('',#31972,#31973,#26849,.T.) ;
#39046 = EDGE_CURVE('',#31973,#31974,#9771,.T.) ;
#39047 = EDGE_CURVE('',#31975,#31974,#9772,.T.) ;
#39048 = EDGE_CURVE('',#31975,#31969,#9773,.T.) ;
#39049 = EDGE_CURVE('',#31976,#31977,#9774,.T.) ;
#39050 = EDGE_CURVE('',#31976,#31978,#9775,.T.) ;
#39051 = EDGE_CURVE('',#31978,#31979,#26850,.T.) ;
#39052 = EDGE_CURVE('',#31980,#31979,#9776,.T.) ;
#39053 = EDGE_CURVE('',#31981,#31980,#9777,.T.) ;
#39054 = EDGE_CURVE('',#31982,#31981,#9778,.T.) ;
#39055 = EDGE_CURVE('',#31982,#31977,#26851,.T.) ;
#39056 = EDGE_CURVE('',#31973,#31982,#9779,.T.) ;
#39057 = EDGE_CURVE('',#31974,#31981,#9780,.T.) ;
#39058 = EDGE_CURVE('',#31983,#31984,#9781,.T.) ;
#39059 = EDGE_CURVE('',#31985,#31983,#9782,.T.) ;
#39060 = EDGE_CURVE('',#31985,#31986,#26852,.T.) ;
#39061 = EDGE_CURVE('',#31987,#31986,#9783,.T.) ;
#39062 = EDGE_CURVE('',#31988,#31987,#9784,.T.) ;
#39063 = EDGE_CURVE('',#31989,#31988,#9785,.T.) ;
#39064 = EDGE_CURVE('',#31989,#31984,#26853,.T.) ;
#39065 = EDGE_CURVE('',#31990,#31991,#9786,.T.) ;
#39066 = EDGE_CURVE('',#31990,#31989,#9787,.T.) ;
#39067 = EDGE_CURVE('',#31991,#31988,#9788,.T.) ;
#39068 = EDGE_CURVE('',#31992,#31993,#26854,.T.) ;
#39069 = EDGE_CURVE('',#31993,#31994,#9789,.T.) ;
#39070 = EDGE_CURVE('',#31995,#31994,#9790,.T.) ;
#39071 = EDGE_CURVE('',#31995,#31990,#26855,.T.) ;
#39072 = EDGE_CURVE('',#31996,#31991,#9791,.T.) ;
#39073 = EDGE_CURVE('',#31996,#31992,#9792,.T.) ;
#39074 = EDGE_CURVE('',#31979,#31969,#9793,.T.) ;
#39075 = EDGE_CURVE('',#31980,#31975,#9794,.T.) ;
#39076 = EDGE_CURVE('',#31986,#31992,#9795,.T.) ;
#39077 = EDGE_CURVE('',#31987,#31996,#9796,.T.) ;
#39078 = EDGE_CURVE('',#31977,#31972,#9797,.T.) ;
#39079 = EDGE_CURVE('',#31984,#31995,#9798,.T.) ;
#39080 = EDGE_CURVE('',#31970,#31978,#9799,.T.) ;
#39081 = EDGE_CURVE('',#31993,#31985,#9800,.T.) ;
#39082 = EDGE_CURVE('',#31968,#31967,#9801,.T.) ;
#39083 = EDGE_CURVE('',#31976,#31971,#9802,.T.) ;
#39084 = EDGE_CURVE('',#31994,#31983,#9803,.T.) ;
#39085 = EDGE_CURVE('',#31962,#31965,#9804,.T.) ;
#39086 = EDGE_CURVE('',#31966,#31962,#9805,.T.) ;
#39087 = EDGE_CURVE('',#31997,#31964,#26856,.T.) ;
#39088 = EDGE_CURVE('',#31998,#31998,#26857,.T.) ;
#39089 = EDGE_CURVE('',#31998,#31999,#26858,.T.) ;
#39090 = EDGE_CURVE('',#32000,#31999,#26859,.T.) ;
#39091 = EDGE_CURVE('',#31999,#32000,#26860,.T.) ;
#39092 = EDGE_CURVE('',#32001,#32001,#26861,.T.) ;
#39093 = EDGE_CURVE('',#32001,#32002,#26862,.T.) ;
#39094 = EDGE_CURVE('',#32002,#32002,#26863,.T.) ;
#39095 = EDGE_CURVE('',#32003,#32004,#26864,.T.) ;
#39096 = EDGE_CURVE('',#32005,#32003,#26865,.T.) ;
#39097 = EDGE_CURVE('',#32005,#32004,#26866,.T.) ;
#39098 = EDGE_CURVE('',#32006,#32007,#4973,.T.) ;
#39099 = EDGE_CURVE('',#32006,#32008,#26867,.T.) ;
#39100 = EDGE_CURVE('',#32009,#32008,#9806,.T.) ;
#39101 = EDGE_CURVE('',#32010,#32009,#26868,.T.) ;
#39102 = EDGE_CURVE('',#32011,#32010,#9807,.T.) ;
#39103 = EDGE_CURVE('',#32012,#32011,#9808,.T.) ;
#39104 = EDGE_CURVE('',#32012,#32007,#290,.T.) ;
#39105 = EDGE_CURVE('',#32013,#32013,#26869,.T.) ;
#39106 = EDGE_CURVE('',#32013,#32014,#26870,.T.) ;
#39107 = EDGE_CURVE('',#32015,#32014,#26871,.T.) ;
#39108 = EDGE_CURVE('',#32014,#32015,#26872,.T.) ;
#39109 = EDGE_CURVE('',#32016,#32016,#26873,.T.) ;
#39110 = EDGE_CURVE('',#32016,#32017,#26874,.T.) ;
#39111 = EDGE_CURVE('',#32017,#32017,#26875,.T.) ;
#39112 = EDGE_CURVE('',#32018,#32019,#26876,.T.) ;
#39113 = EDGE_CURVE('',#32020,#32018,#26877,.T.) ;
#39114 = EDGE_CURVE('',#32020,#32019,#26878,.T.) ;
#39115 = EDGE_CURVE('',#32021,#32022,#4974,.T.) ;
#39116 = EDGE_CURVE('',#32021,#32023,#26879,.T.) ;
#39117 = EDGE_CURVE('',#32024,#32023,#9809,.T.) ;
#39118 = EDGE_CURVE('',#32025,#32024,#26880,.T.) ;
#39119 = EDGE_CURVE('',#32026,#32025,#9810,.T.) ;
#39120 = EDGE_CURVE('',#32027,#32026,#9811,.T.) ;
#39121 = EDGE_CURVE('',#32027,#32022,#291,.T.) ;
#39122 = EDGE_CURVE('',#32028,#32028,#26881,.T.) ;
#39123 = EDGE_CURVE('',#32028,#32029,#26882,.T.) ;
#39124 = EDGE_CURVE('',#32030,#32029,#26883,.T.) ;
#39125 = EDGE_CURVE('',#32029,#32030,#26884,.T.) ;
#39126 = EDGE_CURVE('',#32031,#32031,#26885,.T.) ;
#39127 = EDGE_CURVE('',#32031,#32032,#26886,.T.) ;
#39128 = EDGE_CURVE('',#32032,#32032,#26887,.T.) ;
#39129 = EDGE_CURVE('',#32033,#32034,#26888,.T.) ;
#39130 = EDGE_CURVE('',#32035,#32033,#26889,.T.) ;
#39131 = EDGE_CURVE('',#32035,#32034,#26890,.T.) ;
#39132 = EDGE_CURVE('',#32036,#32037,#4975,.T.) ;
#39133 = EDGE_CURVE('',#32036,#32038,#26891,.T.) ;
#39134 = EDGE_CURVE('',#32039,#32038,#9812,.T.) ;
#39135 = EDGE_CURVE('',#32040,#32039,#26892,.T.) ;
#39136 = EDGE_CURVE('',#32041,#32040,#9813,.T.) ;
#39137 = EDGE_CURVE('',#32042,#32041,#9814,.T.) ;
#39138 = EDGE_CURVE('',#32042,#32037,#292,.T.) ;
#39139 = EDGE_CURVE('',#32043,#32043,#26893,.T.) ;
#39140 = EDGE_CURVE('',#32043,#32044,#26894,.T.) ;
#39141 = EDGE_CURVE('',#32045,#32044,#26895,.T.) ;
#39142 = EDGE_CURVE('',#32044,#32045,#26896,.T.) ;
#39143 = EDGE_CURVE('',#32046,#32046,#26897,.T.) ;
#39144 = EDGE_CURVE('',#32046,#32047,#26898,.T.) ;
#39145 = EDGE_CURVE('',#32047,#32047,#26899,.T.) ;
#39146 = EDGE_CURVE('',#32048,#32049,#26900,.T.) ;
#39147 = EDGE_CURVE('',#32050,#32048,#26901,.T.) ;
#39148 = EDGE_CURVE('',#32050,#32049,#26902,.T.) ;
#39149 = EDGE_CURVE('',#32051,#32052,#4976,.T.) ;
#39150 = EDGE_CURVE('',#32051,#32053,#26903,.T.) ;
#39151 = EDGE_CURVE('',#32054,#32053,#9815,.T.) ;
#39152 = EDGE_CURVE('',#32055,#32054,#26904,.T.) ;
#39153 = EDGE_CURVE('',#32056,#32055,#9816,.T.) ;
#39154 = EDGE_CURVE('',#32057,#32056,#9817,.T.) ;
#39155 = EDGE_CURVE('',#32057,#32052,#293,.T.) ;
#39156 = EDGE_CURVE('',#32058,#32058,#26905,.T.) ;
#39157 = EDGE_CURVE('',#32058,#32059,#26906,.T.) ;
#39158 = EDGE_CURVE('',#32060,#32059,#26907,.T.) ;
#39159 = EDGE_CURVE('',#32059,#32060,#26908,.T.) ;
#39160 = EDGE_CURVE('',#32061,#32061,#26909,.T.) ;
#39161 = EDGE_CURVE('',#32061,#32062,#26910,.T.) ;
#39162 = EDGE_CURVE('',#32062,#32062,#26911,.T.) ;
#39163 = EDGE_CURVE('',#32063,#32064,#26912,.T.) ;
#39164 = EDGE_CURVE('',#32065,#32063,#26913,.T.) ;
#39165 = EDGE_CURVE('',#32065,#32064,#26914,.T.) ;
#39166 = EDGE_CURVE('',#32066,#32067,#4977,.T.) ;
#39167 = EDGE_CURVE('',#32066,#32068,#26915,.T.) ;
#39168 = EDGE_CURVE('',#32069,#32068,#9818,.T.) ;
#39169 = EDGE_CURVE('',#32070,#32069,#26916,.T.) ;
#39170 = EDGE_CURVE('',#32071,#32070,#9819,.T.) ;
#39171 = EDGE_CURVE('',#32072,#32071,#9820,.T.) ;
#39172 = EDGE_CURVE('',#32072,#32067,#294,.T.) ;
#39173 = EDGE_CURVE('',#32073,#32073,#26917,.T.) ;
#39174 = EDGE_CURVE('',#32073,#32074,#26918,.T.) ;
#39175 = EDGE_CURVE('',#32075,#32074,#26919,.T.) ;
#39176 = EDGE_CURVE('',#32074,#32075,#26920,.T.) ;
#39177 = EDGE_CURVE('',#32076,#32076,#26921,.T.) ;
#39178 = EDGE_CURVE('',#32076,#32077,#26922,.T.) ;
#39179 = EDGE_CURVE('',#32077,#32077,#26923,.T.) ;
#39180 = EDGE_CURVE('',#32078,#32079,#26924,.T.) ;
#39181 = EDGE_CURVE('',#32080,#32078,#26925,.T.) ;
#39182 = EDGE_CURVE('',#32080,#32079,#26926,.T.) ;
#39183 = EDGE_CURVE('',#32081,#32082,#4978,.T.) ;
#39184 = EDGE_CURVE('',#32081,#32083,#26927,.T.) ;
#39185 = EDGE_CURVE('',#32084,#32083,#9821,.T.) ;
#39186 = EDGE_CURVE('',#32085,#32084,#26928,.T.) ;
#39187 = EDGE_CURVE('',#32086,#32085,#9822,.T.) ;
#39188 = EDGE_CURVE('',#32087,#32086,#9823,.T.) ;
#39189 = EDGE_CURVE('',#32087,#32082,#295,.T.) ;
#39190 = EDGE_CURVE('',#32088,#32088,#26929,.T.) ;
#39191 = EDGE_CURVE('',#32088,#32089,#26930,.T.) ;
#39192 = EDGE_CURVE('',#32090,#32089,#26931,.T.) ;
#39193 = EDGE_CURVE('',#32089,#32090,#26932,.T.) ;
#39194 = EDGE_CURVE('',#32091,#32091,#26933,.T.) ;
#39195 = EDGE_CURVE('',#32091,#32092,#26934,.T.) ;
#39196 = EDGE_CURVE('',#32092,#32092,#26935,.T.) ;
#39197 = EDGE_CURVE('',#32093,#32094,#26936,.T.) ;
#39198 = EDGE_CURVE('',#32095,#32093,#26937,.T.) ;
#39199 = EDGE_CURVE('',#32095,#32094,#26938,.T.) ;
#39200 = EDGE_CURVE('',#32096,#32097,#4979,.T.) ;
#39201 = EDGE_CURVE('',#32096,#32098,#26939,.T.) ;
#39202 = EDGE_CURVE('',#32099,#32098,#9824,.T.) ;
#39203 = EDGE_CURVE('',#32100,#32099,#26940,.T.) ;
#39204 = EDGE_CURVE('',#32101,#32100,#9825,.T.) ;
#39205 = EDGE_CURVE('',#32102,#32101,#9826,.T.) ;
#39206 = EDGE_CURVE('',#32102,#32097,#296,.T.) ;
#39207 = EDGE_CURVE('',#32103,#32103,#26941,.T.) ;
#39208 = EDGE_CURVE('',#32103,#32104,#26942,.T.) ;
#39209 = EDGE_CURVE('',#32105,#32104,#26943,.T.) ;
#39210 = EDGE_CURVE('',#32104,#32105,#26944,.T.) ;
#39211 = EDGE_CURVE('',#32106,#32106,#26945,.T.) ;
#39212 = EDGE_CURVE('',#32106,#32107,#26946,.T.) ;
#39213 = EDGE_CURVE('',#32107,#32107,#26947,.T.) ;
#39214 = EDGE_CURVE('',#32108,#32109,#26948,.T.) ;
#39215 = EDGE_CURVE('',#32110,#32108,#26949,.T.) ;
#39216 = EDGE_CURVE('',#32110,#32109,#26950,.T.) ;
#39217 = EDGE_CURVE('',#32111,#32112,#4980,.T.) ;
#39218 = EDGE_CURVE('',#32111,#32113,#26951,.T.) ;
#39219 = EDGE_CURVE('',#32114,#32113,#9827,.T.) ;
#39220 = EDGE_CURVE('',#32115,#32114,#26952,.T.) ;
#39221 = EDGE_CURVE('',#32116,#32115,#9828,.T.) ;
#39222 = EDGE_CURVE('',#32117,#32116,#9829,.T.) ;
#39223 = EDGE_CURVE('',#32117,#32112,#297,.T.) ;
#39224 = EDGE_CURVE('',#32118,#32118,#26953,.T.) ;
#39225 = EDGE_CURVE('',#32118,#32119,#26954,.T.) ;
#39226 = EDGE_CURVE('',#32120,#32119,#26955,.T.) ;
#39227 = EDGE_CURVE('',#32119,#32120,#26956,.T.) ;
#39228 = EDGE_CURVE('',#32121,#32122,#26957,.T.) ;
#39229 = EDGE_CURVE('',#32123,#32121,#26958,.T.) ;
#39230 = EDGE_CURVE('',#32124,#32123,#26959,.T.) ;
#39231 = EDGE_CURVE('',#32124,#32122,#26960,.T.) ;
#39232 = EDGE_CURVE('',#32125,#32126,#26961,.T.) ;
#39233 = EDGE_CURVE('',#32127,#32125,#26962,.T.) ;
#39234 = EDGE_CURVE('',#32128,#32127,#26963,.T.) ;
#39235 = EDGE_CURVE('',#32128,#32126,#26964,.T.) ;
#39236 = EDGE_CURVE('',#32129,#32130,#26965,.T.) ;
#39237 = EDGE_CURVE('',#32131,#32129,#26966,.T.) ;
#39238 = EDGE_CURVE('',#32132,#32131,#26967,.T.) ;
#39239 = EDGE_CURVE('',#32132,#32130,#26968,.T.) ;
#39240 = EDGE_CURVE('',#32133,#32134,#26969,.T.) ;
#39241 = EDGE_CURVE('',#32135,#32133,#26970,.T.) ;
#39242 = EDGE_CURVE('',#32136,#32135,#26971,.T.) ;
#39243 = EDGE_CURVE('',#32136,#32134,#26972,.T.) ;
#39244 = EDGE_CURVE('',#32137,#32138,#26973,.T.) ;
#39245 = EDGE_CURVE('',#32139,#32137,#26974,.T.) ;
#39246 = EDGE_CURVE('',#32140,#32139,#26975,.T.) ;
#39247 = EDGE_CURVE('',#32140,#32138,#26976,.T.) ;
#39248 = EDGE_CURVE('',#32141,#32142,#26977,.T.) ;
#39249 = EDGE_CURVE('',#32143,#32141,#26978,.T.) ;
#39250 = EDGE_CURVE('',#32144,#32143,#26979,.T.) ;
#39251 = EDGE_CURVE('',#32144,#32142,#26980,.T.) ;
#39252 = EDGE_CURVE('',#32145,#32146,#26981,.T.) ;
#39253 = EDGE_CURVE('',#32147,#32145,#26982,.T.) ;
#39254 = EDGE_CURVE('',#32148,#32147,#26983,.T.) ;
#39255 = EDGE_CURVE('',#32148,#32146,#26984,.T.) ;
#39256 = EDGE_CURVE('',#32149,#32150,#26985,.T.) ;
#39257 = EDGE_CURVE('',#32151,#32149,#26986,.T.) ;
#39258 = EDGE_CURVE('',#32152,#32151,#26987,.T.) ;
#39259 = EDGE_CURVE('',#32152,#32150,#26988,.T.) ;
#39260 = EDGE_CURVE('',#32153,#32154,#26989,.T.) ;
#39261 = EDGE_CURVE('',#32155,#32153,#26990,.T.) ;
#39262 = EDGE_CURVE('',#32156,#32155,#26991,.T.) ;
#39263 = EDGE_CURVE('',#32156,#32154,#26992,.T.) ;
#39264 = EDGE_CURVE('',#32157,#32157,#26993,.T.) ;
#39265 = EDGE_CURVE('',#32157,#32158,#26994,.T.) ;
#39266 = EDGE_CURVE('',#32158,#32158,#26995,.T.) ;
#39267 = EDGE_CURVE('',#32159,#32160,#26996,.T.) ;
#39268 = EDGE_CURVE('',#32161,#32159,#26997,.T.) ;
#39269 = EDGE_CURVE('',#32161,#32160,#26998,.T.) ;
#39270 = EDGE_CURVE('',#32162,#32163,#4981,.T.) ;
#39271 = EDGE_CURVE('',#32162,#32164,#26999,.T.) ;
#39272 = EDGE_CURVE('',#32165,#32164,#9830,.T.) ;
#39273 = EDGE_CURVE('',#32166,#32165,#27000,.T.) ;
#39274 = EDGE_CURVE('',#32167,#32166,#9831,.T.) ;
#39275 = EDGE_CURVE('',#32168,#32167,#9832,.T.) ;
#39276 = EDGE_CURVE('',#32168,#32163,#298,.T.) ;
#39277 = EDGE_CURVE('',#32002,#32000,#9833,.T.) ;
#39278 = EDGE_CURVE('',#32017,#32015,#9834,.T.) ;
#39279 = EDGE_CURVE('',#32032,#32030,#9835,.T.) ;
#39280 = EDGE_CURVE('',#32047,#32045,#9836,.T.) ;
#39281 = EDGE_CURVE('',#32062,#32060,#9837,.T.) ;
#39282 = EDGE_CURVE('',#32077,#32075,#9838,.T.) ;
#39283 = EDGE_CURVE('',#32092,#32090,#9839,.T.) ;
#39284 = EDGE_CURVE('',#32107,#32105,#9840,.T.) ;
#39285 = EDGE_CURVE('',#32158,#32120,#9841,.T.) ;
#39286 = EDGE_CURVE('',#32169,#32170,#27001,.T.) ;
#39287 = EDGE_CURVE('',#32170,#32124,#9842,.T.) ;
#39288 = EDGE_CURVE('',#32169,#32123,#9843,.T.) ;
#39289 = EDGE_CURVE('',#32171,#32172,#27002,.T.) ;
#39290 = EDGE_CURVE('',#32172,#32128,#9844,.T.) ;
#39291 = EDGE_CURVE('',#32171,#32127,#9845,.T.) ;
#39292 = EDGE_CURVE('',#32173,#32174,#27003,.T.) ;
#39293 = EDGE_CURVE('',#32174,#32132,#9846,.T.) ;
#39294 = EDGE_CURVE('',#32173,#32131,#9847,.T.) ;
#39295 = EDGE_CURVE('',#32175,#32176,#27004,.T.) ;
#39296 = EDGE_CURVE('',#32176,#32136,#9848,.T.) ;
#39297 = EDGE_CURVE('',#32175,#32135,#9849,.T.) ;
#39298 = EDGE_CURVE('',#32177,#32178,#27005,.T.) ;
#39299 = EDGE_CURVE('',#32178,#32140,#9850,.T.) ;
#39300 = EDGE_CURVE('',#32177,#32139,#9851,.T.) ;
#39301 = EDGE_CURVE('',#32179,#32180,#27006,.T.) ;
#39302 = EDGE_CURVE('',#32180,#32144,#9852,.T.) ;
#39303 = EDGE_CURVE('',#32179,#32143,#9853,.T.) ;
#39304 = EDGE_CURVE('',#32181,#32182,#27007,.T.) ;
#39305 = EDGE_CURVE('',#32182,#32148,#9854,.T.) ;
#39306 = EDGE_CURVE('',#32181,#32147,#9855,.T.) ;
#39307 = EDGE_CURVE('',#32183,#32184,#27008,.T.) ;
#39308 = EDGE_CURVE('',#32184,#32152,#9856,.T.) ;
#39309 = EDGE_CURVE('',#32183,#32151,#9857,.T.) ;
#39310 = EDGE_CURVE('',#32185,#32186,#27009,.T.) ;
#39311 = EDGE_CURVE('',#32186,#32156,#9858,.T.) ;
#39312 = EDGE_CURVE('',#32185,#32155,#9859,.T.) ;
#39313 = EDGE_CURVE('',#32187,#32187,#27010,.T.) ;
#39314 = EDGE_CURVE('',#32187,#32188,#27011,.T.) ;
#39315 = EDGE_CURVE('',#32189,#32188,#27012,.T.) ;
#39316 = EDGE_CURVE('',#32188,#32189,#27013,.T.) ;
#39317 = EDGE_CURVE('',#32190,#32191,#27014,.T.) ;
#39318 = EDGE_CURVE('',#32192,#32190,#27015,.T.) ;
#39319 = EDGE_CURVE('',#32193,#32192,#27016,.T.) ;
#39320 = EDGE_CURVE('',#32193,#32191,#27017,.T.) ;
#39321 = EDGE_CURVE('',#32194,#32194,#27018,.T.) ;
#39322 = EDGE_CURVE('',#32194,#32195,#27019,.T.) ;
#39323 = EDGE_CURVE('',#32195,#32195,#27020,.T.) ;
#39324 = EDGE_CURVE('',#32196,#32197,#27021,.T.) ;
#39325 = EDGE_CURVE('',#32198,#32196,#27022,.T.) ;
#39326 = EDGE_CURVE('',#32198,#32197,#27023,.T.) ;
#39327 = EDGE_CURVE('',#32199,#32200,#4982,.T.) ;
#39328 = EDGE_CURVE('',#32199,#32201,#27024,.T.) ;
#39329 = EDGE_CURVE('',#32202,#32201,#9860,.T.) ;
#39330 = EDGE_CURVE('',#32203,#32202,#27025,.T.) ;
#39331 = EDGE_CURVE('',#32204,#32203,#9861,.T.) ;
#39332 = EDGE_CURVE('',#32205,#32204,#9862,.T.) ;
#39333 = EDGE_CURVE('',#32205,#32200,#299,.T.) ;
#39334 = EDGE_CURVE('',#32195,#32189,#9863,.T.) ;
#39335 = EDGE_CURVE('',#32206,#32207,#27026,.T.) ;
#39336 = EDGE_CURVE('',#32207,#32193,#9864,.T.) ;
#39337 = EDGE_CURVE('',#32206,#32192,#9865,.T.) ;
#39338 = EDGE_CURVE('',#32208,#32209,#9866,.T.) ;
#39339 = EDGE_CURVE('',#32209,#32210,#27027,.T.) ;
#39340 = EDGE_CURVE('',#32210,#32211,#9867,.T.) ;
#39341 = EDGE_CURVE('',#32211,#32011,#27028,.T.) ;
#39342 = EDGE_CURVE('',#32212,#32010,#27029,.T.) ;
#39343 = EDGE_CURVE('',#32212,#32213,#9868,.T.) ;
#39344 = EDGE_CURVE('',#32213,#32214,#9869,.T.) ;
#39345 = EDGE_CURVE('',#32214,#32215,#9870,.T.) ;
#39346 = EDGE_CURVE('',#32215,#32216,#9871,.T.) ;
#39347 = EDGE_CURVE('',#32216,#32217,#9872,.T.) ;
#39348 = EDGE_CURVE('',#32208,#32217,#27030,.T.) ;
#39349 = EDGE_CURVE('',#32218,#32219,#9873,.T.) ;
#39350 = EDGE_CURVE('',#32219,#32220,#27031,.T.) ;
#39351 = EDGE_CURVE('',#32220,#32221,#9874,.T.) ;
#39352 = EDGE_CURVE('',#32221,#32026,#27032,.T.) ;
#39353 = EDGE_CURVE('',#32222,#32025,#27033,.T.) ;
#39354 = EDGE_CURVE('',#32222,#32223,#9875,.T.) ;
#39355 = EDGE_CURVE('',#32223,#32224,#9876,.T.) ;
#39356 = EDGE_CURVE('',#32224,#32225,#9877,.T.) ;
#39357 = EDGE_CURVE('',#32225,#32226,#9878,.T.) ;
#39358 = EDGE_CURVE('',#32226,#32227,#9879,.T.) ;
#39359 = EDGE_CURVE('',#32218,#32227,#27034,.T.) ;
#39360 = EDGE_CURVE('',#32228,#32229,#9880,.T.) ;
#39361 = EDGE_CURVE('',#32229,#32230,#27035,.T.) ;
#39362 = EDGE_CURVE('',#32230,#32231,#9881,.T.) ;
#39363 = EDGE_CURVE('',#32231,#32041,#27036,.T.) ;
#39364 = EDGE_CURVE('',#32232,#32040,#27037,.T.) ;
#39365 = EDGE_CURVE('',#32232,#32233,#9882,.T.) ;
#39366 = EDGE_CURVE('',#32233,#32234,#9883,.T.) ;
#39367 = EDGE_CURVE('',#32234,#32235,#9884,.T.) ;
#39368 = EDGE_CURVE('',#32235,#32236,#9885,.T.) ;
#39369 = EDGE_CURVE('',#32236,#32237,#9886,.T.) ;
#39370 = EDGE_CURVE('',#32228,#32237,#27038,.T.) ;
#39371 = EDGE_CURVE('',#32238,#32239,#9887,.T.) ;
#39372 = EDGE_CURVE('',#32239,#32240,#27039,.T.) ;
#39373 = EDGE_CURVE('',#32240,#32241,#9888,.T.) ;
#39374 = EDGE_CURVE('',#32241,#32056,#27040,.T.) ;
#39375 = EDGE_CURVE('',#32242,#32055,#27041,.T.) ;
#39376 = EDGE_CURVE('',#32242,#32243,#9889,.T.) ;
#39377 = EDGE_CURVE('',#32243,#32244,#9890,.T.) ;
#39378 = EDGE_CURVE('',#32244,#32245,#9891,.T.) ;
#39379 = EDGE_CURVE('',#32245,#32246,#9892,.T.) ;
#39380 = EDGE_CURVE('',#32246,#32247,#9893,.T.) ;
#39381 = EDGE_CURVE('',#32238,#32247,#27042,.T.) ;
#39382 = EDGE_CURVE('',#32248,#32249,#9894,.T.) ;
#39383 = EDGE_CURVE('',#32249,#32250,#27043,.T.) ;
#39384 = EDGE_CURVE('',#32250,#32251,#9895,.T.) ;
#39385 = EDGE_CURVE('',#32251,#32071,#27044,.T.) ;
#39386 = EDGE_CURVE('',#32252,#32070,#27045,.T.) ;
#39387 = EDGE_CURVE('',#32252,#32253,#9896,.T.) ;
#39388 = EDGE_CURVE('',#32253,#32254,#9897,.T.) ;
#39389 = EDGE_CURVE('',#32254,#32255,#9898,.T.) ;
#39390 = EDGE_CURVE('',#32255,#32256,#9899,.T.) ;
#39391 = EDGE_CURVE('',#32256,#32257,#9900,.T.) ;
#39392 = EDGE_CURVE('',#32248,#32257,#27046,.T.) ;
#39393 = EDGE_CURVE('',#32258,#32259,#9901,.T.) ;
#39394 = EDGE_CURVE('',#32259,#32260,#27047,.T.) ;
#39395 = EDGE_CURVE('',#32260,#32261,#9902,.T.) ;
#39396 = EDGE_CURVE('',#32261,#32086,#27048,.T.) ;
#39397 = EDGE_CURVE('',#32262,#32085,#27049,.T.) ;
#39398 = EDGE_CURVE('',#32262,#32263,#9903,.T.) ;
#39399 = EDGE_CURVE('',#32263,#32264,#9904,.T.) ;
#39400 = EDGE_CURVE('',#32264,#32265,#9905,.T.) ;
#39401 = EDGE_CURVE('',#32265,#32266,#9906,.T.) ;
#39402 = EDGE_CURVE('',#32266,#32267,#9907,.T.) ;
#39403 = EDGE_CURVE('',#32258,#32267,#27050,.T.) ;
#39404 = EDGE_CURVE('',#32268,#32269,#9908,.T.) ;
#39405 = EDGE_CURVE('',#32269,#32270,#27051,.T.) ;
#39406 = EDGE_CURVE('',#32270,#32271,#9909,.T.) ;
#39407 = EDGE_CURVE('',#32271,#32101,#27052,.T.) ;
#39408 = EDGE_CURVE('',#32272,#32100,#27053,.T.) ;
#39409 = EDGE_CURVE('',#32272,#32273,#9910,.T.) ;
#39410 = EDGE_CURVE('',#32273,#32274,#9911,.T.) ;
#39411 = EDGE_CURVE('',#32274,#32275,#9912,.T.) ;
#39412 = EDGE_CURVE('',#32275,#32276,#9913,.T.) ;
#39413 = EDGE_CURVE('',#32276,#32277,#9914,.T.) ;
#39414 = EDGE_CURVE('',#32268,#32277,#27054,.T.) ;
#39415 = EDGE_CURVE('',#32278,#32279,#9915,.T.) ;
#39416 = EDGE_CURVE('',#32279,#32280,#27055,.T.) ;
#39417 = EDGE_CURVE('',#32280,#32281,#9916,.T.) ;
#39418 = EDGE_CURVE('',#32281,#32116,#27056,.T.) ;
#39419 = EDGE_CURVE('',#32282,#32115,#27057,.T.) ;
#39420 = EDGE_CURVE('',#32282,#32283,#9917,.T.) ;
#39421 = EDGE_CURVE('',#32283,#32284,#9918,.T.) ;
#39422 = EDGE_CURVE('',#32284,#32285,#9919,.T.) ;
#39423 = EDGE_CURVE('',#32285,#32286,#9920,.T.) ;
#39424 = EDGE_CURVE('',#32286,#32287,#9921,.T.) ;
#39425 = EDGE_CURVE('',#32278,#32287,#27058,.T.) ;
#39426 = EDGE_CURVE('',#32288,#32289,#9922,.T.) ;
#39427 = EDGE_CURVE('',#32289,#32290,#27059,.T.) ;
#39428 = EDGE_CURVE('',#32290,#32291,#9923,.T.) ;
#39429 = EDGE_CURVE('',#32291,#32167,#27060,.T.) ;
#39430 = EDGE_CURVE('',#32292,#32166,#27061,.T.) ;
#39431 = EDGE_CURVE('',#32292,#32293,#9924,.T.) ;
#39432 = EDGE_CURVE('',#32293,#32294,#9925,.T.) ;
#39433 = EDGE_CURVE('',#32294,#32295,#9926,.T.) ;
#39434 = EDGE_CURVE('',#32295,#32296,#9927,.T.) ;
#39435 = EDGE_CURVE('',#32296,#32297,#9928,.T.) ;
#39436 = EDGE_CURVE('',#32288,#32297,#27062,.T.) ;
#39437 = EDGE_CURVE('',#32298,#32299,#27063,.T.) ;
#39438 = EDGE_CURVE('',#32298,#32300,#9929,.T.) ;
#39439 = EDGE_CURVE('',#32300,#32301,#9930,.T.) ;
#39440 = EDGE_CURVE('',#32301,#32302,#9931,.T.) ;
#39441 = EDGE_CURVE('',#32302,#32299,#9932,.T.) ;
#39442 = EDGE_CURVE('',#32303,#32304,#27064,.T.) ;
#39443 = EDGE_CURVE('',#32303,#32305,#9933,.T.) ;
#39444 = EDGE_CURVE('',#32305,#32306,#9934,.T.) ;
#39445 = EDGE_CURVE('',#32306,#32307,#9935,.T.) ;
#39446 = EDGE_CURVE('',#32307,#32304,#9936,.T.) ;
#39447 = EDGE_CURVE('',#32308,#32309,#27065,.T.) ;
#39448 = EDGE_CURVE('',#32308,#32310,#9937,.T.) ;
#39449 = EDGE_CURVE('',#32310,#32311,#9938,.T.) ;
#39450 = EDGE_CURVE('',#32311,#32312,#9939,.T.) ;
#39451 = EDGE_CURVE('',#32312,#32309,#9940,.T.) ;
#39452 = EDGE_CURVE('',#32313,#32314,#27066,.T.) ;
#39453 = EDGE_CURVE('',#32313,#32315,#9941,.T.) ;
#39454 = EDGE_CURVE('',#32315,#32316,#9942,.T.) ;
#39455 = EDGE_CURVE('',#32316,#32317,#9943,.T.) ;
#39456 = EDGE_CURVE('',#32317,#32314,#9944,.T.) ;
#39457 = EDGE_CURVE('',#32318,#32319,#27067,.T.) ;
#39458 = EDGE_CURVE('',#32318,#32320,#9945,.T.) ;
#39459 = EDGE_CURVE('',#32320,#32321,#9946,.T.) ;
#39460 = EDGE_CURVE('',#32321,#32322,#9947,.T.) ;
#39461 = EDGE_CURVE('',#32322,#32319,#9948,.T.) ;
#39462 = EDGE_CURVE('',#32323,#32324,#27068,.T.) ;
#39463 = EDGE_CURVE('',#32323,#32325,#9949,.T.) ;
#39464 = EDGE_CURVE('',#32325,#32326,#9950,.T.) ;
#39465 = EDGE_CURVE('',#32326,#32327,#9951,.T.) ;
#39466 = EDGE_CURVE('',#32327,#32324,#9952,.T.) ;
#39467 = EDGE_CURVE('',#32328,#32329,#27069,.T.) ;
#39468 = EDGE_CURVE('',#32328,#32330,#9953,.T.) ;
#39469 = EDGE_CURVE('',#32330,#32331,#9954,.T.) ;
#39470 = EDGE_CURVE('',#32331,#32332,#9955,.T.) ;
#39471 = EDGE_CURVE('',#32332,#32329,#9956,.T.) ;
#39472 = EDGE_CURVE('',#32333,#32334,#27070,.T.) ;
#39473 = EDGE_CURVE('',#32333,#32335,#9957,.T.) ;
#39474 = EDGE_CURVE('',#32335,#32336,#9958,.T.) ;
#39475 = EDGE_CURVE('',#32336,#32337,#9959,.T.) ;
#39476 = EDGE_CURVE('',#32337,#32334,#9960,.T.) ;
#39477 = EDGE_CURVE('',#32338,#32339,#27071,.T.) ;
#39478 = EDGE_CURVE('',#32338,#32340,#9961,.T.) ;
#39479 = EDGE_CURVE('',#32340,#32341,#9962,.T.) ;
#39480 = EDGE_CURVE('',#32341,#32342,#9963,.T.) ;
#39481 = EDGE_CURVE('',#32342,#32339,#9964,.T.) ;
#39482 = EDGE_CURVE('',#32343,#32344,#27072,.T.) ;
#39483 = EDGE_CURVE('',#32343,#32345,#9965,.T.) ;
#39484 = EDGE_CURVE('',#32345,#32346,#9966,.T.) ;
#39485 = EDGE_CURVE('',#32346,#32347,#9967,.T.) ;
#39486 = EDGE_CURVE('',#32347,#32344,#9968,.T.) ;
#39487 = EDGE_CURVE('',#32348,#32349,#27073,.T.) ;
#39488 = EDGE_CURVE('',#32348,#32350,#9969,.T.) ;
#39489 = EDGE_CURVE('',#32350,#32351,#9970,.T.) ;
#39490 = EDGE_CURVE('',#32351,#32352,#9971,.T.) ;
#39491 = EDGE_CURVE('',#32352,#32349,#9972,.T.) ;
#39492 = EDGE_CURVE('',#32353,#32354,#27074,.T.) ;
#39493 = EDGE_CURVE('',#32353,#32355,#9973,.T.) ;
#39494 = EDGE_CURVE('',#32355,#32356,#9974,.T.) ;
#39495 = EDGE_CURVE('',#32356,#32357,#9975,.T.) ;
#39496 = EDGE_CURVE('',#32357,#32354,#9976,.T.) ;
#39497 = EDGE_CURVE('',#32358,#32359,#27075,.T.) ;
#39498 = EDGE_CURVE('',#32358,#32360,#9977,.T.) ;
#39499 = EDGE_CURVE('',#32360,#32361,#9978,.T.) ;
#39500 = EDGE_CURVE('',#32361,#32362,#9979,.T.) ;
#39501 = EDGE_CURVE('',#32362,#32359,#9980,.T.) ;
#39502 = EDGE_CURVE('',#32363,#32364,#27076,.T.) ;
#39503 = EDGE_CURVE('',#32363,#32365,#9981,.T.) ;
#39504 = EDGE_CURVE('',#32365,#32366,#9982,.T.) ;
#39505 = EDGE_CURVE('',#32366,#32367,#9983,.T.) ;
#39506 = EDGE_CURVE('',#32367,#32364,#9984,.T.) ;
#39507 = EDGE_CURVE('',#32368,#32369,#27077,.T.) ;
#39508 = EDGE_CURVE('',#32368,#32370,#9985,.T.) ;
#39509 = EDGE_CURVE('',#32370,#32371,#9986,.T.) ;
#39510 = EDGE_CURVE('',#32371,#32372,#9987,.T.) ;
#39511 = EDGE_CURVE('',#32372,#32369,#9988,.T.) ;
#39512 = EDGE_CURVE('',#32373,#32374,#27078,.T.) ;
#39513 = EDGE_CURVE('',#32373,#32375,#9989,.T.) ;
#39514 = EDGE_CURVE('',#32375,#32376,#9990,.T.) ;
#39515 = EDGE_CURVE('',#32376,#32377,#9991,.T.) ;
#39516 = EDGE_CURVE('',#32377,#32374,#9992,.T.) ;
#39517 = EDGE_CURVE('',#32378,#32379,#27079,.T.) ;
#39518 = EDGE_CURVE('',#32378,#32380,#9993,.T.) ;
#39519 = EDGE_CURVE('',#32380,#32381,#9994,.T.) ;
#39520 = EDGE_CURVE('',#32381,#32382,#9995,.T.) ;
#39521 = EDGE_CURVE('',#32382,#32379,#9996,.T.) ;
#39522 = EDGE_CURVE('',#32383,#32384,#27080,.T.) ;
#39523 = EDGE_CURVE('',#32383,#32385,#9997,.T.) ;
#39524 = EDGE_CURVE('',#32385,#32386,#9998,.T.) ;
#39525 = EDGE_CURVE('',#32386,#32387,#9999,.T.) ;
#39526 = EDGE_CURVE('',#32387,#32384,#10000,.T.) ;
#39527 = EDGE_CURVE('',#32388,#32389,#10001,.T.) ;
#39528 = EDGE_CURVE('',#32388,#32390,#27081,.T.) ;
#39529 = EDGE_CURVE('',#32390,#32391,#10002,.T.) ;
#39530 = EDGE_CURVE('',#32391,#32389,#27082,.T.) ;
#39531 = EDGE_CURVE('',#32392,#32393,#10003,.T.) ;
#39532 = EDGE_CURVE('',#32392,#32394,#27083,.T.) ;
#39533 = EDGE_CURVE('',#32394,#32395,#10004,.T.) ;
#39534 = EDGE_CURVE('',#32395,#32393,#27084,.T.) ;
#39535 = EDGE_CURVE('',#32396,#32397,#10005,.T.) ;
#39536 = EDGE_CURVE('',#32396,#32398,#27085,.T.) ;
#39537 = EDGE_CURVE('',#32398,#32399,#10006,.T.) ;
#39538 = EDGE_CURVE('',#32399,#32397,#27086,.T.) ;
#39539 = EDGE_CURVE('',#32400,#32401,#10007,.T.) ;
#39540 = EDGE_CURVE('',#32400,#32402,#27087,.T.) ;
#39541 = EDGE_CURVE('',#32402,#32403,#10008,.T.) ;
#39542 = EDGE_CURVE('',#32403,#32401,#27088,.T.) ;
#39543 = EDGE_CURVE('',#32404,#32405,#10009,.T.) ;
#39544 = EDGE_CURVE('',#32404,#32406,#27089,.T.) ;
#39545 = EDGE_CURVE('',#32406,#32407,#10010,.T.) ;
#39546 = EDGE_CURVE('',#32407,#32405,#27090,.T.) ;
#39547 = EDGE_CURVE('',#32408,#32409,#10011,.T.) ;
#39548 = EDGE_CURVE('',#32408,#32410,#27091,.T.) ;
#39549 = EDGE_CURVE('',#32410,#32411,#10012,.T.) ;
#39550 = EDGE_CURVE('',#32411,#32409,#27092,.T.) ;
#39551 = EDGE_CURVE('',#32412,#32413,#10013,.T.) ;
#39552 = EDGE_CURVE('',#32412,#32414,#27093,.T.) ;
#39553 = EDGE_CURVE('',#32414,#32415,#10014,.T.) ;
#39554 = EDGE_CURVE('',#32415,#32413,#27094,.T.) ;
#39555 = EDGE_CURVE('',#32416,#32417,#10015,.T.) ;
#39556 = EDGE_CURVE('',#32416,#32418,#27095,.T.) ;
#39557 = EDGE_CURVE('',#32418,#32419,#10016,.T.) ;
#39558 = EDGE_CURVE('',#32419,#32417,#27096,.T.) ;
#39559 = EDGE_CURVE('',#32420,#32421,#10017,.T.) ;
#39560 = EDGE_CURVE('',#32420,#32422,#27097,.T.) ;
#39561 = EDGE_CURVE('',#32422,#32423,#10018,.T.) ;
#39562 = EDGE_CURVE('',#32423,#32421,#27098,.T.) ;
#39563 = EDGE_CURVE('',#32424,#32425,#10019,.T.) ;
#39564 = EDGE_CURVE('',#32425,#32426,#27099,.T.) ;
#39565 = EDGE_CURVE('',#32426,#32427,#10020,.T.) ;
#39566 = EDGE_CURVE('',#32427,#32204,#27100,.T.) ;
#39567 = EDGE_CURVE('',#32428,#32203,#27101,.T.) ;
#39568 = EDGE_CURVE('',#32428,#32429,#10021,.T.) ;
#39569 = EDGE_CURVE('',#32429,#32430,#10022,.T.) ;
#39570 = EDGE_CURVE('',#32430,#32431,#10023,.T.) ;
#39571 = EDGE_CURVE('',#32431,#32432,#10024,.T.) ;
#39572 = EDGE_CURVE('',#32432,#32433,#10025,.T.) ;
#39573 = EDGE_CURVE('',#32424,#32433,#27102,.T.) ;
#39574 = EDGE_CURVE('',#32434,#32435,#27103,.T.) ;
#39575 = EDGE_CURVE('',#32434,#32436,#10026,.T.) ;
#39576 = EDGE_CURVE('',#32436,#32437,#10027,.T.) ;
#39577 = EDGE_CURVE('',#32437,#32438,#10028,.T.) ;
#39578 = EDGE_CURVE('',#32438,#32435,#10029,.T.) ;
#39579 = EDGE_CURVE('',#32439,#32440,#27104,.T.) ;
#39580 = EDGE_CURVE('',#32439,#32441,#10030,.T.) ;
#39581 = EDGE_CURVE('',#32441,#32442,#10031,.T.) ;
#39582 = EDGE_CURVE('',#32442,#32443,#10032,.T.) ;
#39583 = EDGE_CURVE('',#32443,#32440,#10033,.T.) ;
#39584 = EDGE_CURVE('',#32444,#32445,#10034,.T.) ;
#39585 = EDGE_CURVE('',#32444,#32446,#27105,.T.) ;
#39586 = EDGE_CURVE('',#32446,#32447,#10035,.T.) ;
#39587 = EDGE_CURVE('',#32447,#32445,#27106,.T.) ;
#39588 = EDGE_CURVE('',#32448,#32449,#10036,.T.) ;
#39589 = EDGE_CURVE('',#32448,#32450,#27107,.T.) ;
#39590 = EDGE_CURVE('',#32450,#32451,#10037,.T.) ;
#39591 = EDGE_CURVE('',#32451,#32449,#27108,.T.) ;
#39592 = EDGE_CURVE('',#32452,#32453,#27109,.T.) ;
#39593 = EDGE_CURVE('',#32452,#32454,#10038,.T.) ;
#39594 = EDGE_CURVE('',#32455,#32454,#10039,.T.) ;
#39595 = EDGE_CURVE('',#32455,#32448,#10040,.T.) ;
#39596 = EDGE_CURVE('',#32449,#32447,#10041,.T.) ;
#39597 = EDGE_CURVE('',#32446,#32456,#10042,.T.) ;
#39598 = EDGE_CURVE('',#32457,#32456,#27110,.T.) ;
#39599 = EDGE_CURVE('',#32457,#32458,#10043,.T.) ;
#39600 = EDGE_CURVE('',#32459,#32458,#27111,.T.) ;
#39601 = EDGE_CURVE('',#32459,#32391,#10044,.T.) ;
#39602 = EDGE_CURVE('',#32390,#32460,#10045,.T.) ;
#39603 = EDGE_CURVE('',#32461,#32460,#27112,.T.) ;
#39604 = EDGE_CURVE('',#32461,#32462,#10046,.T.) ;
#39605 = EDGE_CURVE('',#32463,#32462,#27113,.T.) ;
#39606 = EDGE_CURVE('',#32463,#32395,#10047,.T.) ;
#39607 = EDGE_CURVE('',#32394,#32464,#10048,.T.) ;
#39608 = EDGE_CURVE('',#32465,#32464,#27114,.T.) ;
#39609 = EDGE_CURVE('',#32465,#32466,#10049,.T.) ;
#39610 = EDGE_CURVE('',#32467,#32466,#27115,.T.) ;
#39611 = EDGE_CURVE('',#32467,#32399,#10050,.T.) ;
#39612 = EDGE_CURVE('',#32398,#32468,#10051,.T.) ;
#39613 = EDGE_CURVE('',#32469,#32468,#27116,.T.) ;
#39614 = EDGE_CURVE('',#32469,#32470,#10052,.T.) ;
#39615 = EDGE_CURVE('',#32471,#32470,#27117,.T.) ;
#39616 = EDGE_CURVE('',#32471,#32403,#10053,.T.) ;
#39617 = EDGE_CURVE('',#32402,#32472,#10054,.T.) ;
#39618 = EDGE_CURVE('',#32473,#32472,#27118,.T.) ;
#39619 = EDGE_CURVE('',#32473,#32474,#10055,.T.) ;
#39620 = EDGE_CURVE('',#32475,#32474,#27119,.T.) ;
#39621 = EDGE_CURVE('',#32475,#32407,#10056,.T.) ;
#39622 = EDGE_CURVE('',#32406,#32476,#10057,.T.) ;
#39623 = EDGE_CURVE('',#32477,#32476,#27120,.T.) ;
#39624 = EDGE_CURVE('',#32477,#32478,#10058,.T.) ;
#39625 = EDGE_CURVE('',#32479,#32478,#27121,.T.) ;
#39626 = EDGE_CURVE('',#32479,#32411,#10059,.T.) ;
#39627 = EDGE_CURVE('',#32410,#32480,#10060,.T.) ;
#39628 = EDGE_CURVE('',#32481,#32480,#27122,.T.) ;
#39629 = EDGE_CURVE('',#32481,#32482,#10061,.T.) ;
#39630 = EDGE_CURVE('',#32483,#32482,#27123,.T.) ;
#39631 = EDGE_CURVE('',#32483,#32415,#10062,.T.) ;
#39632 = EDGE_CURVE('',#32414,#32484,#10063,.T.) ;
#39633 = EDGE_CURVE('',#32485,#32484,#27124,.T.) ;
#39634 = EDGE_CURVE('',#32485,#32486,#10064,.T.) ;
#39635 = EDGE_CURVE('',#32487,#32486,#27125,.T.) ;
#39636 = EDGE_CURVE('',#32487,#32419,#10065,.T.) ;
#39637 = EDGE_CURVE('',#32418,#32488,#10066,.T.) ;
#39638 = EDGE_CURVE('',#32489,#32488,#27126,.T.) ;
#39639 = EDGE_CURVE('',#32489,#32490,#10067,.T.) ;
#39640 = EDGE_CURVE('',#32491,#32490,#27127,.T.) ;
#39641 = EDGE_CURVE('',#32491,#32423,#10068,.T.) ;
#39642 = EDGE_CURVE('',#32422,#32492,#10069,.T.) ;
#39643 = EDGE_CURVE('',#32493,#32492,#27128,.T.) ;
#39644 = EDGE_CURVE('',#32493,#32453,#10070,.T.) ;
#39645 = EDGE_CURVE('',#32454,#32494,#27129,.T.) ;
#39646 = EDGE_CURVE('',#32495,#32494,#10071,.T.) ;
#39647 = EDGE_CURVE('',#32495,#32455,#27130,.T.) ;
#39648 = EDGE_CURVE('',#32496,#32497,#27131,.T.) ;
#39649 = EDGE_CURVE('',#32496,#32420,#10072,.T.) ;
#39650 = EDGE_CURVE('',#32421,#32498,#10073,.T.) ;
#39651 = EDGE_CURVE('',#32499,#32498,#27132,.T.) ;
#39652 = EDGE_CURVE('',#32499,#32500,#10074,.T.) ;
#39653 = EDGE_CURVE('',#32501,#32500,#27133,.T.) ;
#39654 = EDGE_CURVE('',#32501,#32416,#10075,.T.) ;
#39655 = EDGE_CURVE('',#32417,#32502,#10076,.T.) ;
#39656 = EDGE_CURVE('',#32503,#32502,#27134,.T.) ;
#39657 = EDGE_CURVE('',#32503,#32504,#10077,.T.) ;
#39658 = EDGE_CURVE('',#32505,#32504,#27135,.T.) ;
#39659 = EDGE_CURVE('',#32505,#32412,#10078,.T.) ;
#39660 = EDGE_CURVE('',#32413,#32506,#10079,.T.) ;
#39661 = EDGE_CURVE('',#32507,#32506,#27136,.T.) ;
#39662 = EDGE_CURVE('',#32507,#32508,#10080,.T.) ;
#39663 = EDGE_CURVE('',#32509,#32508,#27137,.T.) ;
#39664 = EDGE_CURVE('',#32509,#32408,#10081,.T.) ;
#39665 = EDGE_CURVE('',#32409,#32510,#10082,.T.) ;
#39666 = EDGE_CURVE('',#32511,#32510,#27138,.T.) ;
#39667 = EDGE_CURVE('',#32511,#32512,#10083,.T.) ;
#39668 = EDGE_CURVE('',#32513,#32512,#27139,.T.) ;
#39669 = EDGE_CURVE('',#32513,#32404,#10084,.T.) ;
#39670 = EDGE_CURVE('',#32405,#32514,#10085,.T.) ;
#39671 = EDGE_CURVE('',#32515,#32514,#27140,.T.) ;
#39672 = EDGE_CURVE('',#32515,#32516,#10086,.T.) ;
#39673 = EDGE_CURVE('',#32517,#32516,#27141,.T.) ;
#39674 = EDGE_CURVE('',#32517,#32400,#10087,.T.) ;
#39675 = EDGE_CURVE('',#32401,#32518,#10088,.T.) ;
#39676 = EDGE_CURVE('',#32519,#32518,#27142,.T.) ;
#39677 = EDGE_CURVE('',#32519,#32520,#10089,.T.) ;
#39678 = EDGE_CURVE('',#32521,#32520,#27143,.T.) ;
#39679 = EDGE_CURVE('',#32521,#32396,#10090,.T.) ;
#39680 = EDGE_CURVE('',#32397,#32522,#10091,.T.) ;
#39681 = EDGE_CURVE('',#32523,#32522,#27144,.T.) ;
#39682 = EDGE_CURVE('',#32523,#32524,#10092,.T.) ;
#39683 = EDGE_CURVE('',#32525,#32524,#27145,.T.) ;
#39684 = EDGE_CURVE('',#32525,#32392,#10093,.T.) ;
#39685 = EDGE_CURVE('',#32393,#32526,#10094,.T.) ;
#39686 = EDGE_CURVE('',#32527,#32526,#27146,.T.) ;
#39687 = EDGE_CURVE('',#32527,#32528,#10095,.T.) ;
#39688 = EDGE_CURVE('',#32529,#32528,#27147,.T.) ;
#39689 = EDGE_CURVE('',#32529,#32388,#10096,.T.) ;
#39690 = EDGE_CURVE('',#32389,#32530,#10097,.T.) ;
#39691 = EDGE_CURVE('',#32531,#32530,#27148,.T.) ;
#39692 = EDGE_CURVE('',#32531,#32532,#10098,.T.) ;
#39693 = EDGE_CURVE('',#32533,#32532,#27149,.T.) ;
#39694 = EDGE_CURVE('',#32533,#32444,#10099,.T.) ;
#39695 = EDGE_CURVE('',#32445,#32534,#10100,.T.) ;
#39696 = EDGE_CURVE('',#32535,#32534,#10101,.T.) ;
#39697 = EDGE_CURVE('',#32535,#32495,#10102,.T.) ;
#39698 = EDGE_CURVE('',#32494,#32536,#10103,.T.) ;
#39699 = EDGE_CURVE('',#32537,#32536,#27150,.T.) ;
#39700 = EDGE_CURVE('',#32537,#32497,#10104,.T.) ;
#39701 = EDGE_CURVE('',#32538,#32539,#10105,.T.) ;
#39702 = EDGE_CURVE('',#32538,#32535,#27151,.T.) ;
#39703 = EDGE_CURVE('',#32534,#32539,#27152,.T.) ;
#39704 = EDGE_CURVE('',#32540,#32541,#10106,.T.) ;
#39705 = EDGE_CURVE('',#32540,#32538,#10107,.T.) ;
#39706 = EDGE_CURVE('',#32539,#32541,#10108,.T.) ;
#39707 = EDGE_CURVE('',#32542,#32543,#10109,.T.) ;
#39708 = EDGE_CURVE('',#32542,#32540,#27153,.T.) ;
#39709 = EDGE_CURVE('',#32541,#32543,#27154,.T.) ;
#39710 = EDGE_CURVE('',#32544,#32545,#10110,.T.) ;
#39711 = EDGE_CURVE('',#32544,#32542,#10111,.T.) ;
#39712 = EDGE_CURVE('',#32543,#32545,#10112,.T.) ;
#39713 = EDGE_CURVE('',#32546,#32547,#10113,.T.) ;
#39714 = EDGE_CURVE('',#32546,#32544,#27155,.T.) ;
#39715 = EDGE_CURVE('',#32545,#32547,#27156,.T.) ;
#39716 = EDGE_CURVE('',#32548,#32549,#10114,.T.) ;
#39717 = EDGE_CURVE('',#32548,#32546,#10115,.T.) ;
#39718 = EDGE_CURVE('',#32547,#32549,#10116,.T.) ;
#39719 = EDGE_CURVE('',#32550,#32551,#10117,.T.) ;
#39720 = EDGE_CURVE('',#32550,#32548,#27157,.T.) ;
#39721 = EDGE_CURVE('',#32549,#32551,#27158,.T.) ;
#39722 = EDGE_CURVE('',#32552,#32553,#10118,.T.) ;
#39723 = EDGE_CURVE('',#32552,#32550,#10119,.T.) ;
#39724 = EDGE_CURVE('',#32551,#32553,#10120,.T.) ;
#39725 = EDGE_CURVE('',#32554,#32555,#10121,.T.) ;
#39726 = EDGE_CURVE('',#32554,#32552,#27159,.T.) ;
#39727 = EDGE_CURVE('',#32553,#32555,#27160,.T.) ;
#39728 = EDGE_CURVE('',#32556,#32557,#10122,.T.) ;
#39729 = EDGE_CURVE('',#32556,#32554,#10123,.T.) ;
#39730 = EDGE_CURVE('',#32555,#32557,#10124,.T.) ;
#39731 = EDGE_CURVE('',#32558,#32559,#10125,.T.) ;
#39732 = EDGE_CURVE('',#32558,#32556,#27161,.T.) ;
#39733 = EDGE_CURVE('',#32557,#32559,#27162,.T.) ;
#39734 = EDGE_CURVE('',#32450,#32558,#10126,.T.) ;
#39735 = EDGE_CURVE('',#32559,#32451,#10127,.T.) ;
#39736 = EDGE_CURVE('',#32560,#32561,#27163,.T.) ;
#39737 = EDGE_CURVE('',#32561,#32562,#10128,.T.) ;
#39738 = EDGE_CURVE('',#32562,#32563,#10129,.T.) ;
#39739 = EDGE_CURVE('',#32563,#32564,#10130,.T.) ;
#39740 = EDGE_CURVE('',#32564,#32565,#27164,.T.) ;
#39741 = EDGE_CURVE('',#32565,#32566,#10131,.T.) ;
#39742 = EDGE_CURVE('',#32566,#32567,#27165,.T.) ;
#39743 = EDGE_CURVE('',#32567,#32153,#10132,.T.) ;
#39744 = EDGE_CURVE('',#32154,#32568,#10133,.T.) ;
#39745 = EDGE_CURVE('',#32568,#32569,#27166,.T.) ;
#39746 = EDGE_CURVE('',#32569,#32570,#10134,.T.) ;
#39747 = EDGE_CURVE('',#32570,#32571,#10135,.T.) ;
#39748 = EDGE_CURVE('',#32571,#32572,#10136,.T.) ;
#39749 = EDGE_CURVE('',#32572,#32573,#27167,.T.) ;
#39750 = EDGE_CURVE('',#32573,#32574,#10137,.T.) ;
#39751 = EDGE_CURVE('',#32574,#32575,#27168,.T.) ;
#39752 = EDGE_CURVE('',#32575,#32576,#10138,.T.) ;
#39753 = EDGE_CURVE('',#32576,#32577,#27169,.T.) ;
#39754 = EDGE_CURVE('',#32577,#32578,#27170,.T.) ;
#39755 = EDGE_CURVE('',#32578,#32579,#27171,.T.) ;
#39756 = EDGE_CURVE('',#32579,#32580,#10139,.T.) ;
#39757 = EDGE_CURVE('',#32580,#32581,#27172,.T.) ;
#39758 = EDGE_CURVE('',#32581,#32560,#10140,.T.) ;
#39759 = EDGE_CURVE('',#32582,#32583,#27173,.T.) ;
#39760 = EDGE_CURVE('',#32583,#32584,#10141,.T.) ;
#39761 = EDGE_CURVE('',#32584,#32585,#10142,.T.) ;
#39762 = EDGE_CURVE('',#32585,#32586,#10143,.T.) ;
#39763 = EDGE_CURVE('',#32586,#32587,#27174,.T.) ;
#39764 = EDGE_CURVE('',#32587,#32588,#10144,.T.) ;
#39765 = EDGE_CURVE('',#32588,#32589,#27175,.T.) ;
#39766 = EDGE_CURVE('',#32589,#32149,#10145,.T.) ;
#39767 = EDGE_CURVE('',#32150,#32590,#10146,.T.) ;
#39768 = EDGE_CURVE('',#32590,#32591,#27176,.T.) ;
#39769 = EDGE_CURVE('',#32591,#32592,#10147,.T.) ;
#39770 = EDGE_CURVE('',#32592,#32593,#10148,.T.) ;
#39771 = EDGE_CURVE('',#32593,#32594,#10149,.T.) ;
#39772 = EDGE_CURVE('',#32594,#32595,#27177,.T.) ;
#39773 = EDGE_CURVE('',#32595,#32596,#10150,.T.) ;
#39774 = EDGE_CURVE('',#32596,#32597,#27178,.T.) ;
#39775 = EDGE_CURVE('',#32597,#32598,#10151,.T.) ;
#39776 = EDGE_CURVE('',#32598,#32599,#27179,.T.) ;
#39777 = EDGE_CURVE('',#32599,#32600,#27180,.T.) ;
#39778 = EDGE_CURVE('',#32600,#32601,#27181,.T.) ;
#39779 = EDGE_CURVE('',#32601,#32602,#10152,.T.) ;
#39780 = EDGE_CURVE('',#32602,#32603,#27182,.T.) ;
#39781 = EDGE_CURVE('',#32603,#32582,#10153,.T.) ;
#39782 = EDGE_CURVE('',#32604,#32605,#27183,.T.) ;
#39783 = EDGE_CURVE('',#32605,#32606,#10154,.T.) ;
#39784 = EDGE_CURVE('',#32606,#32607,#10155,.T.) ;
#39785 = EDGE_CURVE('',#32607,#32608,#10156,.T.) ;
#39786 = EDGE_CURVE('',#32608,#32609,#27184,.T.) ;
#39787 = EDGE_CURVE('',#32609,#32610,#10157,.T.) ;
#39788 = EDGE_CURVE('',#32610,#32611,#27185,.T.) ;
#39789 = EDGE_CURVE('',#32611,#32145,#10158,.T.) ;
#39790 = EDGE_CURVE('',#32146,#32612,#10159,.T.) ;
#39791 = EDGE_CURVE('',#32612,#32613,#27186,.T.) ;
#39792 = EDGE_CURVE('',#32613,#32614,#10160,.T.) ;
#39793 = EDGE_CURVE('',#32614,#32615,#10161,.T.) ;
#39794 = EDGE_CURVE('',#32615,#32616,#10162,.T.) ;
#39795 = EDGE_CURVE('',#32616,#32617,#27187,.T.) ;
#39796 = EDGE_CURVE('',#32617,#32618,#10163,.T.) ;
#39797 = EDGE_CURVE('',#32618,#32619,#27188,.T.) ;
#39798 = EDGE_CURVE('',#32619,#32620,#10164,.T.) ;
#39799 = EDGE_CURVE('',#32620,#32621,#27189,.T.) ;
#39800 = EDGE_CURVE('',#32621,#32622,#27190,.T.) ;
#39801 = EDGE_CURVE('',#32622,#32623,#27191,.T.) ;
#39802 = EDGE_CURVE('',#32623,#32624,#10165,.T.) ;
#39803 = EDGE_CURVE('',#32624,#32625,#27192,.T.) ;
#39804 = EDGE_CURVE('',#32625,#32604,#10166,.T.) ;
#39805 = EDGE_CURVE('',#32626,#32627,#27193,.T.) ;
#39806 = EDGE_CURVE('',#32627,#32628,#10167,.T.) ;
#39807 = EDGE_CURVE('',#32628,#32629,#10168,.T.) ;
#39808 = EDGE_CURVE('',#32629,#32630,#10169,.T.) ;
#39809 = EDGE_CURVE('',#32630,#32631,#27194,.T.) ;
#39810 = EDGE_CURVE('',#32631,#32632,#10170,.T.) ;
#39811 = EDGE_CURVE('',#32632,#32633,#27195,.T.) ;
#39812 = EDGE_CURVE('',#32633,#32141,#10171,.T.) ;
#39813 = EDGE_CURVE('',#32142,#32634,#10172,.T.) ;
#39814 = EDGE_CURVE('',#32634,#32635,#27196,.T.) ;
#39815 = EDGE_CURVE('',#32635,#32636,#10173,.T.) ;
#39816 = EDGE_CURVE('',#32636,#32637,#10174,.T.) ;
#39817 = EDGE_CURVE('',#32637,#32638,#10175,.T.) ;
#39818 = EDGE_CURVE('',#32638,#32639,#27197,.T.) ;
#39819 = EDGE_CURVE('',#32639,#32640,#10176,.T.) ;
#39820 = EDGE_CURVE('',#32640,#32641,#27198,.T.) ;
#39821 = EDGE_CURVE('',#32641,#32642,#10177,.T.) ;
#39822 = EDGE_CURVE('',#32642,#32643,#27199,.T.) ;
#39823 = EDGE_CURVE('',#32643,#32644,#27200,.T.) ;
#39824 = EDGE_CURVE('',#32644,#32645,#27201,.T.) ;
#39825 = EDGE_CURVE('',#32645,#32646,#10178,.T.) ;
#39826 = EDGE_CURVE('',#32646,#32647,#27202,.T.) ;
#39827 = EDGE_CURVE('',#32647,#32626,#10179,.T.) ;
#39828 = EDGE_CURVE('',#32648,#32649,#27203,.T.) ;
#39829 = EDGE_CURVE('',#32649,#32650,#10180,.T.) ;
#39830 = EDGE_CURVE('',#32650,#32651,#10181,.T.) ;
#39831 = EDGE_CURVE('',#32651,#32652,#10182,.T.) ;
#39832 = EDGE_CURVE('',#32652,#32653,#27204,.T.) ;
#39833 = EDGE_CURVE('',#32653,#32654,#10183,.T.) ;
#39834 = EDGE_CURVE('',#32654,#32655,#27205,.T.) ;
#39835 = EDGE_CURVE('',#32655,#32137,#10184,.T.) ;
#39836 = EDGE_CURVE('',#32138,#32656,#10185,.T.) ;
#39837 = EDGE_CURVE('',#32656,#32657,#27206,.T.) ;
#39838 = EDGE_CURVE('',#32657,#32658,#10186,.T.) ;
#39839 = EDGE_CURVE('',#32658,#32659,#10187,.T.) ;
#39840 = EDGE_CURVE('',#32659,#32660,#10188,.T.) ;
#39841 = EDGE_CURVE('',#32660,#32661,#27207,.T.) ;
#39842 = EDGE_CURVE('',#32661,#32662,#10189,.T.) ;
#39843 = EDGE_CURVE('',#32662,#32663,#27208,.T.) ;
#39844 = EDGE_CURVE('',#32663,#32664,#10190,.T.) ;
#39845 = EDGE_CURVE('',#32664,#32665,#27209,.T.) ;
#39846 = EDGE_CURVE('',#32665,#32666,#27210,.T.) ;
#39847 = EDGE_CURVE('',#32666,#32667,#27211,.T.) ;
#39848 = EDGE_CURVE('',#32667,#32668,#10191,.T.) ;
#39849 = EDGE_CURVE('',#32668,#32669,#27212,.T.) ;
#39850 = EDGE_CURVE('',#32669,#32648,#10192,.T.) ;
#39851 = EDGE_CURVE('',#32670,#32671,#27213,.T.) ;
#39852 = EDGE_CURVE('',#32671,#32672,#10193,.T.) ;
#39853 = EDGE_CURVE('',#32672,#32673,#10194,.T.) ;
#39854 = EDGE_CURVE('',#32673,#32674,#10195,.T.) ;
#39855 = EDGE_CURVE('',#32674,#32675,#27214,.T.) ;
#39856 = EDGE_CURVE('',#32675,#32676,#10196,.T.) ;
#39857 = EDGE_CURVE('',#32676,#32677,#27215,.T.) ;
#39858 = EDGE_CURVE('',#32677,#32133,#10197,.T.) ;
#39859 = EDGE_CURVE('',#32134,#32678,#10198,.T.) ;
#39860 = EDGE_CURVE('',#32678,#32679,#27216,.T.) ;
#39861 = EDGE_CURVE('',#32679,#32680,#10199,.T.) ;
#39862 = EDGE_CURVE('',#32680,#32681,#10200,.T.) ;
#39863 = EDGE_CURVE('',#32681,#32682,#10201,.T.) ;
#39864 = EDGE_CURVE('',#32682,#32683,#27217,.T.) ;
#39865 = EDGE_CURVE('',#32683,#32684,#10202,.T.) ;
#39866 = EDGE_CURVE('',#32684,#32685,#27218,.T.) ;
#39867 = EDGE_CURVE('',#32685,#32686,#10203,.T.) ;
#39868 = EDGE_CURVE('',#32686,#32687,#27219,.T.) ;
#39869 = EDGE_CURVE('',#32687,#32688,#27220,.T.) ;
#39870 = EDGE_CURVE('',#32688,#32689,#27221,.T.) ;
#39871 = EDGE_CURVE('',#32689,#32690,#10204,.T.) ;
#39872 = EDGE_CURVE('',#32690,#32691,#27222,.T.) ;
#39873 = EDGE_CURVE('',#32691,#32670,#10205,.T.) ;
#39874 = EDGE_CURVE('',#32692,#32693,#27223,.T.) ;
#39875 = EDGE_CURVE('',#32693,#32694,#10206,.T.) ;
#39876 = EDGE_CURVE('',#32694,#32695,#10207,.T.) ;
#39877 = EDGE_CURVE('',#32695,#32696,#10208,.T.) ;
#39878 = EDGE_CURVE('',#32696,#32697,#27224,.T.) ;
#39879 = EDGE_CURVE('',#32697,#32698,#10209,.T.) ;
#39880 = EDGE_CURVE('',#32698,#32699,#27225,.T.) ;
#39881 = EDGE_CURVE('',#32699,#32129,#10210,.T.) ;
#39882 = EDGE_CURVE('',#32130,#32700,#10211,.T.) ;
#39883 = EDGE_CURVE('',#32700,#32701,#27226,.T.) ;
#39884 = EDGE_CURVE('',#32701,#32702,#10212,.T.) ;
#39885 = EDGE_CURVE('',#32702,#32703,#10213,.T.) ;
#39886 = EDGE_CURVE('',#32703,#32704,#10214,.T.) ;
#39887 = EDGE_CURVE('',#32704,#32705,#27227,.T.) ;
#39888 = EDGE_CURVE('',#32705,#32706,#10215,.T.) ;
#39889 = EDGE_CURVE('',#32706,#32707,#27228,.T.) ;
#39890 = EDGE_CURVE('',#32707,#32708,#10216,.T.) ;
#39891 = EDGE_CURVE('',#32708,#32709,#27229,.T.) ;
#39892 = EDGE_CURVE('',#32709,#32710,#27230,.T.) ;
#39893 = EDGE_CURVE('',#32710,#32711,#27231,.T.) ;
#39894 = EDGE_CURVE('',#32711,#32712,#10217,.T.) ;
#39895 = EDGE_CURVE('',#32712,#32713,#27232,.T.) ;
#39896 = EDGE_CURVE('',#32713,#32692,#10218,.T.) ;
#39897 = EDGE_CURVE('',#32714,#32715,#27233,.T.) ;
#39898 = EDGE_CURVE('',#32715,#32716,#10219,.T.) ;
#39899 = EDGE_CURVE('',#32716,#32717,#10220,.T.) ;
#39900 = EDGE_CURVE('',#32717,#32718,#10221,.T.) ;
#39901 = EDGE_CURVE('',#32718,#32719,#27234,.T.) ;
#39902 = EDGE_CURVE('',#32719,#32720,#10222,.T.) ;
#39903 = EDGE_CURVE('',#32720,#32721,#27235,.T.) ;
#39904 = EDGE_CURVE('',#32721,#32125,#10223,.T.) ;
#39905 = EDGE_CURVE('',#32126,#32722,#10224,.T.) ;
#39906 = EDGE_CURVE('',#32722,#32723,#27236,.T.) ;
#39907 = EDGE_CURVE('',#32723,#32724,#10225,.T.) ;
#39908 = EDGE_CURVE('',#32724,#32725,#10226,.T.) ;
#39909 = EDGE_CURVE('',#32725,#32726,#10227,.T.) ;
#39910 = EDGE_CURVE('',#32726,#32727,#27237,.T.) ;
#39911 = EDGE_CURVE('',#32727,#32728,#10228,.T.) ;
#39912 = EDGE_CURVE('',#32728,#32729,#27238,.T.) ;
#39913 = EDGE_CURVE('',#32729,#32730,#10229,.T.) ;
#39914 = EDGE_CURVE('',#32730,#32731,#27239,.T.) ;
#39915 = EDGE_CURVE('',#32731,#32732,#27240,.T.) ;
#39916 = EDGE_CURVE('',#32732,#32733,#27241,.T.) ;
#39917 = EDGE_CURVE('',#32733,#32734,#10230,.T.) ;
#39918 = EDGE_CURVE('',#32734,#32735,#27242,.T.) ;
#39919 = EDGE_CURVE('',#32735,#32714,#10231,.T.) ;
#39920 = EDGE_CURVE('',#32736,#32737,#27243,.T.) ;
#39921 = EDGE_CURVE('',#32737,#32738,#10232,.T.) ;
#39922 = EDGE_CURVE('',#32738,#32739,#10233,.T.) ;
#39923 = EDGE_CURVE('',#32739,#32740,#10234,.T.) ;
#39924 = EDGE_CURVE('',#32740,#32741,#27244,.T.) ;
#39925 = EDGE_CURVE('',#32741,#32742,#10235,.T.) ;
#39926 = EDGE_CURVE('',#32742,#32743,#27245,.T.) ;
#39927 = EDGE_CURVE('',#32743,#32121,#10236,.T.) ;
#39928 = EDGE_CURVE('',#32122,#32744,#10237,.T.) ;
#39929 = EDGE_CURVE('',#32744,#32745,#27246,.T.) ;
#39930 = EDGE_CURVE('',#32745,#32746,#10238,.T.) ;
#39931 = EDGE_CURVE('',#32746,#32747,#10239,.T.) ;
#39932 = EDGE_CURVE('',#32747,#32748,#10240,.T.) ;
#39933 = EDGE_CURVE('',#32748,#32749,#27247,.T.) ;
#39934 = EDGE_CURVE('',#32749,#32750,#10241,.T.) ;
#39935 = EDGE_CURVE('',#32750,#32751,#27248,.T.) ;
#39936 = EDGE_CURVE('',#32751,#32752,#10242,.T.) ;
#39937 = EDGE_CURVE('',#32752,#32753,#27249,.T.) ;
#39938 = EDGE_CURVE('',#32753,#32754,#27250,.T.) ;
#39939 = EDGE_CURVE('',#32754,#32755,#27251,.T.) ;
#39940 = EDGE_CURVE('',#32755,#32756,#10243,.T.) ;
#39941 = EDGE_CURVE('',#32756,#32757,#27252,.T.) ;
#39942 = EDGE_CURVE('',#32757,#32736,#10244,.T.) ;
#39943 = EDGE_CURVE('',#32758,#32759,#27253,.T.) ;
#39944 = EDGE_CURVE('',#32759,#32760,#10245,.T.) ;
#39945 = EDGE_CURVE('',#32760,#32761,#10246,.T.) ;
#39946 = EDGE_CURVE('',#32761,#32762,#10247,.T.) ;
#39947 = EDGE_CURVE('',#32762,#32763,#27254,.T.) ;
#39948 = EDGE_CURVE('',#32763,#32764,#10248,.T.) ;
#39949 = EDGE_CURVE('',#32764,#32765,#27255,.T.) ;
#39950 = EDGE_CURVE('',#32765,#32190,#10249,.T.) ;
#39951 = EDGE_CURVE('',#32191,#32766,#10250,.T.) ;
#39952 = EDGE_CURVE('',#32766,#32767,#27256,.T.) ;
#39953 = EDGE_CURVE('',#32767,#32768,#10251,.T.) ;
#39954 = EDGE_CURVE('',#32768,#32769,#10252,.T.) ;
#39955 = EDGE_CURVE('',#32769,#32770,#10253,.T.) ;
#39956 = EDGE_CURVE('',#32770,#32771,#27257,.T.) ;
#39957 = EDGE_CURVE('',#32771,#32772,#10254,.T.) ;
#39958 = EDGE_CURVE('',#32772,#32773,#27258,.T.) ;
#39959 = EDGE_CURVE('',#32773,#32774,#10255,.T.) ;
#39960 = EDGE_CURVE('',#32774,#32775,#27259,.T.) ;
#39961 = EDGE_CURVE('',#32775,#32776,#27260,.T.) ;
#39962 = EDGE_CURVE('',#32776,#32777,#27261,.T.) ;
#39963 = EDGE_CURVE('',#32777,#32778,#10256,.T.) ;
#39964 = EDGE_CURVE('',#32778,#32779,#27262,.T.) ;
#39965 = EDGE_CURVE('',#32779,#32758,#10257,.T.) ;
#39966 = EDGE_CURVE('',#32780,#32781,#10258,.T.) ;
#39967 = EDGE_CURVE('',#32781,#32782,#10259,.T.) ;
#39968 = EDGE_CURVE('',#32782,#32783,#10260,.T.) ;
#39969 = EDGE_CURVE('',#32783,#32784,#10261,.T.) ;
#39970 = EDGE_CURVE('',#32784,#32785,#27263,.T.) ;
#39971 = EDGE_CURVE('',#32785,#32786,#10262,.T.) ;
#39972 = EDGE_CURVE('',#32786,#32787,#10263,.T.) ;
#39973 = EDGE_CURVE('',#32787,#32788,#10264,.T.) ;
#39974 = EDGE_CURVE('',#32788,#32789,#27264,.T.) ;
#39975 = EDGE_CURVE('',#32789,#32780,#10265,.T.) ;
#39976 = EDGE_CURVE('',#32790,#32791,#10266,.T.) ;
#39977 = EDGE_CURVE('',#32791,#32792,#10267,.T.) ;
#39978 = EDGE_CURVE('',#32792,#32793,#10268,.T.) ;
#39979 = EDGE_CURVE('',#32793,#32794,#10269,.T.) ;
#39980 = EDGE_CURVE('',#32794,#32795,#27265,.T.) ;
#39981 = EDGE_CURVE('',#32795,#32796,#10270,.T.) ;
#39982 = EDGE_CURVE('',#32796,#32797,#10271,.T.) ;
#39983 = EDGE_CURVE('',#32797,#32798,#10272,.T.) ;
#39984 = EDGE_CURVE('',#32798,#32799,#27266,.T.) ;
#39985 = EDGE_CURVE('',#32799,#32790,#10273,.T.) ;
#39986 = EDGE_CURVE('',#32800,#32801,#10274,.T.) ;
#39987 = EDGE_CURVE('',#32801,#32802,#10275,.T.) ;
#39988 = EDGE_CURVE('',#32802,#32803,#10276,.T.) ;
#39989 = EDGE_CURVE('',#32803,#32804,#10277,.T.) ;
#39990 = EDGE_CURVE('',#32804,#32805,#10278,.T.) ;
#39991 = EDGE_CURVE('',#32805,#32806,#10279,.T.) ;
#39992 = EDGE_CURVE('',#32807,#32806,#27267,.T.) ;
#39993 = EDGE_CURVE('',#32807,#32808,#10280,.T.) ;
#39994 = EDGE_CURVE('',#32809,#32808,#27268,.T.) ;
#39995 = EDGE_CURVE('',#32809,#32800,#10281,.T.) ;
#39996 = EDGE_CURVE('',#32810,#32811,#10282,.T.) ;
#39997 = EDGE_CURVE('',#32811,#32812,#10283,.T.) ;
#39998 = EDGE_CURVE('',#32812,#32813,#10284,.T.) ;
#39999 = EDGE_CURVE('',#32813,#32810,#10285,.T.) ;
#40000 = EDGE_CURVE('',#32201,#32814,#10286,.T.) ;
#40001 = EDGE_CURVE('',#32814,#32815,#10287,.T.) ;
#40002 = EDGE_CURVE('',#32815,#32202,#10288,.T.) ;
#40003 = EDGE_CURVE('',#32816,#32817,#10289,.T.) ;
#40004 = EDGE_CURVE('',#32817,#32818,#10290,.T.) ;
#40005 = EDGE_CURVE('',#32818,#32819,#10291,.T.) ;
#40006 = EDGE_CURVE('',#32819,#32816,#10292,.T.) ;
#40007 = EDGE_CURVE('',#32820,#32821,#10293,.T.) ;
#40008 = EDGE_CURVE('',#32821,#32822,#10294,.T.) ;
#40009 = EDGE_CURVE('',#32822,#32823,#10295,.T.) ;
#40010 = EDGE_CURVE('',#32823,#32820,#10296,.T.) ;
#40011 = EDGE_CURVE('',#32824,#32825,#10297,.T.) ;
#40012 = EDGE_CURVE('',#32825,#32826,#10298,.T.) ;
#40013 = EDGE_CURVE('',#32826,#32827,#10299,.T.) ;
#40014 = EDGE_CURVE('',#32827,#32824,#10300,.T.) ;
#40015 = EDGE_CURVE('',#32828,#32829,#10301,.T.) ;
#40016 = EDGE_CURVE('',#32828,#32830,#27269,.T.) ;
#40017 = EDGE_CURVE('',#32830,#32831,#10302,.T.) ;
#40018 = EDGE_CURVE('',#32831,#32829,#27270,.T.) ;
#40019 = EDGE_CURVE('',#32830,#32832,#10303,.T.) ;
#40020 = EDGE_CURVE('',#32832,#32833,#10304,.T.) ;
#40021 = EDGE_CURVE('',#32833,#32831,#10305,.T.) ;
#40022 = EDGE_CURVE('',#32832,#32834,#27271,.T.) ;
#40023 = EDGE_CURVE('',#32834,#32835,#10306,.T.) ;
#40024 = EDGE_CURVE('',#32835,#32833,#27272,.T.) ;
#40025 = EDGE_CURVE('',#32834,#32836,#10307,.T.) ;
#40026 = EDGE_CURVE('',#32836,#32837,#10308,.T.) ;
#40027 = EDGE_CURVE('',#32837,#32835,#10309,.T.) ;
#40028 = EDGE_CURVE('',#32836,#32838,#27273,.T.) ;
#40029 = EDGE_CURVE('',#32838,#32839,#10310,.T.) ;
#40030 = EDGE_CURVE('',#32839,#32837,#27274,.T.) ;
#40031 = EDGE_CURVE('',#32838,#32196,#10311,.T.) ;
#40032 = EDGE_CURVE('',#32196,#32840,#10312,.T.) ;
#40033 = EDGE_CURVE('',#32840,#32839,#10313,.T.) ;
#40034 = EDGE_CURVE('',#32197,#32841,#10314,.T.) ;
#40035 = EDGE_CURVE('',#32841,#32840,#27275,.T.) ;
#40036 = EDGE_CURVE('',#32197,#32206,#10315,.T.) ;
#40037 = EDGE_CURVE('',#32192,#32841,#10316,.T.) ;
#40038 = EDGE_CURVE('',#32207,#32842,#10317,.T.) ;
#40039 = EDGE_CURVE('',#32842,#32843,#10318,.T.) ;
#40040 = EDGE_CURVE('',#32843,#32193,#10319,.T.) ;
#40041 = EDGE_CURVE('',#32842,#32844,#27276,.T.) ;
#40042 = EDGE_CURVE('',#32844,#32845,#10320,.T.) ;
#40043 = EDGE_CURVE('',#32845,#32843,#27277,.T.) ;
#40044 = EDGE_CURVE('',#32844,#32846,#10321,.T.) ;
#40045 = EDGE_CURVE('',#32846,#32847,#10322,.T.) ;
#40046 = EDGE_CURVE('',#32847,#32845,#10323,.T.) ;
#40047 = EDGE_CURVE('',#32846,#32848,#27278,.T.) ;
#40048 = EDGE_CURVE('',#32848,#32849,#10324,.T.) ;
#40049 = EDGE_CURVE('',#32849,#32847,#27279,.T.) ;
#40050 = EDGE_CURVE('',#32848,#32850,#10325,.T.) ;
#40051 = EDGE_CURVE('',#32850,#32851,#10326,.T.) ;
#40052 = EDGE_CURVE('',#32851,#32849,#10327,.T.) ;
#40053 = EDGE_CURVE('',#32850,#32852,#27280,.T.) ;
#40054 = EDGE_CURVE('',#32852,#32853,#10328,.T.) ;
#40055 = EDGE_CURVE('',#32853,#32851,#27281,.T.) ;
#40056 = EDGE_CURVE('',#32852,#32854,#10329,.T.) ;
#40057 = EDGE_CURVE('',#32854,#32855,#10330,.T.) ;
#40058 = EDGE_CURVE('',#32855,#32853,#10331,.T.) ;
#40059 = EDGE_CURVE('',#32854,#32856,#27282,.T.) ;
#40060 = EDGE_CURVE('',#32856,#32857,#10332,.T.) ;
#40061 = EDGE_CURVE('',#32857,#32855,#27283,.T.) ;
#40062 = EDGE_CURVE('',#32856,#32858,#10333,.T.) ;
#40063 = EDGE_CURVE('',#32858,#32859,#10334,.T.) ;
#40064 = EDGE_CURVE('',#32859,#32857,#10335,.T.) ;
#40065 = EDGE_CURVE('',#32858,#32860,#27284,.T.) ;
#40066 = EDGE_CURVE('',#32860,#32861,#10336,.T.) ;
#40067 = EDGE_CURVE('',#32861,#32859,#27285,.T.) ;
#40068 = EDGE_CURVE('',#32860,#32862,#10337,.T.) ;
#40069 = EDGE_CURVE('',#32862,#32863,#10338,.T.) ;
#40070 = EDGE_CURVE('',#32863,#32861,#10339,.T.) ;
#40071 = EDGE_CURVE('',#32862,#32864,#27286,.T.) ;
#40072 = EDGE_CURVE('',#32864,#32865,#10340,.T.) ;
#40073 = EDGE_CURVE('',#32865,#32863,#27287,.T.) ;
#40074 = EDGE_CURVE('',#32864,#32866,#27288,.T.) ;
#40075 = EDGE_CURVE('',#32866,#32867,#10341,.T.) ;
#40076 = EDGE_CURVE('',#32867,#32865,#27289,.T.) ;
#40077 = EDGE_CURVE('',#32866,#32868,#27290,.T.) ;
#40078 = EDGE_CURVE('',#32868,#32869,#10342,.T.) ;
#40079 = EDGE_CURVE('',#32869,#32867,#27291,.T.) ;
#40080 = EDGE_CURVE('',#32868,#32870,#10343,.T.) ;
#40081 = EDGE_CURVE('',#32870,#32871,#10344,.T.) ;
#40082 = EDGE_CURVE('',#32871,#32869,#10345,.T.) ;
#40083 = EDGE_CURVE('',#32870,#32872,#27292,.T.) ;
#40084 = EDGE_CURVE('',#32872,#32873,#10346,.T.) ;
#40085 = EDGE_CURVE('',#32873,#32871,#27293,.T.) ;
#40086 = EDGE_CURVE('',#32872,#32874,#10347,.T.) ;
#40087 = EDGE_CURVE('',#32874,#32875,#10348,.T.) ;
#40088 = EDGE_CURVE('',#32875,#32873,#10349,.T.) ;
#40089 = EDGE_CURVE('',#32874,#32876,#27294,.T.) ;
#40090 = EDGE_CURVE('',#32876,#32877,#10350,.T.) ;
#40091 = EDGE_CURVE('',#32877,#32875,#27295,.T.) ;
#40092 = EDGE_CURVE('',#32876,#32828,#10351,.T.) ;
#40093 = EDGE_CURVE('',#32829,#32877,#10352,.T.) ;
#40094 = EDGE_CURVE('',#32878,#32879,#27296,.T.) ;
#40095 = EDGE_CURVE('',#32879,#32880,#10353,.T.) ;
#40096 = EDGE_CURVE('',#32880,#32881,#27297,.T.) ;
#40097 = EDGE_CURVE('',#32881,#32882,#10354,.T.) ;
#40098 = EDGE_CURVE('',#32882,#32883,#10355,.T.) ;
#40099 = EDGE_CURVE('',#32883,#32884,#10356,.T.) ;
#40100 = EDGE_CURVE('',#32884,#32885,#27298,.T.) ;
#40101 = EDGE_CURVE('',#32885,#32886,#10357,.T.) ;
#40102 = EDGE_CURVE('',#32886,#32887,#10358,.T.) ;
#40103 = EDGE_CURVE('',#32887,#32888,#10359,.T.) ;
#40104 = EDGE_CURVE('',#32888,#32889,#27299,.T.) ;
#40105 = EDGE_CURVE('',#32889,#32890,#10360,.T.) ;
#40106 = EDGE_CURVE('',#32890,#32891,#27300,.T.) ;
#40107 = EDGE_CURVE('',#32891,#32892,#10361,.T.) ;
#40108 = EDGE_CURVE('',#32892,#32893,#10362,.T.) ;
#40109 = EDGE_CURVE('',#32893,#32198,#10363,.T.) ;
#40110 = EDGE_CURVE('',#32198,#32894,#10364,.T.) ;
#40111 = EDGE_CURVE('',#32894,#32878,#10365,.T.) ;
#40112 = EDGE_CURVE('',#32895,#32896,#10366,.T.) ;
#40113 = EDGE_CURVE('',#32895,#32897,#27301,.T.) ;
#40114 = EDGE_CURVE('',#32897,#32898,#10367,.T.) ;
#40115 = EDGE_CURVE('',#32898,#32899,#27302,.T.) ;
#40116 = EDGE_CURVE('',#32899,#32900,#10368,.T.) ;
#40117 = EDGE_CURVE('',#32900,#32901,#27303,.T.) ;
#40118 = EDGE_CURVE('',#32901,#32902,#10369,.T.) ;
#40119 = EDGE_CURVE('',#32902,#32896,#27304,.T.) ;
#40120 = EDGE_CURVE('',#32822,#32809,#27305,.T.) ;
#40121 = EDGE_CURVE('',#32800,#32821,#27306,.T.) ;
#40122 = EDGE_CURVE('',#32823,#32816,#27307,.T.) ;
#40123 = EDGE_CURVE('',#32817,#32822,#27308,.T.) ;
#40124 = EDGE_CURVE('',#32823,#32903,#27309,.T.) ;
#40125 = EDGE_CURVE('',#32903,#32816,#27310,.T.) ;
#40126 = EDGE_CURVE('',#32800,#32826,#27311,.T.) ;
#40127 = EDGE_CURVE('',#32826,#32821,#27312,.T.) ;
#40128 = EDGE_CURVE('',#32817,#32808,#27313,.T.) ;
#40129 = EDGE_CURVE('',#32199,#32819,#27314,.T.) ;
#40130 = EDGE_CURVE('',#32200,#32904,#300,.T.) ;
#40131 = EDGE_CURVE('',#32903,#32904,#10370,.T.) ;
#40132 = EDGE_CURVE('',#32905,#32903,#301,.T.) ;
#40133 = EDGE_CURVE('',#32905,#32906,#302,.T.) ;
#40134 = EDGE_CURVE('',#32425,#32906,#10371,.T.) ;
#40135 = EDGE_CURVE('',#32820,#32424,#27315,.T.) ;
#40136 = EDGE_CURVE('',#32827,#32820,#27316,.T.) ;
#40137 = EDGE_CURVE('',#32801,#32825,#27317,.T.) ;
#40138 = EDGE_CURVE('',#32818,#32807,#27318,.T.) ;
#40139 = EDGE_CURVE('',#32819,#32201,#27319,.T.) ;
#40140 = EDGE_CURVE('',#32814,#32818,#27320,.T.) ;
#40141 = EDGE_CURVE('',#32827,#32433,#27321,.T.) ;
#40142 = EDGE_CURVE('',#32801,#32440,#27322,.T.) ;
#40143 = EDGE_CURVE('',#32439,#32825,#27323,.T.) ;
#40144 = EDGE_CURVE('',#32814,#32806,#27324,.T.) ;
#40145 = EDGE_CURVE('',#32824,#32432,#27325,.T.) ;
#40146 = EDGE_CURVE('',#32441,#32824,#27326,.T.) ;
#40147 = EDGE_CURVE('',#32907,#32440,#10372,.T.) ;
#40148 = EDGE_CURVE('',#32802,#32907,#27327,.T.) ;
#40149 = EDGE_CURVE('',#32815,#32805,#27328,.T.) ;
#40150 = EDGE_CURVE('',#32202,#32810,#27329,.T.) ;
#40151 = EDGE_CURVE('',#32811,#32815,#27330,.T.) ;
#40152 = EDGE_CURVE('',#32428,#32810,#27331,.T.) ;
#40153 = EDGE_CURVE('',#32441,#32432,#27332,.T.) ;
#40154 = EDGE_CURVE('',#32446,#32443,#27333,.T.) ;
#40155 = EDGE_CURVE('',#32443,#32444,#27334,.T.) ;
#40156 = EDGE_CURVE('',#32907,#32533,#27335,.T.) ;
#40157 = EDGE_CURVE('',#32908,#32907,#27336,.T.) ;
#40158 = EDGE_CURVE('',#32802,#32908,#27337,.T.) ;
#40159 = EDGE_CURVE('',#32811,#32805,#27338,.T.) ;
#40160 = EDGE_CURVE('',#32429,#32813,#27339,.T.) ;
#40161 = EDGE_CURVE('',#32442,#32431,#27340,.T.) ;
#40162 = EDGE_CURVE('',#32456,#32442,#27341,.T.) ;
#40163 = EDGE_CURVE('',#32908,#32532,#27342,.T.) ;
#40164 = EDGE_CURVE('',#32909,#32908,#10373,.T.) ;
#40165 = EDGE_CURVE('',#32803,#32909,#27343,.T.) ;
#40166 = EDGE_CURVE('',#32812,#32804,#27344,.T.) ;
#40167 = EDGE_CURVE('',#32813,#32438,#27345,.T.) ;
#40168 = EDGE_CURVE('',#32435,#32812,#27346,.T.) ;
#40169 = EDGE_CURVE('',#32429,#32438,#27347,.T.) ;
#40170 = EDGE_CURVE('',#32457,#32431,#27348,.T.) ;
#40171 = EDGE_CURVE('',#32909,#32531,#27349,.T.) ;
#40172 = EDGE_CURVE('',#32910,#32909,#27350,.T.) ;
#40173 = EDGE_CURVE('',#32803,#32910,#27351,.T.) ;
#40174 = EDGE_CURVE('',#32434,#32804,#27352,.T.) ;
#40175 = EDGE_CURVE('',#32430,#32437,#27353,.T.) ;
#40176 = EDGE_CURVE('',#32458,#32430,#27354,.T.) ;
#40177 = EDGE_CURVE('',#32910,#32530,#27355,.T.) ;
#40178 = EDGE_CURVE('',#32434,#32910,#10374,.T.) ;
#40179 = EDGE_CURVE('',#32459,#32437,#27356,.T.) ;
#40180 = EDGE_CURVE('',#32436,#32389,#27357,.T.) ;
#40181 = EDGE_CURVE('',#32391,#32436,#27358,.T.) ;
#40182 = EDGE_CURVE('',#32786,#32546,#27359,.T.) ;
#40183 = EDGE_CURVE('',#32544,#32786,#27360,.T.) ;
#40184 = EDGE_CURVE('',#32542,#32785,#27361,.T.) ;
#40185 = EDGE_CURVE('',#32787,#32548,#27362,.T.) ;
#40186 = EDGE_CURVE('',#32540,#32784,#27363,.T.) ;
#40187 = EDGE_CURVE('',#32787,#32550,#27364,.T.) ;
#40188 = EDGE_CURVE('',#32538,#32783,#27365,.T.) ;
#40189 = EDGE_CURVE('',#32788,#32552,#27366,.T.) ;
#40190 = EDGE_CURVE('',#32535,#32783,#27367,.T.) ;
#40191 = EDGE_CURVE('',#32789,#32554,#27368,.T.) ;
#40192 = EDGE_CURVE('',#32495,#32782,#27369,.T.) ;
#40193 = EDGE_CURVE('',#32780,#32556,#27370,.T.) ;
#40194 = EDGE_CURVE('',#32455,#32782,#27371,.T.) ;
#40195 = EDGE_CURVE('',#32780,#32558,#27372,.T.) ;
#40196 = EDGE_CURVE('',#32448,#32781,#27373,.T.) ;
#40197 = EDGE_CURVE('',#32781,#32450,#27374,.T.) ;
#40198 = EDGE_CURVE('',#32547,#32797,#27375,.T.) ;
#40199 = EDGE_CURVE('',#32797,#32545,#27376,.T.) ;
#40200 = EDGE_CURVE('',#32798,#32543,#27377,.T.) ;
#40201 = EDGE_CURVE('',#32549,#32796,#27378,.T.) ;
#40202 = EDGE_CURVE('',#32799,#32541,#27379,.T.) ;
#40203 = EDGE_CURVE('',#32551,#32796,#27380,.T.) ;
#40204 = EDGE_CURVE('',#32790,#32539,#27381,.T.) ;
#40205 = EDGE_CURVE('',#32553,#32795,#27382,.T.) ;
#40206 = EDGE_CURVE('',#32790,#32534,#27383,.T.) ;
#40207 = EDGE_CURVE('',#32555,#32794,#27384,.T.) ;
#40208 = EDGE_CURVE('',#32791,#32445,#27385,.T.) ;
#40209 = EDGE_CURVE('',#32557,#32793,#27386,.T.) ;
#40210 = EDGE_CURVE('',#32791,#32447,#27387,.T.) ;
#40211 = EDGE_CURVE('',#32559,#32793,#27388,.T.) ;
#40212 = EDGE_CURVE('',#32792,#32449,#27389,.T.) ;
#40213 = EDGE_CURVE('',#32451,#32792,#27390,.T.) ;
#40214 = EDGE_CURVE('',#32854,#32887,#27391,.T.) ;
#40215 = EDGE_CURVE('',#32888,#32852,#27392,.T.) ;
#40216 = EDGE_CURVE('',#32889,#32850,#27393,.T.) ;
#40217 = EDGE_CURVE('',#32856,#32887,#27394,.T.) ;
#40218 = EDGE_CURVE('',#32890,#32848,#27395,.T.) ;
#40219 = EDGE_CURVE('',#32858,#32886,#27396,.T.) ;
#40220 = EDGE_CURVE('',#32891,#32846,#27397,.T.) ;
#40221 = EDGE_CURVE('',#32860,#32886,#27398,.T.) ;
#40222 = EDGE_CURVE('',#32892,#32844,#27399,.T.) ;
#40223 = EDGE_CURVE('',#32862,#32885,#27400,.T.) ;
#40224 = EDGE_CURVE('',#32892,#32842,#27401,.T.) ;
#40225 = EDGE_CURVE('',#32864,#32885,#27402,.T.) ;
#40226 = EDGE_CURVE('',#32893,#32207,#27403,.T.) ;
#40227 = EDGE_CURVE('',#32866,#32884,#27404,.T.) ;
#40228 = EDGE_CURVE('',#32893,#32206,#27405,.T.) ;
#40229 = EDGE_CURVE('',#32868,#32884,#27406,.T.) ;
#40230 = EDGE_CURVE('',#32870,#32883,#27407,.T.) ;
#40231 = EDGE_CURVE('',#32872,#32883,#27408,.T.) ;
#40232 = EDGE_CURVE('',#32894,#32838,#27409,.T.) ;
#40233 = EDGE_CURVE('',#32874,#32882,#27410,.T.) ;
#40234 = EDGE_CURVE('',#32894,#32836,#27411,.T.) ;
#40235 = EDGE_CURVE('',#32876,#32882,#27412,.T.) ;
#40236 = EDGE_CURVE('',#32878,#32834,#27413,.T.) ;
#40237 = EDGE_CURVE('',#32828,#32881,#27414,.T.) ;
#40238 = EDGE_CURVE('',#32879,#32832,#27415,.T.) ;
#40239 = EDGE_CURVE('',#32830,#32880,#27416,.T.) ;
#40240 = EDGE_CURVE('',#32849,#32768,#27417,.T.) ;
#40241 = EDGE_CURVE('',#32769,#32851,#27418,.T.) ;
#40242 = EDGE_CURVE('',#32847,#32768,#27419,.T.) ;
#40243 = EDGE_CURVE('',#32769,#32853,#27420,.T.) ;
#40244 = EDGE_CURVE('',#32845,#32767,#27421,.T.) ;
#40245 = EDGE_CURVE('',#32770,#32855,#27422,.T.) ;
#40246 = EDGE_CURVE('',#32843,#32766,#27423,.T.) ;
#40247 = EDGE_CURVE('',#32771,#32857,#27424,.T.) ;
#40248 = EDGE_CURVE('',#32772,#32859,#27425,.T.) ;
#40249 = EDGE_CURVE('',#32773,#32861,#27426,.T.) ;
#40250 = EDGE_CURVE('',#32841,#32765,#27427,.T.) ;
#40251 = EDGE_CURVE('',#32774,#32863,#27428,.T.) ;
#40252 = EDGE_CURVE('',#32840,#32764,#27429,.T.) ;
#40253 = EDGE_CURVE('',#32775,#32865,#27430,.T.) ;
#40254 = EDGE_CURVE('',#32839,#32763,#27431,.T.) ;
#40255 = EDGE_CURVE('',#32776,#32867,#27432,.T.) ;
#40256 = EDGE_CURVE('',#32837,#32762,#27433,.T.) ;
#40257 = EDGE_CURVE('',#32777,#32869,#27434,.T.) ;
#40258 = EDGE_CURVE('',#32835,#32761,#27435,.T.) ;
#40259 = EDGE_CURVE('',#32778,#32871,#27436,.T.) ;
#40260 = EDGE_CURVE('',#32833,#32761,#27437,.T.) ;
#40261 = EDGE_CURVE('',#32779,#32873,#27438,.T.) ;
#40262 = EDGE_CURVE('',#32831,#32760,#27439,.T.) ;
#40263 = EDGE_CURVE('',#32758,#32875,#27440,.T.) ;
#40264 = EDGE_CURVE('',#32829,#32760,#27441,.T.) ;
#40265 = EDGE_CURVE('',#32759,#32877,#27442,.T.) ;
#40266 = EDGE_CURVE('',#32911,#32912,#10375,.T.) ;
#40267 = EDGE_CURVE('',#32912,#32913,#10376,.T.) ;
#40268 = EDGE_CURVE('',#32913,#32914,#10377,.T.) ;
#40269 = EDGE_CURVE('',#32914,#32911,#10378,.T.) ;
#40270 = EDGE_CURVE('',#32915,#32916,#10379,.T.) ;
#40271 = EDGE_CURVE('',#32916,#32917,#10380,.T.) ;
#40272 = EDGE_CURVE('',#32917,#32918,#10381,.T.) ;
#40273 = EDGE_CURVE('',#32918,#32915,#10382,.T.) ;
#40274 = EDGE_CURVE('',#32919,#32920,#10383,.T.) ;
#40275 = EDGE_CURVE('',#32920,#32921,#10384,.T.) ;
#40276 = EDGE_CURVE('',#32921,#32922,#10385,.T.) ;
#40277 = EDGE_CURVE('',#32922,#32919,#10386,.T.) ;
#40278 = EDGE_CURVE('',#32923,#32924,#10387,.T.) ;
#40279 = EDGE_CURVE('',#32924,#32925,#10388,.T.) ;
#40280 = EDGE_CURVE('',#32925,#32926,#10389,.T.) ;
#40281 = EDGE_CURVE('',#32926,#32923,#10390,.T.) ;
#40282 = EDGE_CURVE('',#32927,#32928,#10391,.T.) ;
#40283 = EDGE_CURVE('',#32928,#32929,#10392,.T.) ;
#40284 = EDGE_CURVE('',#32930,#32929,#10393,.T.) ;
#40285 = EDGE_CURVE('',#32930,#32927,#10394,.T.) ;
#40286 = EDGE_CURVE('',#32931,#32932,#10395,.T.) ;
#40287 = EDGE_CURVE('',#32932,#32425,#27443,.T.) ;
#40288 = EDGE_CURVE('',#32906,#32933,#27444,.T.) ;
#40289 = EDGE_CURVE('',#32933,#32934,#10396,.T.) ;
#40290 = EDGE_CURVE('',#32934,#32931,#10397,.T.) ;
#40291 = EDGE_CURVE('',#32935,#32936,#10398,.T.) ;
#40292 = EDGE_CURVE('',#32936,#32205,#27445,.T.) ;
#40293 = EDGE_CURVE('',#32204,#32937,#27446,.T.) ;
#40294 = EDGE_CURVE('',#32937,#32938,#10399,.T.) ;
#40295 = EDGE_CURVE('',#32938,#32935,#10400,.T.) ;
#40296 = EDGE_CURVE('',#32904,#32912,#27447,.T.) ;
#40297 = EDGE_CURVE('',#32911,#32905,#27448,.T.) ;
#40298 = EDGE_CURVE('',#32929,#32427,#27449,.T.) ;
#40299 = EDGE_CURVE('',#32426,#32930,#27450,.T.) ;
#40300 = EDGE_CURVE('',#32939,#32940,#10401,.T.) ;
#40301 = EDGE_CURVE('',#32940,#32941,#10402,.T.) ;
#40302 = EDGE_CURVE('',#32941,#32942,#10403,.T.) ;
#40303 = EDGE_CURVE('',#32942,#32939,#10404,.T.) ;
#40304 = EDGE_CURVE('',#32943,#32944,#10405,.T.) ;
#40305 = EDGE_CURVE('',#32944,#32898,#10406,.T.) ;
#40306 = EDGE_CURVE('',#32897,#32943,#10407,.T.) ;
#40307 = EDGE_CURVE('',#32901,#32945,#10408,.T.) ;
#40308 = EDGE_CURVE('',#32945,#32946,#10409,.T.) ;
#40309 = EDGE_CURVE('',#32946,#32902,#10410,.T.) ;
#40310 = EDGE_CURVE('',#32947,#32948,#10411,.T.) ;
#40311 = EDGE_CURVE('',#32948,#32949,#10412,.T.) ;
#40312 = EDGE_CURVE('',#32949,#32950,#10413,.T.) ;
#40313 = EDGE_CURVE('',#32950,#32947,#10414,.T.) ;
#40314 = EDGE_CURVE('',#32951,#32952,#10415,.T.) ;
#40315 = EDGE_CURVE('',#32952,#32953,#10416,.T.) ;
#40316 = EDGE_CURVE('',#32953,#32954,#10417,.T.) ;
#40317 = EDGE_CURVE('',#32954,#32951,#10418,.T.) ;
#40318 = EDGE_CURVE('',#32955,#32956,#10419,.T.) ;
#40319 = EDGE_CURVE('',#32956,#32895,#10420,.T.) ;
#40320 = EDGE_CURVE('',#32896,#32955,#10421,.T.) ;
#40321 = EDGE_CURVE('',#32899,#32957,#10422,.T.) ;
#40322 = EDGE_CURVE('',#32957,#32958,#10423,.T.) ;
#40323 = EDGE_CURVE('',#32958,#32900,#10424,.T.) ;
#40324 = EDGE_CURVE('',#32959,#32960,#10425,.T.) ;
#40325 = EDGE_CURVE('',#32960,#32961,#10426,.T.) ;
#40326 = EDGE_CURVE('',#32961,#32962,#10427,.T.) ;
#40327 = EDGE_CURVE('',#32962,#32959,#10428,.T.) ;
#40328 = EDGE_CURVE('',#32963,#32964,#10429,.T.) ;
#40329 = EDGE_CURVE('',#32964,#32965,#10430,.T.) ;
#40330 = EDGE_CURVE('',#32965,#32966,#10431,.T.) ;
#40331 = EDGE_CURVE('',#32966,#32963,#10432,.T.) ;
#40332 = EDGE_CURVE('',#32967,#32968,#10433,.T.) ;
#40333 = EDGE_CURVE('',#32968,#32969,#10434,.T.) ;
#40334 = EDGE_CURVE('',#32969,#32970,#10435,.T.) ;
#40335 = EDGE_CURVE('',#32970,#32967,#10436,.T.) ;
#40336 = EDGE_CURVE('',#32971,#32972,#10437,.T.) ;
#40337 = EDGE_CURVE('',#32972,#32973,#10438,.T.) ;
#40338 = EDGE_CURVE('',#32973,#32974,#10439,.T.) ;
#40339 = EDGE_CURVE('',#32974,#32971,#10440,.T.) ;
#40340 = EDGE_CURVE('',#32961,#32923,#27451,.T.) ;
#40341 = EDGE_CURVE('',#32962,#32926,#27452,.T.) ;
#40342 = EDGE_CURVE('',#32923,#32928,#27453,.T.) ;
#40343 = EDGE_CURVE('',#32927,#32924,#27454,.T.) ;
#40344 = EDGE_CURVE('',#32962,#32919,#27455,.T.) ;
#40345 = EDGE_CURVE('',#32919,#32926,#27456,.T.) ;
#40346 = EDGE_CURVE('',#32924,#32964,#27457,.T.) ;
#40347 = EDGE_CURVE('',#32925,#32963,#27458,.T.) ;
#40348 = EDGE_CURVE('',#32920,#32925,#27459,.T.) ;
#40349 = EDGE_CURVE('',#32959,#32922,#27460,.T.) ;
#40350 = EDGE_CURVE('',#32920,#32963,#27461,.T.) ;
#40351 = EDGE_CURVE('',#32959,#32915,#27462,.T.) ;
#40352 = EDGE_CURVE('',#32915,#32922,#27463,.T.) ;
#40353 = EDGE_CURVE('',#32921,#32966,#27464,.T.) ;
#40354 = EDGE_CURVE('',#32916,#32921,#27465,.T.) ;
#40355 = EDGE_CURVE('',#32918,#32960,#27466,.T.) ;
#40356 = EDGE_CURVE('',#32916,#32966,#27467,.T.) ;
#40357 = EDGE_CURVE('',#32913,#32918,#27468,.T.) ;
#40358 = EDGE_CURVE('',#32917,#32914,#27469,.T.) ;
#40359 = EDGE_CURVE('',#32965,#32917,#27470,.T.) ;
#40360 = EDGE_CURVE('',#32969,#32939,#27471,.T.) ;
#40361 = EDGE_CURVE('',#32970,#32942,#27472,.T.) ;
#40362 = EDGE_CURVE('',#32939,#32944,#27473,.T.) ;
#40363 = EDGE_CURVE('',#32943,#32940,#27474,.T.) ;
#40364 = EDGE_CURVE('',#32970,#32953,#27475,.T.) ;
#40365 = EDGE_CURVE('',#32953,#32942,#27476,.T.) ;
#40366 = EDGE_CURVE('',#32940,#32972,#27477,.T.) ;
#40367 = EDGE_CURVE('',#32941,#32971,#27478,.T.) ;
#40368 = EDGE_CURVE('',#32954,#32941,#27479,.T.) ;
#40369 = EDGE_CURVE('',#32967,#32952,#27480,.T.) ;
#40370 = EDGE_CURVE('',#32954,#32971,#27481,.T.) ;
#40371 = EDGE_CURVE('',#32967,#32947,#27482,.T.) ;
#40372 = EDGE_CURVE('',#32947,#32952,#27483,.T.) ;
#40373 = EDGE_CURVE('',#32951,#32974,#27484,.T.) ;
#40374 = EDGE_CURVE('',#32948,#32951,#27485,.T.) ;
#40375 = EDGE_CURVE('',#32950,#32968,#27486,.T.) ;
#40376 = EDGE_CURVE('',#32948,#32974,#27487,.T.) ;
#40377 = EDGE_CURVE('',#32945,#32950,#27488,.T.) ;
#40378 = EDGE_CURVE('',#32949,#32946,#27489,.T.) ;
#40379 = EDGE_CURVE('',#32973,#32949,#27490,.T.) ;
#40380 = EDGE_CURVE('',#32937,#32929,#27491,.T.) ;
#40381 = EDGE_CURVE('',#32938,#32928,#27492,.T.) ;
#40382 = EDGE_CURVE('',#32938,#32961,#27493,.T.) ;
#40383 = EDGE_CURVE('',#32935,#32960,#27494,.T.) ;
#40384 = EDGE_CURVE('',#32935,#32913,#27495,.T.) ;
#40385 = EDGE_CURVE('',#32936,#32912,#27496,.T.) ;
#40386 = EDGE_CURVE('',#32933,#32911,#27497,.T.) ;
#40387 = EDGE_CURVE('',#32934,#32914,#27498,.T.) ;
#40388 = EDGE_CURVE('',#32934,#32965,#27499,.T.) ;
#40389 = EDGE_CURVE('',#32931,#32964,#27500,.T.) ;
#40390 = EDGE_CURVE('',#32931,#32927,#27501,.T.) ;
#40391 = EDGE_CURVE('',#32932,#32930,#27502,.T.) ;
#40392 = EDGE_CURVE('',#32957,#32944,#27503,.T.) ;
#40393 = EDGE_CURVE('',#32957,#32969,#27504,.T.) ;
#40394 = EDGE_CURVE('',#32958,#32968,#27505,.T.) ;
#40395 = EDGE_CURVE('',#32958,#32945,#27506,.T.) ;
#40396 = EDGE_CURVE('',#32943,#32956,#27507,.T.) ;
#40397 = EDGE_CURVE('',#32972,#32956,#27508,.T.) ;
#40398 = EDGE_CURVE('',#32973,#32955,#27509,.T.) ;
#40399 = EDGE_CURVE('',#32955,#32946,#27510,.T.) ;
#40400 = EDGE_CURVE('',#32975,#32976,#10441,.T.) ;
#40401 = EDGE_CURVE('',#32976,#32977,#10442,.T.) ;
#40402 = EDGE_CURVE('',#32977,#32978,#10443,.T.) ;
#40403 = EDGE_CURVE('',#32978,#32979,#10444,.T.) ;
#40404 = EDGE_CURVE('',#32979,#32980,#10445,.T.) ;
#40405 = EDGE_CURVE('',#32980,#32981,#10446,.T.) ;
#40406 = EDGE_CURVE('',#32982,#32981,#27511,.T.) ;
#40407 = EDGE_CURVE('',#32982,#32983,#10447,.T.) ;
#40408 = EDGE_CURVE('',#32984,#32983,#27512,.T.) ;
#40409 = EDGE_CURVE('',#32984,#32975,#10448,.T.) ;
#40410 = EDGE_CURVE('',#32985,#32986,#10449,.T.) ;
#40411 = EDGE_CURVE('',#32986,#32987,#10450,.T.) ;
#40412 = EDGE_CURVE('',#32987,#32988,#10451,.T.) ;
#40413 = EDGE_CURVE('',#32988,#32989,#10452,.T.) ;
#40414 = EDGE_CURVE('',#32989,#32990,#10453,.T.) ;
#40415 = EDGE_CURVE('',#32990,#32991,#10454,.T.) ;
#40416 = EDGE_CURVE('',#32992,#32991,#27513,.T.) ;
#40417 = EDGE_CURVE('',#32992,#32993,#10455,.T.) ;
#40418 = EDGE_CURVE('',#32994,#32993,#27514,.T.) ;
#40419 = EDGE_CURVE('',#32994,#32985,#10456,.T.) ;
#40420 = EDGE_CURVE('',#32995,#32996,#10457,.T.) ;
#40421 = EDGE_CURVE('',#32996,#32997,#10458,.T.) ;
#40422 = EDGE_CURVE('',#32997,#32998,#10459,.T.) ;
#40423 = EDGE_CURVE('',#32998,#32999,#10460,.T.) ;
#40424 = EDGE_CURVE('',#32999,#33000,#10461,.T.) ;
#40425 = EDGE_CURVE('',#33000,#33001,#10462,.T.) ;
#40426 = EDGE_CURVE('',#33002,#33001,#27515,.T.) ;
#40427 = EDGE_CURVE('',#33002,#33003,#10463,.T.) ;
#40428 = EDGE_CURVE('',#33004,#33003,#27516,.T.) ;
#40429 = EDGE_CURVE('',#33004,#32995,#10464,.T.) ;
#40430 = EDGE_CURVE('',#33005,#33006,#10465,.T.) ;
#40431 = EDGE_CURVE('',#33006,#33007,#10466,.T.) ;
#40432 = EDGE_CURVE('',#33007,#33008,#10467,.T.) ;
#40433 = EDGE_CURVE('',#33008,#33009,#10468,.T.) ;
#40434 = EDGE_CURVE('',#33009,#33010,#10469,.T.) ;
#40435 = EDGE_CURVE('',#33010,#33011,#10470,.T.) ;
#40436 = EDGE_CURVE('',#33012,#33011,#27517,.T.) ;
#40437 = EDGE_CURVE('',#33012,#33013,#10471,.T.) ;
#40438 = EDGE_CURVE('',#33014,#33013,#27518,.T.) ;
#40439 = EDGE_CURVE('',#33014,#33005,#10472,.T.) ;
#40440 = EDGE_CURVE('',#33015,#33016,#10473,.T.) ;
#40441 = EDGE_CURVE('',#33016,#33017,#10474,.T.) ;
#40442 = EDGE_CURVE('',#33017,#33018,#10475,.T.) ;
#40443 = EDGE_CURVE('',#33018,#33019,#10476,.T.) ;
#40444 = EDGE_CURVE('',#33019,#33020,#10477,.T.) ;
#40445 = EDGE_CURVE('',#33020,#33021,#10478,.T.) ;
#40446 = EDGE_CURVE('',#33022,#33021,#27519,.T.) ;
#40447 = EDGE_CURVE('',#33022,#33023,#10479,.T.) ;
#40448 = EDGE_CURVE('',#33024,#33023,#27520,.T.) ;
#40449 = EDGE_CURVE('',#33024,#33015,#10480,.T.) ;
#40450 = EDGE_CURVE('',#33025,#33026,#10481,.T.) ;
#40451 = EDGE_CURVE('',#33026,#33027,#10482,.T.) ;
#40452 = EDGE_CURVE('',#33027,#33028,#10483,.T.) ;
#40453 = EDGE_CURVE('',#33028,#33029,#10484,.T.) ;
#40454 = EDGE_CURVE('',#33029,#33030,#10485,.T.) ;
#40455 = EDGE_CURVE('',#33030,#33031,#10486,.T.) ;
#40456 = EDGE_CURVE('',#33032,#33031,#27521,.T.) ;
#40457 = EDGE_CURVE('',#33032,#33033,#10487,.T.) ;
#40458 = EDGE_CURVE('',#33034,#33033,#27522,.T.) ;
#40459 = EDGE_CURVE('',#33034,#33025,#10488,.T.) ;
#40460 = EDGE_CURVE('',#33035,#33036,#10489,.T.) ;
#40461 = EDGE_CURVE('',#33036,#33037,#10490,.T.) ;
#40462 = EDGE_CURVE('',#33037,#33038,#10491,.T.) ;
#40463 = EDGE_CURVE('',#33038,#33039,#10492,.T.) ;
#40464 = EDGE_CURVE('',#33039,#33040,#10493,.T.) ;
#40465 = EDGE_CURVE('',#33040,#33041,#10494,.T.) ;
#40466 = EDGE_CURVE('',#33042,#33041,#27523,.T.) ;
#40467 = EDGE_CURVE('',#33042,#33043,#10495,.T.) ;
#40468 = EDGE_CURVE('',#33044,#33043,#27524,.T.) ;
#40469 = EDGE_CURVE('',#33044,#33035,#10496,.T.) ;
#40470 = EDGE_CURVE('',#33045,#33046,#10497,.T.) ;
#40471 = EDGE_CURVE('',#33046,#33047,#10498,.T.) ;
#40472 = EDGE_CURVE('',#33047,#33048,#10499,.T.) ;
#40473 = EDGE_CURVE('',#33048,#33049,#10500,.T.) ;
#40474 = EDGE_CURVE('',#33049,#33050,#10501,.T.) ;
#40475 = EDGE_CURVE('',#33050,#33051,#10502,.T.) ;
#40476 = EDGE_CURVE('',#33052,#33051,#27525,.T.) ;
#40477 = EDGE_CURVE('',#33052,#33053,#10503,.T.) ;
#40478 = EDGE_CURVE('',#33054,#33053,#27526,.T.) ;
#40479 = EDGE_CURVE('',#33054,#33045,#10504,.T.) ;
#40480 = EDGE_CURVE('',#33055,#33056,#10505,.T.) ;
#40481 = EDGE_CURVE('',#33056,#33057,#10506,.T.) ;
#40482 = EDGE_CURVE('',#33057,#33058,#10507,.T.) ;
#40483 = EDGE_CURVE('',#33058,#33059,#10508,.T.) ;
#40484 = EDGE_CURVE('',#33059,#33060,#10509,.T.) ;
#40485 = EDGE_CURVE('',#33060,#33061,#10510,.T.) ;
#40486 = EDGE_CURVE('',#33062,#33061,#27527,.T.) ;
#40487 = EDGE_CURVE('',#33062,#33063,#10511,.T.) ;
#40488 = EDGE_CURVE('',#33064,#33063,#27528,.T.) ;
#40489 = EDGE_CURVE('',#33064,#33055,#10512,.T.) ;
#40490 = EDGE_CURVE('',#33065,#33066,#10513,.T.) ;
#40491 = EDGE_CURVE('',#33066,#33067,#10514,.T.) ;
#40492 = EDGE_CURVE('',#33067,#33068,#10515,.T.) ;
#40493 = EDGE_CURVE('',#33068,#33065,#10516,.T.) ;
#40494 = EDGE_CURVE('',#32164,#33069,#10517,.T.) ;
#40495 = EDGE_CURVE('',#33069,#33070,#10518,.T.) ;
#40496 = EDGE_CURVE('',#33070,#32165,#10519,.T.) ;
#40497 = EDGE_CURVE('',#33071,#33072,#10520,.T.) ;
#40498 = EDGE_CURVE('',#33072,#33073,#10521,.T.) ;
#40499 = EDGE_CURVE('',#33073,#33074,#10522,.T.) ;
#40500 = EDGE_CURVE('',#33074,#33071,#10523,.T.) ;
#40501 = EDGE_CURVE('',#33075,#33076,#10524,.T.) ;
#40502 = EDGE_CURVE('',#33076,#33077,#10525,.T.) ;
#40503 = EDGE_CURVE('',#33077,#33078,#10526,.T.) ;
#40504 = EDGE_CURVE('',#33078,#33075,#10527,.T.) ;
#40505 = EDGE_CURVE('',#33079,#33080,#10528,.T.) ;
#40506 = EDGE_CURVE('',#33080,#33081,#10529,.T.) ;
#40507 = EDGE_CURVE('',#33081,#33082,#10530,.T.) ;
#40508 = EDGE_CURVE('',#33082,#33079,#10531,.T.) ;
#40509 = EDGE_CURVE('',#33083,#33084,#10532,.T.) ;
#40510 = EDGE_CURVE('',#33084,#33085,#10533,.T.) ;
#40511 = EDGE_CURVE('',#33085,#33086,#10534,.T.) ;
#40512 = EDGE_CURVE('',#33086,#33083,#10535,.T.) ;
#40513 = EDGE_CURVE('',#32113,#33087,#10536,.T.) ;
#40514 = EDGE_CURVE('',#33087,#33088,#10537,.T.) ;
#40515 = EDGE_CURVE('',#33088,#32114,#10538,.T.) ;
#40516 = EDGE_CURVE('',#33089,#33090,#10539,.T.) ;
#40517 = EDGE_CURVE('',#33090,#33091,#10540,.T.) ;
#40518 = EDGE_CURVE('',#33091,#33092,#10541,.T.) ;
#40519 = EDGE_CURVE('',#33092,#33089,#10542,.T.) ;
#40520 = EDGE_CURVE('',#33093,#33094,#10543,.T.) ;
#40521 = EDGE_CURVE('',#33094,#33095,#10544,.T.) ;
#40522 = EDGE_CURVE('',#33095,#33096,#10545,.T.) ;
#40523 = EDGE_CURVE('',#33096,#33093,#10546,.T.) ;
#40524 = EDGE_CURVE('',#33097,#33098,#10547,.T.) ;
#40525 = EDGE_CURVE('',#33098,#33099,#10548,.T.) ;
#40526 = EDGE_CURVE('',#33099,#33100,#10549,.T.) ;
#40527 = EDGE_CURVE('',#33100,#33097,#10550,.T.) ;
#40528 = EDGE_CURVE('',#33101,#33102,#10551,.T.) ;
#40529 = EDGE_CURVE('',#33102,#33103,#10552,.T.) ;
#40530 = EDGE_CURVE('',#33103,#33104,#10553,.T.) ;
#40531 = EDGE_CURVE('',#33104,#33101,#10554,.T.) ;
#40532 = EDGE_CURVE('',#32098,#33105,#10555,.T.) ;
#40533 = EDGE_CURVE('',#33105,#33106,#10556,.T.) ;
#40534 = EDGE_CURVE('',#33106,#32099,#10557,.T.) ;
#40535 = EDGE_CURVE('',#33107,#33108,#10558,.T.) ;
#40536 = EDGE_CURVE('',#33108,#33109,#10559,.T.) ;
#40537 = EDGE_CURVE('',#33109,#33110,#10560,.T.) ;
#40538 = EDGE_CURVE('',#33110,#33107,#10561,.T.) ;
#40539 = EDGE_CURVE('',#33111,#33112,#10562,.T.) ;
#40540 = EDGE_CURVE('',#33112,#33113,#10563,.T.) ;
#40541 = EDGE_CURVE('',#33113,#33114,#10564,.T.) ;
#40542 = EDGE_CURVE('',#33114,#33111,#10565,.T.) ;
#40543 = EDGE_CURVE('',#33115,#33116,#10566,.T.) ;
#40544 = EDGE_CURVE('',#33116,#33117,#10567,.T.) ;
#40545 = EDGE_CURVE('',#33117,#33118,#10568,.T.) ;
#40546 = EDGE_CURVE('',#33118,#33115,#10569,.T.) ;
#40547 = EDGE_CURVE('',#33119,#33120,#10570,.T.) ;
#40548 = EDGE_CURVE('',#33120,#33121,#10571,.T.) ;
#40549 = EDGE_CURVE('',#33121,#33122,#10572,.T.) ;
#40550 = EDGE_CURVE('',#33122,#33119,#10573,.T.) ;
#40551 = EDGE_CURVE('',#32083,#33123,#10574,.T.) ;
#40552 = EDGE_CURVE('',#33123,#33124,#10575,.T.) ;
#40553 = EDGE_CURVE('',#33124,#32084,#10576,.T.) ;
#40554 = EDGE_CURVE('',#33125,#33126,#10577,.T.) ;
#40555 = EDGE_CURVE('',#33126,#33127,#10578,.T.) ;
#40556 = EDGE_CURVE('',#33127,#33128,#10579,.T.) ;
#40557 = EDGE_CURVE('',#33128,#33125,#10580,.T.) ;
#40558 = EDGE_CURVE('',#33129,#33130,#10581,.T.) ;
#40559 = EDGE_CURVE('',#33130,#33131,#10582,.T.) ;
#40560 = EDGE_CURVE('',#33131,#33132,#10583,.T.) ;
#40561 = EDGE_CURVE('',#33132,#33129,#10584,.T.) ;
#40562 = EDGE_CURVE('',#33133,#33134,#10585,.T.) ;
#40563 = EDGE_CURVE('',#33134,#33135,#10586,.T.) ;
#40564 = EDGE_CURVE('',#33135,#33136,#10587,.T.) ;
#40565 = EDGE_CURVE('',#33136,#33133,#10588,.T.) ;
#40566 = EDGE_CURVE('',#33137,#33138,#10589,.T.) ;
#40567 = EDGE_CURVE('',#33138,#33139,#10590,.T.) ;
#40568 = EDGE_CURVE('',#33139,#33140,#10591,.T.) ;
#40569 = EDGE_CURVE('',#33140,#33137,#10592,.T.) ;
#40570 = EDGE_CURVE('',#32068,#33141,#10593,.T.) ;
#40571 = EDGE_CURVE('',#33141,#33142,#10594,.T.) ;
#40572 = EDGE_CURVE('',#33142,#32069,#10595,.T.) ;
#40573 = EDGE_CURVE('',#33143,#33144,#10596,.T.) ;
#40574 = EDGE_CURVE('',#33144,#33145,#10597,.T.) ;
#40575 = EDGE_CURVE('',#33145,#33146,#10598,.T.) ;
#40576 = EDGE_CURVE('',#33146,#33143,#10599,.T.) ;
#40577 = EDGE_CURVE('',#33147,#33148,#10600,.T.) ;
#40578 = EDGE_CURVE('',#33148,#33149,#10601,.T.) ;
#40579 = EDGE_CURVE('',#33149,#33150,#10602,.T.) ;
#40580 = EDGE_CURVE('',#33150,#33147,#10603,.T.) ;
#40581 = EDGE_CURVE('',#33151,#33152,#10604,.T.) ;
#40582 = EDGE_CURVE('',#33152,#33153,#10605,.T.) ;
#40583 = EDGE_CURVE('',#33153,#33154,#10606,.T.) ;
#40584 = EDGE_CURVE('',#33154,#33151,#10607,.T.) ;
#40585 = EDGE_CURVE('',#33155,#33156,#10608,.T.) ;
#40586 = EDGE_CURVE('',#33156,#33157,#10609,.T.) ;
#40587 = EDGE_CURVE('',#33157,#33158,#10610,.T.) ;
#40588 = EDGE_CURVE('',#33158,#33155,#10611,.T.) ;
#40589 = EDGE_CURVE('',#32053,#33159,#10612,.T.) ;
#40590 = EDGE_CURVE('',#33159,#33160,#10613,.T.) ;
#40591 = EDGE_CURVE('',#33160,#32054,#10614,.T.) ;
#40592 = EDGE_CURVE('',#33161,#33162,#10615,.T.) ;
#40593 = EDGE_CURVE('',#33162,#33163,#10616,.T.) ;
#40594 = EDGE_CURVE('',#33163,#33164,#10617,.T.) ;
#40595 = EDGE_CURVE('',#33164,#33161,#10618,.T.) ;
#40596 = EDGE_CURVE('',#33165,#33166,#10619,.T.) ;
#40597 = EDGE_CURVE('',#33166,#33167,#10620,.T.) ;
#40598 = EDGE_CURVE('',#33167,#33168,#10621,.T.) ;
#40599 = EDGE_CURVE('',#33168,#33165,#10622,.T.) ;
#40600 = EDGE_CURVE('',#33169,#33170,#10623,.T.) ;
#40601 = EDGE_CURVE('',#33170,#33171,#10624,.T.) ;
#40602 = EDGE_CURVE('',#33171,#33172,#10625,.T.) ;
#40603 = EDGE_CURVE('',#33172,#33169,#10626,.T.) ;
#40604 = EDGE_CURVE('',#33173,#33174,#10627,.T.) ;
#40605 = EDGE_CURVE('',#33174,#33175,#10628,.T.) ;
#40606 = EDGE_CURVE('',#33175,#33176,#10629,.T.) ;
#40607 = EDGE_CURVE('',#33176,#33173,#10630,.T.) ;
#40608 = EDGE_CURVE('',#32038,#33177,#10631,.T.) ;
#40609 = EDGE_CURVE('',#33177,#33178,#10632,.T.) ;
#40610 = EDGE_CURVE('',#33178,#32039,#10633,.T.) ;
#40611 = EDGE_CURVE('',#33179,#33180,#10634,.T.) ;
#40612 = EDGE_CURVE('',#33180,#33181,#10635,.T.) ;
#40613 = EDGE_CURVE('',#33181,#33182,#10636,.T.) ;
#40614 = EDGE_CURVE('',#33182,#33179,#10637,.T.) ;
#40615 = EDGE_CURVE('',#33183,#33184,#10638,.T.) ;
#40616 = EDGE_CURVE('',#33184,#33185,#10639,.T.) ;
#40617 = EDGE_CURVE('',#33185,#33186,#10640,.T.) ;
#40618 = EDGE_CURVE('',#33186,#33183,#10641,.T.) ;
#40619 = EDGE_CURVE('',#33187,#33188,#10642,.T.) ;
#40620 = EDGE_CURVE('',#33188,#33189,#10643,.T.) ;
#40621 = EDGE_CURVE('',#33189,#33190,#10644,.T.) ;
#40622 = EDGE_CURVE('',#33190,#33187,#10645,.T.) ;
#40623 = EDGE_CURVE('',#33191,#33192,#10646,.T.) ;
#40624 = EDGE_CURVE('',#33192,#33193,#10647,.T.) ;
#40625 = EDGE_CURVE('',#33193,#33194,#10648,.T.) ;
#40626 = EDGE_CURVE('',#33194,#33191,#10649,.T.) ;
#40627 = EDGE_CURVE('',#32023,#33195,#10650,.T.) ;
#40628 = EDGE_CURVE('',#33195,#33196,#10651,.T.) ;
#40629 = EDGE_CURVE('',#33196,#32024,#10652,.T.) ;
#40630 = EDGE_CURVE('',#33197,#33198,#10653,.T.) ;
#40631 = EDGE_CURVE('',#33198,#33199,#10654,.T.) ;
#40632 = EDGE_CURVE('',#33199,#33200,#10655,.T.) ;
#40633 = EDGE_CURVE('',#33200,#33197,#10656,.T.) ;
#40634 = EDGE_CURVE('',#33201,#33202,#10657,.T.) ;
#40635 = EDGE_CURVE('',#33202,#33203,#10658,.T.) ;
#40636 = EDGE_CURVE('',#33203,#33204,#10659,.T.) ;
#40637 = EDGE_CURVE('',#33204,#33201,#10660,.T.) ;
#40638 = EDGE_CURVE('',#33205,#33206,#10661,.T.) ;
#40639 = EDGE_CURVE('',#33206,#33207,#10662,.T.) ;
#40640 = EDGE_CURVE('',#33207,#33208,#10663,.T.) ;
#40641 = EDGE_CURVE('',#33208,#33205,#10664,.T.) ;
#40642 = EDGE_CURVE('',#33209,#33210,#10665,.T.) ;
#40643 = EDGE_CURVE('',#33210,#33211,#10666,.T.) ;
#40644 = EDGE_CURVE('',#33211,#33212,#10667,.T.) ;
#40645 = EDGE_CURVE('',#33212,#33209,#10668,.T.) ;
#40646 = EDGE_CURVE('',#32008,#33213,#10669,.T.) ;
#40647 = EDGE_CURVE('',#33213,#33214,#10670,.T.) ;
#40648 = EDGE_CURVE('',#33214,#32009,#10671,.T.) ;
#40649 = EDGE_CURVE('',#33215,#33216,#10672,.T.) ;
#40650 = EDGE_CURVE('',#33216,#33217,#10673,.T.) ;
#40651 = EDGE_CURVE('',#33217,#33218,#10674,.T.) ;
#40652 = EDGE_CURVE('',#33218,#33215,#10675,.T.) ;
#40653 = EDGE_CURVE('',#33219,#33220,#10676,.T.) ;
#40654 = EDGE_CURVE('',#33220,#33221,#10677,.T.) ;
#40655 = EDGE_CURVE('',#33221,#33222,#10678,.T.) ;
#40656 = EDGE_CURVE('',#33222,#33219,#10679,.T.) ;
#40657 = EDGE_CURVE('',#33223,#33224,#10680,.T.) ;
#40658 = EDGE_CURVE('',#33224,#33225,#10681,.T.) ;
#40659 = EDGE_CURVE('',#33225,#33226,#10682,.T.) ;
#40660 = EDGE_CURVE('',#33226,#33223,#10683,.T.) ;
#40661 = EDGE_CURVE('',#33227,#33228,#10684,.T.) ;
#40662 = EDGE_CURVE('',#33227,#33229,#27529,.T.) ;
#40663 = EDGE_CURVE('',#33229,#33230,#10685,.T.) ;
#40664 = EDGE_CURVE('',#33230,#33228,#27530,.T.) ;
#40665 = EDGE_CURVE('',#33229,#33231,#10686,.T.) ;
#40666 = EDGE_CURVE('',#33231,#33232,#10687,.T.) ;
#40667 = EDGE_CURVE('',#33232,#33230,#10688,.T.) ;
#40668 = EDGE_CURVE('',#33231,#33233,#27531,.T.) ;
#40669 = EDGE_CURVE('',#33233,#33234,#10689,.T.) ;
#40670 = EDGE_CURVE('',#33234,#33232,#27532,.T.) ;
#40671 = EDGE_CURVE('',#33233,#33235,#10690,.T.) ;
#40672 = EDGE_CURVE('',#33235,#33236,#10691,.T.) ;
#40673 = EDGE_CURVE('',#33236,#33234,#10692,.T.) ;
#40674 = EDGE_CURVE('',#33235,#33237,#27533,.T.) ;
#40675 = EDGE_CURVE('',#33237,#33238,#10693,.T.) ;
#40676 = EDGE_CURVE('',#33238,#33236,#27534,.T.) ;
#40677 = EDGE_CURVE('',#33237,#32003,#10694,.T.) ;
#40678 = EDGE_CURVE('',#32003,#33239,#10695,.T.) ;
#40679 = EDGE_CURVE('',#33239,#33238,#10696,.T.) ;
#40680 = EDGE_CURVE('',#32004,#33240,#10697,.T.) ;
#40681 = EDGE_CURVE('',#33240,#33239,#27535,.T.) ;
#40682 = EDGE_CURVE('',#32004,#32185,#10698,.T.) ;
#40683 = EDGE_CURVE('',#32155,#33240,#10699,.T.) ;
#40684 = EDGE_CURVE('',#32186,#33241,#10700,.T.) ;
#40685 = EDGE_CURVE('',#33241,#33242,#10701,.T.) ;
#40686 = EDGE_CURVE('',#33242,#32156,#10702,.T.) ;
#40687 = EDGE_CURVE('',#33241,#33243,#27536,.T.) ;
#40688 = EDGE_CURVE('',#33243,#33244,#10703,.T.) ;
#40689 = EDGE_CURVE('',#33244,#33242,#27537,.T.) ;
#40690 = EDGE_CURVE('',#33243,#33245,#10704,.T.) ;
#40691 = EDGE_CURVE('',#33245,#33246,#10705,.T.) ;
#40692 = EDGE_CURVE('',#33246,#33244,#10706,.T.) ;
#40693 = EDGE_CURVE('',#33245,#33247,#27538,.T.) ;
#40694 = EDGE_CURVE('',#33247,#33248,#10707,.T.) ;
#40695 = EDGE_CURVE('',#33248,#33246,#27539,.T.) ;
#40696 = EDGE_CURVE('',#33247,#33249,#10708,.T.) ;
#40697 = EDGE_CURVE('',#33249,#33250,#10709,.T.) ;
#40698 = EDGE_CURVE('',#33250,#33248,#10710,.T.) ;
#40699 = EDGE_CURVE('',#33249,#33251,#27540,.T.) ;
#40700 = EDGE_CURVE('',#33251,#33252,#10711,.T.) ;
#40701 = EDGE_CURVE('',#33252,#33250,#27541,.T.) ;
#40702 = EDGE_CURVE('',#33251,#33253,#10712,.T.) ;
#40703 = EDGE_CURVE('',#33253,#33254,#10713,.T.) ;
#40704 = EDGE_CURVE('',#33254,#33252,#10714,.T.) ;
#40705 = EDGE_CURVE('',#33253,#33255,#27542,.T.) ;
#40706 = EDGE_CURVE('',#33255,#33256,#10715,.T.) ;
#40707 = EDGE_CURVE('',#33256,#33254,#27543,.T.) ;
#40708 = EDGE_CURVE('',#33255,#33257,#10716,.T.) ;
#40709 = EDGE_CURVE('',#33257,#33258,#10717,.T.) ;
#40710 = EDGE_CURVE('',#33258,#33256,#10718,.T.) ;
#40711 = EDGE_CURVE('',#33257,#33259,#27544,.T.) ;
#40712 = EDGE_CURVE('',#33259,#33260,#10719,.T.) ;
#40713 = EDGE_CURVE('',#33260,#33258,#27545,.T.) ;
#40714 = EDGE_CURVE('',#33259,#33261,#10720,.T.) ;
#40715 = EDGE_CURVE('',#33261,#33262,#10721,.T.) ;
#40716 = EDGE_CURVE('',#33262,#33260,#10722,.T.) ;
#40717 = EDGE_CURVE('',#33261,#33263,#27546,.T.) ;
#40718 = EDGE_CURVE('',#33263,#33264,#10723,.T.) ;
#40719 = EDGE_CURVE('',#33264,#33262,#27547,.T.) ;
#40720 = EDGE_CURVE('',#33263,#33265,#27548,.T.) ;
#40721 = EDGE_CURVE('',#33265,#33266,#10724,.T.) ;
#40722 = EDGE_CURVE('',#33266,#33264,#27549,.T.) ;
#40723 = EDGE_CURVE('',#33265,#33267,#27550,.T.) ;
#40724 = EDGE_CURVE('',#33267,#33268,#10725,.T.) ;
#40725 = EDGE_CURVE('',#33268,#33266,#27551,.T.) ;
#40726 = EDGE_CURVE('',#33267,#33269,#10726,.T.) ;
#40727 = EDGE_CURVE('',#33269,#33270,#10727,.T.) ;
#40728 = EDGE_CURVE('',#33270,#33268,#10728,.T.) ;
#40729 = EDGE_CURVE('',#33269,#33271,#27552,.T.) ;
#40730 = EDGE_CURVE('',#33271,#33272,#10729,.T.) ;
#40731 = EDGE_CURVE('',#33272,#33270,#27553,.T.) ;
#40732 = EDGE_CURVE('',#33271,#33273,#10730,.T.) ;
#40733 = EDGE_CURVE('',#33273,#33274,#10731,.T.) ;
#40734 = EDGE_CURVE('',#33274,#33272,#10732,.T.) ;
#40735 = EDGE_CURVE('',#33273,#33275,#27554,.T.) ;
#40736 = EDGE_CURVE('',#33275,#33276,#10733,.T.) ;
#40737 = EDGE_CURVE('',#33276,#33274,#27555,.T.) ;
#40738 = EDGE_CURVE('',#33275,#33227,#10734,.T.) ;
#40739 = EDGE_CURVE('',#33228,#33276,#10735,.T.) ;
#40740 = EDGE_CURVE('',#33277,#33278,#27556,.T.) ;
#40741 = EDGE_CURVE('',#33278,#33279,#10736,.T.) ;
#40742 = EDGE_CURVE('',#33279,#33280,#27557,.T.) ;
#40743 = EDGE_CURVE('',#33280,#33281,#10737,.T.) ;
#40744 = EDGE_CURVE('',#33281,#33282,#10738,.T.) ;
#40745 = EDGE_CURVE('',#33282,#33283,#10739,.T.) ;
#40746 = EDGE_CURVE('',#33283,#33284,#27558,.T.) ;
#40747 = EDGE_CURVE('',#33284,#33285,#10740,.T.) ;
#40748 = EDGE_CURVE('',#33285,#33286,#10741,.T.) ;
#40749 = EDGE_CURVE('',#33286,#33287,#10742,.T.) ;
#40750 = EDGE_CURVE('',#33287,#33288,#27559,.T.) ;
#40751 = EDGE_CURVE('',#33288,#33289,#10743,.T.) ;
#40752 = EDGE_CURVE('',#33289,#33290,#27560,.T.) ;
#40753 = EDGE_CURVE('',#33290,#33291,#10744,.T.) ;
#40754 = EDGE_CURVE('',#33291,#33292,#10745,.T.) ;
#40755 = EDGE_CURVE('',#33292,#32005,#10746,.T.) ;
#40756 = EDGE_CURVE('',#32005,#33293,#10747,.T.) ;
#40757 = EDGE_CURVE('',#33293,#33277,#10748,.T.) ;
#40758 = EDGE_CURVE('',#33294,#33295,#10749,.T.) ;
#40759 = EDGE_CURVE('',#33294,#33296,#27561,.T.) ;
#40760 = EDGE_CURVE('',#33296,#33297,#10750,.T.) ;
#40761 = EDGE_CURVE('',#33297,#33295,#27562,.T.) ;
#40762 = EDGE_CURVE('',#33296,#33298,#10751,.T.) ;
#40763 = EDGE_CURVE('',#33298,#33299,#10752,.T.) ;
#40764 = EDGE_CURVE('',#33299,#33297,#10753,.T.) ;
#40765 = EDGE_CURVE('',#33298,#33300,#27563,.T.) ;
#40766 = EDGE_CURVE('',#33300,#33301,#10754,.T.) ;
#40767 = EDGE_CURVE('',#33301,#33299,#27564,.T.) ;
#40768 = EDGE_CURVE('',#33300,#33302,#10755,.T.) ;
#40769 = EDGE_CURVE('',#33302,#33303,#10756,.T.) ;
#40770 = EDGE_CURVE('',#33303,#33301,#10757,.T.) ;
#40771 = EDGE_CURVE('',#33302,#33304,#27565,.T.) ;
#40772 = EDGE_CURVE('',#33304,#33305,#10758,.T.) ;
#40773 = EDGE_CURVE('',#33305,#33303,#27566,.T.) ;
#40774 = EDGE_CURVE('',#33304,#32018,#10759,.T.) ;
#40775 = EDGE_CURVE('',#32018,#33306,#10760,.T.) ;
#40776 = EDGE_CURVE('',#33306,#33305,#10761,.T.) ;
#40777 = EDGE_CURVE('',#32019,#33307,#10762,.T.) ;
#40778 = EDGE_CURVE('',#33307,#33306,#27567,.T.) ;
#40779 = EDGE_CURVE('',#32019,#32183,#10763,.T.) ;
#40780 = EDGE_CURVE('',#32151,#33307,#10764,.T.) ;
#40781 = EDGE_CURVE('',#32184,#33308,#10765,.T.) ;
#40782 = EDGE_CURVE('',#33308,#33309,#10766,.T.) ;
#40783 = EDGE_CURVE('',#33309,#32152,#10767,.T.) ;
#40784 = EDGE_CURVE('',#33308,#33310,#27568,.T.) ;
#40785 = EDGE_CURVE('',#33310,#33311,#10768,.T.) ;
#40786 = EDGE_CURVE('',#33311,#33309,#27569,.T.) ;
#40787 = EDGE_CURVE('',#33310,#33312,#10769,.T.) ;
#40788 = EDGE_CURVE('',#33312,#33313,#10770,.T.) ;
#40789 = EDGE_CURVE('',#33313,#33311,#10771,.T.) ;
#40790 = EDGE_CURVE('',#33312,#33314,#27570,.T.) ;
#40791 = EDGE_CURVE('',#33314,#33315,#10772,.T.) ;
#40792 = EDGE_CURVE('',#33315,#33313,#27571,.T.) ;
#40793 = EDGE_CURVE('',#33314,#33316,#10773,.T.) ;
#40794 = EDGE_CURVE('',#33316,#33317,#10774,.T.) ;
#40795 = EDGE_CURVE('',#33317,#33315,#10775,.T.) ;
#40796 = EDGE_CURVE('',#33316,#33318,#27572,.T.) ;
#40797 = EDGE_CURVE('',#33318,#33319,#10776,.T.) ;
#40798 = EDGE_CURVE('',#33319,#33317,#27573,.T.) ;
#40799 = EDGE_CURVE('',#33318,#33320,#10777,.T.) ;
#40800 = EDGE_CURVE('',#33320,#33321,#10778,.T.) ;
#40801 = EDGE_CURVE('',#33321,#33319,#10779,.T.) ;
#40802 = EDGE_CURVE('',#33320,#33322,#27574,.T.) ;
#40803 = EDGE_CURVE('',#33322,#33323,#10780,.T.) ;
#40804 = EDGE_CURVE('',#33323,#33321,#27575,.T.) ;
#40805 = EDGE_CURVE('',#33322,#33324,#10781,.T.) ;
#40806 = EDGE_CURVE('',#33324,#33325,#10782,.T.) ;
#40807 = EDGE_CURVE('',#33325,#33323,#10783,.T.) ;
#40808 = EDGE_CURVE('',#33324,#33326,#27576,.T.) ;
#40809 = EDGE_CURVE('',#33326,#33327,#10784,.T.) ;
#40810 = EDGE_CURVE('',#33327,#33325,#27577,.T.) ;
#40811 = EDGE_CURVE('',#33326,#33328,#10785,.T.) ;
#40812 = EDGE_CURVE('',#33328,#33329,#10786,.T.) ;
#40813 = EDGE_CURVE('',#33329,#33327,#10787,.T.) ;
#40814 = EDGE_CURVE('',#33328,#33330,#27578,.T.) ;
#40815 = EDGE_CURVE('',#33330,#33331,#10788,.T.) ;
#40816 = EDGE_CURVE('',#33331,#33329,#27579,.T.) ;
#40817 = EDGE_CURVE('',#33330,#33332,#27580,.T.) ;
#40818 = EDGE_CURVE('',#33332,#33333,#10789,.T.) ;
#40819 = EDGE_CURVE('',#33333,#33331,#27581,.T.) ;
#40820 = EDGE_CURVE('',#33332,#33334,#27582,.T.) ;
#40821 = EDGE_CURVE('',#33334,#33335,#10790,.T.) ;
#40822 = EDGE_CURVE('',#33335,#33333,#27583,.T.) ;
#40823 = EDGE_CURVE('',#33334,#33336,#10791,.T.) ;
#40824 = EDGE_CURVE('',#33336,#33337,#10792,.T.) ;
#40825 = EDGE_CURVE('',#33337,#33335,#10793,.T.) ;
#40826 = EDGE_CURVE('',#33336,#33338,#27584,.T.) ;
#40827 = EDGE_CURVE('',#33338,#33339,#10794,.T.) ;
#40828 = EDGE_CURVE('',#33339,#33337,#27585,.T.) ;
#40829 = EDGE_CURVE('',#33338,#33340,#10795,.T.) ;
#40830 = EDGE_CURVE('',#33340,#33341,#10796,.T.) ;
#40831 = EDGE_CURVE('',#33341,#33339,#10797,.T.) ;
#40832 = EDGE_CURVE('',#33340,#33342,#27586,.T.) ;
#40833 = EDGE_CURVE('',#33342,#33343,#10798,.T.) ;
#40834 = EDGE_CURVE('',#33343,#33341,#27587,.T.) ;
#40835 = EDGE_CURVE('',#33342,#33294,#10799,.T.) ;
#40836 = EDGE_CURVE('',#33295,#33343,#10800,.T.) ;
#40837 = EDGE_CURVE('',#33344,#33345,#27588,.T.) ;
#40838 = EDGE_CURVE('',#33345,#33346,#10801,.T.) ;
#40839 = EDGE_CURVE('',#33346,#33347,#27589,.T.) ;
#40840 = EDGE_CURVE('',#33347,#33348,#10802,.T.) ;
#40841 = EDGE_CURVE('',#33348,#33349,#10803,.T.) ;
#40842 = EDGE_CURVE('',#33349,#33350,#10804,.T.) ;
#40843 = EDGE_CURVE('',#33350,#33351,#27590,.T.) ;
#40844 = EDGE_CURVE('',#33351,#33352,#10805,.T.) ;
#40845 = EDGE_CURVE('',#33352,#33353,#10806,.T.) ;
#40846 = EDGE_CURVE('',#33353,#33354,#10807,.T.) ;
#40847 = EDGE_CURVE('',#33354,#33355,#27591,.T.) ;
#40848 = EDGE_CURVE('',#33355,#33356,#10808,.T.) ;
#40849 = EDGE_CURVE('',#33356,#33357,#27592,.T.) ;
#40850 = EDGE_CURVE('',#33357,#33358,#10809,.T.) ;
#40851 = EDGE_CURVE('',#33358,#33359,#10810,.T.) ;
#40852 = EDGE_CURVE('',#33359,#32020,#10811,.T.) ;
#40853 = EDGE_CURVE('',#32020,#33360,#10812,.T.) ;
#40854 = EDGE_CURVE('',#33360,#33344,#10813,.T.) ;
#40855 = EDGE_CURVE('',#33361,#33362,#10814,.T.) ;
#40856 = EDGE_CURVE('',#33361,#33363,#27593,.T.) ;
#40857 = EDGE_CURVE('',#33363,#33364,#10815,.T.) ;
#40858 = EDGE_CURVE('',#33364,#33362,#27594,.T.) ;
#40859 = EDGE_CURVE('',#33363,#33365,#10816,.T.) ;
#40860 = EDGE_CURVE('',#33365,#33366,#10817,.T.) ;
#40861 = EDGE_CURVE('',#33366,#33364,#10818,.T.) ;
#40862 = EDGE_CURVE('',#33365,#33367,#27595,.T.) ;
#40863 = EDGE_CURVE('',#33367,#33368,#10819,.T.) ;
#40864 = EDGE_CURVE('',#33368,#33366,#27596,.T.) ;
#40865 = EDGE_CURVE('',#33367,#33369,#10820,.T.) ;
#40866 = EDGE_CURVE('',#33369,#33370,#10821,.T.) ;
#40867 = EDGE_CURVE('',#33370,#33368,#10822,.T.) ;
#40868 = EDGE_CURVE('',#33369,#33371,#27597,.T.) ;
#40869 = EDGE_CURVE('',#33371,#33372,#10823,.T.) ;
#40870 = EDGE_CURVE('',#33372,#33370,#27598,.T.) ;
#40871 = EDGE_CURVE('',#33371,#32033,#10824,.T.) ;
#40872 = EDGE_CURVE('',#32033,#33373,#10825,.T.) ;
#40873 = EDGE_CURVE('',#33373,#33372,#10826,.T.) ;
#40874 = EDGE_CURVE('',#32034,#33374,#10827,.T.) ;
#40875 = EDGE_CURVE('',#33374,#33373,#27599,.T.) ;
#40876 = EDGE_CURVE('',#32034,#32181,#10828,.T.) ;
#40877 = EDGE_CURVE('',#32147,#33374,#10829,.T.) ;
#40878 = EDGE_CURVE('',#32182,#33375,#10830,.T.) ;
#40879 = EDGE_CURVE('',#33375,#33376,#10831,.T.) ;
#40880 = EDGE_CURVE('',#33376,#32148,#10832,.T.) ;
#40881 = EDGE_CURVE('',#33375,#33377,#27600,.T.) ;
#40882 = EDGE_CURVE('',#33377,#33378,#10833,.T.) ;
#40883 = EDGE_CURVE('',#33378,#33376,#27601,.T.) ;
#40884 = EDGE_CURVE('',#33377,#33379,#10834,.T.) ;
#40885 = EDGE_CURVE('',#33379,#33380,#10835,.T.) ;
#40886 = EDGE_CURVE('',#33380,#33378,#10836,.T.) ;
#40887 = EDGE_CURVE('',#33379,#33381,#27602,.T.) ;
#40888 = EDGE_CURVE('',#33381,#33382,#10837,.T.) ;
#40889 = EDGE_CURVE('',#33382,#33380,#27603,.T.) ;
#40890 = EDGE_CURVE('',#33381,#33383,#10838,.T.) ;
#40891 = EDGE_CURVE('',#33383,#33384,#10839,.T.) ;
#40892 = EDGE_CURVE('',#33384,#33382,#10840,.T.) ;
#40893 = EDGE_CURVE('',#33383,#33385,#27604,.T.) ;
#40894 = EDGE_CURVE('',#33385,#33386,#10841,.T.) ;
#40895 = EDGE_CURVE('',#33386,#33384,#27605,.T.) ;
#40896 = EDGE_CURVE('',#33385,#33387,#10842,.T.) ;
#40897 = EDGE_CURVE('',#33387,#33388,#10843,.T.) ;
#40898 = EDGE_CURVE('',#33388,#33386,#10844,.T.) ;
#40899 = EDGE_CURVE('',#33387,#33389,#27606,.T.) ;
#40900 = EDGE_CURVE('',#33389,#33390,#10845,.T.) ;
#40901 = EDGE_CURVE('',#33390,#33388,#27607,.T.) ;
#40902 = EDGE_CURVE('',#33389,#33391,#10846,.T.) ;
#40903 = EDGE_CURVE('',#33391,#33392,#10847,.T.) ;
#40904 = EDGE_CURVE('',#33392,#33390,#10848,.T.) ;
#40905 = EDGE_CURVE('',#33391,#33393,#27608,.T.) ;
#40906 = EDGE_CURVE('',#33393,#33394,#10849,.T.) ;
#40907 = EDGE_CURVE('',#33394,#33392,#27609,.T.) ;
#40908 = EDGE_CURVE('',#33393,#33395,#10850,.T.) ;
#40909 = EDGE_CURVE('',#33395,#33396,#10851,.T.) ;
#40910 = EDGE_CURVE('',#33396,#33394,#10852,.T.) ;
#40911 = EDGE_CURVE('',#33395,#33397,#27610,.T.) ;
#40912 = EDGE_CURVE('',#33397,#33398,#10853,.T.) ;
#40913 = EDGE_CURVE('',#33398,#33396,#27611,.T.) ;
#40914 = EDGE_CURVE('',#33397,#33399,#27612,.T.) ;
#40915 = EDGE_CURVE('',#33399,#33400,#10854,.T.) ;
#40916 = EDGE_CURVE('',#33400,#33398,#27613,.T.) ;
#40917 = EDGE_CURVE('',#33399,#33401,#27614,.T.) ;
#40918 = EDGE_CURVE('',#33401,#33402,#10855,.T.) ;
#40919 = EDGE_CURVE('',#33402,#33400,#27615,.T.) ;
#40920 = EDGE_CURVE('',#33401,#33403,#10856,.T.) ;
#40921 = EDGE_CURVE('',#33403,#33404,#10857,.T.) ;
#40922 = EDGE_CURVE('',#33404,#33402,#10858,.T.) ;
#40923 = EDGE_CURVE('',#33403,#33405,#27616,.T.) ;
#40924 = EDGE_CURVE('',#33405,#33406,#10859,.T.) ;
#40925 = EDGE_CURVE('',#33406,#33404,#27617,.T.) ;
#40926 = EDGE_CURVE('',#33405,#33407,#10860,.T.) ;
#40927 = EDGE_CURVE('',#33407,#33408,#10861,.T.) ;
#40928 = EDGE_CURVE('',#33408,#33406,#10862,.T.) ;
#40929 = EDGE_CURVE('',#33407,#33409,#27618,.T.) ;
#40930 = EDGE_CURVE('',#33409,#33410,#10863,.T.) ;
#40931 = EDGE_CURVE('',#33410,#33408,#27619,.T.) ;
#40932 = EDGE_CURVE('',#33409,#33361,#10864,.T.) ;
#40933 = EDGE_CURVE('',#33362,#33410,#10865,.T.) ;
#40934 = EDGE_CURVE('',#33411,#33412,#27620,.T.) ;
#40935 = EDGE_CURVE('',#33412,#33413,#10866,.T.) ;
#40936 = EDGE_CURVE('',#33413,#33414,#27621,.T.) ;
#40937 = EDGE_CURVE('',#33414,#33415,#10867,.T.) ;
#40938 = EDGE_CURVE('',#33415,#33416,#10868,.T.) ;
#40939 = EDGE_CURVE('',#33416,#33417,#10869,.T.) ;
#40940 = EDGE_CURVE('',#33417,#33418,#27622,.T.) ;
#40941 = EDGE_CURVE('',#33418,#33419,#10870,.T.) ;
#40942 = EDGE_CURVE('',#33419,#33420,#10871,.T.) ;
#40943 = EDGE_CURVE('',#33420,#33421,#10872,.T.) ;
#40944 = EDGE_CURVE('',#33421,#33422,#27623,.T.) ;
#40945 = EDGE_CURVE('',#33422,#33423,#10873,.T.) ;
#40946 = EDGE_CURVE('',#33423,#33424,#27624,.T.) ;
#40947 = EDGE_CURVE('',#33424,#33425,#10874,.T.) ;
#40948 = EDGE_CURVE('',#33425,#33426,#10875,.T.) ;
#40949 = EDGE_CURVE('',#33426,#32035,#10876,.T.) ;
#40950 = EDGE_CURVE('',#32035,#33427,#10877,.T.) ;
#40951 = EDGE_CURVE('',#33427,#33411,#10878,.T.) ;
#40952 = EDGE_CURVE('',#33428,#33429,#10879,.T.) ;
#40953 = EDGE_CURVE('',#33428,#33430,#27625,.T.) ;
#40954 = EDGE_CURVE('',#33430,#33431,#10880,.T.) ;
#40955 = EDGE_CURVE('',#33431,#33429,#27626,.T.) ;
#40956 = EDGE_CURVE('',#33430,#33432,#10881,.T.) ;
#40957 = EDGE_CURVE('',#33432,#33433,#10882,.T.) ;
#40958 = EDGE_CURVE('',#33433,#33431,#10883,.T.) ;
#40959 = EDGE_CURVE('',#33432,#33434,#27627,.T.) ;
#40960 = EDGE_CURVE('',#33434,#33435,#10884,.T.) ;
#40961 = EDGE_CURVE('',#33435,#33433,#27628,.T.) ;
#40962 = EDGE_CURVE('',#33434,#33436,#10885,.T.) ;
#40963 = EDGE_CURVE('',#33436,#33437,#10886,.T.) ;
#40964 = EDGE_CURVE('',#33437,#33435,#10887,.T.) ;
#40965 = EDGE_CURVE('',#33436,#33438,#27629,.T.) ;
#40966 = EDGE_CURVE('',#33438,#33439,#10888,.T.) ;
#40967 = EDGE_CURVE('',#33439,#33437,#27630,.T.) ;
#40968 = EDGE_CURVE('',#33438,#32048,#10889,.T.) ;
#40969 = EDGE_CURVE('',#32048,#33440,#10890,.T.) ;
#40970 = EDGE_CURVE('',#33440,#33439,#10891,.T.) ;
#40971 = EDGE_CURVE('',#32049,#33441,#10892,.T.) ;
#40972 = EDGE_CURVE('',#33441,#33440,#27631,.T.) ;
#40973 = EDGE_CURVE('',#32049,#32179,#10893,.T.) ;
#40974 = EDGE_CURVE('',#32143,#33441,#10894,.T.) ;
#40975 = EDGE_CURVE('',#32180,#33442,#10895,.T.) ;
#40976 = EDGE_CURVE('',#33442,#33443,#10896,.T.) ;
#40977 = EDGE_CURVE('',#33443,#32144,#10897,.T.) ;
#40978 = EDGE_CURVE('',#33442,#33444,#27632,.T.) ;
#40979 = EDGE_CURVE('',#33444,#33445,#10898,.T.) ;
#40980 = EDGE_CURVE('',#33445,#33443,#27633,.T.) ;
#40981 = EDGE_CURVE('',#33444,#33446,#10899,.T.) ;
#40982 = EDGE_CURVE('',#33446,#33447,#10900,.T.) ;
#40983 = EDGE_CURVE('',#33447,#33445,#10901,.T.) ;
#40984 = EDGE_CURVE('',#33446,#33448,#27634,.T.) ;
#40985 = EDGE_CURVE('',#33448,#33449,#10902,.T.) ;
#40986 = EDGE_CURVE('',#33449,#33447,#27635,.T.) ;
#40987 = EDGE_CURVE('',#33448,#33450,#10903,.T.) ;
#40988 = EDGE_CURVE('',#33450,#33451,#10904,.T.) ;
#40989 = EDGE_CURVE('',#33451,#33449,#10905,.T.) ;
#40990 = EDGE_CURVE('',#33450,#33452,#27636,.T.) ;
#40991 = EDGE_CURVE('',#33452,#33453,#10906,.T.) ;
#40992 = EDGE_CURVE('',#33453,#33451,#27637,.T.) ;
#40993 = EDGE_CURVE('',#33452,#33454,#10907,.T.) ;
#40994 = EDGE_CURVE('',#33454,#33455,#10908,.T.) ;
#40995 = EDGE_CURVE('',#33455,#33453,#10909,.T.) ;
#40996 = EDGE_CURVE('',#33454,#33456,#27638,.T.) ;
#40997 = EDGE_CURVE('',#33456,#33457,#10910,.T.) ;
#40998 = EDGE_CURVE('',#33457,#33455,#27639,.T.) ;
#40999 = EDGE_CURVE('',#33456,#33458,#10911,.T.) ;
#41000 = EDGE_CURVE('',#33458,#33459,#10912,.T.) ;
#41001 = EDGE_CURVE('',#33459,#33457,#10913,.T.) ;
#41002 = EDGE_CURVE('',#33458,#33460,#27640,.T.) ;
#41003 = EDGE_CURVE('',#33460,#33461,#10914,.T.) ;
#41004 = EDGE_CURVE('',#33461,#33459,#27641,.T.) ;
#41005 = EDGE_CURVE('',#33460,#33462,#10915,.T.) ;
#41006 = EDGE_CURVE('',#33462,#33463,#10916,.T.) ;
#41007 = EDGE_CURVE('',#33463,#33461,#10917,.T.) ;
#41008 = EDGE_CURVE('',#33462,#33464,#27642,.T.) ;
#41009 = EDGE_CURVE('',#33464,#33465,#10918,.T.) ;
#41010 = EDGE_CURVE('',#33465,#33463,#27643,.T.) ;
#41011 = EDGE_CURVE('',#33464,#33466,#27644,.T.) ;
#41012 = EDGE_CURVE('',#33466,#33467,#10919,.T.) ;
#41013 = EDGE_CURVE('',#33467,#33465,#27645,.T.) ;
#41014 = EDGE_CURVE('',#33466,#33468,#27646,.T.) ;
#41015 = EDGE_CURVE('',#33468,#33469,#10920,.T.) ;
#41016 = EDGE_CURVE('',#33469,#33467,#27647,.T.) ;
#41017 = EDGE_CURVE('',#33468,#33470,#10921,.T.) ;
#41018 = EDGE_CURVE('',#33470,#33471,#10922,.T.) ;
#41019 = EDGE_CURVE('',#33471,#33469,#10923,.T.) ;
#41020 = EDGE_CURVE('',#33470,#33472,#27648,.T.) ;
#41021 = EDGE_CURVE('',#33472,#33473,#10924,.T.) ;
#41022 = EDGE_CURVE('',#33473,#33471,#27649,.T.) ;
#41023 = EDGE_CURVE('',#33472,#33474,#10925,.T.) ;
#41024 = EDGE_CURVE('',#33474,#33475,#10926,.T.) ;
#41025 = EDGE_CURVE('',#33475,#33473,#10927,.T.) ;
#41026 = EDGE_CURVE('',#33474,#33476,#27650,.T.) ;
#41027 = EDGE_CURVE('',#33476,#33477,#10928,.T.) ;
#41028 = EDGE_CURVE('',#33477,#33475,#27651,.T.) ;
#41029 = EDGE_CURVE('',#33476,#33428,#10929,.T.) ;
#41030 = EDGE_CURVE('',#33429,#33477,#10930,.T.) ;
#41031 = EDGE_CURVE('',#33478,#33479,#27652,.T.) ;
#41032 = EDGE_CURVE('',#33479,#33480,#10931,.T.) ;
#41033 = EDGE_CURVE('',#33480,#33481,#27653,.T.) ;
#41034 = EDGE_CURVE('',#33481,#33482,#10932,.T.) ;
#41035 = EDGE_CURVE('',#33482,#33483,#10933,.T.) ;
#41036 = EDGE_CURVE('',#33483,#33484,#10934,.T.) ;
#41037 = EDGE_CURVE('',#33484,#33485,#27654,.T.) ;
#41038 = EDGE_CURVE('',#33485,#33486,#10935,.T.) ;
#41039 = EDGE_CURVE('',#33486,#33487,#10936,.T.) ;
#41040 = EDGE_CURVE('',#33487,#33488,#10937,.T.) ;
#41041 = EDGE_CURVE('',#33488,#33489,#27655,.T.) ;
#41042 = EDGE_CURVE('',#33489,#33490,#10938,.T.) ;
#41043 = EDGE_CURVE('',#33490,#33491,#27656,.T.) ;
#41044 = EDGE_CURVE('',#33491,#33492,#10939,.T.) ;
#41045 = EDGE_CURVE('',#33492,#33493,#10940,.T.) ;
#41046 = EDGE_CURVE('',#33493,#32050,#10941,.T.) ;
#41047 = EDGE_CURVE('',#32050,#33494,#10942,.T.) ;
#41048 = EDGE_CURVE('',#33494,#33478,#10943,.T.) ;
#41049 = EDGE_CURVE('',#33495,#33496,#10944,.T.) ;
#41050 = EDGE_CURVE('',#33495,#33497,#27657,.T.) ;
#41051 = EDGE_CURVE('',#33497,#33498,#10945,.T.) ;
#41052 = EDGE_CURVE('',#33498,#33496,#27658,.T.) ;
#41053 = EDGE_CURVE('',#33497,#33499,#10946,.T.) ;
#41054 = EDGE_CURVE('',#33499,#33500,#10947,.T.) ;
#41055 = EDGE_CURVE('',#33500,#33498,#10948,.T.) ;
#41056 = EDGE_CURVE('',#33499,#33501,#27659,.T.) ;
#41057 = EDGE_CURVE('',#33501,#33502,#10949,.T.) ;
#41058 = EDGE_CURVE('',#33502,#33500,#27660,.T.) ;
#41059 = EDGE_CURVE('',#33501,#33503,#10950,.T.) ;
#41060 = EDGE_CURVE('',#33503,#33504,#10951,.T.) ;
#41061 = EDGE_CURVE('',#33504,#33502,#10952,.T.) ;
#41062 = EDGE_CURVE('',#33503,#33505,#27661,.T.) ;
#41063 = EDGE_CURVE('',#33505,#33506,#10953,.T.) ;
#41064 = EDGE_CURVE('',#33506,#33504,#27662,.T.) ;
#41065 = EDGE_CURVE('',#33505,#32063,#10954,.T.) ;
#41066 = EDGE_CURVE('',#32063,#33507,#10955,.T.) ;
#41067 = EDGE_CURVE('',#33507,#33506,#10956,.T.) ;
#41068 = EDGE_CURVE('',#32064,#33508,#10957,.T.) ;
#41069 = EDGE_CURVE('',#33508,#33507,#27663,.T.) ;
#41070 = EDGE_CURVE('',#32064,#32177,#10958,.T.) ;
#41071 = EDGE_CURVE('',#32139,#33508,#10959,.T.) ;
#41072 = EDGE_CURVE('',#32178,#33509,#10960,.T.) ;
#41073 = EDGE_CURVE('',#33509,#33510,#10961,.T.) ;
#41074 = EDGE_CURVE('',#33510,#32140,#10962,.T.) ;
#41075 = EDGE_CURVE('',#33509,#33511,#27664,.T.) ;
#41076 = EDGE_CURVE('',#33511,#33512,#10963,.T.) ;
#41077 = EDGE_CURVE('',#33512,#33510,#27665,.T.) ;
#41078 = EDGE_CURVE('',#33511,#33513,#10964,.T.) ;
#41079 = EDGE_CURVE('',#33513,#33514,#10965,.T.) ;
#41080 = EDGE_CURVE('',#33514,#33512,#10966,.T.) ;
#41081 = EDGE_CURVE('',#33513,#33515,#27666,.T.) ;
#41082 = EDGE_CURVE('',#33515,#33516,#10967,.T.) ;
#41083 = EDGE_CURVE('',#33516,#33514,#27667,.T.) ;
#41084 = EDGE_CURVE('',#33515,#33517,#10968,.T.) ;
#41085 = EDGE_CURVE('',#33517,#33518,#10969,.T.) ;
#41086 = EDGE_CURVE('',#33518,#33516,#10970,.T.) ;
#41087 = EDGE_CURVE('',#33517,#33519,#27668,.T.) ;
#41088 = EDGE_CURVE('',#33519,#33520,#10971,.T.) ;
#41089 = EDGE_CURVE('',#33520,#33518,#27669,.T.) ;
#41090 = EDGE_CURVE('',#33519,#33521,#10972,.T.) ;
#41091 = EDGE_CURVE('',#33521,#33522,#10973,.T.) ;
#41092 = EDGE_CURVE('',#33522,#33520,#10974,.T.) ;
#41093 = EDGE_CURVE('',#33521,#33523,#27670,.T.) ;
#41094 = EDGE_CURVE('',#33523,#33524,#10975,.T.) ;
#41095 = EDGE_CURVE('',#33524,#33522,#27671,.T.) ;
#41096 = EDGE_CURVE('',#33523,#33525,#10976,.T.) ;
#41097 = EDGE_CURVE('',#33525,#33526,#10977,.T.) ;
#41098 = EDGE_CURVE('',#33526,#33524,#10978,.T.) ;
#41099 = EDGE_CURVE('',#33525,#33527,#27672,.T.) ;
#41100 = EDGE_CURVE('',#33527,#33528,#10979,.T.) ;
#41101 = EDGE_CURVE('',#33528,#33526,#27673,.T.) ;
#41102 = EDGE_CURVE('',#33527,#33529,#10980,.T.) ;
#41103 = EDGE_CURVE('',#33529,#33530,#10981,.T.) ;
#41104 = EDGE_CURVE('',#33530,#33528,#10982,.T.) ;
#41105 = EDGE_CURVE('',#33529,#33531,#27674,.T.) ;
#41106 = EDGE_CURVE('',#33531,#33532,#10983,.T.) ;
#41107 = EDGE_CURVE('',#33532,#33530,#27675,.T.) ;
#41108 = EDGE_CURVE('',#33531,#33533,#27676,.T.) ;
#41109 = EDGE_CURVE('',#33533,#33534,#10984,.T.) ;
#41110 = EDGE_CURVE('',#33534,#33532,#27677,.T.) ;
#41111 = EDGE_CURVE('',#33533,#33535,#27678,.T.) ;
#41112 = EDGE_CURVE('',#33535,#33536,#10985,.T.) ;
#41113 = EDGE_CURVE('',#33536,#33534,#27679,.T.) ;
#41114 = EDGE_CURVE('',#33535,#33537,#10986,.T.) ;
#41115 = EDGE_CURVE('',#33537,#33538,#10987,.T.) ;
#41116 = EDGE_CURVE('',#33538,#33536,#10988,.T.) ;
#41117 = EDGE_CURVE('',#33537,#33539,#27680,.T.) ;
#41118 = EDGE_CURVE('',#33539,#33540,#10989,.T.) ;
#41119 = EDGE_CURVE('',#33540,#33538,#27681,.T.) ;
#41120 = EDGE_CURVE('',#33539,#33541,#10990,.T.) ;
#41121 = EDGE_CURVE('',#33541,#33542,#10991,.T.) ;
#41122 = EDGE_CURVE('',#33542,#33540,#10992,.T.) ;
#41123 = EDGE_CURVE('',#33541,#33543,#27682,.T.) ;
#41124 = EDGE_CURVE('',#33543,#33544,#10993,.T.) ;
#41125 = EDGE_CURVE('',#33544,#33542,#27683,.T.) ;
#41126 = EDGE_CURVE('',#33543,#33495,#10994,.T.) ;
#41127 = EDGE_CURVE('',#33496,#33544,#10995,.T.) ;
#41128 = EDGE_CURVE('',#33545,#33546,#27684,.T.) ;
#41129 = EDGE_CURVE('',#33546,#33547,#10996,.T.) ;
#41130 = EDGE_CURVE('',#33547,#33548,#27685,.T.) ;
#41131 = EDGE_CURVE('',#33548,#33549,#10997,.T.) ;
#41132 = EDGE_CURVE('',#33549,#33550,#10998,.T.) ;
#41133 = EDGE_CURVE('',#33550,#33551,#10999,.T.) ;
#41134 = EDGE_CURVE('',#33551,#33552,#27686,.T.) ;
#41135 = EDGE_CURVE('',#33552,#33553,#11000,.T.) ;
#41136 = EDGE_CURVE('',#33553,#33554,#11001,.T.) ;
#41137 = EDGE_CURVE('',#33554,#33555,#11002,.T.) ;
#41138 = EDGE_CURVE('',#33555,#33556,#27687,.T.) ;
#41139 = EDGE_CURVE('',#33556,#33557,#11003,.T.) ;
#41140 = EDGE_CURVE('',#33557,#33558,#27688,.T.) ;
#41141 = EDGE_CURVE('',#33558,#33559,#11004,.T.) ;
#41142 = EDGE_CURVE('',#33559,#33560,#11005,.T.) ;
#41143 = EDGE_CURVE('',#33560,#32065,#11006,.T.) ;
#41144 = EDGE_CURVE('',#32065,#33561,#11007,.T.) ;
#41145 = EDGE_CURVE('',#33561,#33545,#11008,.T.) ;
#41146 = EDGE_CURVE('',#33562,#33563,#11009,.T.) ;
#41147 = EDGE_CURVE('',#33562,#33564,#27689,.T.) ;
#41148 = EDGE_CURVE('',#33564,#33565,#11010,.T.) ;
#41149 = EDGE_CURVE('',#33565,#33563,#27690,.T.) ;
#41150 = EDGE_CURVE('',#33564,#33566,#11011,.T.) ;
#41151 = EDGE_CURVE('',#33566,#33567,#11012,.T.) ;
#41152 = EDGE_CURVE('',#33567,#33565,#11013,.T.) ;
#41153 = EDGE_CURVE('',#33566,#33568,#27691,.T.) ;
#41154 = EDGE_CURVE('',#33568,#33569,#11014,.T.) ;
#41155 = EDGE_CURVE('',#33569,#33567,#27692,.T.) ;
#41156 = EDGE_CURVE('',#33568,#33570,#11015,.T.) ;
#41157 = EDGE_CURVE('',#33570,#33571,#11016,.T.) ;
#41158 = EDGE_CURVE('',#33571,#33569,#11017,.T.) ;
#41159 = EDGE_CURVE('',#33570,#33572,#27693,.T.) ;
#41160 = EDGE_CURVE('',#33572,#33573,#11018,.T.) ;
#41161 = EDGE_CURVE('',#33573,#33571,#27694,.T.) ;
#41162 = EDGE_CURVE('',#33572,#32078,#11019,.T.) ;
#41163 = EDGE_CURVE('',#32078,#33574,#11020,.T.) ;
#41164 = EDGE_CURVE('',#33574,#33573,#11021,.T.) ;
#41165 = EDGE_CURVE('',#32079,#33575,#11022,.T.) ;
#41166 = EDGE_CURVE('',#33575,#33574,#27695,.T.) ;
#41167 = EDGE_CURVE('',#32079,#32175,#11023,.T.) ;
#41168 = EDGE_CURVE('',#32135,#33575,#11024,.T.) ;
#41169 = EDGE_CURVE('',#32176,#33576,#11025,.T.) ;
#41170 = EDGE_CURVE('',#33576,#33577,#11026,.T.) ;
#41171 = EDGE_CURVE('',#33577,#32136,#11027,.T.) ;
#41172 = EDGE_CURVE('',#33576,#33578,#27696,.T.) ;
#41173 = EDGE_CURVE('',#33578,#33579,#11028,.T.) ;
#41174 = EDGE_CURVE('',#33579,#33577,#27697,.T.) ;
#41175 = EDGE_CURVE('',#33578,#33580,#11029,.T.) ;
#41176 = EDGE_CURVE('',#33580,#33581,#11030,.T.) ;
#41177 = EDGE_CURVE('',#33581,#33579,#11031,.T.) ;
#41178 = EDGE_CURVE('',#33580,#33582,#27698,.T.) ;
#41179 = EDGE_CURVE('',#33582,#33583,#11032,.T.) ;
#41180 = EDGE_CURVE('',#33583,#33581,#27699,.T.) ;
#41181 = EDGE_CURVE('',#33582,#33584,#11033,.T.) ;
#41182 = EDGE_CURVE('',#33584,#33585,#11034,.T.) ;
#41183 = EDGE_CURVE('',#33585,#33583,#11035,.T.) ;
#41184 = EDGE_CURVE('',#33584,#33586,#27700,.T.) ;
#41185 = EDGE_CURVE('',#33586,#33587,#11036,.T.) ;
#41186 = EDGE_CURVE('',#33587,#33585,#27701,.T.) ;
#41187 = EDGE_CURVE('',#33586,#33588,#11037,.T.) ;
#41188 = EDGE_CURVE('',#33588,#33589,#11038,.T.) ;
#41189 = EDGE_CURVE('',#33589,#33587,#11039,.T.) ;
#41190 = EDGE_CURVE('',#33588,#33590,#27702,.T.) ;
#41191 = EDGE_CURVE('',#33590,#33591,#11040,.T.) ;
#41192 = EDGE_CURVE('',#33591,#33589,#27703,.T.) ;
#41193 = EDGE_CURVE('',#33590,#33592,#11041,.T.) ;
#41194 = EDGE_CURVE('',#33592,#33593,#11042,.T.) ;
#41195 = EDGE_CURVE('',#33593,#33591,#11043,.T.) ;
#41196 = EDGE_CURVE('',#33592,#33594,#27704,.T.) ;
#41197 = EDGE_CURVE('',#33594,#33595,#11044,.T.) ;
#41198 = EDGE_CURVE('',#33595,#33593,#27705,.T.) ;
#41199 = EDGE_CURVE('',#33594,#33596,#11045,.T.) ;
#41200 = EDGE_CURVE('',#33596,#33597,#11046,.T.) ;
#41201 = EDGE_CURVE('',#33597,#33595,#11047,.T.) ;
#41202 = EDGE_CURVE('',#33596,#33598,#27706,.T.) ;
#41203 = EDGE_CURVE('',#33598,#33599,#11048,.T.) ;
#41204 = EDGE_CURVE('',#33599,#33597,#27707,.T.) ;
#41205 = EDGE_CURVE('',#33598,#33600,#27708,.T.) ;
#41206 = EDGE_CURVE('',#33600,#33601,#11049,.T.) ;
#41207 = EDGE_CURVE('',#33601,#33599,#27709,.T.) ;
#41208 = EDGE_CURVE('',#33600,#33602,#27710,.T.) ;
#41209 = EDGE_CURVE('',#33602,#33603,#11050,.T.) ;
#41210 = EDGE_CURVE('',#33603,#33601,#27711,.T.) ;
#41211 = EDGE_CURVE('',#33602,#33604,#11051,.T.) ;
#41212 = EDGE_CURVE('',#33604,#33605,#11052,.T.) ;
#41213 = EDGE_CURVE('',#33605,#33603,#11053,.T.) ;
#41214 = EDGE_CURVE('',#33604,#33606,#27712,.T.) ;
#41215 = EDGE_CURVE('',#33606,#33607,#11054,.T.) ;
#41216 = EDGE_CURVE('',#33607,#33605,#27713,.T.) ;
#41217 = EDGE_CURVE('',#33606,#33608,#11055,.T.) ;
#41218 = EDGE_CURVE('',#33608,#33609,#11056,.T.) ;
#41219 = EDGE_CURVE('',#33609,#33607,#11057,.T.) ;
#41220 = EDGE_CURVE('',#33608,#33610,#27714,.T.) ;
#41221 = EDGE_CURVE('',#33610,#33611,#11058,.T.) ;
#41222 = EDGE_CURVE('',#33611,#33609,#27715,.T.) ;
#41223 = EDGE_CURVE('',#33610,#33562,#11059,.T.) ;
#41224 = EDGE_CURVE('',#33563,#33611,#11060,.T.) ;
#41225 = EDGE_CURVE('',#33612,#33613,#27716,.T.) ;
#41226 = EDGE_CURVE('',#33613,#33614,#11061,.T.) ;
#41227 = EDGE_CURVE('',#33614,#33615,#27717,.T.) ;
#41228 = EDGE_CURVE('',#33615,#33616,#11062,.T.) ;
#41229 = EDGE_CURVE('',#33616,#33617,#11063,.T.) ;
#41230 = EDGE_CURVE('',#33617,#33618,#11064,.T.) ;
#41231 = EDGE_CURVE('',#33618,#33619,#27718,.T.) ;
#41232 = EDGE_CURVE('',#33619,#33620,#11065,.T.) ;
#41233 = EDGE_CURVE('',#33620,#33621,#11066,.T.) ;
#41234 = EDGE_CURVE('',#33621,#33622,#11067,.T.) ;
#41235 = EDGE_CURVE('',#33622,#33623,#27719,.T.) ;
#41236 = EDGE_CURVE('',#33623,#33624,#11068,.T.) ;
#41237 = EDGE_CURVE('',#33624,#33625,#27720,.T.) ;
#41238 = EDGE_CURVE('',#33625,#33626,#11069,.T.) ;
#41239 = EDGE_CURVE('',#33626,#33627,#11070,.T.) ;
#41240 = EDGE_CURVE('',#33627,#32080,#11071,.T.) ;
#41241 = EDGE_CURVE('',#32080,#33628,#11072,.T.) ;
#41242 = EDGE_CURVE('',#33628,#33612,#11073,.T.) ;
#41243 = EDGE_CURVE('',#33629,#33630,#11074,.T.) ;
#41244 = EDGE_CURVE('',#33629,#33631,#27721,.T.) ;
#41245 = EDGE_CURVE('',#33631,#33632,#11075,.T.) ;
#41246 = EDGE_CURVE('',#33632,#33630,#27722,.T.) ;
#41247 = EDGE_CURVE('',#33631,#33633,#11076,.T.) ;
#41248 = EDGE_CURVE('',#33633,#33634,#11077,.T.) ;
#41249 = EDGE_CURVE('',#33634,#33632,#11078,.T.) ;
#41250 = EDGE_CURVE('',#33633,#33635,#27723,.T.) ;
#41251 = EDGE_CURVE('',#33635,#33636,#11079,.T.) ;
#41252 = EDGE_CURVE('',#33636,#33634,#27724,.T.) ;
#41253 = EDGE_CURVE('',#33635,#33637,#11080,.T.) ;
#41254 = EDGE_CURVE('',#33637,#33638,#11081,.T.) ;
#41255 = EDGE_CURVE('',#33638,#33636,#11082,.T.) ;
#41256 = EDGE_CURVE('',#33637,#33639,#27725,.T.) ;
#41257 = EDGE_CURVE('',#33639,#33640,#11083,.T.) ;
#41258 = EDGE_CURVE('',#33640,#33638,#27726,.T.) ;
#41259 = EDGE_CURVE('',#33639,#32093,#11084,.T.) ;
#41260 = EDGE_CURVE('',#32093,#33641,#11085,.T.) ;
#41261 = EDGE_CURVE('',#33641,#33640,#11086,.T.) ;
#41262 = EDGE_CURVE('',#32094,#33642,#11087,.T.) ;
#41263 = EDGE_CURVE('',#33642,#33641,#27727,.T.) ;
#41264 = EDGE_CURVE('',#32094,#32173,#11088,.T.) ;
#41265 = EDGE_CURVE('',#32131,#33642,#11089,.T.) ;
#41266 = EDGE_CURVE('',#32174,#33643,#11090,.T.) ;
#41267 = EDGE_CURVE('',#33643,#33644,#11091,.T.) ;
#41268 = EDGE_CURVE('',#33644,#32132,#11092,.T.) ;
#41269 = EDGE_CURVE('',#33643,#33645,#27728,.T.) ;
#41270 = EDGE_CURVE('',#33645,#33646,#11093,.T.) ;
#41271 = EDGE_CURVE('',#33646,#33644,#27729,.T.) ;
#41272 = EDGE_CURVE('',#33645,#33647,#11094,.T.) ;
#41273 = EDGE_CURVE('',#33647,#33648,#11095,.T.) ;
#41274 = EDGE_CURVE('',#33648,#33646,#11096,.T.) ;
#41275 = EDGE_CURVE('',#33647,#33649,#27730,.T.) ;
#41276 = EDGE_CURVE('',#33649,#33650,#11097,.T.) ;
#41277 = EDGE_CURVE('',#33650,#33648,#27731,.T.) ;
#41278 = EDGE_CURVE('',#33649,#33651,#11098,.T.) ;
#41279 = EDGE_CURVE('',#33651,#33652,#11099,.T.) ;
#41280 = EDGE_CURVE('',#33652,#33650,#11100,.T.) ;
#41281 = EDGE_CURVE('',#33651,#33653,#27732,.T.) ;
#41282 = EDGE_CURVE('',#33653,#33654,#11101,.T.) ;
#41283 = EDGE_CURVE('',#33654,#33652,#27733,.T.) ;
#41284 = EDGE_CURVE('',#33653,#33655,#11102,.T.) ;
#41285 = EDGE_CURVE('',#33655,#33656,#11103,.T.) ;
#41286 = EDGE_CURVE('',#33656,#33654,#11104,.T.) ;
#41287 = EDGE_CURVE('',#33655,#33657,#27734,.T.) ;
#41288 = EDGE_CURVE('',#33657,#33658,#11105,.T.) ;
#41289 = EDGE_CURVE('',#33658,#33656,#27735,.T.) ;
#41290 = EDGE_CURVE('',#33657,#33659,#11106,.T.) ;
#41291 = EDGE_CURVE('',#33659,#33660,#11107,.T.) ;
#41292 = EDGE_CURVE('',#33660,#33658,#11108,.T.) ;
#41293 = EDGE_CURVE('',#33659,#33661,#27736,.T.) ;
#41294 = EDGE_CURVE('',#33661,#33662,#11109,.T.) ;
#41295 = EDGE_CURVE('',#33662,#33660,#27737,.T.) ;
#41296 = EDGE_CURVE('',#33661,#33663,#11110,.T.) ;
#41297 = EDGE_CURVE('',#33663,#33664,#11111,.T.) ;
#41298 = EDGE_CURVE('',#33664,#33662,#11112,.T.) ;
#41299 = EDGE_CURVE('',#33663,#33665,#27738,.T.) ;
#41300 = EDGE_CURVE('',#33665,#33666,#11113,.T.) ;
#41301 = EDGE_CURVE('',#33666,#33664,#27739,.T.) ;
#41302 = EDGE_CURVE('',#33665,#33667,#27740,.T.) ;
#41303 = EDGE_CURVE('',#33667,#33668,#11114,.T.) ;
#41304 = EDGE_CURVE('',#33668,#33666,#27741,.T.) ;
#41305 = EDGE_CURVE('',#33667,#33669,#27742,.T.) ;
#41306 = EDGE_CURVE('',#33669,#33670,#11115,.T.) ;
#41307 = EDGE_CURVE('',#33670,#33668,#27743,.T.) ;
#41308 = EDGE_CURVE('',#33669,#33671,#11116,.T.) ;
#41309 = EDGE_CURVE('',#33671,#33672,#11117,.T.) ;
#41310 = EDGE_CURVE('',#33672,#33670,#11118,.T.) ;
#41311 = EDGE_CURVE('',#33671,#33673,#27744,.T.) ;
#41312 = EDGE_CURVE('',#33673,#33674,#11119,.T.) ;
#41313 = EDGE_CURVE('',#33674,#33672,#27745,.T.) ;
#41314 = EDGE_CURVE('',#33673,#33675,#11120,.T.) ;
#41315 = EDGE_CURVE('',#33675,#33676,#11121,.T.) ;
#41316 = EDGE_CURVE('',#33676,#33674,#11122,.T.) ;
#41317 = EDGE_CURVE('',#33675,#33677,#27746,.T.) ;
#41318 = EDGE_CURVE('',#33677,#33678,#11123,.T.) ;
#41319 = EDGE_CURVE('',#33678,#33676,#27747,.T.) ;
#41320 = EDGE_CURVE('',#33677,#33629,#11124,.T.) ;
#41321 = EDGE_CURVE('',#33630,#33678,#11125,.T.) ;
#41322 = EDGE_CURVE('',#33679,#33680,#27748,.T.) ;
#41323 = EDGE_CURVE('',#33680,#33681,#11126,.T.) ;
#41324 = EDGE_CURVE('',#33681,#33682,#27749,.T.) ;
#41325 = EDGE_CURVE('',#33682,#33683,#11127,.T.) ;
#41326 = EDGE_CURVE('',#33683,#33684,#11128,.T.) ;
#41327 = EDGE_CURVE('',#33684,#33685,#11129,.T.) ;
#41328 = EDGE_CURVE('',#33685,#33686,#27750,.T.) ;
#41329 = EDGE_CURVE('',#33686,#33687,#11130,.T.) ;
#41330 = EDGE_CURVE('',#33687,#33688,#11131,.T.) ;
#41331 = EDGE_CURVE('',#33688,#33689,#11132,.T.) ;
#41332 = EDGE_CURVE('',#33689,#33690,#27751,.T.) ;
#41333 = EDGE_CURVE('',#33690,#33691,#11133,.T.) ;
#41334 = EDGE_CURVE('',#33691,#33692,#27752,.T.) ;
#41335 = EDGE_CURVE('',#33692,#33693,#11134,.T.) ;
#41336 = EDGE_CURVE('',#33693,#33694,#11135,.T.) ;
#41337 = EDGE_CURVE('',#33694,#32095,#11136,.T.) ;
#41338 = EDGE_CURVE('',#32095,#33695,#11137,.T.) ;
#41339 = EDGE_CURVE('',#33695,#33679,#11138,.T.) ;
#41340 = EDGE_CURVE('',#33696,#33697,#11139,.T.) ;
#41341 = EDGE_CURVE('',#33696,#33698,#27753,.T.) ;
#41342 = EDGE_CURVE('',#33698,#33699,#11140,.T.) ;
#41343 = EDGE_CURVE('',#33699,#33697,#27754,.T.) ;
#41344 = EDGE_CURVE('',#33698,#33700,#11141,.T.) ;
#41345 = EDGE_CURVE('',#33700,#33701,#11142,.T.) ;
#41346 = EDGE_CURVE('',#33701,#33699,#11143,.T.) ;
#41347 = EDGE_CURVE('',#33700,#33702,#27755,.T.) ;
#41348 = EDGE_CURVE('',#33702,#33703,#11144,.T.) ;
#41349 = EDGE_CURVE('',#33703,#33701,#27756,.T.) ;
#41350 = EDGE_CURVE('',#33702,#33704,#11145,.T.) ;
#41351 = EDGE_CURVE('',#33704,#33705,#11146,.T.) ;
#41352 = EDGE_CURVE('',#33705,#33703,#11147,.T.) ;
#41353 = EDGE_CURVE('',#33704,#33706,#27757,.T.) ;
#41354 = EDGE_CURVE('',#33706,#33707,#11148,.T.) ;
#41355 = EDGE_CURVE('',#33707,#33705,#27758,.T.) ;
#41356 = EDGE_CURVE('',#33706,#32108,#11149,.T.) ;
#41357 = EDGE_CURVE('',#32108,#33708,#11150,.T.) ;
#41358 = EDGE_CURVE('',#33708,#33707,#11151,.T.) ;
#41359 = EDGE_CURVE('',#32109,#33709,#11152,.T.) ;
#41360 = EDGE_CURVE('',#33709,#33708,#27759,.T.) ;
#41361 = EDGE_CURVE('',#32109,#32171,#11153,.T.) ;
#41362 = EDGE_CURVE('',#32127,#33709,#11154,.T.) ;
#41363 = EDGE_CURVE('',#32172,#33710,#11155,.T.) ;
#41364 = EDGE_CURVE('',#33710,#33711,#11156,.T.) ;
#41365 = EDGE_CURVE('',#33711,#32128,#11157,.T.) ;
#41366 = EDGE_CURVE('',#33710,#33712,#27760,.T.) ;
#41367 = EDGE_CURVE('',#33712,#33713,#11158,.T.) ;
#41368 = EDGE_CURVE('',#33713,#33711,#27761,.T.) ;
#41369 = EDGE_CURVE('',#33712,#33714,#11159,.T.) ;
#41370 = EDGE_CURVE('',#33714,#33715,#11160,.T.) ;
#41371 = EDGE_CURVE('',#33715,#33713,#11161,.T.) ;
#41372 = EDGE_CURVE('',#33714,#33716,#27762,.T.) ;
#41373 = EDGE_CURVE('',#33716,#33717,#11162,.T.) ;
#41374 = EDGE_CURVE('',#33717,#33715,#27763,.T.) ;
#41375 = EDGE_CURVE('',#33716,#33718,#11163,.T.) ;
#41376 = EDGE_CURVE('',#33718,#33719,#11164,.T.) ;
#41377 = EDGE_CURVE('',#33719,#33717,#11165,.T.) ;
#41378 = EDGE_CURVE('',#33718,#33720,#27764,.T.) ;
#41379 = EDGE_CURVE('',#33720,#33721,#11166,.T.) ;
#41380 = EDGE_CURVE('',#33721,#33719,#27765,.T.) ;
#41381 = EDGE_CURVE('',#33720,#33722,#11167,.T.) ;
#41382 = EDGE_CURVE('',#33722,#33723,#11168,.T.) ;
#41383 = EDGE_CURVE('',#33723,#33721,#11169,.T.) ;
#41384 = EDGE_CURVE('',#33722,#33724,#27766,.T.) ;
#41385 = EDGE_CURVE('',#33724,#33725,#11170,.T.) ;
#41386 = EDGE_CURVE('',#33725,#33723,#27767,.T.) ;
#41387 = EDGE_CURVE('',#33724,#33726,#11171,.T.) ;
#41388 = EDGE_CURVE('',#33726,#33727,#11172,.T.) ;
#41389 = EDGE_CURVE('',#33727,#33725,#11173,.T.) ;
#41390 = EDGE_CURVE('',#33726,#33728,#27768,.T.) ;
#41391 = EDGE_CURVE('',#33728,#33729,#11174,.T.) ;
#41392 = EDGE_CURVE('',#33729,#33727,#27769,.T.) ;
#41393 = EDGE_CURVE('',#33728,#33730,#11175,.T.) ;
#41394 = EDGE_CURVE('',#33730,#33731,#11176,.T.) ;
#41395 = EDGE_CURVE('',#33731,#33729,#11177,.T.) ;
#41396 = EDGE_CURVE('',#33730,#33732,#27770,.T.) ;
#41397 = EDGE_CURVE('',#33732,#33733,#11178,.T.) ;
#41398 = EDGE_CURVE('',#33733,#33731,#27771,.T.) ;
#41399 = EDGE_CURVE('',#33732,#33734,#27772,.T.) ;
#41400 = EDGE_CURVE('',#33734,#33735,#11179,.T.) ;
#41401 = EDGE_CURVE('',#33735,#33733,#27773,.T.) ;
#41402 = EDGE_CURVE('',#33734,#33736,#27774,.T.) ;
#41403 = EDGE_CURVE('',#33736,#33737,#11180,.T.) ;
#41404 = EDGE_CURVE('',#33737,#33735,#27775,.T.) ;
#41405 = EDGE_CURVE('',#33736,#33738,#11181,.T.) ;
#41406 = EDGE_CURVE('',#33738,#33739,#11182,.T.) ;
#41407 = EDGE_CURVE('',#33739,#33737,#11183,.T.) ;
#41408 = EDGE_CURVE('',#33738,#33740,#27776,.T.) ;
#41409 = EDGE_CURVE('',#33740,#33741,#11184,.T.) ;
#41410 = EDGE_CURVE('',#33741,#33739,#27777,.T.) ;
#41411 = EDGE_CURVE('',#33740,#33742,#11185,.T.) ;
#41412 = EDGE_CURVE('',#33742,#33743,#11186,.T.) ;
#41413 = EDGE_CURVE('',#33743,#33741,#11187,.T.) ;
#41414 = EDGE_CURVE('',#33742,#33744,#27778,.T.) ;
#41415 = EDGE_CURVE('',#33744,#33745,#11188,.T.) ;
#41416 = EDGE_CURVE('',#33745,#33743,#27779,.T.) ;
#41417 = EDGE_CURVE('',#33744,#33696,#11189,.T.) ;
#41418 = EDGE_CURVE('',#33697,#33745,#11190,.T.) ;
#41419 = EDGE_CURVE('',#33746,#33747,#27780,.T.) ;
#41420 = EDGE_CURVE('',#33747,#33748,#11191,.T.) ;
#41421 = EDGE_CURVE('',#33748,#33749,#27781,.T.) ;
#41422 = EDGE_CURVE('',#33749,#33750,#11192,.T.) ;
#41423 = EDGE_CURVE('',#33750,#33751,#11193,.T.) ;
#41424 = EDGE_CURVE('',#33751,#33752,#11194,.T.) ;
#41425 = EDGE_CURVE('',#33752,#33753,#27782,.T.) ;
#41426 = EDGE_CURVE('',#33753,#33754,#11195,.T.) ;
#41427 = EDGE_CURVE('',#33754,#33755,#11196,.T.) ;
#41428 = EDGE_CURVE('',#33755,#33756,#11197,.T.) ;
#41429 = EDGE_CURVE('',#33756,#33757,#27783,.T.) ;
#41430 = EDGE_CURVE('',#33757,#33758,#11198,.T.) ;
#41431 = EDGE_CURVE('',#33758,#33759,#27784,.T.) ;
#41432 = EDGE_CURVE('',#33759,#33760,#11199,.T.) ;
#41433 = EDGE_CURVE('',#33760,#33761,#11200,.T.) ;
#41434 = EDGE_CURVE('',#33761,#32110,#11201,.T.) ;
#41435 = EDGE_CURVE('',#32110,#33762,#11202,.T.) ;
#41436 = EDGE_CURVE('',#33762,#33746,#11203,.T.) ;
#41437 = EDGE_CURVE('',#33763,#33764,#11204,.T.) ;
#41438 = EDGE_CURVE('',#33763,#33765,#27785,.T.) ;
#41439 = EDGE_CURVE('',#33765,#33766,#11205,.T.) ;
#41440 = EDGE_CURVE('',#33766,#33764,#27786,.T.) ;
#41441 = EDGE_CURVE('',#33765,#33767,#11206,.T.) ;
#41442 = EDGE_CURVE('',#33767,#33768,#11207,.T.) ;
#41443 = EDGE_CURVE('',#33768,#33766,#11208,.T.) ;
#41444 = EDGE_CURVE('',#33767,#33769,#27787,.T.) ;
#41445 = EDGE_CURVE('',#33769,#33770,#11209,.T.) ;
#41446 = EDGE_CURVE('',#33770,#33768,#27788,.T.) ;
#41447 = EDGE_CURVE('',#33769,#33771,#11210,.T.) ;
#41448 = EDGE_CURVE('',#33771,#33772,#11211,.T.) ;
#41449 = EDGE_CURVE('',#33772,#33770,#11212,.T.) ;
#41450 = EDGE_CURVE('',#33771,#33773,#27789,.T.) ;
#41451 = EDGE_CURVE('',#33773,#33774,#11213,.T.) ;
#41452 = EDGE_CURVE('',#33774,#33772,#27790,.T.) ;
#41453 = EDGE_CURVE('',#33773,#32159,#11214,.T.) ;
#41454 = EDGE_CURVE('',#32159,#33775,#11215,.T.) ;
#41455 = EDGE_CURVE('',#33775,#33774,#11216,.T.) ;
#41456 = EDGE_CURVE('',#32160,#33776,#11217,.T.) ;
#41457 = EDGE_CURVE('',#33776,#33775,#27791,.T.) ;
#41458 = EDGE_CURVE('',#32160,#32169,#11218,.T.) ;
#41459 = EDGE_CURVE('',#32123,#33776,#11219,.T.) ;
#41460 = EDGE_CURVE('',#32170,#33777,#11220,.T.) ;
#41461 = EDGE_CURVE('',#33777,#33778,#11221,.T.) ;
#41462 = EDGE_CURVE('',#33778,#32124,#11222,.T.) ;
#41463 = EDGE_CURVE('',#33777,#33779,#27792,.T.) ;
#41464 = EDGE_CURVE('',#33779,#33780,#11223,.T.) ;
#41465 = EDGE_CURVE('',#33780,#33778,#27793,.T.) ;
#41466 = EDGE_CURVE('',#33779,#33781,#11224,.T.) ;
#41467 = EDGE_CURVE('',#33781,#33782,#11225,.T.) ;
#41468 = EDGE_CURVE('',#33782,#33780,#11226,.T.) ;
#41469 = EDGE_CURVE('',#33781,#33783,#27794,.T.) ;
#41470 = EDGE_CURVE('',#33783,#33784,#11227,.T.) ;
#41471 = EDGE_CURVE('',#33784,#33782,#27795,.T.) ;
#41472 = EDGE_CURVE('',#33783,#33785,#11228,.T.) ;
#41473 = EDGE_CURVE('',#33785,#33786,#11229,.T.) ;
#41474 = EDGE_CURVE('',#33786,#33784,#11230,.T.) ;
#41475 = EDGE_CURVE('',#33785,#33787,#27796,.T.) ;
#41476 = EDGE_CURVE('',#33787,#33788,#11231,.T.) ;
#41477 = EDGE_CURVE('',#33788,#33786,#27797,.T.) ;
#41478 = EDGE_CURVE('',#33787,#33789,#11232,.T.) ;
#41479 = EDGE_CURVE('',#33789,#33790,#11233,.T.) ;
#41480 = EDGE_CURVE('',#33790,#33788,#11234,.T.) ;
#41481 = EDGE_CURVE('',#33789,#33791,#27798,.T.) ;
#41482 = EDGE_CURVE('',#33791,#33792,#11235,.T.) ;
#41483 = EDGE_CURVE('',#33792,#33790,#27799,.T.) ;
#41484 = EDGE_CURVE('',#33791,#33793,#11236,.T.) ;
#41485 = EDGE_CURVE('',#33793,#33794,#11237,.T.) ;
#41486 = EDGE_CURVE('',#33794,#33792,#11238,.T.) ;
#41487 = EDGE_CURVE('',#33793,#33795,#27800,.T.) ;
#41488 = EDGE_CURVE('',#33795,#33796,#11239,.T.) ;
#41489 = EDGE_CURVE('',#33796,#33794,#27801,.T.) ;
#41490 = EDGE_CURVE('',#33795,#33797,#11240,.T.) ;
#41491 = EDGE_CURVE('',#33797,#33798,#11241,.T.) ;
#41492 = EDGE_CURVE('',#33798,#33796,#11242,.T.) ;
#41493 = EDGE_CURVE('',#33797,#33799,#27802,.T.) ;
#41494 = EDGE_CURVE('',#33799,#33800,#11243,.T.) ;
#41495 = EDGE_CURVE('',#33800,#33798,#27803,.T.) ;
#41496 = EDGE_CURVE('',#33799,#33801,#27804,.T.) ;
#41497 = EDGE_CURVE('',#33801,#33802,#11244,.T.) ;
#41498 = EDGE_CURVE('',#33802,#33800,#27805,.T.) ;
#41499 = EDGE_CURVE('',#33801,#33803,#27806,.T.) ;
#41500 = EDGE_CURVE('',#33803,#33804,#11245,.T.) ;
#41501 = EDGE_CURVE('',#33804,#33802,#27807,.T.) ;
#41502 = EDGE_CURVE('',#33803,#33805,#11246,.T.) ;
#41503 = EDGE_CURVE('',#33805,#33806,#11247,.T.) ;
#41504 = EDGE_CURVE('',#33806,#33804,#11248,.T.) ;
#41505 = EDGE_CURVE('',#33805,#33807,#27808,.T.) ;
#41506 = EDGE_CURVE('',#33807,#33808,#11249,.T.) ;
#41507 = EDGE_CURVE('',#33808,#33806,#27809,.T.) ;
#41508 = EDGE_CURVE('',#33807,#33809,#11250,.T.) ;
#41509 = EDGE_CURVE('',#33809,#33810,#11251,.T.) ;
#41510 = EDGE_CURVE('',#33810,#33808,#11252,.T.) ;
#41511 = EDGE_CURVE('',#33809,#33811,#27810,.T.) ;
#41512 = EDGE_CURVE('',#33811,#33812,#11253,.T.) ;
#41513 = EDGE_CURVE('',#33812,#33810,#27811,.T.) ;
#41514 = EDGE_CURVE('',#33811,#33763,#11254,.T.) ;
#41515 = EDGE_CURVE('',#33764,#33812,#11255,.T.) ;
#41516 = EDGE_CURVE('',#33813,#33814,#27812,.T.) ;
#41517 = EDGE_CURVE('',#33814,#33815,#11256,.T.) ;
#41518 = EDGE_CURVE('',#33815,#33816,#27813,.T.) ;
#41519 = EDGE_CURVE('',#33816,#33817,#11257,.T.) ;
#41520 = EDGE_CURVE('',#33817,#33818,#11258,.T.) ;
#41521 = EDGE_CURVE('',#33818,#33819,#11259,.T.) ;
#41522 = EDGE_CURVE('',#33819,#33820,#27814,.T.) ;
#41523 = EDGE_CURVE('',#33820,#33821,#11260,.T.) ;
#41524 = EDGE_CURVE('',#33821,#33822,#11261,.T.) ;
#41525 = EDGE_CURVE('',#33822,#33823,#11262,.T.) ;
#41526 = EDGE_CURVE('',#33823,#33824,#27815,.T.) ;
#41527 = EDGE_CURVE('',#33824,#33825,#11263,.T.) ;
#41528 = EDGE_CURVE('',#33825,#33826,#27816,.T.) ;
#41529 = EDGE_CURVE('',#33826,#33827,#11264,.T.) ;
#41530 = EDGE_CURVE('',#33827,#33828,#11265,.T.) ;
#41531 = EDGE_CURVE('',#33828,#32161,#11266,.T.) ;
#41532 = EDGE_CURVE('',#32161,#33829,#11267,.T.) ;
#41533 = EDGE_CURVE('',#33829,#33813,#11268,.T.) ;
#41534 = EDGE_CURVE('',#33830,#33831,#11269,.T.) ;
#41535 = EDGE_CURVE('',#33830,#33832,#27817,.T.) ;
#41536 = EDGE_CURVE('',#33832,#33833,#11270,.T.) ;
#41537 = EDGE_CURVE('',#33833,#33834,#27818,.T.) ;
#41538 = EDGE_CURVE('',#33834,#33835,#11271,.T.) ;
#41539 = EDGE_CURVE('',#33835,#33836,#27819,.T.) ;
#41540 = EDGE_CURVE('',#33836,#33837,#11272,.T.) ;
#41541 = EDGE_CURVE('',#33837,#33831,#27820,.T.) ;
#41542 = EDGE_CURVE('',#33838,#33839,#11273,.T.) ;
#41543 = EDGE_CURVE('',#33838,#33840,#27821,.T.) ;
#41544 = EDGE_CURVE('',#33840,#33841,#11274,.T.) ;
#41545 = EDGE_CURVE('',#33841,#33842,#27822,.T.) ;
#41546 = EDGE_CURVE('',#33842,#33843,#11275,.T.) ;
#41547 = EDGE_CURVE('',#33843,#33844,#27823,.T.) ;
#41548 = EDGE_CURVE('',#33844,#33845,#11276,.T.) ;
#41549 = EDGE_CURVE('',#33845,#33839,#27824,.T.) ;
#41550 = EDGE_CURVE('',#33846,#33847,#11277,.T.) ;
#41551 = EDGE_CURVE('',#33846,#33848,#27825,.T.) ;
#41552 = EDGE_CURVE('',#33848,#33849,#11278,.T.) ;
#41553 = EDGE_CURVE('',#33849,#33850,#27826,.T.) ;
#41554 = EDGE_CURVE('',#33850,#33851,#11279,.T.) ;
#41555 = EDGE_CURVE('',#33851,#33852,#27827,.T.) ;
#41556 = EDGE_CURVE('',#33852,#33853,#11280,.T.) ;
#41557 = EDGE_CURVE('',#33853,#33847,#27828,.T.) ;
#41558 = EDGE_CURVE('',#33854,#33855,#11281,.T.) ;
#41559 = EDGE_CURVE('',#33854,#33856,#27829,.T.) ;
#41560 = EDGE_CURVE('',#33856,#33857,#11282,.T.) ;
#41561 = EDGE_CURVE('',#33857,#33858,#27830,.T.) ;
#41562 = EDGE_CURVE('',#33858,#33859,#11283,.T.) ;
#41563 = EDGE_CURVE('',#33859,#33860,#27831,.T.) ;
#41564 = EDGE_CURVE('',#33860,#33861,#11284,.T.) ;
#41565 = EDGE_CURVE('',#33861,#33855,#27832,.T.) ;
#41566 = EDGE_CURVE('',#33862,#33863,#11285,.T.) ;
#41567 = EDGE_CURVE('',#33862,#33864,#27833,.T.) ;
#41568 = EDGE_CURVE('',#33864,#33865,#11286,.T.) ;
#41569 = EDGE_CURVE('',#33865,#33866,#27834,.T.) ;
#41570 = EDGE_CURVE('',#33866,#33867,#11287,.T.) ;
#41571 = EDGE_CURVE('',#33867,#33868,#27835,.T.) ;
#41572 = EDGE_CURVE('',#33868,#33869,#11288,.T.) ;
#41573 = EDGE_CURVE('',#33869,#33863,#27836,.T.) ;
#41574 = EDGE_CURVE('',#33870,#33871,#11289,.T.) ;
#41575 = EDGE_CURVE('',#33870,#33872,#27837,.T.) ;
#41576 = EDGE_CURVE('',#33872,#33873,#11290,.T.) ;
#41577 = EDGE_CURVE('',#33873,#33874,#27838,.T.) ;
#41578 = EDGE_CURVE('',#33874,#33875,#11291,.T.) ;
#41579 = EDGE_CURVE('',#33875,#33876,#27839,.T.) ;
#41580 = EDGE_CURVE('',#33876,#33877,#11292,.T.) ;
#41581 = EDGE_CURVE('',#33877,#33871,#27840,.T.) ;
#41582 = EDGE_CURVE('',#33878,#33879,#11293,.T.) ;
#41583 = EDGE_CURVE('',#33878,#33880,#27841,.T.) ;
#41584 = EDGE_CURVE('',#33880,#33881,#11294,.T.) ;
#41585 = EDGE_CURVE('',#33881,#33882,#27842,.T.) ;
#41586 = EDGE_CURVE('',#33882,#33883,#11295,.T.) ;
#41587 = EDGE_CURVE('',#33883,#33884,#27843,.T.) ;
#41588 = EDGE_CURVE('',#33884,#33885,#11296,.T.) ;
#41589 = EDGE_CURVE('',#33885,#33879,#27844,.T.) ;
#41590 = EDGE_CURVE('',#33886,#33887,#11297,.T.) ;
#41591 = EDGE_CURVE('',#33886,#33888,#27845,.T.) ;
#41592 = EDGE_CURVE('',#33888,#33889,#11298,.T.) ;
#41593 = EDGE_CURVE('',#33889,#33890,#27846,.T.) ;
#41594 = EDGE_CURVE('',#33890,#33891,#11299,.T.) ;
#41595 = EDGE_CURVE('',#33891,#33892,#27847,.T.) ;
#41596 = EDGE_CURVE('',#33892,#33893,#11300,.T.) ;
#41597 = EDGE_CURVE('',#33893,#33887,#27848,.T.) ;
#41598 = EDGE_CURVE('',#33894,#33895,#11301,.T.) ;
#41599 = EDGE_CURVE('',#33894,#33896,#27849,.T.) ;
#41600 = EDGE_CURVE('',#33896,#33897,#11302,.T.) ;
#41601 = EDGE_CURVE('',#33897,#33898,#27850,.T.) ;
#41602 = EDGE_CURVE('',#33898,#33899,#11303,.T.) ;
#41603 = EDGE_CURVE('',#33899,#33900,#27851,.T.) ;
#41604 = EDGE_CURVE('',#33900,#33901,#11304,.T.) ;
#41605 = EDGE_CURVE('',#33901,#33895,#27852,.T.) ;
#41606 = EDGE_CURVE('',#33077,#33064,#27853,.T.) ;
#41607 = EDGE_CURVE('',#33055,#33076,#27854,.T.) ;
#41608 = EDGE_CURVE('',#33078,#33071,#27855,.T.) ;
#41609 = EDGE_CURVE('',#33072,#33077,#27856,.T.) ;
#41610 = EDGE_CURVE('',#33078,#33902,#27857,.T.) ;
#41611 = EDGE_CURVE('',#33902,#33071,#27858,.T.) ;
#41612 = EDGE_CURVE('',#33055,#33081,#27859,.T.) ;
#41613 = EDGE_CURVE('',#33081,#33076,#27860,.T.) ;
#41614 = EDGE_CURVE('',#33072,#33063,#27861,.T.) ;
#41615 = EDGE_CURVE('',#32162,#33074,#27862,.T.) ;
#41616 = EDGE_CURVE('',#32163,#33903,#303,.T.) ;
#41617 = EDGE_CURVE('',#33902,#33903,#11305,.T.) ;
#41618 = EDGE_CURVE('',#33904,#33902,#304,.T.) ;
#41619 = EDGE_CURVE('',#33904,#33905,#305,.T.) ;
#41620 = EDGE_CURVE('',#32289,#33905,#11306,.T.) ;
#41621 = EDGE_CURVE('',#33075,#32288,#27863,.T.) ;
#41622 = EDGE_CURVE('',#33082,#33075,#27864,.T.) ;
#41623 = EDGE_CURVE('',#33056,#33080,#27865,.T.) ;
#41624 = EDGE_CURVE('',#33073,#33062,#27866,.T.) ;
#41625 = EDGE_CURVE('',#33074,#32164,#27867,.T.) ;
#41626 = EDGE_CURVE('',#33069,#33073,#27868,.T.) ;
#41627 = EDGE_CURVE('',#33082,#32297,#27869,.T.) ;
#41628 = EDGE_CURVE('',#33056,#32384,#27870,.T.) ;
#41629 = EDGE_CURVE('',#32383,#33080,#27871,.T.) ;
#41630 = EDGE_CURVE('',#33069,#33061,#27872,.T.) ;
#41631 = EDGE_CURVE('',#33079,#32296,#27873,.T.) ;
#41632 = EDGE_CURVE('',#32385,#33079,#27874,.T.) ;
#41633 = EDGE_CURVE('',#33906,#32384,#11307,.T.) ;
#41634 = EDGE_CURVE('',#33057,#33906,#27875,.T.) ;
#41635 = EDGE_CURVE('',#33070,#33060,#27876,.T.) ;
#41636 = EDGE_CURVE('',#32165,#33065,#27877,.T.) ;
#41637 = EDGE_CURVE('',#33066,#33070,#27878,.T.) ;
#41638 = EDGE_CURVE('',#32292,#33065,#27879,.T.) ;
#41639 = EDGE_CURVE('',#32385,#32296,#27880,.T.) ;
#41640 = EDGE_CURVE('',#32390,#32387,#27881,.T.) ;
#41641 = EDGE_CURVE('',#32387,#32388,#27882,.T.) ;
#41642 = EDGE_CURVE('',#33906,#32529,#27883,.T.) ;
#41643 = EDGE_CURVE('',#33907,#33906,#27884,.T.) ;
#41644 = EDGE_CURVE('',#33057,#33907,#27885,.T.) ;
#41645 = EDGE_CURVE('',#33066,#33060,#27886,.T.) ;
#41646 = EDGE_CURVE('',#32293,#33068,#27887,.T.) ;
#41647 = EDGE_CURVE('',#32386,#32295,#27888,.T.) ;
#41648 = EDGE_CURVE('',#32460,#32386,#27889,.T.) ;
#41649 = EDGE_CURVE('',#33907,#32528,#27890,.T.) ;
#41650 = EDGE_CURVE('',#33908,#33907,#11308,.T.) ;
#41651 = EDGE_CURVE('',#33058,#33908,#27891,.T.) ;
#41652 = EDGE_CURVE('',#33067,#33059,#27892,.T.) ;
#41653 = EDGE_CURVE('',#33068,#32382,#27893,.T.) ;
#41654 = EDGE_CURVE('',#32379,#33067,#27894,.T.) ;
#41655 = EDGE_CURVE('',#32293,#32382,#27895,.T.) ;
#41656 = EDGE_CURVE('',#32461,#32295,#27896,.T.) ;
#41657 = EDGE_CURVE('',#33908,#32527,#27897,.T.) ;
#41658 = EDGE_CURVE('',#33909,#33908,#27898,.T.) ;
#41659 = EDGE_CURVE('',#33058,#33909,#27899,.T.) ;
#41660 = EDGE_CURVE('',#32378,#33059,#27900,.T.) ;
#41661 = EDGE_CURVE('',#32294,#32381,#27901,.T.) ;
#41662 = EDGE_CURVE('',#32462,#32294,#27902,.T.) ;
#41663 = EDGE_CURVE('',#33909,#32526,#27903,.T.) ;
#41664 = EDGE_CURVE('',#32378,#33909,#11309,.T.) ;
#41665 = EDGE_CURVE('',#32463,#32381,#27904,.T.) ;
#41666 = EDGE_CURVE('',#32380,#32393,#27905,.T.) ;
#41667 = EDGE_CURVE('',#32395,#32380,#27906,.T.) ;
#41668 = EDGE_CURVE('',#33789,#33822,#27907,.T.) ;
#41669 = EDGE_CURVE('',#33823,#33787,#27908,.T.) ;
#41670 = EDGE_CURVE('',#33824,#33785,#27909,.T.) ;
#41671 = EDGE_CURVE('',#33791,#33822,#27910,.T.) ;
#41672 = EDGE_CURVE('',#33825,#33783,#27911,.T.) ;
#41673 = EDGE_CURVE('',#33793,#33821,#27912,.T.) ;
#41674 = EDGE_CURVE('',#33826,#33781,#27913,.T.) ;
#41675 = EDGE_CURVE('',#33795,#33821,#27914,.T.) ;
#41676 = EDGE_CURVE('',#33827,#33779,#27915,.T.) ;
#41677 = EDGE_CURVE('',#33797,#33820,#27916,.T.) ;
#41678 = EDGE_CURVE('',#33827,#33777,#27917,.T.) ;
#41679 = EDGE_CURVE('',#33799,#33820,#27918,.T.) ;
#41680 = EDGE_CURVE('',#33828,#32170,#27919,.T.) ;
#41681 = EDGE_CURVE('',#33801,#33819,#27920,.T.) ;
#41682 = EDGE_CURVE('',#33828,#32169,#27921,.T.) ;
#41683 = EDGE_CURVE('',#33803,#33819,#27922,.T.) ;
#41684 = EDGE_CURVE('',#33805,#33818,#27923,.T.) ;
#41685 = EDGE_CURVE('',#33807,#33818,#27924,.T.) ;
#41686 = EDGE_CURVE('',#33829,#33773,#27925,.T.) ;
#41687 = EDGE_CURVE('',#33809,#33817,#27926,.T.) ;
#41688 = EDGE_CURVE('',#33829,#33771,#27927,.T.) ;
#41689 = EDGE_CURVE('',#33811,#33817,#27928,.T.) ;
#41690 = EDGE_CURVE('',#33813,#33769,#27929,.T.) ;
#41691 = EDGE_CURVE('',#33763,#33816,#27930,.T.) ;
#41692 = EDGE_CURVE('',#33814,#33767,#27931,.T.) ;
#41693 = EDGE_CURVE('',#33765,#33815,#27932,.T.) ;
#41694 = EDGE_CURVE('',#33248,#32570,#27933,.T.) ;
#41695 = EDGE_CURVE('',#32571,#33250,#27934,.T.) ;
#41696 = EDGE_CURVE('',#33246,#32570,#27935,.T.) ;
#41697 = EDGE_CURVE('',#32571,#33252,#27936,.T.) ;
#41698 = EDGE_CURVE('',#33244,#32569,#27937,.T.) ;
#41699 = EDGE_CURVE('',#32572,#33254,#27938,.T.) ;
#41700 = EDGE_CURVE('',#33242,#32568,#27939,.T.) ;
#41701 = EDGE_CURVE('',#32573,#33256,#27940,.T.) ;
#41702 = EDGE_CURVE('',#32574,#33258,#27941,.T.) ;
#41703 = EDGE_CURVE('',#32575,#33260,#27942,.T.) ;
#41704 = EDGE_CURVE('',#33240,#32567,#27943,.T.) ;
#41705 = EDGE_CURVE('',#32576,#33262,#27944,.T.) ;
#41706 = EDGE_CURVE('',#33239,#32566,#27945,.T.) ;
#41707 = EDGE_CURVE('',#32577,#33264,#27946,.T.) ;
#41708 = EDGE_CURVE('',#33238,#32565,#27947,.T.) ;
#41709 = EDGE_CURVE('',#32578,#33266,#27948,.T.) ;
#41710 = EDGE_CURVE('',#33236,#32564,#27949,.T.) ;
#41711 = EDGE_CURVE('',#32579,#33268,#27950,.T.) ;
#41712 = EDGE_CURVE('',#33234,#32563,#27951,.T.) ;
#41713 = EDGE_CURVE('',#32580,#33270,#27952,.T.) ;
#41714 = EDGE_CURVE('',#33232,#32563,#27953,.T.) ;
#41715 = EDGE_CURVE('',#32581,#33272,#27954,.T.) ;
#41716 = EDGE_CURVE('',#33230,#32562,#27955,.T.) ;
#41717 = EDGE_CURVE('',#32560,#33274,#27956,.T.) ;
#41718 = EDGE_CURVE('',#33228,#32562,#27957,.T.) ;
#41719 = EDGE_CURVE('',#32561,#33276,#27958,.T.) ;
#41720 = EDGE_CURVE('',#33315,#32592,#27959,.T.) ;
#41721 = EDGE_CURVE('',#32593,#33317,#27960,.T.) ;
#41722 = EDGE_CURVE('',#33313,#32592,#27961,.T.) ;
#41723 = EDGE_CURVE('',#32593,#33319,#27962,.T.) ;
#41724 = EDGE_CURVE('',#33311,#32591,#27963,.T.) ;
#41725 = EDGE_CURVE('',#32594,#33321,#27964,.T.) ;
#41726 = EDGE_CURVE('',#33309,#32590,#27965,.T.) ;
#41727 = EDGE_CURVE('',#32595,#33323,#27966,.T.) ;
#41728 = EDGE_CURVE('',#32596,#33325,#27967,.T.) ;
#41729 = EDGE_CURVE('',#32597,#33327,#27968,.T.) ;
#41730 = EDGE_CURVE('',#33307,#32589,#27969,.T.) ;
#41731 = EDGE_CURVE('',#32598,#33329,#27970,.T.) ;
#41732 = EDGE_CURVE('',#33306,#32588,#27971,.T.) ;
#41733 = EDGE_CURVE('',#32599,#33331,#27972,.T.) ;
#41734 = EDGE_CURVE('',#33305,#32587,#27973,.T.) ;
#41735 = EDGE_CURVE('',#32600,#33333,#27974,.T.) ;
#41736 = EDGE_CURVE('',#33303,#32586,#27975,.T.) ;
#41737 = EDGE_CURVE('',#32601,#33335,#27976,.T.) ;
#41738 = EDGE_CURVE('',#33301,#32585,#27977,.T.) ;
#41739 = EDGE_CURVE('',#32602,#33337,#27978,.T.) ;
#41740 = EDGE_CURVE('',#33299,#32585,#27979,.T.) ;
#41741 = EDGE_CURVE('',#32603,#33339,#27980,.T.) ;
#41742 = EDGE_CURVE('',#33297,#32584,#27981,.T.) ;
#41743 = EDGE_CURVE('',#32582,#33341,#27982,.T.) ;
#41744 = EDGE_CURVE('',#33295,#32584,#27983,.T.) ;
#41745 = EDGE_CURVE('',#32583,#33343,#27984,.T.) ;
#41746 = EDGE_CURVE('',#33382,#32614,#27985,.T.) ;
#41747 = EDGE_CURVE('',#32615,#33384,#27986,.T.) ;
#41748 = EDGE_CURVE('',#33380,#32614,#27987,.T.) ;
#41749 = EDGE_CURVE('',#32615,#33386,#27988,.T.) ;
#41750 = EDGE_CURVE('',#33378,#32613,#27989,.T.) ;
#41751 = EDGE_CURVE('',#32616,#33388,#27990,.T.) ;
#41752 = EDGE_CURVE('',#33376,#32612,#27991,.T.) ;
#41753 = EDGE_CURVE('',#32617,#33390,#27992,.T.) ;
#41754 = EDGE_CURVE('',#32618,#33392,#27993,.T.) ;
#41755 = EDGE_CURVE('',#32619,#33394,#27994,.T.) ;
#41756 = EDGE_CURVE('',#33374,#32611,#27995,.T.) ;
#41757 = EDGE_CURVE('',#32620,#33396,#27996,.T.) ;
#41758 = EDGE_CURVE('',#33373,#32610,#27997,.T.) ;
#41759 = EDGE_CURVE('',#32621,#33398,#27998,.T.) ;
#41760 = EDGE_CURVE('',#33372,#32609,#27999,.T.) ;
#41761 = EDGE_CURVE('',#32622,#33400,#28000,.T.) ;
#41762 = EDGE_CURVE('',#33370,#32608,#28001,.T.) ;
#41763 = EDGE_CURVE('',#32623,#33402,#28002,.T.) ;
#41764 = EDGE_CURVE('',#33368,#32607,#28003,.T.) ;
#41765 = EDGE_CURVE('',#32624,#33404,#28004,.T.) ;
#41766 = EDGE_CURVE('',#33366,#32607,#28005,.T.) ;
#41767 = EDGE_CURVE('',#32625,#33406,#28006,.T.) ;
#41768 = EDGE_CURVE('',#33364,#32606,#28007,.T.) ;
#41769 = EDGE_CURVE('',#32604,#33408,#28008,.T.) ;
#41770 = EDGE_CURVE('',#33362,#32606,#28009,.T.) ;
#41771 = EDGE_CURVE('',#32605,#33410,#28010,.T.) ;
#41772 = EDGE_CURVE('',#33449,#32636,#28011,.T.) ;
#41773 = EDGE_CURVE('',#32637,#33451,#28012,.T.) ;
#41774 = EDGE_CURVE('',#33447,#32636,#28013,.T.) ;
#41775 = EDGE_CURVE('',#32637,#33453,#28014,.T.) ;
#41776 = EDGE_CURVE('',#33445,#32635,#28015,.T.) ;
#41777 = EDGE_CURVE('',#32638,#33455,#28016,.T.) ;
#41778 = EDGE_CURVE('',#33443,#32634,#28017,.T.) ;
#41779 = EDGE_CURVE('',#32639,#33457,#28018,.T.) ;
#41780 = EDGE_CURVE('',#32640,#33459,#28019,.T.) ;
#41781 = EDGE_CURVE('',#32641,#33461,#28020,.T.) ;
#41782 = EDGE_CURVE('',#33441,#32633,#28021,.T.) ;
#41783 = EDGE_CURVE('',#32642,#33463,#28022,.T.) ;
#41784 = EDGE_CURVE('',#33440,#32632,#28023,.T.) ;
#41785 = EDGE_CURVE('',#32643,#33465,#28024,.T.) ;
#41786 = EDGE_CURVE('',#33439,#32631,#28025,.T.) ;
#41787 = EDGE_CURVE('',#32644,#33467,#28026,.T.) ;
#41788 = EDGE_CURVE('',#33437,#32630,#28027,.T.) ;
#41789 = EDGE_CURVE('',#32645,#33469,#28028,.T.) ;
#41790 = EDGE_CURVE('',#33435,#32629,#28029,.T.) ;
#41791 = EDGE_CURVE('',#32646,#33471,#28030,.T.) ;
#41792 = EDGE_CURVE('',#33433,#32629,#28031,.T.) ;
#41793 = EDGE_CURVE('',#32647,#33473,#28032,.T.) ;
#41794 = EDGE_CURVE('',#33431,#32628,#28033,.T.) ;
#41795 = EDGE_CURVE('',#32626,#33475,#28034,.T.) ;
#41796 = EDGE_CURVE('',#33429,#32628,#28035,.T.) ;
#41797 = EDGE_CURVE('',#32627,#33477,#28036,.T.) ;
#41798 = EDGE_CURVE('',#33516,#32658,#28037,.T.) ;
#41799 = EDGE_CURVE('',#32659,#33518,#28038,.T.) ;
#41800 = EDGE_CURVE('',#33514,#32658,#28039,.T.) ;
#41801 = EDGE_CURVE('',#32659,#33520,#28040,.T.) ;
#41802 = EDGE_CURVE('',#33512,#32657,#28041,.T.) ;
#41803 = EDGE_CURVE('',#32660,#33522,#28042,.T.) ;
#41804 = EDGE_CURVE('',#33510,#32656,#28043,.T.) ;
#41805 = EDGE_CURVE('',#32661,#33524,#28044,.T.) ;
#41806 = EDGE_CURVE('',#32662,#33526,#28045,.T.) ;
#41807 = EDGE_CURVE('',#32663,#33528,#28046,.T.) ;
#41808 = EDGE_CURVE('',#33508,#32655,#28047,.T.) ;
#41809 = EDGE_CURVE('',#32664,#33530,#28048,.T.) ;
#41810 = EDGE_CURVE('',#33507,#32654,#28049,.T.) ;
#41811 = EDGE_CURVE('',#32665,#33532,#28050,.T.) ;
#41812 = EDGE_CURVE('',#33506,#32653,#28051,.T.) ;
#41813 = EDGE_CURVE('',#32666,#33534,#28052,.T.) ;
#41814 = EDGE_CURVE('',#33504,#32652,#28053,.T.) ;
#41815 = EDGE_CURVE('',#32667,#33536,#28054,.T.) ;
#41816 = EDGE_CURVE('',#33502,#32651,#28055,.T.) ;
#41817 = EDGE_CURVE('',#32668,#33538,#28056,.T.) ;
#41818 = EDGE_CURVE('',#33500,#32651,#28057,.T.) ;
#41819 = EDGE_CURVE('',#32669,#33540,#28058,.T.) ;
#41820 = EDGE_CURVE('',#33498,#32650,#28059,.T.) ;
#41821 = EDGE_CURVE('',#32648,#33542,#28060,.T.) ;
#41822 = EDGE_CURVE('',#33496,#32650,#28061,.T.) ;
#41823 = EDGE_CURVE('',#32649,#33544,#28062,.T.) ;
#41824 = EDGE_CURVE('',#33583,#32680,#28063,.T.) ;
#41825 = EDGE_CURVE('',#32681,#33585,#28064,.T.) ;
#41826 = EDGE_CURVE('',#33581,#32680,#28065,.T.) ;
#41827 = EDGE_CURVE('',#32681,#33587,#28066,.T.) ;
#41828 = EDGE_CURVE('',#33579,#32679,#28067,.T.) ;
#41829 = EDGE_CURVE('',#32682,#33589,#28068,.T.) ;
#41830 = EDGE_CURVE('',#33577,#32678,#28069,.T.) ;
#41831 = EDGE_CURVE('',#32683,#33591,#28070,.T.) ;
#41832 = EDGE_CURVE('',#32684,#33593,#28071,.T.) ;
#41833 = EDGE_CURVE('',#32685,#33595,#28072,.T.) ;
#41834 = EDGE_CURVE('',#33575,#32677,#28073,.T.) ;
#41835 = EDGE_CURVE('',#32686,#33597,#28074,.T.) ;
#41836 = EDGE_CURVE('',#33574,#32676,#28075,.T.) ;
#41837 = EDGE_CURVE('',#32687,#33599,#28076,.T.) ;
#41838 = EDGE_CURVE('',#33573,#32675,#28077,.T.) ;
#41839 = EDGE_CURVE('',#32688,#33601,#28078,.T.) ;
#41840 = EDGE_CURVE('',#33571,#32674,#28079,.T.) ;
#41841 = EDGE_CURVE('',#32689,#33603,#28080,.T.) ;
#41842 = EDGE_CURVE('',#33569,#32673,#28081,.T.) ;
#41843 = EDGE_CURVE('',#32690,#33605,#28082,.T.) ;
#41844 = EDGE_CURVE('',#33567,#32673,#28083,.T.) ;
#41845 = EDGE_CURVE('',#32691,#33607,#28084,.T.) ;
#41846 = EDGE_CURVE('',#33565,#32672,#28085,.T.) ;
#41847 = EDGE_CURVE('',#32670,#33609,#28086,.T.) ;
#41848 = EDGE_CURVE('',#33563,#32672,#28087,.T.) ;
#41849 = EDGE_CURVE('',#32671,#33611,#28088,.T.) ;
#41850 = EDGE_CURVE('',#33650,#32702,#28089,.T.) ;
#41851 = EDGE_CURVE('',#32703,#33652,#28090,.T.) ;
#41852 = EDGE_CURVE('',#33648,#32702,#28091,.T.) ;
#41853 = EDGE_CURVE('',#32703,#33654,#28092,.T.) ;
#41854 = EDGE_CURVE('',#33646,#32701,#28093,.T.) ;
#41855 = EDGE_CURVE('',#32704,#33656,#28094,.T.) ;
#41856 = EDGE_CURVE('',#33644,#32700,#28095,.T.) ;
#41857 = EDGE_CURVE('',#32705,#33658,#28096,.T.) ;
#41858 = EDGE_CURVE('',#32706,#33660,#28097,.T.) ;
#41859 = EDGE_CURVE('',#32707,#33662,#28098,.T.) ;
#41860 = EDGE_CURVE('',#33642,#32699,#28099,.T.) ;
#41861 = EDGE_CURVE('',#32708,#33664,#28100,.T.) ;
#41862 = EDGE_CURVE('',#33641,#32698,#28101,.T.) ;
#41863 = EDGE_CURVE('',#32709,#33666,#28102,.T.) ;
#41864 = EDGE_CURVE('',#33640,#32697,#28103,.T.) ;
#41865 = EDGE_CURVE('',#32710,#33668,#28104,.T.) ;
#41866 = EDGE_CURVE('',#33638,#32696,#28105,.T.) ;
#41867 = EDGE_CURVE('',#32711,#33670,#28106,.T.) ;
#41868 = EDGE_CURVE('',#33636,#32695,#28107,.T.) ;
#41869 = EDGE_CURVE('',#32712,#33672,#28108,.T.) ;
#41870 = EDGE_CURVE('',#33634,#32695,#28109,.T.) ;
#41871 = EDGE_CURVE('',#32713,#33674,#28110,.T.) ;
#41872 = EDGE_CURVE('',#33632,#32694,#28111,.T.) ;
#41873 = EDGE_CURVE('',#32692,#33676,#28112,.T.) ;
#41874 = EDGE_CURVE('',#33630,#32694,#28113,.T.) ;
#41875 = EDGE_CURVE('',#32693,#33678,#28114,.T.) ;
#41876 = EDGE_CURVE('',#33717,#32724,#28115,.T.) ;
#41877 = EDGE_CURVE('',#32725,#33719,#28116,.T.) ;
#41878 = EDGE_CURVE('',#33715,#32724,#28117,.T.) ;
#41879 = EDGE_CURVE('',#32725,#33721,#28118,.T.) ;
#41880 = EDGE_CURVE('',#33713,#32723,#28119,.T.) ;
#41881 = EDGE_CURVE('',#32726,#33723,#28120,.T.) ;
#41882 = EDGE_CURVE('',#33711,#32722,#28121,.T.) ;
#41883 = EDGE_CURVE('',#32727,#33725,#28122,.T.) ;
#41884 = EDGE_CURVE('',#32728,#33727,#28123,.T.) ;
#41885 = EDGE_CURVE('',#32729,#33729,#28124,.T.) ;
#41886 = EDGE_CURVE('',#33709,#32721,#28125,.T.) ;
#41887 = EDGE_CURVE('',#32730,#33731,#28126,.T.) ;
#41888 = EDGE_CURVE('',#33708,#32720,#28127,.T.) ;
#41889 = EDGE_CURVE('',#32731,#33733,#28128,.T.) ;
#41890 = EDGE_CURVE('',#33707,#32719,#28129,.T.) ;
#41891 = EDGE_CURVE('',#32732,#33735,#28130,.T.) ;
#41892 = EDGE_CURVE('',#33705,#32718,#28131,.T.) ;
#41893 = EDGE_CURVE('',#32733,#33737,#28132,.T.) ;
#41894 = EDGE_CURVE('',#33703,#32717,#28133,.T.) ;
#41895 = EDGE_CURVE('',#32734,#33739,#28134,.T.) ;
#41896 = EDGE_CURVE('',#33701,#32717,#28135,.T.) ;
#41897 = EDGE_CURVE('',#32735,#33741,#28136,.T.) ;
#41898 = EDGE_CURVE('',#33699,#32716,#28137,.T.) ;
#41899 = EDGE_CURVE('',#32714,#33743,#28138,.T.) ;
#41900 = EDGE_CURVE('',#33697,#32716,#28139,.T.) ;
#41901 = EDGE_CURVE('',#32715,#33745,#28140,.T.) ;
#41902 = EDGE_CURVE('',#33784,#32746,#28141,.T.) ;
#41903 = EDGE_CURVE('',#32747,#33786,#28142,.T.) ;
#41904 = EDGE_CURVE('',#33782,#32746,#28143,.T.) ;
#41905 = EDGE_CURVE('',#32747,#33788,#28144,.T.) ;
#41906 = EDGE_CURVE('',#33780,#32745,#28145,.T.) ;
#41907 = EDGE_CURVE('',#32748,#33790,#28146,.T.) ;
#41908 = EDGE_CURVE('',#33778,#32744,#28147,.T.) ;
#41909 = EDGE_CURVE('',#32749,#33792,#28148,.T.) ;
#41910 = EDGE_CURVE('',#32750,#33794,#28149,.T.) ;
#41911 = EDGE_CURVE('',#32751,#33796,#28150,.T.) ;
#41912 = EDGE_CURVE('',#33776,#32743,#28151,.T.) ;
#41913 = EDGE_CURVE('',#32752,#33798,#28152,.T.) ;
#41914 = EDGE_CURVE('',#33775,#32742,#28153,.T.) ;
#41915 = EDGE_CURVE('',#32753,#33800,#28154,.T.) ;
#41916 = EDGE_CURVE('',#33774,#32741,#28155,.T.) ;
#41917 = EDGE_CURVE('',#32754,#33802,#28156,.T.) ;
#41918 = EDGE_CURVE('',#33772,#32740,#28157,.T.) ;
#41919 = EDGE_CURVE('',#32755,#33804,#28158,.T.) ;
#41920 = EDGE_CURVE('',#33770,#32739,#28159,.T.) ;
#41921 = EDGE_CURVE('',#32756,#33806,#28160,.T.) ;
#41922 = EDGE_CURVE('',#33768,#32739,#28161,.T.) ;
#41923 = EDGE_CURVE('',#32757,#33808,#28162,.T.) ;
#41924 = EDGE_CURVE('',#33766,#32738,#28163,.T.) ;
#41925 = EDGE_CURVE('',#32736,#33810,#28164,.T.) ;
#41926 = EDGE_CURVE('',#33764,#32738,#28165,.T.) ;
#41927 = EDGE_CURVE('',#32737,#33812,#28166,.T.) ;
#41928 = EDGE_CURVE('',#33095,#33054,#28167,.T.) ;
#41929 = EDGE_CURVE('',#33045,#33094,#28168,.T.) ;
#41930 = EDGE_CURVE('',#33096,#33089,#28169,.T.) ;
#41931 = EDGE_CURVE('',#33090,#33095,#28170,.T.) ;
#41932 = EDGE_CURVE('',#33096,#33910,#28171,.T.) ;
#41933 = EDGE_CURVE('',#33910,#33089,#28172,.T.) ;
#41934 = EDGE_CURVE('',#33045,#33099,#28173,.T.) ;
#41935 = EDGE_CURVE('',#33099,#33094,#28174,.T.) ;
#41936 = EDGE_CURVE('',#33090,#33053,#28175,.T.) ;
#41937 = EDGE_CURVE('',#32111,#33092,#28176,.T.) ;
#41938 = EDGE_CURVE('',#32112,#33911,#306,.T.) ;
#41939 = EDGE_CURVE('',#33910,#33911,#11310,.T.) ;
#41940 = EDGE_CURVE('',#33912,#33910,#307,.T.) ;
#41941 = EDGE_CURVE('',#33912,#33913,#308,.T.) ;
#41942 = EDGE_CURVE('',#32279,#33913,#11311,.T.) ;
#41943 = EDGE_CURVE('',#33093,#32278,#28177,.T.) ;
#41944 = EDGE_CURVE('',#33100,#33093,#28178,.T.) ;
#41945 = EDGE_CURVE('',#33046,#33098,#28179,.T.) ;
#41946 = EDGE_CURVE('',#33091,#33052,#28180,.T.) ;
#41947 = EDGE_CURVE('',#33092,#32113,#28181,.T.) ;
#41948 = EDGE_CURVE('',#33087,#33091,#28182,.T.) ;
#41949 = EDGE_CURVE('',#33100,#32287,#28183,.T.) ;
#41950 = EDGE_CURVE('',#33046,#32374,#28184,.T.) ;
#41951 = EDGE_CURVE('',#32373,#33098,#28185,.T.) ;
#41952 = EDGE_CURVE('',#33087,#33051,#28186,.T.) ;
#41953 = EDGE_CURVE('',#33097,#32286,#28187,.T.) ;
#41954 = EDGE_CURVE('',#32375,#33097,#28188,.T.) ;
#41955 = EDGE_CURVE('',#33914,#32374,#11312,.T.) ;
#41956 = EDGE_CURVE('',#33047,#33914,#28189,.T.) ;
#41957 = EDGE_CURVE('',#33088,#33050,#28190,.T.) ;
#41958 = EDGE_CURVE('',#32114,#33083,#28191,.T.) ;
#41959 = EDGE_CURVE('',#33084,#33088,#28192,.T.) ;
#41960 = EDGE_CURVE('',#32282,#33083,#28193,.T.) ;
#41961 = EDGE_CURVE('',#32375,#32286,#28194,.T.) ;
#41962 = EDGE_CURVE('',#32394,#32377,#28195,.T.) ;
#41963 = EDGE_CURVE('',#32377,#32392,#28196,.T.) ;
#41964 = EDGE_CURVE('',#33914,#32525,#28197,.T.) ;
#41965 = EDGE_CURVE('',#33915,#33914,#28198,.T.) ;
#41966 = EDGE_CURVE('',#33047,#33915,#28199,.T.) ;
#41967 = EDGE_CURVE('',#33084,#33050,#28200,.T.) ;
#41968 = EDGE_CURVE('',#32283,#33086,#28201,.T.) ;
#41969 = EDGE_CURVE('',#32376,#32285,#28202,.T.) ;
#41970 = EDGE_CURVE('',#32464,#32376,#28203,.T.) ;
#41971 = EDGE_CURVE('',#33915,#32524,#28204,.T.) ;
#41972 = EDGE_CURVE('',#33916,#33915,#11313,.T.) ;
#41973 = EDGE_CURVE('',#33048,#33916,#28205,.T.) ;
#41974 = EDGE_CURVE('',#33085,#33049,#28206,.T.) ;
#41975 = EDGE_CURVE('',#33086,#32372,#28207,.T.) ;
#41976 = EDGE_CURVE('',#32369,#33085,#28208,.T.) ;
#41977 = EDGE_CURVE('',#32283,#32372,#28209,.T.) ;
#41978 = EDGE_CURVE('',#32465,#32285,#28210,.T.) ;
#41979 = EDGE_CURVE('',#33916,#32523,#28211,.T.) ;
#41980 = EDGE_CURVE('',#33917,#33916,#28212,.T.) ;
#41981 = EDGE_CURVE('',#33048,#33917,#28213,.T.) ;
#41982 = EDGE_CURVE('',#32368,#33049,#28214,.T.) ;
#41983 = EDGE_CURVE('',#32284,#32371,#28215,.T.) ;
#41984 = EDGE_CURVE('',#32466,#32284,#28216,.T.) ;
#41985 = EDGE_CURVE('',#33917,#32522,#28217,.T.) ;
#41986 = EDGE_CURVE('',#32368,#33917,#11314,.T.) ;
#41987 = EDGE_CURVE('',#32467,#32371,#28218,.T.) ;
#41988 = EDGE_CURVE('',#32370,#32397,#28219,.T.) ;
#41989 = EDGE_CURVE('',#32399,#32370,#28220,.T.) ;
#41990 = EDGE_CURVE('',#33722,#33755,#28221,.T.) ;
#41991 = EDGE_CURVE('',#33756,#33720,#28222,.T.) ;
#41992 = EDGE_CURVE('',#33757,#33718,#28223,.T.) ;
#41993 = EDGE_CURVE('',#33724,#33755,#28224,.T.) ;
#41994 = EDGE_CURVE('',#33758,#33716,#28225,.T.) ;
#41995 = EDGE_CURVE('',#33726,#33754,#28226,.T.) ;
#41996 = EDGE_CURVE('',#33759,#33714,#28227,.T.) ;
#41997 = EDGE_CURVE('',#33728,#33754,#28228,.T.) ;
#41998 = EDGE_CURVE('',#33760,#33712,#28229,.T.) ;
#41999 = EDGE_CURVE('',#33730,#33753,#28230,.T.) ;
#42000 = EDGE_CURVE('',#33760,#33710,#28231,.T.) ;
#42001 = EDGE_CURVE('',#33732,#33753,#28232,.T.) ;
#42002 = EDGE_CURVE('',#33761,#32172,#28233,.T.) ;
#42003 = EDGE_CURVE('',#33734,#33752,#28234,.T.) ;
#42004 = EDGE_CURVE('',#33761,#32171,#28235,.T.) ;
#42005 = EDGE_CURVE('',#33736,#33752,#28236,.T.) ;
#42006 = EDGE_CURVE('',#33738,#33751,#28237,.T.) ;
#42007 = EDGE_CURVE('',#33740,#33751,#28238,.T.) ;
#42008 = EDGE_CURVE('',#33762,#33706,#28239,.T.) ;
#42009 = EDGE_CURVE('',#33742,#33750,#28240,.T.) ;
#42010 = EDGE_CURVE('',#33762,#33704,#28241,.T.) ;
#42011 = EDGE_CURVE('',#33744,#33750,#28242,.T.) ;
#42012 = EDGE_CURVE('',#33746,#33702,#28243,.T.) ;
#42013 = EDGE_CURVE('',#33696,#33749,#28244,.T.) ;
#42014 = EDGE_CURVE('',#33747,#33700,#28245,.T.) ;
#42015 = EDGE_CURVE('',#33698,#33748,#28246,.T.) ;
#42016 = EDGE_CURVE('',#33113,#33044,#28247,.T.) ;
#42017 = EDGE_CURVE('',#33035,#33112,#28248,.T.) ;
#42018 = EDGE_CURVE('',#33114,#33107,#28249,.T.) ;
#42019 = EDGE_CURVE('',#33108,#33113,#28250,.T.) ;
#42020 = EDGE_CURVE('',#33114,#33918,#28251,.T.) ;
#42021 = EDGE_CURVE('',#33918,#33107,#28252,.T.) ;
#42022 = EDGE_CURVE('',#33035,#33117,#28253,.T.) ;
#42023 = EDGE_CURVE('',#33117,#33112,#28254,.T.) ;
#42024 = EDGE_CURVE('',#33108,#33043,#28255,.T.) ;
#42025 = EDGE_CURVE('',#32096,#33110,#28256,.T.) ;
#42026 = EDGE_CURVE('',#32097,#33919,#309,.T.) ;
#42027 = EDGE_CURVE('',#33918,#33919,#11315,.T.) ;
#42028 = EDGE_CURVE('',#33920,#33918,#310,.T.) ;
#42029 = EDGE_CURVE('',#33920,#33921,#311,.T.) ;
#42030 = EDGE_CURVE('',#32269,#33921,#11316,.T.) ;
#42031 = EDGE_CURVE('',#33111,#32268,#28257,.T.) ;
#42032 = EDGE_CURVE('',#33118,#33111,#28258,.T.) ;
#42033 = EDGE_CURVE('',#33036,#33116,#28259,.T.) ;
#42034 = EDGE_CURVE('',#33109,#33042,#28260,.T.) ;
#42035 = EDGE_CURVE('',#33110,#32098,#28261,.T.) ;
#42036 = EDGE_CURVE('',#33105,#33109,#28262,.T.) ;
#42037 = EDGE_CURVE('',#33118,#32277,#28263,.T.) ;
#42038 = EDGE_CURVE('',#33036,#32364,#28264,.T.) ;
#42039 = EDGE_CURVE('',#32363,#33116,#28265,.T.) ;
#42040 = EDGE_CURVE('',#33105,#33041,#28266,.T.) ;
#42041 = EDGE_CURVE('',#33115,#32276,#28267,.T.) ;
#42042 = EDGE_CURVE('',#32365,#33115,#28268,.T.) ;
#42043 = EDGE_CURVE('',#33922,#32364,#11317,.T.) ;
#42044 = EDGE_CURVE('',#33037,#33922,#28269,.T.) ;
#42045 = EDGE_CURVE('',#33106,#33040,#28270,.T.) ;
#42046 = EDGE_CURVE('',#32099,#33101,#28271,.T.) ;
#42047 = EDGE_CURVE('',#33102,#33106,#28272,.T.) ;
#42048 = EDGE_CURVE('',#32272,#33101,#28273,.T.) ;
#42049 = EDGE_CURVE('',#32365,#32276,#28274,.T.) ;
#42050 = EDGE_CURVE('',#32398,#32367,#28275,.T.) ;
#42051 = EDGE_CURVE('',#32367,#32396,#28276,.T.) ;
#42052 = EDGE_CURVE('',#33922,#32521,#28277,.T.) ;
#42053 = EDGE_CURVE('',#33923,#33922,#28278,.T.) ;
#42054 = EDGE_CURVE('',#33037,#33923,#28279,.T.) ;
#42055 = EDGE_CURVE('',#33102,#33040,#28280,.T.) ;
#42056 = EDGE_CURVE('',#32273,#33104,#28281,.T.) ;
#42057 = EDGE_CURVE('',#32366,#32275,#28282,.T.) ;
#42058 = EDGE_CURVE('',#32468,#32366,#28283,.T.) ;
#42059 = EDGE_CURVE('',#33923,#32520,#28284,.T.) ;
#42060 = EDGE_CURVE('',#33924,#33923,#11318,.T.) ;
#42061 = EDGE_CURVE('',#33038,#33924,#28285,.T.) ;
#42062 = EDGE_CURVE('',#33103,#33039,#28286,.T.) ;
#42063 = EDGE_CURVE('',#33104,#32362,#28287,.T.) ;
#42064 = EDGE_CURVE('',#32359,#33103,#28288,.T.) ;
#42065 = EDGE_CURVE('',#32273,#32362,#28289,.T.) ;
#42066 = EDGE_CURVE('',#32469,#32275,#28290,.T.) ;
#42067 = EDGE_CURVE('',#33924,#32519,#28291,.T.) ;
#42068 = EDGE_CURVE('',#33925,#33924,#28292,.T.) ;
#42069 = EDGE_CURVE('',#33038,#33925,#28293,.T.) ;
#42070 = EDGE_CURVE('',#32358,#33039,#28294,.T.) ;
#42071 = EDGE_CURVE('',#32274,#32361,#28295,.T.) ;
#42072 = EDGE_CURVE('',#32470,#32274,#28296,.T.) ;
#42073 = EDGE_CURVE('',#33925,#32518,#28297,.T.) ;
#42074 = EDGE_CURVE('',#32358,#33925,#11319,.T.) ;
#42075 = EDGE_CURVE('',#32471,#32361,#28298,.T.) ;
#42076 = EDGE_CURVE('',#32360,#32401,#28299,.T.) ;
#42077 = EDGE_CURVE('',#32403,#32360,#28300,.T.) ;
#42078 = EDGE_CURVE('',#33655,#33688,#28301,.T.) ;
#42079 = EDGE_CURVE('',#33689,#33653,#28302,.T.) ;
#42080 = EDGE_CURVE('',#33690,#33651,#28303,.T.) ;
#42081 = EDGE_CURVE('',#33657,#33688,#28304,.T.) ;
#42082 = EDGE_CURVE('',#33691,#33649,#28305,.T.) ;
#42083 = EDGE_CURVE('',#33659,#33687,#28306,.T.) ;
#42084 = EDGE_CURVE('',#33692,#33647,#28307,.T.) ;
#42085 = EDGE_CURVE('',#33661,#33687,#28308,.T.) ;
#42086 = EDGE_CURVE('',#33693,#33645,#28309,.T.) ;
#42087 = EDGE_CURVE('',#33663,#33686,#28310,.T.) ;
#42088 = EDGE_CURVE('',#33693,#33643,#28311,.T.) ;
#42089 = EDGE_CURVE('',#33665,#33686,#28312,.T.) ;
#42090 = EDGE_CURVE('',#33694,#32174,#28313,.T.) ;
#42091 = EDGE_CURVE('',#33667,#33685,#28314,.T.) ;
#42092 = EDGE_CURVE('',#33694,#32173,#28315,.T.) ;
#42093 = EDGE_CURVE('',#33669,#33685,#28316,.T.) ;
#42094 = EDGE_CURVE('',#33671,#33684,#28317,.T.) ;
#42095 = EDGE_CURVE('',#33673,#33684,#28318,.T.) ;
#42096 = EDGE_CURVE('',#33695,#33639,#28319,.T.) ;
#42097 = EDGE_CURVE('',#33675,#33683,#28320,.T.) ;
#42098 = EDGE_CURVE('',#33695,#33637,#28321,.T.) ;
#42099 = EDGE_CURVE('',#33677,#33683,#28322,.T.) ;
#42100 = EDGE_CURVE('',#33679,#33635,#28323,.T.) ;
#42101 = EDGE_CURVE('',#33629,#33682,#28324,.T.) ;
#42102 = EDGE_CURVE('',#33680,#33633,#28325,.T.) ;
#42103 = EDGE_CURVE('',#33631,#33681,#28326,.T.) ;
#42104 = EDGE_CURVE('',#33131,#33034,#28327,.T.) ;
#42105 = EDGE_CURVE('',#33025,#33130,#28328,.T.) ;
#42106 = EDGE_CURVE('',#33132,#33125,#28329,.T.) ;
#42107 = EDGE_CURVE('',#33126,#33131,#28330,.T.) ;
#42108 = EDGE_CURVE('',#33132,#33926,#28331,.T.) ;
#42109 = EDGE_CURVE('',#33926,#33125,#28332,.T.) ;
#42110 = EDGE_CURVE('',#33025,#33135,#28333,.T.) ;
#42111 = EDGE_CURVE('',#33135,#33130,#28334,.T.) ;
#42112 = EDGE_CURVE('',#33126,#33033,#28335,.T.) ;
#42113 = EDGE_CURVE('',#32081,#33128,#28336,.T.) ;
#42114 = EDGE_CURVE('',#32082,#33927,#312,.T.) ;
#42115 = EDGE_CURVE('',#33926,#33927,#11320,.T.) ;
#42116 = EDGE_CURVE('',#33928,#33926,#313,.T.) ;
#42117 = EDGE_CURVE('',#33928,#33929,#314,.T.) ;
#42118 = EDGE_CURVE('',#32259,#33929,#11321,.T.) ;
#42119 = EDGE_CURVE('',#33129,#32258,#28337,.T.) ;
#42120 = EDGE_CURVE('',#33136,#33129,#28338,.T.) ;
#42121 = EDGE_CURVE('',#33026,#33134,#28339,.T.) ;
#42122 = EDGE_CURVE('',#33127,#33032,#28340,.T.) ;
#42123 = EDGE_CURVE('',#33128,#32083,#28341,.T.) ;
#42124 = EDGE_CURVE('',#33123,#33127,#28342,.T.) ;
#42125 = EDGE_CURVE('',#33136,#32267,#28343,.T.) ;
#42126 = EDGE_CURVE('',#33026,#32354,#28344,.T.) ;
#42127 = EDGE_CURVE('',#32353,#33134,#28345,.T.) ;
#42128 = EDGE_CURVE('',#33123,#33031,#28346,.T.) ;
#42129 = EDGE_CURVE('',#33133,#32266,#28347,.T.) ;
#42130 = EDGE_CURVE('',#32355,#33133,#28348,.T.) ;
#42131 = EDGE_CURVE('',#33930,#32354,#11322,.T.) ;
#42132 = EDGE_CURVE('',#33027,#33930,#28349,.T.) ;
#42133 = EDGE_CURVE('',#33124,#33030,#28350,.T.) ;
#42134 = EDGE_CURVE('',#32084,#33119,#28351,.T.) ;
#42135 = EDGE_CURVE('',#33120,#33124,#28352,.T.) ;
#42136 = EDGE_CURVE('',#32262,#33119,#28353,.T.) ;
#42137 = EDGE_CURVE('',#32355,#32266,#28354,.T.) ;
#42138 = EDGE_CURVE('',#32402,#32357,#28355,.T.) ;
#42139 = EDGE_CURVE('',#32357,#32400,#28356,.T.) ;
#42140 = EDGE_CURVE('',#33930,#32517,#28357,.T.) ;
#42141 = EDGE_CURVE('',#33931,#33930,#28358,.T.) ;
#42142 = EDGE_CURVE('',#33027,#33931,#28359,.T.) ;
#42143 = EDGE_CURVE('',#33120,#33030,#28360,.T.) ;
#42144 = EDGE_CURVE('',#32263,#33122,#28361,.T.) ;
#42145 = EDGE_CURVE('',#32356,#32265,#28362,.T.) ;
#42146 = EDGE_CURVE('',#32472,#32356,#28363,.T.) ;
#42147 = EDGE_CURVE('',#33931,#32516,#28364,.T.) ;
#42148 = EDGE_CURVE('',#33932,#33931,#11323,.T.) ;
#42149 = EDGE_CURVE('',#33028,#33932,#28365,.T.) ;
#42150 = EDGE_CURVE('',#33121,#33029,#28366,.T.) ;
#42151 = EDGE_CURVE('',#33122,#32352,#28367,.T.) ;
#42152 = EDGE_CURVE('',#32349,#33121,#28368,.T.) ;
#42153 = EDGE_CURVE('',#32263,#32352,#28369,.T.) ;
#42154 = EDGE_CURVE('',#32473,#32265,#28370,.T.) ;
#42155 = EDGE_CURVE('',#33932,#32515,#28371,.T.) ;
#42156 = EDGE_CURVE('',#33933,#33932,#28372,.T.) ;
#42157 = EDGE_CURVE('',#33028,#33933,#28373,.T.) ;
#42158 = EDGE_CURVE('',#32348,#33029,#28374,.T.) ;
#42159 = EDGE_CURVE('',#32264,#32351,#28375,.T.) ;
#42160 = EDGE_CURVE('',#32474,#32264,#28376,.T.) ;
#42161 = EDGE_CURVE('',#33933,#32514,#28377,.T.) ;
#42162 = EDGE_CURVE('',#32348,#33933,#11324,.T.) ;
#42163 = EDGE_CURVE('',#32475,#32351,#28378,.T.) ;
#42164 = EDGE_CURVE('',#32350,#32405,#28379,.T.) ;
#42165 = EDGE_CURVE('',#32407,#32350,#28380,.T.) ;
#42166 = EDGE_CURVE('',#33588,#33621,#28381,.T.) ;
#42167 = EDGE_CURVE('',#33622,#33586,#28382,.T.) ;
#42168 = EDGE_CURVE('',#33623,#33584,#28383,.T.) ;
#42169 = EDGE_CURVE('',#33590,#33621,#28384,.T.) ;
#42170 = EDGE_CURVE('',#33624,#33582,#28385,.T.) ;
#42171 = EDGE_CURVE('',#33592,#33620,#28386,.T.) ;
#42172 = EDGE_CURVE('',#33625,#33580,#28387,.T.) ;
#42173 = EDGE_CURVE('',#33594,#33620,#28388,.T.) ;
#42174 = EDGE_CURVE('',#33626,#33578,#28389,.T.) ;
#42175 = EDGE_CURVE('',#33596,#33619,#28390,.T.) ;
#42176 = EDGE_CURVE('',#33626,#33576,#28391,.T.) ;
#42177 = EDGE_CURVE('',#33598,#33619,#28392,.T.) ;
#42178 = EDGE_CURVE('',#33627,#32176,#28393,.T.) ;
#42179 = EDGE_CURVE('',#33600,#33618,#28394,.T.) ;
#42180 = EDGE_CURVE('',#33627,#32175,#28395,.T.) ;
#42181 = EDGE_CURVE('',#33602,#33618,#28396,.T.) ;
#42182 = EDGE_CURVE('',#33604,#33617,#28397,.T.) ;
#42183 = EDGE_CURVE('',#33606,#33617,#28398,.T.) ;
#42184 = EDGE_CURVE('',#33628,#33572,#28399,.T.) ;
#42185 = EDGE_CURVE('',#33608,#33616,#28400,.T.) ;
#42186 = EDGE_CURVE('',#33628,#33570,#28401,.T.) ;
#42187 = EDGE_CURVE('',#33610,#33616,#28402,.T.) ;
#42188 = EDGE_CURVE('',#33612,#33568,#28403,.T.) ;
#42189 = EDGE_CURVE('',#33562,#33615,#28404,.T.) ;
#42190 = EDGE_CURVE('',#33613,#33566,#28405,.T.) ;
#42191 = EDGE_CURVE('',#33564,#33614,#28406,.T.) ;
#42192 = EDGE_CURVE('',#33149,#33024,#28407,.T.) ;
#42193 = EDGE_CURVE('',#33015,#33148,#28408,.T.) ;
#42194 = EDGE_CURVE('',#33150,#33143,#28409,.T.) ;
#42195 = EDGE_CURVE('',#33144,#33149,#28410,.T.) ;
#42196 = EDGE_CURVE('',#33150,#33934,#28411,.T.) ;
#42197 = EDGE_CURVE('',#33934,#33143,#28412,.T.) ;
#42198 = EDGE_CURVE('',#33015,#33153,#28413,.T.) ;
#42199 = EDGE_CURVE('',#33153,#33148,#28414,.T.) ;
#42200 = EDGE_CURVE('',#33144,#33023,#28415,.T.) ;
#42201 = EDGE_CURVE('',#32066,#33146,#28416,.T.) ;
#42202 = EDGE_CURVE('',#32067,#33935,#315,.T.) ;
#42203 = EDGE_CURVE('',#33934,#33935,#11325,.T.) ;
#42204 = EDGE_CURVE('',#33936,#33934,#316,.T.) ;
#42205 = EDGE_CURVE('',#33936,#33937,#317,.T.) ;
#42206 = EDGE_CURVE('',#32249,#33937,#11326,.T.) ;
#42207 = EDGE_CURVE('',#33147,#32248,#28417,.T.) ;
#42208 = EDGE_CURVE('',#33154,#33147,#28418,.T.) ;
#42209 = EDGE_CURVE('',#33016,#33152,#28419,.T.) ;
#42210 = EDGE_CURVE('',#33145,#33022,#28420,.T.) ;
#42211 = EDGE_CURVE('',#33146,#32068,#28421,.T.) ;
#42212 = EDGE_CURVE('',#33141,#33145,#28422,.T.) ;
#42213 = EDGE_CURVE('',#33154,#32257,#28423,.T.) ;
#42214 = EDGE_CURVE('',#33016,#32344,#28424,.T.) ;
#42215 = EDGE_CURVE('',#32343,#33152,#28425,.T.) ;
#42216 = EDGE_CURVE('',#33141,#33021,#28426,.T.) ;
#42217 = EDGE_CURVE('',#33151,#32256,#28427,.T.) ;
#42218 = EDGE_CURVE('',#32345,#33151,#28428,.T.) ;
#42219 = EDGE_CURVE('',#33938,#32344,#11327,.T.) ;
#42220 = EDGE_CURVE('',#33017,#33938,#28429,.T.) ;
#42221 = EDGE_CURVE('',#33142,#33020,#28430,.T.) ;
#42222 = EDGE_CURVE('',#32069,#33137,#28431,.T.) ;
#42223 = EDGE_CURVE('',#33138,#33142,#28432,.T.) ;
#42224 = EDGE_CURVE('',#32252,#33137,#28433,.T.) ;
#42225 = EDGE_CURVE('',#32345,#32256,#28434,.T.) ;
#42226 = EDGE_CURVE('',#32406,#32347,#28435,.T.) ;
#42227 = EDGE_CURVE('',#32347,#32404,#28436,.T.) ;
#42228 = EDGE_CURVE('',#33938,#32513,#28437,.T.) ;
#42229 = EDGE_CURVE('',#33939,#33938,#28438,.T.) ;
#42230 = EDGE_CURVE('',#33017,#33939,#28439,.T.) ;
#42231 = EDGE_CURVE('',#33138,#33020,#28440,.T.) ;
#42232 = EDGE_CURVE('',#32253,#33140,#28441,.T.) ;
#42233 = EDGE_CURVE('',#32346,#32255,#28442,.T.) ;
#42234 = EDGE_CURVE('',#32476,#32346,#28443,.T.) ;
#42235 = EDGE_CURVE('',#33939,#32512,#28444,.T.) ;
#42236 = EDGE_CURVE('',#33940,#33939,#11328,.T.) ;
#42237 = EDGE_CURVE('',#33018,#33940,#28445,.T.) ;
#42238 = EDGE_CURVE('',#33139,#33019,#28446,.T.) ;
#42239 = EDGE_CURVE('',#33140,#32342,#28447,.T.) ;
#42240 = EDGE_CURVE('',#32339,#33139,#28448,.T.) ;
#42241 = EDGE_CURVE('',#32253,#32342,#28449,.T.) ;
#42242 = EDGE_CURVE('',#32477,#32255,#28450,.T.) ;
#42243 = EDGE_CURVE('',#33940,#32511,#28451,.T.) ;
#42244 = EDGE_CURVE('',#33941,#33940,#28452,.T.) ;
#42245 = EDGE_CURVE('',#33018,#33941,#28453,.T.) ;
#42246 = EDGE_CURVE('',#32338,#33019,#28454,.T.) ;
#42247 = EDGE_CURVE('',#32254,#32341,#28455,.T.) ;
#42248 = EDGE_CURVE('',#32478,#32254,#28456,.T.) ;
#42249 = EDGE_CURVE('',#33941,#32510,#28457,.T.) ;
#42250 = EDGE_CURVE('',#32338,#33941,#11329,.T.) ;
#42251 = EDGE_CURVE('',#32479,#32341,#28458,.T.) ;
#42252 = EDGE_CURVE('',#32340,#32409,#28459,.T.) ;
#42253 = EDGE_CURVE('',#32411,#32340,#28460,.T.) ;
#42254 = EDGE_CURVE('',#33521,#33554,#28461,.T.) ;
#42255 = EDGE_CURVE('',#33555,#33519,#28462,.T.) ;
#42256 = EDGE_CURVE('',#33556,#33517,#28463,.T.) ;
#42257 = EDGE_CURVE('',#33523,#33554,#28464,.T.) ;
#42258 = EDGE_CURVE('',#33557,#33515,#28465,.T.) ;
#42259 = EDGE_CURVE('',#33525,#33553,#28466,.T.) ;
#42260 = EDGE_CURVE('',#33558,#33513,#28467,.T.) ;
#42261 = EDGE_CURVE('',#33527,#33553,#28468,.T.) ;
#42262 = EDGE_CURVE('',#33559,#33511,#28469,.T.) ;
#42263 = EDGE_CURVE('',#33529,#33552,#28470,.T.) ;
#42264 = EDGE_CURVE('',#33559,#33509,#28471,.T.) ;
#42265 = EDGE_CURVE('',#33531,#33552,#28472,.T.) ;
#42266 = EDGE_CURVE('',#33560,#32178,#28473,.T.) ;
#42267 = EDGE_CURVE('',#33533,#33551,#28474,.T.) ;
#42268 = EDGE_CURVE('',#33560,#32177,#28475,.T.) ;
#42269 = EDGE_CURVE('',#33535,#33551,#28476,.T.) ;
#42270 = EDGE_CURVE('',#33537,#33550,#28477,.T.) ;
#42271 = EDGE_CURVE('',#33539,#33550,#28478,.T.) ;
#42272 = EDGE_CURVE('',#33561,#33505,#28479,.T.) ;
#42273 = EDGE_CURVE('',#33541,#33549,#28480,.T.) ;
#42274 = EDGE_CURVE('',#33561,#33503,#28481,.T.) ;
#42275 = EDGE_CURVE('',#33543,#33549,#28482,.T.) ;
#42276 = EDGE_CURVE('',#33545,#33501,#28483,.T.) ;
#42277 = EDGE_CURVE('',#33495,#33548,#28484,.T.) ;
#42278 = EDGE_CURVE('',#33546,#33499,#28485,.T.) ;
#42279 = EDGE_CURVE('',#33497,#33547,#28486,.T.) ;
#42280 = EDGE_CURVE('',#33167,#33014,#28487,.T.) ;
#42281 = EDGE_CURVE('',#33005,#33166,#28488,.T.) ;
#42282 = EDGE_CURVE('',#33168,#33161,#28489,.T.) ;
#42283 = EDGE_CURVE('',#33162,#33167,#28490,.T.) ;
#42284 = EDGE_CURVE('',#33168,#33942,#28491,.T.) ;
#42285 = EDGE_CURVE('',#33942,#33161,#28492,.T.) ;
#42286 = EDGE_CURVE('',#33005,#33171,#28493,.T.) ;
#42287 = EDGE_CURVE('',#33171,#33166,#28494,.T.) ;
#42288 = EDGE_CURVE('',#33162,#33013,#28495,.T.) ;
#42289 = EDGE_CURVE('',#32051,#33164,#28496,.T.) ;
#42290 = EDGE_CURVE('',#32052,#33943,#318,.T.) ;
#42291 = EDGE_CURVE('',#33942,#33943,#11330,.T.) ;
#42292 = EDGE_CURVE('',#33944,#33942,#319,.T.) ;
#42293 = EDGE_CURVE('',#33944,#33945,#320,.T.) ;
#42294 = EDGE_CURVE('',#32239,#33945,#11331,.T.) ;
#42295 = EDGE_CURVE('',#33165,#32238,#28497,.T.) ;
#42296 = EDGE_CURVE('',#33172,#33165,#28498,.T.) ;
#42297 = EDGE_CURVE('',#33006,#33170,#28499,.T.) ;
#42298 = EDGE_CURVE('',#33163,#33012,#28500,.T.) ;
#42299 = EDGE_CURVE('',#33164,#32053,#28501,.T.) ;
#42300 = EDGE_CURVE('',#33159,#33163,#28502,.T.) ;
#42301 = EDGE_CURVE('',#33172,#32247,#28503,.T.) ;
#42302 = EDGE_CURVE('',#33006,#32334,#28504,.T.) ;
#42303 = EDGE_CURVE('',#32333,#33170,#28505,.T.) ;
#42304 = EDGE_CURVE('',#33159,#33011,#28506,.T.) ;
#42305 = EDGE_CURVE('',#33169,#32246,#28507,.T.) ;
#42306 = EDGE_CURVE('',#32335,#33169,#28508,.T.) ;
#42307 = EDGE_CURVE('',#33946,#32334,#11332,.T.) ;
#42308 = EDGE_CURVE('',#33007,#33946,#28509,.T.) ;
#42309 = EDGE_CURVE('',#33160,#33010,#28510,.T.) ;
#42310 = EDGE_CURVE('',#32054,#33155,#28511,.T.) ;
#42311 = EDGE_CURVE('',#33156,#33160,#28512,.T.) ;
#42312 = EDGE_CURVE('',#32242,#33155,#28513,.T.) ;
#42313 = EDGE_CURVE('',#32335,#32246,#28514,.T.) ;
#42314 = EDGE_CURVE('',#32410,#32337,#28515,.T.) ;
#42315 = EDGE_CURVE('',#32337,#32408,#28516,.T.) ;
#42316 = EDGE_CURVE('',#33946,#32509,#28517,.T.) ;
#42317 = EDGE_CURVE('',#33947,#33946,#28518,.T.) ;
#42318 = EDGE_CURVE('',#33007,#33947,#28519,.T.) ;
#42319 = EDGE_CURVE('',#33156,#33010,#28520,.T.) ;
#42320 = EDGE_CURVE('',#32243,#33158,#28521,.T.) ;
#42321 = EDGE_CURVE('',#32336,#32245,#28522,.T.) ;
#42322 = EDGE_CURVE('',#32480,#32336,#28523,.T.) ;
#42323 = EDGE_CURVE('',#33947,#32508,#28524,.T.) ;
#42324 = EDGE_CURVE('',#33948,#33947,#11333,.T.) ;
#42325 = EDGE_CURVE('',#33008,#33948,#28525,.T.) ;
#42326 = EDGE_CURVE('',#33157,#33009,#28526,.T.) ;
#42327 = EDGE_CURVE('',#33158,#32332,#28527,.T.) ;
#42328 = EDGE_CURVE('',#32329,#33157,#28528,.T.) ;
#42329 = EDGE_CURVE('',#32243,#32332,#28529,.T.) ;
#42330 = EDGE_CURVE('',#32481,#32245,#28530,.T.) ;
#42331 = EDGE_CURVE('',#33948,#32507,#28531,.T.) ;
#42332 = EDGE_CURVE('',#33949,#33948,#28532,.T.) ;
#42333 = EDGE_CURVE('',#33008,#33949,#28533,.T.) ;
#42334 = EDGE_CURVE('',#32328,#33009,#28534,.T.) ;
#42335 = EDGE_CURVE('',#32244,#32331,#28535,.T.) ;
#42336 = EDGE_CURVE('',#32482,#32244,#28536,.T.) ;
#42337 = EDGE_CURVE('',#33949,#32506,#28537,.T.) ;
#42338 = EDGE_CURVE('',#32328,#33949,#11334,.T.) ;
#42339 = EDGE_CURVE('',#32483,#32331,#28538,.T.) ;
#42340 = EDGE_CURVE('',#32330,#32413,#28539,.T.) ;
#42341 = EDGE_CURVE('',#32415,#32330,#28540,.T.) ;
#42342 = EDGE_CURVE('',#33454,#33487,#28541,.T.) ;
#42343 = EDGE_CURVE('',#33488,#33452,#28542,.T.) ;
#42344 = EDGE_CURVE('',#33489,#33450,#28543,.T.) ;
#42345 = EDGE_CURVE('',#33456,#33487,#28544,.T.) ;
#42346 = EDGE_CURVE('',#33490,#33448,#28545,.T.) ;
#42347 = EDGE_CURVE('',#33458,#33486,#28546,.T.) ;
#42348 = EDGE_CURVE('',#33491,#33446,#28547,.T.) ;
#42349 = EDGE_CURVE('',#33460,#33486,#28548,.T.) ;
#42350 = EDGE_CURVE('',#33492,#33444,#28549,.T.) ;
#42351 = EDGE_CURVE('',#33462,#33485,#28550,.T.) ;
#42352 = EDGE_CURVE('',#33492,#33442,#28551,.T.) ;
#42353 = EDGE_CURVE('',#33464,#33485,#28552,.T.) ;
#42354 = EDGE_CURVE('',#33493,#32180,#28553,.T.) ;
#42355 = EDGE_CURVE('',#33466,#33484,#28554,.T.) ;
#42356 = EDGE_CURVE('',#33493,#32179,#28555,.T.) ;
#42357 = EDGE_CURVE('',#33468,#33484,#28556,.T.) ;
#42358 = EDGE_CURVE('',#33470,#33483,#28557,.T.) ;
#42359 = EDGE_CURVE('',#33472,#33483,#28558,.T.) ;
#42360 = EDGE_CURVE('',#33494,#33438,#28559,.T.) ;
#42361 = EDGE_CURVE('',#33474,#33482,#28560,.T.) ;
#42362 = EDGE_CURVE('',#33494,#33436,#28561,.T.) ;
#42363 = EDGE_CURVE('',#33476,#33482,#28562,.T.) ;
#42364 = EDGE_CURVE('',#33478,#33434,#28563,.T.) ;
#42365 = EDGE_CURVE('',#33428,#33481,#28564,.T.) ;
#42366 = EDGE_CURVE('',#33479,#33432,#28565,.T.) ;
#42367 = EDGE_CURVE('',#33430,#33480,#28566,.T.) ;
#42368 = EDGE_CURVE('',#33185,#33004,#28567,.T.) ;
#42369 = EDGE_CURVE('',#32995,#33184,#28568,.T.) ;
#42370 = EDGE_CURVE('',#33186,#33179,#28569,.T.) ;
#42371 = EDGE_CURVE('',#33180,#33185,#28570,.T.) ;
#42372 = EDGE_CURVE('',#33186,#33950,#28571,.T.) ;
#42373 = EDGE_CURVE('',#33950,#33179,#28572,.T.) ;
#42374 = EDGE_CURVE('',#32995,#33189,#28573,.T.) ;
#42375 = EDGE_CURVE('',#33189,#33184,#28574,.T.) ;
#42376 = EDGE_CURVE('',#33180,#33003,#28575,.T.) ;
#42377 = EDGE_CURVE('',#32036,#33182,#28576,.T.) ;
#42378 = EDGE_CURVE('',#32037,#33951,#321,.T.) ;
#42379 = EDGE_CURVE('',#33950,#33951,#11335,.T.) ;
#42380 = EDGE_CURVE('',#33952,#33950,#322,.T.) ;
#42381 = EDGE_CURVE('',#33952,#33953,#323,.T.) ;
#42382 = EDGE_CURVE('',#32229,#33953,#11336,.T.) ;
#42383 = EDGE_CURVE('',#33183,#32228,#28577,.T.) ;
#42384 = EDGE_CURVE('',#33190,#33183,#28578,.T.) ;
#42385 = EDGE_CURVE('',#32996,#33188,#28579,.T.) ;
#42386 = EDGE_CURVE('',#33181,#33002,#28580,.T.) ;
#42387 = EDGE_CURVE('',#33182,#32038,#28581,.T.) ;
#42388 = EDGE_CURVE('',#33177,#33181,#28582,.T.) ;
#42389 = EDGE_CURVE('',#33190,#32237,#28583,.T.) ;
#42390 = EDGE_CURVE('',#32996,#32324,#28584,.T.) ;
#42391 = EDGE_CURVE('',#32323,#33188,#28585,.T.) ;
#42392 = EDGE_CURVE('',#33177,#33001,#28586,.T.) ;
#42393 = EDGE_CURVE('',#33187,#32236,#28587,.T.) ;
#42394 = EDGE_CURVE('',#32325,#33187,#28588,.T.) ;
#42395 = EDGE_CURVE('',#33954,#32324,#11337,.T.) ;
#42396 = EDGE_CURVE('',#32997,#33954,#28589,.T.) ;
#42397 = EDGE_CURVE('',#33178,#33000,#28590,.T.) ;
#42398 = EDGE_CURVE('',#32039,#33173,#28591,.T.) ;
#42399 = EDGE_CURVE('',#33174,#33178,#28592,.T.) ;
#42400 = EDGE_CURVE('',#32232,#33173,#28593,.T.) ;
#42401 = EDGE_CURVE('',#32325,#32236,#28594,.T.) ;
#42402 = EDGE_CURVE('',#32414,#32327,#28595,.T.) ;
#42403 = EDGE_CURVE('',#32327,#32412,#28596,.T.) ;
#42404 = EDGE_CURVE('',#33954,#32505,#28597,.T.) ;
#42405 = EDGE_CURVE('',#33955,#33954,#28598,.T.) ;
#42406 = EDGE_CURVE('',#32997,#33955,#28599,.T.) ;
#42407 = EDGE_CURVE('',#33174,#33000,#28600,.T.) ;
#42408 = EDGE_CURVE('',#32233,#33176,#28601,.T.) ;
#42409 = EDGE_CURVE('',#32326,#32235,#28602,.T.) ;
#42410 = EDGE_CURVE('',#32484,#32326,#28603,.T.) ;
#42411 = EDGE_CURVE('',#33955,#32504,#28604,.T.) ;
#42412 = EDGE_CURVE('',#33956,#33955,#11338,.T.) ;
#42413 = EDGE_CURVE('',#32998,#33956,#28605,.T.) ;
#42414 = EDGE_CURVE('',#33175,#32999,#28606,.T.) ;
#42415 = EDGE_CURVE('',#33176,#32322,#28607,.T.) ;
#42416 = EDGE_CURVE('',#32319,#33175,#28608,.T.) ;
#42417 = EDGE_CURVE('',#32233,#32322,#28609,.T.) ;
#42418 = EDGE_CURVE('',#32485,#32235,#28610,.T.) ;
#42419 = EDGE_CURVE('',#33956,#32503,#28611,.T.) ;
#42420 = EDGE_CURVE('',#33957,#33956,#28612,.T.) ;
#42421 = EDGE_CURVE('',#32998,#33957,#28613,.T.) ;
#42422 = EDGE_CURVE('',#32318,#32999,#28614,.T.) ;
#42423 = EDGE_CURVE('',#32234,#32321,#28615,.T.) ;
#42424 = EDGE_CURVE('',#32486,#32234,#28616,.T.) ;
#42425 = EDGE_CURVE('',#33957,#32502,#28617,.T.) ;
#42426 = EDGE_CURVE('',#32318,#33957,#11339,.T.) ;
#42427 = EDGE_CURVE('',#32487,#32321,#28618,.T.) ;
#42428 = EDGE_CURVE('',#32320,#32417,#28619,.T.) ;
#42429 = EDGE_CURVE('',#32419,#32320,#28620,.T.) ;
#42430 = EDGE_CURVE('',#33387,#33420,#28621,.T.) ;
#42431 = EDGE_CURVE('',#33421,#33385,#28622,.T.) ;
#42432 = EDGE_CURVE('',#33422,#33383,#28623,.T.) ;
#42433 = EDGE_CURVE('',#33389,#33420,#28624,.T.) ;
#42434 = EDGE_CURVE('',#33423,#33381,#28625,.T.) ;
#42435 = EDGE_CURVE('',#33391,#33419,#28626,.T.) ;
#42436 = EDGE_CURVE('',#33424,#33379,#28627,.T.) ;
#42437 = EDGE_CURVE('',#33393,#33419,#28628,.T.) ;
#42438 = EDGE_CURVE('',#33425,#33377,#28629,.T.) ;
#42439 = EDGE_CURVE('',#33395,#33418,#28630,.T.) ;
#42440 = EDGE_CURVE('',#33425,#33375,#28631,.T.) ;
#42441 = EDGE_CURVE('',#33397,#33418,#28632,.T.) ;
#42442 = EDGE_CURVE('',#33426,#32182,#28633,.T.) ;
#42443 = EDGE_CURVE('',#33399,#33417,#28634,.T.) ;
#42444 = EDGE_CURVE('',#33426,#32181,#28635,.T.) ;
#42445 = EDGE_CURVE('',#33401,#33417,#28636,.T.) ;
#42446 = EDGE_CURVE('',#33403,#33416,#28637,.T.) ;
#42447 = EDGE_CURVE('',#33405,#33416,#28638,.T.) ;
#42448 = EDGE_CURVE('',#33427,#33371,#28639,.T.) ;
#42449 = EDGE_CURVE('',#33407,#33415,#28640,.T.) ;
#42450 = EDGE_CURVE('',#33427,#33369,#28641,.T.) ;
#42451 = EDGE_CURVE('',#33409,#33415,#28642,.T.) ;
#42452 = EDGE_CURVE('',#33411,#33367,#28643,.T.) ;
#42453 = EDGE_CURVE('',#33361,#33414,#28644,.T.) ;
#42454 = EDGE_CURVE('',#33412,#33365,#28645,.T.) ;
#42455 = EDGE_CURVE('',#33363,#33413,#28646,.T.) ;
#42456 = EDGE_CURVE('',#33203,#32994,#28647,.T.) ;
#42457 = EDGE_CURVE('',#32985,#33202,#28648,.T.) ;
#42458 = EDGE_CURVE('',#33204,#33197,#28649,.T.) ;
#42459 = EDGE_CURVE('',#33198,#33203,#28650,.T.) ;
#42460 = EDGE_CURVE('',#33204,#33958,#28651,.T.) ;
#42461 = EDGE_CURVE('',#33958,#33197,#28652,.T.) ;
#42462 = EDGE_CURVE('',#32985,#33207,#28653,.T.) ;
#42463 = EDGE_CURVE('',#33207,#33202,#28654,.T.) ;
#42464 = EDGE_CURVE('',#33198,#32993,#28655,.T.) ;
#42465 = EDGE_CURVE('',#32021,#33200,#28656,.T.) ;
#42466 = EDGE_CURVE('',#32022,#33959,#324,.T.) ;
#42467 = EDGE_CURVE('',#33958,#33959,#11340,.T.) ;
#42468 = EDGE_CURVE('',#33960,#33958,#325,.T.) ;
#42469 = EDGE_CURVE('',#33960,#33961,#326,.T.) ;
#42470 = EDGE_CURVE('',#32219,#33961,#11341,.T.) ;
#42471 = EDGE_CURVE('',#33201,#32218,#28657,.T.) ;
#42472 = EDGE_CURVE('',#33208,#33201,#28658,.T.) ;
#42473 = EDGE_CURVE('',#32986,#33206,#28659,.T.) ;
#42474 = EDGE_CURVE('',#33199,#32992,#28660,.T.) ;
#42475 = EDGE_CURVE('',#33200,#32023,#28661,.T.) ;
#42476 = EDGE_CURVE('',#33195,#33199,#28662,.T.) ;
#42477 = EDGE_CURVE('',#33208,#32227,#28663,.T.) ;
#42478 = EDGE_CURVE('',#32986,#32314,#28664,.T.) ;
#42479 = EDGE_CURVE('',#32313,#33206,#28665,.T.) ;
#42480 = EDGE_CURVE('',#33195,#32991,#28666,.T.) ;
#42481 = EDGE_CURVE('',#33205,#32226,#28667,.T.) ;
#42482 = EDGE_CURVE('',#32315,#33205,#28668,.T.) ;
#42483 = EDGE_CURVE('',#33962,#32314,#11342,.T.) ;
#42484 = EDGE_CURVE('',#32987,#33962,#28669,.T.) ;
#42485 = EDGE_CURVE('',#33196,#32990,#28670,.T.) ;
#42486 = EDGE_CURVE('',#32024,#33191,#28671,.T.) ;
#42487 = EDGE_CURVE('',#33192,#33196,#28672,.T.) ;
#42488 = EDGE_CURVE('',#32222,#33191,#28673,.T.) ;
#42489 = EDGE_CURVE('',#32315,#32226,#28674,.T.) ;
#42490 = EDGE_CURVE('',#32418,#32317,#28675,.T.) ;
#42491 = EDGE_CURVE('',#32317,#32416,#28676,.T.) ;
#42492 = EDGE_CURVE('',#33962,#32501,#28677,.T.) ;
#42493 = EDGE_CURVE('',#33963,#33962,#28678,.T.) ;
#42494 = EDGE_CURVE('',#32987,#33963,#28679,.T.) ;
#42495 = EDGE_CURVE('',#33192,#32990,#28680,.T.) ;
#42496 = EDGE_CURVE('',#32223,#33194,#28681,.T.) ;
#42497 = EDGE_CURVE('',#32316,#32225,#28682,.T.) ;
#42498 = EDGE_CURVE('',#32488,#32316,#28683,.T.) ;
#42499 = EDGE_CURVE('',#33963,#32500,#28684,.T.) ;
#42500 = EDGE_CURVE('',#33964,#33963,#11343,.T.) ;
#42501 = EDGE_CURVE('',#32988,#33964,#28685,.T.) ;
#42502 = EDGE_CURVE('',#33193,#32989,#28686,.T.) ;
#42503 = EDGE_CURVE('',#33194,#32312,#28687,.T.) ;
#42504 = EDGE_CURVE('',#32309,#33193,#28688,.T.) ;
#42505 = EDGE_CURVE('',#32223,#32312,#28689,.T.) ;
#42506 = EDGE_CURVE('',#32489,#32225,#28690,.T.) ;
#42507 = EDGE_CURVE('',#33964,#32499,#28691,.T.) ;
#42508 = EDGE_CURVE('',#33965,#33964,#28692,.T.) ;
#42509 = EDGE_CURVE('',#32988,#33965,#28693,.T.) ;
#42510 = EDGE_CURVE('',#32308,#32989,#28694,.T.) ;
#42511 = EDGE_CURVE('',#32224,#32311,#28695,.T.) ;
#42512 = EDGE_CURVE('',#32490,#32224,#28696,.T.) ;
#42513 = EDGE_CURVE('',#33965,#32498,#28697,.T.) ;
#42514 = EDGE_CURVE('',#32308,#33965,#11344,.T.) ;
#42515 = EDGE_CURVE('',#32491,#32311,#28698,.T.) ;
#42516 = EDGE_CURVE('',#32310,#32421,#28699,.T.) ;
#42517 = EDGE_CURVE('',#32423,#32310,#28700,.T.) ;
#42518 = EDGE_CURVE('',#33320,#33353,#28701,.T.) ;
#42519 = EDGE_CURVE('',#33354,#33318,#28702,.T.) ;
#42520 = EDGE_CURVE('',#33355,#33316,#28703,.T.) ;
#42521 = EDGE_CURVE('',#33322,#33353,#28704,.T.) ;
#42522 = EDGE_CURVE('',#33356,#33314,#28705,.T.) ;
#42523 = EDGE_CURVE('',#33324,#33352,#28706,.T.) ;
#42524 = EDGE_CURVE('',#33357,#33312,#28707,.T.) ;
#42525 = EDGE_CURVE('',#33326,#33352,#28708,.T.) ;
#42526 = EDGE_CURVE('',#33358,#33310,#28709,.T.) ;
#42527 = EDGE_CURVE('',#33328,#33351,#28710,.T.) ;
#42528 = EDGE_CURVE('',#33358,#33308,#28711,.T.) ;
#42529 = EDGE_CURVE('',#33330,#33351,#28712,.T.) ;
#42530 = EDGE_CURVE('',#33359,#32184,#28713,.T.) ;
#42531 = EDGE_CURVE('',#33332,#33350,#28714,.T.) ;
#42532 = EDGE_CURVE('',#33359,#32183,#28715,.T.) ;
#42533 = EDGE_CURVE('',#33334,#33350,#28716,.T.) ;
#42534 = EDGE_CURVE('',#33336,#33349,#28717,.T.) ;
#42535 = EDGE_CURVE('',#33338,#33349,#28718,.T.) ;
#42536 = EDGE_CURVE('',#33360,#33304,#28719,.T.) ;
#42537 = EDGE_CURVE('',#33340,#33348,#28720,.T.) ;
#42538 = EDGE_CURVE('',#33360,#33302,#28721,.T.) ;
#42539 = EDGE_CURVE('',#33342,#33348,#28722,.T.) ;
#42540 = EDGE_CURVE('',#33344,#33300,#28723,.T.) ;
#42541 = EDGE_CURVE('',#33294,#33347,#28724,.T.) ;
#42542 = EDGE_CURVE('',#33345,#33298,#28725,.T.) ;
#42543 = EDGE_CURVE('',#33296,#33346,#28726,.T.) ;
#42544 = EDGE_CURVE('',#33221,#32984,#28727,.T.) ;
#42545 = EDGE_CURVE('',#32975,#33220,#28728,.T.) ;
#42546 = EDGE_CURVE('',#33222,#33215,#28729,.T.) ;
#42547 = EDGE_CURVE('',#33216,#33221,#28730,.T.) ;
#42548 = EDGE_CURVE('',#33222,#33966,#28731,.T.) ;
#42549 = EDGE_CURVE('',#33966,#33215,#28732,.T.) ;
#42550 = EDGE_CURVE('',#32975,#33225,#28733,.T.) ;
#42551 = EDGE_CURVE('',#33225,#33220,#28734,.T.) ;
#42552 = EDGE_CURVE('',#33216,#32983,#28735,.T.) ;
#42553 = EDGE_CURVE('',#32006,#33218,#28736,.T.) ;
#42554 = EDGE_CURVE('',#32007,#33967,#327,.T.) ;
#42555 = EDGE_CURVE('',#33966,#33967,#11345,.T.) ;
#42556 = EDGE_CURVE('',#33968,#33966,#328,.T.) ;
#42557 = EDGE_CURVE('',#33968,#33969,#329,.T.) ;
#42558 = EDGE_CURVE('',#32209,#33969,#11346,.T.) ;
#42559 = EDGE_CURVE('',#33219,#32208,#28737,.T.) ;
#42560 = EDGE_CURVE('',#33226,#33219,#28738,.T.) ;
#42561 = EDGE_CURVE('',#32976,#33224,#28739,.T.) ;
#42562 = EDGE_CURVE('',#33217,#32982,#28740,.T.) ;
#42563 = EDGE_CURVE('',#33218,#32008,#28741,.T.) ;
#42564 = EDGE_CURVE('',#33213,#33217,#28742,.T.) ;
#42565 = EDGE_CURVE('',#33226,#32217,#28743,.T.) ;
#42566 = EDGE_CURVE('',#32976,#32304,#28744,.T.) ;
#42567 = EDGE_CURVE('',#32303,#33224,#28745,.T.) ;
#42568 = EDGE_CURVE('',#33213,#32981,#28746,.T.) ;
#42569 = EDGE_CURVE('',#33223,#32216,#28747,.T.) ;
#42570 = EDGE_CURVE('',#32305,#33223,#28748,.T.) ;
#42571 = EDGE_CURVE('',#33970,#32304,#11347,.T.) ;
#42572 = EDGE_CURVE('',#32977,#33970,#28749,.T.) ;
#42573 = EDGE_CURVE('',#33214,#32980,#28750,.T.) ;
#42574 = EDGE_CURVE('',#32009,#33209,#28751,.T.) ;
#42575 = EDGE_CURVE('',#33210,#33214,#28752,.T.) ;
#42576 = EDGE_CURVE('',#32212,#33209,#28753,.T.) ;
#42577 = EDGE_CURVE('',#32305,#32216,#28754,.T.) ;
#42578 = EDGE_CURVE('',#32422,#32307,#28755,.T.) ;
#42579 = EDGE_CURVE('',#32307,#32420,#28756,.T.) ;
#42580 = EDGE_CURVE('',#33970,#32496,#28757,.T.) ;
#42581 = EDGE_CURVE('',#33971,#33970,#28758,.T.) ;
#42582 = EDGE_CURVE('',#32977,#33971,#28759,.T.) ;
#42583 = EDGE_CURVE('',#33210,#32980,#28760,.T.) ;
#42584 = EDGE_CURVE('',#32213,#33212,#28761,.T.) ;
#42585 = EDGE_CURVE('',#32306,#32215,#28762,.T.) ;
#42586 = EDGE_CURVE('',#32492,#32306,#28763,.T.) ;
#42587 = EDGE_CURVE('',#33971,#32497,#28764,.T.) ;
#42588 = EDGE_CURVE('',#33972,#33971,#11348,.T.) ;
#42589 = EDGE_CURVE('',#32978,#33972,#28765,.T.) ;
#42590 = EDGE_CURVE('',#33211,#32979,#28766,.T.) ;
#42591 = EDGE_CURVE('',#33212,#32302,#28767,.T.) ;
#42592 = EDGE_CURVE('',#32299,#33211,#28768,.T.) ;
#42593 = EDGE_CURVE('',#32213,#32302,#28769,.T.) ;
#42594 = EDGE_CURVE('',#32493,#32215,#28770,.T.) ;
#42595 = EDGE_CURVE('',#33972,#32537,#28771,.T.) ;
#42596 = EDGE_CURVE('',#33973,#33972,#28772,.T.) ;
#42597 = EDGE_CURVE('',#32978,#33973,#28773,.T.) ;
#42598 = EDGE_CURVE('',#32298,#32979,#28774,.T.) ;
#42599 = EDGE_CURVE('',#32214,#32301,#28775,.T.) ;
#42600 = EDGE_CURVE('',#32453,#32214,#28776,.T.) ;
#42601 = EDGE_CURVE('',#33973,#32536,#28777,.T.) ;
#42602 = EDGE_CURVE('',#32298,#33973,#11349,.T.) ;
#42603 = EDGE_CURVE('',#32452,#32301,#28778,.T.) ;
#42604 = EDGE_CURVE('',#32300,#32494,#28779,.T.) ;
#42605 = EDGE_CURVE('',#32454,#32300,#28780,.T.) ;
#42606 = EDGE_CURVE('',#33253,#33286,#28781,.T.) ;
#42607 = EDGE_CURVE('',#33287,#33251,#28782,.T.) ;
#42608 = EDGE_CURVE('',#33288,#33249,#28783,.T.) ;
#42609 = EDGE_CURVE('',#33255,#33286,#28784,.T.) ;
#42610 = EDGE_CURVE('',#33289,#33247,#28785,.T.) ;
#42611 = EDGE_CURVE('',#33257,#33285,#28786,.T.) ;
#42612 = EDGE_CURVE('',#33290,#33245,#28787,.T.) ;
#42613 = EDGE_CURVE('',#33259,#33285,#28788,.T.) ;
#42614 = EDGE_CURVE('',#33291,#33243,#28789,.T.) ;
#42615 = EDGE_CURVE('',#33261,#33284,#28790,.T.) ;
#42616 = EDGE_CURVE('',#33291,#33241,#28791,.T.) ;
#42617 = EDGE_CURVE('',#33263,#33284,#28792,.T.) ;
#42618 = EDGE_CURVE('',#33292,#32186,#28793,.T.) ;
#42619 = EDGE_CURVE('',#33265,#33283,#28794,.T.) ;
#42620 = EDGE_CURVE('',#33292,#32185,#28795,.T.) ;
#42621 = EDGE_CURVE('',#33267,#33283,#28796,.T.) ;
#42622 = EDGE_CURVE('',#33269,#33282,#28797,.T.) ;
#42623 = EDGE_CURVE('',#33271,#33282,#28798,.T.) ;
#42624 = EDGE_CURVE('',#33293,#33237,#28799,.T.) ;
#42625 = EDGE_CURVE('',#33273,#33281,#28800,.T.) ;
#42626 = EDGE_CURVE('',#33293,#33235,#28801,.T.) ;
#42627 = EDGE_CURVE('',#33275,#33281,#28802,.T.) ;
#42628 = EDGE_CURVE('',#33277,#33233,#28803,.T.) ;
#42629 = EDGE_CURVE('',#33227,#33280,#28804,.T.) ;
#42630 = EDGE_CURVE('',#33278,#33231,#28805,.T.) ;
#42631 = EDGE_CURVE('',#33229,#33279,#28806,.T.) ;
#42632 = EDGE_CURVE('',#33974,#33975,#11350,.T.) ;
#42633 = EDGE_CURVE('',#33975,#33976,#11351,.T.) ;
#42634 = EDGE_CURVE('',#33976,#33977,#11352,.T.) ;
#42635 = EDGE_CURVE('',#33977,#33974,#11353,.T.) ;
#42636 = EDGE_CURVE('',#33978,#33979,#11354,.T.) ;
#42637 = EDGE_CURVE('',#33979,#33980,#11355,.T.) ;
#42638 = EDGE_CURVE('',#33980,#33981,#11356,.T.) ;
#42639 = EDGE_CURVE('',#33981,#33978,#11357,.T.) ;
#42640 = EDGE_CURVE('',#33982,#33983,#11358,.T.) ;
#42641 = EDGE_CURVE('',#33983,#33984,#11359,.T.) ;
#42642 = EDGE_CURVE('',#33984,#33985,#11360,.T.) ;
#42643 = EDGE_CURVE('',#33985,#33982,#11361,.T.) ;
#42644 = EDGE_CURVE('',#33986,#33987,#11362,.T.) ;
#42645 = EDGE_CURVE('',#33987,#33988,#11363,.T.) ;
#42646 = EDGE_CURVE('',#33988,#33989,#11364,.T.) ;
#42647 = EDGE_CURVE('',#33989,#33986,#11365,.T.) ;
#42648 = EDGE_CURVE('',#33990,#33991,#11366,.T.) ;
#42649 = EDGE_CURVE('',#33991,#33992,#11367,.T.) ;
#42650 = EDGE_CURVE('',#33993,#33992,#11368,.T.) ;
#42651 = EDGE_CURVE('',#33993,#33990,#11369,.T.) ;
#42652 = EDGE_CURVE('',#33994,#33995,#11370,.T.) ;
#42653 = EDGE_CURVE('',#33995,#32289,#28807,.T.) ;
#42654 = EDGE_CURVE('',#33905,#33996,#28808,.T.) ;
#42655 = EDGE_CURVE('',#33996,#33997,#11371,.T.) ;
#42656 = EDGE_CURVE('',#33997,#33994,#11372,.T.) ;
#42657 = EDGE_CURVE('',#33998,#33999,#11373,.T.) ;
#42658 = EDGE_CURVE('',#33999,#32168,#28809,.T.) ;
#42659 = EDGE_CURVE('',#32167,#34000,#28810,.T.) ;
#42660 = EDGE_CURVE('',#34000,#34001,#11374,.T.) ;
#42661 = EDGE_CURVE('',#34001,#33998,#11375,.T.) ;
#42662 = EDGE_CURVE('',#33903,#33975,#28811,.T.) ;
#42663 = EDGE_CURVE('',#33974,#33904,#28812,.T.) ;
#42664 = EDGE_CURVE('',#33992,#32291,#28813,.T.) ;
#42665 = EDGE_CURVE('',#32290,#33993,#28814,.T.) ;
#42666 = EDGE_CURVE('',#34002,#34003,#11376,.T.) ;
#42667 = EDGE_CURVE('',#34003,#34004,#11377,.T.) ;
#42668 = EDGE_CURVE('',#34004,#34005,#11378,.T.) ;
#42669 = EDGE_CURVE('',#34005,#34002,#11379,.T.) ;
#42670 = EDGE_CURVE('',#34006,#34007,#11380,.T.) ;
#42671 = EDGE_CURVE('',#34007,#33833,#11381,.T.) ;
#42672 = EDGE_CURVE('',#33832,#34006,#11382,.T.) ;
#42673 = EDGE_CURVE('',#33836,#34008,#11383,.T.) ;
#42674 = EDGE_CURVE('',#34008,#34009,#11384,.T.) ;
#42675 = EDGE_CURVE('',#34009,#33837,#11385,.T.) ;
#42676 = EDGE_CURVE('',#34010,#34011,#11386,.T.) ;
#42677 = EDGE_CURVE('',#34011,#34012,#11387,.T.) ;
#42678 = EDGE_CURVE('',#34012,#34013,#11388,.T.) ;
#42679 = EDGE_CURVE('',#34013,#34010,#11389,.T.) ;
#42680 = EDGE_CURVE('',#34014,#34015,#11390,.T.) ;
#42681 = EDGE_CURVE('',#34015,#34016,#11391,.T.) ;
#42682 = EDGE_CURVE('',#34016,#34017,#11392,.T.) ;
#42683 = EDGE_CURVE('',#34017,#34014,#11393,.T.) ;
#42684 = EDGE_CURVE('',#34018,#34019,#11394,.T.) ;
#42685 = EDGE_CURVE('',#34019,#33830,#11395,.T.) ;
#42686 = EDGE_CURVE('',#33831,#34018,#11396,.T.) ;
#42687 = EDGE_CURVE('',#33834,#34020,#11397,.T.) ;
#42688 = EDGE_CURVE('',#34020,#34021,#11398,.T.) ;
#42689 = EDGE_CURVE('',#34021,#33835,#11399,.T.) ;
#42690 = EDGE_CURVE('',#34022,#34023,#11400,.T.) ;
#42691 = EDGE_CURVE('',#34023,#34024,#11401,.T.) ;
#42692 = EDGE_CURVE('',#34024,#34025,#11402,.T.) ;
#42693 = EDGE_CURVE('',#34025,#34022,#11403,.T.) ;
#42694 = EDGE_CURVE('',#34026,#34027,#11404,.T.) ;
#42695 = EDGE_CURVE('',#34027,#34028,#11405,.T.) ;
#42696 = EDGE_CURVE('',#34028,#34029,#11406,.T.) ;
#42697 = EDGE_CURVE('',#34029,#34026,#11407,.T.) ;
#42698 = EDGE_CURVE('',#34030,#34031,#11408,.T.) ;
#42699 = EDGE_CURVE('',#34031,#34032,#11409,.T.) ;
#42700 = EDGE_CURVE('',#34032,#34033,#11410,.T.) ;
#42701 = EDGE_CURVE('',#34033,#34030,#11411,.T.) ;
#42702 = EDGE_CURVE('',#34034,#34035,#11412,.T.) ;
#42703 = EDGE_CURVE('',#34035,#34036,#11413,.T.) ;
#42704 = EDGE_CURVE('',#34036,#34037,#11414,.T.) ;
#42705 = EDGE_CURVE('',#34037,#34034,#11415,.T.) ;
#42706 = EDGE_CURVE('',#34038,#34039,#11416,.T.) ;
#42707 = EDGE_CURVE('',#34039,#34040,#11417,.T.) ;
#42708 = EDGE_CURVE('',#34041,#34040,#11418,.T.) ;
#42709 = EDGE_CURVE('',#34041,#34038,#11419,.T.) ;
#42710 = EDGE_CURVE('',#34042,#34043,#11420,.T.) ;
#42711 = EDGE_CURVE('',#34043,#32279,#28815,.T.) ;
#42712 = EDGE_CURVE('',#33913,#34044,#28816,.T.) ;
#42713 = EDGE_CURVE('',#34044,#34045,#11421,.T.) ;
#42714 = EDGE_CURVE('',#34045,#34042,#11422,.T.) ;
#42715 = EDGE_CURVE('',#34046,#34047,#11423,.T.) ;
#42716 = EDGE_CURVE('',#34047,#32117,#28817,.T.) ;
#42717 = EDGE_CURVE('',#32116,#34048,#28818,.T.) ;
#42718 = EDGE_CURVE('',#34048,#34049,#11424,.T.) ;
#42719 = EDGE_CURVE('',#34049,#34046,#11425,.T.) ;
#42720 = EDGE_CURVE('',#33911,#34023,#28819,.T.) ;
#42721 = EDGE_CURVE('',#34022,#33912,#28820,.T.) ;
#42722 = EDGE_CURVE('',#34040,#32281,#28821,.T.) ;
#42723 = EDGE_CURVE('',#32280,#34041,#28822,.T.) ;
#42724 = EDGE_CURVE('',#34050,#34051,#11426,.T.) ;
#42725 = EDGE_CURVE('',#34051,#34052,#11427,.T.) ;
#42726 = EDGE_CURVE('',#34052,#34053,#11428,.T.) ;
#42727 = EDGE_CURVE('',#34053,#34050,#11429,.T.) ;
#42728 = EDGE_CURVE('',#34054,#34055,#11430,.T.) ;
#42729 = EDGE_CURVE('',#34055,#33841,#11431,.T.) ;
#42730 = EDGE_CURVE('',#33840,#34054,#11432,.T.) ;
#42731 = EDGE_CURVE('',#33844,#34056,#11433,.T.) ;
#42732 = EDGE_CURVE('',#34056,#34057,#11434,.T.) ;
#42733 = EDGE_CURVE('',#34057,#33845,#11435,.T.) ;
#42734 = EDGE_CURVE('',#34058,#34059,#11436,.T.) ;
#42735 = EDGE_CURVE('',#34059,#34060,#11437,.T.) ;
#42736 = EDGE_CURVE('',#34060,#34061,#11438,.T.) ;
#42737 = EDGE_CURVE('',#34061,#34058,#11439,.T.) ;
#42738 = EDGE_CURVE('',#34062,#34063,#11440,.T.) ;
#42739 = EDGE_CURVE('',#34063,#34064,#11441,.T.) ;
#42740 = EDGE_CURVE('',#34064,#34065,#11442,.T.) ;
#42741 = EDGE_CURVE('',#34065,#34062,#11443,.T.) ;
#42742 = EDGE_CURVE('',#34066,#34067,#11444,.T.) ;
#42743 = EDGE_CURVE('',#34067,#33838,#11445,.T.) ;
#42744 = EDGE_CURVE('',#33839,#34066,#11446,.T.) ;
#42745 = EDGE_CURVE('',#33842,#34068,#11447,.T.) ;
#42746 = EDGE_CURVE('',#34068,#34069,#11448,.T.) ;
#42747 = EDGE_CURVE('',#34069,#33843,#11449,.T.) ;
#42748 = EDGE_CURVE('',#34070,#34071,#11450,.T.) ;
#42749 = EDGE_CURVE('',#34071,#34072,#11451,.T.) ;
#42750 = EDGE_CURVE('',#34072,#34073,#11452,.T.) ;
#42751 = EDGE_CURVE('',#34073,#34070,#11453,.T.) ;
#42752 = EDGE_CURVE('',#34074,#34075,#11454,.T.) ;
#42753 = EDGE_CURVE('',#34075,#34076,#11455,.T.) ;
#42754 = EDGE_CURVE('',#34076,#34077,#11456,.T.) ;
#42755 = EDGE_CURVE('',#34077,#34074,#11457,.T.) ;
#42756 = EDGE_CURVE('',#34078,#34079,#11458,.T.) ;
#42757 = EDGE_CURVE('',#34079,#34080,#11459,.T.) ;
#42758 = EDGE_CURVE('',#34080,#34081,#11460,.T.) ;
#42759 = EDGE_CURVE('',#34081,#34078,#11461,.T.) ;
#42760 = EDGE_CURVE('',#34082,#34083,#11462,.T.) ;
#42761 = EDGE_CURVE('',#34083,#34084,#11463,.T.) ;
#42762 = EDGE_CURVE('',#34084,#34085,#11464,.T.) ;
#42763 = EDGE_CURVE('',#34085,#34082,#11465,.T.) ;
#42764 = EDGE_CURVE('',#34086,#34087,#11466,.T.) ;
#42765 = EDGE_CURVE('',#34087,#34088,#11467,.T.) ;
#42766 = EDGE_CURVE('',#34089,#34088,#11468,.T.) ;
#42767 = EDGE_CURVE('',#34089,#34086,#11469,.T.) ;
#42768 = EDGE_CURVE('',#34090,#34091,#11470,.T.) ;
#42769 = EDGE_CURVE('',#34091,#32269,#28823,.T.) ;
#42770 = EDGE_CURVE('',#33921,#34092,#28824,.T.) ;
#42771 = EDGE_CURVE('',#34092,#34093,#11471,.T.) ;
#42772 = EDGE_CURVE('',#34093,#34090,#11472,.T.) ;
#42773 = EDGE_CURVE('',#34094,#34095,#11473,.T.) ;
#42774 = EDGE_CURVE('',#34095,#32102,#28825,.T.) ;
#42775 = EDGE_CURVE('',#32101,#34096,#28826,.T.) ;
#42776 = EDGE_CURVE('',#34096,#34097,#11474,.T.) ;
#42777 = EDGE_CURVE('',#34097,#34094,#11475,.T.) ;
#42778 = EDGE_CURVE('',#33919,#34071,#28827,.T.) ;
#42779 = EDGE_CURVE('',#34070,#33920,#28828,.T.) ;
#42780 = EDGE_CURVE('',#34088,#32271,#28829,.T.) ;
#42781 = EDGE_CURVE('',#32270,#34089,#28830,.T.) ;
#42782 = EDGE_CURVE('',#34098,#34099,#11476,.T.) ;
#42783 = EDGE_CURVE('',#34099,#34100,#11477,.T.) ;
#42784 = EDGE_CURVE('',#34100,#34101,#11478,.T.) ;
#42785 = EDGE_CURVE('',#34101,#34098,#11479,.T.) ;
#42786 = EDGE_CURVE('',#34102,#34103,#11480,.T.) ;
#42787 = EDGE_CURVE('',#34103,#33849,#11481,.T.) ;
#42788 = EDGE_CURVE('',#33848,#34102,#11482,.T.) ;
#42789 = EDGE_CURVE('',#33852,#34104,#11483,.T.) ;
#42790 = EDGE_CURVE('',#34104,#34105,#11484,.T.) ;
#42791 = EDGE_CURVE('',#34105,#33853,#11485,.T.) ;
#42792 = EDGE_CURVE('',#34106,#34107,#11486,.T.) ;
#42793 = EDGE_CURVE('',#34107,#34108,#11487,.T.) ;
#42794 = EDGE_CURVE('',#34108,#34109,#11488,.T.) ;
#42795 = EDGE_CURVE('',#34109,#34106,#11489,.T.) ;
#42796 = EDGE_CURVE('',#34110,#34111,#11490,.T.) ;
#42797 = EDGE_CURVE('',#34111,#34112,#11491,.T.) ;
#42798 = EDGE_CURVE('',#34112,#34113,#11492,.T.) ;
#42799 = EDGE_CURVE('',#34113,#34110,#11493,.T.) ;
#42800 = EDGE_CURVE('',#34114,#34115,#11494,.T.) ;
#42801 = EDGE_CURVE('',#34115,#33846,#11495,.T.) ;
#42802 = EDGE_CURVE('',#33847,#34114,#11496,.T.) ;
#42803 = EDGE_CURVE('',#33850,#34116,#11497,.T.) ;
#42804 = EDGE_CURVE('',#34116,#34117,#11498,.T.) ;
#42805 = EDGE_CURVE('',#34117,#33851,#11499,.T.) ;
#42806 = EDGE_CURVE('',#34118,#34119,#11500,.T.) ;
#42807 = EDGE_CURVE('',#34119,#34120,#11501,.T.) ;
#42808 = EDGE_CURVE('',#34120,#34121,#11502,.T.) ;
#42809 = EDGE_CURVE('',#34121,#34118,#11503,.T.) ;
#42810 = EDGE_CURVE('',#34122,#34123,#11504,.T.) ;
#42811 = EDGE_CURVE('',#34123,#34124,#11505,.T.) ;
#42812 = EDGE_CURVE('',#34124,#34125,#11506,.T.) ;
#42813 = EDGE_CURVE('',#34125,#34122,#11507,.T.) ;
#42814 = EDGE_CURVE('',#34126,#34127,#11508,.T.) ;
#42815 = EDGE_CURVE('',#34127,#34128,#11509,.T.) ;
#42816 = EDGE_CURVE('',#34128,#34129,#11510,.T.) ;
#42817 = EDGE_CURVE('',#34129,#34126,#11511,.T.) ;
#42818 = EDGE_CURVE('',#34130,#34131,#11512,.T.) ;
#42819 = EDGE_CURVE('',#34131,#34132,#11513,.T.) ;
#42820 = EDGE_CURVE('',#34132,#34133,#11514,.T.) ;
#42821 = EDGE_CURVE('',#34133,#34130,#11515,.T.) ;
#42822 = EDGE_CURVE('',#34134,#34135,#11516,.T.) ;
#42823 = EDGE_CURVE('',#34135,#34136,#11517,.T.) ;
#42824 = EDGE_CURVE('',#34137,#34136,#11518,.T.) ;
#42825 = EDGE_CURVE('',#34137,#34134,#11519,.T.) ;
#42826 = EDGE_CURVE('',#34138,#34139,#11520,.T.) ;
#42827 = EDGE_CURVE('',#34139,#32259,#28831,.T.) ;
#42828 = EDGE_CURVE('',#33929,#34140,#28832,.T.) ;
#42829 = EDGE_CURVE('',#34140,#34141,#11521,.T.) ;
#42830 = EDGE_CURVE('',#34141,#34138,#11522,.T.) ;
#42831 = EDGE_CURVE('',#34142,#34143,#11523,.T.) ;
#42832 = EDGE_CURVE('',#34143,#32087,#28833,.T.) ;
#42833 = EDGE_CURVE('',#32086,#34144,#28834,.T.) ;
#42834 = EDGE_CURVE('',#34144,#34145,#11524,.T.) ;
#42835 = EDGE_CURVE('',#34145,#34142,#11525,.T.) ;
#42836 = EDGE_CURVE('',#33927,#34119,#28835,.T.) ;
#42837 = EDGE_CURVE('',#34118,#33928,#28836,.T.) ;
#42838 = EDGE_CURVE('',#34136,#32261,#28837,.T.) ;
#42839 = EDGE_CURVE('',#32260,#34137,#28838,.T.) ;
#42840 = EDGE_CURVE('',#34146,#34147,#11526,.T.) ;
#42841 = EDGE_CURVE('',#34147,#34148,#11527,.T.) ;
#42842 = EDGE_CURVE('',#34148,#34149,#11528,.T.) ;
#42843 = EDGE_CURVE('',#34149,#34146,#11529,.T.) ;
#42844 = EDGE_CURVE('',#34150,#34151,#11530,.T.) ;
#42845 = EDGE_CURVE('',#34151,#33857,#11531,.T.) ;
#42846 = EDGE_CURVE('',#33856,#34150,#11532,.T.) ;
#42847 = EDGE_CURVE('',#33860,#34152,#11533,.T.) ;
#42848 = EDGE_CURVE('',#34152,#34153,#11534,.T.) ;
#42849 = EDGE_CURVE('',#34153,#33861,#11535,.T.) ;
#42850 = EDGE_CURVE('',#34154,#34155,#11536,.T.) ;
#42851 = EDGE_CURVE('',#34155,#34156,#11537,.T.) ;
#42852 = EDGE_CURVE('',#34156,#34157,#11538,.T.) ;
#42853 = EDGE_CURVE('',#34157,#34154,#11539,.T.) ;
#42854 = EDGE_CURVE('',#34158,#34159,#11540,.T.) ;
#42855 = EDGE_CURVE('',#34159,#34160,#11541,.T.) ;
#42856 = EDGE_CURVE('',#34160,#34161,#11542,.T.) ;
#42857 = EDGE_CURVE('',#34161,#34158,#11543,.T.) ;
#42858 = EDGE_CURVE('',#34162,#34163,#11544,.T.) ;
#42859 = EDGE_CURVE('',#34163,#33854,#11545,.T.) ;
#42860 = EDGE_CURVE('',#33855,#34162,#11546,.T.) ;
#42861 = EDGE_CURVE('',#33858,#34164,#11547,.T.) ;
#42862 = EDGE_CURVE('',#34164,#34165,#11548,.T.) ;
#42863 = EDGE_CURVE('',#34165,#33859,#11549,.T.) ;
#42864 = EDGE_CURVE('',#34166,#34167,#11550,.T.) ;
#42865 = EDGE_CURVE('',#34167,#34168,#11551,.T.) ;
#42866 = EDGE_CURVE('',#34168,#34169,#11552,.T.) ;
#42867 = EDGE_CURVE('',#34169,#34166,#11553,.T.) ;
#42868 = EDGE_CURVE('',#34170,#34171,#11554,.T.) ;
#42869 = EDGE_CURVE('',#34171,#34172,#11555,.T.) ;
#42870 = EDGE_CURVE('',#34172,#34173,#11556,.T.) ;
#42871 = EDGE_CURVE('',#34173,#34170,#11557,.T.) ;
#42872 = EDGE_CURVE('',#34174,#34175,#11558,.T.) ;
#42873 = EDGE_CURVE('',#34175,#34176,#11559,.T.) ;
#42874 = EDGE_CURVE('',#34176,#34177,#11560,.T.) ;
#42875 = EDGE_CURVE('',#34177,#34174,#11561,.T.) ;
#42876 = EDGE_CURVE('',#34178,#34179,#11562,.T.) ;
#42877 = EDGE_CURVE('',#34179,#34180,#11563,.T.) ;
#42878 = EDGE_CURVE('',#34180,#34181,#11564,.T.) ;
#42879 = EDGE_CURVE('',#34181,#34178,#11565,.T.) ;
#42880 = EDGE_CURVE('',#34182,#34183,#11566,.T.) ;
#42881 = EDGE_CURVE('',#34183,#34184,#11567,.T.) ;
#42882 = EDGE_CURVE('',#34185,#34184,#11568,.T.) ;
#42883 = EDGE_CURVE('',#34185,#34182,#11569,.T.) ;
#42884 = EDGE_CURVE('',#34186,#34187,#11570,.T.) ;
#42885 = EDGE_CURVE('',#34187,#32249,#28839,.T.) ;
#42886 = EDGE_CURVE('',#33937,#34188,#28840,.T.) ;
#42887 = EDGE_CURVE('',#34188,#34189,#11571,.T.) ;
#42888 = EDGE_CURVE('',#34189,#34186,#11572,.T.) ;
#42889 = EDGE_CURVE('',#34190,#34191,#11573,.T.) ;
#42890 = EDGE_CURVE('',#34191,#32072,#28841,.T.) ;
#42891 = EDGE_CURVE('',#32071,#34192,#28842,.T.) ;
#42892 = EDGE_CURVE('',#34192,#34193,#11574,.T.) ;
#42893 = EDGE_CURVE('',#34193,#34190,#11575,.T.) ;
#42894 = EDGE_CURVE('',#33935,#34167,#28843,.T.) ;
#42895 = EDGE_CURVE('',#34166,#33936,#28844,.T.) ;
#42896 = EDGE_CURVE('',#34184,#32251,#28845,.T.) ;
#42897 = EDGE_CURVE('',#32250,#34185,#28846,.T.) ;
#42898 = EDGE_CURVE('',#34194,#34195,#11576,.T.) ;
#42899 = EDGE_CURVE('',#34195,#34196,#11577,.T.) ;
#42900 = EDGE_CURVE('',#34196,#34197,#11578,.T.) ;
#42901 = EDGE_CURVE('',#34197,#34194,#11579,.T.) ;
#42902 = EDGE_CURVE('',#34198,#34199,#11580,.T.) ;
#42903 = EDGE_CURVE('',#34199,#33865,#11581,.T.) ;
#42904 = EDGE_CURVE('',#33864,#34198,#11582,.T.) ;
#42905 = EDGE_CURVE('',#33868,#34200,#11583,.T.) ;
#42906 = EDGE_CURVE('',#34200,#34201,#11584,.T.) ;
#42907 = EDGE_CURVE('',#34201,#33869,#11585,.T.) ;
#42908 = EDGE_CURVE('',#34202,#34203,#11586,.T.) ;
#42909 = EDGE_CURVE('',#34203,#34204,#11587,.T.) ;
#42910 = EDGE_CURVE('',#34204,#34205,#11588,.T.) ;
#42911 = EDGE_CURVE('',#34205,#34202,#11589,.T.) ;
#42912 = EDGE_CURVE('',#34206,#34207,#11590,.T.) ;
#42913 = EDGE_CURVE('',#34207,#34208,#11591,.T.) ;
#42914 = EDGE_CURVE('',#34208,#34209,#11592,.T.) ;
#42915 = EDGE_CURVE('',#34209,#34206,#11593,.T.) ;
#42916 = EDGE_CURVE('',#34210,#34211,#11594,.T.) ;
#42917 = EDGE_CURVE('',#34211,#33862,#11595,.T.) ;
#42918 = EDGE_CURVE('',#33863,#34210,#11596,.T.) ;
#42919 = EDGE_CURVE('',#33866,#34212,#11597,.T.) ;
#42920 = EDGE_CURVE('',#34212,#34213,#11598,.T.) ;
#42921 = EDGE_CURVE('',#34213,#33867,#11599,.T.) ;
#42922 = EDGE_CURVE('',#34214,#34215,#11600,.T.) ;
#42923 = EDGE_CURVE('',#34215,#34216,#11601,.T.) ;
#42924 = EDGE_CURVE('',#34216,#34217,#11602,.T.) ;
#42925 = EDGE_CURVE('',#34217,#34214,#11603,.T.) ;
#42926 = EDGE_CURVE('',#34218,#34219,#11604,.T.) ;
#42927 = EDGE_CURVE('',#34219,#34220,#11605,.T.) ;
#42928 = EDGE_CURVE('',#34220,#34221,#11606,.T.) ;
#42929 = EDGE_CURVE('',#34221,#34218,#11607,.T.) ;
#42930 = EDGE_CURVE('',#34222,#34223,#11608,.T.) ;
#42931 = EDGE_CURVE('',#34223,#34224,#11609,.T.) ;
#42932 = EDGE_CURVE('',#34224,#34225,#11610,.T.) ;
#42933 = EDGE_CURVE('',#34225,#34222,#11611,.T.) ;
#42934 = EDGE_CURVE('',#34226,#34227,#11612,.T.) ;
#42935 = EDGE_CURVE('',#34227,#34228,#11613,.T.) ;
#42936 = EDGE_CURVE('',#34228,#34229,#11614,.T.) ;
#42937 = EDGE_CURVE('',#34229,#34226,#11615,.T.) ;
#42938 = EDGE_CURVE('',#34230,#34231,#11616,.T.) ;
#42939 = EDGE_CURVE('',#34231,#34232,#11617,.T.) ;
#42940 = EDGE_CURVE('',#34233,#34232,#11618,.T.) ;
#42941 = EDGE_CURVE('',#34233,#34230,#11619,.T.) ;
#42942 = EDGE_CURVE('',#34234,#34235,#11620,.T.) ;
#42943 = EDGE_CURVE('',#34235,#32239,#28847,.T.) ;
#42944 = EDGE_CURVE('',#33945,#34236,#28848,.T.) ;
#42945 = EDGE_CURVE('',#34236,#34237,#11621,.T.) ;
#42946 = EDGE_CURVE('',#34237,#34234,#11622,.T.) ;
#42947 = EDGE_CURVE('',#34238,#34239,#11623,.T.) ;
#42948 = EDGE_CURVE('',#34239,#32057,#28849,.T.) ;
#42949 = EDGE_CURVE('',#32056,#34240,#28850,.T.) ;
#42950 = EDGE_CURVE('',#34240,#34241,#11624,.T.) ;
#42951 = EDGE_CURVE('',#34241,#34238,#11625,.T.) ;
#42952 = EDGE_CURVE('',#33943,#34215,#28851,.T.) ;
#42953 = EDGE_CURVE('',#34214,#33944,#28852,.T.) ;
#42954 = EDGE_CURVE('',#34232,#32241,#28853,.T.) ;
#42955 = EDGE_CURVE('',#32240,#34233,#28854,.T.) ;
#42956 = EDGE_CURVE('',#34242,#34243,#11626,.T.) ;
#42957 = EDGE_CURVE('',#34243,#34244,#11627,.T.) ;
#42958 = EDGE_CURVE('',#34244,#34245,#11628,.T.) ;
#42959 = EDGE_CURVE('',#34245,#34242,#11629,.T.) ;
#42960 = EDGE_CURVE('',#34246,#34247,#11630,.T.) ;
#42961 = EDGE_CURVE('',#34247,#33873,#11631,.T.) ;
#42962 = EDGE_CURVE('',#33872,#34246,#11632,.T.) ;
#42963 = EDGE_CURVE('',#33876,#34248,#11633,.T.) ;
#42964 = EDGE_CURVE('',#34248,#34249,#11634,.T.) ;
#42965 = EDGE_CURVE('',#34249,#33877,#11635,.T.) ;
#42966 = EDGE_CURVE('',#34250,#34251,#11636,.T.) ;
#42967 = EDGE_CURVE('',#34251,#34252,#11637,.T.) ;
#42968 = EDGE_CURVE('',#34252,#34253,#11638,.T.) ;
#42969 = EDGE_CURVE('',#34253,#34250,#11639,.T.) ;
#42970 = EDGE_CURVE('',#34254,#34255,#11640,.T.) ;
#42971 = EDGE_CURVE('',#34255,#34256,#11641,.T.) ;
#42972 = EDGE_CURVE('',#34256,#34257,#11642,.T.) ;
#42973 = EDGE_CURVE('',#34257,#34254,#11643,.T.) ;
#42974 = EDGE_CURVE('',#34258,#34259,#11644,.T.) ;
#42975 = EDGE_CURVE('',#34259,#33870,#11645,.T.) ;
#42976 = EDGE_CURVE('',#33871,#34258,#11646,.T.) ;
#42977 = EDGE_CURVE('',#33874,#34260,#11647,.T.) ;
#42978 = EDGE_CURVE('',#34260,#34261,#11648,.T.) ;
#42979 = EDGE_CURVE('',#34261,#33875,#11649,.T.) ;
#42980 = EDGE_CURVE('',#34262,#34263,#11650,.T.) ;
#42981 = EDGE_CURVE('',#34263,#34264,#11651,.T.) ;
#42982 = EDGE_CURVE('',#34264,#34265,#11652,.T.) ;
#42983 = EDGE_CURVE('',#34265,#34262,#11653,.T.) ;
#42984 = EDGE_CURVE('',#34266,#34267,#11654,.T.) ;
#42985 = EDGE_CURVE('',#34267,#34268,#11655,.T.) ;
#42986 = EDGE_CURVE('',#34268,#34269,#11656,.T.) ;
#42987 = EDGE_CURVE('',#34269,#34266,#11657,.T.) ;
#42988 = EDGE_CURVE('',#34270,#34271,#11658,.T.) ;
#42989 = EDGE_CURVE('',#34271,#34272,#11659,.T.) ;
#42990 = EDGE_CURVE('',#34272,#34273,#11660,.T.) ;
#42991 = EDGE_CURVE('',#34273,#34270,#11661,.T.) ;
#42992 = EDGE_CURVE('',#34274,#34275,#11662,.T.) ;
#42993 = EDGE_CURVE('',#34275,#34276,#11663,.T.) ;
#42994 = EDGE_CURVE('',#34276,#34277,#11664,.T.) ;
#42995 = EDGE_CURVE('',#34277,#34274,#11665,.T.) ;
#42996 = EDGE_CURVE('',#34278,#34279,#11666,.T.) ;
#42997 = EDGE_CURVE('',#34279,#34280,#11667,.T.) ;
#42998 = EDGE_CURVE('',#34281,#34280,#11668,.T.) ;
#42999 = EDGE_CURVE('',#34281,#34278,#11669,.T.) ;
#43000 = EDGE_CURVE('',#34282,#34283,#11670,.T.) ;
#43001 = EDGE_CURVE('',#34283,#32229,#28855,.T.) ;
#43002 = EDGE_CURVE('',#33953,#34284,#28856,.T.) ;
#43003 = EDGE_CURVE('',#34284,#34285,#11671,.T.) ;
#43004 = EDGE_CURVE('',#34285,#34282,#11672,.T.) ;
#43005 = EDGE_CURVE('',#34286,#34287,#11673,.T.) ;
#43006 = EDGE_CURVE('',#34287,#32042,#28857,.T.) ;
#43007 = EDGE_CURVE('',#32041,#34288,#28858,.T.) ;
#43008 = EDGE_CURVE('',#34288,#34289,#11674,.T.) ;
#43009 = EDGE_CURVE('',#34289,#34286,#11675,.T.) ;
#43010 = EDGE_CURVE('',#33951,#34263,#28859,.T.) ;
#43011 = EDGE_CURVE('',#34262,#33952,#28860,.T.) ;
#43012 = EDGE_CURVE('',#34280,#32231,#28861,.T.) ;
#43013 = EDGE_CURVE('',#32230,#34281,#28862,.T.) ;
#43014 = EDGE_CURVE('',#34290,#34291,#11676,.T.) ;
#43015 = EDGE_CURVE('',#34291,#34292,#11677,.T.) ;
#43016 = EDGE_CURVE('',#34292,#34293,#11678,.T.) ;
#43017 = EDGE_CURVE('',#34293,#34290,#11679,.T.) ;
#43018 = EDGE_CURVE('',#34294,#34295,#11680,.T.) ;
#43019 = EDGE_CURVE('',#34295,#33881,#11681,.T.) ;
#43020 = EDGE_CURVE('',#33880,#34294,#11682,.T.) ;
#43021 = EDGE_CURVE('',#33884,#34296,#11683,.T.) ;
#43022 = EDGE_CURVE('',#34296,#34297,#11684,.T.) ;
#43023 = EDGE_CURVE('',#34297,#33885,#11685,.T.) ;
#43024 = EDGE_CURVE('',#34298,#34299,#11686,.T.) ;
#43025 = EDGE_CURVE('',#34299,#34300,#11687,.T.) ;
#43026 = EDGE_CURVE('',#34300,#34301,#11688,.T.) ;
#43027 = EDGE_CURVE('',#34301,#34298,#11689,.T.) ;
#43028 = EDGE_CURVE('',#34302,#34303,#11690,.T.) ;
#43029 = EDGE_CURVE('',#34303,#34304,#11691,.T.) ;
#43030 = EDGE_CURVE('',#34304,#34305,#11692,.T.) ;
#43031 = EDGE_CURVE('',#34305,#34302,#11693,.T.) ;
#43032 = EDGE_CURVE('',#34306,#34307,#11694,.T.) ;
#43033 = EDGE_CURVE('',#34307,#33878,#11695,.T.) ;
#43034 = EDGE_CURVE('',#33879,#34306,#11696,.T.) ;
#43035 = EDGE_CURVE('',#33882,#34308,#11697,.T.) ;
#43036 = EDGE_CURVE('',#34308,#34309,#11698,.T.) ;
#43037 = EDGE_CURVE('',#34309,#33883,#11699,.T.) ;
#43038 = EDGE_CURVE('',#34310,#34311,#11700,.T.) ;
#43039 = EDGE_CURVE('',#34311,#34312,#11701,.T.) ;
#43040 = EDGE_CURVE('',#34312,#34313,#11702,.T.) ;
#43041 = EDGE_CURVE('',#34313,#34310,#11703,.T.) ;
#43042 = EDGE_CURVE('',#34314,#34315,#11704,.T.) ;
#43043 = EDGE_CURVE('',#34315,#34316,#11705,.T.) ;
#43044 = EDGE_CURVE('',#34316,#34317,#11706,.T.) ;
#43045 = EDGE_CURVE('',#34317,#34314,#11707,.T.) ;
#43046 = EDGE_CURVE('',#34318,#34319,#11708,.T.) ;
#43047 = EDGE_CURVE('',#34319,#34320,#11709,.T.) ;
#43048 = EDGE_CURVE('',#34320,#34321,#11710,.T.) ;
#43049 = EDGE_CURVE('',#34321,#34318,#11711,.T.) ;
#43050 = EDGE_CURVE('',#34322,#34323,#11712,.T.) ;
#43051 = EDGE_CURVE('',#34323,#34324,#11713,.T.) ;
#43052 = EDGE_CURVE('',#34324,#34325,#11714,.T.) ;
#43053 = EDGE_CURVE('',#34325,#34322,#11715,.T.) ;
#43054 = EDGE_CURVE('',#34326,#34327,#11716,.T.) ;
#43055 = EDGE_CURVE('',#34327,#34328,#11717,.T.) ;
#43056 = EDGE_CURVE('',#34329,#34328,#11718,.T.) ;
#43057 = EDGE_CURVE('',#34329,#34326,#11719,.T.) ;
#43058 = EDGE_CURVE('',#34330,#34331,#11720,.T.) ;
#43059 = EDGE_CURVE('',#34331,#32219,#28863,.T.) ;
#43060 = EDGE_CURVE('',#33961,#34332,#28864,.T.) ;
#43061 = EDGE_CURVE('',#34332,#34333,#11721,.T.) ;
#43062 = EDGE_CURVE('',#34333,#34330,#11722,.T.) ;
#43063 = EDGE_CURVE('',#34334,#34335,#11723,.T.) ;
#43064 = EDGE_CURVE('',#34335,#32027,#28865,.T.) ;
#43065 = EDGE_CURVE('',#32026,#34336,#28866,.T.) ;
#43066 = EDGE_CURVE('',#34336,#34337,#11724,.T.) ;
#43067 = EDGE_CURVE('',#34337,#34334,#11725,.T.) ;
#43068 = EDGE_CURVE('',#33959,#34311,#28867,.T.) ;
#43069 = EDGE_CURVE('',#34310,#33960,#28868,.T.) ;
#43070 = EDGE_CURVE('',#34328,#32221,#28869,.T.) ;
#43071 = EDGE_CURVE('',#32220,#34329,#28870,.T.) ;
#43072 = EDGE_CURVE('',#34338,#34339,#11726,.T.) ;
#43073 = EDGE_CURVE('',#34339,#34340,#11727,.T.) ;
#43074 = EDGE_CURVE('',#34340,#34341,#11728,.T.) ;
#43075 = EDGE_CURVE('',#34341,#34338,#11729,.T.) ;
#43076 = EDGE_CURVE('',#34342,#34343,#11730,.T.) ;
#43077 = EDGE_CURVE('',#34343,#33889,#11731,.T.) ;
#43078 = EDGE_CURVE('',#33888,#34342,#11732,.T.) ;
#43079 = EDGE_CURVE('',#33892,#34344,#11733,.T.) ;
#43080 = EDGE_CURVE('',#34344,#34345,#11734,.T.) ;
#43081 = EDGE_CURVE('',#34345,#33893,#11735,.T.) ;
#43082 = EDGE_CURVE('',#34346,#34347,#11736,.T.) ;
#43083 = EDGE_CURVE('',#34347,#34348,#11737,.T.) ;
#43084 = EDGE_CURVE('',#34348,#34349,#11738,.T.) ;
#43085 = EDGE_CURVE('',#34349,#34346,#11739,.T.) ;
#43086 = EDGE_CURVE('',#34350,#34351,#11740,.T.) ;
#43087 = EDGE_CURVE('',#34351,#34352,#11741,.T.) ;
#43088 = EDGE_CURVE('',#34352,#34353,#11742,.T.) ;
#43089 = EDGE_CURVE('',#34353,#34350,#11743,.T.) ;
#43090 = EDGE_CURVE('',#34354,#34355,#11744,.T.) ;
#43091 = EDGE_CURVE('',#34355,#33886,#11745,.T.) ;
#43092 = EDGE_CURVE('',#33887,#34354,#11746,.T.) ;
#43093 = EDGE_CURVE('',#33890,#34356,#11747,.T.) ;
#43094 = EDGE_CURVE('',#34356,#34357,#11748,.T.) ;
#43095 = EDGE_CURVE('',#34357,#33891,#11749,.T.) ;
#43096 = EDGE_CURVE('',#34358,#34359,#11750,.T.) ;
#43097 = EDGE_CURVE('',#34359,#34360,#11751,.T.) ;
#43098 = EDGE_CURVE('',#34360,#34361,#11752,.T.) ;
#43099 = EDGE_CURVE('',#34361,#34358,#11753,.T.) ;
#43100 = EDGE_CURVE('',#34362,#34363,#11754,.T.) ;
#43101 = EDGE_CURVE('',#34363,#34364,#11755,.T.) ;
#43102 = EDGE_CURVE('',#34364,#34365,#11756,.T.) ;
#43103 = EDGE_CURVE('',#34365,#34362,#11757,.T.) ;
#43104 = EDGE_CURVE('',#34366,#34367,#11758,.T.) ;
#43105 = EDGE_CURVE('',#34367,#34368,#11759,.T.) ;
#43106 = EDGE_CURVE('',#34368,#34369,#11760,.T.) ;
#43107 = EDGE_CURVE('',#34369,#34366,#11761,.T.) ;
#43108 = EDGE_CURVE('',#34370,#34371,#11762,.T.) ;
#43109 = EDGE_CURVE('',#34371,#34372,#11763,.T.) ;
#43110 = EDGE_CURVE('',#34372,#34373,#11764,.T.) ;
#43111 = EDGE_CURVE('',#34373,#34370,#11765,.T.) ;
#43112 = EDGE_CURVE('',#34374,#34375,#11766,.T.) ;
#43113 = EDGE_CURVE('',#34375,#34376,#11767,.T.) ;
#43114 = EDGE_CURVE('',#34377,#34376,#11768,.T.) ;
#43115 = EDGE_CURVE('',#34377,#34374,#11769,.T.) ;
#43116 = EDGE_CURVE('',#34378,#34379,#11770,.T.) ;
#43117 = EDGE_CURVE('',#34379,#32209,#28871,.T.) ;
#43118 = EDGE_CURVE('',#33969,#34380,#28872,.T.) ;
#43119 = EDGE_CURVE('',#34380,#34381,#11771,.T.) ;
#43120 = EDGE_CURVE('',#34381,#34378,#11772,.T.) ;
#43121 = EDGE_CURVE('',#34382,#34383,#11773,.T.) ;
#43122 = EDGE_CURVE('',#34383,#32012,#28873,.T.) ;
#43123 = EDGE_CURVE('',#32011,#34384,#28874,.T.) ;
#43124 = EDGE_CURVE('',#34384,#34385,#11774,.T.) ;
#43125 = EDGE_CURVE('',#34385,#34382,#11775,.T.) ;
#43126 = EDGE_CURVE('',#33967,#34359,#28875,.T.) ;
#43127 = EDGE_CURVE('',#34358,#33968,#28876,.T.) ;
#43128 = EDGE_CURVE('',#34376,#32211,#28877,.T.) ;
#43129 = EDGE_CURVE('',#32210,#34377,#28878,.T.) ;
#43130 = EDGE_CURVE('',#34386,#34387,#11776,.T.) ;
#43131 = EDGE_CURVE('',#34387,#34388,#11777,.T.) ;
#43132 = EDGE_CURVE('',#34388,#34389,#11778,.T.) ;
#43133 = EDGE_CURVE('',#34389,#34386,#11779,.T.) ;
#43134 = EDGE_CURVE('',#34390,#34391,#11780,.T.) ;
#43135 = EDGE_CURVE('',#34391,#33897,#11781,.T.) ;
#43136 = EDGE_CURVE('',#33896,#34390,#11782,.T.) ;
#43137 = EDGE_CURVE('',#33900,#34392,#11783,.T.) ;
#43138 = EDGE_CURVE('',#34392,#34393,#11784,.T.) ;
#43139 = EDGE_CURVE('',#34393,#33901,#11785,.T.) ;
#43140 = EDGE_CURVE('',#34394,#34395,#11786,.T.) ;
#43141 = EDGE_CURVE('',#34395,#34396,#11787,.T.) ;
#43142 = EDGE_CURVE('',#34396,#34397,#11788,.T.) ;
#43143 = EDGE_CURVE('',#34397,#34394,#11789,.T.) ;
#43144 = EDGE_CURVE('',#34398,#34399,#11790,.T.) ;
#43145 = EDGE_CURVE('',#34399,#34400,#11791,.T.) ;
#43146 = EDGE_CURVE('',#34400,#34401,#11792,.T.) ;
#43147 = EDGE_CURVE('',#34401,#34398,#11793,.T.) ;
#43148 = EDGE_CURVE('',#34402,#34403,#11794,.T.) ;
#43149 = EDGE_CURVE('',#34403,#33894,#11795,.T.) ;
#43150 = EDGE_CURVE('',#33895,#34402,#11796,.T.) ;
#43151 = EDGE_CURVE('',#33898,#34404,#11797,.T.) ;
#43152 = EDGE_CURVE('',#34404,#34405,#11798,.T.) ;
#43153 = EDGE_CURVE('',#34405,#33899,#11799,.T.) ;
#43154 = EDGE_CURVE('',#34406,#34407,#11800,.T.) ;
#43155 = EDGE_CURVE('',#34407,#34408,#11801,.T.) ;
#43156 = EDGE_CURVE('',#34408,#34409,#11802,.T.) ;
#43157 = EDGE_CURVE('',#34409,#34406,#11803,.T.) ;
#43158 = EDGE_CURVE('',#34410,#34411,#11804,.T.) ;
#43159 = EDGE_CURVE('',#34411,#34412,#11805,.T.) ;
#43160 = EDGE_CURVE('',#34412,#34413,#11806,.T.) ;
#43161 = EDGE_CURVE('',#34413,#34410,#11807,.T.) ;
#43162 = EDGE_CURVE('',#34414,#34415,#11808,.T.) ;
#43163 = EDGE_CURVE('',#34415,#34416,#11809,.T.) ;
#43164 = EDGE_CURVE('',#34416,#34417,#11810,.T.) ;
#43165 = EDGE_CURVE('',#34417,#34414,#11811,.T.) ;
#43166 = EDGE_CURVE('',#34418,#34419,#11812,.T.) ;
#43167 = EDGE_CURVE('',#34419,#34420,#11813,.T.) ;
#43168 = EDGE_CURVE('',#34420,#34421,#11814,.T.) ;
#43169 = EDGE_CURVE('',#34421,#34418,#11815,.T.) ;
#43170 = EDGE_CURVE('',#34422,#34423,#11816,.T.) ;
#43171 = EDGE_CURVE('',#34423,#34424,#11817,.T.) ;
#43172 = EDGE_CURVE('',#34424,#34425,#11818,.T.) ;
#43173 = EDGE_CURVE('',#34425,#34422,#11819,.T.) ;
#43174 = EDGE_CURVE('',#34426,#34427,#11820,.T.) ;
#43175 = EDGE_CURVE('',#34427,#34428,#11821,.T.) ;
#43176 = EDGE_CURVE('',#34428,#34429,#11822,.T.) ;
#43177 = EDGE_CURVE('',#34429,#34426,#11823,.T.) ;
#43178 = EDGE_CURVE('',#34430,#34431,#11824,.T.) ;
#43179 = EDGE_CURVE('',#34431,#34432,#11825,.T.) ;
#43180 = EDGE_CURVE('',#34432,#34433,#11826,.T.) ;
#43181 = EDGE_CURVE('',#34433,#34430,#11827,.T.) ;
#43182 = EDGE_CURVE('',#34434,#34435,#11828,.T.) ;
#43183 = EDGE_CURVE('',#34435,#34436,#11829,.T.) ;
#43184 = EDGE_CURVE('',#34436,#34437,#11830,.T.) ;
#43185 = EDGE_CURVE('',#34437,#34434,#11831,.T.) ;
#43186 = EDGE_CURVE('',#34438,#34439,#11832,.T.) ;
#43187 = EDGE_CURVE('',#34439,#34440,#11833,.T.) ;
#43188 = EDGE_CURVE('',#34440,#34441,#11834,.T.) ;
#43189 = EDGE_CURVE('',#34441,#34438,#11835,.T.) ;
#43190 = EDGE_CURVE('',#34442,#34443,#11836,.T.) ;
#43191 = EDGE_CURVE('',#34443,#34444,#11837,.T.) ;
#43192 = EDGE_CURVE('',#34444,#34445,#11838,.T.) ;
#43193 = EDGE_CURVE('',#34445,#34442,#11839,.T.) ;
#43194 = EDGE_CURVE('',#34446,#34447,#11840,.T.) ;
#43195 = EDGE_CURVE('',#34447,#34448,#11841,.T.) ;
#43196 = EDGE_CURVE('',#34448,#34449,#11842,.T.) ;
#43197 = EDGE_CURVE('',#34449,#34446,#11843,.T.) ;
#43198 = EDGE_CURVE('',#34450,#34451,#11844,.T.) ;
#43199 = EDGE_CURVE('',#34451,#34452,#11845,.T.) ;
#43200 = EDGE_CURVE('',#34452,#34453,#11846,.T.) ;
#43201 = EDGE_CURVE('',#34453,#34450,#11847,.T.) ;
#43202 = EDGE_CURVE('',#34454,#34455,#11848,.T.) ;
#43203 = EDGE_CURVE('',#34455,#34456,#11849,.T.) ;
#43204 = EDGE_CURVE('',#34456,#34457,#11850,.T.) ;
#43205 = EDGE_CURVE('',#34457,#34454,#11851,.T.) ;
#43206 = EDGE_CURVE('',#34458,#34459,#11852,.T.) ;
#43207 = EDGE_CURVE('',#34459,#34460,#11853,.T.) ;
#43208 = EDGE_CURVE('',#34460,#34461,#11854,.T.) ;
#43209 = EDGE_CURVE('',#34461,#34458,#11855,.T.) ;
#43210 = EDGE_CURVE('',#34462,#34463,#11856,.T.) ;
#43211 = EDGE_CURVE('',#34463,#34464,#11857,.T.) ;
#43212 = EDGE_CURVE('',#34464,#34465,#11858,.T.) ;
#43213 = EDGE_CURVE('',#34465,#34462,#11859,.T.) ;
#43214 = EDGE_CURVE('',#34466,#34467,#11860,.T.) ;
#43215 = EDGE_CURVE('',#34467,#34468,#11861,.T.) ;
#43216 = EDGE_CURVE('',#34468,#34469,#11862,.T.) ;
#43217 = EDGE_CURVE('',#34469,#34466,#11863,.T.) ;
#43218 = EDGE_CURVE('',#34470,#34471,#11864,.T.) ;
#43219 = EDGE_CURVE('',#34471,#34472,#11865,.T.) ;
#43220 = EDGE_CURVE('',#34472,#34473,#11866,.T.) ;
#43221 = EDGE_CURVE('',#34473,#34470,#11867,.T.) ;
#43222 = EDGE_CURVE('',#34474,#34475,#11868,.T.) ;
#43223 = EDGE_CURVE('',#34475,#34476,#11869,.T.) ;
#43224 = EDGE_CURVE('',#34476,#34477,#11870,.T.) ;
#43225 = EDGE_CURVE('',#34477,#34474,#11871,.T.) ;
#43226 = EDGE_CURVE('',#34478,#34479,#11872,.T.) ;
#43227 = EDGE_CURVE('',#34479,#34480,#11873,.T.) ;
#43228 = EDGE_CURVE('',#34480,#34481,#11874,.T.) ;
#43229 = EDGE_CURVE('',#34481,#34478,#11875,.T.) ;
#43230 = EDGE_CURVE('',#34482,#34483,#11876,.T.) ;
#43231 = EDGE_CURVE('',#34483,#34484,#11877,.T.) ;
#43232 = EDGE_CURVE('',#34484,#34485,#11878,.T.) ;
#43233 = EDGE_CURVE('',#34485,#34482,#11879,.T.) ;
#43234 = EDGE_CURVE('',#34486,#34487,#11880,.T.) ;
#43235 = EDGE_CURVE('',#34487,#34488,#11881,.T.) ;
#43236 = EDGE_CURVE('',#34488,#34489,#11882,.T.) ;
#43237 = EDGE_CURVE('',#34489,#34486,#11883,.T.) ;
#43238 = EDGE_CURVE('',#34490,#34491,#11884,.T.) ;
#43239 = EDGE_CURVE('',#34491,#34492,#11885,.T.) ;
#43240 = EDGE_CURVE('',#34492,#34493,#11886,.T.) ;
#43241 = EDGE_CURVE('',#34493,#34490,#11887,.T.) ;
#43242 = EDGE_CURVE('',#34494,#34495,#11888,.T.) ;
#43243 = EDGE_CURVE('',#34495,#34496,#11889,.T.) ;
#43244 = EDGE_CURVE('',#34496,#34497,#11890,.T.) ;
#43245 = EDGE_CURVE('',#34497,#34494,#11891,.T.) ;
#43246 = EDGE_CURVE('',#34498,#34499,#11892,.T.) ;
#43247 = EDGE_CURVE('',#34499,#34500,#11893,.T.) ;
#43248 = EDGE_CURVE('',#34500,#34501,#11894,.T.) ;
#43249 = EDGE_CURVE('',#34501,#34498,#11895,.T.) ;
#43250 = EDGE_CURVE('',#34502,#34503,#11896,.T.) ;
#43251 = EDGE_CURVE('',#34503,#34504,#11897,.T.) ;
#43252 = EDGE_CURVE('',#34504,#34505,#11898,.T.) ;
#43253 = EDGE_CURVE('',#34505,#34502,#11899,.T.) ;
#43254 = EDGE_CURVE('',#34506,#34507,#11900,.T.) ;
#43255 = EDGE_CURVE('',#34507,#34508,#11901,.T.) ;
#43256 = EDGE_CURVE('',#34508,#34509,#11902,.T.) ;
#43257 = EDGE_CURVE('',#34509,#34506,#11903,.T.) ;
#43258 = EDGE_CURVE('',#34510,#34511,#11904,.T.) ;
#43259 = EDGE_CURVE('',#34511,#34512,#11905,.T.) ;
#43260 = EDGE_CURVE('',#34512,#34513,#11906,.T.) ;
#43261 = EDGE_CURVE('',#34513,#34510,#11907,.T.) ;
#43262 = EDGE_CURVE('',#34514,#34515,#11908,.T.) ;
#43263 = EDGE_CURVE('',#34515,#34516,#11909,.T.) ;
#43264 = EDGE_CURVE('',#34516,#34517,#11910,.T.) ;
#43265 = EDGE_CURVE('',#34517,#34514,#11911,.T.) ;
#43266 = EDGE_CURVE('',#34518,#34519,#11912,.T.) ;
#43267 = EDGE_CURVE('',#34519,#34520,#11913,.T.) ;
#43268 = EDGE_CURVE('',#34520,#34521,#11914,.T.) ;
#43269 = EDGE_CURVE('',#34521,#34518,#11915,.T.) ;
#43270 = EDGE_CURVE('',#34522,#34523,#11916,.T.) ;
#43271 = EDGE_CURVE('',#34523,#34524,#11917,.T.) ;
#43272 = EDGE_CURVE('',#34524,#34525,#11918,.T.) ;
#43273 = EDGE_CURVE('',#34525,#34522,#11919,.T.) ;
#43274 = EDGE_CURVE('',#34526,#34527,#11920,.T.) ;
#43275 = EDGE_CURVE('',#34527,#34528,#11921,.T.) ;
#43276 = EDGE_CURVE('',#34528,#34529,#11922,.T.) ;
#43277 = EDGE_CURVE('',#34529,#34526,#11923,.T.) ;
#43278 = EDGE_CURVE('',#34530,#34531,#11924,.T.) ;
#43279 = EDGE_CURVE('',#34531,#34532,#11925,.T.) ;
#43280 = EDGE_CURVE('',#34532,#34533,#11926,.T.) ;
#43281 = EDGE_CURVE('',#34533,#34530,#11927,.T.) ;
#43282 = EDGE_CURVE('',#34534,#34535,#11928,.T.) ;
#43283 = EDGE_CURVE('',#34535,#34536,#11929,.T.) ;
#43284 = EDGE_CURVE('',#34536,#34537,#11930,.T.) ;
#43285 = EDGE_CURVE('',#34537,#34534,#11931,.T.) ;
#43286 = EDGE_CURVE('',#34538,#34539,#11932,.T.) ;
#43287 = EDGE_CURVE('',#34539,#34540,#11933,.T.) ;
#43288 = EDGE_CURVE('',#34540,#34541,#11934,.T.) ;
#43289 = EDGE_CURVE('',#34541,#34538,#11935,.T.) ;
#43290 = EDGE_CURVE('',#34542,#34543,#11936,.T.) ;
#43291 = EDGE_CURVE('',#34543,#34544,#11937,.T.) ;
#43292 = EDGE_CURVE('',#34544,#34545,#11938,.T.) ;
#43293 = EDGE_CURVE('',#34545,#34542,#11939,.T.) ;
#43294 = EDGE_CURVE('',#34546,#34547,#11940,.T.) ;
#43295 = EDGE_CURVE('',#34547,#34548,#11941,.T.) ;
#43296 = EDGE_CURVE('',#34548,#34549,#11942,.T.) ;
#43297 = EDGE_CURVE('',#34549,#34546,#11943,.T.) ;
#43298 = EDGE_CURVE('',#34472,#33986,#28879,.T.) ;
#43299 = EDGE_CURVE('',#34473,#33989,#28880,.T.) ;
#43300 = EDGE_CURVE('',#33986,#33991,#28881,.T.) ;
#43301 = EDGE_CURVE('',#33990,#33987,#28882,.T.) ;
#43302 = EDGE_CURVE('',#34473,#33982,#28883,.T.) ;
#43303 = EDGE_CURVE('',#33982,#33989,#28884,.T.) ;
#43304 = EDGE_CURVE('',#33987,#34475,#28885,.T.) ;
#43305 = EDGE_CURVE('',#33988,#34474,#28886,.T.) ;
#43306 = EDGE_CURVE('',#33983,#33988,#28887,.T.) ;
#43307 = EDGE_CURVE('',#34470,#33985,#28888,.T.) ;
#43308 = EDGE_CURVE('',#33983,#34474,#28889,.T.) ;
#43309 = EDGE_CURVE('',#34470,#33978,#28890,.T.) ;
#43310 = EDGE_CURVE('',#33978,#33985,#28891,.T.) ;
#43311 = EDGE_CURVE('',#33984,#34477,#28892,.T.) ;
#43312 = EDGE_CURVE('',#33979,#33984,#28893,.T.) ;
#43313 = EDGE_CURVE('',#33981,#34471,#28894,.T.) ;
#43314 = EDGE_CURVE('',#33979,#34477,#28895,.T.) ;
#43315 = EDGE_CURVE('',#33976,#33981,#28896,.T.) ;
#43316 = EDGE_CURVE('',#33980,#33977,#28897,.T.) ;
#43317 = EDGE_CURVE('',#34476,#33980,#28898,.T.) ;
#43318 = EDGE_CURVE('',#34544,#34002,#28899,.T.) ;
#43319 = EDGE_CURVE('',#34545,#34005,#28900,.T.) ;
#43320 = EDGE_CURVE('',#34002,#34007,#28901,.T.) ;
#43321 = EDGE_CURVE('',#34006,#34003,#28902,.T.) ;
#43322 = EDGE_CURVE('',#34545,#34016,#28903,.T.) ;
#43323 = EDGE_CURVE('',#34016,#34005,#28904,.T.) ;
#43324 = EDGE_CURVE('',#34003,#34547,#28905,.T.) ;
#43325 = EDGE_CURVE('',#34004,#34546,#28906,.T.) ;
#43326 = EDGE_CURVE('',#34017,#34004,#28907,.T.) ;
#43327 = EDGE_CURVE('',#34542,#34015,#28908,.T.) ;
#43328 = EDGE_CURVE('',#34017,#34546,#28909,.T.) ;
#43329 = EDGE_CURVE('',#34542,#34010,#28910,.T.) ;
#43330 = EDGE_CURVE('',#34010,#34015,#28911,.T.) ;
#43331 = EDGE_CURVE('',#34014,#34549,#28912,.T.) ;
#43332 = EDGE_CURVE('',#34011,#34014,#28913,.T.) ;
#43333 = EDGE_CURVE('',#34013,#34543,#28914,.T.) ;
#43334 = EDGE_CURVE('',#34011,#34549,#28915,.T.) ;
#43335 = EDGE_CURVE('',#34008,#34013,#28916,.T.) ;
#43336 = EDGE_CURVE('',#34012,#34009,#28917,.T.) ;
#43337 = EDGE_CURVE('',#34548,#34012,#28918,.T.) ;
#43338 = EDGE_CURVE('',#34464,#34034,#28919,.T.) ;
#43339 = EDGE_CURVE('',#34465,#34037,#28920,.T.) ;
#43340 = EDGE_CURVE('',#34034,#34039,#28921,.T.) ;
#43341 = EDGE_CURVE('',#34038,#34035,#28922,.T.) ;
#43342 = EDGE_CURVE('',#34465,#34030,#28923,.T.) ;
#43343 = EDGE_CURVE('',#34030,#34037,#28924,.T.) ;
#43344 = EDGE_CURVE('',#34035,#34467,#28925,.T.) ;
#43345 = EDGE_CURVE('',#34036,#34466,#28926,.T.) ;
#43346 = EDGE_CURVE('',#34031,#34036,#28927,.T.) ;
#43347 = EDGE_CURVE('',#34462,#34033,#28928,.T.) ;
#43348 = EDGE_CURVE('',#34031,#34466,#28929,.T.) ;
#43349 = EDGE_CURVE('',#34462,#34026,#28930,.T.) ;
#43350 = EDGE_CURVE('',#34026,#34033,#28931,.T.) ;
#43351 = EDGE_CURVE('',#34032,#34469,#28932,.T.) ;
#43352 = EDGE_CURVE('',#34027,#34032,#28933,.T.) ;
#43353 = EDGE_CURVE('',#34029,#34463,#28934,.T.) ;
#43354 = EDGE_CURVE('',#34027,#34469,#28935,.T.) ;
#43355 = EDGE_CURVE('',#34024,#34029,#28936,.T.) ;
#43356 = EDGE_CURVE('',#34028,#34025,#28937,.T.) ;
#43357 = EDGE_CURVE('',#34468,#34028,#28938,.T.) ;
#43358 = EDGE_CURVE('',#34536,#34050,#28939,.T.) ;
#43359 = EDGE_CURVE('',#34537,#34053,#28940,.T.) ;
#43360 = EDGE_CURVE('',#34050,#34055,#28941,.T.) ;
#43361 = EDGE_CURVE('',#34054,#34051,#28942,.T.) ;
#43362 = EDGE_CURVE('',#34537,#34064,#28943,.T.) ;
#43363 = EDGE_CURVE('',#34064,#34053,#28944,.T.) ;
#43364 = EDGE_CURVE('',#34051,#34539,#28945,.T.) ;
#43365 = EDGE_CURVE('',#34052,#34538,#28946,.T.) ;
#43366 = EDGE_CURVE('',#34065,#34052,#28947,.T.) ;
#43367 = EDGE_CURVE('',#34534,#34063,#28948,.T.) ;
#43368 = EDGE_CURVE('',#34065,#34538,#28949,.T.) ;
#43369 = EDGE_CURVE('',#34534,#34058,#28950,.T.) ;
#43370 = EDGE_CURVE('',#34058,#34063,#28951,.T.) ;
#43371 = EDGE_CURVE('',#34062,#34541,#28952,.T.) ;
#43372 = EDGE_CURVE('',#34059,#34062,#28953,.T.) ;
#43373 = EDGE_CURVE('',#34061,#34535,#28954,.T.) ;
#43374 = EDGE_CURVE('',#34059,#34541,#28955,.T.) ;
#43375 = EDGE_CURVE('',#34056,#34061,#28956,.T.) ;
#43376 = EDGE_CURVE('',#34060,#34057,#28957,.T.) ;
#43377 = EDGE_CURVE('',#34540,#34060,#28958,.T.) ;
#43378 = EDGE_CURVE('',#34456,#34082,#28959,.T.) ;
#43379 = EDGE_CURVE('',#34457,#34085,#28960,.T.) ;
#43380 = EDGE_CURVE('',#34082,#34087,#28961,.T.) ;
#43381 = EDGE_CURVE('',#34086,#34083,#28962,.T.) ;
#43382 = EDGE_CURVE('',#34457,#34078,#28963,.T.) ;
#43383 = EDGE_CURVE('',#34078,#34085,#28964,.T.) ;
#43384 = EDGE_CURVE('',#34083,#34459,#28965,.T.) ;
#43385 = EDGE_CURVE('',#34084,#34458,#28966,.T.) ;
#43386 = EDGE_CURVE('',#34079,#34084,#28967,.T.) ;
#43387 = EDGE_CURVE('',#34454,#34081,#28968,.T.) ;
#43388 = EDGE_CURVE('',#34079,#34458,#28969,.T.) ;
#43389 = EDGE_CURVE('',#34454,#34074,#28970,.T.) ;
#43390 = EDGE_CURVE('',#34074,#34081,#28971,.T.) ;
#43391 = EDGE_CURVE('',#34080,#34461,#28972,.T.) ;
#43392 = EDGE_CURVE('',#34075,#34080,#28973,.T.) ;
#43393 = EDGE_CURVE('',#34077,#34455,#28974,.T.) ;
#43394 = EDGE_CURVE('',#34075,#34461,#28975,.T.) ;
#43395 = EDGE_CURVE('',#34072,#34077,#28976,.T.) ;
#43396 = EDGE_CURVE('',#34076,#34073,#28977,.T.) ;
#43397 = EDGE_CURVE('',#34460,#34076,#28978,.T.) ;
#43398 = EDGE_CURVE('',#34528,#34098,#28979,.T.) ;
#43399 = EDGE_CURVE('',#34529,#34101,#28980,.T.) ;
#43400 = EDGE_CURVE('',#34098,#34103,#28981,.T.) ;
#43401 = EDGE_CURVE('',#34102,#34099,#28982,.T.) ;
#43402 = EDGE_CURVE('',#34529,#34112,#28983,.T.) ;
#43403 = EDGE_CURVE('',#34112,#34101,#28984,.T.) ;
#43404 = EDGE_CURVE('',#34099,#34531,#28985,.T.) ;
#43405 = EDGE_CURVE('',#34100,#34530,#28986,.T.) ;
#43406 = EDGE_CURVE('',#34113,#34100,#28987,.T.) ;
#43407 = EDGE_CURVE('',#34526,#34111,#28988,.T.) ;
#43408 = EDGE_CURVE('',#34113,#34530,#28989,.T.) ;
#43409 = EDGE_CURVE('',#34526,#34106,#28990,.T.) ;
#43410 = EDGE_CURVE('',#34106,#34111,#28991,.T.) ;
#43411 = EDGE_CURVE('',#34110,#34533,#28992,.T.) ;
#43412 = EDGE_CURVE('',#34107,#34110,#28993,.T.) ;
#43413 = EDGE_CURVE('',#34109,#34527,#28994,.T.) ;
#43414 = EDGE_CURVE('',#34107,#34533,#28995,.T.) ;
#43415 = EDGE_CURVE('',#34104,#34109,#28996,.T.) ;
#43416 = EDGE_CURVE('',#34108,#34105,#28997,.T.) ;
#43417 = EDGE_CURVE('',#34532,#34108,#28998,.T.) ;
#43418 = EDGE_CURVE('',#34448,#34130,#28999,.T.) ;
#43419 = EDGE_CURVE('',#34449,#34133,#29000,.T.) ;
#43420 = EDGE_CURVE('',#34130,#34135,#29001,.T.) ;
#43421 = EDGE_CURVE('',#34134,#34131,#29002,.T.) ;
#43422 = EDGE_CURVE('',#34449,#34126,#29003,.T.) ;
#43423 = EDGE_CURVE('',#34126,#34133,#29004,.T.) ;
#43424 = EDGE_CURVE('',#34131,#34451,#29005,.T.) ;
#43425 = EDGE_CURVE('',#34132,#34450,#29006,.T.) ;
#43426 = EDGE_CURVE('',#34127,#34132,#29007,.T.) ;
#43427 = EDGE_CURVE('',#34446,#34129,#29008,.T.) ;
#43428 = EDGE_CURVE('',#34127,#34450,#29009,.T.) ;
#43429 = EDGE_CURVE('',#34446,#34122,#29010,.T.) ;
#43430 = EDGE_CURVE('',#34122,#34129,#29011,.T.) ;
#43431 = EDGE_CURVE('',#34128,#34453,#29012,.T.) ;
#43432 = EDGE_CURVE('',#34123,#34128,#29013,.T.) ;
#43433 = EDGE_CURVE('',#34125,#34447,#29014,.T.) ;
#43434 = EDGE_CURVE('',#34123,#34453,#29015,.T.) ;
#43435 = EDGE_CURVE('',#34120,#34125,#29016,.T.) ;
#43436 = EDGE_CURVE('',#34124,#34121,#29017,.T.) ;
#43437 = EDGE_CURVE('',#34452,#34124,#29018,.T.) ;
#43438 = EDGE_CURVE('',#34520,#34146,#29019,.T.) ;
#43439 = EDGE_CURVE('',#34521,#34149,#29020,.T.) ;
#43440 = EDGE_CURVE('',#34146,#34151,#29021,.T.) ;
#43441 = EDGE_CURVE('',#34150,#34147,#29022,.T.) ;
#43442 = EDGE_CURVE('',#34521,#34160,#29023,.T.) ;
#43443 = EDGE_CURVE('',#34160,#34149,#29024,.T.) ;
#43444 = EDGE_CURVE('',#34147,#34523,#29025,.T.) ;
#43445 = EDGE_CURVE('',#34148,#34522,#29026,.T.) ;
#43446 = EDGE_CURVE('',#34161,#34148,#29027,.T.) ;
#43447 = EDGE_CURVE('',#34518,#34159,#29028,.T.) ;
#43448 = EDGE_CURVE('',#34161,#34522,#29029,.T.) ;
#43449 = EDGE_CURVE('',#34518,#34154,#29030,.T.) ;
#43450 = EDGE_CURVE('',#34154,#34159,#29031,.T.) ;
#43451 = EDGE_CURVE('',#34158,#34525,#29032,.T.) ;
#43452 = EDGE_CURVE('',#34155,#34158,#29033,.T.) ;
#43453 = EDGE_CURVE('',#34157,#34519,#29034,.T.) ;
#43454 = EDGE_CURVE('',#34155,#34525,#29035,.T.) ;
#43455 = EDGE_CURVE('',#34152,#34157,#29036,.T.) ;
#43456 = EDGE_CURVE('',#34156,#34153,#29037,.T.) ;
#43457 = EDGE_CURVE('',#34524,#34156,#29038,.T.) ;
#43458 = EDGE_CURVE('',#34440,#34178,#29039,.T.) ;
#43459 = EDGE_CURVE('',#34441,#34181,#29040,.T.) ;
#43460 = EDGE_CURVE('',#34178,#34183,#29041,.T.) ;
#43461 = EDGE_CURVE('',#34182,#34179,#29042,.T.) ;
#43462 = EDGE_CURVE('',#34441,#34174,#29043,.T.) ;
#43463 = EDGE_CURVE('',#34174,#34181,#29044,.T.) ;
#43464 = EDGE_CURVE('',#34179,#34443,#29045,.T.) ;
#43465 = EDGE_CURVE('',#34180,#34442,#29046,.T.) ;
#43466 = EDGE_CURVE('',#34175,#34180,#29047,.T.) ;
#43467 = EDGE_CURVE('',#34438,#34177,#29048,.T.) ;
#43468 = EDGE_CURVE('',#34175,#34442,#29049,.T.) ;
#43469 = EDGE_CURVE('',#34438,#34170,#29050,.T.) ;
#43470 = EDGE_CURVE('',#34170,#34177,#29051,.T.) ;
#43471 = EDGE_CURVE('',#34176,#34445,#29052,.T.) ;
#43472 = EDGE_CURVE('',#34171,#34176,#29053,.T.) ;
#43473 = EDGE_CURVE('',#34173,#34439,#29054,.T.) ;
#43474 = EDGE_CURVE('',#34171,#34445,#29055,.T.) ;
#43475 = EDGE_CURVE('',#34168,#34173,#29056,.T.) ;
#43476 = EDGE_CURVE('',#34172,#34169,#29057,.T.) ;
#43477 = EDGE_CURVE('',#34444,#34172,#29058,.T.) ;
#43478 = EDGE_CURVE('',#34512,#34194,#29059,.T.) ;
#43479 = EDGE_CURVE('',#34513,#34197,#29060,.T.) ;
#43480 = EDGE_CURVE('',#34194,#34199,#29061,.T.) ;
#43481 = EDGE_CURVE('',#34198,#34195,#29062,.T.) ;
#43482 = EDGE_CURVE('',#34513,#34208,#29063,.T.) ;
#43483 = EDGE_CURVE('',#34208,#34197,#29064,.T.) ;
#43484 = EDGE_CURVE('',#34195,#34515,#29065,.T.) ;
#43485 = EDGE_CURVE('',#34196,#34514,#29066,.T.) ;
#43486 = EDGE_CURVE('',#34209,#34196,#29067,.T.) ;
#43487 = EDGE_CURVE('',#34510,#34207,#29068,.T.) ;
#43488 = EDGE_CURVE('',#34209,#34514,#29069,.T.) ;
#43489 = EDGE_CURVE('',#34510,#34202,#29070,.T.) ;
#43490 = EDGE_CURVE('',#34202,#34207,#29071,.T.) ;
#43491 = EDGE_CURVE('',#34206,#34517,#29072,.T.) ;
#43492 = EDGE_CURVE('',#34203,#34206,#29073,.T.) ;
#43493 = EDGE_CURVE('',#34205,#34511,#29074,.T.) ;
#43494 = EDGE_CURVE('',#34203,#34517,#29075,.T.) ;
#43495 = EDGE_CURVE('',#34200,#34205,#29076,.T.) ;
#43496 = EDGE_CURVE('',#34204,#34201,#29077,.T.) ;
#43497 = EDGE_CURVE('',#34516,#34204,#29078,.T.) ;
#43498 = EDGE_CURVE('',#34432,#34226,#29079,.T.) ;
#43499 = EDGE_CURVE('',#34433,#34229,#29080,.T.) ;
#43500 = EDGE_CURVE('',#34226,#34231,#29081,.T.) ;
#43501 = EDGE_CURVE('',#34230,#34227,#29082,.T.) ;
#43502 = EDGE_CURVE('',#34433,#34222,#29083,.T.) ;
#43503 = EDGE_CURVE('',#34222,#34229,#29084,.T.) ;
#43504 = EDGE_CURVE('',#34227,#34435,#29085,.T.) ;
#43505 = EDGE_CURVE('',#34228,#34434,#29086,.T.) ;
#43506 = EDGE_CURVE('',#34223,#34228,#29087,.T.) ;
#43507 = EDGE_CURVE('',#34430,#34225,#29088,.T.) ;
#43508 = EDGE_CURVE('',#34223,#34434,#29089,.T.) ;
#43509 = EDGE_CURVE('',#34430,#34218,#29090,.T.) ;
#43510 = EDGE_CURVE('',#34218,#34225,#29091,.T.) ;
#43511 = EDGE_CURVE('',#34224,#34437,#29092,.T.) ;
#43512 = EDGE_CURVE('',#34219,#34224,#29093,.T.) ;
#43513 = EDGE_CURVE('',#34221,#34431,#29094,.T.) ;
#43514 = EDGE_CURVE('',#34219,#34437,#29095,.T.) ;
#43515 = EDGE_CURVE('',#34216,#34221,#29096,.T.) ;
#43516 = EDGE_CURVE('',#34220,#34217,#29097,.T.) ;
#43517 = EDGE_CURVE('',#34436,#34220,#29098,.T.) ;
#43518 = EDGE_CURVE('',#34504,#34242,#29099,.T.) ;
#43519 = EDGE_CURVE('',#34505,#34245,#29100,.T.) ;
#43520 = EDGE_CURVE('',#34242,#34247,#29101,.T.) ;
#43521 = EDGE_CURVE('',#34246,#34243,#29102,.T.) ;
#43522 = EDGE_CURVE('',#34505,#34256,#29103,.T.) ;
#43523 = EDGE_CURVE('',#34256,#34245,#29104,.T.) ;
#43524 = EDGE_CURVE('',#34243,#34507,#29105,.T.) ;
#43525 = EDGE_CURVE('',#34244,#34506,#29106,.T.) ;
#43526 = EDGE_CURVE('',#34257,#34244,#29107,.T.) ;
#43527 = EDGE_CURVE('',#34502,#34255,#29108,.T.) ;
#43528 = EDGE_CURVE('',#34257,#34506,#29109,.T.) ;
#43529 = EDGE_CURVE('',#34502,#34250,#29110,.T.) ;
#43530 = EDGE_CURVE('',#34250,#34255,#29111,.T.) ;
#43531 = EDGE_CURVE('',#34254,#34509,#29112,.T.) ;
#43532 = EDGE_CURVE('',#34251,#34254,#29113,.T.) ;
#43533 = EDGE_CURVE('',#34253,#34503,#29114,.T.) ;
#43534 = EDGE_CURVE('',#34251,#34509,#29115,.T.) ;
#43535 = EDGE_CURVE('',#34248,#34253,#29116,.T.) ;
#43536 = EDGE_CURVE('',#34252,#34249,#29117,.T.) ;
#43537 = EDGE_CURVE('',#34508,#34252,#29118,.T.) ;
#43538 = EDGE_CURVE('',#34424,#34274,#29119,.T.) ;
#43539 = EDGE_CURVE('',#34425,#34277,#29120,.T.) ;
#43540 = EDGE_CURVE('',#34274,#34279,#29121,.T.) ;
#43541 = EDGE_CURVE('',#34278,#34275,#29122,.T.) ;
#43542 = EDGE_CURVE('',#34425,#34270,#29123,.T.) ;
#43543 = EDGE_CURVE('',#34270,#34277,#29124,.T.) ;
#43544 = EDGE_CURVE('',#34275,#34427,#29125,.T.) ;
#43545 = EDGE_CURVE('',#34276,#34426,#29126,.T.) ;
#43546 = EDGE_CURVE('',#34271,#34276,#29127,.T.) ;
#43547 = EDGE_CURVE('',#34422,#34273,#29128,.T.) ;
#43548 = EDGE_CURVE('',#34271,#34426,#29129,.T.) ;
#43549 = EDGE_CURVE('',#34422,#34266,#29130,.T.) ;
#43550 = EDGE_CURVE('',#34266,#34273,#29131,.T.) ;
#43551 = EDGE_CURVE('',#34272,#34429,#29132,.T.) ;
#43552 = EDGE_CURVE('',#34267,#34272,#29133,.T.) ;
#43553 = EDGE_CURVE('',#34269,#34423,#29134,.T.) ;
#43554 = EDGE_CURVE('',#34267,#34429,#29135,.T.) ;
#43555 = EDGE_CURVE('',#34264,#34269,#29136,.T.) ;
#43556 = EDGE_CURVE('',#34268,#34265,#29137,.T.) ;
#43557 = EDGE_CURVE('',#34428,#34268,#29138,.T.) ;
#43558 = EDGE_CURVE('',#34496,#34290,#29139,.T.) ;
#43559 = EDGE_CURVE('',#34497,#34293,#29140,.T.) ;
#43560 = EDGE_CURVE('',#34290,#34295,#29141,.T.) ;
#43561 = EDGE_CURVE('',#34294,#34291,#29142,.T.) ;
#43562 = EDGE_CURVE('',#34497,#34304,#29143,.T.) ;
#43563 = EDGE_CURVE('',#34304,#34293,#29144,.T.) ;
#43564 = EDGE_CURVE('',#34291,#34499,#29145,.T.) ;
#43565 = EDGE_CURVE('',#34292,#34498,#29146,.T.) ;
#43566 = EDGE_CURVE('',#34305,#34292,#29147,.T.) ;
#43567 = EDGE_CURVE('',#34494,#34303,#29148,.T.) ;
#43568 = EDGE_CURVE('',#34305,#34498,#29149,.T.) ;
#43569 = EDGE_CURVE('',#34494,#34298,#29150,.T.) ;
#43570 = EDGE_CURVE('',#34298,#34303,#29151,.T.) ;
#43571 = EDGE_CURVE('',#34302,#34501,#29152,.T.) ;
#43572 = EDGE_CURVE('',#34299,#34302,#29153,.T.) ;
#43573 = EDGE_CURVE('',#34301,#34495,#29154,.T.) ;
#43574 = EDGE_CURVE('',#34299,#34501,#29155,.T.) ;
#43575 = EDGE_CURVE('',#34296,#34301,#29156,.T.) ;
#43576 = EDGE_CURVE('',#34300,#34297,#29157,.T.) ;
#43577 = EDGE_CURVE('',#34500,#34300,#29158,.T.) ;
#43578 = EDGE_CURVE('',#34416,#34322,#29159,.T.) ;
#43579 = EDGE_CURVE('',#34417,#34325,#29160,.T.) ;
#43580 = EDGE_CURVE('',#34322,#34327,#29161,.T.) ;
#43581 = EDGE_CURVE('',#34326,#34323,#29162,.T.) ;
#43582 = EDGE_CURVE('',#34417,#34318,#29163,.T.) ;
#43583 = EDGE_CURVE('',#34318,#34325,#29164,.T.) ;
#43584 = EDGE_CURVE('',#34323,#34419,#29165,.T.) ;
#43585 = EDGE_CURVE('',#34324,#34418,#29166,.T.) ;
#43586 = EDGE_CURVE('',#34319,#34324,#29167,.T.) ;
#43587 = EDGE_CURVE('',#34414,#34321,#29168,.T.) ;
#43588 = EDGE_CURVE('',#34319,#34418,#29169,.T.) ;
#43589 = EDGE_CURVE('',#34414,#34314,#29170,.T.) ;
#43590 = EDGE_CURVE('',#34314,#34321,#29171,.T.) ;
#43591 = EDGE_CURVE('',#34320,#34421,#29172,.T.) ;
#43592 = EDGE_CURVE('',#34315,#34320,#29173,.T.) ;
#43593 = EDGE_CURVE('',#34317,#34415,#29174,.T.) ;
#43594 = EDGE_CURVE('',#34315,#34421,#29175,.T.) ;
#43595 = EDGE_CURVE('',#34312,#34317,#29176,.T.) ;
#43596 = EDGE_CURVE('',#34316,#34313,#29177,.T.) ;
#43597 = EDGE_CURVE('',#34420,#34316,#29178,.T.) ;
#43598 = EDGE_CURVE('',#34488,#34338,#29179,.T.) ;
#43599 = EDGE_CURVE('',#34489,#34341,#29180,.T.) ;
#43600 = EDGE_CURVE('',#34338,#34343,#29181,.T.) ;
#43601 = EDGE_CURVE('',#34342,#34339,#29182,.T.) ;
#43602 = EDGE_CURVE('',#34489,#34352,#29183,.T.) ;
#43603 = EDGE_CURVE('',#34352,#34341,#29184,.T.) ;
#43604 = EDGE_CURVE('',#34339,#34491,#29185,.T.) ;
#43605 = EDGE_CURVE('',#34340,#34490,#29186,.T.) ;
#43606 = EDGE_CURVE('',#34353,#34340,#29187,.T.) ;
#43607 = EDGE_CURVE('',#34486,#34351,#29188,.T.) ;
#43608 = EDGE_CURVE('',#34353,#34490,#29189,.T.) ;
#43609 = EDGE_CURVE('',#34486,#34346,#29190,.T.) ;
#43610 = EDGE_CURVE('',#34346,#34351,#29191,.T.) ;
#43611 = EDGE_CURVE('',#34350,#34493,#29192,.T.) ;
#43612 = EDGE_CURVE('',#34347,#34350,#29193,.T.) ;
#43613 = EDGE_CURVE('',#34349,#34487,#29194,.T.) ;
#43614 = EDGE_CURVE('',#34347,#34493,#29195,.T.) ;
#43615 = EDGE_CURVE('',#34344,#34349,#29196,.T.) ;
#43616 = EDGE_CURVE('',#34348,#34345,#29197,.T.) ;
#43617 = EDGE_CURVE('',#34492,#34348,#29198,.T.) ;
#43618 = EDGE_CURVE('',#34408,#34370,#29199,.T.) ;
#43619 = EDGE_CURVE('',#34409,#34373,#29200,.T.) ;
#43620 = EDGE_CURVE('',#34370,#34375,#29201,.T.) ;
#43621 = EDGE_CURVE('',#34374,#34371,#29202,.T.) ;
#43622 = EDGE_CURVE('',#34409,#34366,#29203,.T.) ;
#43623 = EDGE_CURVE('',#34366,#34373,#29204,.T.) ;
#43624 = EDGE_CURVE('',#34371,#34411,#29205,.T.) ;
#43625 = EDGE_CURVE('',#34372,#34410,#29206,.T.) ;
#43626 = EDGE_CURVE('',#34367,#34372,#29207,.T.) ;
#43627 = EDGE_CURVE('',#34406,#34369,#29208,.T.) ;
#43628 = EDGE_CURVE('',#34367,#34410,#29209,.T.) ;
#43629 = EDGE_CURVE('',#34406,#34362,#29210,.T.) ;
#43630 = EDGE_CURVE('',#34362,#34369,#29211,.T.) ;
#43631 = EDGE_CURVE('',#34368,#34413,#29212,.T.) ;
#43632 = EDGE_CURVE('',#34363,#34368,#29213,.T.) ;
#43633 = EDGE_CURVE('',#34365,#34407,#29214,.T.) ;
#43634 = EDGE_CURVE('',#34363,#34413,#29215,.T.) ;
#43635 = EDGE_CURVE('',#34360,#34365,#29216,.T.) ;
#43636 = EDGE_CURVE('',#34364,#34361,#29217,.T.) ;
#43637 = EDGE_CURVE('',#34412,#34364,#29218,.T.) ;
#43638 = EDGE_CURVE('',#34480,#34386,#29219,.T.) ;
#43639 = EDGE_CURVE('',#34481,#34389,#29220,.T.) ;
#43640 = EDGE_CURVE('',#34386,#34391,#29221,.T.) ;
#43641 = EDGE_CURVE('',#34390,#34387,#29222,.T.) ;
#43642 = EDGE_CURVE('',#34481,#34400,#29223,.T.) ;
#43643 = EDGE_CURVE('',#34400,#34389,#29224,.T.) ;
#43644 = EDGE_CURVE('',#34387,#34483,#29225,.T.) ;
#43645 = EDGE_CURVE('',#34388,#34482,#29226,.T.) ;
#43646 = EDGE_CURVE('',#34401,#34388,#29227,.T.) ;
#43647 = EDGE_CURVE('',#34478,#34399,#29228,.T.) ;
#43648 = EDGE_CURVE('',#34401,#34482,#29229,.T.) ;
#43649 = EDGE_CURVE('',#34478,#34394,#29230,.T.) ;
#43650 = EDGE_CURVE('',#34394,#34399,#29231,.T.) ;
#43651 = EDGE_CURVE('',#34398,#34485,#29232,.T.) ;
#43652 = EDGE_CURVE('',#34395,#34398,#29233,.T.) ;
#43653 = EDGE_CURVE('',#34397,#34479,#29234,.T.) ;
#43654 = EDGE_CURVE('',#34395,#34485,#29235,.T.) ;
#43655 = EDGE_CURVE('',#34392,#34397,#29236,.T.) ;
#43656 = EDGE_CURVE('',#34396,#34393,#29237,.T.) ;
#43657 = EDGE_CURVE('',#34484,#34396,#29238,.T.) ;
#43658 = EDGE_CURVE('',#34000,#33992,#29239,.T.) ;
#43659 = EDGE_CURVE('',#34001,#33991,#29240,.T.) ;
#43660 = EDGE_CURVE('',#34001,#34472,#29241,.T.) ;
#43661 = EDGE_CURVE('',#33998,#34471,#29242,.T.) ;
#43662 = EDGE_CURVE('',#33998,#33976,#29243,.T.) ;
#43663 = EDGE_CURVE('',#33999,#33975,#29244,.T.) ;
#43664 = EDGE_CURVE('',#33996,#33974,#29245,.T.) ;
#43665 = EDGE_CURVE('',#33997,#33977,#29246,.T.) ;
#43666 = EDGE_CURVE('',#33997,#34476,#29247,.T.) ;
#43667 = EDGE_CURVE('',#33994,#34475,#29248,.T.) ;
#43668 = EDGE_CURVE('',#33994,#33990,#29249,.T.) ;
#43669 = EDGE_CURVE('',#33995,#33993,#29250,.T.) ;
#43670 = EDGE_CURVE('',#34020,#34007,#29251,.T.) ;
#43671 = EDGE_CURVE('',#34020,#34544,#29252,.T.) ;
#43672 = EDGE_CURVE('',#34021,#34543,#29253,.T.) ;
#43673 = EDGE_CURVE('',#34021,#34008,#29254,.T.) ;
#43674 = EDGE_CURVE('',#34006,#34019,#29255,.T.) ;
#43675 = EDGE_CURVE('',#34547,#34019,#29256,.T.) ;
#43676 = EDGE_CURVE('',#34548,#34018,#29257,.T.) ;
#43677 = EDGE_CURVE('',#34018,#34009,#29258,.T.) ;
#43678 = EDGE_CURVE('',#34048,#34040,#29259,.T.) ;
#43679 = EDGE_CURVE('',#34049,#34039,#29260,.T.) ;
#43680 = EDGE_CURVE('',#34049,#34464,#29261,.T.) ;
#43681 = EDGE_CURVE('',#34046,#34463,#29262,.T.) ;
#43682 = EDGE_CURVE('',#34046,#34024,#29263,.T.) ;
#43683 = EDGE_CURVE('',#34047,#34023,#29264,.T.) ;
#43684 = EDGE_CURVE('',#34044,#34022,#29265,.T.) ;
#43685 = EDGE_CURVE('',#34045,#34025,#29266,.T.) ;
#43686 = EDGE_CURVE('',#34045,#34468,#29267,.T.) ;
#43687 = EDGE_CURVE('',#34042,#34467,#29268,.T.) ;
#43688 = EDGE_CURVE('',#34042,#34038,#29269,.T.) ;
#43689 = EDGE_CURVE('',#34043,#34041,#29270,.T.) ;
#43690 = EDGE_CURVE('',#34068,#34055,#29271,.T.) ;
#43691 = EDGE_CURVE('',#34068,#34536,#29272,.T.) ;
#43692 = EDGE_CURVE('',#34069,#34535,#29273,.T.) ;
#43693 = EDGE_CURVE('',#34069,#34056,#29274,.T.) ;
#43694 = EDGE_CURVE('',#34054,#34067,#29275,.T.) ;
#43695 = EDGE_CURVE('',#34539,#34067,#29276,.T.) ;
#43696 = EDGE_CURVE('',#34540,#34066,#29277,.T.) ;
#43697 = EDGE_CURVE('',#34066,#34057,#29278,.T.) ;
#43698 = EDGE_CURVE('',#34096,#34088,#29279,.T.) ;
#43699 = EDGE_CURVE('',#34097,#34087,#29280,.T.) ;
#43700 = EDGE_CURVE('',#34097,#34456,#29281,.T.) ;
#43701 = EDGE_CURVE('',#34094,#34455,#29282,.T.) ;
#43702 = EDGE_CURVE('',#34094,#34072,#29283,.T.) ;
#43703 = EDGE_CURVE('',#34095,#34071,#29284,.T.) ;
#43704 = EDGE_CURVE('',#34092,#34070,#29285,.T.) ;
#43705 = EDGE_CURVE('',#34093,#34073,#29286,.T.) ;
#43706 = EDGE_CURVE('',#34093,#34460,#29287,.T.) ;
#43707 = EDGE_CURVE('',#34090,#34459,#29288,.T.) ;
#43708 = EDGE_CURVE('',#34090,#34086,#29289,.T.) ;
#43709 = EDGE_CURVE('',#34091,#34089,#29290,.T.) ;
#43710 = EDGE_CURVE('',#34116,#34103,#29291,.T.) ;
#43711 = EDGE_CURVE('',#34116,#34528,#29292,.T.) ;
#43712 = EDGE_CURVE('',#34117,#34527,#29293,.T.) ;
#43713 = EDGE_CURVE('',#34117,#34104,#29294,.T.) ;
#43714 = EDGE_CURVE('',#34102,#34115,#29295,.T.) ;
#43715 = EDGE_CURVE('',#34531,#34115,#29296,.T.) ;
#43716 = EDGE_CURVE('',#34532,#34114,#29297,.T.) ;
#43717 = EDGE_CURVE('',#34114,#34105,#29298,.T.) ;
#43718 = EDGE_CURVE('',#34144,#34136,#29299,.T.) ;
#43719 = EDGE_CURVE('',#34145,#34135,#29300,.T.) ;
#43720 = EDGE_CURVE('',#34145,#34448,#29301,.T.) ;
#43721 = EDGE_CURVE('',#34142,#34447,#29302,.T.) ;
#43722 = EDGE_CURVE('',#34142,#34120,#29303,.T.) ;
#43723 = EDGE_CURVE('',#34143,#34119,#29304,.T.) ;
#43724 = EDGE_CURVE('',#34140,#34118,#29305,.T.) ;
#43725 = EDGE_CURVE('',#34141,#34121,#29306,.T.) ;
#43726 = EDGE_CURVE('',#34141,#34452,#29307,.T.) ;
#43727 = EDGE_CURVE('',#34138,#34451,#29308,.T.) ;
#43728 = EDGE_CURVE('',#34138,#34134,#29309,.T.) ;
#43729 = EDGE_CURVE('',#34139,#34137,#29310,.T.) ;
#43730 = EDGE_CURVE('',#34164,#34151,#29311,.T.) ;
#43731 = EDGE_CURVE('',#34164,#34520,#29312,.T.) ;
#43732 = EDGE_CURVE('',#34165,#34519,#29313,.T.) ;
#43733 = EDGE_CURVE('',#34165,#34152,#29314,.T.) ;
#43734 = EDGE_CURVE('',#34150,#34163,#29315,.T.) ;
#43735 = EDGE_CURVE('',#34523,#34163,#29316,.T.) ;
#43736 = EDGE_CURVE('',#34524,#34162,#29317,.T.) ;
#43737 = EDGE_CURVE('',#34162,#34153,#29318,.T.) ;
#43738 = EDGE_CURVE('',#34192,#34184,#29319,.T.) ;
#43739 = EDGE_CURVE('',#34193,#34183,#29320,.T.) ;
#43740 = EDGE_CURVE('',#34193,#34440,#29321,.T.) ;
#43741 = EDGE_CURVE('',#34190,#34439,#29322,.T.) ;
#43742 = EDGE_CURVE('',#34190,#34168,#29323,.T.) ;
#43743 = EDGE_CURVE('',#34191,#34167,#29324,.T.) ;
#43744 = EDGE_CURVE('',#34188,#34166,#29325,.T.) ;
#43745 = EDGE_CURVE('',#34189,#34169,#29326,.T.) ;
#43746 = EDGE_CURVE('',#34189,#34444,#29327,.T.) ;
#43747 = EDGE_CURVE('',#34186,#34443,#29328,.T.) ;
#43748 = EDGE_CURVE('',#34186,#34182,#29329,.T.) ;
#43749 = EDGE_CURVE('',#34187,#34185,#29330,.T.) ;
#43750 = EDGE_CURVE('',#34212,#34199,#29331,.T.) ;
#43751 = EDGE_CURVE('',#34212,#34512,#29332,.T.) ;
#43752 = EDGE_CURVE('',#34213,#34511,#29333,.T.) ;
#43753 = EDGE_CURVE('',#34213,#34200,#29334,.T.) ;
#43754 = EDGE_CURVE('',#34198,#34211,#29335,.T.) ;
#43755 = EDGE_CURVE('',#34515,#34211,#29336,.T.) ;
#43756 = EDGE_CURVE('',#34516,#34210,#29337,.T.) ;
#43757 = EDGE_CURVE('',#34210,#34201,#29338,.T.) ;
#43758 = EDGE_CURVE('',#34240,#34232,#29339,.T.) ;
#43759 = EDGE_CURVE('',#34241,#34231,#29340,.T.) ;
#43760 = EDGE_CURVE('',#34241,#34432,#29341,.T.) ;
#43761 = EDGE_CURVE('',#34238,#34431,#29342,.T.) ;
#43762 = EDGE_CURVE('',#34238,#34216,#29343,.T.) ;
#43763 = EDGE_CURVE('',#34239,#34215,#29344,.T.) ;
#43764 = EDGE_CURVE('',#34236,#34214,#29345,.T.) ;
#43765 = EDGE_CURVE('',#34237,#34217,#29346,.T.) ;
#43766 = EDGE_CURVE('',#34237,#34436,#29347,.T.) ;
#43767 = EDGE_CURVE('',#34234,#34435,#29348,.T.) ;
#43768 = EDGE_CURVE('',#34234,#34230,#29349,.T.) ;
#43769 = EDGE_CURVE('',#34235,#34233,#29350,.T.) ;
#43770 = EDGE_CURVE('',#34260,#34247,#29351,.T.) ;
#43771 = EDGE_CURVE('',#34260,#34504,#29352,.T.) ;
#43772 = EDGE_CURVE('',#34261,#34503,#29353,.T.) ;
#43773 = EDGE_CURVE('',#34261,#34248,#29354,.T.) ;
#43774 = EDGE_CURVE('',#34246,#34259,#29355,.T.) ;
#43775 = EDGE_CURVE('',#34507,#34259,#29356,.T.) ;
#43776 = EDGE_CURVE('',#34508,#34258,#29357,.T.) ;
#43777 = EDGE_CURVE('',#34258,#34249,#29358,.T.) ;
#43778 = EDGE_CURVE('',#34288,#34280,#29359,.T.) ;
#43779 = EDGE_CURVE('',#34289,#34279,#29360,.T.) ;
#43780 = EDGE_CURVE('',#34289,#34424,#29361,.T.) ;
#43781 = EDGE_CURVE('',#34286,#34423,#29362,.T.) ;
#43782 = EDGE_CURVE('',#34286,#34264,#29363,.T.) ;
#43783 = EDGE_CURVE('',#34287,#34263,#29364,.T.) ;
#43784 = EDGE_CURVE('',#34284,#34262,#29365,.T.) ;
#43785 = EDGE_CURVE('',#34285,#34265,#29366,.T.) ;
#43786 = EDGE_CURVE('',#34285,#34428,#29367,.T.) ;
#43787 = EDGE_CURVE('',#34282,#34427,#29368,.T.) ;
#43788 = EDGE_CURVE('',#34282,#34278,#29369,.T.) ;
#43789 = EDGE_CURVE('',#34283,#34281,#29370,.T.) ;
#43790 = EDGE_CURVE('',#34308,#34295,#29371,.T.) ;
#43791 = EDGE_CURVE('',#34308,#34496,#29372,.T.) ;
#43792 = EDGE_CURVE('',#34309,#34495,#29373,.T.) ;
#43793 = EDGE_CURVE('',#34309,#34296,#29374,.T.) ;
#43794 = EDGE_CURVE('',#34294,#34307,#29375,.T.) ;
#43795 = EDGE_CURVE('',#34499,#34307,#29376,.T.) ;
#43796 = EDGE_CURVE('',#34500,#34306,#29377,.T.) ;
#43797 = EDGE_CURVE('',#34306,#34297,#29378,.T.) ;
#43798 = EDGE_CURVE('',#34336,#34328,#29379,.T.) ;
#43799 = EDGE_CURVE('',#34337,#34327,#29380,.T.) ;
#43800 = EDGE_CURVE('',#34337,#34416,#29381,.T.) ;
#43801 = EDGE_CURVE('',#34334,#34415,#29382,.T.) ;
#43802 = EDGE_CURVE('',#34334,#34312,#29383,.T.) ;
#43803 = EDGE_CURVE('',#34335,#34311,#29384,.T.) ;
#43804 = EDGE_CURVE('',#34332,#34310,#29385,.T.) ;
#43805 = EDGE_CURVE('',#34333,#34313,#29386,.T.) ;
#43806 = EDGE_CURVE('',#34333,#34420,#29387,.T.) ;
#43807 = EDGE_CURVE('',#34330,#34419,#29388,.T.) ;
#43808 = EDGE_CURVE('',#34330,#34326,#29389,.T.) ;
#43809 = EDGE_CURVE('',#34331,#34329,#29390,.T.) ;
#43810 = EDGE_CURVE('',#34356,#34343,#29391,.T.) ;
#43811 = EDGE_CURVE('',#34356,#34488,#29392,.T.) ;
#43812 = EDGE_CURVE('',#34357,#34487,#29393,.T.) ;
#43813 = EDGE_CURVE('',#34357,#34344,#29394,.T.) ;
#43814 = EDGE_CURVE('',#34342,#34355,#29395,.T.) ;
#43815 = EDGE_CURVE('',#34491,#34355,#29396,.T.) ;
#43816 = EDGE_CURVE('',#34492,#34354,#29397,.T.) ;
#43817 = EDGE_CURVE('',#34354,#34345,#29398,.T.) ;
#43818 = EDGE_CURVE('',#34384,#34376,#29399,.T.) ;
#43819 = EDGE_CURVE('',#34385,#34375,#29400,.T.) ;
#43820 = EDGE_CURVE('',#34385,#34408,#29401,.T.) ;
#43821 = EDGE_CURVE('',#34382,#34407,#29402,.T.) ;
#43822 = EDGE_CURVE('',#34382,#34360,#29403,.T.) ;
#43823 = EDGE_CURVE('',#34383,#34359,#29404,.T.) ;
#43824 = EDGE_CURVE('',#34380,#34358,#29405,.T.) ;
#43825 = EDGE_CURVE('',#34381,#34361,#29406,.T.) ;
#43826 = EDGE_CURVE('',#34381,#34412,#29407,.T.) ;
#43827 = EDGE_CURVE('',#34378,#34411,#29408,.T.) ;
#43828 = EDGE_CURVE('',#34378,#34374,#29409,.T.) ;
#43829 = EDGE_CURVE('',#34379,#34377,#29410,.T.) ;
#43830 = EDGE_CURVE('',#34404,#34391,#29411,.T.) ;
#43831 = EDGE_CURVE('',#34404,#34480,#29412,.T.) ;
#43832 = EDGE_CURVE('',#34405,#34479,#29413,.T.) ;
#43833 = EDGE_CURVE('',#34405,#34392,#29414,.T.) ;
#43834 = EDGE_CURVE('',#34390,#34403,#29415,.T.) ;
#43835 = EDGE_CURVE('',#34483,#34403,#29416,.T.) ;
#43836 = EDGE_CURVE('',#34484,#34402,#29417,.T.) ;
#43837 = EDGE_CURVE('',#34402,#34393,#29418,.T.) ;
#43838 = EDGE_CURVE('',#34550,#34551,#11944,.T.) ;
#43839 = EDGE_CURVE('',#34550,#34552,#330,.T.) ;
#43840 = EDGE_CURVE('',#34552,#34553,#11945,.T.) ;
#43841 = EDGE_CURVE('',#34551,#34553,#331,.F.) ;
#43842 = EDGE_CURVE('',#34554,#34555,#11946,.T.) ;
#43843 = EDGE_CURVE('',#34554,#34550,#332,.T.) ;
#43844 = EDGE_CURVE('',#34555,#34551,#333,.F.) ;
#43845 = EDGE_CURVE('',#34556,#34557,#11947,.T.) ;
#43846 = EDGE_CURVE('',#34556,#34554,#334,.T.) ;
#43847 = EDGE_CURVE('',#34557,#34555,#335,.F.) ;
#43848 = EDGE_CURVE('',#34558,#34559,#11948,.T.) ;
#43849 = EDGE_CURVE('',#34558,#34556,#336,.T.) ;
#43850 = EDGE_CURVE('',#34559,#34557,#337,.F.) ;
#43851 = EDGE_CURVE('',#34560,#34561,#11949,.T.) ;
#43852 = EDGE_CURVE('',#34560,#34558,#338,.T.) ;
#43853 = EDGE_CURVE('',#34561,#34559,#339,.F.) ;
#43854 = EDGE_CURVE('',#34562,#34563,#11950,.T.) ;
#43855 = EDGE_CURVE('',#34562,#34560,#340,.T.) ;
#43856 = EDGE_CURVE('',#34563,#34561,#341,.F.) ;
#43857 = EDGE_CURVE('',#34564,#34565,#11951,.T.) ;
#43858 = EDGE_CURVE('',#34564,#34562,#342,.T.) ;
#43859 = EDGE_CURVE('',#34565,#34563,#343,.F.) ;
#43860 = EDGE_CURVE('',#34566,#34567,#11952,.T.) ;
#43861 = EDGE_CURVE('',#34566,#34564,#344,.T.) ;
#43862 = EDGE_CURVE('',#34567,#34565,#345,.F.) ;
#43863 = EDGE_CURVE('',#34568,#34569,#11953,.T.) ;
#43864 = EDGE_CURVE('',#34568,#34566,#346,.T.) ;
#43865 = EDGE_CURVE('',#34569,#34567,#347,.F.) ;
#43866 = EDGE_CURVE('',#34570,#34571,#11954,.T.) ;
#43867 = EDGE_CURVE('',#34570,#34568,#348,.T.) ;
#43868 = EDGE_CURVE('',#34571,#34569,#349,.F.) ;
#43869 = EDGE_CURVE('',#34572,#34573,#11955,.T.) ;
#43870 = EDGE_CURVE('',#34574,#34572,#350,.F.) ;
#43871 = EDGE_CURVE('',#34574,#34575,#29419,.T.) ;
#43872 = EDGE_CURVE('',#34575,#34573,#351,.T.) ;
#43873 = EDGE_CURVE('',#34576,#34577,#11956,.T.) ;
#43874 = EDGE_CURVE('',#34572,#34576,#352,.F.) ;
#43875 = EDGE_CURVE('',#34573,#34577,#353,.T.) ;
#43876 = EDGE_CURVE('',#34578,#34579,#11957,.T.) ;
#43877 = EDGE_CURVE('',#34576,#34578,#354,.F.) ;
#43878 = EDGE_CURVE('',#34577,#34579,#355,.T.) ;
#43879 = EDGE_CURVE('',#34580,#34581,#11958,.T.) ;
#43880 = EDGE_CURVE('',#34578,#34580,#356,.F.) ;
#43881 = EDGE_CURVE('',#34579,#34581,#357,.T.) ;
#43882 = EDGE_CURVE('',#34582,#34583,#11959,.T.) ;
#43883 = EDGE_CURVE('',#34580,#34582,#358,.F.) ;
#43884 = EDGE_CURVE('',#34581,#34583,#359,.T.) ;
#43885 = EDGE_CURVE('',#34584,#34585,#11960,.T.) ;
#43886 = EDGE_CURVE('',#34582,#34584,#360,.F.) ;
#43887 = EDGE_CURVE('',#34583,#34585,#361,.T.) ;
#43888 = EDGE_CURVE('',#34586,#34587,#11961,.T.) ;
#43889 = EDGE_CURVE('',#34584,#34586,#362,.F.) ;
#43890 = EDGE_CURVE('',#34585,#34587,#363,.T.) ;
#43891 = EDGE_CURVE('',#34588,#34589,#11962,.T.) ;
#43892 = EDGE_CURVE('',#34586,#34588,#364,.F.) ;
#43893 = EDGE_CURVE('',#34587,#34589,#365,.T.) ;
#43894 = EDGE_CURVE('',#34590,#34590,#29420,.T.) ;
#43895 = EDGE_CURVE('',#34590,#34591,#11963,.T.) ;
#43896 = EDGE_CURVE('',#34591,#34592,#366,.T.) ;
#43897 = EDGE_CURVE('',#34592,#34593,#4983,.T.) ;
#43898 = EDGE_CURVE('',#34593,#34594,#11964,.T.) ;
#43899 = EDGE_CURVE('',#34594,#34595,#4984,.T.) ;
#43900 = EDGE_CURVE('',#34596,#34595,#367,.F.) ;
#43901 = EDGE_CURVE('',#34596,#34597,#11965,.T.) ;
#43902 = EDGE_CURVE('',#34597,#34591,#368,.T.) ;
#43903 = EDGE_CURVE('',#34588,#34596,#369,.F.) ;
#43904 = EDGE_CURVE('',#34589,#34597,#370,.T.) ;
#43905 = EDGE_CURVE('',#34598,#34571,#371,.F.) ;
#43906 = EDGE_CURVE('',#34599,#34598,#29421,.T.) ;
#43907 = EDGE_CURVE('',#34599,#34570,#372,.T.) ;
#43908 = EDGE_CURVE('',#34600,#34600,#29422,.T.) ;
#43909 = EDGE_CURVE('',#34600,#34601,#11966,.T.) ;
#43910 = EDGE_CURVE('',#34601,#34601,#29423,.T.) ;
#43911 = EDGE_CURVE('',#34602,#34602,#29424,.T.) ;
#43912 = EDGE_CURVE('',#34602,#34600,#11967,.T.) ;
#43913 = EDGE_CURVE('',#34603,#34602,#11968,.T.) ;
#43914 = EDGE_CURVE('',#34604,#34604,#29425,.T.) ;
#43915 = EDGE_CURVE('',#34604,#34590,#29426,.T.) ;
#43916 = EDGE_CURVE('',#34574,#34605,#373,.F.) ;
#43917 = EDGE_CURVE('',#34605,#34606,#11969,.T.) ;
#43918 = EDGE_CURVE('',#34606,#34606,#29427,.T.) ;
#43919 = EDGE_CURVE('',#34605,#34599,#374,.F.) ;
#43920 = EDGE_CURVE('',#34598,#34575,#375,.T.) ;
#43921 = EDGE_CURVE('',#34607,#34608,#11970,.T.) ;
#43922 = EDGE_CURVE('',#34607,#34609,#29428,.T.) ;
#43923 = EDGE_CURVE('',#34610,#34609,#11971,.T.) ;
#43924 = EDGE_CURVE('',#34610,#34608,#29429,.T.) ;
#43925 = EDGE_CURVE('',#34611,#34612,#11972,.T.) ;
#43926 = EDGE_CURVE('',#34611,#34613,#29430,.T.) ;
#43927 = EDGE_CURVE('',#34614,#34613,#11973,.T.) ;
#43928 = EDGE_CURVE('',#34614,#34612,#29431,.T.) ;
#43929 = EDGE_CURVE('',#34615,#34616,#11974,.T.) ;
#43930 = EDGE_CURVE('',#34615,#34617,#29432,.T.) ;
#43931 = EDGE_CURVE('',#34618,#34617,#11975,.T.) ;
#43932 = EDGE_CURVE('',#34618,#34616,#29433,.T.) ;
#43933 = EDGE_CURVE('',#34619,#34620,#11976,.T.) ;
#43934 = EDGE_CURVE('',#34619,#34621,#29434,.T.) ;
#43935 = EDGE_CURVE('',#34622,#34621,#11977,.T.) ;
#43936 = EDGE_CURVE('',#34622,#34620,#29435,.T.) ;
#43937 = EDGE_CURVE('',#34623,#34624,#11978,.T.) ;
#43938 = EDGE_CURVE('',#34623,#34625,#29436,.T.) ;
#43939 = EDGE_CURVE('',#34626,#34625,#11979,.T.) ;
#43940 = EDGE_CURVE('',#34626,#34624,#29437,.T.) ;
#43941 = EDGE_CURVE('',#34627,#34628,#11980,.T.) ;
#43942 = EDGE_CURVE('',#34627,#34629,#29438,.T.) ;
#43943 = EDGE_CURVE('',#34630,#34629,#11981,.T.) ;
#43944 = EDGE_CURVE('',#34630,#34628,#29439,.T.) ;
#43945 = EDGE_CURVE('',#34611,#34631,#43,.T.) ;
#43946 = EDGE_CURVE('',#34632,#34631,#29440,.T.) ;
#43947 = EDGE_CURVE('',#34632,#34613,#44,.T.) ;
#43948 = EDGE_CURVE('',#34631,#34633,#29441,.T.) ;
#43949 = EDGE_CURVE('',#34631,#34608,#45,.T.) ;
#43950 = EDGE_CURVE('',#34610,#34633,#46,.T.) ;
#43951 = EDGE_CURVE('',#34633,#34634,#29442,.T.) ;
#43952 = EDGE_CURVE('',#34633,#34616,#47,.T.) ;
#43953 = EDGE_CURVE('',#34618,#34634,#48,.T.) ;
#43954 = EDGE_CURVE('',#34634,#34635,#29443,.T.) ;
#43955 = EDGE_CURVE('',#34634,#34620,#49,.T.) ;
#43956 = EDGE_CURVE('',#34622,#34635,#50,.T.) ;
#43957 = EDGE_CURVE('',#34635,#34636,#29444,.T.) ;
#43958 = EDGE_CURVE('',#34635,#34624,#51,.T.) ;
#43959 = EDGE_CURVE('',#34626,#34636,#52,.T.) ;
#43960 = EDGE_CURVE('',#34636,#34632,#29445,.T.) ;
#43961 = EDGE_CURVE('',#34636,#34628,#53,.T.) ;
#43962 = EDGE_CURVE('',#34630,#34632,#54,.T.) ;
#43963 = EDGE_CURVE('',#34607,#34637,#55,.T.) ;
#43964 = EDGE_CURVE('',#34638,#34637,#29446,.T.) ;
#43965 = EDGE_CURVE('',#34638,#34609,#56,.T.) ;
#43966 = EDGE_CURVE('',#34637,#34639,#29447,.T.) ;
#43967 = EDGE_CURVE('',#34637,#34612,#57,.T.) ;
#43968 = EDGE_CURVE('',#34614,#34639,#58,.T.) ;
#43969 = EDGE_CURVE('',#34615,#34638,#59,.T.) ;
#43970 = EDGE_CURVE('',#34640,#34638,#29448,.T.) ;
#43971 = EDGE_CURVE('',#34640,#34617,#60,.T.) ;
#43972 = EDGE_CURVE('',#34619,#34640,#61,.T.) ;
#43973 = EDGE_CURVE('',#34641,#34640,#29449,.T.) ;
#43974 = EDGE_CURVE('',#34641,#34621,#62,.T.) ;
#43975 = EDGE_CURVE('',#34623,#34641,#63,.T.) ;
#43976 = EDGE_CURVE('',#34642,#34641,#29450,.T.) ;
#43977 = EDGE_CURVE('',#34642,#34625,#64,.T.) ;
#43978 = EDGE_CURVE('',#34627,#34642,#65,.T.) ;
#43979 = EDGE_CURVE('',#34639,#34642,#29451,.T.) ;
#43980 = EDGE_CURVE('',#34639,#34629,#66,.T.) ;
#43981 = EDGE_CURVE('',#34595,#34552,#11982,.T.) ;
#43982 = EDGE_CURVE('',#34643,#34553,#29452,.T.) ;
#43983 = EDGE_CURVE('',#34592,#34643,#376,.T.) ;
#43984 = EDGE_CURVE('',#34594,#34552,#11983,.T.) ;
#43985 = EDGE_CURVE('',#34593,#34553,#11984,.T.) ;
#43986 = EDGE_CURVE('',#34644,#34645,#11985,.T.) ;
#43987 = EDGE_CURVE('',#34645,#34646,#29453,.T.) ;
#43988 = EDGE_CURVE('',#34646,#34647,#29454,.T.) ;
#43989 = EDGE_CURVE('',#34647,#34648,#29455,.T.) ;
#43990 = EDGE_CURVE('',#34648,#34649,#29456,.T.) ;
#43991 = EDGE_CURVE('',#34649,#34650,#29457,.T.) ;
#43992 = EDGE_CURVE('',#34650,#34651,#29458,.T.) ;
#43993 = EDGE_CURVE('',#34651,#34652,#29459,.T.) ;
#43994 = EDGE_CURVE('',#34652,#34653,#29460,.T.) ;
#43995 = EDGE_CURVE('',#34653,#34654,#29461,.T.) ;
#43996 = EDGE_CURVE('',#34654,#34655,#29462,.T.) ;
#43997 = EDGE_CURVE('',#34655,#34656,#29463,.T.) ;
#43998 = EDGE_CURVE('',#34656,#34657,#29464,.T.) ;
#43999 = EDGE_CURVE('',#34657,#34658,#29465,.T.) ;
#44000 = EDGE_CURVE('',#34658,#34659,#29466,.T.) ;
#44001 = EDGE_CURVE('',#34659,#34660,#29467,.T.) ;
#44002 = EDGE_CURVE('',#34660,#34661,#29468,.T.) ;
#44003 = EDGE_CURVE('',#34661,#34645,#29469,.T.) ;
#44004 = EDGE_CURVE('',#34653,#34654,#4985,.T.) ;
#44005 = EDGE_CURVE('',#34662,#34662,#29470,.T.) ;
#44006 = EDGE_CURVE('',#34662,#34663,#29471,.T.) ;
#44007 = EDGE_CURVE('',#34663,#34663,#29472,.T.) ;
#44008 = EDGE_CURVE('',#34664,#34664,#29473,.T.) ;
#44009 = EDGE_CURVE('',#34664,#34665,#29474,.T.) ;
#44010 = EDGE_CURVE('',#34665,#34665,#29475,.T.) ;
#44011 = EDGE_CURVE('',#34665,#34666,#11986,.T.) ;
#44012 = EDGE_CURVE('',#34666,#34666,#29476,.T.) ;
#44013 = EDGE_CURVE('',#34663,#34667,#11987,.T.) ;
#44014 = EDGE_CURVE('',#34667,#34667,#29477,.T.) ;
#44015 = EDGE_CURVE('',#34668,#34669,#29478,.T.) ;
#44016 = EDGE_CURVE('',#34670,#34669,#29479,.T.) ;
#44017 = EDGE_CURVE('',#34671,#34670,#29480,.T.) ;
#44018 = EDGE_CURVE('',#34672,#34671,#29481,.T.) ;
#44019 = EDGE_CURVE('',#34672,#34673,#29482,.T.) ;
#44020 = EDGE_CURVE('',#34674,#34673,#29483,.T.) ;
#44021 = EDGE_CURVE('',#34675,#34674,#29484,.T.) ;
#44022 = EDGE_CURVE('',#34676,#34675,#29485,.T.) ;
#44023 = EDGE_CURVE('',#34676,#34677,#29486,.T.) ;
#44024 = EDGE_CURVE('',#34678,#34677,#29487,.T.) ;
#44025 = EDGE_CURVE('',#34679,#34678,#29488,.T.) ;
#44026 = EDGE_CURVE('',#34680,#34679,#29489,.T.) ;
#44027 = EDGE_CURVE('',#34680,#34681,#29490,.T.) ;
#44028 = EDGE_CURVE('',#34682,#34681,#29491,.T.) ;
#44029 = EDGE_CURVE('',#34683,#34682,#29492,.T.) ;
#44030 = EDGE_CURVE('',#34668,#34683,#29493,.T.) ;
#44031 = EDGE_CURVE('',#34683,#34659,#67,.T.) ;
#44032 = EDGE_CURVE('',#34659,#34684,#11988,.T.) ;
#44033 = EDGE_CURVE('',#34668,#34684,#11989,.T.) ;
#44034 = EDGE_CURVE('',#34685,#34648,#11990,.T.) ;
#44035 = EDGE_CURVE('',#34648,#34678,#68,.T.) ;
#44036 = EDGE_CURVE('',#34677,#34685,#11991,.T.) ;
#44037 = EDGE_CURVE('',#34686,#34656,#11992,.T.) ;
#44038 = EDGE_CURVE('',#34656,#34670,#69,.T.) ;
#44039 = EDGE_CURVE('',#34669,#34686,#11993,.T.) ;
#44040 = EDGE_CURVE('',#34675,#34651,#70,.T.) ;
#44041 = EDGE_CURVE('',#34651,#34687,#11994,.T.) ;
#44042 = EDGE_CURVE('',#34676,#34687,#11995,.T.) ;
#44043 = EDGE_CURVE('',#34657,#34658,#4986,.T.) ;
#44044 = EDGE_CURVE('',#34686,#34657,#11996,.T.) ;
#44045 = EDGE_CURVE('',#34658,#34684,#11997,.T.) ;
#44046 = EDGE_CURVE('',#34649,#34650,#4987,.T.) ;
#44047 = EDGE_CURVE('',#34685,#34649,#11998,.T.) ;
#44048 = EDGE_CURVE('',#34650,#34687,#11999,.T.) ;
#44049 = EDGE_CURVE('',#34688,#34653,#12000,.T.) ;
#44050 = EDGE_CURVE('',#34688,#34652,#12001,.T.) ;
#44051 = EDGE_CURVE('',#34647,#34689,#12002,.T.) ;
#44052 = EDGE_CURVE('',#34646,#34689,#12003,.T.) ;
#44053 = EDGE_CURVE('',#34690,#34661,#12004,.T.) ;
#44054 = EDGE_CURVE('',#34690,#34660,#12005,.T.) ;
#44055 = EDGE_CURVE('',#34671,#34655,#71,.T.) ;
#44056 = EDGE_CURVE('',#34655,#34691,#12006,.T.) ;
#44057 = EDGE_CURVE('',#34672,#34691,#12007,.T.) ;
#44058 = EDGE_CURVE('',#34652,#34674,#72,.T.) ;
#44059 = EDGE_CURVE('',#34673,#34688,#12008,.T.) ;
#44060 = EDGE_CURVE('',#34654,#34691,#12009,.T.) ;
#44061 = EDGE_CURVE('',#34661,#34646,#4988,.T.) ;
#44062 = EDGE_CURVE('',#34681,#34690,#12010,.T.) ;
#44063 = EDGE_CURVE('',#34680,#34689,#12011,.T.) ;
#44064 = EDGE_CURVE('',#34660,#34682,#73,.T.) ;
#44065 = EDGE_CURVE('',#34679,#34647,#74,.T.) ;
#44066 = ORIENTED_EDGE('',*,*,#34692,.F.) ;
#44067 = ORIENTED_EDGE('',*,*,#34693,.F.) ;
#44068 = ORIENTED_EDGE('',*,*,#34694,.T.) ;
#44069 = ORIENTED_EDGE('',*,*,#34695,.F.) ;
#44070 = ORIENTED_EDGE('',*,*,#34694,.F.) ;
#44071 = ORIENTED_EDGE('',*,*,#34696,.F.) ;
#44072 = ORIENTED_EDGE('',*,*,#34697,.T.) ;
#44073 = ORIENTED_EDGE('',*,*,#34698,.F.) ;
#44074 = ORIENTED_EDGE('',*,*,#34699,.F.) ;
#44075 = ORIENTED_EDGE('',*,*,#34697,.F.) ;
#44076 = ORIENTED_EDGE('',*,*,#34700,.F.) ;
#44077 = ORIENTED_EDGE('',*,*,#34701,.F.) ;
#44078 = ORIENTED_EDGE('',*,*,#34702,.T.) ;
#44079 = ORIENTED_EDGE('',*,*,#34703,.F.) ;
#44080 = ORIENTED_EDGE('',*,*,#34704,.F.) ;
#44081 = ORIENTED_EDGE('',*,*,#34702,.F.) ;
#44082 = ORIENTED_EDGE('',*,*,#34705,.F.) ;
#44083 = ORIENTED_EDGE('',*,*,#34706,.T.) ;
#44084 = ORIENTED_EDGE('',*,*,#34707,.F.) ;
#44085 = ORIENTED_EDGE('',*,*,#34706,.F.) ;
#44086 = ORIENTED_EDGE('',*,*,#34708,.F.) ;
#44087 = ORIENTED_EDGE('',*,*,#34709,.F.) ;
#44088 = ORIENTED_EDGE('',*,*,#34710,.T.) ;
#44089 = ORIENTED_EDGE('',*,*,#34711,.F.) ;
#44090 = ORIENTED_EDGE('',*,*,#34712,.F.) ;
#44091 = ORIENTED_EDGE('',*,*,#34710,.F.) ;
#44092 = ORIENTED_EDGE('',*,*,#34713,.F.) ;
#44093 = ORIENTED_EDGE('',*,*,#34714,.T.) ;
#44094 = ORIENTED_EDGE('',*,*,#34715,.F.) ;
#44095 = ORIENTED_EDGE('',*,*,#34714,.F.) ;
#44096 = ORIENTED_EDGE('',*,*,#34708,.T.) ;
#44097 = ORIENTED_EDGE('',*,*,#34709,.T.) ;
#44098 = ORIENTED_EDGE('',*,*,#34716,.T.) ;
#44099 = ORIENTED_EDGE('',*,*,#34717,.T.) ;
#44100 = ORIENTED_EDGE('',*,*,#34716,.F.) ;
#44101 = ORIENTED_EDGE('',*,*,#34715,.T.) ;
#44102 = ORIENTED_EDGE('',*,*,#34718,.T.) ;
#44103 = ORIENTED_EDGE('',*,*,#34711,.T.) ;
#44104 = ORIENTED_EDGE('',*,*,#34712,.T.) ;
#44105 = ORIENTED_EDGE('',*,*,#34718,.F.) ;
#44106 = ORIENTED_EDGE('',*,*,#34700,.T.) ;
#44107 = ORIENTED_EDGE('',*,*,#34701,.T.) ;
#44108 = ORIENTED_EDGE('',*,*,#34719,.T.) ;
#44109 = ORIENTED_EDGE('',*,*,#34720,.T.) ;
#44110 = ORIENTED_EDGE('',*,*,#34719,.F.) ;
#44111 = ORIENTED_EDGE('',*,*,#34707,.T.) ;
#44112 = ORIENTED_EDGE('',*,*,#34721,.T.) ;
#44113 = ORIENTED_EDGE('',*,*,#34703,.T.) ;
#44114 = ORIENTED_EDGE('',*,*,#34704,.T.) ;
#44115 = ORIENTED_EDGE('',*,*,#34721,.F.) ;
#44116 = ORIENTED_EDGE('',*,*,#34692,.T.) ;
#44117 = ORIENTED_EDGE('',*,*,#34693,.T.) ;
#44118 = ORIENTED_EDGE('',*,*,#34722,.T.) ;
#44119 = ORIENTED_EDGE('',*,*,#34698,.T.) ;
#44120 = ORIENTED_EDGE('',*,*,#34699,.T.) ;
#44121 = ORIENTED_EDGE('',*,*,#34722,.F.) ;
#44122 = ORIENTED_EDGE('',*,*,#34723,.T.) ;
#44123 = ORIENTED_EDGE('',*,*,#34724,.T.) ;
#44124 = ORIENTED_EDGE('',*,*,#34725,.T.) ;
#44125 = ORIENTED_EDGE('',*,*,#34726,.T.) ;
#44126 = ORIENTED_EDGE('',*,*,#34727,.F.) ;
#44127 = ORIENTED_EDGE('',*,*,#34728,.F.) ;
#44128 = ORIENTED_EDGE('',*,*,#34729,.F.) ;
#44129 = ORIENTED_EDGE('',*,*,#34730,.T.) ;
#44130 = ORIENTED_EDGE('',*,*,#34731,.F.) ;
#44131 = ORIENTED_EDGE('',*,*,#34732,.T.) ;
#44132 = ORIENTED_EDGE('',*,*,#34733,.F.) ;
#44133 = ORIENTED_EDGE('',*,*,#34734,.T.) ;
#44134 = ORIENTED_EDGE('',*,*,#34735,.F.) ;
#44135 = ORIENTED_EDGE('',*,*,#34736,.T.) ;
#44136 = ORIENTED_EDGE('',*,*,#34696,.T.) ;
#44137 = ORIENTED_EDGE('',*,*,#34737,.T.) ;
#44138 = ORIENTED_EDGE('',*,*,#34738,.T.) ;
#44139 = ORIENTED_EDGE('',*,*,#34739,.F.) ;
#44140 = ORIENTED_EDGE('',*,*,#34740,.F.) ;
#44141 = ORIENTED_EDGE('',*,*,#34741,.T.) ;
#44142 = ORIENTED_EDGE('',*,*,#34742,.T.) ;
#44143 = ORIENTED_EDGE('',*,*,#34743,.F.) ;
#44144 = ORIENTED_EDGE('',*,*,#34744,.T.) ;
#44145 = ORIENTED_EDGE('',*,*,#34745,.F.) ;
#44146 = ORIENTED_EDGE('',*,*,#34746,.T.) ;
#44147 = ORIENTED_EDGE('',*,*,#34747,.F.) ;
#44148 = ORIENTED_EDGE('',*,*,#34748,.T.) ;
#44149 = ORIENTED_EDGE('',*,*,#34749,.F.) ;
#44150 = ORIENTED_EDGE('',*,*,#34750,.T.) ;
#44151 = ORIENTED_EDGE('',*,*,#34695,.T.) ;
#44152 = ORIENTED_EDGE('',*,*,#34751,.F.) ;
#44153 = ORIENTED_EDGE('',*,*,#34752,.T.) ;
#44154 = ORIENTED_EDGE('',*,*,#34753,.F.) ;
#44155 = ORIENTED_EDGE('',*,*,#34754,.F.) ;
#44156 = ORIENTED_EDGE('',*,*,#34755,.T.) ;
#44157 = ORIENTED_EDGE('',*,*,#34756,.T.) ;
#44158 = ORIENTED_EDGE('',*,*,#34757,.T.) ;
#44159 = ORIENTED_EDGE('',*,*,#34758,.F.) ;
#44160 = ORIENTED_EDGE('',*,*,#34759,.T.) ;
#44161 = ORIENTED_EDGE('',*,*,#34760,.T.) ;
#44162 = ORIENTED_EDGE('',*,*,#34761,.T.) ;
#44163 = ORIENTED_EDGE('',*,*,#34762,.F.) ;
#44164 = ORIENTED_EDGE('',*,*,#34763,.T.) ;
#44165 = ORIENTED_EDGE('',*,*,#34764,.F.) ;
#44166 = ORIENTED_EDGE('',*,*,#34765,.T.) ;
#44167 = ORIENTED_EDGE('',*,*,#34766,.F.) ;
#44168 = ORIENTED_EDGE('',*,*,#34767,.T.) ;
#44169 = ORIENTED_EDGE('',*,*,#34768,.F.) ;
#44170 = ORIENTED_EDGE('',*,*,#34769,.T.) ;
#44171 = ORIENTED_EDGE('',*,*,#34770,.F.) ;
#44172 = ORIENTED_EDGE('',*,*,#34771,.T.) ;
#44173 = ORIENTED_EDGE('',*,*,#34772,.F.) ;
#44174 = ORIENTED_EDGE('',*,*,#34773,.T.) ;
#44175 = ORIENTED_EDGE('',*,*,#34774,.F.) ;
#44176 = ORIENTED_EDGE('',*,*,#34775,.T.) ;
#44177 = ORIENTED_EDGE('',*,*,#34776,.F.) ;
#44178 = ORIENTED_EDGE('',*,*,#34777,.T.) ;
#44179 = ORIENTED_EDGE('',*,*,#34778,.F.) ;
#44180 = ORIENTED_EDGE('',*,*,#34779,.T.) ;
#44181 = ORIENTED_EDGE('',*,*,#34780,.F.) ;
#44182 = ORIENTED_EDGE('',*,*,#34781,.T.) ;
#44183 = ORIENTED_EDGE('',*,*,#34782,.F.) ;
#44184 = ORIENTED_EDGE('',*,*,#34783,.T.) ;
#44185 = ORIENTED_EDGE('',*,*,#34784,.F.) ;
#44186 = ORIENTED_EDGE('',*,*,#34785,.T.) ;
#44187 = ORIENTED_EDGE('',*,*,#34786,.F.) ;
#44188 = ORIENTED_EDGE('',*,*,#34787,.T.) ;
#44189 = ORIENTED_EDGE('',*,*,#34788,.F.) ;
#44190 = ORIENTED_EDGE('',*,*,#34789,.T.) ;
#44191 = ORIENTED_EDGE('',*,*,#34790,.F.) ;
#44192 = ORIENTED_EDGE('',*,*,#34791,.T.) ;
#44193 = ORIENTED_EDGE('',*,*,#34792,.F.) ;
#44194 = ORIENTED_EDGE('',*,*,#34793,.T.) ;
#44195 = ORIENTED_EDGE('',*,*,#34794,.T.) ;
#44196 = ORIENTED_EDGE('',*,*,#34795,.T.) ;
#44197 = ORIENTED_EDGE('',*,*,#34796,.F.) ;
#44198 = ORIENTED_EDGE('',*,*,#34797,.T.) ;
#44199 = ORIENTED_EDGE('',*,*,#34798,.T.) ;
#44200 = ORIENTED_EDGE('',*,*,#34799,.T.) ;
#44201 = ORIENTED_EDGE('',*,*,#34800,.F.) ;
#44202 = ORIENTED_EDGE('',*,*,#34801,.T.) ;
#44203 = ORIENTED_EDGE('',*,*,#34802,.T.) ;
#44204 = ORIENTED_EDGE('',*,*,#34803,.T.) ;
#44205 = ORIENTED_EDGE('',*,*,#34804,.T.) ;
#44206 = ORIENTED_EDGE('',*,*,#34805,.F.) ;
#44207 = ORIENTED_EDGE('',*,*,#34806,.T.) ;
#44208 = ORIENTED_EDGE('',*,*,#34807,.F.) ;
#44209 = ORIENTED_EDGE('',*,*,#34808,.T.) ;
#44210 = ORIENTED_EDGE('',*,*,#34809,.F.) ;
#44211 = ORIENTED_EDGE('',*,*,#34810,.T.) ;
#44212 = ORIENTED_EDGE('',*,*,#34811,.F.) ;
#44213 = ORIENTED_EDGE('',*,*,#34812,.T.) ;
#44214 = ORIENTED_EDGE('',*,*,#34813,.F.) ;
#44215 = ORIENTED_EDGE('',*,*,#34814,.T.) ;
#44216 = ORIENTED_EDGE('',*,*,#34815,.F.) ;
#44217 = ORIENTED_EDGE('',*,*,#34816,.T.) ;
#44218 = ORIENTED_EDGE('',*,*,#34817,.F.) ;
#44219 = ORIENTED_EDGE('',*,*,#34818,.T.) ;
#44220 = ORIENTED_EDGE('',*,*,#34819,.F.) ;
#44221 = ORIENTED_EDGE('',*,*,#34820,.T.) ;
#44222 = ORIENTED_EDGE('',*,*,#34821,.F.) ;
#44223 = ORIENTED_EDGE('',*,*,#34822,.T.) ;
#44224 = ORIENTED_EDGE('',*,*,#34823,.F.) ;
#44225 = ORIENTED_EDGE('',*,*,#34824,.T.) ;
#44226 = ORIENTED_EDGE('',*,*,#34825,.F.) ;
#44227 = ORIENTED_EDGE('',*,*,#34826,.T.) ;
#44228 = ORIENTED_EDGE('',*,*,#34827,.F.) ;
#44229 = ORIENTED_EDGE('',*,*,#34828,.T.) ;
#44230 = ORIENTED_EDGE('',*,*,#34829,.F.) ;
#44231 = ORIENTED_EDGE('',*,*,#34830,.T.) ;
#44232 = ORIENTED_EDGE('',*,*,#34831,.F.) ;
#44233 = ORIENTED_EDGE('',*,*,#34832,.T.) ;
#44234 = ORIENTED_EDGE('',*,*,#34833,.F.) ;
#44235 = ORIENTED_EDGE('',*,*,#34834,.T.) ;
#44236 = ORIENTED_EDGE('',*,*,#34835,.F.) ;
#44237 = ORIENTED_EDGE('',*,*,#34836,.T.) ;
#44238 = ORIENTED_EDGE('',*,*,#34837,.T.) ;
#44239 = ORIENTED_EDGE('',*,*,#34838,.T.) ;
#44240 = ORIENTED_EDGE('',*,*,#34839,.F.) ;
#44241 = ORIENTED_EDGE('',*,*,#34840,.T.) ;
#44242 = ORIENTED_EDGE('',*,*,#34841,.T.) ;
#44243 = ORIENTED_EDGE('',*,*,#34842,.T.) ;
#44244 = ORIENTED_EDGE('',*,*,#34843,.F.) ;
#44245 = ORIENTED_EDGE('',*,*,#34844,.T.) ;
#44246 = ORIENTED_EDGE('',*,*,#34845,.T.) ;
#44247 = ORIENTED_EDGE('',*,*,#34846,.T.) ;
#44248 = ORIENTED_EDGE('',*,*,#34847,.T.) ;
#44249 = ORIENTED_EDGE('',*,*,#34848,.F.) ;
#44250 = ORIENTED_EDGE('',*,*,#34849,.T.) ;
#44251 = ORIENTED_EDGE('',*,*,#34850,.F.) ;
#44252 = ORIENTED_EDGE('',*,*,#34851,.T.) ;
#44253 = ORIENTED_EDGE('',*,*,#34852,.F.) ;
#44254 = ORIENTED_EDGE('',*,*,#34853,.T.) ;
#44255 = ORIENTED_EDGE('',*,*,#34854,.F.) ;
#44256 = ORIENTED_EDGE('',*,*,#34855,.T.) ;
#44257 = ORIENTED_EDGE('',*,*,#34856,.F.) ;
#44258 = ORIENTED_EDGE('',*,*,#34857,.T.) ;
#44259 = ORIENTED_EDGE('',*,*,#34858,.F.) ;
#44260 = ORIENTED_EDGE('',*,*,#34859,.T.) ;
#44261 = ORIENTED_EDGE('',*,*,#34860,.F.) ;
#44262 = ORIENTED_EDGE('',*,*,#34861,.T.) ;
#44263 = ORIENTED_EDGE('',*,*,#34862,.F.) ;
#44264 = ORIENTED_EDGE('',*,*,#34863,.T.) ;
#44265 = ORIENTED_EDGE('',*,*,#34864,.F.) ;
#44266 = ORIENTED_EDGE('',*,*,#34865,.T.) ;
#44267 = ORIENTED_EDGE('',*,*,#34866,.F.) ;
#44268 = ORIENTED_EDGE('',*,*,#34867,.T.) ;
#44269 = ORIENTED_EDGE('',*,*,#34868,.F.) ;
#44270 = ORIENTED_EDGE('',*,*,#34869,.T.) ;
#44271 = ORIENTED_EDGE('',*,*,#34870,.F.) ;
#44272 = ORIENTED_EDGE('',*,*,#34871,.T.) ;
#44273 = ORIENTED_EDGE('',*,*,#34872,.F.) ;
#44274 = ORIENTED_EDGE('',*,*,#34873,.T.) ;
#44275 = ORIENTED_EDGE('',*,*,#34874,.F.) ;
#44276 = ORIENTED_EDGE('',*,*,#34875,.T.) ;
#44277 = ORIENTED_EDGE('',*,*,#34876,.F.) ;
#44278 = ORIENTED_EDGE('',*,*,#34877,.T.) ;
#44279 = ORIENTED_EDGE('',*,*,#34878,.F.) ;
#44280 = ORIENTED_EDGE('',*,*,#34879,.T.) ;
#44281 = ORIENTED_EDGE('',*,*,#34880,.F.) ;
#44282 = ORIENTED_EDGE('',*,*,#34881,.T.) ;
#44283 = ORIENTED_EDGE('',*,*,#34882,.F.) ;
#44284 = ORIENTED_EDGE('',*,*,#34883,.T.) ;
#44285 = ORIENTED_EDGE('',*,*,#34884,.F.) ;
#44286 = ORIENTED_EDGE('',*,*,#34885,.T.) ;
#44287 = ORIENTED_EDGE('',*,*,#34886,.F.) ;
#44288 = ORIENTED_EDGE('',*,*,#34887,.T.) ;
#44289 = ORIENTED_EDGE('',*,*,#34888,.F.) ;
#44290 = ORIENTED_EDGE('',*,*,#34889,.T.) ;
#44291 = ORIENTED_EDGE('',*,*,#34890,.F.) ;
#44292 = ORIENTED_EDGE('',*,*,#34891,.T.) ;
#44293 = ORIENTED_EDGE('',*,*,#34892,.F.) ;
#44294 = ORIENTED_EDGE('',*,*,#34893,.T.) ;
#44295 = ORIENTED_EDGE('',*,*,#34894,.F.) ;
#44296 = ORIENTED_EDGE('',*,*,#34895,.T.) ;
#44297 = ORIENTED_EDGE('',*,*,#34896,.F.) ;
#44298 = ORIENTED_EDGE('',*,*,#34897,.T.) ;
#44299 = ORIENTED_EDGE('',*,*,#34898,.F.) ;
#44300 = ORIENTED_EDGE('',*,*,#34899,.T.) ;
#44301 = ORIENTED_EDGE('',*,*,#34900,.F.) ;
#44302 = ORIENTED_EDGE('',*,*,#34901,.T.) ;
#44303 = ORIENTED_EDGE('',*,*,#34902,.F.) ;
#44304 = ORIENTED_EDGE('',*,*,#34903,.T.) ;
#44305 = ORIENTED_EDGE('',*,*,#34904,.F.) ;
#44306 = ORIENTED_EDGE('',*,*,#34905,.T.) ;
#44307 = ORIENTED_EDGE('',*,*,#34906,.F.) ;
#44308 = ORIENTED_EDGE('',*,*,#34907,.F.) ;
#44309 = ORIENTED_EDGE('',*,*,#34908,.T.) ;
#44310 = ORIENTED_EDGE('',*,*,#34909,.T.) ;
#44311 = ORIENTED_EDGE('',*,*,#34910,.T.) ;
#44312 = ORIENTED_EDGE('',*,*,#34911,.F.) ;
#44313 = ORIENTED_EDGE('',*,*,#34912,.T.) ;
#44314 = ORIENTED_EDGE('',*,*,#34913,.T.) ;
#44315 = ORIENTED_EDGE('',*,*,#34914,.T.) ;
#44316 = ORIENTED_EDGE('',*,*,#34915,.F.) ;
#44317 = ORIENTED_EDGE('',*,*,#34916,.T.) ;
#44318 = ORIENTED_EDGE('',*,*,#34917,.F.) ;
#44319 = ORIENTED_EDGE('',*,*,#34918,.T.) ;
#44320 = ORIENTED_EDGE('',*,*,#34919,.F.) ;
#44321 = ORIENTED_EDGE('',*,*,#34920,.T.) ;
#44322 = ORIENTED_EDGE('',*,*,#34921,.F.) ;
#44323 = ORIENTED_EDGE('',*,*,#34922,.T.) ;
#44324 = ORIENTED_EDGE('',*,*,#34923,.F.) ;
#44325 = ORIENTED_EDGE('',*,*,#34924,.T.) ;
#44326 = ORIENTED_EDGE('',*,*,#34925,.F.) ;
#44327 = ORIENTED_EDGE('',*,*,#34926,.T.) ;
#44328 = ORIENTED_EDGE('',*,*,#34927,.F.) ;
#44329 = ORIENTED_EDGE('',*,*,#34928,.T.) ;
#44330 = ORIENTED_EDGE('',*,*,#34929,.F.) ;
#44331 = ORIENTED_EDGE('',*,*,#34930,.T.) ;
#44332 = ORIENTED_EDGE('',*,*,#34931,.F.) ;
#44333 = ORIENTED_EDGE('',*,*,#34932,.T.) ;
#44334 = ORIENTED_EDGE('',*,*,#34933,.F.) ;
#44335 = ORIENTED_EDGE('',*,*,#34934,.T.) ;
#44336 = ORIENTED_EDGE('',*,*,#34935,.F.) ;
#44337 = ORIENTED_EDGE('',*,*,#34936,.T.) ;
#44338 = ORIENTED_EDGE('',*,*,#34937,.F.) ;
#44339 = ORIENTED_EDGE('',*,*,#34938,.T.) ;
#44340 = ORIENTED_EDGE('',*,*,#34939,.F.) ;
#44341 = ORIENTED_EDGE('',*,*,#34940,.T.) ;
#44342 = ORIENTED_EDGE('',*,*,#34941,.F.) ;
#44343 = ORIENTED_EDGE('',*,*,#34942,.T.) ;
#44344 = ORIENTED_EDGE('',*,*,#34943,.F.) ;
#44345 = ORIENTED_EDGE('',*,*,#34944,.T.) ;
#44346 = ORIENTED_EDGE('',*,*,#34945,.F.) ;
#44347 = ORIENTED_EDGE('',*,*,#34946,.T.) ;
#44348 = ORIENTED_EDGE('',*,*,#34947,.F.) ;
#44349 = ORIENTED_EDGE('',*,*,#34948,.T.) ;
#44350 = ORIENTED_EDGE('',*,*,#34949,.F.) ;
#44351 = ORIENTED_EDGE('',*,*,#34950,.T.) ;
#44352 = ORIENTED_EDGE('',*,*,#34951,.F.) ;
#44353 = ORIENTED_EDGE('',*,*,#34952,.T.) ;
#44354 = ORIENTED_EDGE('',*,*,#34953,.F.) ;
#44355 = ORIENTED_EDGE('',*,*,#34954,.T.) ;
#44356 = ORIENTED_EDGE('',*,*,#34955,.F.) ;
#44357 = ORIENTED_EDGE('',*,*,#34956,.T.) ;
#44358 = ORIENTED_EDGE('',*,*,#34957,.F.) ;
#44359 = ORIENTED_EDGE('',*,*,#34958,.T.) ;
#44360 = ORIENTED_EDGE('',*,*,#34959,.F.) ;
#44361 = ORIENTED_EDGE('',*,*,#34960,.T.) ;
#44362 = ORIENTED_EDGE('',*,*,#34961,.F.) ;
#44363 = ORIENTED_EDGE('',*,*,#34962,.T.) ;
#44364 = ORIENTED_EDGE('',*,*,#34963,.F.) ;
#44365 = ORIENTED_EDGE('',*,*,#34964,.T.) ;
#44366 = ORIENTED_EDGE('',*,*,#34965,.F.) ;
#44367 = ORIENTED_EDGE('',*,*,#34966,.T.) ;
#44368 = ORIENTED_EDGE('',*,*,#34967,.F.) ;
#44369 = ORIENTED_EDGE('',*,*,#34968,.T.) ;
#44370 = ORIENTED_EDGE('',*,*,#34969,.F.) ;
#44371 = ORIENTED_EDGE('',*,*,#34970,.T.) ;
#44372 = ORIENTED_EDGE('',*,*,#34971,.F.) ;
#44373 = ORIENTED_EDGE('',*,*,#34972,.T.) ;
#44374 = ORIENTED_EDGE('',*,*,#34973,.F.) ;
#44375 = ORIENTED_EDGE('',*,*,#34974,.T.) ;
#44376 = ORIENTED_EDGE('',*,*,#34975,.T.) ;
#44377 = ORIENTED_EDGE('',*,*,#34976,.T.) ;
#44378 = ORIENTED_EDGE('',*,*,#34977,.F.) ;
#44379 = ORIENTED_EDGE('',*,*,#34978,.T.) ;
#44380 = ORIENTED_EDGE('',*,*,#34979,.T.) ;
#44381 = ORIENTED_EDGE('',*,*,#34980,.T.) ;
#44382 = ORIENTED_EDGE('',*,*,#34717,.F.) ;
#44383 = ORIENTED_EDGE('',*,*,#34720,.F.) ;
#44384 = ORIENTED_EDGE('',*,*,#34981,.T.) ;
#44385 = ORIENTED_EDGE('',*,*,#34982,.T.) ;
#44386 = ORIENTED_EDGE('',*,*,#34983,.F.) ;
#44387 = ORIENTED_EDGE('',*,*,#34984,.T.) ;
#44388 = ORIENTED_EDGE('',*,*,#34985,.T.) ;
#44389 = ORIENTED_EDGE('',*,*,#34986,.T.) ;
#44390 = ORIENTED_EDGE('',*,*,#34987,.F.) ;
#44391 = ORIENTED_EDGE('',*,*,#34988,.T.) ;
#44392 = ORIENTED_EDGE('',*,*,#34989,.F.) ;
#44393 = ORIENTED_EDGE('',*,*,#34990,.F.) ;
#44394 = ORIENTED_EDGE('',*,*,#34713,.T.) ;
#44395 = ORIENTED_EDGE('',*,*,#34705,.T.) ;
#44396 = ORIENTED_EDGE('',*,*,#34991,.T.) ;
#44397 = ORIENTED_EDGE('',*,*,#34992,.T.) ;
#44398 = ORIENTED_EDGE('',*,*,#34993,.T.) ;
#44399 = ORIENTED_EDGE('',*,*,#34994,.T.) ;
#44400 = ORIENTED_EDGE('',*,*,#34995,.T.) ;
#44401 = ORIENTED_EDGE('',*,*,#34996,.T.) ;
#44402 = ORIENTED_EDGE('',*,*,#34997,.T.) ;
#44403 = ORIENTED_EDGE('',*,*,#34998,.T.) ;
#44404 = ORIENTED_EDGE('',*,*,#34999,.T.) ;
#44405 = ORIENTED_EDGE('',*,*,#35000,.T.) ;
#44406 = ORIENTED_EDGE('',*,*,#35001,.T.) ;
#44407 = ORIENTED_EDGE('',*,*,#35002,.T.) ;
#44408 = ORIENTED_EDGE('',*,*,#35003,.T.) ;
#44409 = ORIENTED_EDGE('',*,*,#35004,.T.) ;
#44410 = ORIENTED_EDGE('',*,*,#35005,.T.) ;
#44411 = ORIENTED_EDGE('',*,*,#35006,.T.) ;
#44412 = ORIENTED_EDGE('',*,*,#35007,.T.) ;
#44413 = ORIENTED_EDGE('',*,*,#35008,.T.) ;
#44414 = ORIENTED_EDGE('',*,*,#35009,.T.) ;
#44415 = ORIENTED_EDGE('',*,*,#35010,.T.) ;
#44416 = ORIENTED_EDGE('',*,*,#34997,.F.) ;
#44417 = ORIENTED_EDGE('',*,*,#35011,.T.) ;
#44418 = ORIENTED_EDGE('',*,*,#35012,.F.) ;
#44419 = ORIENTED_EDGE('',*,*,#35013,.T.) ;
#44420 = ORIENTED_EDGE('',*,*,#35014,.T.) ;
#44421 = ORIENTED_EDGE('',*,*,#35015,.T.) ;
#44422 = ORIENTED_EDGE('',*,*,#35016,.F.) ;
#44423 = ORIENTED_EDGE('',*,*,#35017,.T.) ;
#44424 = ORIENTED_EDGE('',*,*,#34973,.T.) ;
#44425 = ORIENTED_EDGE('',*,*,#35018,.T.) ;
#44426 = ORIENTED_EDGE('',*,*,#34837,.F.) ;
#44427 = ORIENTED_EDGE('',*,*,#35016,.T.) ;
#44428 = ORIENTED_EDGE('',*,*,#34906,.T.) ;
#44429 = ORIENTED_EDGE('',*,*,#35019,.T.) ;
#44430 = ORIENTED_EDGE('',*,*,#34981,.F.) ;
#44431 = ORIENTED_EDGE('',*,*,#35014,.F.) ;
#44432 = ORIENTED_EDGE('',*,*,#35020,.T.) ;
#44433 = ORIENTED_EDGE('',*,*,#35021,.T.) ;
#44434 = ORIENTED_EDGE('',*,*,#35022,.T.) ;
#44435 = ORIENTED_EDGE('',*,*,#35023,.T.) ;
#44436 = ORIENTED_EDGE('',*,*,#35024,.T.) ;
#44437 = ORIENTED_EDGE('',*,*,#35025,.T.) ;
#44438 = ORIENTED_EDGE('',*,*,#35026,.T.) ;
#44439 = ORIENTED_EDGE('',*,*,#35027,.T.) ;
#44440 = ORIENTED_EDGE('',*,*,#35028,.T.) ;
#44441 = ORIENTED_EDGE('',*,*,#35029,.T.) ;
#44442 = ORIENTED_EDGE('',*,*,#35030,.T.) ;
#44443 = ORIENTED_EDGE('',*,*,#35031,.T.) ;
#44444 = ORIENTED_EDGE('',*,*,#35032,.T.) ;
#44445 = ORIENTED_EDGE('',*,*,#35033,.T.) ;
#44446 = ORIENTED_EDGE('',*,*,#35034,.T.) ;
#44447 = ORIENTED_EDGE('',*,*,#35035,.T.) ;
#44448 = ORIENTED_EDGE('',*,*,#35036,.T.) ;
#44449 = ORIENTED_EDGE('',*,*,#35037,.T.) ;
#44450 = ORIENTED_EDGE('',*,*,#35038,.T.) ;
#44451 = ORIENTED_EDGE('',*,*,#35039,.T.) ;
#44452 = ORIENTED_EDGE('',*,*,#35040,.T.) ;
#44453 = ORIENTED_EDGE('',*,*,#35041,.T.) ;
#44454 = ORIENTED_EDGE('',*,*,#35042,.T.) ;
#44455 = ORIENTED_EDGE('',*,*,#35043,.T.) ;
#44456 = ORIENTED_EDGE('',*,*,#35012,.T.) ;
#44457 = ORIENTED_EDGE('',*,*,#35044,.T.) ;
#44458 = ORIENTED_EDGE('',*,*,#35045,.T.) ;
#44459 = ORIENTED_EDGE('',*,*,#35046,.T.) ;
#44460 = ORIENTED_EDGE('',*,*,#34847,.F.) ;
#44461 = ORIENTED_EDGE('',*,*,#35047,.T.) ;
#44462 = ORIENTED_EDGE('',*,*,#34907,.T.) ;
#44463 = ORIENTED_EDGE('',*,*,#35017,.F.) ;
#44464 = ORIENTED_EDGE('',*,*,#35048,.T.) ;
#44465 = ORIENTED_EDGE('',*,*,#35049,.T.) ;
#44466 = ORIENTED_EDGE('',*,*,#35050,.T.) ;
#44467 = ORIENTED_EDGE('',*,*,#35051,.T.) ;
#44468 = ORIENTED_EDGE('',*,*,#35052,.T.) ;
#44469 = ORIENTED_EDGE('',*,*,#35053,.T.) ;
#44470 = ORIENTED_EDGE('',*,*,#35054,.T.) ;
#44471 = ORIENTED_EDGE('',*,*,#35055,.T.) ;
#44472 = ORIENTED_EDGE('',*,*,#35056,.T.) ;
#44473 = ORIENTED_EDGE('',*,*,#35057,.T.) ;
#44474 = ORIENTED_EDGE('',*,*,#35058,.T.) ;
#44475 = ORIENTED_EDGE('',*,*,#35059,.T.) ;
#44476 = ORIENTED_EDGE('',*,*,#34739,.T.) ;
#44477 = ORIENTED_EDGE('',*,*,#35060,.T.) ;
#44478 = ORIENTED_EDGE('',*,*,#34723,.F.) ;
#44479 = ORIENTED_EDGE('',*,*,#35061,.F.) ;
#44480 = ORIENTED_EDGE('',*,*,#34727,.T.) ;
#44481 = ORIENTED_EDGE('',*,*,#35062,.T.) ;
#44482 = ORIENTED_EDGE('',*,*,#34741,.F.) ;
#44483 = ORIENTED_EDGE('',*,*,#35063,.T.) ;
#44484 = ORIENTED_EDGE('',*,*,#35063,.F.) ;
#44485 = ORIENTED_EDGE('',*,*,#35064,.T.) ;
#44486 = ORIENTED_EDGE('',*,*,#35065,.T.) ;
#44487 = ORIENTED_EDGE('',*,*,#35066,.F.) ;
#44488 = ORIENTED_EDGE('',*,*,#35067,.T.) ;
#44489 = ORIENTED_EDGE('',*,*,#35061,.T.) ;
#44490 = ORIENTED_EDGE('',*,*,#35068,.F.) ;
#44491 = ORIENTED_EDGE('',*,*,#35015,.F.) ;
#44492 = ORIENTED_EDGE('',*,*,#34974,.F.) ;
#44493 = ORIENTED_EDGE('',*,*,#35068,.T.) ;
#44494 = ORIENTED_EDGE('',*,*,#34728,.T.) ;
#44495 = ORIENTED_EDGE('',*,*,#35066,.T.) ;
#44496 = ORIENTED_EDGE('',*,*,#34990,.T.) ;
#44497 = ORIENTED_EDGE('',*,*,#35064,.F.) ;
#44498 = ORIENTED_EDGE('',*,*,#34740,.T.) ;
#44499 = ORIENTED_EDGE('',*,*,#35067,.F.) ;
#44500 = ORIENTED_EDGE('',*,*,#35069,.F.) ;
#44501 = ORIENTED_EDGE('',*,*,#35070,.T.) ;
#44502 = ORIENTED_EDGE('',*,*,#34991,.F.) ;
#44503 = ORIENTED_EDGE('',*,*,#35071,.T.) ;
#44504 = ORIENTED_EDGE('',*,*,#35072,.T.) ;
#44505 = ORIENTED_EDGE('',*,*,#35073,.T.) ;
#44506 = ORIENTED_EDGE('',*,*,#35074,.F.) ;
#44507 = ORIENTED_EDGE('',*,*,#35065,.F.) ;
#44508 = ORIENTED_EDGE('',*,*,#34753,.T.) ;
#44509 = ORIENTED_EDGE('',*,*,#35075,.T.) ;
#44510 = ORIENTED_EDGE('',*,*,#34975,.F.) ;
#44511 = ORIENTED_EDGE('',*,*,#35074,.T.) ;
#44512 = ORIENTED_EDGE('',*,*,#34989,.T.) ;
#44513 = ORIENTED_EDGE('',*,*,#35076,.T.) ;
#44514 = ORIENTED_EDGE('',*,*,#34794,.F.) ;
#44515 = ORIENTED_EDGE('',*,*,#35072,.F.) ;
#44516 = ORIENTED_EDGE('',*,*,#35077,.T.) ;
#44517 = ORIENTED_EDGE('',*,*,#35078,.T.) ;
#44518 = ORIENTED_EDGE('',*,*,#35079,.T.) ;
#44519 = ORIENTED_EDGE('',*,*,#35080,.T.) ;
#44520 = ORIENTED_EDGE('',*,*,#35081,.T.) ;
#44521 = ORIENTED_EDGE('',*,*,#35082,.T.) ;
#44522 = ORIENTED_EDGE('',*,*,#35083,.T.) ;
#44523 = ORIENTED_EDGE('',*,*,#35084,.T.) ;
#44524 = ORIENTED_EDGE('',*,*,#35085,.T.) ;
#44525 = ORIENTED_EDGE('',*,*,#35086,.T.) ;
#44526 = ORIENTED_EDGE('',*,*,#35087,.T.) ;
#44527 = ORIENTED_EDGE('',*,*,#35088,.T.) ;
#44528 = ORIENTED_EDGE('',*,*,#35089,.T.) ;
#44529 = ORIENTED_EDGE('',*,*,#35090,.T.) ;
#44530 = ORIENTED_EDGE('',*,*,#35091,.T.) ;
#44531 = ORIENTED_EDGE('',*,*,#35092,.T.) ;
#44532 = ORIENTED_EDGE('',*,*,#35093,.T.) ;
#44533 = ORIENTED_EDGE('',*,*,#35094,.T.) ;
#44534 = ORIENTED_EDGE('',*,*,#35095,.T.) ;
#44535 = ORIENTED_EDGE('',*,*,#35096,.T.) ;
#44536 = ORIENTED_EDGE('',*,*,#35097,.T.) ;
#44537 = ORIENTED_EDGE('',*,*,#35098,.T.) ;
#44538 = ORIENTED_EDGE('',*,*,#35099,.T.) ;
#44539 = ORIENTED_EDGE('',*,*,#35100,.T.) ;
#44540 = ORIENTED_EDGE('',*,*,#34804,.F.) ;
#44541 = ORIENTED_EDGE('',*,*,#35101,.T.) ;
#44542 = ORIENTED_EDGE('',*,*,#34754,.T.) ;
#44543 = ORIENTED_EDGE('',*,*,#35073,.F.) ;
#44544 = ORIENTED_EDGE('',*,*,#35102,.T.) ;
#44545 = ORIENTED_EDGE('',*,*,#35103,.T.) ;
#44546 = ORIENTED_EDGE('',*,*,#35069,.T.) ;
#44547 = ORIENTED_EDGE('',*,*,#35104,.T.) ;
#44548 = ORIENTED_EDGE('',*,*,#35105,.T.) ;
#44549 = ORIENTED_EDGE('',*,*,#35106,.T.) ;
#44550 = ORIENTED_EDGE('',*,*,#35107,.T.) ;
#44551 = ORIENTED_EDGE('',*,*,#35108,.T.) ;
#44552 = ORIENTED_EDGE('',*,*,#35109,.T.) ;
#44553 = ORIENTED_EDGE('',*,*,#35110,.T.) ;
#44554 = ORIENTED_EDGE('',*,*,#35111,.T.) ;
#44555 = ORIENTED_EDGE('',*,*,#35112,.T.) ;
#44556 = ORIENTED_EDGE('',*,*,#35113,.T.) ;
#44557 = ORIENTED_EDGE('',*,*,#35114,.T.) ;
#44558 = ORIENTED_EDGE('',*,*,#35115,.T.) ;
#44559 = ORIENTED_EDGE('',*,*,#35116,.T.) ;
#44560 = ORIENTED_EDGE('',*,*,#35117,.T.) ;
#44561 = ORIENTED_EDGE('',*,*,#35118,.T.) ;
#44562 = ORIENTED_EDGE('',*,*,#35119,.T.) ;
#44563 = ORIENTED_EDGE('',*,*,#35120,.T.) ;
#44564 = ORIENTED_EDGE('',*,*,#35121,.T.) ;
#44565 = ORIENTED_EDGE('',*,*,#35122,.T.) ;
#44566 = ORIENTED_EDGE('',*,*,#35123,.T.) ;
#44567 = ORIENTED_EDGE('',*,*,#35124,.T.) ;
#44568 = ORIENTED_EDGE('',*,*,#35125,.T.) ;
#44569 = ORIENTED_EDGE('',*,*,#35126,.T.) ;
#44570 = ORIENTED_EDGE('',*,*,#35127,.T.) ;
#44571 = ORIENTED_EDGE('',*,*,#35128,.T.) ;
#44572 = ORIENTED_EDGE('',*,*,#35129,.T.) ;
#44573 = ORIENTED_EDGE('',*,*,#35130,.T.) ;
#44574 = ORIENTED_EDGE('',*,*,#35131,.T.) ;
#44575 = ORIENTED_EDGE('',*,*,#35132,.T.) ;
#44576 = ORIENTED_EDGE('',*,*,#35133,.T.) ;
#44577 = ORIENTED_EDGE('',*,*,#35134,.T.) ;
#44578 = ORIENTED_EDGE('',*,*,#35135,.T.) ;
#44579 = ORIENTED_EDGE('',*,*,#35136,.T.) ;
#44580 = ORIENTED_EDGE('',*,*,#35137,.T.) ;
#44581 = ORIENTED_EDGE('',*,*,#35138,.T.) ;
#44582 = ORIENTED_EDGE('',*,*,#35139,.T.) ;
#44583 = ORIENTED_EDGE('',*,*,#35140,.T.) ;
#44584 = ORIENTED_EDGE('',*,*,#35141,.T.) ;
#44585 = ORIENTED_EDGE('',*,*,#35142,.T.) ;
#44586 = ORIENTED_EDGE('',*,*,#35143,.T.) ;
#44587 = ORIENTED_EDGE('',*,*,#35144,.T.) ;
#44588 = ORIENTED_EDGE('',*,*,#35145,.T.) ;
#44589 = ORIENTED_EDGE('',*,*,#35146,.T.) ;
#44590 = ORIENTED_EDGE('',*,*,#35147,.T.) ;
#44591 = ORIENTED_EDGE('',*,*,#35148,.T.) ;
#44592 = ORIENTED_EDGE('',*,*,#35149,.T.) ;
#44593 = ORIENTED_EDGE('',*,*,#35150,.T.) ;
#44594 = ORIENTED_EDGE('',*,*,#35151,.T.) ;
#44595 = ORIENTED_EDGE('',*,*,#35152,.T.) ;
#44596 = ORIENTED_EDGE('',*,*,#35153,.T.) ;
#44597 = ORIENTED_EDGE('',*,*,#35154,.T.) ;
#44598 = ORIENTED_EDGE('',*,*,#35155,.T.) ;
#44599 = ORIENTED_EDGE('',*,*,#35156,.T.) ;
#44600 = ORIENTED_EDGE('',*,*,#35157,.T.) ;
#44601 = ORIENTED_EDGE('',*,*,#35158,.T.) ;
#44602 = ORIENTED_EDGE('',*,*,#35159,.T.) ;
#44603 = ORIENTED_EDGE('',*,*,#35160,.T.) ;
#44604 = ORIENTED_EDGE('',*,*,#35161,.T.) ;
#44605 = ORIENTED_EDGE('',*,*,#35162,.T.) ;
#44606 = ORIENTED_EDGE('',*,*,#35163,.T.) ;
#44607 = ORIENTED_EDGE('',*,*,#35164,.T.) ;
#44608 = ORIENTED_EDGE('',*,*,#35165,.T.) ;
#44609 = ORIENTED_EDGE('',*,*,#35166,.T.) ;
#44610 = ORIENTED_EDGE('',*,*,#35167,.T.) ;
#44611 = ORIENTED_EDGE('',*,*,#35168,.T.) ;
#44612 = ORIENTED_EDGE('',*,*,#35169,.T.) ;
#44613 = ORIENTED_EDGE('',*,*,#35170,.T.) ;
#44614 = ORIENTED_EDGE('',*,*,#35171,.T.) ;
#44615 = ORIENTED_EDGE('',*,*,#35172,.T.) ;
#44616 = ORIENTED_EDGE('',*,*,#35173,.T.) ;
#44617 = ORIENTED_EDGE('',*,*,#35174,.T.) ;
#44618 = ORIENTED_EDGE('',*,*,#35175,.T.) ;
#44619 = ORIENTED_EDGE('',*,*,#35176,.T.) ;
#44620 = ORIENTED_EDGE('',*,*,#35177,.T.) ;
#44621 = ORIENTED_EDGE('',*,*,#35178,.T.) ;
#44622 = ORIENTED_EDGE('',*,*,#35179,.T.) ;
#44623 = ORIENTED_EDGE('',*,*,#35180,.T.) ;
#44624 = ORIENTED_EDGE('',*,*,#35181,.T.) ;
#44625 = ORIENTED_EDGE('',*,*,#35182,.T.) ;
#44626 = ORIENTED_EDGE('',*,*,#35183,.T.) ;
#44627 = ORIENTED_EDGE('',*,*,#35184,.T.) ;
#44628 = ORIENTED_EDGE('',*,*,#35185,.T.) ;
#44629 = ORIENTED_EDGE('',*,*,#35186,.T.) ;
#44630 = ORIENTED_EDGE('',*,*,#35187,.T.) ;
#44631 = ORIENTED_EDGE('',*,*,#35188,.T.) ;
#44632 = ORIENTED_EDGE('',*,*,#35189,.T.) ;
#44633 = ORIENTED_EDGE('',*,*,#35190,.T.) ;
#44634 = ORIENTED_EDGE('',*,*,#35191,.T.) ;
#44635 = ORIENTED_EDGE('',*,*,#35192,.T.) ;
#44636 = ORIENTED_EDGE('',*,*,#35193,.T.) ;
#44637 = ORIENTED_EDGE('',*,*,#35194,.T.) ;
#44638 = ORIENTED_EDGE('',*,*,#35195,.T.) ;
#44639 = ORIENTED_EDGE('',*,*,#35196,.T.) ;
#44640 = ORIENTED_EDGE('',*,*,#35197,.T.) ;
#44641 = ORIENTED_EDGE('',*,*,#35198,.T.) ;
#44642 = ORIENTED_EDGE('',*,*,#35199,.T.) ;
#44643 = ORIENTED_EDGE('',*,*,#35200,.T.) ;
#44644 = ORIENTED_EDGE('',*,*,#35201,.T.) ;
#44645 = ORIENTED_EDGE('',*,*,#35202,.T.) ;
#44646 = ORIENTED_EDGE('',*,*,#35203,.T.) ;
#44647 = ORIENTED_EDGE('',*,*,#35204,.T.) ;
#44648 = ORIENTED_EDGE('',*,*,#35205,.T.) ;
#44649 = ORIENTED_EDGE('',*,*,#35206,.T.) ;
#44650 = ORIENTED_EDGE('',*,*,#35207,.T.) ;
#44651 = ORIENTED_EDGE('',*,*,#35208,.T.) ;
#44652 = ORIENTED_EDGE('',*,*,#35209,.T.) ;
#44653 = ORIENTED_EDGE('',*,*,#35210,.T.) ;
#44654 = ORIENTED_EDGE('',*,*,#35211,.T.) ;
#44655 = ORIENTED_EDGE('',*,*,#35212,.T.) ;
#44656 = ORIENTED_EDGE('',*,*,#35213,.T.) ;
#44657 = ORIENTED_EDGE('',*,*,#35214,.T.) ;
#44658 = ORIENTED_EDGE('',*,*,#35215,.T.) ;
#44659 = ORIENTED_EDGE('',*,*,#35216,.T.) ;
#44660 = ORIENTED_EDGE('',*,*,#35217,.T.) ;
#44661 = ORIENTED_EDGE('',*,*,#35218,.T.) ;
#44662 = ORIENTED_EDGE('',*,*,#35219,.T.) ;
#44663 = ORIENTED_EDGE('',*,*,#35220,.T.) ;
#44664 = ORIENTED_EDGE('',*,*,#35221,.T.) ;
#44665 = ORIENTED_EDGE('',*,*,#35222,.T.) ;
#44666 = ORIENTED_EDGE('',*,*,#35223,.T.) ;
#44667 = ORIENTED_EDGE('',*,*,#35224,.T.) ;
#44668 = ORIENTED_EDGE('',*,*,#35225,.T.) ;
#44669 = ORIENTED_EDGE('',*,*,#35226,.T.) ;
#44670 = ORIENTED_EDGE('',*,*,#35227,.T.) ;
#44671 = ORIENTED_EDGE('',*,*,#35228,.T.) ;
#44672 = ORIENTED_EDGE('',*,*,#35229,.T.) ;
#44673 = ORIENTED_EDGE('',*,*,#35230,.T.) ;
#44674 = ORIENTED_EDGE('',*,*,#35231,.T.) ;
#44675 = ORIENTED_EDGE('',*,*,#35232,.T.) ;
#44676 = ORIENTED_EDGE('',*,*,#35233,.T.) ;
#44677 = ORIENTED_EDGE('',*,*,#35234,.T.) ;
#44678 = ORIENTED_EDGE('',*,*,#35235,.T.) ;
#44679 = ORIENTED_EDGE('',*,*,#35236,.T.) ;
#44680 = ORIENTED_EDGE('',*,*,#35237,.T.) ;
#44681 = ORIENTED_EDGE('',*,*,#35238,.T.) ;
#44682 = ORIENTED_EDGE('',*,*,#35239,.T.) ;
#44683 = ORIENTED_EDGE('',*,*,#35240,.T.) ;
#44684 = ORIENTED_EDGE('',*,*,#35241,.T.) ;
#44685 = ORIENTED_EDGE('',*,*,#35242,.T.) ;
#44686 = ORIENTED_EDGE('',*,*,#35243,.T.) ;
#44687 = ORIENTED_EDGE('',*,*,#35244,.T.) ;
#44688 = ORIENTED_EDGE('',*,*,#35245,.T.) ;
#44689 = ORIENTED_EDGE('',*,*,#35246,.T.) ;
#44690 = ORIENTED_EDGE('',*,*,#35247,.T.) ;
#44691 = ORIENTED_EDGE('',*,*,#35248,.T.) ;
#44692 = ORIENTED_EDGE('',*,*,#35249,.T.) ;
#44693 = ORIENTED_EDGE('',*,*,#35250,.T.) ;
#44694 = ORIENTED_EDGE('',*,*,#35251,.T.) ;
#44695 = ORIENTED_EDGE('',*,*,#35252,.T.) ;
#44696 = ORIENTED_EDGE('',*,*,#35253,.T.) ;
#44697 = ORIENTED_EDGE('',*,*,#35254,.T.) ;
#44698 = ORIENTED_EDGE('',*,*,#35255,.T.) ;
#44699 = ORIENTED_EDGE('',*,*,#35256,.T.) ;
#44700 = ORIENTED_EDGE('',*,*,#35257,.T.) ;
#44701 = ORIENTED_EDGE('',*,*,#35258,.T.) ;
#44702 = ORIENTED_EDGE('',*,*,#35259,.T.) ;
#44703 = ORIENTED_EDGE('',*,*,#35260,.T.) ;
#44704 = ORIENTED_EDGE('',*,*,#35261,.T.) ;
#44705 = ORIENTED_EDGE('',*,*,#35262,.T.) ;
#44706 = ORIENTED_EDGE('',*,*,#35263,.T.) ;
#44707 = ORIENTED_EDGE('',*,*,#35264,.T.) ;
#44708 = ORIENTED_EDGE('',*,*,#35265,.T.) ;
#44709 = ORIENTED_EDGE('',*,*,#35266,.T.) ;
#44710 = ORIENTED_EDGE('',*,*,#35267,.T.) ;
#44711 = ORIENTED_EDGE('',*,*,#35268,.T.) ;
#44712 = ORIENTED_EDGE('',*,*,#35269,.T.) ;
#44713 = ORIENTED_EDGE('',*,*,#35270,.T.) ;
#44714 = ORIENTED_EDGE('',*,*,#35271,.T.) ;
#44715 = ORIENTED_EDGE('',*,*,#35272,.T.) ;
#44716 = ORIENTED_EDGE('',*,*,#35273,.T.) ;
#44717 = ORIENTED_EDGE('',*,*,#35274,.T.) ;
#44718 = ORIENTED_EDGE('',*,*,#35275,.T.) ;
#44719 = ORIENTED_EDGE('',*,*,#35276,.T.) ;
#44720 = ORIENTED_EDGE('',*,*,#35277,.T.) ;
#44721 = ORIENTED_EDGE('',*,*,#35278,.T.) ;
#44722 = ORIENTED_EDGE('',*,*,#35279,.T.) ;
#44723 = ORIENTED_EDGE('',*,*,#35280,.T.) ;
#44724 = ORIENTED_EDGE('',*,*,#35281,.T.) ;
#44725 = ORIENTED_EDGE('',*,*,#35282,.T.) ;
#44726 = ORIENTED_EDGE('',*,*,#35283,.T.) ;
#44727 = ORIENTED_EDGE('',*,*,#35284,.T.) ;
#44728 = ORIENTED_EDGE('',*,*,#35285,.T.) ;
#44729 = ORIENTED_EDGE('',*,*,#35286,.T.) ;
#44730 = ORIENTED_EDGE('',*,*,#35287,.T.) ;
#44731 = ORIENTED_EDGE('',*,*,#35288,.T.) ;
#44732 = ORIENTED_EDGE('',*,*,#35289,.T.) ;
#44733 = ORIENTED_EDGE('',*,*,#35290,.T.) ;
#44734 = ORIENTED_EDGE('',*,*,#35291,.T.) ;
#44735 = ORIENTED_EDGE('',*,*,#35292,.T.) ;
#44736 = ORIENTED_EDGE('',*,*,#35293,.T.) ;
#44737 = ORIENTED_EDGE('',*,*,#35294,.T.) ;
#44738 = ORIENTED_EDGE('',*,*,#35295,.T.) ;
#44739 = ORIENTED_EDGE('',*,*,#35296,.T.) ;
#44740 = ORIENTED_EDGE('',*,*,#35297,.F.) ;
#44741 = ORIENTED_EDGE('',*,*,#34755,.F.) ;
#44742 = ORIENTED_EDGE('',*,*,#35298,.F.) ;
#44743 = ORIENTED_EDGE('',*,*,#35098,.F.) ;
#44744 = ORIENTED_EDGE('',*,*,#35298,.T.) ;
#44745 = ORIENTED_EDGE('',*,*,#35101,.F.) ;
#44746 = ORIENTED_EDGE('',*,*,#35299,.F.) ;
#44747 = ORIENTED_EDGE('',*,*,#35099,.F.) ;
#44748 = ORIENTED_EDGE('',*,*,#35300,.F.) ;
#44749 = ORIENTED_EDGE('',*,*,#35297,.T.) ;
#44750 = ORIENTED_EDGE('',*,*,#35301,.F.) ;
#44751 = ORIENTED_EDGE('',*,*,#35299,.T.) ;
#44752 = ORIENTED_EDGE('',*,*,#34803,.F.) ;
#44753 = ORIENTED_EDGE('',*,*,#35302,.F.) ;
#44754 = ORIENTED_EDGE('',*,*,#35100,.F.) ;
#44755 = ORIENTED_EDGE('',*,*,#35301,.T.) ;
#44756 = ORIENTED_EDGE('',*,*,#35097,.F.) ;
#44757 = ORIENTED_EDGE('',*,*,#35303,.F.) ;
#44758 = ORIENTED_EDGE('',*,*,#35096,.F.) ;
#44759 = ORIENTED_EDGE('',*,*,#35300,.T.) ;
#44760 = ORIENTED_EDGE('',*,*,#35095,.F.) ;
#44761 = ORIENTED_EDGE('',*,*,#35304,.F.) ;
#44762 = ORIENTED_EDGE('',*,*,#34756,.F.) ;
#44763 = ORIENTED_EDGE('',*,*,#35303,.T.) ;
#44764 = ORIENTED_EDGE('',*,*,#35302,.T.) ;
#44765 = ORIENTED_EDGE('',*,*,#35305,.F.) ;
#44766 = ORIENTED_EDGE('',*,*,#35306,.F.) ;
#44767 = ORIENTED_EDGE('',*,*,#35304,.T.) ;
#44768 = ORIENTED_EDGE('',*,*,#35307,.F.) ;
#44769 = ORIENTED_EDGE('',*,*,#35305,.T.) ;
#44770 = ORIENTED_EDGE('',*,*,#34802,.F.) ;
#44771 = ORIENTED_EDGE('',*,*,#35308,.F.) ;
#44772 = ORIENTED_EDGE('',*,*,#35093,.F.) ;
#44773 = ORIENTED_EDGE('',*,*,#35307,.T.) ;
#44774 = ORIENTED_EDGE('',*,*,#35094,.F.) ;
#44775 = ORIENTED_EDGE('',*,*,#35309,.F.) ;
#44776 = ORIENTED_EDGE('',*,*,#35092,.F.) ;
#44777 = ORIENTED_EDGE('',*,*,#35306,.T.) ;
#44778 = ORIENTED_EDGE('',*,*,#35091,.F.) ;
#44779 = ORIENTED_EDGE('',*,*,#35310,.F.) ;
#44780 = ORIENTED_EDGE('',*,*,#34757,.F.) ;
#44781 = ORIENTED_EDGE('',*,*,#35309,.T.) ;
#44782 = ORIENTED_EDGE('',*,*,#35308,.T.) ;
#44783 = ORIENTED_EDGE('',*,*,#35311,.F.) ;
#44784 = ORIENTED_EDGE('',*,*,#34758,.T.) ;
#44785 = ORIENTED_EDGE('',*,*,#35310,.T.) ;
#44786 = ORIENTED_EDGE('',*,*,#35312,.F.) ;
#44787 = ORIENTED_EDGE('',*,*,#35313,.F.) ;
#44788 = ORIENTED_EDGE('',*,*,#35311,.T.) ;
#44789 = ORIENTED_EDGE('',*,*,#34801,.F.) ;
#44790 = ORIENTED_EDGE('',*,*,#35314,.F.) ;
#44791 = ORIENTED_EDGE('',*,*,#35089,.F.) ;
#44792 = ORIENTED_EDGE('',*,*,#35312,.T.) ;
#44793 = ORIENTED_EDGE('',*,*,#35090,.F.) ;
#44794 = ORIENTED_EDGE('',*,*,#35315,.F.) ;
#44795 = ORIENTED_EDGE('',*,*,#35088,.F.) ;
#44796 = ORIENTED_EDGE('',*,*,#35313,.T.) ;
#44797 = ORIENTED_EDGE('',*,*,#35087,.F.) ;
#44798 = ORIENTED_EDGE('',*,*,#35316,.F.) ;
#44799 = ORIENTED_EDGE('',*,*,#34759,.F.) ;
#44800 = ORIENTED_EDGE('',*,*,#35314,.T.) ;
#44801 = ORIENTED_EDGE('',*,*,#34800,.T.) ;
#44802 = ORIENTED_EDGE('',*,*,#35317,.F.) ;
#44803 = ORIENTED_EDGE('',*,*,#35315,.T.) ;
#44804 = ORIENTED_EDGE('',*,*,#35318,.F.) ;
#44805 = ORIENTED_EDGE('',*,*,#35316,.T.) ;
#44806 = ORIENTED_EDGE('',*,*,#35319,.F.) ;
#44807 = ORIENTED_EDGE('',*,*,#35317,.T.) ;
#44808 = ORIENTED_EDGE('',*,*,#34799,.F.) ;
#44809 = ORIENTED_EDGE('',*,*,#35320,.F.) ;
#44810 = ORIENTED_EDGE('',*,*,#35085,.F.) ;
#44811 = ORIENTED_EDGE('',*,*,#35319,.T.) ;
#44812 = ORIENTED_EDGE('',*,*,#35086,.F.) ;
#44813 = ORIENTED_EDGE('',*,*,#35321,.F.) ;
#44814 = ORIENTED_EDGE('',*,*,#35084,.F.) ;
#44815 = ORIENTED_EDGE('',*,*,#35318,.T.) ;
#44816 = ORIENTED_EDGE('',*,*,#35083,.F.) ;
#44817 = ORIENTED_EDGE('',*,*,#35322,.F.) ;
#44818 = ORIENTED_EDGE('',*,*,#34760,.F.) ;
#44819 = ORIENTED_EDGE('',*,*,#35321,.T.) ;
#44820 = ORIENTED_EDGE('',*,*,#35320,.T.) ;
#44821 = ORIENTED_EDGE('',*,*,#35323,.F.) ;
#44822 = ORIENTED_EDGE('',*,*,#35324,.F.) ;
#44823 = ORIENTED_EDGE('',*,*,#35322,.T.) ;
#44824 = ORIENTED_EDGE('',*,*,#35325,.F.) ;
#44825 = ORIENTED_EDGE('',*,*,#35323,.T.) ;
#44826 = ORIENTED_EDGE('',*,*,#34798,.F.) ;
#44827 = ORIENTED_EDGE('',*,*,#35326,.F.) ;
#44828 = ORIENTED_EDGE('',*,*,#35081,.F.) ;
#44829 = ORIENTED_EDGE('',*,*,#35325,.T.) ;
#44830 = ORIENTED_EDGE('',*,*,#35082,.F.) ;
#44831 = ORIENTED_EDGE('',*,*,#35327,.F.) ;
#44832 = ORIENTED_EDGE('',*,*,#35080,.F.) ;
#44833 = ORIENTED_EDGE('',*,*,#35324,.T.) ;
#44834 = ORIENTED_EDGE('',*,*,#35079,.F.) ;
#44835 = ORIENTED_EDGE('',*,*,#35328,.F.) ;
#44836 = ORIENTED_EDGE('',*,*,#34761,.F.) ;
#44837 = ORIENTED_EDGE('',*,*,#35329,.F.) ;
#44838 = ORIENTED_EDGE('',*,*,#34846,.F.) ;
#44839 = ORIENTED_EDGE('',*,*,#35330,.F.) ;
#44840 = ORIENTED_EDGE('',*,*,#35040,.F.) ;
#44841 = ORIENTED_EDGE('',*,*,#35327,.T.) ;
#44842 = ORIENTED_EDGE('',*,*,#35326,.T.) ;
#44843 = ORIENTED_EDGE('',*,*,#35331,.F.) ;
#44844 = ORIENTED_EDGE('',*,*,#34751,.T.) ;
#44845 = ORIENTED_EDGE('',*,*,#35328,.T.) ;
#44846 = ORIENTED_EDGE('',*,*,#35332,.F.) ;
#44847 = ORIENTED_EDGE('',*,*,#35333,.F.) ;
#44848 = ORIENTED_EDGE('',*,*,#35334,.F.) ;
#44849 = ORIENTED_EDGE('',*,*,#35330,.T.) ;
#44850 = ORIENTED_EDGE('',*,*,#35335,.F.) ;
#44851 = ORIENTED_EDGE('',*,*,#35329,.T.) ;
#44852 = ORIENTED_EDGE('',*,*,#35043,.F.) ;
#44853 = ORIENTED_EDGE('',*,*,#35336,.F.) ;
#44854 = ORIENTED_EDGE('',*,*,#35047,.F.) ;
#44855 = ORIENTED_EDGE('',*,*,#35331,.T.) ;
#44856 = ORIENTED_EDGE('',*,*,#34797,.F.) ;
#44857 = ORIENTED_EDGE('',*,*,#35337,.F.) ;
#44858 = ORIENTED_EDGE('',*,*,#35077,.F.) ;
#44859 = ORIENTED_EDGE('',*,*,#35332,.T.) ;
#44860 = ORIENTED_EDGE('',*,*,#35078,.F.) ;
#44861 = ORIENTED_EDGE('',*,*,#35338,.F.) ;
#44862 = ORIENTED_EDGE('',*,*,#35102,.F.) ;
#44863 = ORIENTED_EDGE('',*,*,#35333,.T.) ;
#44864 = ORIENTED_EDGE('',*,*,#35104,.F.) ;
#44865 = ORIENTED_EDGE('',*,*,#35339,.F.) ;
#44866 = ORIENTED_EDGE('',*,*,#34752,.F.) ;
#44867 = ORIENTED_EDGE('',*,*,#35335,.T.) ;
#44868 = ORIENTED_EDGE('',*,*,#34845,.F.) ;
#44869 = ORIENTED_EDGE('',*,*,#35340,.F.) ;
#44870 = ORIENTED_EDGE('',*,*,#35023,.F.) ;
#44871 = ORIENTED_EDGE('',*,*,#35334,.T.) ;
#44872 = ORIENTED_EDGE('',*,*,#35022,.F.) ;
#44873 = ORIENTED_EDGE('',*,*,#35341,.F.) ;
#44874 = ORIENTED_EDGE('',*,*,#35041,.F.) ;
#44875 = ORIENTED_EDGE('',*,*,#35336,.T.) ;
#44876 = ORIENTED_EDGE('',*,*,#35042,.F.) ;
#44877 = ORIENTED_EDGE('',*,*,#35342,.F.) ;
#44878 = ORIENTED_EDGE('',*,*,#34908,.F.) ;
#44879 = ORIENTED_EDGE('',*,*,#35337,.T.) ;
#44880 = ORIENTED_EDGE('',*,*,#34796,.T.) ;
#44881 = ORIENTED_EDGE('',*,*,#35343,.F.) ;
#44882 = ORIENTED_EDGE('',*,*,#35338,.T.) ;
#44883 = ORIENTED_EDGE('',*,*,#35339,.T.) ;
#44884 = ORIENTED_EDGE('',*,*,#35071,.F.) ;
#44885 = ORIENTED_EDGE('',*,*,#35344,.F.) ;
#44886 = ORIENTED_EDGE('',*,*,#35075,.F.) ;
#44887 = ORIENTED_EDGE('',*,*,#35345,.F.) ;
#44888 = ORIENTED_EDGE('',*,*,#35340,.T.) ;
#44889 = ORIENTED_EDGE('',*,*,#35346,.F.) ;
#44890 = ORIENTED_EDGE('',*,*,#35342,.T.) ;
#44891 = ORIENTED_EDGE('',*,*,#35341,.T.) ;
#44892 = ORIENTED_EDGE('',*,*,#35347,.F.) ;
#44893 = ORIENTED_EDGE('',*,*,#35343,.T.) ;
#44894 = ORIENTED_EDGE('',*,*,#34795,.F.) ;
#44895 = ORIENTED_EDGE('',*,*,#35348,.F.) ;
#44896 = ORIENTED_EDGE('',*,*,#35103,.F.) ;
#44897 = ORIENTED_EDGE('',*,*,#35344,.T.) ;
#44898 = ORIENTED_EDGE('',*,*,#34994,.F.) ;
#44899 = ORIENTED_EDGE('',*,*,#35349,.F.) ;
#44900 = ORIENTED_EDGE('',*,*,#34976,.F.) ;
#44901 = ORIENTED_EDGE('',*,*,#35346,.T.) ;
#44902 = ORIENTED_EDGE('',*,*,#34844,.F.) ;
#44903 = ORIENTED_EDGE('',*,*,#35350,.F.) ;
#44904 = ORIENTED_EDGE('',*,*,#35026,.F.) ;
#44905 = ORIENTED_EDGE('',*,*,#35345,.T.) ;
#44906 = ORIENTED_EDGE('',*,*,#35025,.F.) ;
#44907 = ORIENTED_EDGE('',*,*,#35351,.F.) ;
#44908 = ORIENTED_EDGE('',*,*,#35020,.F.) ;
#44909 = ORIENTED_EDGE('',*,*,#35347,.T.) ;
#44910 = ORIENTED_EDGE('',*,*,#35021,.F.) ;
#44911 = ORIENTED_EDGE('',*,*,#35352,.F.) ;
#44912 = ORIENTED_EDGE('',*,*,#34909,.F.) ;
#44913 = ORIENTED_EDGE('',*,*,#35348,.T.) ;
#44914 = ORIENTED_EDGE('',*,*,#35076,.F.) ;
#44915 = ORIENTED_EDGE('',*,*,#35353,.F.) ;
#44916 = ORIENTED_EDGE('',*,*,#35070,.F.) ;
#44917 = ORIENTED_EDGE('',*,*,#34977,.T.) ;
#44918 = ORIENTED_EDGE('',*,*,#35349,.T.) ;
#44919 = ORIENTED_EDGE('',*,*,#35354,.F.) ;
#44920 = ORIENTED_EDGE('',*,*,#35355,.F.) ;
#44921 = ORIENTED_EDGE('',*,*,#35350,.T.) ;
#44922 = ORIENTED_EDGE('',*,*,#34843,.T.) ;
#44923 = ORIENTED_EDGE('',*,*,#35356,.F.) ;
#44924 = ORIENTED_EDGE('',*,*,#35357,.F.) ;
#44925 = ORIENTED_EDGE('',*,*,#35352,.T.) ;
#44926 = ORIENTED_EDGE('',*,*,#35351,.T.) ;
#44927 = ORIENTED_EDGE('',*,*,#35358,.F.) ;
#44928 = ORIENTED_EDGE('',*,*,#35353,.T.) ;
#44929 = ORIENTED_EDGE('',*,*,#34988,.F.) ;
#44930 = ORIENTED_EDGE('',*,*,#35359,.F.) ;
#44931 = ORIENTED_EDGE('',*,*,#34992,.F.) ;
#44932 = ORIENTED_EDGE('',*,*,#35354,.T.) ;
#44933 = ORIENTED_EDGE('',*,*,#34993,.F.) ;
#44934 = ORIENTED_EDGE('',*,*,#35360,.F.) ;
#44935 = ORIENTED_EDGE('',*,*,#35006,.F.) ;
#44936 = ORIENTED_EDGE('',*,*,#35355,.T.) ;
#44937 = ORIENTED_EDGE('',*,*,#35005,.F.) ;
#44938 = ORIENTED_EDGE('',*,*,#35361,.F.) ;
#44939 = ORIENTED_EDGE('',*,*,#34978,.F.) ;
#44940 = ORIENTED_EDGE('',*,*,#35356,.T.) ;
#44941 = ORIENTED_EDGE('',*,*,#34842,.F.) ;
#44942 = ORIENTED_EDGE('',*,*,#35362,.F.) ;
#44943 = ORIENTED_EDGE('',*,*,#35030,.F.) ;
#44944 = ORIENTED_EDGE('',*,*,#35357,.T.) ;
#44945 = ORIENTED_EDGE('',*,*,#35029,.F.) ;
#44946 = ORIENTED_EDGE('',*,*,#35363,.F.) ;
#44947 = ORIENTED_EDGE('',*,*,#35027,.F.) ;
#44948 = ORIENTED_EDGE('',*,*,#35358,.T.) ;
#44949 = ORIENTED_EDGE('',*,*,#35024,.F.) ;
#44950 = ORIENTED_EDGE('',*,*,#35364,.F.) ;
#44951 = ORIENTED_EDGE('',*,*,#34910,.F.) ;
#44952 = ORIENTED_EDGE('',*,*,#35359,.T.) ;
#44953 = ORIENTED_EDGE('',*,*,#34987,.T.) ;
#44954 = ORIENTED_EDGE('',*,*,#35365,.F.) ;
#44955 = ORIENTED_EDGE('',*,*,#35360,.T.) ;
#44956 = ORIENTED_EDGE('',*,*,#35366,.F.) ;
#44957 = ORIENTED_EDGE('',*,*,#35361,.T.) ;
#44958 = ORIENTED_EDGE('',*,*,#35367,.F.) ;
#44959 = ORIENTED_EDGE('',*,*,#35368,.F.) ;
#44960 = ORIENTED_EDGE('',*,*,#35362,.T.) ;
#44961 = ORIENTED_EDGE('',*,*,#35369,.F.) ;
#44962 = ORIENTED_EDGE('',*,*,#35364,.T.) ;
#44963 = ORIENTED_EDGE('',*,*,#35363,.T.) ;
#44964 = ORIENTED_EDGE('',*,*,#35370,.F.) ;
#44965 = ORIENTED_EDGE('',*,*,#34911,.T.) ;
#44966 = ORIENTED_EDGE('',*,*,#35365,.T.) ;
#44967 = ORIENTED_EDGE('',*,*,#34986,.F.) ;
#44968 = ORIENTED_EDGE('',*,*,#35371,.F.) ;
#44969 = ORIENTED_EDGE('',*,*,#35003,.F.) ;
#44970 = ORIENTED_EDGE('',*,*,#35367,.T.) ;
#44971 = ORIENTED_EDGE('',*,*,#35004,.F.) ;
#44972 = ORIENTED_EDGE('',*,*,#35372,.F.) ;
#44973 = ORIENTED_EDGE('',*,*,#35002,.F.) ;
#44974 = ORIENTED_EDGE('',*,*,#35366,.T.) ;
#44975 = ORIENTED_EDGE('',*,*,#35001,.F.) ;
#44976 = ORIENTED_EDGE('',*,*,#35373,.F.) ;
#44977 = ORIENTED_EDGE('',*,*,#34979,.F.) ;
#44978 = ORIENTED_EDGE('',*,*,#35369,.T.) ;
#44979 = ORIENTED_EDGE('',*,*,#34841,.F.) ;
#44980 = ORIENTED_EDGE('',*,*,#35374,.F.) ;
#44981 = ORIENTED_EDGE('',*,*,#35034,.F.) ;
#44982 = ORIENTED_EDGE('',*,*,#35368,.T.) ;
#44983 = ORIENTED_EDGE('',*,*,#35033,.F.) ;
#44984 = ORIENTED_EDGE('',*,*,#35375,.F.) ;
#44985 = ORIENTED_EDGE('',*,*,#35031,.F.) ;
#44986 = ORIENTED_EDGE('',*,*,#35370,.T.) ;
#44987 = ORIENTED_EDGE('',*,*,#35028,.F.) ;
#44988 = ORIENTED_EDGE('',*,*,#35376,.F.) ;
#44989 = ORIENTED_EDGE('',*,*,#34912,.F.) ;
#44990 = ORIENTED_EDGE('',*,*,#35372,.T.) ;
#44991 = ORIENTED_EDGE('',*,*,#35371,.T.) ;
#44992 = ORIENTED_EDGE('',*,*,#35377,.F.) ;
#44993 = ORIENTED_EDGE('',*,*,#35378,.F.) ;
#44994 = ORIENTED_EDGE('',*,*,#35373,.T.) ;
#44995 = ORIENTED_EDGE('',*,*,#35379,.F.) ;
#44996 = ORIENTED_EDGE('',*,*,#35380,.F.) ;
#44997 = ORIENTED_EDGE('',*,*,#35018,.F.) ;
#44998 = ORIENTED_EDGE('',*,*,#35381,.F.) ;
#44999 = ORIENTED_EDGE('',*,*,#35013,.F.) ;
#45000 = ORIENTED_EDGE('',*,*,#35382,.F.) ;
#45001 = ORIENTED_EDGE('',*,*,#35374,.T.) ;
#45002 = ORIENTED_EDGE('',*,*,#35383,.F.) ;
#45003 = ORIENTED_EDGE('',*,*,#35376,.T.) ;
#45004 = ORIENTED_EDGE('',*,*,#35375,.T.) ;
#45005 = ORIENTED_EDGE('',*,*,#35384,.F.) ;
#45006 = ORIENTED_EDGE('',*,*,#35377,.T.) ;
#45007 = ORIENTED_EDGE('',*,*,#34985,.F.) ;
#45008 = ORIENTED_EDGE('',*,*,#35385,.F.) ;
#45009 = ORIENTED_EDGE('',*,*,#34999,.F.) ;
#45010 = ORIENTED_EDGE('',*,*,#35379,.T.) ;
#45011 = ORIENTED_EDGE('',*,*,#35000,.F.) ;
#45012 = ORIENTED_EDGE('',*,*,#35386,.F.) ;
#45013 = ORIENTED_EDGE('',*,*,#35010,.F.) ;
#45014 = ORIENTED_EDGE('',*,*,#35378,.T.) ;
#45015 = ORIENTED_EDGE('',*,*,#35009,.F.) ;
#45016 = ORIENTED_EDGE('',*,*,#35387,.F.) ;
#45017 = ORIENTED_EDGE('',*,*,#34980,.F.) ;
#45018 = ORIENTED_EDGE('',*,*,#35381,.T.) ;
#45019 = ORIENTED_EDGE('',*,*,#34972,.F.) ;
#45020 = ORIENTED_EDGE('',*,*,#35388,.F.) ;
#45021 = ORIENTED_EDGE('',*,*,#34998,.F.) ;
#45022 = ORIENTED_EDGE('',*,*,#35380,.T.) ;
#45023 = ORIENTED_EDGE('',*,*,#35046,.F.) ;
#45024 = ORIENTED_EDGE('',*,*,#35389,.F.) ;
#45025 = ORIENTED_EDGE('',*,*,#34838,.F.) ;
#45026 = ORIENTED_EDGE('',*,*,#35383,.T.) ;
#45027 = ORIENTED_EDGE('',*,*,#34840,.F.) ;
#45028 = ORIENTED_EDGE('',*,*,#35390,.F.) ;
#45029 = ORIENTED_EDGE('',*,*,#35038,.F.) ;
#45030 = ORIENTED_EDGE('',*,*,#35382,.T.) ;
#45031 = ORIENTED_EDGE('',*,*,#35037,.F.) ;
#45032 = ORIENTED_EDGE('',*,*,#35391,.F.) ;
#45033 = ORIENTED_EDGE('',*,*,#35035,.F.) ;
#45034 = ORIENTED_EDGE('',*,*,#35384,.T.) ;
#45035 = ORIENTED_EDGE('',*,*,#35032,.F.) ;
#45036 = ORIENTED_EDGE('',*,*,#35392,.F.) ;
#45037 = ORIENTED_EDGE('',*,*,#34913,.F.) ;
#45038 = ORIENTED_EDGE('',*,*,#35386,.T.) ;
#45039 = ORIENTED_EDGE('',*,*,#35385,.T.) ;
#45040 = ORIENTED_EDGE('',*,*,#35393,.F.) ;
#45041 = ORIENTED_EDGE('',*,*,#34971,.T.) ;
#45042 = ORIENTED_EDGE('',*,*,#35387,.T.) ;
#45043 = ORIENTED_EDGE('',*,*,#35394,.F.) ;
#45044 = ORIENTED_EDGE('',*,*,#35388,.T.) ;
#45045 = ORIENTED_EDGE('',*,*,#34839,.T.) ;
#45046 = ORIENTED_EDGE('',*,*,#35389,.T.) ;
#45047 = ORIENTED_EDGE('',*,*,#35395,.F.) ;
#45048 = ORIENTED_EDGE('',*,*,#35390,.T.) ;
#45049 = ORIENTED_EDGE('',*,*,#35392,.T.) ;
#45050 = ORIENTED_EDGE('',*,*,#35391,.T.) ;
#45051 = ORIENTED_EDGE('',*,*,#35396,.F.) ;
#45052 = ORIENTED_EDGE('',*,*,#35393,.T.) ;
#45053 = ORIENTED_EDGE('',*,*,#34984,.F.) ;
#45054 = ORIENTED_EDGE('',*,*,#35397,.F.) ;
#45055 = ORIENTED_EDGE('',*,*,#35007,.F.) ;
#45056 = ORIENTED_EDGE('',*,*,#35394,.T.) ;
#45057 = ORIENTED_EDGE('',*,*,#35008,.F.) ;
#45058 = ORIENTED_EDGE('',*,*,#35398,.F.) ;
#45059 = ORIENTED_EDGE('',*,*,#34995,.F.) ;
#45060 = ORIENTED_EDGE('',*,*,#35395,.T.) ;
#45061 = ORIENTED_EDGE('',*,*,#35045,.F.) ;
#45062 = ORIENTED_EDGE('',*,*,#35399,.F.) ;
#45063 = ORIENTED_EDGE('',*,*,#35039,.F.) ;
#45064 = ORIENTED_EDGE('',*,*,#35396,.T.) ;
#45065 = ORIENTED_EDGE('',*,*,#35036,.F.) ;
#45066 = ORIENTED_EDGE('',*,*,#35400,.F.) ;
#45067 = ORIENTED_EDGE('',*,*,#34914,.F.) ;
#45068 = ORIENTED_EDGE('',*,*,#35397,.T.) ;
#45069 = ORIENTED_EDGE('',*,*,#34983,.T.) ;
#45070 = ORIENTED_EDGE('',*,*,#35401,.F.) ;
#45071 = ORIENTED_EDGE('',*,*,#35398,.T.) ;
#45072 = ORIENTED_EDGE('',*,*,#35400,.T.) ;
#45073 = ORIENTED_EDGE('',*,*,#35399,.T.) ;
#45074 = ORIENTED_EDGE('',*,*,#35402,.F.) ;
#45075 = ORIENTED_EDGE('',*,*,#34904,.T.) ;
#45076 = ORIENTED_EDGE('',*,*,#35401,.T.) ;
#45077 = ORIENTED_EDGE('',*,*,#34982,.F.) ;
#45078 = ORIENTED_EDGE('',*,*,#35403,.F.) ;
#45079 = ORIENTED_EDGE('',*,*,#34996,.F.) ;
#45080 = ORIENTED_EDGE('',*,*,#35402,.T.) ;
#45081 = ORIENTED_EDGE('',*,*,#35044,.F.) ;
#45082 = ORIENTED_EDGE('',*,*,#35404,.F.) ;
#45083 = ORIENTED_EDGE('',*,*,#34905,.F.) ;
#45084 = ORIENTED_EDGE('',*,*,#35403,.T.) ;
#45085 = ORIENTED_EDGE('',*,*,#35019,.F.) ;
#45086 = ORIENTED_EDGE('',*,*,#35404,.T.) ;
#45087 = ORIENTED_EDGE('',*,*,#35011,.F.) ;
#45088 = ORIENTED_EDGE('',*,*,#35405,.F.) ;
#45089 = ORIENTED_EDGE('',*,*,#34777,.F.) ;
#45090 = ORIENTED_EDGE('',*,*,#35406,.F.) ;
#45091 = ORIENTED_EDGE('',*,*,#35279,.F.) ;
#45092 = ORIENTED_EDGE('',*,*,#34770,.T.) ;
#45093 = ORIENTED_EDGE('',*,*,#35405,.T.) ;
#45094 = ORIENTED_EDGE('',*,*,#35407,.F.) ;
#45095 = ORIENTED_EDGE('',*,*,#35408,.F.) ;
#45096 = ORIENTED_EDGE('',*,*,#35406,.T.) ;
#45097 = ORIENTED_EDGE('',*,*,#34776,.T.) ;
#45098 = ORIENTED_EDGE('',*,*,#35409,.F.) ;
#45099 = ORIENTED_EDGE('',*,*,#35410,.F.) ;
#45100 = ORIENTED_EDGE('',*,*,#35407,.T.) ;
#45101 = ORIENTED_EDGE('',*,*,#35278,.F.) ;
#45102 = ORIENTED_EDGE('',*,*,#35411,.F.) ;
#45103 = ORIENTED_EDGE('',*,*,#35266,.F.) ;
#45104 = ORIENTED_EDGE('',*,*,#35408,.T.) ;
#45105 = ORIENTED_EDGE('',*,*,#35265,.F.) ;
#45106 = ORIENTED_EDGE('',*,*,#35412,.F.) ;
#45107 = ORIENTED_EDGE('',*,*,#34771,.F.) ;
#45108 = ORIENTED_EDGE('',*,*,#35413,.F.) ;
#45109 = ORIENTED_EDGE('',*,*,#34773,.F.) ;
#45110 = ORIENTED_EDGE('',*,*,#35414,.F.) ;
#45111 = ORIENTED_EDGE('',*,*,#35269,.F.) ;
#45112 = ORIENTED_EDGE('',*,*,#35409,.T.) ;
#45113 = ORIENTED_EDGE('',*,*,#34775,.F.) ;
#45114 = ORIENTED_EDGE('',*,*,#35415,.F.) ;
#45115 = ORIENTED_EDGE('',*,*,#35273,.F.) ;
#45116 = ORIENTED_EDGE('',*,*,#35410,.T.) ;
#45117 = ORIENTED_EDGE('',*,*,#35276,.F.) ;
#45118 = ORIENTED_EDGE('',*,*,#35416,.F.) ;
#45119 = ORIENTED_EDGE('',*,*,#35280,.F.) ;
#45120 = ORIENTED_EDGE('',*,*,#35417,.F.) ;
#45121 = ORIENTED_EDGE('',*,*,#34816,.F.) ;
#45122 = ORIENTED_EDGE('',*,*,#35418,.F.) ;
#45123 = ORIENTED_EDGE('',*,*,#35277,.F.) ;
#45124 = ORIENTED_EDGE('',*,*,#35418,.T.) ;
#45125 = ORIENTED_EDGE('',*,*,#34815,.T.) ;
#45126 = ORIENTED_EDGE('',*,*,#35419,.F.) ;
#45127 = ORIENTED_EDGE('',*,*,#35411,.T.) ;
#45128 = ORIENTED_EDGE('',*,*,#34772,.T.) ;
#45129 = ORIENTED_EDGE('',*,*,#35412,.T.) ;
#45130 = ORIENTED_EDGE('',*,*,#35420,.F.) ;
#45131 = ORIENTED_EDGE('',*,*,#35414,.T.) ;
#45132 = ORIENTED_EDGE('',*,*,#34774,.T.) ;
#45133 = ORIENTED_EDGE('',*,*,#35413,.T.) ;
#45134 = ORIENTED_EDGE('',*,*,#35421,.F.) ;
#45135 = ORIENTED_EDGE('',*,*,#35415,.T.) ;
#45136 = ORIENTED_EDGE('',*,*,#35417,.T.) ;
#45137 = ORIENTED_EDGE('',*,*,#35416,.T.) ;
#45138 = ORIENTED_EDGE('',*,*,#35422,.F.) ;
#45139 = ORIENTED_EDGE('',*,*,#34817,.T.) ;
#45140 = ORIENTED_EDGE('',*,*,#35419,.T.) ;
#45141 = ORIENTED_EDGE('',*,*,#34814,.F.) ;
#45142 = ORIENTED_EDGE('',*,*,#35423,.F.) ;
#45143 = ORIENTED_EDGE('',*,*,#35267,.F.) ;
#45144 = ORIENTED_EDGE('',*,*,#35420,.T.) ;
#45145 = ORIENTED_EDGE('',*,*,#35268,.F.) ;
#45146 = ORIENTED_EDGE('',*,*,#35424,.F.) ;
#45147 = ORIENTED_EDGE('',*,*,#35270,.F.) ;
#45148 = ORIENTED_EDGE('',*,*,#35421,.T.) ;
#45149 = ORIENTED_EDGE('',*,*,#35272,.F.) ;
#45150 = ORIENTED_EDGE('',*,*,#35425,.F.) ;
#45151 = ORIENTED_EDGE('',*,*,#35274,.F.) ;
#45152 = ORIENTED_EDGE('',*,*,#35422,.T.) ;
#45153 = ORIENTED_EDGE('',*,*,#35275,.F.) ;
#45154 = ORIENTED_EDGE('',*,*,#35426,.F.) ;
#45155 = ORIENTED_EDGE('',*,*,#34818,.F.) ;
#45156 = ORIENTED_EDGE('',*,*,#35423,.T.) ;
#45157 = ORIENTED_EDGE('',*,*,#34813,.T.) ;
#45158 = ORIENTED_EDGE('',*,*,#35427,.F.) ;
#45159 = ORIENTED_EDGE('',*,*,#35424,.T.) ;
#45160 = ORIENTED_EDGE('',*,*,#35426,.T.) ;
#45161 = ORIENTED_EDGE('',*,*,#35425,.T.) ;
#45162 = ORIENTED_EDGE('',*,*,#35428,.F.) ;
#45163 = ORIENTED_EDGE('',*,*,#34819,.T.) ;
#45164 = ORIENTED_EDGE('',*,*,#35427,.T.) ;
#45165 = ORIENTED_EDGE('',*,*,#34820,.F.) ;
#45166 = ORIENTED_EDGE('',*,*,#35428,.T.) ;
#45167 = ORIENTED_EDGE('',*,*,#35271,.F.) ;
#45168 = ORIENTED_EDGE('',*,*,#35429,.F.) ;
#45169 = ORIENTED_EDGE('',*,*,#34785,.F.) ;
#45170 = ORIENTED_EDGE('',*,*,#35430,.F.) ;
#45171 = ORIENTED_EDGE('',*,*,#35251,.F.) ;
#45172 = ORIENTED_EDGE('',*,*,#34778,.T.) ;
#45173 = ORIENTED_EDGE('',*,*,#35429,.T.) ;
#45174 = ORIENTED_EDGE('',*,*,#35431,.F.) ;
#45175 = ORIENTED_EDGE('',*,*,#35432,.F.) ;
#45176 = ORIENTED_EDGE('',*,*,#35430,.T.) ;
#45177 = ORIENTED_EDGE('',*,*,#34784,.T.) ;
#45178 = ORIENTED_EDGE('',*,*,#35433,.F.) ;
#45179 = ORIENTED_EDGE('',*,*,#35434,.F.) ;
#45180 = ORIENTED_EDGE('',*,*,#35431,.T.) ;
#45181 = ORIENTED_EDGE('',*,*,#35250,.F.) ;
#45182 = ORIENTED_EDGE('',*,*,#35435,.F.) ;
#45183 = ORIENTED_EDGE('',*,*,#35254,.F.) ;
#45184 = ORIENTED_EDGE('',*,*,#35432,.T.) ;
#45185 = ORIENTED_EDGE('',*,*,#35253,.F.) ;
#45186 = ORIENTED_EDGE('',*,*,#35436,.F.) ;
#45187 = ORIENTED_EDGE('',*,*,#34779,.F.) ;
#45188 = ORIENTED_EDGE('',*,*,#35437,.F.) ;
#45189 = ORIENTED_EDGE('',*,*,#34781,.F.) ;
#45190 = ORIENTED_EDGE('',*,*,#35438,.F.) ;
#45191 = ORIENTED_EDGE('',*,*,#35257,.F.) ;
#45192 = ORIENTED_EDGE('',*,*,#35433,.T.) ;
#45193 = ORIENTED_EDGE('',*,*,#34783,.F.) ;
#45194 = ORIENTED_EDGE('',*,*,#35439,.F.) ;
#45195 = ORIENTED_EDGE('',*,*,#35261,.F.) ;
#45196 = ORIENTED_EDGE('',*,*,#35434,.T.) ;
#45197 = ORIENTED_EDGE('',*,*,#35264,.F.) ;
#45198 = ORIENTED_EDGE('',*,*,#35440,.F.) ;
#45199 = ORIENTED_EDGE('',*,*,#35252,.F.) ;
#45200 = ORIENTED_EDGE('',*,*,#35441,.F.) ;
#45201 = ORIENTED_EDGE('',*,*,#34824,.F.) ;
#45202 = ORIENTED_EDGE('',*,*,#35442,.F.) ;
#45203 = ORIENTED_EDGE('',*,*,#35249,.F.) ;
#45204 = ORIENTED_EDGE('',*,*,#35442,.T.) ;
#45205 = ORIENTED_EDGE('',*,*,#34823,.T.) ;
#45206 = ORIENTED_EDGE('',*,*,#35443,.F.) ;
#45207 = ORIENTED_EDGE('',*,*,#35435,.T.) ;
#45208 = ORIENTED_EDGE('',*,*,#34780,.T.) ;
#45209 = ORIENTED_EDGE('',*,*,#35436,.T.) ;
#45210 = ORIENTED_EDGE('',*,*,#35444,.F.) ;
#45211 = ORIENTED_EDGE('',*,*,#35438,.T.) ;
#45212 = ORIENTED_EDGE('',*,*,#34782,.T.) ;
#45213 = ORIENTED_EDGE('',*,*,#35437,.T.) ;
#45214 = ORIENTED_EDGE('',*,*,#35445,.F.) ;
#45215 = ORIENTED_EDGE('',*,*,#35439,.T.) ;
#45216 = ORIENTED_EDGE('',*,*,#35441,.T.) ;
#45217 = ORIENTED_EDGE('',*,*,#35440,.T.) ;
#45218 = ORIENTED_EDGE('',*,*,#35446,.F.) ;
#45219 = ORIENTED_EDGE('',*,*,#34825,.T.) ;
#45220 = ORIENTED_EDGE('',*,*,#35443,.T.) ;
#45221 = ORIENTED_EDGE('',*,*,#34822,.F.) ;
#45222 = ORIENTED_EDGE('',*,*,#35447,.F.) ;
#45223 = ORIENTED_EDGE('',*,*,#35255,.F.) ;
#45224 = ORIENTED_EDGE('',*,*,#35444,.T.) ;
#45225 = ORIENTED_EDGE('',*,*,#35256,.F.) ;
#45226 = ORIENTED_EDGE('',*,*,#35448,.F.) ;
#45227 = ORIENTED_EDGE('',*,*,#35258,.F.) ;
#45228 = ORIENTED_EDGE('',*,*,#35445,.T.) ;
#45229 = ORIENTED_EDGE('',*,*,#35260,.F.) ;
#45230 = ORIENTED_EDGE('',*,*,#35449,.F.) ;
#45231 = ORIENTED_EDGE('',*,*,#35262,.F.) ;
#45232 = ORIENTED_EDGE('',*,*,#35446,.T.) ;
#45233 = ORIENTED_EDGE('',*,*,#35263,.F.) ;
#45234 = ORIENTED_EDGE('',*,*,#35450,.F.) ;
#45235 = ORIENTED_EDGE('',*,*,#34826,.F.) ;
#45236 = ORIENTED_EDGE('',*,*,#35447,.T.) ;
#45237 = ORIENTED_EDGE('',*,*,#34821,.T.) ;
#45238 = ORIENTED_EDGE('',*,*,#35451,.F.) ;
#45239 = ORIENTED_EDGE('',*,*,#35448,.T.) ;
#45240 = ORIENTED_EDGE('',*,*,#35450,.T.) ;
#45241 = ORIENTED_EDGE('',*,*,#35449,.T.) ;
#45242 = ORIENTED_EDGE('',*,*,#35452,.F.) ;
#45243 = ORIENTED_EDGE('',*,*,#34827,.T.) ;
#45244 = ORIENTED_EDGE('',*,*,#35451,.T.) ;
#45245 = ORIENTED_EDGE('',*,*,#34828,.F.) ;
#45246 = ORIENTED_EDGE('',*,*,#35452,.T.) ;
#45247 = ORIENTED_EDGE('',*,*,#35259,.F.) ;
#45248 = ORIENTED_EDGE('',*,*,#35453,.F.) ;
#45249 = ORIENTED_EDGE('',*,*,#34769,.F.) ;
#45250 = ORIENTED_EDGE('',*,*,#35454,.F.) ;
#45251 = ORIENTED_EDGE('',*,*,#35235,.F.) ;
#45252 = ORIENTED_EDGE('',*,*,#34762,.T.) ;
#45253 = ORIENTED_EDGE('',*,*,#35453,.T.) ;
#45254 = ORIENTED_EDGE('',*,*,#35455,.F.) ;
#45255 = ORIENTED_EDGE('',*,*,#35456,.F.) ;
#45256 = ORIENTED_EDGE('',*,*,#35454,.T.) ;
#45257 = ORIENTED_EDGE('',*,*,#34768,.T.) ;
#45258 = ORIENTED_EDGE('',*,*,#35457,.F.) ;
#45259 = ORIENTED_EDGE('',*,*,#35458,.F.) ;
#45260 = ORIENTED_EDGE('',*,*,#35455,.T.) ;
#45261 = ORIENTED_EDGE('',*,*,#35234,.F.) ;
#45262 = ORIENTED_EDGE('',*,*,#35459,.F.) ;
#45263 = ORIENTED_EDGE('',*,*,#35246,.F.) ;
#45264 = ORIENTED_EDGE('',*,*,#35456,.T.) ;
#45265 = ORIENTED_EDGE('',*,*,#35245,.F.) ;
#45266 = ORIENTED_EDGE('',*,*,#35460,.F.) ;
#45267 = ORIENTED_EDGE('',*,*,#34763,.F.) ;
#45268 = ORIENTED_EDGE('',*,*,#35461,.F.) ;
#45269 = ORIENTED_EDGE('',*,*,#34765,.F.) ;
#45270 = ORIENTED_EDGE('',*,*,#35462,.F.) ;
#45271 = ORIENTED_EDGE('',*,*,#35241,.F.) ;
#45272 = ORIENTED_EDGE('',*,*,#35457,.T.) ;
#45273 = ORIENTED_EDGE('',*,*,#34767,.F.) ;
#45274 = ORIENTED_EDGE('',*,*,#35463,.F.) ;
#45275 = ORIENTED_EDGE('',*,*,#35237,.F.) ;
#45276 = ORIENTED_EDGE('',*,*,#35458,.T.) ;
#45277 = ORIENTED_EDGE('',*,*,#35240,.F.) ;
#45278 = ORIENTED_EDGE('',*,*,#35464,.F.) ;
#45279 = ORIENTED_EDGE('',*,*,#35236,.F.) ;
#45280 = ORIENTED_EDGE('',*,*,#35465,.F.) ;
#45281 = ORIENTED_EDGE('',*,*,#34808,.F.) ;
#45282 = ORIENTED_EDGE('',*,*,#35466,.F.) ;
#45283 = ORIENTED_EDGE('',*,*,#35233,.F.) ;
#45284 = ORIENTED_EDGE('',*,*,#35466,.T.) ;
#45285 = ORIENTED_EDGE('',*,*,#34807,.T.) ;
#45286 = ORIENTED_EDGE('',*,*,#35467,.F.) ;
#45287 = ORIENTED_EDGE('',*,*,#35459,.T.) ;
#45288 = ORIENTED_EDGE('',*,*,#34764,.T.) ;
#45289 = ORIENTED_EDGE('',*,*,#35460,.T.) ;
#45290 = ORIENTED_EDGE('',*,*,#35468,.F.) ;
#45291 = ORIENTED_EDGE('',*,*,#35462,.T.) ;
#45292 = ORIENTED_EDGE('',*,*,#34766,.T.) ;
#45293 = ORIENTED_EDGE('',*,*,#35461,.T.) ;
#45294 = ORIENTED_EDGE('',*,*,#35469,.F.) ;
#45295 = ORIENTED_EDGE('',*,*,#35463,.T.) ;
#45296 = ORIENTED_EDGE('',*,*,#35465,.T.) ;
#45297 = ORIENTED_EDGE('',*,*,#35464,.T.) ;
#45298 = ORIENTED_EDGE('',*,*,#35470,.F.) ;
#45299 = ORIENTED_EDGE('',*,*,#34809,.T.) ;
#45300 = ORIENTED_EDGE('',*,*,#35467,.T.) ;
#45301 = ORIENTED_EDGE('',*,*,#34806,.F.) ;
#45302 = ORIENTED_EDGE('',*,*,#35471,.F.) ;
#45303 = ORIENTED_EDGE('',*,*,#35247,.F.) ;
#45304 = ORIENTED_EDGE('',*,*,#35468,.T.) ;
#45305 = ORIENTED_EDGE('',*,*,#35248,.F.) ;
#45306 = ORIENTED_EDGE('',*,*,#35472,.F.) ;
#45307 = ORIENTED_EDGE('',*,*,#35242,.F.) ;
#45308 = ORIENTED_EDGE('',*,*,#35469,.T.) ;
#45309 = ORIENTED_EDGE('',*,*,#35244,.F.) ;
#45310 = ORIENTED_EDGE('',*,*,#35473,.F.) ;
#45311 = ORIENTED_EDGE('',*,*,#35238,.F.) ;
#45312 = ORIENTED_EDGE('',*,*,#35470,.T.) ;
#45313 = ORIENTED_EDGE('',*,*,#35239,.F.) ;
#45314 = ORIENTED_EDGE('',*,*,#35474,.F.) ;
#45315 = ORIENTED_EDGE('',*,*,#34810,.F.) ;
#45316 = ORIENTED_EDGE('',*,*,#35471,.T.) ;
#45317 = ORIENTED_EDGE('',*,*,#34805,.T.) ;
#45318 = ORIENTED_EDGE('',*,*,#35475,.F.) ;
#45319 = ORIENTED_EDGE('',*,*,#35472,.T.) ;
#45320 = ORIENTED_EDGE('',*,*,#35474,.T.) ;
#45321 = ORIENTED_EDGE('',*,*,#35473,.T.) ;
#45322 = ORIENTED_EDGE('',*,*,#35476,.F.) ;
#45323 = ORIENTED_EDGE('',*,*,#34811,.T.) ;
#45324 = ORIENTED_EDGE('',*,*,#35475,.T.) ;
#45325 = ORIENTED_EDGE('',*,*,#34812,.F.) ;
#45326 = ORIENTED_EDGE('',*,*,#35476,.T.) ;
#45327 = ORIENTED_EDGE('',*,*,#35243,.F.) ;
#45328 = ORIENTED_EDGE('',*,*,#35477,.F.) ;
#45329 = ORIENTED_EDGE('',*,*,#34793,.F.) ;
#45330 = ORIENTED_EDGE('',*,*,#35478,.F.) ;
#45331 = ORIENTED_EDGE('',*,*,#35219,.F.) ;
#45332 = ORIENTED_EDGE('',*,*,#34786,.T.) ;
#45333 = ORIENTED_EDGE('',*,*,#35477,.T.) ;
#45334 = ORIENTED_EDGE('',*,*,#35479,.F.) ;
#45335 = ORIENTED_EDGE('',*,*,#35480,.F.) ;
#45336 = ORIENTED_EDGE('',*,*,#35478,.T.) ;
#45337 = ORIENTED_EDGE('',*,*,#34792,.T.) ;
#45338 = ORIENTED_EDGE('',*,*,#35481,.F.) ;
#45339 = ORIENTED_EDGE('',*,*,#35482,.F.) ;
#45340 = ORIENTED_EDGE('',*,*,#35479,.T.) ;
#45341 = ORIENTED_EDGE('',*,*,#35218,.F.) ;
#45342 = ORIENTED_EDGE('',*,*,#35483,.F.) ;
#45343 = ORIENTED_EDGE('',*,*,#35222,.F.) ;
#45344 = ORIENTED_EDGE('',*,*,#35480,.T.) ;
#45345 = ORIENTED_EDGE('',*,*,#35221,.F.) ;
#45346 = ORIENTED_EDGE('',*,*,#35484,.F.) ;
#45347 = ORIENTED_EDGE('',*,*,#34787,.F.) ;
#45348 = ORIENTED_EDGE('',*,*,#35485,.F.) ;
#45349 = ORIENTED_EDGE('',*,*,#34789,.F.) ;
#45350 = ORIENTED_EDGE('',*,*,#35486,.F.) ;
#45351 = ORIENTED_EDGE('',*,*,#35225,.F.) ;
#45352 = ORIENTED_EDGE('',*,*,#35481,.T.) ;
#45353 = ORIENTED_EDGE('',*,*,#34791,.F.) ;
#45354 = ORIENTED_EDGE('',*,*,#35487,.F.) ;
#45355 = ORIENTED_EDGE('',*,*,#35229,.F.) ;
#45356 = ORIENTED_EDGE('',*,*,#35482,.T.) ;
#45357 = ORIENTED_EDGE('',*,*,#35232,.F.) ;
#45358 = ORIENTED_EDGE('',*,*,#35488,.F.) ;
#45359 = ORIENTED_EDGE('',*,*,#35220,.F.) ;
#45360 = ORIENTED_EDGE('',*,*,#35489,.F.) ;
#45361 = ORIENTED_EDGE('',*,*,#34832,.F.) ;
#45362 = ORIENTED_EDGE('',*,*,#35490,.F.) ;
#45363 = ORIENTED_EDGE('',*,*,#35217,.F.) ;
#45364 = ORIENTED_EDGE('',*,*,#35490,.T.) ;
#45365 = ORIENTED_EDGE('',*,*,#34831,.T.) ;
#45366 = ORIENTED_EDGE('',*,*,#35491,.F.) ;
#45367 = ORIENTED_EDGE('',*,*,#35483,.T.) ;
#45368 = ORIENTED_EDGE('',*,*,#34788,.T.) ;
#45369 = ORIENTED_EDGE('',*,*,#35484,.T.) ;
#45370 = ORIENTED_EDGE('',*,*,#35492,.F.) ;
#45371 = ORIENTED_EDGE('',*,*,#35486,.T.) ;
#45372 = ORIENTED_EDGE('',*,*,#34790,.T.) ;
#45373 = ORIENTED_EDGE('',*,*,#35485,.T.) ;
#45374 = ORIENTED_EDGE('',*,*,#35493,.F.) ;
#45375 = ORIENTED_EDGE('',*,*,#35487,.T.) ;
#45376 = ORIENTED_EDGE('',*,*,#35489,.T.) ;
#45377 = ORIENTED_EDGE('',*,*,#35488,.T.) ;
#45378 = ORIENTED_EDGE('',*,*,#35494,.F.) ;
#45379 = ORIENTED_EDGE('',*,*,#34833,.T.) ;
#45380 = ORIENTED_EDGE('',*,*,#35491,.T.) ;
#45381 = ORIENTED_EDGE('',*,*,#34830,.F.) ;
#45382 = ORIENTED_EDGE('',*,*,#35495,.F.) ;
#45383 = ORIENTED_EDGE('',*,*,#35223,.F.) ;
#45384 = ORIENTED_EDGE('',*,*,#35492,.T.) ;
#45385 = ORIENTED_EDGE('',*,*,#35224,.F.) ;
#45386 = ORIENTED_EDGE('',*,*,#35496,.F.) ;
#45387 = ORIENTED_EDGE('',*,*,#35226,.F.) ;
#45388 = ORIENTED_EDGE('',*,*,#35493,.T.) ;
#45389 = ORIENTED_EDGE('',*,*,#35228,.F.) ;
#45390 = ORIENTED_EDGE('',*,*,#35497,.F.) ;
#45391 = ORIENTED_EDGE('',*,*,#35230,.F.) ;
#45392 = ORIENTED_EDGE('',*,*,#35494,.T.) ;
#45393 = ORIENTED_EDGE('',*,*,#35231,.F.) ;
#45394 = ORIENTED_EDGE('',*,*,#35498,.F.) ;
#45395 = ORIENTED_EDGE('',*,*,#34834,.F.) ;
#45396 = ORIENTED_EDGE('',*,*,#35495,.T.) ;
#45397 = ORIENTED_EDGE('',*,*,#34829,.T.) ;
#45398 = ORIENTED_EDGE('',*,*,#35499,.F.) ;
#45399 = ORIENTED_EDGE('',*,*,#35496,.T.) ;
#45400 = ORIENTED_EDGE('',*,*,#35498,.T.) ;
#45401 = ORIENTED_EDGE('',*,*,#35497,.T.) ;
#45402 = ORIENTED_EDGE('',*,*,#35500,.F.) ;
#45403 = ORIENTED_EDGE('',*,*,#34835,.T.) ;
#45404 = ORIENTED_EDGE('',*,*,#35499,.T.) ;
#45405 = ORIENTED_EDGE('',*,*,#34836,.F.) ;
#45406 = ORIENTED_EDGE('',*,*,#35500,.T.) ;
#45407 = ORIENTED_EDGE('',*,*,#35227,.F.) ;
#45408 = ORIENTED_EDGE('',*,*,#35501,.F.) ;
#45409 = ORIENTED_EDGE('',*,*,#34732,.F.) ;
#45410 = ORIENTED_EDGE('',*,*,#35502,.F.) ;
#45411 = ORIENTED_EDGE('',*,*,#35285,.F.) ;
#45412 = ORIENTED_EDGE('',*,*,#35502,.T.) ;
#45413 = ORIENTED_EDGE('',*,*,#34731,.T.) ;
#45414 = ORIENTED_EDGE('',*,*,#35503,.F.) ;
#45415 = ORIENTED_EDGE('',*,*,#35504,.F.) ;
#45416 = ORIENTED_EDGE('',*,*,#34733,.T.) ;
#45417 = ORIENTED_EDGE('',*,*,#35501,.T.) ;
#45418 = ORIENTED_EDGE('',*,*,#35505,.F.) ;
#45419 = ORIENTED_EDGE('',*,*,#35506,.F.) ;
#45420 = ORIENTED_EDGE('',*,*,#35503,.T.) ;
#45421 = ORIENTED_EDGE('',*,*,#34730,.F.) ;
#45422 = ORIENTED_EDGE('',*,*,#35507,.F.) ;
#45423 = ORIENTED_EDGE('',*,*,#35284,.F.) ;
#45424 = ORIENTED_EDGE('',*,*,#35504,.T.) ;
#45425 = ORIENTED_EDGE('',*,*,#35283,.F.) ;
#45426 = ORIENTED_EDGE('',*,*,#35508,.F.) ;
#45427 = ORIENTED_EDGE('',*,*,#35286,.F.) ;
#45428 = ORIENTED_EDGE('',*,*,#35509,.F.) ;
#45429 = ORIENTED_EDGE('',*,*,#35287,.F.) ;
#45430 = ORIENTED_EDGE('',*,*,#35510,.F.) ;
#45431 = ORIENTED_EDGE('',*,*,#34750,.F.) ;
#45432 = ORIENTED_EDGE('',*,*,#35505,.T.) ;
#45433 = ORIENTED_EDGE('',*,*,#35288,.F.) ;
#45434 = ORIENTED_EDGE('',*,*,#35511,.F.) ;
#45435 = ORIENTED_EDGE('',*,*,#35289,.F.) ;
#45436 = ORIENTED_EDGE('',*,*,#35506,.T.) ;
#45437 = ORIENTED_EDGE('',*,*,#35292,.F.) ;
#45438 = ORIENTED_EDGE('',*,*,#35512,.F.) ;
#45439 = ORIENTED_EDGE('',*,*,#34734,.F.) ;
#45440 = ORIENTED_EDGE('',*,*,#35513,.F.) ;
#45441 = ORIENTED_EDGE('',*,*,#34736,.F.) ;
#45442 = ORIENTED_EDGE('',*,*,#35514,.F.) ;
#45443 = ORIENTED_EDGE('',*,*,#35295,.F.) ;
#45444 = ORIENTED_EDGE('',*,*,#34729,.T.) ;
#45445 = ORIENTED_EDGE('',*,*,#35513,.T.) ;
#45446 = ORIENTED_EDGE('',*,*,#35515,.F.) ;
#45447 = ORIENTED_EDGE('',*,*,#35507,.T.) ;
#45448 = ORIENTED_EDGE('',*,*,#35510,.T.) ;
#45449 = ORIENTED_EDGE('',*,*,#35508,.T.) ;
#45450 = ORIENTED_EDGE('',*,*,#35516,.F.) ;
#45451 = ORIENTED_EDGE('',*,*,#34743,.T.) ;
#45452 = ORIENTED_EDGE('',*,*,#35509,.T.) ;
#45453 = ORIENTED_EDGE('',*,*,#34749,.T.) ;
#45454 = ORIENTED_EDGE('',*,*,#35517,.F.) ;
#45455 = ORIENTED_EDGE('',*,*,#35511,.T.) ;
#45456 = ORIENTED_EDGE('',*,*,#34735,.T.) ;
#45457 = ORIENTED_EDGE('',*,*,#35512,.T.) ;
#45458 = ORIENTED_EDGE('',*,*,#35518,.F.) ;
#45459 = ORIENTED_EDGE('',*,*,#35514,.T.) ;
#45460 = ORIENTED_EDGE('',*,*,#35515,.T.) ;
#45461 = ORIENTED_EDGE('',*,*,#35294,.F.) ;
#45462 = ORIENTED_EDGE('',*,*,#35519,.F.) ;
#45463 = ORIENTED_EDGE('',*,*,#35281,.F.) ;
#45464 = ORIENTED_EDGE('',*,*,#35516,.T.) ;
#45465 = ORIENTED_EDGE('',*,*,#35282,.F.) ;
#45466 = ORIENTED_EDGE('',*,*,#35520,.F.) ;
#45467 = ORIENTED_EDGE('',*,*,#34744,.F.) ;
#45468 = ORIENTED_EDGE('',*,*,#35517,.T.) ;
#45469 = ORIENTED_EDGE('',*,*,#34748,.F.) ;
#45470 = ORIENTED_EDGE('',*,*,#35521,.F.) ;
#45471 = ORIENTED_EDGE('',*,*,#35290,.F.) ;
#45472 = ORIENTED_EDGE('',*,*,#35518,.T.) ;
#45473 = ORIENTED_EDGE('',*,*,#35291,.F.) ;
#45474 = ORIENTED_EDGE('',*,*,#35522,.F.) ;
#45475 = ORIENTED_EDGE('',*,*,#35296,.F.) ;
#45476 = ORIENTED_EDGE('',*,*,#35520,.T.) ;
#45477 = ORIENTED_EDGE('',*,*,#35519,.T.) ;
#45478 = ORIENTED_EDGE('',*,*,#35523,.F.) ;
#45479 = ORIENTED_EDGE('',*,*,#34745,.T.) ;
#45480 = ORIENTED_EDGE('',*,*,#35521,.T.) ;
#45481 = ORIENTED_EDGE('',*,*,#34747,.T.) ;
#45482 = ORIENTED_EDGE('',*,*,#35524,.F.) ;
#45483 = ORIENTED_EDGE('',*,*,#35522,.T.) ;
#45484 = ORIENTED_EDGE('',*,*,#35523,.T.) ;
#45485 = ORIENTED_EDGE('',*,*,#35293,.F.) ;
#45486 = ORIENTED_EDGE('',*,*,#35524,.T.) ;
#45487 = ORIENTED_EDGE('',*,*,#34746,.F.) ;
#45488 = ORIENTED_EDGE('',*,*,#35525,.F.) ;
#45489 = ORIENTED_EDGE('',*,*,#34879,.F.) ;
#45490 = ORIENTED_EDGE('',*,*,#35526,.F.) ;
#45491 = ORIENTED_EDGE('',*,*,#35115,.F.) ;
#45492 = ORIENTED_EDGE('',*,*,#34872,.T.) ;
#45493 = ORIENTED_EDGE('',*,*,#35525,.T.) ;
#45494 = ORIENTED_EDGE('',*,*,#35527,.F.) ;
#45495 = ORIENTED_EDGE('',*,*,#35528,.F.) ;
#45496 = ORIENTED_EDGE('',*,*,#35526,.T.) ;
#45497 = ORIENTED_EDGE('',*,*,#34878,.T.) ;
#45498 = ORIENTED_EDGE('',*,*,#35529,.F.) ;
#45499 = ORIENTED_EDGE('',*,*,#35530,.F.) ;
#45500 = ORIENTED_EDGE('',*,*,#35527,.T.) ;
#45501 = ORIENTED_EDGE('',*,*,#35114,.F.) ;
#45502 = ORIENTED_EDGE('',*,*,#35531,.F.) ;
#45503 = ORIENTED_EDGE('',*,*,#35118,.F.) ;
#45504 = ORIENTED_EDGE('',*,*,#35528,.T.) ;
#45505 = ORIENTED_EDGE('',*,*,#35117,.F.) ;
#45506 = ORIENTED_EDGE('',*,*,#35532,.F.) ;
#45507 = ORIENTED_EDGE('',*,*,#34873,.F.) ;
#45508 = ORIENTED_EDGE('',*,*,#35533,.F.) ;
#45509 = ORIENTED_EDGE('',*,*,#34875,.F.) ;
#45510 = ORIENTED_EDGE('',*,*,#35534,.F.) ;
#45511 = ORIENTED_EDGE('',*,*,#35105,.F.) ;
#45512 = ORIENTED_EDGE('',*,*,#35529,.T.) ;
#45513 = ORIENTED_EDGE('',*,*,#34877,.F.) ;
#45514 = ORIENTED_EDGE('',*,*,#35535,.F.) ;
#45515 = ORIENTED_EDGE('',*,*,#35109,.F.) ;
#45516 = ORIENTED_EDGE('',*,*,#35530,.T.) ;
#45517 = ORIENTED_EDGE('',*,*,#35112,.F.) ;
#45518 = ORIENTED_EDGE('',*,*,#35536,.F.) ;
#45519 = ORIENTED_EDGE('',*,*,#35116,.F.) ;
#45520 = ORIENTED_EDGE('',*,*,#35537,.F.) ;
#45521 = ORIENTED_EDGE('',*,*,#34942,.F.) ;
#45522 = ORIENTED_EDGE('',*,*,#35538,.F.) ;
#45523 = ORIENTED_EDGE('',*,*,#35113,.F.) ;
#45524 = ORIENTED_EDGE('',*,*,#35538,.T.) ;
#45525 = ORIENTED_EDGE('',*,*,#34941,.T.) ;
#45526 = ORIENTED_EDGE('',*,*,#35539,.F.) ;
#45527 = ORIENTED_EDGE('',*,*,#35531,.T.) ;
#45528 = ORIENTED_EDGE('',*,*,#34874,.T.) ;
#45529 = ORIENTED_EDGE('',*,*,#35532,.T.) ;
#45530 = ORIENTED_EDGE('',*,*,#35540,.F.) ;
#45531 = ORIENTED_EDGE('',*,*,#35534,.T.) ;
#45532 = ORIENTED_EDGE('',*,*,#34876,.T.) ;
#45533 = ORIENTED_EDGE('',*,*,#35533,.T.) ;
#45534 = ORIENTED_EDGE('',*,*,#35541,.F.) ;
#45535 = ORIENTED_EDGE('',*,*,#35535,.T.) ;
#45536 = ORIENTED_EDGE('',*,*,#35537,.T.) ;
#45537 = ORIENTED_EDGE('',*,*,#35536,.T.) ;
#45538 = ORIENTED_EDGE('',*,*,#35542,.F.) ;
#45539 = ORIENTED_EDGE('',*,*,#34943,.T.) ;
#45540 = ORIENTED_EDGE('',*,*,#35539,.T.) ;
#45541 = ORIENTED_EDGE('',*,*,#34940,.F.) ;
#45542 = ORIENTED_EDGE('',*,*,#35543,.F.) ;
#45543 = ORIENTED_EDGE('',*,*,#35119,.F.) ;
#45544 = ORIENTED_EDGE('',*,*,#35540,.T.) ;
#45545 = ORIENTED_EDGE('',*,*,#35120,.F.) ;
#45546 = ORIENTED_EDGE('',*,*,#35544,.F.) ;
#45547 = ORIENTED_EDGE('',*,*,#35106,.F.) ;
#45548 = ORIENTED_EDGE('',*,*,#35541,.T.) ;
#45549 = ORIENTED_EDGE('',*,*,#35108,.F.) ;
#45550 = ORIENTED_EDGE('',*,*,#35545,.F.) ;
#45551 = ORIENTED_EDGE('',*,*,#35110,.F.) ;
#45552 = ORIENTED_EDGE('',*,*,#35542,.T.) ;
#45553 = ORIENTED_EDGE('',*,*,#35111,.F.) ;
#45554 = ORIENTED_EDGE('',*,*,#35546,.F.) ;
#45555 = ORIENTED_EDGE('',*,*,#34944,.F.) ;
#45556 = ORIENTED_EDGE('',*,*,#35543,.T.) ;
#45557 = ORIENTED_EDGE('',*,*,#34939,.T.) ;
#45558 = ORIENTED_EDGE('',*,*,#35547,.F.) ;
#45559 = ORIENTED_EDGE('',*,*,#35544,.T.) ;
#45560 = ORIENTED_EDGE('',*,*,#35546,.T.) ;
#45561 = ORIENTED_EDGE('',*,*,#35545,.T.) ;
#45562 = ORIENTED_EDGE('',*,*,#35548,.F.) ;
#45563 = ORIENTED_EDGE('',*,*,#34945,.T.) ;
#45564 = ORIENTED_EDGE('',*,*,#35547,.T.) ;
#45565 = ORIENTED_EDGE('',*,*,#34946,.F.) ;
#45566 = ORIENTED_EDGE('',*,*,#35548,.T.) ;
#45567 = ORIENTED_EDGE('',*,*,#35107,.F.) ;
#45568 = ORIENTED_EDGE('',*,*,#35549,.F.) ;
#45569 = ORIENTED_EDGE('',*,*,#34887,.F.) ;
#45570 = ORIENTED_EDGE('',*,*,#35550,.F.) ;
#45571 = ORIENTED_EDGE('',*,*,#35131,.F.) ;
#45572 = ORIENTED_EDGE('',*,*,#34880,.T.) ;
#45573 = ORIENTED_EDGE('',*,*,#35549,.T.) ;
#45574 = ORIENTED_EDGE('',*,*,#35551,.F.) ;
#45575 = ORIENTED_EDGE('',*,*,#35552,.F.) ;
#45576 = ORIENTED_EDGE('',*,*,#35550,.T.) ;
#45577 = ORIENTED_EDGE('',*,*,#34886,.T.) ;
#45578 = ORIENTED_EDGE('',*,*,#35553,.F.) ;
#45579 = ORIENTED_EDGE('',*,*,#35554,.F.) ;
#45580 = ORIENTED_EDGE('',*,*,#35551,.T.) ;
#45581 = ORIENTED_EDGE('',*,*,#35130,.F.) ;
#45582 = ORIENTED_EDGE('',*,*,#35555,.F.) ;
#45583 = ORIENTED_EDGE('',*,*,#35134,.F.) ;
#45584 = ORIENTED_EDGE('',*,*,#35552,.T.) ;
#45585 = ORIENTED_EDGE('',*,*,#35133,.F.) ;
#45586 = ORIENTED_EDGE('',*,*,#35556,.F.) ;
#45587 = ORIENTED_EDGE('',*,*,#34881,.F.) ;
#45588 = ORIENTED_EDGE('',*,*,#35557,.F.) ;
#45589 = ORIENTED_EDGE('',*,*,#34883,.F.) ;
#45590 = ORIENTED_EDGE('',*,*,#35558,.F.) ;
#45591 = ORIENTED_EDGE('',*,*,#35121,.F.) ;
#45592 = ORIENTED_EDGE('',*,*,#35553,.T.) ;
#45593 = ORIENTED_EDGE('',*,*,#34885,.F.) ;
#45594 = ORIENTED_EDGE('',*,*,#35559,.F.) ;
#45595 = ORIENTED_EDGE('',*,*,#35125,.F.) ;
#45596 = ORIENTED_EDGE('',*,*,#35554,.T.) ;
#45597 = ORIENTED_EDGE('',*,*,#35128,.F.) ;
#45598 = ORIENTED_EDGE('',*,*,#35560,.F.) ;
#45599 = ORIENTED_EDGE('',*,*,#35132,.F.) ;
#45600 = ORIENTED_EDGE('',*,*,#35561,.F.) ;
#45601 = ORIENTED_EDGE('',*,*,#34950,.F.) ;
#45602 = ORIENTED_EDGE('',*,*,#35562,.F.) ;
#45603 = ORIENTED_EDGE('',*,*,#35129,.F.) ;
#45604 = ORIENTED_EDGE('',*,*,#35562,.T.) ;
#45605 = ORIENTED_EDGE('',*,*,#34949,.T.) ;
#45606 = ORIENTED_EDGE('',*,*,#35563,.F.) ;
#45607 = ORIENTED_EDGE('',*,*,#35555,.T.) ;
#45608 = ORIENTED_EDGE('',*,*,#34882,.T.) ;
#45609 = ORIENTED_EDGE('',*,*,#35556,.T.) ;
#45610 = ORIENTED_EDGE('',*,*,#35564,.F.) ;
#45611 = ORIENTED_EDGE('',*,*,#35558,.T.) ;
#45612 = ORIENTED_EDGE('',*,*,#34884,.T.) ;
#45613 = ORIENTED_EDGE('',*,*,#35557,.T.) ;
#45614 = ORIENTED_EDGE('',*,*,#35565,.F.) ;
#45615 = ORIENTED_EDGE('',*,*,#35559,.T.) ;
#45616 = ORIENTED_EDGE('',*,*,#35561,.T.) ;
#45617 = ORIENTED_EDGE('',*,*,#35560,.T.) ;
#45618 = ORIENTED_EDGE('',*,*,#35566,.F.) ;
#45619 = ORIENTED_EDGE('',*,*,#34951,.T.) ;
#45620 = ORIENTED_EDGE('',*,*,#35563,.T.) ;
#45621 = ORIENTED_EDGE('',*,*,#34948,.F.) ;
#45622 = ORIENTED_EDGE('',*,*,#35567,.F.) ;
#45623 = ORIENTED_EDGE('',*,*,#35135,.F.) ;
#45624 = ORIENTED_EDGE('',*,*,#35564,.T.) ;
#45625 = ORIENTED_EDGE('',*,*,#35136,.F.) ;
#45626 = ORIENTED_EDGE('',*,*,#35568,.F.) ;
#45627 = ORIENTED_EDGE('',*,*,#35122,.F.) ;
#45628 = ORIENTED_EDGE('',*,*,#35565,.T.) ;
#45629 = ORIENTED_EDGE('',*,*,#35124,.F.) ;
#45630 = ORIENTED_EDGE('',*,*,#35569,.F.) ;
#45631 = ORIENTED_EDGE('',*,*,#35126,.F.) ;
#45632 = ORIENTED_EDGE('',*,*,#35566,.T.) ;
#45633 = ORIENTED_EDGE('',*,*,#35127,.F.) ;
#45634 = ORIENTED_EDGE('',*,*,#35570,.F.) ;
#45635 = ORIENTED_EDGE('',*,*,#34952,.F.) ;
#45636 = ORIENTED_EDGE('',*,*,#35567,.T.) ;
#45637 = ORIENTED_EDGE('',*,*,#34947,.T.) ;
#45638 = ORIENTED_EDGE('',*,*,#35571,.F.) ;
#45639 = ORIENTED_EDGE('',*,*,#35568,.T.) ;
#45640 = ORIENTED_EDGE('',*,*,#35570,.T.) ;
#45641 = ORIENTED_EDGE('',*,*,#35569,.T.) ;
#45642 = ORIENTED_EDGE('',*,*,#35572,.F.) ;
#45643 = ORIENTED_EDGE('',*,*,#34953,.T.) ;
#45644 = ORIENTED_EDGE('',*,*,#35571,.T.) ;
#45645 = ORIENTED_EDGE('',*,*,#34954,.F.) ;
#45646 = ORIENTED_EDGE('',*,*,#35572,.T.) ;
#45647 = ORIENTED_EDGE('',*,*,#35123,.F.) ;
#45648 = ORIENTED_EDGE('',*,*,#35573,.F.) ;
#45649 = ORIENTED_EDGE('',*,*,#34871,.F.) ;
#45650 = ORIENTED_EDGE('',*,*,#35574,.F.) ;
#45651 = ORIENTED_EDGE('',*,*,#35147,.F.) ;
#45652 = ORIENTED_EDGE('',*,*,#34864,.T.) ;
#45653 = ORIENTED_EDGE('',*,*,#35573,.T.) ;
#45654 = ORIENTED_EDGE('',*,*,#35575,.F.) ;
#45655 = ORIENTED_EDGE('',*,*,#35576,.F.) ;
#45656 = ORIENTED_EDGE('',*,*,#35574,.T.) ;
#45657 = ORIENTED_EDGE('',*,*,#34870,.T.) ;
#45658 = ORIENTED_EDGE('',*,*,#35577,.F.) ;
#45659 = ORIENTED_EDGE('',*,*,#35578,.F.) ;
#45660 = ORIENTED_EDGE('',*,*,#35575,.T.) ;
#45661 = ORIENTED_EDGE('',*,*,#35146,.F.) ;
#45662 = ORIENTED_EDGE('',*,*,#35579,.F.) ;
#45663 = ORIENTED_EDGE('',*,*,#35150,.F.) ;
#45664 = ORIENTED_EDGE('',*,*,#35576,.T.) ;
#45665 = ORIENTED_EDGE('',*,*,#35149,.F.) ;
#45666 = ORIENTED_EDGE('',*,*,#35580,.F.) ;
#45667 = ORIENTED_EDGE('',*,*,#34865,.F.) ;
#45668 = ORIENTED_EDGE('',*,*,#35581,.F.) ;
#45669 = ORIENTED_EDGE('',*,*,#34867,.F.) ;
#45670 = ORIENTED_EDGE('',*,*,#35582,.F.) ;
#45671 = ORIENTED_EDGE('',*,*,#35137,.F.) ;
#45672 = ORIENTED_EDGE('',*,*,#35577,.T.) ;
#45673 = ORIENTED_EDGE('',*,*,#34869,.F.) ;
#45674 = ORIENTED_EDGE('',*,*,#35583,.F.) ;
#45675 = ORIENTED_EDGE('',*,*,#35141,.F.) ;
#45676 = ORIENTED_EDGE('',*,*,#35578,.T.) ;
#45677 = ORIENTED_EDGE('',*,*,#35144,.F.) ;
#45678 = ORIENTED_EDGE('',*,*,#35584,.F.) ;
#45679 = ORIENTED_EDGE('',*,*,#35148,.F.) ;
#45680 = ORIENTED_EDGE('',*,*,#35585,.F.) ;
#45681 = ORIENTED_EDGE('',*,*,#34934,.F.) ;
#45682 = ORIENTED_EDGE('',*,*,#35586,.F.) ;
#45683 = ORIENTED_EDGE('',*,*,#35145,.F.) ;
#45684 = ORIENTED_EDGE('',*,*,#35586,.T.) ;
#45685 = ORIENTED_EDGE('',*,*,#34933,.T.) ;
#45686 = ORIENTED_EDGE('',*,*,#35587,.F.) ;
#45687 = ORIENTED_EDGE('',*,*,#35579,.T.) ;
#45688 = ORIENTED_EDGE('',*,*,#34866,.T.) ;
#45689 = ORIENTED_EDGE('',*,*,#35580,.T.) ;
#45690 = ORIENTED_EDGE('',*,*,#35588,.F.) ;
#45691 = ORIENTED_EDGE('',*,*,#35582,.T.) ;
#45692 = ORIENTED_EDGE('',*,*,#34868,.T.) ;
#45693 = ORIENTED_EDGE('',*,*,#35581,.T.) ;
#45694 = ORIENTED_EDGE('',*,*,#35589,.F.) ;
#45695 = ORIENTED_EDGE('',*,*,#35583,.T.) ;
#45696 = ORIENTED_EDGE('',*,*,#35585,.T.) ;
#45697 = ORIENTED_EDGE('',*,*,#35584,.T.) ;
#45698 = ORIENTED_EDGE('',*,*,#35590,.F.) ;
#45699 = ORIENTED_EDGE('',*,*,#34935,.T.) ;
#45700 = ORIENTED_EDGE('',*,*,#35587,.T.) ;
#45701 = ORIENTED_EDGE('',*,*,#34932,.F.) ;
#45702 = ORIENTED_EDGE('',*,*,#35591,.F.) ;
#45703 = ORIENTED_EDGE('',*,*,#35151,.F.) ;
#45704 = ORIENTED_EDGE('',*,*,#35588,.T.) ;
#45705 = ORIENTED_EDGE('',*,*,#35152,.F.) ;
#45706 = ORIENTED_EDGE('',*,*,#35592,.F.) ;
#45707 = ORIENTED_EDGE('',*,*,#35138,.F.) ;
#45708 = ORIENTED_EDGE('',*,*,#35589,.T.) ;
#45709 = ORIENTED_EDGE('',*,*,#35140,.F.) ;
#45710 = ORIENTED_EDGE('',*,*,#35593,.F.) ;
#45711 = ORIENTED_EDGE('',*,*,#35142,.F.) ;
#45712 = ORIENTED_EDGE('',*,*,#35590,.T.) ;
#45713 = ORIENTED_EDGE('',*,*,#35143,.F.) ;
#45714 = ORIENTED_EDGE('',*,*,#35594,.F.) ;
#45715 = ORIENTED_EDGE('',*,*,#34936,.F.) ;
#45716 = ORIENTED_EDGE('',*,*,#35591,.T.) ;
#45717 = ORIENTED_EDGE('',*,*,#34931,.T.) ;
#45718 = ORIENTED_EDGE('',*,*,#35595,.F.) ;
#45719 = ORIENTED_EDGE('',*,*,#35592,.T.) ;
#45720 = ORIENTED_EDGE('',*,*,#35594,.T.) ;
#45721 = ORIENTED_EDGE('',*,*,#35593,.T.) ;
#45722 = ORIENTED_EDGE('',*,*,#35596,.F.) ;
#45723 = ORIENTED_EDGE('',*,*,#34937,.T.) ;
#45724 = ORIENTED_EDGE('',*,*,#35595,.T.) ;
#45725 = ORIENTED_EDGE('',*,*,#34938,.F.) ;
#45726 = ORIENTED_EDGE('',*,*,#35596,.T.) ;
#45727 = ORIENTED_EDGE('',*,*,#35139,.F.) ;
#45728 = ORIENTED_EDGE('',*,*,#35597,.F.) ;
#45729 = ORIENTED_EDGE('',*,*,#34895,.F.) ;
#45730 = ORIENTED_EDGE('',*,*,#35598,.F.) ;
#45731 = ORIENTED_EDGE('',*,*,#35163,.F.) ;
#45732 = ORIENTED_EDGE('',*,*,#34888,.T.) ;
#45733 = ORIENTED_EDGE('',*,*,#35597,.T.) ;
#45734 = ORIENTED_EDGE('',*,*,#35599,.F.) ;
#45735 = ORIENTED_EDGE('',*,*,#35600,.F.) ;
#45736 = ORIENTED_EDGE('',*,*,#35598,.T.) ;
#45737 = ORIENTED_EDGE('',*,*,#34894,.T.) ;
#45738 = ORIENTED_EDGE('',*,*,#35601,.F.) ;
#45739 = ORIENTED_EDGE('',*,*,#35602,.F.) ;
#45740 = ORIENTED_EDGE('',*,*,#35599,.T.) ;
#45741 = ORIENTED_EDGE('',*,*,#35162,.F.) ;
#45742 = ORIENTED_EDGE('',*,*,#35603,.F.) ;
#45743 = ORIENTED_EDGE('',*,*,#35166,.F.) ;
#45744 = ORIENTED_EDGE('',*,*,#35600,.T.) ;
#45745 = ORIENTED_EDGE('',*,*,#35165,.F.) ;
#45746 = ORIENTED_EDGE('',*,*,#35604,.F.) ;
#45747 = ORIENTED_EDGE('',*,*,#34889,.F.) ;
#45748 = ORIENTED_EDGE('',*,*,#35605,.F.) ;
#45749 = ORIENTED_EDGE('',*,*,#34891,.F.) ;
#45750 = ORIENTED_EDGE('',*,*,#35606,.F.) ;
#45751 = ORIENTED_EDGE('',*,*,#35153,.F.) ;
#45752 = ORIENTED_EDGE('',*,*,#35601,.T.) ;
#45753 = ORIENTED_EDGE('',*,*,#34893,.F.) ;
#45754 = ORIENTED_EDGE('',*,*,#35607,.F.) ;
#45755 = ORIENTED_EDGE('',*,*,#35157,.F.) ;
#45756 = ORIENTED_EDGE('',*,*,#35602,.T.) ;
#45757 = ORIENTED_EDGE('',*,*,#35160,.F.) ;
#45758 = ORIENTED_EDGE('',*,*,#35608,.F.) ;
#45759 = ORIENTED_EDGE('',*,*,#35164,.F.) ;
#45760 = ORIENTED_EDGE('',*,*,#35609,.F.) ;
#45761 = ORIENTED_EDGE('',*,*,#34958,.F.) ;
#45762 = ORIENTED_EDGE('',*,*,#35610,.F.) ;
#45763 = ORIENTED_EDGE('',*,*,#35161,.F.) ;
#45764 = ORIENTED_EDGE('',*,*,#35610,.T.) ;
#45765 = ORIENTED_EDGE('',*,*,#34957,.T.) ;
#45766 = ORIENTED_EDGE('',*,*,#35611,.F.) ;
#45767 = ORIENTED_EDGE('',*,*,#35603,.T.) ;
#45768 = ORIENTED_EDGE('',*,*,#34890,.T.) ;
#45769 = ORIENTED_EDGE('',*,*,#35604,.T.) ;
#45770 = ORIENTED_EDGE('',*,*,#35612,.F.) ;
#45771 = ORIENTED_EDGE('',*,*,#35606,.T.) ;
#45772 = ORIENTED_EDGE('',*,*,#34892,.T.) ;
#45773 = ORIENTED_EDGE('',*,*,#35605,.T.) ;
#45774 = ORIENTED_EDGE('',*,*,#35613,.F.) ;
#45775 = ORIENTED_EDGE('',*,*,#35607,.T.) ;
#45776 = ORIENTED_EDGE('',*,*,#35609,.T.) ;
#45777 = ORIENTED_EDGE('',*,*,#35608,.T.) ;
#45778 = ORIENTED_EDGE('',*,*,#35614,.F.) ;
#45779 = ORIENTED_EDGE('',*,*,#34959,.T.) ;
#45780 = ORIENTED_EDGE('',*,*,#35611,.T.) ;
#45781 = ORIENTED_EDGE('',*,*,#34956,.F.) ;
#45782 = ORIENTED_EDGE('',*,*,#35615,.F.) ;
#45783 = ORIENTED_EDGE('',*,*,#35167,.F.) ;
#45784 = ORIENTED_EDGE('',*,*,#35612,.T.) ;
#45785 = ORIENTED_EDGE('',*,*,#35168,.F.) ;
#45786 = ORIENTED_EDGE('',*,*,#35616,.F.) ;
#45787 = ORIENTED_EDGE('',*,*,#35154,.F.) ;
#45788 = ORIENTED_EDGE('',*,*,#35613,.T.) ;
#45789 = ORIENTED_EDGE('',*,*,#35156,.F.) ;
#45790 = ORIENTED_EDGE('',*,*,#35617,.F.) ;
#45791 = ORIENTED_EDGE('',*,*,#35158,.F.) ;
#45792 = ORIENTED_EDGE('',*,*,#35614,.T.) ;
#45793 = ORIENTED_EDGE('',*,*,#35159,.F.) ;
#45794 = ORIENTED_EDGE('',*,*,#35618,.F.) ;
#45795 = ORIENTED_EDGE('',*,*,#34960,.F.) ;
#45796 = ORIENTED_EDGE('',*,*,#35615,.T.) ;
#45797 = ORIENTED_EDGE('',*,*,#34955,.T.) ;
#45798 = ORIENTED_EDGE('',*,*,#35619,.F.) ;
#45799 = ORIENTED_EDGE('',*,*,#35616,.T.) ;
#45800 = ORIENTED_EDGE('',*,*,#35618,.T.) ;
#45801 = ORIENTED_EDGE('',*,*,#35617,.T.) ;
#45802 = ORIENTED_EDGE('',*,*,#35620,.F.) ;
#45803 = ORIENTED_EDGE('',*,*,#34961,.T.) ;
#45804 = ORIENTED_EDGE('',*,*,#35619,.T.) ;
#45805 = ORIENTED_EDGE('',*,*,#34962,.F.) ;
#45806 = ORIENTED_EDGE('',*,*,#35620,.T.) ;
#45807 = ORIENTED_EDGE('',*,*,#35155,.F.) ;
#45808 = ORIENTED_EDGE('',*,*,#35621,.F.) ;
#45809 = ORIENTED_EDGE('',*,*,#34863,.F.) ;
#45810 = ORIENTED_EDGE('',*,*,#35622,.F.) ;
#45811 = ORIENTED_EDGE('',*,*,#35179,.F.) ;
#45812 = ORIENTED_EDGE('',*,*,#34856,.T.) ;
#45813 = ORIENTED_EDGE('',*,*,#35621,.T.) ;
#45814 = ORIENTED_EDGE('',*,*,#35623,.F.) ;
#45815 = ORIENTED_EDGE('',*,*,#35624,.F.) ;
#45816 = ORIENTED_EDGE('',*,*,#35622,.T.) ;
#45817 = ORIENTED_EDGE('',*,*,#34862,.T.) ;
#45818 = ORIENTED_EDGE('',*,*,#35625,.F.) ;
#45819 = ORIENTED_EDGE('',*,*,#35626,.F.) ;
#45820 = ORIENTED_EDGE('',*,*,#35623,.T.) ;
#45821 = ORIENTED_EDGE('',*,*,#35178,.F.) ;
#45822 = ORIENTED_EDGE('',*,*,#35627,.F.) ;
#45823 = ORIENTED_EDGE('',*,*,#35182,.F.) ;
#45824 = ORIENTED_EDGE('',*,*,#35624,.T.) ;
#45825 = ORIENTED_EDGE('',*,*,#35181,.F.) ;
#45826 = ORIENTED_EDGE('',*,*,#35628,.F.) ;
#45827 = ORIENTED_EDGE('',*,*,#34857,.F.) ;
#45828 = ORIENTED_EDGE('',*,*,#35629,.F.) ;
#45829 = ORIENTED_EDGE('',*,*,#34859,.F.) ;
#45830 = ORIENTED_EDGE('',*,*,#35630,.F.) ;
#45831 = ORIENTED_EDGE('',*,*,#35169,.F.) ;
#45832 = ORIENTED_EDGE('',*,*,#35625,.T.) ;
#45833 = ORIENTED_EDGE('',*,*,#34861,.F.) ;
#45834 = ORIENTED_EDGE('',*,*,#35631,.F.) ;
#45835 = ORIENTED_EDGE('',*,*,#35173,.F.) ;
#45836 = ORIENTED_EDGE('',*,*,#35626,.T.) ;
#45837 = ORIENTED_EDGE('',*,*,#35176,.F.) ;
#45838 = ORIENTED_EDGE('',*,*,#35632,.F.) ;
#45839 = ORIENTED_EDGE('',*,*,#35180,.F.) ;
#45840 = ORIENTED_EDGE('',*,*,#35633,.F.) ;
#45841 = ORIENTED_EDGE('',*,*,#34926,.F.) ;
#45842 = ORIENTED_EDGE('',*,*,#35634,.F.) ;
#45843 = ORIENTED_EDGE('',*,*,#35177,.F.) ;
#45844 = ORIENTED_EDGE('',*,*,#35634,.T.) ;
#45845 = ORIENTED_EDGE('',*,*,#34925,.T.) ;
#45846 = ORIENTED_EDGE('',*,*,#35635,.F.) ;
#45847 = ORIENTED_EDGE('',*,*,#35627,.T.) ;
#45848 = ORIENTED_EDGE('',*,*,#34858,.T.) ;
#45849 = ORIENTED_EDGE('',*,*,#35628,.T.) ;
#45850 = ORIENTED_EDGE('',*,*,#35636,.F.) ;
#45851 = ORIENTED_EDGE('',*,*,#35630,.T.) ;
#45852 = ORIENTED_EDGE('',*,*,#34860,.T.) ;
#45853 = ORIENTED_EDGE('',*,*,#35629,.T.) ;
#45854 = ORIENTED_EDGE('',*,*,#35637,.F.) ;
#45855 = ORIENTED_EDGE('',*,*,#35631,.T.) ;
#45856 = ORIENTED_EDGE('',*,*,#35633,.T.) ;
#45857 = ORIENTED_EDGE('',*,*,#35632,.T.) ;
#45858 = ORIENTED_EDGE('',*,*,#35638,.F.) ;
#45859 = ORIENTED_EDGE('',*,*,#34927,.T.) ;
#45860 = ORIENTED_EDGE('',*,*,#35635,.T.) ;
#45861 = ORIENTED_EDGE('',*,*,#34924,.F.) ;
#45862 = ORIENTED_EDGE('',*,*,#35639,.F.) ;
#45863 = ORIENTED_EDGE('',*,*,#35183,.F.) ;
#45864 = ORIENTED_EDGE('',*,*,#35636,.T.) ;
#45865 = ORIENTED_EDGE('',*,*,#35184,.F.) ;
#45866 = ORIENTED_EDGE('',*,*,#35640,.F.) ;
#45867 = ORIENTED_EDGE('',*,*,#35170,.F.) ;
#45868 = ORIENTED_EDGE('',*,*,#35637,.T.) ;
#45869 = ORIENTED_EDGE('',*,*,#35172,.F.) ;
#45870 = ORIENTED_EDGE('',*,*,#35641,.F.) ;
#45871 = ORIENTED_EDGE('',*,*,#35174,.F.) ;
#45872 = ORIENTED_EDGE('',*,*,#35638,.T.) ;
#45873 = ORIENTED_EDGE('',*,*,#35175,.F.) ;
#45874 = ORIENTED_EDGE('',*,*,#35642,.F.) ;
#45875 = ORIENTED_EDGE('',*,*,#34928,.F.) ;
#45876 = ORIENTED_EDGE('',*,*,#35639,.T.) ;
#45877 = ORIENTED_EDGE('',*,*,#34923,.T.) ;
#45878 = ORIENTED_EDGE('',*,*,#35643,.F.) ;
#45879 = ORIENTED_EDGE('',*,*,#35640,.T.) ;
#45880 = ORIENTED_EDGE('',*,*,#35642,.T.) ;
#45881 = ORIENTED_EDGE('',*,*,#35641,.T.) ;
#45882 = ORIENTED_EDGE('',*,*,#35644,.F.) ;
#45883 = ORIENTED_EDGE('',*,*,#34929,.T.) ;
#45884 = ORIENTED_EDGE('',*,*,#35643,.T.) ;
#45885 = ORIENTED_EDGE('',*,*,#34930,.F.) ;
#45886 = ORIENTED_EDGE('',*,*,#35644,.T.) ;
#45887 = ORIENTED_EDGE('',*,*,#35171,.F.) ;
#45888 = ORIENTED_EDGE('',*,*,#35645,.F.) ;
#45889 = ORIENTED_EDGE('',*,*,#34903,.F.) ;
#45890 = ORIENTED_EDGE('',*,*,#35646,.F.) ;
#45891 = ORIENTED_EDGE('',*,*,#35187,.F.) ;
#45892 = ORIENTED_EDGE('',*,*,#34896,.T.) ;
#45893 = ORIENTED_EDGE('',*,*,#35645,.T.) ;
#45894 = ORIENTED_EDGE('',*,*,#35647,.F.) ;
#45895 = ORIENTED_EDGE('',*,*,#35648,.F.) ;
#45896 = ORIENTED_EDGE('',*,*,#35646,.T.) ;
#45897 = ORIENTED_EDGE('',*,*,#34902,.T.) ;
#45898 = ORIENTED_EDGE('',*,*,#35649,.F.) ;
#45899 = ORIENTED_EDGE('',*,*,#35650,.F.) ;
#45900 = ORIENTED_EDGE('',*,*,#35647,.T.) ;
#45901 = ORIENTED_EDGE('',*,*,#35186,.F.) ;
#45902 = ORIENTED_EDGE('',*,*,#35651,.F.) ;
#45903 = ORIENTED_EDGE('',*,*,#35190,.F.) ;
#45904 = ORIENTED_EDGE('',*,*,#35648,.T.) ;
#45905 = ORIENTED_EDGE('',*,*,#35189,.F.) ;
#45906 = ORIENTED_EDGE('',*,*,#35652,.F.) ;
#45907 = ORIENTED_EDGE('',*,*,#34897,.F.) ;
#45908 = ORIENTED_EDGE('',*,*,#35653,.F.) ;
#45909 = ORIENTED_EDGE('',*,*,#34899,.F.) ;
#45910 = ORIENTED_EDGE('',*,*,#35654,.F.) ;
#45911 = ORIENTED_EDGE('',*,*,#35193,.F.) ;
#45912 = ORIENTED_EDGE('',*,*,#35649,.T.) ;
#45913 = ORIENTED_EDGE('',*,*,#34901,.F.) ;
#45914 = ORIENTED_EDGE('',*,*,#35655,.F.) ;
#45915 = ORIENTED_EDGE('',*,*,#35197,.F.) ;
#45916 = ORIENTED_EDGE('',*,*,#35650,.T.) ;
#45917 = ORIENTED_EDGE('',*,*,#35200,.F.) ;
#45918 = ORIENTED_EDGE('',*,*,#35656,.F.) ;
#45919 = ORIENTED_EDGE('',*,*,#35188,.F.) ;
#45920 = ORIENTED_EDGE('',*,*,#35657,.F.) ;
#45921 = ORIENTED_EDGE('',*,*,#34966,.F.) ;
#45922 = ORIENTED_EDGE('',*,*,#35658,.F.) ;
#45923 = ORIENTED_EDGE('',*,*,#35185,.F.) ;
#45924 = ORIENTED_EDGE('',*,*,#35658,.T.) ;
#45925 = ORIENTED_EDGE('',*,*,#34965,.T.) ;
#45926 = ORIENTED_EDGE('',*,*,#35659,.F.) ;
#45927 = ORIENTED_EDGE('',*,*,#35651,.T.) ;
#45928 = ORIENTED_EDGE('',*,*,#34898,.T.) ;
#45929 = ORIENTED_EDGE('',*,*,#35652,.T.) ;
#45930 = ORIENTED_EDGE('',*,*,#35660,.F.) ;
#45931 = ORIENTED_EDGE('',*,*,#35654,.T.) ;
#45932 = ORIENTED_EDGE('',*,*,#34900,.T.) ;
#45933 = ORIENTED_EDGE('',*,*,#35653,.T.) ;
#45934 = ORIENTED_EDGE('',*,*,#35661,.F.) ;
#45935 = ORIENTED_EDGE('',*,*,#35655,.T.) ;
#45936 = ORIENTED_EDGE('',*,*,#35657,.T.) ;
#45937 = ORIENTED_EDGE('',*,*,#35656,.T.) ;
#45938 = ORIENTED_EDGE('',*,*,#35662,.F.) ;
#45939 = ORIENTED_EDGE('',*,*,#34967,.T.) ;
#45940 = ORIENTED_EDGE('',*,*,#35659,.T.) ;
#45941 = ORIENTED_EDGE('',*,*,#34964,.F.) ;
#45942 = ORIENTED_EDGE('',*,*,#35663,.F.) ;
#45943 = ORIENTED_EDGE('',*,*,#35191,.F.) ;
#45944 = ORIENTED_EDGE('',*,*,#35660,.T.) ;
#45945 = ORIENTED_EDGE('',*,*,#35192,.F.) ;
#45946 = ORIENTED_EDGE('',*,*,#35664,.F.) ;
#45947 = ORIENTED_EDGE('',*,*,#35194,.F.) ;
#45948 = ORIENTED_EDGE('',*,*,#35661,.T.) ;
#45949 = ORIENTED_EDGE('',*,*,#35196,.F.) ;
#45950 = ORIENTED_EDGE('',*,*,#35665,.F.) ;
#45951 = ORIENTED_EDGE('',*,*,#35198,.F.) ;
#45952 = ORIENTED_EDGE('',*,*,#35662,.T.) ;
#45953 = ORIENTED_EDGE('',*,*,#35199,.F.) ;
#45954 = ORIENTED_EDGE('',*,*,#35666,.F.) ;
#45955 = ORIENTED_EDGE('',*,*,#34968,.F.) ;
#45956 = ORIENTED_EDGE('',*,*,#35663,.T.) ;
#45957 = ORIENTED_EDGE('',*,*,#34963,.T.) ;
#45958 = ORIENTED_EDGE('',*,*,#35667,.F.) ;
#45959 = ORIENTED_EDGE('',*,*,#35664,.T.) ;
#45960 = ORIENTED_EDGE('',*,*,#35666,.T.) ;
#45961 = ORIENTED_EDGE('',*,*,#35665,.T.) ;
#45962 = ORIENTED_EDGE('',*,*,#35668,.F.) ;
#45963 = ORIENTED_EDGE('',*,*,#34969,.T.) ;
#45964 = ORIENTED_EDGE('',*,*,#35667,.T.) ;
#45965 = ORIENTED_EDGE('',*,*,#34970,.F.) ;
#45966 = ORIENTED_EDGE('',*,*,#35668,.T.) ;
#45967 = ORIENTED_EDGE('',*,*,#35195,.F.) ;
#45968 = ORIENTED_EDGE('',*,*,#35669,.F.) ;
#45969 = ORIENTED_EDGE('',*,*,#34855,.F.) ;
#45970 = ORIENTED_EDGE('',*,*,#35670,.F.) ;
#45971 = ORIENTED_EDGE('',*,*,#35215,.F.) ;
#45972 = ORIENTED_EDGE('',*,*,#34848,.T.) ;
#45973 = ORIENTED_EDGE('',*,*,#35669,.T.) ;
#45974 = ORIENTED_EDGE('',*,*,#35671,.F.) ;
#45975 = ORIENTED_EDGE('',*,*,#35672,.F.) ;
#45976 = ORIENTED_EDGE('',*,*,#35670,.T.) ;
#45977 = ORIENTED_EDGE('',*,*,#34854,.T.) ;
#45978 = ORIENTED_EDGE('',*,*,#35673,.F.) ;
#45979 = ORIENTED_EDGE('',*,*,#35674,.F.) ;
#45980 = ORIENTED_EDGE('',*,*,#35671,.T.) ;
#45981 = ORIENTED_EDGE('',*,*,#35214,.F.) ;
#45982 = ORIENTED_EDGE('',*,*,#35675,.F.) ;
#45983 = ORIENTED_EDGE('',*,*,#35202,.F.) ;
#45984 = ORIENTED_EDGE('',*,*,#35672,.T.) ;
#45985 = ORIENTED_EDGE('',*,*,#35201,.F.) ;
#45986 = ORIENTED_EDGE('',*,*,#35676,.F.) ;
#45987 = ORIENTED_EDGE('',*,*,#34849,.F.) ;
#45988 = ORIENTED_EDGE('',*,*,#35677,.F.) ;
#45989 = ORIENTED_EDGE('',*,*,#34851,.F.) ;
#45990 = ORIENTED_EDGE('',*,*,#35678,.F.) ;
#45991 = ORIENTED_EDGE('',*,*,#35205,.F.) ;
#45992 = ORIENTED_EDGE('',*,*,#35673,.T.) ;
#45993 = ORIENTED_EDGE('',*,*,#34853,.F.) ;
#45994 = ORIENTED_EDGE('',*,*,#35679,.F.) ;
#45995 = ORIENTED_EDGE('',*,*,#35209,.F.) ;
#45996 = ORIENTED_EDGE('',*,*,#35674,.T.) ;
#45997 = ORIENTED_EDGE('',*,*,#35212,.F.) ;
#45998 = ORIENTED_EDGE('',*,*,#35680,.F.) ;
#45999 = ORIENTED_EDGE('',*,*,#35216,.F.) ;
#46000 = ORIENTED_EDGE('',*,*,#35681,.F.) ;
#46001 = ORIENTED_EDGE('',*,*,#34918,.F.) ;
#46002 = ORIENTED_EDGE('',*,*,#35682,.F.) ;
#46003 = ORIENTED_EDGE('',*,*,#35213,.F.) ;
#46004 = ORIENTED_EDGE('',*,*,#35682,.T.) ;
#46005 = ORIENTED_EDGE('',*,*,#34917,.T.) ;
#46006 = ORIENTED_EDGE('',*,*,#35683,.F.) ;
#46007 = ORIENTED_EDGE('',*,*,#35675,.T.) ;
#46008 = ORIENTED_EDGE('',*,*,#34850,.T.) ;
#46009 = ORIENTED_EDGE('',*,*,#35676,.T.) ;
#46010 = ORIENTED_EDGE('',*,*,#35684,.F.) ;
#46011 = ORIENTED_EDGE('',*,*,#35678,.T.) ;
#46012 = ORIENTED_EDGE('',*,*,#34852,.T.) ;
#46013 = ORIENTED_EDGE('',*,*,#35677,.T.) ;
#46014 = ORIENTED_EDGE('',*,*,#35685,.F.) ;
#46015 = ORIENTED_EDGE('',*,*,#35679,.T.) ;
#46016 = ORIENTED_EDGE('',*,*,#35681,.T.) ;
#46017 = ORIENTED_EDGE('',*,*,#35680,.T.) ;
#46018 = ORIENTED_EDGE('',*,*,#35686,.F.) ;
#46019 = ORIENTED_EDGE('',*,*,#34919,.T.) ;
#46020 = ORIENTED_EDGE('',*,*,#35683,.T.) ;
#46021 = ORIENTED_EDGE('',*,*,#34916,.F.) ;
#46022 = ORIENTED_EDGE('',*,*,#35687,.F.) ;
#46023 = ORIENTED_EDGE('',*,*,#35203,.F.) ;
#46024 = ORIENTED_EDGE('',*,*,#35684,.T.) ;
#46025 = ORIENTED_EDGE('',*,*,#35204,.F.) ;
#46026 = ORIENTED_EDGE('',*,*,#35688,.F.) ;
#46027 = ORIENTED_EDGE('',*,*,#35206,.F.) ;
#46028 = ORIENTED_EDGE('',*,*,#35685,.T.) ;
#46029 = ORIENTED_EDGE('',*,*,#35208,.F.) ;
#46030 = ORIENTED_EDGE('',*,*,#35689,.F.) ;
#46031 = ORIENTED_EDGE('',*,*,#35210,.F.) ;
#46032 = ORIENTED_EDGE('',*,*,#35686,.T.) ;
#46033 = ORIENTED_EDGE('',*,*,#35211,.F.) ;
#46034 = ORIENTED_EDGE('',*,*,#35690,.F.) ;
#46035 = ORIENTED_EDGE('',*,*,#34920,.F.) ;
#46036 = ORIENTED_EDGE('',*,*,#35687,.T.) ;
#46037 = ORIENTED_EDGE('',*,*,#34915,.T.) ;
#46038 = ORIENTED_EDGE('',*,*,#35691,.F.) ;
#46039 = ORIENTED_EDGE('',*,*,#35688,.T.) ;
#46040 = ORIENTED_EDGE('',*,*,#35690,.T.) ;
#46041 = ORIENTED_EDGE('',*,*,#35689,.T.) ;
#46042 = ORIENTED_EDGE('',*,*,#35692,.F.) ;
#46043 = ORIENTED_EDGE('',*,*,#34921,.T.) ;
#46044 = ORIENTED_EDGE('',*,*,#35691,.T.) ;
#46045 = ORIENTED_EDGE('',*,*,#34922,.F.) ;
#46046 = ORIENTED_EDGE('',*,*,#35692,.T.) ;
#46047 = ORIENTED_EDGE('',*,*,#35207,.F.) ;
#46048 = ORIENTED_EDGE('',*,*,#35693,.F.) ;
#46049 = ORIENTED_EDGE('',*,*,#34738,.F.) ;
#46050 = ORIENTED_EDGE('',*,*,#35694,.F.) ;
#46051 = ORIENTED_EDGE('',*,*,#35058,.F.) ;
#46052 = ORIENTED_EDGE('',*,*,#35695,.F.) ;
#46053 = ORIENTED_EDGE('',*,*,#34742,.F.) ;
#46054 = ORIENTED_EDGE('',*,*,#35696,.F.) ;
#46055 = ORIENTED_EDGE('',*,*,#35050,.F.) ;
#46056 = ORIENTED_EDGE('',*,*,#35697,.F.) ;
#46057 = ORIENTED_EDGE('',*,*,#34737,.F.) ;
#46058 = ORIENTED_EDGE('',*,*,#35698,.F.) ;
#46059 = ORIENTED_EDGE('',*,*,#35054,.F.) ;
#46060 = ORIENTED_EDGE('',*,*,#35694,.T.) ;
#46061 = ORIENTED_EDGE('',*,*,#35697,.T.) ;
#46062 = ORIENTED_EDGE('',*,*,#35699,.F.) ;
#46063 = ORIENTED_EDGE('',*,*,#35693,.T.) ;
#46064 = ORIENTED_EDGE('',*,*,#35057,.F.) ;
#46065 = ORIENTED_EDGE('',*,*,#35700,.F.) ;
#46066 = ORIENTED_EDGE('',*,*,#35060,.F.) ;
#46067 = ORIENTED_EDGE('',*,*,#35696,.T.) ;
#46068 = ORIENTED_EDGE('',*,*,#35062,.F.) ;
#46069 = ORIENTED_EDGE('',*,*,#35701,.F.) ;
#46070 = ORIENTED_EDGE('',*,*,#35051,.F.) ;
#46071 = ORIENTED_EDGE('',*,*,#35698,.T.) ;
#46072 = ORIENTED_EDGE('',*,*,#35695,.T.) ;
#46073 = ORIENTED_EDGE('',*,*,#35702,.F.) ;
#46074 = ORIENTED_EDGE('',*,*,#35699,.T.) ;
#46075 = ORIENTED_EDGE('',*,*,#35053,.F.) ;
#46076 = ORIENTED_EDGE('',*,*,#35703,.F.) ;
#46077 = ORIENTED_EDGE('',*,*,#35059,.F.) ;
#46078 = ORIENTED_EDGE('',*,*,#35700,.T.) ;
#46079 = ORIENTED_EDGE('',*,*,#35056,.F.) ;
#46080 = ORIENTED_EDGE('',*,*,#35704,.F.) ;
#46081 = ORIENTED_EDGE('',*,*,#34724,.F.) ;
#46082 = ORIENTED_EDGE('',*,*,#35701,.T.) ;
#46083 = ORIENTED_EDGE('',*,*,#34726,.F.) ;
#46084 = ORIENTED_EDGE('',*,*,#35705,.F.) ;
#46085 = ORIENTED_EDGE('',*,*,#35048,.F.) ;
#46086 = ORIENTED_EDGE('',*,*,#35702,.T.) ;
#46087 = ORIENTED_EDGE('',*,*,#35049,.F.) ;
#46088 = ORIENTED_EDGE('',*,*,#35706,.F.) ;
#46089 = ORIENTED_EDGE('',*,*,#35055,.F.) ;
#46090 = ORIENTED_EDGE('',*,*,#35704,.T.) ;
#46091 = ORIENTED_EDGE('',*,*,#35703,.T.) ;
#46092 = ORIENTED_EDGE('',*,*,#35707,.F.) ;
#46093 = ORIENTED_EDGE('',*,*,#35706,.T.) ;
#46094 = ORIENTED_EDGE('',*,*,#35705,.T.) ;
#46095 = ORIENTED_EDGE('',*,*,#35708,.F.) ;
#46096 = ORIENTED_EDGE('',*,*,#35707,.T.) ;
#46097 = ORIENTED_EDGE('',*,*,#35052,.F.) ;
#46098 = ORIENTED_EDGE('',*,*,#35708,.T.) ;
#46099 = ORIENTED_EDGE('',*,*,#34725,.F.) ;
#46100 = ORIENTED_EDGE('',*,*,#35709,.T.) ;
#46101 = ORIENTED_EDGE('',*,*,#35710,.T.) ;
#46102 = ORIENTED_EDGE('',*,*,#35711,.T.) ;
#46103 = ORIENTED_EDGE('',*,*,#35712,.F.) ;
#46104 = ORIENTED_EDGE('',*,*,#35713,.F.) ;
#46105 = ORIENTED_EDGE('',*,*,#35714,.T.) ;
#46106 = ORIENTED_EDGE('',*,*,#35715,.T.) ;
#46107 = ORIENTED_EDGE('',*,*,#35716,.F.) ;
#46108 = ORIENTED_EDGE('',*,*,#35717,.F.) ;
#46109 = ORIENTED_EDGE('',*,*,#35718,.F.) ;
#46110 = ORIENTED_EDGE('',*,*,#35719,.F.) ;
#46111 = ORIENTED_EDGE('',*,*,#35720,.T.) ;
#46112 = ORIENTED_EDGE('',*,*,#35721,.F.) ;
#46113 = ORIENTED_EDGE('',*,*,#35720,.F.) ;
#46114 = ORIENTED_EDGE('',*,*,#35722,.F.) ;
#46115 = ORIENTED_EDGE('',*,*,#35723,.T.) ;
#46116 = ORIENTED_EDGE('',*,*,#35724,.F.) ;
#46117 = ORIENTED_EDGE('',*,*,#35723,.F.) ;
#46118 = ORIENTED_EDGE('',*,*,#35725,.F.) ;
#46119 = ORIENTED_EDGE('',*,*,#35726,.F.) ;
#46120 = ORIENTED_EDGE('',*,*,#35727,.T.) ;
#46121 = ORIENTED_EDGE('',*,*,#35728,.T.) ;
#46122 = ORIENTED_EDGE('',*,*,#35729,.F.) ;
#46123 = ORIENTED_EDGE('',*,*,#35730,.F.) ;
#46124 = ORIENTED_EDGE('',*,*,#35731,.F.) ;
#46125 = ORIENTED_EDGE('',*,*,#35732,.T.) ;
#46126 = ORIENTED_EDGE('',*,*,#35733,.F.) ;
#46127 = ORIENTED_EDGE('',*,*,#35734,.F.) ;
#46128 = ORIENTED_EDGE('',*,*,#35735,.T.) ;
#46129 = ORIENTED_EDGE('',*,*,#35736,.F.) ;
#46130 = ORIENTED_EDGE('',*,*,#35737,.T.) ;
#46131 = ORIENTED_EDGE('',*,*,#35721,.T.) ;
#46132 = ORIENTED_EDGE('',*,*,#35738,.T.) ;
#46133 = ORIENTED_EDGE('',*,*,#35722,.T.) ;
#46134 = ORIENTED_EDGE('',*,*,#35738,.F.) ;
#46135 = ORIENTED_EDGE('',*,*,#35734,.T.) ;
#46136 = ORIENTED_EDGE('',*,*,#35739,.T.) ;
#46137 = ORIENTED_EDGE('',*,*,#35740,.T.) ;
#46138 = ORIENTED_EDGE('',*,*,#35731,.T.) ;
#46139 = ORIENTED_EDGE('',*,*,#35741,.F.) ;
#46140 = ORIENTED_EDGE('',*,*,#35742,.T.) ;
#46141 = ORIENTED_EDGE('',*,*,#35743,.F.) ;
#46142 = ORIENTED_EDGE('',*,*,#35729,.T.) ;
#46143 = ORIENTED_EDGE('',*,*,#35744,.T.) ;
#46144 = ORIENTED_EDGE('',*,*,#35745,.T.) ;
#46145 = ORIENTED_EDGE('',*,*,#35746,.T.) ;
#46146 = ORIENTED_EDGE('',*,*,#35747,.T.) ;
#46147 = ORIENTED_EDGE('',*,*,#35748,.T.) ;
#46148 = ORIENTED_EDGE('',*,*,#35749,.T.) ;
#46149 = ORIENTED_EDGE('',*,*,#35750,.T.) ;
#46150 = ORIENTED_EDGE('',*,*,#35751,.T.) ;
#46151 = ORIENTED_EDGE('',*,*,#35752,.T.) ;
#46152 = ORIENTED_EDGE('',*,*,#35753,.T.) ;
#46153 = ORIENTED_EDGE('',*,*,#35754,.T.) ;
#46154 = ORIENTED_EDGE('',*,*,#35755,.T.) ;
#46155 = ORIENTED_EDGE('',*,*,#35756,.T.) ;
#46156 = ORIENTED_EDGE('',*,*,#35757,.T.) ;
#46157 = ORIENTED_EDGE('',*,*,#35758,.T.) ;
#46158 = ORIENTED_EDGE('',*,*,#35759,.T.) ;
#46159 = ORIENTED_EDGE('',*,*,#35760,.T.) ;
#46160 = ORIENTED_EDGE('',*,*,#35761,.T.) ;
#46161 = ORIENTED_EDGE('',*,*,#35762,.T.) ;
#46162 = ORIENTED_EDGE('',*,*,#35763,.T.) ;
#46163 = ORIENTED_EDGE('',*,*,#35764,.T.) ;
#46164 = ORIENTED_EDGE('',*,*,#35765,.T.) ;
#46165 = ORIENTED_EDGE('',*,*,#35766,.T.) ;
#46166 = ORIENTED_EDGE('',*,*,#35767,.T.) ;
#46167 = ORIENTED_EDGE('',*,*,#35768,.T.) ;
#46168 = ORIENTED_EDGE('',*,*,#35769,.T.) ;
#46169 = ORIENTED_EDGE('',*,*,#35770,.T.) ;
#46170 = ORIENTED_EDGE('',*,*,#35771,.T.) ;
#46171 = ORIENTED_EDGE('',*,*,#35772,.F.) ;
#46172 = ORIENTED_EDGE('',*,*,#35773,.T.) ;
#46173 = ORIENTED_EDGE('',*,*,#35774,.T.) ;
#46174 = ORIENTED_EDGE('',*,*,#35775,.T.) ;
#46175 = ORIENTED_EDGE('',*,*,#35776,.F.) ;
#46176 = ORIENTED_EDGE('',*,*,#35777,.T.) ;
#46177 = ORIENTED_EDGE('',*,*,#35778,.T.) ;
#46178 = ORIENTED_EDGE('',*,*,#35779,.T.) ;
#46179 = ORIENTED_EDGE('',*,*,#35780,.T.) ;
#46180 = ORIENTED_EDGE('',*,*,#35781,.T.) ;
#46181 = ORIENTED_EDGE('',*,*,#35782,.F.) ;
#46182 = ORIENTED_EDGE('',*,*,#35783,.T.) ;
#46183 = ORIENTED_EDGE('',*,*,#35752,.F.) ;
#46184 = ORIENTED_EDGE('',*,*,#35784,.T.) ;
#46185 = ORIENTED_EDGE('',*,*,#35758,.F.) ;
#46186 = ORIENTED_EDGE('',*,*,#35785,.T.) ;
#46187 = ORIENTED_EDGE('',*,*,#35766,.F.) ;
#46188 = ORIENTED_EDGE('',*,*,#35786,.T.) ;
#46189 = ORIENTED_EDGE('',*,*,#35787,.F.) ;
#46190 = ORIENTED_EDGE('',*,*,#35788,.T.) ;
#46191 = ORIENTED_EDGE('',*,*,#35789,.F.) ;
#46192 = ORIENTED_EDGE('',*,*,#35790,.T.) ;
#46193 = ORIENTED_EDGE('',*,*,#35791,.T.) ;
#46194 = ORIENTED_EDGE('',*,*,#35792,.T.) ;
#46195 = ORIENTED_EDGE('',*,*,#35793,.F.) ;
#46196 = ORIENTED_EDGE('',*,*,#35794,.T.) ;
#46197 = ORIENTED_EDGE('',*,*,#35795,.T.) ;
#46198 = ORIENTED_EDGE('',*,*,#35796,.T.) ;
#46199 = ORIENTED_EDGE('',*,*,#35797,.F.) ;
#46200 = ORIENTED_EDGE('',*,*,#35798,.T.) ;
#46201 = ORIENTED_EDGE('',*,*,#35770,.F.) ;
#46202 = ORIENTED_EDGE('',*,*,#35799,.T.) ;
#46203 = ORIENTED_EDGE('',*,*,#35800,.T.) ;
#46204 = ORIENTED_EDGE('',*,*,#35801,.T.) ;
#46205 = ORIENTED_EDGE('',*,*,#35778,.F.) ;
#46206 = ORIENTED_EDGE('',*,*,#35802,.T.) ;
#46207 = ORIENTED_EDGE('',*,*,#35803,.F.) ;
#46208 = ORIENTED_EDGE('',*,*,#35804,.F.) ;
#46209 = ORIENTED_EDGE('',*,*,#35805,.T.) ;
#46210 = ORIENTED_EDGE('',*,*,#35806,.F.) ;
#46211 = ORIENTED_EDGE('',*,*,#35807,.T.) ;
#46212 = ORIENTED_EDGE('',*,*,#35808,.F.) ;
#46213 = ORIENTED_EDGE('',*,*,#35809,.T.) ;
#46214 = ORIENTED_EDGE('',*,*,#35810,.T.) ;
#46215 = ORIENTED_EDGE('',*,*,#35811,.T.) ;
#46216 = ORIENTED_EDGE('',*,*,#35812,.T.) ;
#46217 = ORIENTED_EDGE('',*,*,#35813,.T.) ;
#46218 = ORIENTED_EDGE('',*,*,#35814,.T.) ;
#46219 = ORIENTED_EDGE('',*,*,#35815,.T.) ;
#46220 = ORIENTED_EDGE('',*,*,#35816,.T.) ;
#46221 = ORIENTED_EDGE('',*,*,#35817,.T.) ;
#46222 = ORIENTED_EDGE('',*,*,#35818,.T.) ;
#46223 = ORIENTED_EDGE('',*,*,#35819,.T.) ;
#46224 = ORIENTED_EDGE('',*,*,#35820,.T.) ;
#46225 = ORIENTED_EDGE('',*,*,#35776,.T.) ;
#46226 = ORIENTED_EDGE('',*,*,#35821,.T.) ;
#46227 = ORIENTED_EDGE('',*,*,#35822,.T.) ;
#46228 = ORIENTED_EDGE('',*,*,#35823,.T.) ;
#46229 = ORIENTED_EDGE('',*,*,#35772,.T.) ;
#46230 = ORIENTED_EDGE('',*,*,#35824,.T.) ;
#46231 = ORIENTED_EDGE('',*,*,#35825,.F.) ;
#46232 = ORIENTED_EDGE('',*,*,#35826,.T.) ;
#46233 = ORIENTED_EDGE('',*,*,#35827,.F.) ;
#46234 = ORIENTED_EDGE('',*,*,#35828,.T.) ;
#46235 = ORIENTED_EDGE('',*,*,#35829,.T.) ;
#46236 = ORIENTED_EDGE('',*,*,#35830,.T.) ;
#46237 = ORIENTED_EDGE('',*,*,#35831,.F.) ;
#46238 = ORIENTED_EDGE('',*,*,#35832,.T.) ;
#46239 = ORIENTED_EDGE('',*,*,#35833,.F.) ;
#46240 = ORIENTED_EDGE('',*,*,#35834,.T.) ;
#46241 = ORIENTED_EDGE('',*,*,#35835,.T.) ;
#46242 = ORIENTED_EDGE('',*,*,#35836,.T.) ;
#46243 = ORIENTED_EDGE('',*,*,#35837,.T.) ;
#46244 = ORIENTED_EDGE('',*,*,#35838,.T.) ;
#46245 = ORIENTED_EDGE('',*,*,#35839,.T.) ;
#46246 = ORIENTED_EDGE('',*,*,#35840,.T.) ;
#46247 = ORIENTED_EDGE('',*,*,#35806,.T.) ;
#46248 = ORIENTED_EDGE('',*,*,#35841,.T.) ;
#46249 = ORIENTED_EDGE('',*,*,#35816,.F.) ;
#46250 = ORIENTED_EDGE('',*,*,#35842,.T.) ;
#46251 = ORIENTED_EDGE('',*,*,#35808,.T.) ;
#46252 = ORIENTED_EDGE('',*,*,#35843,.T.) ;
#46253 = ORIENTED_EDGE('',*,*,#35814,.F.) ;
#46254 = ORIENTED_EDGE('',*,*,#35844,.T.) ;
#46255 = ORIENTED_EDGE('',*,*,#35845,.T.) ;
#46256 = ORIENTED_EDGE('',*,*,#35846,.T.) ;
#46257 = ORIENTED_EDGE('',*,*,#35782,.T.) ;
#46258 = ORIENTED_EDGE('',*,*,#35847,.T.) ;
#46259 = ORIENTED_EDGE('',*,*,#35812,.F.) ;
#46260 = ORIENTED_EDGE('',*,*,#35848,.T.) ;
#46261 = ORIENTED_EDGE('',*,*,#35849,.T.) ;
#46262 = ORIENTED_EDGE('',*,*,#35850,.T.) ;
#46263 = ORIENTED_EDGE('',*,*,#35851,.T.) ;
#46264 = ORIENTED_EDGE('',*,*,#35852,.T.) ;
#46265 = ORIENTED_EDGE('',*,*,#35853,.T.) ;
#46266 = ORIENTED_EDGE('',*,*,#35810,.F.) ;
#46267 = ORIENTED_EDGE('',*,*,#35854,.T.) ;
#46268 = ORIENTED_EDGE('',*,*,#35855,.T.) ;
#46269 = ORIENTED_EDGE('',*,*,#35856,.T.) ;
#46270 = ORIENTED_EDGE('',*,*,#35857,.T.) ;
#46271 = ORIENTED_EDGE('',*,*,#35839,.F.) ;
#46272 = ORIENTED_EDGE('',*,*,#35858,.T.) ;
#46273 = ORIENTED_EDGE('',*,*,#35859,.T.) ;
#46274 = ORIENTED_EDGE('',*,*,#35713,.T.) ;
#46275 = ORIENTED_EDGE('',*,*,#35860,.T.) ;
#46276 = ORIENTED_EDGE('',*,*,#35861,.T.) ;
#46277 = ORIENTED_EDGE('',*,*,#35837,.F.) ;
#46278 = ORIENTED_EDGE('',*,*,#35862,.T.) ;
#46279 = ORIENTED_EDGE('',*,*,#35863,.T.) ;
#46280 = ORIENTED_EDGE('',*,*,#35864,.T.) ;
#46281 = ORIENTED_EDGE('',*,*,#35865,.T.) ;
#46282 = ORIENTED_EDGE('',*,*,#35866,.T.) ;
#46283 = ORIENTED_EDGE('',*,*,#35867,.T.) ;
#46284 = ORIENTED_EDGE('',*,*,#35835,.F.) ;
#46285 = ORIENTED_EDGE('',*,*,#35868,.T.) ;
#46286 = ORIENTED_EDGE('',*,*,#35869,.T.) ;
#46287 = ORIENTED_EDGE('',*,*,#35870,.F.) ;
#46288 = ORIENTED_EDGE('',*,*,#35871,.T.) ;
#46289 = ORIENTED_EDGE('',*,*,#35872,.F.) ;
#46290 = ORIENTED_EDGE('',*,*,#35873,.T.) ;
#46291 = ORIENTED_EDGE('',*,*,#35874,.T.) ;
#46292 = ORIENTED_EDGE('',*,*,#35787,.T.) ;
#46293 = ORIENTED_EDGE('',*,*,#35875,.F.) ;
#46294 = ORIENTED_EDGE('',*,*,#35876,.T.) ;
#46295 = ORIENTED_EDGE('',*,*,#35793,.T.) ;
#46296 = ORIENTED_EDGE('',*,*,#35877,.T.) ;
#46297 = ORIENTED_EDGE('',*,*,#35878,.F.) ;
#46298 = ORIENTED_EDGE('',*,*,#35879,.T.) ;
#46299 = ORIENTED_EDGE('',*,*,#35880,.F.) ;
#46300 = ORIENTED_EDGE('',*,*,#35881,.T.) ;
#46301 = ORIENTED_EDGE('',*,*,#35882,.T.) ;
#46302 = ORIENTED_EDGE('',*,*,#35883,.T.) ;
#46303 = ORIENTED_EDGE('',*,*,#35884,.F.) ;
#46304 = ORIENTED_EDGE('',*,*,#35885,.T.) ;
#46305 = ORIENTED_EDGE('',*,*,#35886,.F.) ;
#46306 = ORIENTED_EDGE('',*,*,#35887,.T.) ;
#46307 = ORIENTED_EDGE('',*,*,#35829,.F.) ;
#46308 = ORIENTED_EDGE('',*,*,#35888,.T.) ;
#46309 = ORIENTED_EDGE('',*,*,#35889,.F.) ;
#46310 = ORIENTED_EDGE('',*,*,#35890,.T.) ;
#46311 = ORIENTED_EDGE('',*,*,#35891,.F.) ;
#46312 = ORIENTED_EDGE('',*,*,#35892,.T.) ;
#46313 = ORIENTED_EDGE('',*,*,#35893,.T.) ;
#46314 = ORIENTED_EDGE('',*,*,#35894,.T.) ;
#46315 = ORIENTED_EDGE('',*,*,#35895,.F.) ;
#46316 = ORIENTED_EDGE('',*,*,#35896,.T.) ;
#46317 = ORIENTED_EDGE('',*,*,#35724,.T.) ;
#46318 = ORIENTED_EDGE('',*,*,#35897,.F.) ;
#46319 = ORIENTED_EDGE('',*,*,#35898,.T.) ;
#46320 = ORIENTED_EDGE('',*,*,#35899,.F.) ;
#46321 = ORIENTED_EDGE('',*,*,#35803,.T.) ;
#46322 = ORIENTED_EDGE('',*,*,#35900,.T.) ;
#46323 = ORIENTED_EDGE('',*,*,#35819,.F.) ;
#46324 = ORIENTED_EDGE('',*,*,#35901,.F.) ;
#46325 = ORIENTED_EDGE('',*,*,#35902,.T.) ;
#46326 = ORIENTED_EDGE('',*,*,#35903,.F.) ;
#46327 = ORIENTED_EDGE('',*,*,#35904,.T.) ;
#46328 = ORIENTED_EDGE('',*,*,#35905,.F.) ;
#46329 = ORIENTED_EDGE('',*,*,#35906,.T.) ;
#46330 = ORIENTED_EDGE('',*,*,#35901,.T.) ;
#46331 = ORIENTED_EDGE('',*,*,#35818,.F.) ;
#46332 = ORIENTED_EDGE('',*,*,#35907,.T.) ;
#46333 = ORIENTED_EDGE('',*,*,#35804,.T.) ;
#46334 = ORIENTED_EDGE('',*,*,#35899,.T.) ;
#46335 = ORIENTED_EDGE('',*,*,#35908,.T.) ;
#46336 = ORIENTED_EDGE('',*,*,#35909,.F.) ;
#46337 = ORIENTED_EDGE('',*,*,#35910,.T.) ;
#46338 = ORIENTED_EDGE('',*,*,#35911,.T.) ;
#46339 = ORIENTED_EDGE('',*,*,#35912,.T.) ;
#46340 = ORIENTED_EDGE('',*,*,#35913,.F.) ;
#46341 = ORIENTED_EDGE('',*,*,#35914,.F.) ;
#46342 = ORIENTED_EDGE('',*,*,#35915,.T.) ;
#46343 = ORIENTED_EDGE('',*,*,#35916,.T.) ;
#46344 = ORIENTED_EDGE('',*,*,#35917,.T.) ;
#46345 = ORIENTED_EDGE('',*,*,#35918,.T.) ;
#46346 = ORIENTED_EDGE('',*,*,#35919,.T.) ;
#46347 = ORIENTED_EDGE('',*,*,#35920,.T.) ;
#46348 = ORIENTED_EDGE('',*,*,#35921,.T.) ;
#46349 = ORIENTED_EDGE('',*,*,#35922,.T.) ;
#46350 = ORIENTED_EDGE('',*,*,#35923,.T.) ;
#46351 = ORIENTED_EDGE('',*,*,#35924,.T.) ;
#46352 = ORIENTED_EDGE('',*,*,#35925,.T.) ;
#46353 = ORIENTED_EDGE('',*,*,#35926,.T.) ;
#46354 = ORIENTED_EDGE('',*,*,#35927,.T.) ;
#46355 = ORIENTED_EDGE('',*,*,#35928,.T.) ;
#46356 = ORIENTED_EDGE('',*,*,#35929,.T.) ;
#46357 = ORIENTED_EDGE('',*,*,#35930,.T.) ;
#46358 = ORIENTED_EDGE('',*,*,#35931,.T.) ;
#46359 = ORIENTED_EDGE('',*,*,#35932,.T.) ;
#46360 = ORIENTED_EDGE('',*,*,#35933,.T.) ;
#46361 = ORIENTED_EDGE('',*,*,#35934,.T.) ;
#46362 = ORIENTED_EDGE('',*,*,#35935,.T.) ;
#46363 = ORIENTED_EDGE('',*,*,#35936,.T.) ;
#46364 = ORIENTED_EDGE('',*,*,#35937,.T.) ;
#46365 = ORIENTED_EDGE('',*,*,#35938,.T.) ;
#46366 = ORIENTED_EDGE('',*,*,#35939,.T.) ;
#46367 = ORIENTED_EDGE('',*,*,#35940,.T.) ;
#46368 = ORIENTED_EDGE('',*,*,#35941,.T.) ;
#46369 = ORIENTED_EDGE('',*,*,#35942,.T.) ;
#46370 = ORIENTED_EDGE('',*,*,#35943,.T.) ;
#46371 = ORIENTED_EDGE('',*,*,#35944,.T.) ;
#46372 = ORIENTED_EDGE('',*,*,#35945,.T.) ;
#46373 = ORIENTED_EDGE('',*,*,#35946,.T.) ;
#46374 = ORIENTED_EDGE('',*,*,#35947,.T.) ;
#46375 = ORIENTED_EDGE('',*,*,#35948,.T.) ;
#46376 = ORIENTED_EDGE('',*,*,#35949,.T.) ;
#46377 = ORIENTED_EDGE('',*,*,#35950,.T.) ;
#46378 = ORIENTED_EDGE('',*,*,#35719,.T.) ;
#46379 = ORIENTED_EDGE('',*,*,#35951,.F.) ;
#46380 = ORIENTED_EDGE('',*,*,#35952,.T.) ;
#46381 = ORIENTED_EDGE('',*,*,#35953,.T.) ;
#46382 = ORIENTED_EDGE('',*,*,#35954,.T.) ;
#46383 = ORIENTED_EDGE('',*,*,#35955,.T.) ;
#46384 = ORIENTED_EDGE('',*,*,#35956,.T.) ;
#46385 = ORIENTED_EDGE('',*,*,#35957,.T.) ;
#46386 = ORIENTED_EDGE('',*,*,#35958,.T.) ;
#46387 = ORIENTED_EDGE('',*,*,#35959,.F.) ;
#46388 = ORIENTED_EDGE('',*,*,#35960,.T.) ;
#46389 = ORIENTED_EDGE('',*,*,#35797,.T.) ;
#46390 = ORIENTED_EDGE('',*,*,#35961,.T.) ;
#46391 = ORIENTED_EDGE('',*,*,#35962,.T.) ;
#46392 = ORIENTED_EDGE('',*,*,#35963,.T.) ;
#46393 = ORIENTED_EDGE('',*,*,#35964,.T.) ;
#46394 = ORIENTED_EDGE('',*,*,#35795,.F.) ;
#46395 = ORIENTED_EDGE('',*,*,#35965,.T.) ;
#46396 = ORIENTED_EDGE('',*,*,#35966,.T.) ;
#46397 = ORIENTED_EDGE('',*,*,#35967,.T.) ;
#46398 = ORIENTED_EDGE('',*,*,#35968,.T.) ;
#46399 = ORIENTED_EDGE('',*,*,#35969,.T.) ;
#46400 = ORIENTED_EDGE('',*,*,#35733,.T.) ;
#46401 = ORIENTED_EDGE('',*,*,#35970,.T.) ;
#46402 = ORIENTED_EDGE('',*,*,#35971,.T.) ;
#46403 = ORIENTED_EDGE('',*,*,#35972,.T.) ;
#46404 = ORIENTED_EDGE('',*,*,#35973,.T.) ;
#46405 = ORIENTED_EDGE('',*,*,#35974,.T.) ;
#46406 = ORIENTED_EDGE('',*,*,#35975,.T.) ;
#46407 = ORIENTED_EDGE('',*,*,#35976,.T.) ;
#46408 = ORIENTED_EDGE('',*,*,#35977,.T.) ;
#46409 = ORIENTED_EDGE('',*,*,#35978,.T.) ;
#46410 = ORIENTED_EDGE('',*,*,#35726,.T.) ;
#46411 = ORIENTED_EDGE('',*,*,#35979,.T.) ;
#46412 = ORIENTED_EDGE('',*,*,#35980,.T.) ;
#46413 = ORIENTED_EDGE('',*,*,#35981,.T.) ;
#46414 = ORIENTED_EDGE('',*,*,#35982,.T.) ;
#46415 = ORIENTED_EDGE('',*,*,#35983,.T.) ;
#46416 = ORIENTED_EDGE('',*,*,#35827,.T.) ;
#46417 = ORIENTED_EDGE('',*,*,#35984,.T.) ;
#46418 = ORIENTED_EDGE('',*,*,#35985,.T.) ;
#46419 = ORIENTED_EDGE('',*,*,#35986,.T.) ;
#46420 = ORIENTED_EDGE('',*,*,#35825,.T.) ;
#46421 = ORIENTED_EDGE('',*,*,#35987,.T.) ;
#46422 = ORIENTED_EDGE('',*,*,#35988,.F.) ;
#46423 = ORIENTED_EDGE('',*,*,#35989,.T.) ;
#46424 = ORIENTED_EDGE('',*,*,#35990,.T.) ;
#46425 = ORIENTED_EDGE('',*,*,#35991,.T.) ;
#46426 = ORIENTED_EDGE('',*,*,#35992,.T.) ;
#46427 = ORIENTED_EDGE('',*,*,#35789,.T.) ;
#46428 = ORIENTED_EDGE('',*,*,#35993,.T.) ;
#46429 = ORIENTED_EDGE('',*,*,#35994,.T.) ;
#46430 = ORIENTED_EDGE('',*,*,#35995,.T.) ;
#46431 = ORIENTED_EDGE('',*,*,#35996,.T.) ;
#46432 = ORIENTED_EDGE('',*,*,#35791,.F.) ;
#46433 = ORIENTED_EDGE('',*,*,#35997,.T.) ;
#46434 = ORIENTED_EDGE('',*,*,#35998,.T.) ;
#46435 = ORIENTED_EDGE('',*,*,#35999,.T.) ;
#46436 = ORIENTED_EDGE('',*,*,#36000,.T.) ;
#46437 = ORIENTED_EDGE('',*,*,#36001,.T.) ;
#46438 = ORIENTED_EDGE('',*,*,#36002,.T.) ;
#46439 = ORIENTED_EDGE('',*,*,#36003,.T.) ;
#46440 = ORIENTED_EDGE('',*,*,#36004,.T.) ;
#46441 = ORIENTED_EDGE('',*,*,#36005,.T.) ;
#46442 = ORIENTED_EDGE('',*,*,#36006,.T.) ;
#46443 = ORIENTED_EDGE('',*,*,#36007,.T.) ;
#46444 = ORIENTED_EDGE('',*,*,#36008,.T.) ;
#46445 = ORIENTED_EDGE('',*,*,#36009,.T.) ;
#46446 = ORIENTED_EDGE('',*,*,#35831,.T.) ;
#46447 = ORIENTED_EDGE('',*,*,#36010,.T.) ;
#46448 = ORIENTED_EDGE('',*,*,#36011,.T.) ;
#46449 = ORIENTED_EDGE('',*,*,#36012,.T.) ;
#46450 = ORIENTED_EDGE('',*,*,#36013,.T.) ;
#46451 = ORIENTED_EDGE('',*,*,#36014,.T.) ;
#46452 = ORIENTED_EDGE('',*,*,#36015,.T.) ;
#46453 = ORIENTED_EDGE('',*,*,#36016,.T.) ;
#46454 = ORIENTED_EDGE('',*,*,#36017,.T.) ;
#46455 = ORIENTED_EDGE('',*,*,#36018,.T.) ;
#46456 = ORIENTED_EDGE('',*,*,#35833,.T.) ;
#46457 = ORIENTED_EDGE('',*,*,#36019,.T.) ;
#46458 = ORIENTED_EDGE('',*,*,#36020,.T.) ;
#46459 = ORIENTED_EDGE('',*,*,#36021,.T.) ;
#46460 = ORIENTED_EDGE('',*,*,#36022,.T.) ;
#46461 = ORIENTED_EDGE('',*,*,#36023,.T.) ;
#46462 = ORIENTED_EDGE('',*,*,#36024,.T.) ;
#46463 = ORIENTED_EDGE('',*,*,#36025,.T.) ;
#46464 = ORIENTED_EDGE('',*,*,#36026,.T.) ;
#46465 = ORIENTED_EDGE('',*,*,#35718,.T.) ;
#46466 = ORIENTED_EDGE('',*,*,#36027,.T.) ;
#46467 = ORIENTED_EDGE('',*,*,#36028,.T.) ;
#46468 = ORIENTED_EDGE('',*,*,#36029,.T.) ;
#46469 = ORIENTED_EDGE('',*,*,#36030,.T.) ;
#46470 = ORIENTED_EDGE('',*,*,#36031,.T.) ;
#46471 = ORIENTED_EDGE('',*,*,#36032,.T.) ;
#46472 = ORIENTED_EDGE('',*,*,#36033,.T.) ;
#46473 = ORIENTED_EDGE('',*,*,#36034,.T.) ;
#46474 = ORIENTED_EDGE('',*,*,#36035,.T.) ;
#46475 = ORIENTED_EDGE('',*,*,#36036,.T.) ;
#46476 = ORIENTED_EDGE('',*,*,#36037,.T.) ;
#46477 = ORIENTED_EDGE('',*,*,#36038,.T.) ;
#46478 = ORIENTED_EDGE('',*,*,#36039,.T.) ;
#46479 = ORIENTED_EDGE('',*,*,#36040,.T.) ;
#46480 = ORIENTED_EDGE('',*,*,#36041,.T.) ;
#46481 = ORIENTED_EDGE('',*,*,#36042,.T.) ;
#46482 = ORIENTED_EDGE('',*,*,#36043,.T.) ;
#46483 = ORIENTED_EDGE('',*,*,#36044,.T.) ;
#46484 = ORIENTED_EDGE('',*,*,#36045,.T.) ;
#46485 = ORIENTED_EDGE('',*,*,#36046,.T.) ;
#46486 = ORIENTED_EDGE('',*,*,#36047,.T.) ;
#46487 = ORIENTED_EDGE('',*,*,#36048,.T.) ;
#46488 = ORIENTED_EDGE('',*,*,#36049,.T.) ;
#46489 = ORIENTED_EDGE('',*,*,#36050,.T.) ;
#46490 = ORIENTED_EDGE('',*,*,#35951,.T.) ;
#46491 = ORIENTED_EDGE('',*,*,#36051,.T.) ;
#46492 = ORIENTED_EDGE('',*,*,#36052,.T.) ;
#46493 = ORIENTED_EDGE('',*,*,#36053,.T.) ;
#46494 = ORIENTED_EDGE('',*,*,#35955,.F.) ;
#46495 = ORIENTED_EDGE('',*,*,#36054,.T.) ;
#46496 = ORIENTED_EDGE('',*,*,#36055,.T.) ;
#46497 = ORIENTED_EDGE('',*,*,#36056,.T.) ;
#46498 = ORIENTED_EDGE('',*,*,#35957,.F.) ;
#46499 = ORIENTED_EDGE('',*,*,#36057,.T.) ;
#46500 = ORIENTED_EDGE('',*,*,#36058,.T.) ;
#46501 = ORIENTED_EDGE('',*,*,#36059,.T.) ;
#46502 = ORIENTED_EDGE('',*,*,#35953,.F.) ;
#46503 = ORIENTED_EDGE('',*,*,#36060,.T.) ;
#46504 = ORIENTED_EDGE('',*,*,#36061,.T.) ;
#46505 = ORIENTED_EDGE('',*,*,#36062,.T.) ;
#46506 = ORIENTED_EDGE('',*,*,#36063,.T.) ;
#46507 = ORIENTED_EDGE('',*,*,#36064,.T.) ;
#46508 = ORIENTED_EDGE('',*,*,#36065,.T.) ;
#46509 = ORIENTED_EDGE('',*,*,#36066,.T.) ;
#46510 = ORIENTED_EDGE('',*,*,#36067,.T.) ;
#46511 = ORIENTED_EDGE('',*,*,#36068,.T.) ;
#46512 = ORIENTED_EDGE('',*,*,#36069,.T.) ;
#46513 = ORIENTED_EDGE('',*,*,#36070,.T.) ;
#46514 = ORIENTED_EDGE('',*,*,#36071,.T.) ;
#46515 = ORIENTED_EDGE('',*,*,#36072,.F.) ;
#46516 = ORIENTED_EDGE('',*,*,#36073,.T.) ;
#46517 = ORIENTED_EDGE('',*,*,#35749,.F.) ;
#46518 = ORIENTED_EDGE('',*,*,#36074,.T.) ;
#46519 = ORIENTED_EDGE('',*,*,#36075,.T.) ;
#46520 = ORIENTED_EDGE('',*,*,#36076,.T.) ;
#46521 = ORIENTED_EDGE('',*,*,#36077,.T.) ;
#46522 = ORIENTED_EDGE('',*,*,#36072,.T.) ;
#46523 = ORIENTED_EDGE('',*,*,#36078,.T.) ;
#46524 = ORIENTED_EDGE('',*,*,#36079,.T.) ;
#46525 = ORIENTED_EDGE('',*,*,#36080,.T.) ;
#46526 = ORIENTED_EDGE('',*,*,#36081,.T.) ;
#46527 = ORIENTED_EDGE('',*,*,#36082,.T.) ;
#46528 = ORIENTED_EDGE('',*,*,#36083,.T.) ;
#46529 = ORIENTED_EDGE('',*,*,#36084,.T.) ;
#46530 = ORIENTED_EDGE('',*,*,#36085,.T.) ;
#46531 = ORIENTED_EDGE('',*,*,#36086,.T.) ;
#46532 = ORIENTED_EDGE('',*,*,#36087,.T.) ;
#46533 = ORIENTED_EDGE('',*,*,#36088,.T.) ;
#46534 = ORIENTED_EDGE('',*,*,#36089,.T.) ;
#46535 = ORIENTED_EDGE('',*,*,#36090,.T.) ;
#46536 = ORIENTED_EDGE('',*,*,#36091,.T.) ;
#46537 = ORIENTED_EDGE('',*,*,#36092,.T.) ;
#46538 = ORIENTED_EDGE('',*,*,#36093,.F.) ;
#46539 = ORIENTED_EDGE('',*,*,#35942,.F.) ;
#46540 = ORIENTED_EDGE('',*,*,#36094,.T.) ;
#46541 = ORIENTED_EDGE('',*,*,#36093,.T.) ;
#46542 = ORIENTED_EDGE('',*,*,#36095,.T.) ;
#46543 = ORIENTED_EDGE('',*,*,#36096,.T.) ;
#46544 = ORIENTED_EDGE('',*,*,#36097,.T.) ;
#46545 = ORIENTED_EDGE('',*,*,#36098,.T.) ;
#46546 = ORIENTED_EDGE('',*,*,#36099,.T.) ;
#46547 = ORIENTED_EDGE('',*,*,#36100,.T.) ;
#46548 = ORIENTED_EDGE('',*,*,#36101,.T.) ;
#46549 = ORIENTED_EDGE('',*,*,#36102,.T.) ;
#46550 = ORIENTED_EDGE('',*,*,#36103,.T.) ;
#46551 = ORIENTED_EDGE('',*,*,#36104,.T.) ;
#46552 = ORIENTED_EDGE('',*,*,#36105,.T.) ;
#46553 = ORIENTED_EDGE('',*,*,#36106,.T.) ;
#46554 = ORIENTED_EDGE('',*,*,#36107,.T.) ;
#46555 = ORIENTED_EDGE('',*,*,#36108,.T.) ;
#46556 = ORIENTED_EDGE('',*,*,#36109,.T.) ;
#46557 = ORIENTED_EDGE('',*,*,#36110,.T.) ;
#46558 = ORIENTED_EDGE('',*,*,#36111,.T.) ;
#46559 = ORIENTED_EDGE('',*,*,#36112,.T.) ;
#46560 = ORIENTED_EDGE('',*,*,#36113,.T.) ;
#46561 = ORIENTED_EDGE('',*,*,#36114,.T.) ;
#46562 = ORIENTED_EDGE('',*,*,#35822,.F.) ;
#46563 = ORIENTED_EDGE('',*,*,#36115,.T.) ;
#46564 = ORIENTED_EDGE('',*,*,#36116,.T.) ;
#46565 = ORIENTED_EDGE('',*,*,#35736,.T.) ;
#46566 = ORIENTED_EDGE('',*,*,#36117,.T.) ;
#46567 = ORIENTED_EDGE('',*,*,#35800,.F.) ;
#46568 = ORIENTED_EDGE('',*,*,#36118,.T.) ;
#46569 = ORIENTED_EDGE('',*,*,#36119,.T.) ;
#46570 = ORIENTED_EDGE('',*,*,#36120,.T.) ;
#46571 = ORIENTED_EDGE('',*,*,#36121,.F.) ;
#46572 = ORIENTED_EDGE('',*,*,#36019,.F.) ;
#46573 = ORIENTED_EDGE('',*,*,#35832,.F.) ;
#46574 = ORIENTED_EDGE('',*,*,#36012,.F.) ;
#46575 = ORIENTED_EDGE('',*,*,#36122,.F.) ;
#46576 = ORIENTED_EDGE('',*,*,#36121,.T.) ;
#46577 = ORIENTED_EDGE('',*,*,#36123,.F.) ;
#46578 = ORIENTED_EDGE('',*,*,#35830,.F.) ;
#46579 = ORIENTED_EDGE('',*,*,#35887,.F.) ;
#46580 = ORIENTED_EDGE('',*,*,#36124,.F.) ;
#46581 = ORIENTED_EDGE('',*,*,#36010,.F.) ;
#46582 = ORIENTED_EDGE('',*,*,#36123,.T.) ;
#46583 = ORIENTED_EDGE('',*,*,#36011,.F.) ;
#46584 = ORIENTED_EDGE('',*,*,#36125,.F.) ;
#46585 = ORIENTED_EDGE('',*,*,#36007,.F.) ;
#46586 = ORIENTED_EDGE('',*,*,#36122,.T.) ;
#46587 = ORIENTED_EDGE('',*,*,#36006,.F.) ;
#46588 = ORIENTED_EDGE('',*,*,#36126,.F.) ;
#46589 = ORIENTED_EDGE('',*,*,#36020,.F.) ;
#46590 = ORIENTED_EDGE('',*,*,#36124,.T.) ;
#46591 = ORIENTED_EDGE('',*,*,#35886,.T.) ;
#46592 = ORIENTED_EDGE('',*,*,#36127,.F.) ;
#46593 = ORIENTED_EDGE('',*,*,#36125,.T.) ;
#46594 = ORIENTED_EDGE('',*,*,#36128,.F.) ;
#46595 = ORIENTED_EDGE('',*,*,#36126,.T.) ;
#46596 = ORIENTED_EDGE('',*,*,#36129,.F.) ;
#46597 = ORIENTED_EDGE('',*,*,#35790,.F.) ;
#46598 = ORIENTED_EDGE('',*,*,#35992,.F.) ;
#46599 = ORIENTED_EDGE('',*,*,#36130,.F.) ;
#46600 = ORIENTED_EDGE('',*,*,#35997,.F.) ;
#46601 = ORIENTED_EDGE('',*,*,#36131,.F.) ;
#46602 = ORIENTED_EDGE('',*,*,#35995,.F.) ;
#46603 = ORIENTED_EDGE('',*,*,#36132,.F.) ;
#46604 = ORIENTED_EDGE('',*,*,#36001,.F.) ;
#46605 = ORIENTED_EDGE('',*,*,#35792,.F.) ;
#46606 = ORIENTED_EDGE('',*,*,#35996,.F.) ;
#46607 = ORIENTED_EDGE('',*,*,#36133,.F.) ;
#46608 = ORIENTED_EDGE('',*,*,#35877,.F.) ;
#46609 = ORIENTED_EDGE('',*,*,#36127,.T.) ;
#46610 = ORIENTED_EDGE('',*,*,#35885,.F.) ;
#46611 = ORIENTED_EDGE('',*,*,#36134,.F.) ;
#46612 = ORIENTED_EDGE('',*,*,#36008,.F.) ;
#46613 = ORIENTED_EDGE('',*,*,#36129,.T.) ;
#46614 = ORIENTED_EDGE('',*,*,#36009,.F.) ;
#46615 = ORIENTED_EDGE('',*,*,#36135,.F.) ;
#46616 = ORIENTED_EDGE('',*,*,#36016,.F.) ;
#46617 = ORIENTED_EDGE('',*,*,#36128,.T.) ;
#46618 = ORIENTED_EDGE('',*,*,#36015,.F.) ;
#46619 = ORIENTED_EDGE('',*,*,#36136,.F.) ;
#46620 = ORIENTED_EDGE('',*,*,#36017,.F.) ;
#46621 = ORIENTED_EDGE('',*,*,#35834,.F.) ;
#46622 = ORIENTED_EDGE('',*,*,#36018,.F.) ;
#46623 = ORIENTED_EDGE('',*,*,#36137,.F.) ;
#46624 = ORIENTED_EDGE('',*,*,#35868,.F.) ;
#46625 = ORIENTED_EDGE('',*,*,#36132,.T.) ;
#46626 = ORIENTED_EDGE('',*,*,#36130,.T.) ;
#46627 = ORIENTED_EDGE('',*,*,#36138,.F.) ;
#46628 = ORIENTED_EDGE('',*,*,#36133,.T.) ;
#46629 = ORIENTED_EDGE('',*,*,#36131,.T.) ;
#46630 = ORIENTED_EDGE('',*,*,#36139,.F.) ;
#46631 = ORIENTED_EDGE('',*,*,#35878,.T.) ;
#46632 = ORIENTED_EDGE('',*,*,#36134,.T.) ;
#46633 = ORIENTED_EDGE('',*,*,#35884,.T.) ;
#46634 = ORIENTED_EDGE('',*,*,#36140,.F.) ;
#46635 = ORIENTED_EDGE('',*,*,#36135,.T.) ;
#46636 = ORIENTED_EDGE('',*,*,#36137,.T.) ;
#46637 = ORIENTED_EDGE('',*,*,#36136,.T.) ;
#46638 = ORIENTED_EDGE('',*,*,#36141,.F.) ;
#46639 = ORIENTED_EDGE('',*,*,#36138,.T.) ;
#46640 = ORIENTED_EDGE('',*,*,#35991,.F.) ;
#46641 = ORIENTED_EDGE('',*,*,#36142,.F.) ;
#46642 = ORIENTED_EDGE('',*,*,#35998,.F.) ;
#46643 = ORIENTED_EDGE('',*,*,#36143,.F.) ;
#46644 = ORIENTED_EDGE('',*,*,#35999,.F.) ;
#46645 = ORIENTED_EDGE('',*,*,#36144,.F.) ;
#46646 = ORIENTED_EDGE('',*,*,#36005,.F.) ;
#46647 = ORIENTED_EDGE('',*,*,#36139,.T.) ;
#46648 = ORIENTED_EDGE('',*,*,#36000,.F.) ;
#46649 = ORIENTED_EDGE('',*,*,#36145,.F.) ;
#46650 = ORIENTED_EDGE('',*,*,#35879,.F.) ;
#46651 = ORIENTED_EDGE('',*,*,#36140,.T.) ;
#46652 = ORIENTED_EDGE('',*,*,#35883,.F.) ;
#46653 = ORIENTED_EDGE('',*,*,#36146,.F.) ;
#46654 = ORIENTED_EDGE('',*,*,#36013,.F.) ;
#46655 = ORIENTED_EDGE('',*,*,#36141,.T.) ;
#46656 = ORIENTED_EDGE('',*,*,#36014,.F.) ;
#46657 = ORIENTED_EDGE('',*,*,#36147,.F.) ;
#46658 = ORIENTED_EDGE('',*,*,#35869,.F.) ;
#46659 = ORIENTED_EDGE('',*,*,#36144,.T.) ;
#46660 = ORIENTED_EDGE('',*,*,#36142,.T.) ;
#46661 = ORIENTED_EDGE('',*,*,#36148,.F.) ;
#46662 = ORIENTED_EDGE('',*,*,#36145,.T.) ;
#46663 = ORIENTED_EDGE('',*,*,#36143,.T.) ;
#46664 = ORIENTED_EDGE('',*,*,#36149,.F.) ;
#46665 = ORIENTED_EDGE('',*,*,#35880,.T.) ;
#46666 = ORIENTED_EDGE('',*,*,#36147,.T.) ;
#46667 = ORIENTED_EDGE('',*,*,#36146,.T.) ;
#46668 = ORIENTED_EDGE('',*,*,#36150,.F.) ;
#46669 = ORIENTED_EDGE('',*,*,#35870,.T.) ;
#46670 = ORIENTED_EDGE('',*,*,#35788,.F.) ;
#46671 = ORIENTED_EDGE('',*,*,#35874,.F.) ;
#46672 = ORIENTED_EDGE('',*,*,#36151,.F.) ;
#46673 = ORIENTED_EDGE('',*,*,#35993,.F.) ;
#46674 = ORIENTED_EDGE('',*,*,#36148,.T.) ;
#46675 = ORIENTED_EDGE('',*,*,#35994,.F.) ;
#46676 = ORIENTED_EDGE('',*,*,#36152,.F.) ;
#46677 = ORIENTED_EDGE('',*,*,#36002,.F.) ;
#46678 = ORIENTED_EDGE('',*,*,#36149,.T.) ;
#46679 = ORIENTED_EDGE('',*,*,#36004,.F.) ;
#46680 = ORIENTED_EDGE('',*,*,#36153,.F.) ;
#46681 = ORIENTED_EDGE('',*,*,#35881,.F.) ;
#46682 = ORIENTED_EDGE('',*,*,#36150,.T.) ;
#46683 = ORIENTED_EDGE('',*,*,#35882,.F.) ;
#46684 = ORIENTED_EDGE('',*,*,#36154,.F.) ;
#46685 = ORIENTED_EDGE('',*,*,#35871,.F.) ;
#46686 = ORIENTED_EDGE('',*,*,#36152,.T.) ;
#46687 = ORIENTED_EDGE('',*,*,#36151,.T.) ;
#46688 = ORIENTED_EDGE('',*,*,#36155,.F.) ;
#46689 = ORIENTED_EDGE('',*,*,#36154,.T.) ;
#46690 = ORIENTED_EDGE('',*,*,#36153,.T.) ;
#46691 = ORIENTED_EDGE('',*,*,#36156,.F.) ;
#46692 = ORIENTED_EDGE('',*,*,#35872,.T.) ;
#46693 = ORIENTED_EDGE('',*,*,#36155,.T.) ;
#46694 = ORIENTED_EDGE('',*,*,#35873,.F.) ;
#46695 = ORIENTED_EDGE('',*,*,#36156,.T.) ;
#46696 = ORIENTED_EDGE('',*,*,#36003,.F.) ;
#46697 = ORIENTED_EDGE('',*,*,#36157,.F.) ;
#46698 = ORIENTED_EDGE('',*,*,#36158,.F.) ;
#46699 = ORIENTED_EDGE('',*,*,#36159,.F.) ;
#46700 = ORIENTED_EDGE('',*,*,#35950,.F.) ;
#46701 = ORIENTED_EDGE('',*,*,#36160,.T.) ;
#46702 = ORIENTED_EDGE('',*,*,#36161,.T.) ;
#46703 = ORIENTED_EDGE('',*,*,#35932,.F.) ;
#46704 = ORIENTED_EDGE('',*,*,#36158,.T.) ;
#46705 = ORIENTED_EDGE('',*,*,#35931,.F.) ;
#46706 = ORIENTED_EDGE('',*,*,#36162,.T.) ;
#46707 = ORIENTED_EDGE('',*,*,#36163,.T.) ;
#46708 = ORIENTED_EDGE('',*,*,#35924,.F.) ;
#46709 = ORIENTED_EDGE('',*,*,#36159,.T.) ;
#46710 = ORIENTED_EDGE('',*,*,#36157,.T.) ;
#46711 = ORIENTED_EDGE('',*,*,#35923,.F.) ;
#46712 = ORIENTED_EDGE('',*,*,#36164,.F.) ;
#46713 = ORIENTED_EDGE('',*,*,#35943,.F.) ;
#46714 = ORIENTED_EDGE('',*,*,#35939,.F.) ;
#46715 = ORIENTED_EDGE('',*,*,#36165,.T.) ;
#46716 = ORIENTED_EDGE('',*,*,#36166,.T.) ;
#46717 = ORIENTED_EDGE('',*,*,#35949,.F.) ;
#46718 = ORIENTED_EDGE('',*,*,#36167,.T.) ;
#46719 = ORIENTED_EDGE('',*,*,#36168,.T.) ;
#46720 = ORIENTED_EDGE('',*,*,#35917,.F.) ;
#46721 = ORIENTED_EDGE('',*,*,#36169,.T.) ;
#46722 = ORIENTED_EDGE('',*,*,#36170,.T.) ;
#46723 = ORIENTED_EDGE('',*,*,#35933,.F.) ;
#46724 = ORIENTED_EDGE('',*,*,#36171,.T.) ;
#46725 = ORIENTED_EDGE('',*,*,#36172,.T.) ;
#46726 = ORIENTED_EDGE('',*,*,#36173,.F.) ;
#46727 = ORIENTED_EDGE('',*,*,#36164,.T.) ;
#46728 = ORIENTED_EDGE('',*,*,#36174,.F.) ;
#46729 = ORIENTED_EDGE('',*,*,#35914,.T.) ;
#46730 = ORIENTED_EDGE('',*,*,#36175,.F.) ;
#46731 = ORIENTED_EDGE('',*,*,#36176,.F.) ;
#46732 = ORIENTED_EDGE('',*,*,#35944,.F.) ;
#46733 = ORIENTED_EDGE('',*,*,#36173,.T.) ;
#46734 = ORIENTED_EDGE('',*,*,#36176,.T.) ;
#46735 = ORIENTED_EDGE('',*,*,#36177,.F.) ;
#46736 = ORIENTED_EDGE('',*,*,#36178,.F.) ;
#46737 = ORIENTED_EDGE('',*,*,#35928,.F.) ;
#46738 = ORIENTED_EDGE('',*,*,#36179,.T.) ;
#46739 = ORIENTED_EDGE('',*,*,#36180,.T.) ;
#46740 = ORIENTED_EDGE('',*,*,#35948,.F.) ;
#46741 = ORIENTED_EDGE('',*,*,#36181,.F.) ;
#46742 = ORIENTED_EDGE('',*,*,#35918,.F.) ;
#46743 = ORIENTED_EDGE('',*,*,#36182,.T.) ;
#46744 = ORIENTED_EDGE('',*,*,#36183,.T.) ;
#46745 = ORIENTED_EDGE('',*,*,#35925,.F.) ;
#46746 = ORIENTED_EDGE('',*,*,#36184,.F.) ;
#46747 = ORIENTED_EDGE('',*,*,#36174,.T.) ;
#46748 = ORIENTED_EDGE('',*,*,#35922,.F.) ;
#46749 = ORIENTED_EDGE('',*,*,#36185,.F.) ;
#46750 = ORIENTED_EDGE('',*,*,#36186,.F.) ;
#46751 = ORIENTED_EDGE('',*,*,#36187,.F.) ;
#46752 = ORIENTED_EDGE('',*,*,#35898,.F.) ;
#46753 = ORIENTED_EDGE('',*,*,#36188,.F.) ;
#46754 = ORIENTED_EDGE('',*,*,#36175,.T.) ;
#46755 = ORIENTED_EDGE('',*,*,#35916,.F.) ;
#46756 = ORIENTED_EDGE('',*,*,#36188,.T.) ;
#46757 = ORIENTED_EDGE('',*,*,#35897,.T.) ;
#46758 = ORIENTED_EDGE('',*,*,#36189,.F.) ;
#46759 = ORIENTED_EDGE('',*,*,#36177,.T.) ;
#46760 = ORIENTED_EDGE('',*,*,#35945,.F.) ;
#46761 = ORIENTED_EDGE('',*,*,#36178,.T.) ;
#46762 = ORIENTED_EDGE('',*,*,#36190,.F.) ;
#46763 = ORIENTED_EDGE('',*,*,#36191,.F.) ;
#46764 = ORIENTED_EDGE('',*,*,#36184,.T.) ;
#46765 = ORIENTED_EDGE('',*,*,#36181,.T.) ;
#46766 = ORIENTED_EDGE('',*,*,#36192,.F.) ;
#46767 = ORIENTED_EDGE('',*,*,#36193,.F.) ;
#46768 = ORIENTED_EDGE('',*,*,#36185,.T.) ;
#46769 = ORIENTED_EDGE('',*,*,#36194,.F.) ;
#46770 = ORIENTED_EDGE('',*,*,#35915,.F.) ;
#46771 = ORIENTED_EDGE('',*,*,#36186,.T.) ;
#46772 = ORIENTED_EDGE('',*,*,#36195,.F.) ;
#46773 = ORIENTED_EDGE('',*,*,#35908,.F.) ;
#46774 = ORIENTED_EDGE('',*,*,#36187,.T.) ;
#46775 = ORIENTED_EDGE('',*,*,#36196,.F.) ;
#46776 = ORIENTED_EDGE('',*,*,#36190,.T.) ;
#46777 = ORIENTED_EDGE('',*,*,#36189,.T.) ;
#46778 = ORIENTED_EDGE('',*,*,#35904,.F.) ;
#46779 = ORIENTED_EDGE('',*,*,#36191,.T.) ;
#46780 = ORIENTED_EDGE('',*,*,#36197,.F.) ;
#46781 = ORIENTED_EDGE('',*,*,#36198,.F.) ;
#46782 = ORIENTED_EDGE('',*,*,#36192,.T.) ;
#46783 = ORIENTED_EDGE('',*,*,#35947,.F.) ;
#46784 = ORIENTED_EDGE('',*,*,#36199,.F.) ;
#46785 = ORIENTED_EDGE('',*,*,#35919,.F.) ;
#46786 = ORIENTED_EDGE('',*,*,#36194,.T.) ;
#46787 = ORIENTED_EDGE('',*,*,#35921,.F.) ;
#46788 = ORIENTED_EDGE('',*,*,#36200,.F.) ;
#46789 = ORIENTED_EDGE('',*,*,#36201,.F.) ;
#46790 = ORIENTED_EDGE('',*,*,#36195,.T.) ;
#46791 = ORIENTED_EDGE('',*,*,#36193,.T.) ;
#46792 = ORIENTED_EDGE('',*,*,#36202,.F.) ;
#46793 = ORIENTED_EDGE('',*,*,#35909,.T.) ;
#46794 = ORIENTED_EDGE('',*,*,#36196,.T.) ;
#46795 = ORIENTED_EDGE('',*,*,#35903,.T.) ;
#46796 = ORIENTED_EDGE('',*,*,#36203,.F.) ;
#46797 = ORIENTED_EDGE('',*,*,#36197,.T.) ;
#46798 = ORIENTED_EDGE('',*,*,#36204,.F.) ;
#46799 = ORIENTED_EDGE('',*,*,#36205,.F.) ;
#46800 = ORIENTED_EDGE('',*,*,#35946,.F.) ;
#46801 = ORIENTED_EDGE('',*,*,#36198,.T.) ;
#46802 = ORIENTED_EDGE('',*,*,#36205,.T.) ;
#46803 = ORIENTED_EDGE('',*,*,#35913,.T.) ;
#46804 = ORIENTED_EDGE('',*,*,#36206,.F.) ;
#46805 = ORIENTED_EDGE('',*,*,#36199,.T.) ;
#46806 = ORIENTED_EDGE('',*,*,#36207,.F.) ;
#46807 = ORIENTED_EDGE('',*,*,#36200,.T.) ;
#46808 = ORIENTED_EDGE('',*,*,#36208,.F.) ;
#46809 = ORIENTED_EDGE('',*,*,#36202,.T.) ;
#46810 = ORIENTED_EDGE('',*,*,#36201,.T.) ;
#46811 = ORIENTED_EDGE('',*,*,#36209,.F.) ;
#46812 = ORIENTED_EDGE('',*,*,#35910,.F.) ;
#46813 = ORIENTED_EDGE('',*,*,#36203,.T.) ;
#46814 = ORIENTED_EDGE('',*,*,#35902,.F.) ;
#46815 = ORIENTED_EDGE('',*,*,#36210,.F.) ;
#46816 = ORIENTED_EDGE('',*,*,#35911,.F.) ;
#46817 = ORIENTED_EDGE('',*,*,#36204,.T.) ;
#46818 = ORIENTED_EDGE('',*,*,#35920,.F.) ;
#46819 = ORIENTED_EDGE('',*,*,#36206,.T.) ;
#46820 = ORIENTED_EDGE('',*,*,#36211,.F.) ;
#46821 = ORIENTED_EDGE('',*,*,#36208,.T.) ;
#46822 = ORIENTED_EDGE('',*,*,#36209,.T.) ;
#46823 = ORIENTED_EDGE('',*,*,#36207,.T.) ;
#46824 = ORIENTED_EDGE('',*,*,#36212,.F.) ;
#46825 = ORIENTED_EDGE('',*,*,#35905,.T.) ;
#46826 = ORIENTED_EDGE('',*,*,#36210,.T.) ;
#46827 = ORIENTED_EDGE('',*,*,#35906,.F.) ;
#46828 = ORIENTED_EDGE('',*,*,#36212,.T.) ;
#46829 = ORIENTED_EDGE('',*,*,#36211,.T.) ;
#46830 = ORIENTED_EDGE('',*,*,#35912,.F.) ;
#46831 = ORIENTED_EDGE('',*,*,#36213,.F.) ;
#46832 = ORIENTED_EDGE('',*,*,#35961,.F.) ;
#46833 = ORIENTED_EDGE('',*,*,#35796,.F.) ;
#46834 = ORIENTED_EDGE('',*,*,#35967,.F.) ;
#46835 = ORIENTED_EDGE('',*,*,#36214,.F.) ;
#46836 = ORIENTED_EDGE('',*,*,#36213,.T.) ;
#46837 = ORIENTED_EDGE('',*,*,#36215,.F.) ;
#46838 = ORIENTED_EDGE('',*,*,#35794,.F.) ;
#46839 = ORIENTED_EDGE('',*,*,#35876,.F.) ;
#46840 = ORIENTED_EDGE('',*,*,#36216,.F.) ;
#46841 = ORIENTED_EDGE('',*,*,#35965,.F.) ;
#46842 = ORIENTED_EDGE('',*,*,#36215,.T.) ;
#46843 = ORIENTED_EDGE('',*,*,#35966,.F.) ;
#46844 = ORIENTED_EDGE('',*,*,#36217,.F.) ;
#46845 = ORIENTED_EDGE('',*,*,#35972,.F.) ;
#46846 = ORIENTED_EDGE('',*,*,#36214,.T.) ;
#46847 = ORIENTED_EDGE('',*,*,#35971,.F.) ;
#46848 = ORIENTED_EDGE('',*,*,#36218,.F.) ;
#46849 = ORIENTED_EDGE('',*,*,#35962,.F.) ;
#46850 = ORIENTED_EDGE('',*,*,#35798,.F.) ;
#46851 = ORIENTED_EDGE('',*,*,#35960,.F.) ;
#46852 = ORIENTED_EDGE('',*,*,#36219,.F.) ;
#46853 = ORIENTED_EDGE('',*,*,#35771,.F.) ;
#46854 = ORIENTED_EDGE('',*,*,#35739,.F.) ;
#46855 = ORIENTED_EDGE('',*,*,#36220,.T.) ;
#46856 = ORIENTED_EDGE('',*,*,#35768,.F.) ;
#46857 = ORIENTED_EDGE('',*,*,#36221,.F.) ;
#46858 = ORIENTED_EDGE('',*,*,#36216,.T.) ;
#46859 = ORIENTED_EDGE('',*,*,#35875,.T.) ;
#46860 = ORIENTED_EDGE('',*,*,#36222,.F.) ;
#46861 = ORIENTED_EDGE('',*,*,#36217,.T.) ;
#46862 = ORIENTED_EDGE('',*,*,#36223,.F.) ;
#46863 = ORIENTED_EDGE('',*,*,#36218,.T.) ;
#46864 = ORIENTED_EDGE('',*,*,#36224,.F.) ;
#46865 = ORIENTED_EDGE('',*,*,#36219,.T.) ;
#46866 = ORIENTED_EDGE('',*,*,#35959,.T.) ;
#46867 = ORIENTED_EDGE('',*,*,#36225,.F.) ;
#46868 = ORIENTED_EDGE('',*,*,#36221,.T.) ;
#46869 = ORIENTED_EDGE('',*,*,#36222,.T.) ;
#46870 = ORIENTED_EDGE('',*,*,#35896,.F.) ;
#46871 = ORIENTED_EDGE('',*,*,#36226,.F.) ;
#46872 = ORIENTED_EDGE('',*,*,#35973,.F.) ;
#46873 = ORIENTED_EDGE('',*,*,#36224,.T.) ;
#46874 = ORIENTED_EDGE('',*,*,#35974,.F.) ;
#46875 = ORIENTED_EDGE('',*,*,#36227,.F.) ;
#46876 = ORIENTED_EDGE('',*,*,#35968,.F.) ;
#46877 = ORIENTED_EDGE('',*,*,#36223,.T.) ;
#46878 = ORIENTED_EDGE('',*,*,#35970,.F.) ;
#46879 = ORIENTED_EDGE('',*,*,#36228,.F.) ;
#46880 = ORIENTED_EDGE('',*,*,#35963,.F.) ;
#46881 = ORIENTED_EDGE('',*,*,#36225,.T.) ;
#46882 = ORIENTED_EDGE('',*,*,#35964,.F.) ;
#46883 = ORIENTED_EDGE('',*,*,#36229,.F.) ;
#46884 = ORIENTED_EDGE('',*,*,#35740,.F.) ;
#46885 = ORIENTED_EDGE('',*,*,#35774,.F.) ;
#46886 = ORIENTED_EDGE('',*,*,#36230,.T.) ;
#46887 = ORIENTED_EDGE('',*,*,#35745,.F.) ;
#46888 = ORIENTED_EDGE('',*,*,#36231,.F.) ;
#46889 = ORIENTED_EDGE('',*,*,#35824,.F.) ;
#46890 = ORIENTED_EDGE('',*,*,#35775,.F.) ;
#46891 = ORIENTED_EDGE('',*,*,#36232,.F.) ;
#46892 = ORIENTED_EDGE('',*,*,#35987,.F.) ;
#46893 = ORIENTED_EDGE('',*,*,#35826,.F.) ;
#46894 = ORIENTED_EDGE('',*,*,#35986,.F.) ;
#46895 = ORIENTED_EDGE('',*,*,#36233,.F.) ;
#46896 = ORIENTED_EDGE('',*,*,#35984,.F.) ;
#46897 = ORIENTED_EDGE('',*,*,#36226,.T.) ;
#46898 = ORIENTED_EDGE('',*,*,#35895,.T.) ;
#46899 = ORIENTED_EDGE('',*,*,#36234,.F.) ;
#46900 = ORIENTED_EDGE('',*,*,#36227,.T.) ;
#46901 = ORIENTED_EDGE('',*,*,#36229,.T.) ;
#46902 = ORIENTED_EDGE('',*,*,#36228,.T.) ;
#46903 = ORIENTED_EDGE('',*,*,#35732,.F.) ;
#46904 = ORIENTED_EDGE('',*,*,#36232,.T.) ;
#46905 = ORIENTED_EDGE('',*,*,#36231,.T.) ;
#46906 = ORIENTED_EDGE('',*,*,#36235,.F.) ;
#46907 = ORIENTED_EDGE('',*,*,#35988,.T.) ;
#46908 = ORIENTED_EDGE('',*,*,#36236,.F.) ;
#46909 = ORIENTED_EDGE('',*,*,#36233,.T.) ;
#46910 = ORIENTED_EDGE('',*,*,#36237,.F.) ;
#46911 = ORIENTED_EDGE('',*,*,#36234,.T.) ;
#46912 = ORIENTED_EDGE('',*,*,#35894,.F.) ;
#46913 = ORIENTED_EDGE('',*,*,#36238,.F.) ;
#46914 = ORIENTED_EDGE('',*,*,#35969,.F.) ;
#46915 = ORIENTED_EDGE('',*,*,#36235,.T.) ;
#46916 = ORIENTED_EDGE('',*,*,#35744,.F.) ;
#46917 = ORIENTED_EDGE('',*,*,#36239,.F.) ;
#46918 = ORIENTED_EDGE('',*,*,#35989,.F.) ;
#46919 = ORIENTED_EDGE('',*,*,#36240,.F.) ;
#46920 = ORIENTED_EDGE('',*,*,#35990,.F.) ;
#46921 = ORIENTED_EDGE('',*,*,#36241,.F.) ;
#46922 = ORIENTED_EDGE('',*,*,#35981,.F.) ;
#46923 = ORIENTED_EDGE('',*,*,#36237,.T.) ;
#46924 = ORIENTED_EDGE('',*,*,#35985,.F.) ;
#46925 = ORIENTED_EDGE('',*,*,#36242,.F.) ;
#46926 = ORIENTED_EDGE('',*,*,#35975,.F.) ;
#46927 = ORIENTED_EDGE('',*,*,#36236,.T.) ;
#46928 = ORIENTED_EDGE('',*,*,#35978,.F.) ;
#46929 = ORIENTED_EDGE('',*,*,#36243,.F.) ;
#46930 = ORIENTED_EDGE('',*,*,#35982,.F.) ;
#46931 = ORIENTED_EDGE('',*,*,#35828,.F.) ;
#46932 = ORIENTED_EDGE('',*,*,#35983,.F.) ;
#46933 = ORIENTED_EDGE('',*,*,#36244,.F.) ;
#46934 = ORIENTED_EDGE('',*,*,#35888,.F.) ;
#46935 = ORIENTED_EDGE('',*,*,#35730,.T.) ;
#46936 = ORIENTED_EDGE('',*,*,#36238,.T.) ;
#46937 = ORIENTED_EDGE('',*,*,#36245,.F.) ;
#46938 = ORIENTED_EDGE('',*,*,#35741,.T.) ;
#46939 = ORIENTED_EDGE('',*,*,#36241,.T.) ;
#46940 = ORIENTED_EDGE('',*,*,#36239,.T.) ;
#46941 = ORIENTED_EDGE('',*,*,#35728,.F.) ;
#46942 = ORIENTED_EDGE('',*,*,#36246,.F.) ;
#46943 = ORIENTED_EDGE('',*,*,#36246,.T.) ;
#46944 = ORIENTED_EDGE('',*,*,#35727,.F.) ;
#46945 = ORIENTED_EDGE('',*,*,#36242,.T.) ;
#46946 = ORIENTED_EDGE('',*,*,#36240,.T.) ;
#46947 = ORIENTED_EDGE('',*,*,#36247,.F.) ;
#46948 = ORIENTED_EDGE('',*,*,#36244,.T.) ;
#46949 = ORIENTED_EDGE('',*,*,#36243,.T.) ;
#46950 = ORIENTED_EDGE('',*,*,#36248,.F.) ;
#46951 = ORIENTED_EDGE('',*,*,#35889,.T.) ;
#46952 = ORIENTED_EDGE('',*,*,#36245,.T.) ;
#46953 = ORIENTED_EDGE('',*,*,#35893,.F.) ;
#46954 = ORIENTED_EDGE('',*,*,#36249,.F.) ;
#46955 = ORIENTED_EDGE('',*,*,#35742,.F.) ;
#46956 = ORIENTED_EDGE('',*,*,#36247,.T.) ;
#46957 = ORIENTED_EDGE('',*,*,#35980,.F.) ;
#46958 = ORIENTED_EDGE('',*,*,#36250,.F.) ;
#46959 = ORIENTED_EDGE('',*,*,#35976,.F.) ;
#46960 = ORIENTED_EDGE('',*,*,#36248,.T.) ;
#46961 = ORIENTED_EDGE('',*,*,#35977,.F.) ;
#46962 = ORIENTED_EDGE('',*,*,#36251,.F.) ;
#46963 = ORIENTED_EDGE('',*,*,#35890,.F.) ;
#46964 = ORIENTED_EDGE('',*,*,#35743,.T.) ;
#46965 = ORIENTED_EDGE('',*,*,#36249,.T.) ;
#46966 = ORIENTED_EDGE('',*,*,#36252,.F.) ;
#46967 = ORIENTED_EDGE('',*,*,#35725,.T.) ;
#46968 = ORIENTED_EDGE('',*,*,#36251,.T.) ;
#46969 = ORIENTED_EDGE('',*,*,#36250,.T.) ;
#46970 = ORIENTED_EDGE('',*,*,#36253,.F.) ;
#46971 = ORIENTED_EDGE('',*,*,#35891,.T.) ;
#46972 = ORIENTED_EDGE('',*,*,#36252,.T.) ;
#46973 = ORIENTED_EDGE('',*,*,#35892,.F.) ;
#46974 = ORIENTED_EDGE('',*,*,#36253,.T.) ;
#46975 = ORIENTED_EDGE('',*,*,#35979,.F.) ;
#46976 = ORIENTED_EDGE('',*,*,#35748,.F.) ;
#46977 = ORIENTED_EDGE('',*,*,#36254,.T.) ;
#46978 = ORIENTED_EDGE('',*,*,#36069,.F.) ;
#46979 = ORIENTED_EDGE('',*,*,#36255,.F.) ;
#46980 = ORIENTED_EDGE('',*,*,#36074,.F.) ;
#46981 = ORIENTED_EDGE('',*,*,#36068,.F.) ;
#46982 = ORIENTED_EDGE('',*,*,#36256,.T.) ;
#46983 = ORIENTED_EDGE('',*,*,#36075,.F.) ;
#46984 = ORIENTED_EDGE('',*,*,#36255,.T.) ;
#46985 = ORIENTED_EDGE('',*,*,#36071,.F.) ;
#46986 = ORIENTED_EDGE('',*,*,#36257,.T.) ;
#46987 = ORIENTED_EDGE('',*,*,#35937,.F.) ;
#46988 = ORIENTED_EDGE('',*,*,#36095,.F.) ;
#46989 = ORIENTED_EDGE('',*,*,#36258,.F.) ;
#46990 = ORIENTED_EDGE('',*,*,#36080,.F.) ;
#46991 = ORIENTED_EDGE('',*,*,#36259,.T.) ;
#46992 = ORIENTED_EDGE('',*,*,#36108,.F.) ;
#46993 = ORIENTED_EDGE('',*,*,#36260,.F.) ;
#46994 = ORIENTED_EDGE('',*,*,#36065,.F.) ;
#46995 = ORIENTED_EDGE('',*,*,#36261,.T.) ;
#46996 = ORIENTED_EDGE('',*,*,#35750,.F.) ;
#46997 = ORIENTED_EDGE('',*,*,#36073,.F.) ;
#46998 = ORIENTED_EDGE('',*,*,#36262,.F.) ;
#46999 = ORIENTED_EDGE('',*,*,#36092,.F.) ;
#47000 = ORIENTED_EDGE('',*,*,#36263,.T.) ;
#47001 = ORIENTED_EDGE('',*,*,#36066,.F.) ;
#47002 = ORIENTED_EDGE('',*,*,#36258,.T.) ;
#47003 = ORIENTED_EDGE('',*,*,#36264,.F.) ;
#47004 = ORIENTED_EDGE('',*,*,#36260,.T.) ;
#47005 = ORIENTED_EDGE('',*,*,#36265,.F.) ;
#47006 = ORIENTED_EDGE('',*,*,#36077,.F.) ;
#47007 = ORIENTED_EDGE('',*,*,#36266,.T.) ;
#47008 = ORIENTED_EDGE('',*,*,#36060,.F.) ;
#47009 = ORIENTED_EDGE('',*,*,#36262,.T.) ;
#47010 = ORIENTED_EDGE('',*,*,#36110,.F.) ;
#47011 = ORIENTED_EDGE('',*,*,#36267,.T.) ;
#47012 = ORIENTED_EDGE('',*,*,#36086,.F.) ;
#47013 = ORIENTED_EDGE('',*,*,#36268,.F.) ;
#47014 = ORIENTED_EDGE('',*,*,#36265,.T.) ;
#47015 = ORIENTED_EDGE('',*,*,#36111,.F.) ;
#47016 = ORIENTED_EDGE('',*,*,#36269,.F.) ;
#47017 = ORIENTED_EDGE('',*,*,#36085,.F.) ;
#47018 = ORIENTED_EDGE('',*,*,#36264,.T.) ;
#47019 = ORIENTED_EDGE('',*,*,#36084,.F.) ;
#47020 = ORIENTED_EDGE('',*,*,#36270,.F.) ;
#47021 = ORIENTED_EDGE('',*,*,#36081,.F.) ;
#47022 = ORIENTED_EDGE('',*,*,#36106,.F.) ;
#47023 = ORIENTED_EDGE('',*,*,#36271,.T.) ;
#47024 = ORIENTED_EDGE('',*,*,#36078,.F.) ;
#47025 = ORIENTED_EDGE('',*,*,#36272,.F.) ;
#47026 = ORIENTED_EDGE('',*,*,#36269,.T.) ;
#47027 = ORIENTED_EDGE('',*,*,#36268,.T.) ;
#47028 = ORIENTED_EDGE('',*,*,#36273,.F.) ;
#47029 = ORIENTED_EDGE('',*,*,#36272,.T.) ;
#47030 = ORIENTED_EDGE('',*,*,#36270,.T.) ;
#47031 = ORIENTED_EDGE('',*,*,#36274,.F.) ;
#47032 = ORIENTED_EDGE('',*,*,#36273,.T.) ;
#47033 = ORIENTED_EDGE('',*,*,#36089,.F.) ;
#47034 = ORIENTED_EDGE('',*,*,#36275,.F.) ;
#47035 = ORIENTED_EDGE('',*,*,#36082,.F.) ;
#47036 = ORIENTED_EDGE('',*,*,#36274,.T.) ;
#47037 = ORIENTED_EDGE('',*,*,#36083,.F.) ;
#47038 = ORIENTED_EDGE('',*,*,#36276,.F.) ;
#47039 = ORIENTED_EDGE('',*,*,#36107,.F.) ;
#47040 = ORIENTED_EDGE('',*,*,#36276,.T.) ;
#47041 = ORIENTED_EDGE('',*,*,#36275,.T.) ;
#47042 = ORIENTED_EDGE('',*,*,#36277,.F.) ;
#47043 = ORIENTED_EDGE('',*,*,#36088,.F.) ;
#47044 = ORIENTED_EDGE('',*,*,#36278,.T.) ;
#47045 = ORIENTED_EDGE('',*,*,#36104,.F.) ;
#47046 = ORIENTED_EDGE('',*,*,#36277,.T.) ;
#47047 = ORIENTED_EDGE('',*,*,#36062,.F.) ;
#47048 = ORIENTED_EDGE('',*,*,#36279,.T.) ;
#47049 = ORIENTED_EDGE('',*,*,#36090,.F.) ;
#47050 = ORIENTED_EDGE('',*,*,#36280,.F.) ;
#47051 = ORIENTED_EDGE('',*,*,#35941,.F.) ;
#47052 = ORIENTED_EDGE('',*,*,#36281,.T.) ;
#47053 = ORIENTED_EDGE('',*,*,#36063,.F.) ;
#47054 = ORIENTED_EDGE('',*,*,#36280,.T.) ;
#47055 = ORIENTED_EDGE('',*,*,#36094,.F.) ;
#47056 = ORIENTED_EDGE('',*,*,#36053,.F.) ;
#47057 = ORIENTED_EDGE('',*,*,#36282,.T.) ;
#47058 = ORIENTED_EDGE('',*,*,#36054,.F.) ;
#47059 = ORIENTED_EDGE('',*,*,#35956,.F.) ;
#47060 = ORIENTED_EDGE('',*,*,#36059,.F.) ;
#47061 = ORIENTED_EDGE('',*,*,#36283,.T.) ;
#47062 = ORIENTED_EDGE('',*,*,#36051,.F.) ;
#47063 = ORIENTED_EDGE('',*,*,#35954,.F.) ;
#47064 = ORIENTED_EDGE('',*,*,#36038,.F.) ;
#47065 = ORIENTED_EDGE('',*,*,#36284,.T.) ;
#47066 = ORIENTED_EDGE('',*,*,#36096,.F.) ;
#47067 = ORIENTED_EDGE('',*,*,#36285,.F.) ;
#47068 = ORIENTED_EDGE('',*,*,#36098,.F.) ;
#47069 = ORIENTED_EDGE('',*,*,#36286,.T.) ;
#47070 = ORIENTED_EDGE('',*,*,#36044,.F.) ;
#47071 = ORIENTED_EDGE('',*,*,#36287,.F.) ;
#47072 = ORIENTED_EDGE('',*,*,#36288,.F.) ;
#47073 = ORIENTED_EDGE('',*,*,#36099,.F.) ;
#47074 = ORIENTED_EDGE('',*,*,#36289,.F.) ;
#47075 = ORIENTED_EDGE('',*,*,#36043,.F.) ;
#47076 = ORIENTED_EDGE('',*,*,#36285,.T.) ;
#47077 = ORIENTED_EDGE('',*,*,#36288,.T.) ;
#47078 = ORIENTED_EDGE('',*,*,#36290,.F.) ;
#47079 = ORIENTED_EDGE('',*,*,#36056,.F.) ;
#47080 = ORIENTED_EDGE('',*,*,#36291,.T.) ;
#47081 = ORIENTED_EDGE('',*,*,#36048,.F.) ;
#47082 = ORIENTED_EDGE('',*,*,#35958,.F.) ;
#47083 = ORIENTED_EDGE('',*,*,#36050,.F.) ;
#47084 = ORIENTED_EDGE('',*,*,#36292,.T.) ;
#47085 = ORIENTED_EDGE('',*,*,#36057,.F.) ;
#47086 = ORIENTED_EDGE('',*,*,#35952,.F.) ;
#47087 = ORIENTED_EDGE('',*,*,#36289,.T.) ;
#47088 = ORIENTED_EDGE('',*,*,#36287,.T.) ;
#47089 = ORIENTED_EDGE('',*,*,#36293,.F.) ;
#47090 = ORIENTED_EDGE('',*,*,#36290,.T.) ;
#47091 = ORIENTED_EDGE('',*,*,#36042,.F.) ;
#47092 = ORIENTED_EDGE('',*,*,#36294,.F.) ;
#47093 = ORIENTED_EDGE('',*,*,#36039,.F.) ;
#47094 = ORIENTED_EDGE('',*,*,#36102,.F.) ;
#47095 = ORIENTED_EDGE('',*,*,#36295,.T.) ;
#47096 = ORIENTED_EDGE('',*,*,#36036,.F.) ;
#47097 = ORIENTED_EDGE('',*,*,#36296,.F.) ;
#47098 = ORIENTED_EDGE('',*,*,#36046,.F.) ;
#47099 = ORIENTED_EDGE('',*,*,#36297,.T.) ;
#47100 = ORIENTED_EDGE('',*,*,#36100,.F.) ;
#47101 = ORIENTED_EDGE('',*,*,#36298,.F.) ;
#47102 = ORIENTED_EDGE('',*,*,#36293,.T.) ;
#47103 = ORIENTED_EDGE('',*,*,#36047,.F.) ;
#47104 = ORIENTED_EDGE('',*,*,#36299,.F.) ;
#47105 = ORIENTED_EDGE('',*,*,#36040,.F.) ;
#47106 = ORIENTED_EDGE('',*,*,#36296,.T.) ;
#47107 = ORIENTED_EDGE('',*,*,#36294,.T.) ;
#47108 = ORIENTED_EDGE('',*,*,#36300,.F.) ;
#47109 = ORIENTED_EDGE('',*,*,#36299,.T.) ;
#47110 = ORIENTED_EDGE('',*,*,#36298,.T.) ;
#47111 = ORIENTED_EDGE('',*,*,#36301,.F.) ;
#47112 = ORIENTED_EDGE('',*,*,#36300,.T.) ;
#47113 = ORIENTED_EDGE('',*,*,#36041,.F.) ;
#47114 = ORIENTED_EDGE('',*,*,#36301,.T.) ;
#47115 = ORIENTED_EDGE('',*,*,#36103,.F.) ;
#47116 = ORIENTED_EDGE('',*,*,#35785,.F.) ;
#47117 = ORIENTED_EDGE('',*,*,#35761,.F.) ;
#47118 = ORIENTED_EDGE('',*,*,#36302,.F.) ;
#47119 = ORIENTED_EDGE('',*,*,#35767,.F.) ;
#47120 = ORIENTED_EDGE('',*,*,#36023,.F.) ;
#47121 = ORIENTED_EDGE('',*,*,#36303,.T.) ;
#47122 = ORIENTED_EDGE('',*,*,#35762,.F.) ;
#47123 = ORIENTED_EDGE('',*,*,#36304,.F.) ;
#47124 = ORIENTED_EDGE('',*,*,#36304,.T.) ;
#47125 = ORIENTED_EDGE('',*,*,#36302,.T.) ;
#47126 = ORIENTED_EDGE('',*,*,#36305,.F.) ;
#47127 = ORIENTED_EDGE('',*,*,#35784,.F.) ;
#47128 = ORIENTED_EDGE('',*,*,#35757,.F.) ;
#47129 = ORIENTED_EDGE('',*,*,#36306,.F.) ;
#47130 = ORIENTED_EDGE('',*,*,#35759,.F.) ;
#47131 = ORIENTED_EDGE('',*,*,#36305,.T.) ;
#47132 = ORIENTED_EDGE('',*,*,#35760,.F.) ;
#47133 = ORIENTED_EDGE('',*,*,#36307,.F.) ;
#47134 = ORIENTED_EDGE('',*,*,#36024,.F.) ;
#47135 = ORIENTED_EDGE('',*,*,#36307,.T.) ;
#47136 = ORIENTED_EDGE('',*,*,#36306,.T.) ;
#47137 = ORIENTED_EDGE('',*,*,#36308,.F.) ;
#47138 = ORIENTED_EDGE('',*,*,#35756,.F.) ;
#47139 = ORIENTED_EDGE('',*,*,#36309,.T.) ;
#47140 = ORIENTED_EDGE('',*,*,#36021,.F.) ;
#47141 = ORIENTED_EDGE('',*,*,#36308,.T.) ;
#47142 = ORIENTED_EDGE('',*,*,#35860,.F.) ;
#47143 = ORIENTED_EDGE('',*,*,#35712,.T.) ;
#47144 = ORIENTED_EDGE('',*,*,#36310,.T.) ;
#47145 = ORIENTED_EDGE('',*,*,#36032,.F.) ;
#47146 = ORIENTED_EDGE('',*,*,#36311,.F.) ;
#47147 = ORIENTED_EDGE('',*,*,#35838,.F.) ;
#47148 = ORIENTED_EDGE('',*,*,#35861,.F.) ;
#47149 = ORIENTED_EDGE('',*,*,#36312,.F.) ;
#47150 = ORIENTED_EDGE('',*,*,#35858,.F.) ;
#47151 = ORIENTED_EDGE('',*,*,#36312,.T.) ;
#47152 = ORIENTED_EDGE('',*,*,#36311,.T.) ;
#47153 = ORIENTED_EDGE('',*,*,#36313,.F.) ;
#47154 = ORIENTED_EDGE('',*,*,#36313,.T.) ;
#47155 = ORIENTED_EDGE('',*,*,#36035,.F.) ;
#47156 = ORIENTED_EDGE('',*,*,#36314,.F.) ;
#47157 = ORIENTED_EDGE('',*,*,#35856,.F.) ;
#47158 = ORIENTED_EDGE('',*,*,#35840,.F.) ;
#47159 = ORIENTED_EDGE('',*,*,#35857,.F.) ;
#47160 = ORIENTED_EDGE('',*,*,#36315,.F.) ;
#47161 = ORIENTED_EDGE('',*,*,#35854,.F.) ;
#47162 = ORIENTED_EDGE('',*,*,#36315,.T.) ;
#47163 = ORIENTED_EDGE('',*,*,#36314,.T.) ;
#47164 = ORIENTED_EDGE('',*,*,#36316,.F.) ;
#47165 = ORIENTED_EDGE('',*,*,#36034,.F.) ;
#47166 = ORIENTED_EDGE('',*,*,#35716,.T.) ;
#47167 = ORIENTED_EDGE('',*,*,#36317,.T.) ;
#47168 = ORIENTED_EDGE('',*,*,#35855,.F.) ;
#47169 = ORIENTED_EDGE('',*,*,#36316,.T.) ;
#47170 = ORIENTED_EDGE('',*,*,#35935,.F.) ;
#47171 = ORIENTED_EDGE('',*,*,#36318,.T.) ;
#47172 = ORIENTED_EDGE('',*,*,#35746,.F.) ;
#47173 = ORIENTED_EDGE('',*,*,#36319,.T.) ;
#47174 = ORIENTED_EDGE('',*,*,#35805,.F.) ;
#47175 = ORIENTED_EDGE('',*,*,#35907,.F.) ;
#47176 = ORIENTED_EDGE('',*,*,#35817,.F.) ;
#47177 = ORIENTED_EDGE('',*,*,#35841,.F.) ;
#47178 = ORIENTED_EDGE('',*,*,#35807,.F.) ;
#47179 = ORIENTED_EDGE('',*,*,#35842,.F.) ;
#47180 = ORIENTED_EDGE('',*,*,#35815,.F.) ;
#47181 = ORIENTED_EDGE('',*,*,#35843,.F.) ;
#47182 = ORIENTED_EDGE('',*,*,#35809,.F.) ;
#47183 = ORIENTED_EDGE('',*,*,#35844,.F.) ;
#47184 = ORIENTED_EDGE('',*,*,#35813,.F.) ;
#47185 = ORIENTED_EDGE('',*,*,#35847,.F.) ;
#47186 = ORIENTED_EDGE('',*,*,#35802,.F.) ;
#47187 = ORIENTED_EDGE('',*,*,#35777,.F.) ;
#47188 = ORIENTED_EDGE('',*,*,#35820,.F.) ;
#47189 = ORIENTED_EDGE('',*,*,#35900,.F.) ;
#47190 = ORIENTED_EDGE('',*,*,#36120,.F.) ;
#47191 = ORIENTED_EDGE('',*,*,#36320,.T.) ;
#47192 = ORIENTED_EDGE('',*,*,#35779,.F.) ;
#47193 = ORIENTED_EDGE('',*,*,#35801,.F.) ;
#47194 = ORIENTED_EDGE('',*,*,#36115,.F.) ;
#47195 = ORIENTED_EDGE('',*,*,#36321,.T.) ;
#47196 = ORIENTED_EDGE('',*,*,#35780,.F.) ;
#47197 = ORIENTED_EDGE('',*,*,#36322,.T.) ;
#47198 = ORIENTED_EDGE('',*,*,#35781,.F.) ;
#47199 = ORIENTED_EDGE('',*,*,#36323,.T.) ;
#47200 = ORIENTED_EDGE('',*,*,#36112,.F.) ;
#47201 = ORIENTED_EDGE('',*,*,#35821,.F.) ;
#47202 = ORIENTED_EDGE('',*,*,#36160,.F.) ;
#47203 = ORIENTED_EDGE('',*,*,#36166,.F.) ;
#47204 = ORIENTED_EDGE('',*,*,#36165,.F.) ;
#47205 = ORIENTED_EDGE('',*,*,#36324,.F.) ;
#47206 = ORIENTED_EDGE('',*,*,#36161,.F.) ;
#47207 = ORIENTED_EDGE('',*,*,#36254,.F.) ;
#47208 = ORIENTED_EDGE('',*,*,#35747,.F.) ;
#47209 = ORIENTED_EDGE('',*,*,#36325,.F.) ;
#47210 = ORIENTED_EDGE('',*,*,#35929,.F.) ;
#47211 = ORIENTED_EDGE('',*,*,#36324,.T.) ;
#47212 = ORIENTED_EDGE('',*,*,#35938,.F.) ;
#47213 = ORIENTED_EDGE('',*,*,#36257,.F.) ;
#47214 = ORIENTED_EDGE('',*,*,#36070,.F.) ;
#47215 = ORIENTED_EDGE('',*,*,#36325,.T.) ;
#47216 = ORIENTED_EDGE('',*,*,#36318,.F.) ;
#47217 = ORIENTED_EDGE('',*,*,#36326,.F.) ;
#47218 = ORIENTED_EDGE('',*,*,#36326,.T.) ;
#47219 = ORIENTED_EDGE('',*,*,#35934,.F.) ;
#47220 = ORIENTED_EDGE('',*,*,#36327,.F.) ;
#47221 = ORIENTED_EDGE('',*,*,#35930,.F.) ;
#47222 = ORIENTED_EDGE('',*,*,#36169,.F.) ;
#47223 = ORIENTED_EDGE('',*,*,#36163,.F.) ;
#47224 = ORIENTED_EDGE('',*,*,#36162,.F.) ;
#47225 = ORIENTED_EDGE('',*,*,#36327,.T.) ;
#47226 = ORIENTED_EDGE('',*,*,#36170,.F.) ;
#47227 = ORIENTED_EDGE('',*,*,#36182,.F.) ;
#47228 = ORIENTED_EDGE('',*,*,#36172,.F.) ;
#47229 = ORIENTED_EDGE('',*,*,#36171,.F.) ;
#47230 = ORIENTED_EDGE('',*,*,#36328,.F.) ;
#47231 = ORIENTED_EDGE('',*,*,#36183,.F.) ;
#47232 = ORIENTED_EDGE('',*,*,#36328,.T.) ;
#47233 = ORIENTED_EDGE('',*,*,#35936,.F.) ;
#47234 = ORIENTED_EDGE('',*,*,#36329,.F.) ;
#47235 = ORIENTED_EDGE('',*,*,#35926,.F.) ;
#47236 = ORIENTED_EDGE('',*,*,#36329,.T.) ;
#47237 = ORIENTED_EDGE('',*,*,#36319,.F.) ;
#47238 = ORIENTED_EDGE('',*,*,#36330,.F.) ;
#47239 = ORIENTED_EDGE('',*,*,#36281,.F.) ;
#47240 = ORIENTED_EDGE('',*,*,#35940,.F.) ;
#47241 = ORIENTED_EDGE('',*,*,#36331,.F.) ;
#47242 = ORIENTED_EDGE('',*,*,#35927,.F.) ;
#47243 = ORIENTED_EDGE('',*,*,#36330,.T.) ;
#47244 = ORIENTED_EDGE('',*,*,#35751,.F.) ;
#47245 = ORIENTED_EDGE('',*,*,#36261,.F.) ;
#47246 = ORIENTED_EDGE('',*,*,#36064,.F.) ;
#47247 = ORIENTED_EDGE('',*,*,#36331,.T.) ;
#47248 = ORIENTED_EDGE('',*,*,#36168,.F.) ;
#47249 = ORIENTED_EDGE('',*,*,#36167,.F.) ;
#47250 = ORIENTED_EDGE('',*,*,#36180,.F.) ;
#47251 = ORIENTED_EDGE('',*,*,#36179,.F.) ;
#47252 = ORIENTED_EDGE('',*,*,#35755,.F.) ;
#47253 = ORIENTED_EDGE('',*,*,#36332,.T.) ;
#47254 = ORIENTED_EDGE('',*,*,#36025,.F.) ;
#47255 = ORIENTED_EDGE('',*,*,#36333,.F.) ;
#47256 = ORIENTED_EDGE('',*,*,#36309,.F.) ;
#47257 = ORIENTED_EDGE('',*,*,#36333,.T.) ;
#47258 = ORIENTED_EDGE('',*,*,#36031,.F.) ;
#47259 = ORIENTED_EDGE('',*,*,#36334,.F.) ;
#47260 = ORIENTED_EDGE('',*,*,#36022,.F.) ;
#47261 = ORIENTED_EDGE('',*,*,#36334,.T.) ;
#47262 = ORIENTED_EDGE('',*,*,#36030,.F.) ;
#47263 = ORIENTED_EDGE('',*,*,#36335,.F.) ;
#47264 = ORIENTED_EDGE('',*,*,#36336,.F.) ;
#47265 = ORIENTED_EDGE('',*,*,#36337,.F.) ;
#47266 = ORIENTED_EDGE('',*,*,#36338,.F.) ;
#47267 = ORIENTED_EDGE('',*,*,#35763,.F.) ;
#47268 = ORIENTED_EDGE('',*,*,#36303,.F.) ;
#47269 = ORIENTED_EDGE('',*,*,#35786,.F.) ;
#47270 = ORIENTED_EDGE('',*,*,#35765,.F.) ;
#47271 = ORIENTED_EDGE('',*,*,#36339,.F.) ;
#47272 = ORIENTED_EDGE('',*,*,#35863,.F.) ;
#47273 = ORIENTED_EDGE('',*,*,#35764,.F.) ;
#47274 = ORIENTED_EDGE('',*,*,#36338,.T.) ;
#47275 = ORIENTED_EDGE('',*,*,#36337,.T.) ;
#47276 = ORIENTED_EDGE('',*,*,#36336,.T.) ;
#47277 = ORIENTED_EDGE('',*,*,#36335,.T.) ;
#47278 = ORIENTED_EDGE('',*,*,#36340,.F.) ;
#47279 = ORIENTED_EDGE('',*,*,#35864,.F.) ;
#47280 = ORIENTED_EDGE('',*,*,#36339,.T.) ;
#47281 = ORIENTED_EDGE('',*,*,#35715,.F.) ;
#47282 = ORIENTED_EDGE('',*,*,#36341,.T.) ;
#47283 = ORIENTED_EDGE('',*,*,#35851,.F.) ;
#47284 = ORIENTED_EDGE('',*,*,#36317,.F.) ;
#47285 = ORIENTED_EDGE('',*,*,#36340,.T.) ;
#47286 = ORIENTED_EDGE('',*,*,#36029,.F.) ;
#47287 = ORIENTED_EDGE('',*,*,#36342,.F.) ;
#47288 = ORIENTED_EDGE('',*,*,#35865,.F.) ;
#47289 = ORIENTED_EDGE('',*,*,#35836,.F.) ;
#47290 = ORIENTED_EDGE('',*,*,#35867,.F.) ;
#47291 = ORIENTED_EDGE('',*,*,#36343,.F.) ;
#47292 = ORIENTED_EDGE('',*,*,#35862,.F.) ;
#47293 = ORIENTED_EDGE('',*,*,#35717,.T.) ;
#47294 = ORIENTED_EDGE('',*,*,#36033,.F.) ;
#47295 = ORIENTED_EDGE('',*,*,#36344,.F.) ;
#47296 = ORIENTED_EDGE('',*,*,#36027,.F.) ;
#47297 = ORIENTED_EDGE('',*,*,#35866,.F.) ;
#47298 = ORIENTED_EDGE('',*,*,#36342,.T.) ;
#47299 = ORIENTED_EDGE('',*,*,#36345,.F.) ;
#47300 = ORIENTED_EDGE('',*,*,#36346,.F.) ;
#47301 = ORIENTED_EDGE('',*,*,#36347,.F.) ;
#47302 = ORIENTED_EDGE('',*,*,#35710,.F.) ;
#47303 = ORIENTED_EDGE('',*,*,#35709,.F.) ;
#47304 = ORIENTED_EDGE('',*,*,#35859,.F.) ;
#47305 = ORIENTED_EDGE('',*,*,#36343,.T.) ;
#47306 = ORIENTED_EDGE('',*,*,#35711,.F.) ;
#47307 = ORIENTED_EDGE('',*,*,#36347,.T.) ;
#47308 = ORIENTED_EDGE('',*,*,#36346,.T.) ;
#47309 = ORIENTED_EDGE('',*,*,#36345,.T.) ;
#47310 = ORIENTED_EDGE('',*,*,#36028,.F.) ;
#47311 = ORIENTED_EDGE('',*,*,#36344,.T.) ;
#47312 = ORIENTED_EDGE('',*,*,#36310,.F.) ;
#47313 = ORIENTED_EDGE('',*,*,#36348,.F.) ;
#47314 = ORIENTED_EDGE('',*,*,#35773,.F.) ;
#47315 = ORIENTED_EDGE('',*,*,#35823,.F.) ;
#47316 = ORIENTED_EDGE('',*,*,#36114,.F.) ;
#47317 = ORIENTED_EDGE('',*,*,#36230,.F.) ;
#47318 = ORIENTED_EDGE('',*,*,#36348,.T.) ;
#47319 = ORIENTED_EDGE('',*,*,#36349,.F.) ;
#47320 = ORIENTED_EDGE('',*,*,#35735,.F.) ;
#47321 = ORIENTED_EDGE('',*,*,#36349,.T.) ;
#47322 = ORIENTED_EDGE('',*,*,#36113,.F.) ;
#47323 = ORIENTED_EDGE('',*,*,#36350,.F.) ;
#47324 = ORIENTED_EDGE('',*,*,#36117,.F.) ;
#47325 = ORIENTED_EDGE('',*,*,#36323,.F.) ;
#47326 = ORIENTED_EDGE('',*,*,#36321,.F.) ;
#47327 = ORIENTED_EDGE('',*,*,#36350,.T.) ;
#47328 = ORIENTED_EDGE('',*,*,#36351,.T.) ;
#47329 = ORIENTED_EDGE('',*,*,#36256,.F.) ;
#47330 = ORIENTED_EDGE('',*,*,#36352,.F.) ;
#47331 = ORIENTED_EDGE('',*,*,#36259,.F.) ;
#47332 = ORIENTED_EDGE('',*,*,#36351,.F.) ;
#47333 = ORIENTED_EDGE('',*,*,#36079,.F.) ;
#47334 = ORIENTED_EDGE('',*,*,#36353,.F.) ;
#47335 = ORIENTED_EDGE('',*,*,#36076,.F.) ;
#47336 = ORIENTED_EDGE('',*,*,#36352,.T.) ;
#47337 = ORIENTED_EDGE('',*,*,#36067,.F.) ;
#47338 = ORIENTED_EDGE('',*,*,#36354,.F.) ;
#47339 = ORIENTED_EDGE('',*,*,#36109,.F.) ;
#47340 = ORIENTED_EDGE('',*,*,#36353,.T.) ;
#47341 = ORIENTED_EDGE('',*,*,#36271,.F.) ;
#47342 = ORIENTED_EDGE('',*,*,#36355,.F.) ;
#47343 = ORIENTED_EDGE('',*,*,#36266,.F.) ;
#47344 = ORIENTED_EDGE('',*,*,#36354,.T.) ;
#47345 = ORIENTED_EDGE('',*,*,#36263,.F.) ;
#47346 = ORIENTED_EDGE('',*,*,#36356,.F.) ;
#47347 = ORIENTED_EDGE('',*,*,#36267,.F.) ;
#47348 = ORIENTED_EDGE('',*,*,#36355,.T.) ;
#47349 = ORIENTED_EDGE('',*,*,#36105,.F.) ;
#47350 = ORIENTED_EDGE('',*,*,#36357,.F.) ;
#47351 = ORIENTED_EDGE('',*,*,#36061,.F.) ;
#47352 = ORIENTED_EDGE('',*,*,#36356,.T.) ;
#47353 = ORIENTED_EDGE('',*,*,#36091,.F.) ;
#47354 = ORIENTED_EDGE('',*,*,#36358,.F.) ;
#47355 = ORIENTED_EDGE('',*,*,#36087,.F.) ;
#47356 = ORIENTED_EDGE('',*,*,#36357,.T.) ;
#47357 = ORIENTED_EDGE('',*,*,#36278,.F.) ;
#47358 = ORIENTED_EDGE('',*,*,#36358,.T.) ;
#47359 = ORIENTED_EDGE('',*,*,#36279,.F.) ;
#47360 = ORIENTED_EDGE('',*,*,#36359,.T.) ;
#47361 = ORIENTED_EDGE('',*,*,#36282,.F.) ;
#47362 = ORIENTED_EDGE('',*,*,#36360,.F.) ;
#47363 = ORIENTED_EDGE('',*,*,#36284,.F.) ;
#47364 = ORIENTED_EDGE('',*,*,#36359,.F.) ;
#47365 = ORIENTED_EDGE('',*,*,#36037,.F.) ;
#47366 = ORIENTED_EDGE('',*,*,#36361,.F.) ;
#47367 = ORIENTED_EDGE('',*,*,#36055,.F.) ;
#47368 = ORIENTED_EDGE('',*,*,#36360,.T.) ;
#47369 = ORIENTED_EDGE('',*,*,#36052,.F.) ;
#47370 = ORIENTED_EDGE('',*,*,#36362,.F.) ;
#47371 = ORIENTED_EDGE('',*,*,#36097,.F.) ;
#47372 = ORIENTED_EDGE('',*,*,#36361,.T.) ;
#47373 = ORIENTED_EDGE('',*,*,#36295,.F.) ;
#47374 = ORIENTED_EDGE('',*,*,#36363,.F.) ;
#47375 = ORIENTED_EDGE('',*,*,#36291,.F.) ;
#47376 = ORIENTED_EDGE('',*,*,#36362,.T.) ;
#47377 = ORIENTED_EDGE('',*,*,#36283,.F.) ;
#47378 = ORIENTED_EDGE('',*,*,#36364,.F.) ;
#47379 = ORIENTED_EDGE('',*,*,#36286,.F.) ;
#47380 = ORIENTED_EDGE('',*,*,#36363,.T.) ;
#47381 = ORIENTED_EDGE('',*,*,#36101,.F.) ;
#47382 = ORIENTED_EDGE('',*,*,#36365,.F.) ;
#47383 = ORIENTED_EDGE('',*,*,#36049,.F.) ;
#47384 = ORIENTED_EDGE('',*,*,#36364,.T.) ;
#47385 = ORIENTED_EDGE('',*,*,#36058,.F.) ;
#47386 = ORIENTED_EDGE('',*,*,#36366,.F.) ;
#47387 = ORIENTED_EDGE('',*,*,#36045,.F.) ;
#47388 = ORIENTED_EDGE('',*,*,#36365,.T.) ;
#47389 = ORIENTED_EDGE('',*,*,#36297,.F.) ;
#47390 = ORIENTED_EDGE('',*,*,#36366,.T.) ;
#47391 = ORIENTED_EDGE('',*,*,#36292,.F.) ;
#47392 = ORIENTED_EDGE('',*,*,#35799,.F.) ;
#47393 = ORIENTED_EDGE('',*,*,#35769,.F.) ;
#47394 = ORIENTED_EDGE('',*,*,#36367,.F.) ;
#47395 = ORIENTED_EDGE('',*,*,#36118,.F.) ;
#47396 = ORIENTED_EDGE('',*,*,#36367,.T.) ;
#47397 = ORIENTED_EDGE('',*,*,#36220,.F.) ;
#47398 = ORIENTED_EDGE('',*,*,#35737,.F.) ;
#47399 = ORIENTED_EDGE('',*,*,#36368,.F.) ;
#47400 = ORIENTED_EDGE('',*,*,#36368,.T.) ;
#47401 = ORIENTED_EDGE('',*,*,#36116,.F.) ;
#47402 = ORIENTED_EDGE('',*,*,#36369,.F.) ;
#47403 = ORIENTED_EDGE('',*,*,#36119,.F.) ;
#47404 = ORIENTED_EDGE('',*,*,#36322,.F.) ;
#47405 = ORIENTED_EDGE('',*,*,#36320,.F.) ;
#47406 = ORIENTED_EDGE('',*,*,#36369,.T.) ;
#47407 = ORIENTED_EDGE('',*,*,#35853,.F.) ;
#47408 = ORIENTED_EDGE('',*,*,#36370,.F.) ;
#47409 = ORIENTED_EDGE('',*,*,#35848,.F.) ;
#47410 = ORIENTED_EDGE('',*,*,#35811,.F.) ;
#47411 = ORIENTED_EDGE('',*,*,#35852,.F.) ;
#47412 = ORIENTED_EDGE('',*,*,#36341,.F.) ;
#47413 = ORIENTED_EDGE('',*,*,#35714,.F.) ;
#47414 = ORIENTED_EDGE('',*,*,#36371,.F.) ;
#47415 = ORIENTED_EDGE('',*,*,#35849,.F.) ;
#47416 = ORIENTED_EDGE('',*,*,#36370,.T.) ;
#47417 = ORIENTED_EDGE('',*,*,#36371,.T.) ;
#47418 = ORIENTED_EDGE('',*,*,#36026,.F.) ;
#47419 = ORIENTED_EDGE('',*,*,#36372,.F.) ;
#47420 = ORIENTED_EDGE('',*,*,#35850,.F.) ;
#47421 = ORIENTED_EDGE('',*,*,#36332,.F.) ;
#47422 = ORIENTED_EDGE('',*,*,#35754,.F.) ;
#47423 = ORIENTED_EDGE('',*,*,#36373,.F.) ;
#47424 = ORIENTED_EDGE('',*,*,#35845,.F.) ;
#47425 = ORIENTED_EDGE('',*,*,#36372,.T.) ;
#47426 = ORIENTED_EDGE('',*,*,#35783,.F.) ;
#47427 = ORIENTED_EDGE('',*,*,#35846,.F.) ;
#47428 = ORIENTED_EDGE('',*,*,#36373,.T.) ;
#47429 = ORIENTED_EDGE('',*,*,#35753,.F.) ;
#47430 = ORIENTED_EDGE('',*,*,#36374,.T.) ;
#47431 = ORIENTED_EDGE('',*,*,#36375,.T.) ;
#47432 = ORIENTED_EDGE('',*,*,#36376,.T.) ;
#47433 = ORIENTED_EDGE('',*,*,#36377,.F.) ;
#47434 = ORIENTED_EDGE('',*,*,#36378,.F.) ;
#47435 = ORIENTED_EDGE('',*,*,#36379,.T.) ;
#47436 = ORIENTED_EDGE('',*,*,#36380,.T.) ;
#47437 = ORIENTED_EDGE('',*,*,#36381,.F.) ;
#47438 = ORIENTED_EDGE('',*,*,#36382,.F.) ;
#47439 = ORIENTED_EDGE('',*,*,#36383,.F.) ;
#47440 = ORIENTED_EDGE('',*,*,#36384,.F.) ;
#47441 = ORIENTED_EDGE('',*,*,#36385,.T.) ;
#47442 = ORIENTED_EDGE('',*,*,#36386,.F.) ;
#47443 = ORIENTED_EDGE('',*,*,#36385,.F.) ;
#47444 = ORIENTED_EDGE('',*,*,#36387,.F.) ;
#47445 = ORIENTED_EDGE('',*,*,#36388,.T.) ;
#47446 = ORIENTED_EDGE('',*,*,#36389,.F.) ;
#47447 = ORIENTED_EDGE('',*,*,#36388,.F.) ;
#47448 = ORIENTED_EDGE('',*,*,#36390,.F.) ;
#47449 = ORIENTED_EDGE('',*,*,#36391,.F.) ;
#47450 = ORIENTED_EDGE('',*,*,#36392,.T.) ;
#47451 = ORIENTED_EDGE('',*,*,#36393,.T.) ;
#47452 = ORIENTED_EDGE('',*,*,#36394,.F.) ;
#47453 = ORIENTED_EDGE('',*,*,#36395,.F.) ;
#47454 = ORIENTED_EDGE('',*,*,#36396,.F.) ;
#47455 = ORIENTED_EDGE('',*,*,#36397,.T.) ;
#47456 = ORIENTED_EDGE('',*,*,#36398,.F.) ;
#47457 = ORIENTED_EDGE('',*,*,#36399,.F.) ;
#47458 = ORIENTED_EDGE('',*,*,#36400,.T.) ;
#47459 = ORIENTED_EDGE('',*,*,#36401,.F.) ;
#47460 = ORIENTED_EDGE('',*,*,#36402,.T.) ;
#47461 = ORIENTED_EDGE('',*,*,#36386,.T.) ;
#47462 = ORIENTED_EDGE('',*,*,#36403,.T.) ;
#47463 = ORIENTED_EDGE('',*,*,#36387,.T.) ;
#47464 = ORIENTED_EDGE('',*,*,#36403,.F.) ;
#47465 = ORIENTED_EDGE('',*,*,#36399,.T.) ;
#47466 = ORIENTED_EDGE('',*,*,#36404,.T.) ;
#47467 = ORIENTED_EDGE('',*,*,#36405,.T.) ;
#47468 = ORIENTED_EDGE('',*,*,#36396,.T.) ;
#47469 = ORIENTED_EDGE('',*,*,#36406,.F.) ;
#47470 = ORIENTED_EDGE('',*,*,#36407,.T.) ;
#47471 = ORIENTED_EDGE('',*,*,#36408,.F.) ;
#47472 = ORIENTED_EDGE('',*,*,#36394,.T.) ;
#47473 = ORIENTED_EDGE('',*,*,#36409,.T.) ;
#47474 = ORIENTED_EDGE('',*,*,#36410,.T.) ;
#47475 = ORIENTED_EDGE('',*,*,#36411,.T.) ;
#47476 = ORIENTED_EDGE('',*,*,#36412,.T.) ;
#47477 = ORIENTED_EDGE('',*,*,#36413,.T.) ;
#47478 = ORIENTED_EDGE('',*,*,#36414,.T.) ;
#47479 = ORIENTED_EDGE('',*,*,#36415,.T.) ;
#47480 = ORIENTED_EDGE('',*,*,#36416,.T.) ;
#47481 = ORIENTED_EDGE('',*,*,#36417,.T.) ;
#47482 = ORIENTED_EDGE('',*,*,#36418,.T.) ;
#47483 = ORIENTED_EDGE('',*,*,#36419,.T.) ;
#47484 = ORIENTED_EDGE('',*,*,#36420,.T.) ;
#47485 = ORIENTED_EDGE('',*,*,#36421,.T.) ;
#47486 = ORIENTED_EDGE('',*,*,#36422,.T.) ;
#47487 = ORIENTED_EDGE('',*,*,#36423,.T.) ;
#47488 = ORIENTED_EDGE('',*,*,#36424,.T.) ;
#47489 = ORIENTED_EDGE('',*,*,#36425,.T.) ;
#47490 = ORIENTED_EDGE('',*,*,#36426,.T.) ;
#47491 = ORIENTED_EDGE('',*,*,#36427,.T.) ;
#47492 = ORIENTED_EDGE('',*,*,#36428,.T.) ;
#47493 = ORIENTED_EDGE('',*,*,#36429,.T.) ;
#47494 = ORIENTED_EDGE('',*,*,#36430,.T.) ;
#47495 = ORIENTED_EDGE('',*,*,#36431,.T.) ;
#47496 = ORIENTED_EDGE('',*,*,#36432,.T.) ;
#47497 = ORIENTED_EDGE('',*,*,#36433,.T.) ;
#47498 = ORIENTED_EDGE('',*,*,#36434,.T.) ;
#47499 = ORIENTED_EDGE('',*,*,#36435,.T.) ;
#47500 = ORIENTED_EDGE('',*,*,#36436,.T.) ;
#47501 = ORIENTED_EDGE('',*,*,#36437,.F.) ;
#47502 = ORIENTED_EDGE('',*,*,#36438,.T.) ;
#47503 = ORIENTED_EDGE('',*,*,#36439,.T.) ;
#47504 = ORIENTED_EDGE('',*,*,#36440,.T.) ;
#47505 = ORIENTED_EDGE('',*,*,#36441,.F.) ;
#47506 = ORIENTED_EDGE('',*,*,#36442,.T.) ;
#47507 = ORIENTED_EDGE('',*,*,#36443,.T.) ;
#47508 = ORIENTED_EDGE('',*,*,#36444,.T.) ;
#47509 = ORIENTED_EDGE('',*,*,#36445,.T.) ;
#47510 = ORIENTED_EDGE('',*,*,#36446,.T.) ;
#47511 = ORIENTED_EDGE('',*,*,#36447,.F.) ;
#47512 = ORIENTED_EDGE('',*,*,#36448,.T.) ;
#47513 = ORIENTED_EDGE('',*,*,#36417,.F.) ;
#47514 = ORIENTED_EDGE('',*,*,#36449,.T.) ;
#47515 = ORIENTED_EDGE('',*,*,#36423,.F.) ;
#47516 = ORIENTED_EDGE('',*,*,#36450,.T.) ;
#47517 = ORIENTED_EDGE('',*,*,#36431,.F.) ;
#47518 = ORIENTED_EDGE('',*,*,#36451,.T.) ;
#47519 = ORIENTED_EDGE('',*,*,#36452,.F.) ;
#47520 = ORIENTED_EDGE('',*,*,#36453,.T.) ;
#47521 = ORIENTED_EDGE('',*,*,#36454,.F.) ;
#47522 = ORIENTED_EDGE('',*,*,#36455,.T.) ;
#47523 = ORIENTED_EDGE('',*,*,#36456,.T.) ;
#47524 = ORIENTED_EDGE('',*,*,#36457,.T.) ;
#47525 = ORIENTED_EDGE('',*,*,#36458,.F.) ;
#47526 = ORIENTED_EDGE('',*,*,#36459,.T.) ;
#47527 = ORIENTED_EDGE('',*,*,#36460,.T.) ;
#47528 = ORIENTED_EDGE('',*,*,#36461,.T.) ;
#47529 = ORIENTED_EDGE('',*,*,#36462,.F.) ;
#47530 = ORIENTED_EDGE('',*,*,#36463,.T.) ;
#47531 = ORIENTED_EDGE('',*,*,#36435,.F.) ;
#47532 = ORIENTED_EDGE('',*,*,#36464,.T.) ;
#47533 = ORIENTED_EDGE('',*,*,#36465,.T.) ;
#47534 = ORIENTED_EDGE('',*,*,#36466,.T.) ;
#47535 = ORIENTED_EDGE('',*,*,#36443,.F.) ;
#47536 = ORIENTED_EDGE('',*,*,#36467,.T.) ;
#47537 = ORIENTED_EDGE('',*,*,#36468,.F.) ;
#47538 = ORIENTED_EDGE('',*,*,#36469,.F.) ;
#47539 = ORIENTED_EDGE('',*,*,#36470,.T.) ;
#47540 = ORIENTED_EDGE('',*,*,#36471,.F.) ;
#47541 = ORIENTED_EDGE('',*,*,#36472,.T.) ;
#47542 = ORIENTED_EDGE('',*,*,#36473,.F.) ;
#47543 = ORIENTED_EDGE('',*,*,#36474,.T.) ;
#47544 = ORIENTED_EDGE('',*,*,#36475,.T.) ;
#47545 = ORIENTED_EDGE('',*,*,#36476,.T.) ;
#47546 = ORIENTED_EDGE('',*,*,#36477,.T.) ;
#47547 = ORIENTED_EDGE('',*,*,#36478,.T.) ;
#47548 = ORIENTED_EDGE('',*,*,#36479,.T.) ;
#47549 = ORIENTED_EDGE('',*,*,#36480,.T.) ;
#47550 = ORIENTED_EDGE('',*,*,#36481,.T.) ;
#47551 = ORIENTED_EDGE('',*,*,#36482,.T.) ;
#47552 = ORIENTED_EDGE('',*,*,#36483,.T.) ;
#47553 = ORIENTED_EDGE('',*,*,#36484,.T.) ;
#47554 = ORIENTED_EDGE('',*,*,#36485,.T.) ;
#47555 = ORIENTED_EDGE('',*,*,#36441,.T.) ;
#47556 = ORIENTED_EDGE('',*,*,#36486,.T.) ;
#47557 = ORIENTED_EDGE('',*,*,#36487,.T.) ;
#47558 = ORIENTED_EDGE('',*,*,#36488,.T.) ;
#47559 = ORIENTED_EDGE('',*,*,#36437,.T.) ;
#47560 = ORIENTED_EDGE('',*,*,#36489,.T.) ;
#47561 = ORIENTED_EDGE('',*,*,#36490,.F.) ;
#47562 = ORIENTED_EDGE('',*,*,#36491,.T.) ;
#47563 = ORIENTED_EDGE('',*,*,#36492,.F.) ;
#47564 = ORIENTED_EDGE('',*,*,#36493,.T.) ;
#47565 = ORIENTED_EDGE('',*,*,#36494,.T.) ;
#47566 = ORIENTED_EDGE('',*,*,#36495,.T.) ;
#47567 = ORIENTED_EDGE('',*,*,#36496,.F.) ;
#47568 = ORIENTED_EDGE('',*,*,#36497,.T.) ;
#47569 = ORIENTED_EDGE('',*,*,#36498,.F.) ;
#47570 = ORIENTED_EDGE('',*,*,#36499,.T.) ;
#47571 = ORIENTED_EDGE('',*,*,#36500,.T.) ;
#47572 = ORIENTED_EDGE('',*,*,#36501,.T.) ;
#47573 = ORIENTED_EDGE('',*,*,#36502,.T.) ;
#47574 = ORIENTED_EDGE('',*,*,#36503,.T.) ;
#47575 = ORIENTED_EDGE('',*,*,#36504,.T.) ;
#47576 = ORIENTED_EDGE('',*,*,#36505,.T.) ;
#47577 = ORIENTED_EDGE('',*,*,#36471,.T.) ;
#47578 = ORIENTED_EDGE('',*,*,#36506,.T.) ;
#47579 = ORIENTED_EDGE('',*,*,#36481,.F.) ;
#47580 = ORIENTED_EDGE('',*,*,#36507,.T.) ;
#47581 = ORIENTED_EDGE('',*,*,#36473,.T.) ;
#47582 = ORIENTED_EDGE('',*,*,#36508,.T.) ;
#47583 = ORIENTED_EDGE('',*,*,#36479,.F.) ;
#47584 = ORIENTED_EDGE('',*,*,#36509,.T.) ;
#47585 = ORIENTED_EDGE('',*,*,#36510,.T.) ;
#47586 = ORIENTED_EDGE('',*,*,#36511,.T.) ;
#47587 = ORIENTED_EDGE('',*,*,#36447,.T.) ;
#47588 = ORIENTED_EDGE('',*,*,#36512,.T.) ;
#47589 = ORIENTED_EDGE('',*,*,#36477,.F.) ;
#47590 = ORIENTED_EDGE('',*,*,#36513,.T.) ;
#47591 = ORIENTED_EDGE('',*,*,#36514,.T.) ;
#47592 = ORIENTED_EDGE('',*,*,#36515,.T.) ;
#47593 = ORIENTED_EDGE('',*,*,#36516,.T.) ;
#47594 = ORIENTED_EDGE('',*,*,#36517,.T.) ;
#47595 = ORIENTED_EDGE('',*,*,#36518,.T.) ;
#47596 = ORIENTED_EDGE('',*,*,#36475,.F.) ;
#47597 = ORIENTED_EDGE('',*,*,#36519,.T.) ;
#47598 = ORIENTED_EDGE('',*,*,#36520,.T.) ;
#47599 = ORIENTED_EDGE('',*,*,#36521,.T.) ;
#47600 = ORIENTED_EDGE('',*,*,#36522,.T.) ;
#47601 = ORIENTED_EDGE('',*,*,#36504,.F.) ;
#47602 = ORIENTED_EDGE('',*,*,#36523,.T.) ;
#47603 = ORIENTED_EDGE('',*,*,#36524,.T.) ;
#47604 = ORIENTED_EDGE('',*,*,#36378,.T.) ;
#47605 = ORIENTED_EDGE('',*,*,#36525,.T.) ;
#47606 = ORIENTED_EDGE('',*,*,#36526,.T.) ;
#47607 = ORIENTED_EDGE('',*,*,#36502,.F.) ;
#47608 = ORIENTED_EDGE('',*,*,#36527,.T.) ;
#47609 = ORIENTED_EDGE('',*,*,#36528,.T.) ;
#47610 = ORIENTED_EDGE('',*,*,#36529,.T.) ;
#47611 = ORIENTED_EDGE('',*,*,#36530,.T.) ;
#47612 = ORIENTED_EDGE('',*,*,#36531,.T.) ;
#47613 = ORIENTED_EDGE('',*,*,#36532,.T.) ;
#47614 = ORIENTED_EDGE('',*,*,#36500,.F.) ;
#47615 = ORIENTED_EDGE('',*,*,#36533,.T.) ;
#47616 = ORIENTED_EDGE('',*,*,#36534,.T.) ;
#47617 = ORIENTED_EDGE('',*,*,#36535,.F.) ;
#47618 = ORIENTED_EDGE('',*,*,#36536,.T.) ;
#47619 = ORIENTED_EDGE('',*,*,#36537,.F.) ;
#47620 = ORIENTED_EDGE('',*,*,#36538,.T.) ;
#47621 = ORIENTED_EDGE('',*,*,#36539,.T.) ;
#47622 = ORIENTED_EDGE('',*,*,#36452,.T.) ;
#47623 = ORIENTED_EDGE('',*,*,#36540,.F.) ;
#47624 = ORIENTED_EDGE('',*,*,#36541,.T.) ;
#47625 = ORIENTED_EDGE('',*,*,#36458,.T.) ;
#47626 = ORIENTED_EDGE('',*,*,#36542,.T.) ;
#47627 = ORIENTED_EDGE('',*,*,#36543,.F.) ;
#47628 = ORIENTED_EDGE('',*,*,#36544,.T.) ;
#47629 = ORIENTED_EDGE('',*,*,#36545,.F.) ;
#47630 = ORIENTED_EDGE('',*,*,#36546,.T.) ;
#47631 = ORIENTED_EDGE('',*,*,#36547,.T.) ;
#47632 = ORIENTED_EDGE('',*,*,#36548,.T.) ;
#47633 = ORIENTED_EDGE('',*,*,#36549,.F.) ;
#47634 = ORIENTED_EDGE('',*,*,#36550,.T.) ;
#47635 = ORIENTED_EDGE('',*,*,#36551,.F.) ;
#47636 = ORIENTED_EDGE('',*,*,#36552,.T.) ;
#47637 = ORIENTED_EDGE('',*,*,#36494,.F.) ;
#47638 = ORIENTED_EDGE('',*,*,#36553,.T.) ;
#47639 = ORIENTED_EDGE('',*,*,#36554,.F.) ;
#47640 = ORIENTED_EDGE('',*,*,#36555,.T.) ;
#47641 = ORIENTED_EDGE('',*,*,#36556,.F.) ;
#47642 = ORIENTED_EDGE('',*,*,#36557,.T.) ;
#47643 = ORIENTED_EDGE('',*,*,#36558,.T.) ;
#47644 = ORIENTED_EDGE('',*,*,#36559,.T.) ;
#47645 = ORIENTED_EDGE('',*,*,#36560,.F.) ;
#47646 = ORIENTED_EDGE('',*,*,#36561,.T.) ;
#47647 = ORIENTED_EDGE('',*,*,#36389,.T.) ;
#47648 = ORIENTED_EDGE('',*,*,#36562,.F.) ;
#47649 = ORIENTED_EDGE('',*,*,#36563,.T.) ;
#47650 = ORIENTED_EDGE('',*,*,#36564,.F.) ;
#47651 = ORIENTED_EDGE('',*,*,#36468,.T.) ;
#47652 = ORIENTED_EDGE('',*,*,#36565,.T.) ;
#47653 = ORIENTED_EDGE('',*,*,#36484,.F.) ;
#47654 = ORIENTED_EDGE('',*,*,#36566,.F.) ;
#47655 = ORIENTED_EDGE('',*,*,#36567,.T.) ;
#47656 = ORIENTED_EDGE('',*,*,#36568,.F.) ;
#47657 = ORIENTED_EDGE('',*,*,#36569,.T.) ;
#47658 = ORIENTED_EDGE('',*,*,#36570,.F.) ;
#47659 = ORIENTED_EDGE('',*,*,#36571,.T.) ;
#47660 = ORIENTED_EDGE('',*,*,#36566,.T.) ;
#47661 = ORIENTED_EDGE('',*,*,#36483,.F.) ;
#47662 = ORIENTED_EDGE('',*,*,#36572,.T.) ;
#47663 = ORIENTED_EDGE('',*,*,#36469,.T.) ;
#47664 = ORIENTED_EDGE('',*,*,#36564,.T.) ;
#47665 = ORIENTED_EDGE('',*,*,#36573,.T.) ;
#47666 = ORIENTED_EDGE('',*,*,#36574,.F.) ;
#47667 = ORIENTED_EDGE('',*,*,#36575,.T.) ;
#47668 = ORIENTED_EDGE('',*,*,#36576,.T.) ;
#47669 = ORIENTED_EDGE('',*,*,#36577,.T.) ;
#47670 = ORIENTED_EDGE('',*,*,#36578,.F.) ;
#47671 = ORIENTED_EDGE('',*,*,#36579,.F.) ;
#47672 = ORIENTED_EDGE('',*,*,#36580,.T.) ;
#47673 = ORIENTED_EDGE('',*,*,#36581,.T.) ;
#47674 = ORIENTED_EDGE('',*,*,#36582,.T.) ;
#47675 = ORIENTED_EDGE('',*,*,#36583,.T.) ;
#47676 = ORIENTED_EDGE('',*,*,#36584,.T.) ;
#47677 = ORIENTED_EDGE('',*,*,#36585,.T.) ;
#47678 = ORIENTED_EDGE('',*,*,#36586,.T.) ;
#47679 = ORIENTED_EDGE('',*,*,#36587,.T.) ;
#47680 = ORIENTED_EDGE('',*,*,#36588,.T.) ;
#47681 = ORIENTED_EDGE('',*,*,#36589,.T.) ;
#47682 = ORIENTED_EDGE('',*,*,#36590,.T.) ;
#47683 = ORIENTED_EDGE('',*,*,#36591,.T.) ;
#47684 = ORIENTED_EDGE('',*,*,#36592,.T.) ;
#47685 = ORIENTED_EDGE('',*,*,#36593,.T.) ;
#47686 = ORIENTED_EDGE('',*,*,#36594,.T.) ;
#47687 = ORIENTED_EDGE('',*,*,#36595,.T.) ;
#47688 = ORIENTED_EDGE('',*,*,#36596,.T.) ;
#47689 = ORIENTED_EDGE('',*,*,#36597,.T.) ;
#47690 = ORIENTED_EDGE('',*,*,#36598,.T.) ;
#47691 = ORIENTED_EDGE('',*,*,#36599,.T.) ;
#47692 = ORIENTED_EDGE('',*,*,#36600,.T.) ;
#47693 = ORIENTED_EDGE('',*,*,#36601,.T.) ;
#47694 = ORIENTED_EDGE('',*,*,#36602,.T.) ;
#47695 = ORIENTED_EDGE('',*,*,#36603,.T.) ;
#47696 = ORIENTED_EDGE('',*,*,#36604,.T.) ;
#47697 = ORIENTED_EDGE('',*,*,#36605,.T.) ;
#47698 = ORIENTED_EDGE('',*,*,#36606,.T.) ;
#47699 = ORIENTED_EDGE('',*,*,#36607,.T.) ;
#47700 = ORIENTED_EDGE('',*,*,#36608,.T.) ;
#47701 = ORIENTED_EDGE('',*,*,#36609,.T.) ;
#47702 = ORIENTED_EDGE('',*,*,#36610,.T.) ;
#47703 = ORIENTED_EDGE('',*,*,#36611,.T.) ;
#47704 = ORIENTED_EDGE('',*,*,#36612,.T.) ;
#47705 = ORIENTED_EDGE('',*,*,#36613,.T.) ;
#47706 = ORIENTED_EDGE('',*,*,#36614,.T.) ;
#47707 = ORIENTED_EDGE('',*,*,#36615,.T.) ;
#47708 = ORIENTED_EDGE('',*,*,#36384,.T.) ;
#47709 = ORIENTED_EDGE('',*,*,#36616,.F.) ;
#47710 = ORIENTED_EDGE('',*,*,#36617,.T.) ;
#47711 = ORIENTED_EDGE('',*,*,#36618,.T.) ;
#47712 = ORIENTED_EDGE('',*,*,#36619,.T.) ;
#47713 = ORIENTED_EDGE('',*,*,#36620,.T.) ;
#47714 = ORIENTED_EDGE('',*,*,#36621,.T.) ;
#47715 = ORIENTED_EDGE('',*,*,#36622,.T.) ;
#47716 = ORIENTED_EDGE('',*,*,#36623,.T.) ;
#47717 = ORIENTED_EDGE('',*,*,#36624,.F.) ;
#47718 = ORIENTED_EDGE('',*,*,#36625,.T.) ;
#47719 = ORIENTED_EDGE('',*,*,#36462,.T.) ;
#47720 = ORIENTED_EDGE('',*,*,#36626,.T.) ;
#47721 = ORIENTED_EDGE('',*,*,#36627,.T.) ;
#47722 = ORIENTED_EDGE('',*,*,#36628,.T.) ;
#47723 = ORIENTED_EDGE('',*,*,#36629,.T.) ;
#47724 = ORIENTED_EDGE('',*,*,#36460,.F.) ;
#47725 = ORIENTED_EDGE('',*,*,#36630,.T.) ;
#47726 = ORIENTED_EDGE('',*,*,#36631,.T.) ;
#47727 = ORIENTED_EDGE('',*,*,#36632,.T.) ;
#47728 = ORIENTED_EDGE('',*,*,#36633,.T.) ;
#47729 = ORIENTED_EDGE('',*,*,#36634,.T.) ;
#47730 = ORIENTED_EDGE('',*,*,#36398,.T.) ;
#47731 = ORIENTED_EDGE('',*,*,#36635,.T.) ;
#47732 = ORIENTED_EDGE('',*,*,#36636,.T.) ;
#47733 = ORIENTED_EDGE('',*,*,#36637,.T.) ;
#47734 = ORIENTED_EDGE('',*,*,#36638,.T.) ;
#47735 = ORIENTED_EDGE('',*,*,#36639,.T.) ;
#47736 = ORIENTED_EDGE('',*,*,#36640,.T.) ;
#47737 = ORIENTED_EDGE('',*,*,#36641,.T.) ;
#47738 = ORIENTED_EDGE('',*,*,#36642,.T.) ;
#47739 = ORIENTED_EDGE('',*,*,#36643,.T.) ;
#47740 = ORIENTED_EDGE('',*,*,#36391,.T.) ;
#47741 = ORIENTED_EDGE('',*,*,#36644,.T.) ;
#47742 = ORIENTED_EDGE('',*,*,#36645,.T.) ;
#47743 = ORIENTED_EDGE('',*,*,#36646,.T.) ;
#47744 = ORIENTED_EDGE('',*,*,#36647,.T.) ;
#47745 = ORIENTED_EDGE('',*,*,#36648,.T.) ;
#47746 = ORIENTED_EDGE('',*,*,#36492,.T.) ;
#47747 = ORIENTED_EDGE('',*,*,#36649,.T.) ;
#47748 = ORIENTED_EDGE('',*,*,#36650,.T.) ;
#47749 = ORIENTED_EDGE('',*,*,#36651,.T.) ;
#47750 = ORIENTED_EDGE('',*,*,#36490,.T.) ;
#47751 = ORIENTED_EDGE('',*,*,#36652,.T.) ;
#47752 = ORIENTED_EDGE('',*,*,#36653,.F.) ;
#47753 = ORIENTED_EDGE('',*,*,#36654,.T.) ;
#47754 = ORIENTED_EDGE('',*,*,#36655,.T.) ;
#47755 = ORIENTED_EDGE('',*,*,#36656,.T.) ;
#47756 = ORIENTED_EDGE('',*,*,#36657,.T.) ;
#47757 = ORIENTED_EDGE('',*,*,#36454,.T.) ;
#47758 = ORIENTED_EDGE('',*,*,#36658,.T.) ;
#47759 = ORIENTED_EDGE('',*,*,#36659,.T.) ;
#47760 = ORIENTED_EDGE('',*,*,#36660,.T.) ;
#47761 = ORIENTED_EDGE('',*,*,#36661,.T.) ;
#47762 = ORIENTED_EDGE('',*,*,#36456,.F.) ;
#47763 = ORIENTED_EDGE('',*,*,#36662,.T.) ;
#47764 = ORIENTED_EDGE('',*,*,#36663,.T.) ;
#47765 = ORIENTED_EDGE('',*,*,#36664,.T.) ;
#47766 = ORIENTED_EDGE('',*,*,#36665,.T.) ;
#47767 = ORIENTED_EDGE('',*,*,#36666,.T.) ;
#47768 = ORIENTED_EDGE('',*,*,#36667,.T.) ;
#47769 = ORIENTED_EDGE('',*,*,#36668,.T.) ;
#47770 = ORIENTED_EDGE('',*,*,#36669,.T.) ;
#47771 = ORIENTED_EDGE('',*,*,#36670,.T.) ;
#47772 = ORIENTED_EDGE('',*,*,#36671,.T.) ;
#47773 = ORIENTED_EDGE('',*,*,#36672,.T.) ;
#47774 = ORIENTED_EDGE('',*,*,#36673,.T.) ;
#47775 = ORIENTED_EDGE('',*,*,#36674,.T.) ;
#47776 = ORIENTED_EDGE('',*,*,#36496,.T.) ;
#47777 = ORIENTED_EDGE('',*,*,#36675,.T.) ;
#47778 = ORIENTED_EDGE('',*,*,#36676,.T.) ;
#47779 = ORIENTED_EDGE('',*,*,#36677,.T.) ;
#47780 = ORIENTED_EDGE('',*,*,#36678,.T.) ;
#47781 = ORIENTED_EDGE('',*,*,#36679,.T.) ;
#47782 = ORIENTED_EDGE('',*,*,#36680,.T.) ;
#47783 = ORIENTED_EDGE('',*,*,#36681,.T.) ;
#47784 = ORIENTED_EDGE('',*,*,#36682,.T.) ;
#47785 = ORIENTED_EDGE('',*,*,#36683,.T.) ;
#47786 = ORIENTED_EDGE('',*,*,#36498,.T.) ;
#47787 = ORIENTED_EDGE('',*,*,#36684,.T.) ;
#47788 = ORIENTED_EDGE('',*,*,#36685,.T.) ;
#47789 = ORIENTED_EDGE('',*,*,#36686,.T.) ;
#47790 = ORIENTED_EDGE('',*,*,#36687,.T.) ;
#47791 = ORIENTED_EDGE('',*,*,#36688,.T.) ;
#47792 = ORIENTED_EDGE('',*,*,#36689,.T.) ;
#47793 = ORIENTED_EDGE('',*,*,#36690,.T.) ;
#47794 = ORIENTED_EDGE('',*,*,#36691,.T.) ;
#47795 = ORIENTED_EDGE('',*,*,#36383,.T.) ;
#47796 = ORIENTED_EDGE('',*,*,#36692,.T.) ;
#47797 = ORIENTED_EDGE('',*,*,#36693,.T.) ;
#47798 = ORIENTED_EDGE('',*,*,#36694,.T.) ;
#47799 = ORIENTED_EDGE('',*,*,#36695,.T.) ;
#47800 = ORIENTED_EDGE('',*,*,#36696,.T.) ;
#47801 = ORIENTED_EDGE('',*,*,#36697,.T.) ;
#47802 = ORIENTED_EDGE('',*,*,#36698,.T.) ;
#47803 = ORIENTED_EDGE('',*,*,#36699,.T.) ;
#47804 = ORIENTED_EDGE('',*,*,#36700,.T.) ;
#47805 = ORIENTED_EDGE('',*,*,#36701,.T.) ;
#47806 = ORIENTED_EDGE('',*,*,#36702,.T.) ;
#47807 = ORIENTED_EDGE('',*,*,#36703,.T.) ;
#47808 = ORIENTED_EDGE('',*,*,#36704,.T.) ;
#47809 = ORIENTED_EDGE('',*,*,#36705,.T.) ;
#47810 = ORIENTED_EDGE('',*,*,#36706,.T.) ;
#47811 = ORIENTED_EDGE('',*,*,#36707,.T.) ;
#47812 = ORIENTED_EDGE('',*,*,#36708,.T.) ;
#47813 = ORIENTED_EDGE('',*,*,#36709,.T.) ;
#47814 = ORIENTED_EDGE('',*,*,#36710,.T.) ;
#47815 = ORIENTED_EDGE('',*,*,#36711,.T.) ;
#47816 = ORIENTED_EDGE('',*,*,#36712,.T.) ;
#47817 = ORIENTED_EDGE('',*,*,#36713,.T.) ;
#47818 = ORIENTED_EDGE('',*,*,#36714,.T.) ;
#47819 = ORIENTED_EDGE('',*,*,#36715,.T.) ;
#47820 = ORIENTED_EDGE('',*,*,#36616,.T.) ;
#47821 = ORIENTED_EDGE('',*,*,#36716,.T.) ;
#47822 = ORIENTED_EDGE('',*,*,#36717,.T.) ;
#47823 = ORIENTED_EDGE('',*,*,#36718,.T.) ;
#47824 = ORIENTED_EDGE('',*,*,#36620,.F.) ;
#47825 = ORIENTED_EDGE('',*,*,#36719,.T.) ;
#47826 = ORIENTED_EDGE('',*,*,#36720,.T.) ;
#47827 = ORIENTED_EDGE('',*,*,#36721,.T.) ;
#47828 = ORIENTED_EDGE('',*,*,#36622,.F.) ;
#47829 = ORIENTED_EDGE('',*,*,#36722,.T.) ;
#47830 = ORIENTED_EDGE('',*,*,#36723,.T.) ;
#47831 = ORIENTED_EDGE('',*,*,#36724,.T.) ;
#47832 = ORIENTED_EDGE('',*,*,#36618,.F.) ;
#47833 = ORIENTED_EDGE('',*,*,#36725,.T.) ;
#47834 = ORIENTED_EDGE('',*,*,#36726,.T.) ;
#47835 = ORIENTED_EDGE('',*,*,#36727,.T.) ;
#47836 = ORIENTED_EDGE('',*,*,#36728,.T.) ;
#47837 = ORIENTED_EDGE('',*,*,#36729,.T.) ;
#47838 = ORIENTED_EDGE('',*,*,#36730,.T.) ;
#47839 = ORIENTED_EDGE('',*,*,#36731,.T.) ;
#47840 = ORIENTED_EDGE('',*,*,#36732,.T.) ;
#47841 = ORIENTED_EDGE('',*,*,#36733,.T.) ;
#47842 = ORIENTED_EDGE('',*,*,#36734,.T.) ;
#47843 = ORIENTED_EDGE('',*,*,#36735,.T.) ;
#47844 = ORIENTED_EDGE('',*,*,#36736,.T.) ;
#47845 = ORIENTED_EDGE('',*,*,#36737,.F.) ;
#47846 = ORIENTED_EDGE('',*,*,#36738,.T.) ;
#47847 = ORIENTED_EDGE('',*,*,#36414,.F.) ;
#47848 = ORIENTED_EDGE('',*,*,#36739,.T.) ;
#47849 = ORIENTED_EDGE('',*,*,#36740,.T.) ;
#47850 = ORIENTED_EDGE('',*,*,#36741,.T.) ;
#47851 = ORIENTED_EDGE('',*,*,#36742,.T.) ;
#47852 = ORIENTED_EDGE('',*,*,#36737,.T.) ;
#47853 = ORIENTED_EDGE('',*,*,#36743,.T.) ;
#47854 = ORIENTED_EDGE('',*,*,#36744,.T.) ;
#47855 = ORIENTED_EDGE('',*,*,#36745,.T.) ;
#47856 = ORIENTED_EDGE('',*,*,#36746,.T.) ;
#47857 = ORIENTED_EDGE('',*,*,#36747,.T.) ;
#47858 = ORIENTED_EDGE('',*,*,#36748,.T.) ;
#47859 = ORIENTED_EDGE('',*,*,#36749,.T.) ;
#47860 = ORIENTED_EDGE('',*,*,#36750,.T.) ;
#47861 = ORIENTED_EDGE('',*,*,#36751,.T.) ;
#47862 = ORIENTED_EDGE('',*,*,#36752,.T.) ;
#47863 = ORIENTED_EDGE('',*,*,#36753,.T.) ;
#47864 = ORIENTED_EDGE('',*,*,#36754,.T.) ;
#47865 = ORIENTED_EDGE('',*,*,#36755,.T.) ;
#47866 = ORIENTED_EDGE('',*,*,#36756,.T.) ;
#47867 = ORIENTED_EDGE('',*,*,#36757,.T.) ;
#47868 = ORIENTED_EDGE('',*,*,#36758,.F.) ;
#47869 = ORIENTED_EDGE('',*,*,#36607,.F.) ;
#47870 = ORIENTED_EDGE('',*,*,#36759,.T.) ;
#47871 = ORIENTED_EDGE('',*,*,#36758,.T.) ;
#47872 = ORIENTED_EDGE('',*,*,#36760,.T.) ;
#47873 = ORIENTED_EDGE('',*,*,#36761,.T.) ;
#47874 = ORIENTED_EDGE('',*,*,#36762,.T.) ;
#47875 = ORIENTED_EDGE('',*,*,#36763,.T.) ;
#47876 = ORIENTED_EDGE('',*,*,#36764,.T.) ;
#47877 = ORIENTED_EDGE('',*,*,#36765,.T.) ;
#47878 = ORIENTED_EDGE('',*,*,#36766,.T.) ;
#47879 = ORIENTED_EDGE('',*,*,#36767,.T.) ;
#47880 = ORIENTED_EDGE('',*,*,#36768,.T.) ;
#47881 = ORIENTED_EDGE('',*,*,#36769,.T.) ;
#47882 = ORIENTED_EDGE('',*,*,#36770,.T.) ;
#47883 = ORIENTED_EDGE('',*,*,#36771,.T.) ;
#47884 = ORIENTED_EDGE('',*,*,#36772,.T.) ;
#47885 = ORIENTED_EDGE('',*,*,#36773,.T.) ;
#47886 = ORIENTED_EDGE('',*,*,#36774,.T.) ;
#47887 = ORIENTED_EDGE('',*,*,#36775,.T.) ;
#47888 = ORIENTED_EDGE('',*,*,#36776,.T.) ;
#47889 = ORIENTED_EDGE('',*,*,#36777,.T.) ;
#47890 = ORIENTED_EDGE('',*,*,#36778,.T.) ;
#47891 = ORIENTED_EDGE('',*,*,#36779,.T.) ;
#47892 = ORIENTED_EDGE('',*,*,#36487,.F.) ;
#47893 = ORIENTED_EDGE('',*,*,#36780,.T.) ;
#47894 = ORIENTED_EDGE('',*,*,#36781,.T.) ;
#47895 = ORIENTED_EDGE('',*,*,#36401,.T.) ;
#47896 = ORIENTED_EDGE('',*,*,#36782,.T.) ;
#47897 = ORIENTED_EDGE('',*,*,#36465,.F.) ;
#47898 = ORIENTED_EDGE('',*,*,#36783,.T.) ;
#47899 = ORIENTED_EDGE('',*,*,#36784,.T.) ;
#47900 = ORIENTED_EDGE('',*,*,#36785,.T.) ;
#47901 = ORIENTED_EDGE('',*,*,#36786,.F.) ;
#47902 = ORIENTED_EDGE('',*,*,#36684,.F.) ;
#47903 = ORIENTED_EDGE('',*,*,#36497,.F.) ;
#47904 = ORIENTED_EDGE('',*,*,#36677,.F.) ;
#47905 = ORIENTED_EDGE('',*,*,#36787,.F.) ;
#47906 = ORIENTED_EDGE('',*,*,#36786,.T.) ;
#47907 = ORIENTED_EDGE('',*,*,#36788,.F.) ;
#47908 = ORIENTED_EDGE('',*,*,#36495,.F.) ;
#47909 = ORIENTED_EDGE('',*,*,#36552,.F.) ;
#47910 = ORIENTED_EDGE('',*,*,#36789,.F.) ;
#47911 = ORIENTED_EDGE('',*,*,#36675,.F.) ;
#47912 = ORIENTED_EDGE('',*,*,#36788,.T.) ;
#47913 = ORIENTED_EDGE('',*,*,#36676,.F.) ;
#47914 = ORIENTED_EDGE('',*,*,#36790,.F.) ;
#47915 = ORIENTED_EDGE('',*,*,#36672,.F.) ;
#47916 = ORIENTED_EDGE('',*,*,#36787,.T.) ;
#47917 = ORIENTED_EDGE('',*,*,#36671,.F.) ;
#47918 = ORIENTED_EDGE('',*,*,#36791,.F.) ;
#47919 = ORIENTED_EDGE('',*,*,#36685,.F.) ;
#47920 = ORIENTED_EDGE('',*,*,#36789,.T.) ;
#47921 = ORIENTED_EDGE('',*,*,#36551,.T.) ;
#47922 = ORIENTED_EDGE('',*,*,#36792,.F.) ;
#47923 = ORIENTED_EDGE('',*,*,#36790,.T.) ;
#47924 = ORIENTED_EDGE('',*,*,#36793,.F.) ;
#47925 = ORIENTED_EDGE('',*,*,#36791,.T.) ;
#47926 = ORIENTED_EDGE('',*,*,#36794,.F.) ;
#47927 = ORIENTED_EDGE('',*,*,#36455,.F.) ;
#47928 = ORIENTED_EDGE('',*,*,#36657,.F.) ;
#47929 = ORIENTED_EDGE('',*,*,#36795,.F.) ;
#47930 = ORIENTED_EDGE('',*,*,#36662,.F.) ;
#47931 = ORIENTED_EDGE('',*,*,#36796,.F.) ;
#47932 = ORIENTED_EDGE('',*,*,#36660,.F.) ;
#47933 = ORIENTED_EDGE('',*,*,#36797,.F.) ;
#47934 = ORIENTED_EDGE('',*,*,#36666,.F.) ;
#47935 = ORIENTED_EDGE('',*,*,#36457,.F.) ;
#47936 = ORIENTED_EDGE('',*,*,#36661,.F.) ;
#47937 = ORIENTED_EDGE('',*,*,#36798,.F.) ;
#47938 = ORIENTED_EDGE('',*,*,#36542,.F.) ;
#47939 = ORIENTED_EDGE('',*,*,#36792,.T.) ;
#47940 = ORIENTED_EDGE('',*,*,#36550,.F.) ;
#47941 = ORIENTED_EDGE('',*,*,#36799,.F.) ;
#47942 = ORIENTED_EDGE('',*,*,#36673,.F.) ;
#47943 = ORIENTED_EDGE('',*,*,#36794,.T.) ;
#47944 = ORIENTED_EDGE('',*,*,#36674,.F.) ;
#47945 = ORIENTED_EDGE('',*,*,#36800,.F.) ;
#47946 = ORIENTED_EDGE('',*,*,#36681,.F.) ;
#47947 = ORIENTED_EDGE('',*,*,#36793,.T.) ;
#47948 = ORIENTED_EDGE('',*,*,#36680,.F.) ;
#47949 = ORIENTED_EDGE('',*,*,#36801,.F.) ;
#47950 = ORIENTED_EDGE('',*,*,#36682,.F.) ;
#47951 = ORIENTED_EDGE('',*,*,#36499,.F.) ;
#47952 = ORIENTED_EDGE('',*,*,#36683,.F.) ;
#47953 = ORIENTED_EDGE('',*,*,#36802,.F.) ;
#47954 = ORIENTED_EDGE('',*,*,#36533,.F.) ;
#47955 = ORIENTED_EDGE('',*,*,#36797,.T.) ;
#47956 = ORIENTED_EDGE('',*,*,#36795,.T.) ;
#47957 = ORIENTED_EDGE('',*,*,#36803,.F.) ;
#47958 = ORIENTED_EDGE('',*,*,#36798,.T.) ;
#47959 = ORIENTED_EDGE('',*,*,#36796,.T.) ;
#47960 = ORIENTED_EDGE('',*,*,#36804,.F.) ;
#47961 = ORIENTED_EDGE('',*,*,#36543,.T.) ;
#47962 = ORIENTED_EDGE('',*,*,#36799,.T.) ;
#47963 = ORIENTED_EDGE('',*,*,#36549,.T.) ;
#47964 = ORIENTED_EDGE('',*,*,#36805,.F.) ;
#47965 = ORIENTED_EDGE('',*,*,#36800,.T.) ;
#47966 = ORIENTED_EDGE('',*,*,#36802,.T.) ;
#47967 = ORIENTED_EDGE('',*,*,#36801,.T.) ;
#47968 = ORIENTED_EDGE('',*,*,#36806,.F.) ;
#47969 = ORIENTED_EDGE('',*,*,#36803,.T.) ;
#47970 = ORIENTED_EDGE('',*,*,#36656,.F.) ;
#47971 = ORIENTED_EDGE('',*,*,#36807,.F.) ;
#47972 = ORIENTED_EDGE('',*,*,#36663,.F.) ;
#47973 = ORIENTED_EDGE('',*,*,#36808,.F.) ;
#47974 = ORIENTED_EDGE('',*,*,#36664,.F.) ;
#47975 = ORIENTED_EDGE('',*,*,#36809,.F.) ;
#47976 = ORIENTED_EDGE('',*,*,#36670,.F.) ;
#47977 = ORIENTED_EDGE('',*,*,#36804,.T.) ;
#47978 = ORIENTED_EDGE('',*,*,#36665,.F.) ;
#47979 = ORIENTED_EDGE('',*,*,#36810,.F.) ;
#47980 = ORIENTED_EDGE('',*,*,#36544,.F.) ;
#47981 = ORIENTED_EDGE('',*,*,#36805,.T.) ;
#47982 = ORIENTED_EDGE('',*,*,#36548,.F.) ;
#47983 = ORIENTED_EDGE('',*,*,#36811,.F.) ;
#47984 = ORIENTED_EDGE('',*,*,#36678,.F.) ;
#47985 = ORIENTED_EDGE('',*,*,#36806,.T.) ;
#47986 = ORIENTED_EDGE('',*,*,#36679,.F.) ;
#47987 = ORIENTED_EDGE('',*,*,#36812,.F.) ;
#47988 = ORIENTED_EDGE('',*,*,#36534,.F.) ;
#47989 = ORIENTED_EDGE('',*,*,#36809,.T.) ;
#47990 = ORIENTED_EDGE('',*,*,#36807,.T.) ;
#47991 = ORIENTED_EDGE('',*,*,#36813,.F.) ;
#47992 = ORIENTED_EDGE('',*,*,#36810,.T.) ;
#47993 = ORIENTED_EDGE('',*,*,#36808,.T.) ;
#47994 = ORIENTED_EDGE('',*,*,#36814,.F.) ;
#47995 = ORIENTED_EDGE('',*,*,#36545,.T.) ;
#47996 = ORIENTED_EDGE('',*,*,#36812,.T.) ;
#47997 = ORIENTED_EDGE('',*,*,#36811,.T.) ;
#47998 = ORIENTED_EDGE('',*,*,#36815,.F.) ;
#47999 = ORIENTED_EDGE('',*,*,#36535,.T.) ;
#48000 = ORIENTED_EDGE('',*,*,#36453,.F.) ;
#48001 = ORIENTED_EDGE('',*,*,#36539,.F.) ;
#48002 = ORIENTED_EDGE('',*,*,#36816,.F.) ;
#48003 = ORIENTED_EDGE('',*,*,#36658,.F.) ;
#48004 = ORIENTED_EDGE('',*,*,#36813,.T.) ;
#48005 = ORIENTED_EDGE('',*,*,#36659,.F.) ;
#48006 = ORIENTED_EDGE('',*,*,#36817,.F.) ;
#48007 = ORIENTED_EDGE('',*,*,#36667,.F.) ;
#48008 = ORIENTED_EDGE('',*,*,#36814,.T.) ;
#48009 = ORIENTED_EDGE('',*,*,#36669,.F.) ;
#48010 = ORIENTED_EDGE('',*,*,#36818,.F.) ;
#48011 = ORIENTED_EDGE('',*,*,#36546,.F.) ;
#48012 = ORIENTED_EDGE('',*,*,#36815,.T.) ;
#48013 = ORIENTED_EDGE('',*,*,#36547,.F.) ;
#48014 = ORIENTED_EDGE('',*,*,#36819,.F.) ;
#48015 = ORIENTED_EDGE('',*,*,#36536,.F.) ;
#48016 = ORIENTED_EDGE('',*,*,#36817,.T.) ;
#48017 = ORIENTED_EDGE('',*,*,#36816,.T.) ;
#48018 = ORIENTED_EDGE('',*,*,#36820,.F.) ;
#48019 = ORIENTED_EDGE('',*,*,#36819,.T.) ;
#48020 = ORIENTED_EDGE('',*,*,#36818,.T.) ;
#48021 = ORIENTED_EDGE('',*,*,#36821,.F.) ;
#48022 = ORIENTED_EDGE('',*,*,#36537,.T.) ;
#48023 = ORIENTED_EDGE('',*,*,#36820,.T.) ;
#48024 = ORIENTED_EDGE('',*,*,#36538,.F.) ;
#48025 = ORIENTED_EDGE('',*,*,#36821,.T.) ;
#48026 = ORIENTED_EDGE('',*,*,#36668,.F.) ;
#48027 = ORIENTED_EDGE('',*,*,#36822,.F.) ;
#48028 = ORIENTED_EDGE('',*,*,#36823,.F.) ;
#48029 = ORIENTED_EDGE('',*,*,#36824,.F.) ;
#48030 = ORIENTED_EDGE('',*,*,#36615,.F.) ;
#48031 = ORIENTED_EDGE('',*,*,#36825,.T.) ;
#48032 = ORIENTED_EDGE('',*,*,#36826,.T.) ;
#48033 = ORIENTED_EDGE('',*,*,#36597,.F.) ;
#48034 = ORIENTED_EDGE('',*,*,#36823,.T.) ;
#48035 = ORIENTED_EDGE('',*,*,#36596,.F.) ;
#48036 = ORIENTED_EDGE('',*,*,#36827,.T.) ;
#48037 = ORIENTED_EDGE('',*,*,#36828,.T.) ;
#48038 = ORIENTED_EDGE('',*,*,#36589,.F.) ;
#48039 = ORIENTED_EDGE('',*,*,#36824,.T.) ;
#48040 = ORIENTED_EDGE('',*,*,#36822,.T.) ;
#48041 = ORIENTED_EDGE('',*,*,#36588,.F.) ;
#48042 = ORIENTED_EDGE('',*,*,#36829,.F.) ;
#48043 = ORIENTED_EDGE('',*,*,#36608,.F.) ;
#48044 = ORIENTED_EDGE('',*,*,#36604,.F.) ;
#48045 = ORIENTED_EDGE('',*,*,#36830,.T.) ;
#48046 = ORIENTED_EDGE('',*,*,#36831,.T.) ;
#48047 = ORIENTED_EDGE('',*,*,#36614,.F.) ;
#48048 = ORIENTED_EDGE('',*,*,#36832,.T.) ;
#48049 = ORIENTED_EDGE('',*,*,#36833,.T.) ;
#48050 = ORIENTED_EDGE('',*,*,#36582,.F.) ;
#48051 = ORIENTED_EDGE('',*,*,#36834,.T.) ;
#48052 = ORIENTED_EDGE('',*,*,#36835,.T.) ;
#48053 = ORIENTED_EDGE('',*,*,#36598,.F.) ;
#48054 = ORIENTED_EDGE('',*,*,#36836,.T.) ;
#48055 = ORIENTED_EDGE('',*,*,#36837,.T.) ;
#48056 = ORIENTED_EDGE('',*,*,#36838,.F.) ;
#48057 = ORIENTED_EDGE('',*,*,#36829,.T.) ;
#48058 = ORIENTED_EDGE('',*,*,#36839,.F.) ;
#48059 = ORIENTED_EDGE('',*,*,#36579,.T.) ;
#48060 = ORIENTED_EDGE('',*,*,#36840,.F.) ;
#48061 = ORIENTED_EDGE('',*,*,#36841,.F.) ;
#48062 = ORIENTED_EDGE('',*,*,#36609,.F.) ;
#48063 = ORIENTED_EDGE('',*,*,#36838,.T.) ;
#48064 = ORIENTED_EDGE('',*,*,#36841,.T.) ;
#48065 = ORIENTED_EDGE('',*,*,#36842,.F.) ;
#48066 = ORIENTED_EDGE('',*,*,#36843,.F.) ;
#48067 = ORIENTED_EDGE('',*,*,#36593,.F.) ;
#48068 = ORIENTED_EDGE('',*,*,#36844,.T.) ;
#48069 = ORIENTED_EDGE('',*,*,#36845,.T.) ;
#48070 = ORIENTED_EDGE('',*,*,#36613,.F.) ;
#48071 = ORIENTED_EDGE('',*,*,#36846,.F.) ;
#48072 = ORIENTED_EDGE('',*,*,#36583,.F.) ;
#48073 = ORIENTED_EDGE('',*,*,#36847,.T.) ;
#48074 = ORIENTED_EDGE('',*,*,#36848,.T.) ;
#48075 = ORIENTED_EDGE('',*,*,#36590,.F.) ;
#48076 = ORIENTED_EDGE('',*,*,#36849,.F.) ;
#48077 = ORIENTED_EDGE('',*,*,#36839,.T.) ;
#48078 = ORIENTED_EDGE('',*,*,#36587,.F.) ;
#48079 = ORIENTED_EDGE('',*,*,#36850,.F.) ;
#48080 = ORIENTED_EDGE('',*,*,#36851,.F.) ;
#48081 = ORIENTED_EDGE('',*,*,#36852,.F.) ;
#48082 = ORIENTED_EDGE('',*,*,#36563,.F.) ;
#48083 = ORIENTED_EDGE('',*,*,#36853,.F.) ;
#48084 = ORIENTED_EDGE('',*,*,#36840,.T.) ;
#48085 = ORIENTED_EDGE('',*,*,#36581,.F.) ;
#48086 = ORIENTED_EDGE('',*,*,#36853,.T.) ;
#48087 = ORIENTED_EDGE('',*,*,#36562,.T.) ;
#48088 = ORIENTED_EDGE('',*,*,#36854,.F.) ;
#48089 = ORIENTED_EDGE('',*,*,#36842,.T.) ;
#48090 = ORIENTED_EDGE('',*,*,#36610,.F.) ;
#48091 = ORIENTED_EDGE('',*,*,#36843,.T.) ;
#48092 = ORIENTED_EDGE('',*,*,#36855,.F.) ;
#48093 = ORIENTED_EDGE('',*,*,#36856,.F.) ;
#48094 = ORIENTED_EDGE('',*,*,#36849,.T.) ;
#48095 = ORIENTED_EDGE('',*,*,#36846,.T.) ;
#48096 = ORIENTED_EDGE('',*,*,#36857,.F.) ;
#48097 = ORIENTED_EDGE('',*,*,#36858,.F.) ;
#48098 = ORIENTED_EDGE('',*,*,#36850,.T.) ;
#48099 = ORIENTED_EDGE('',*,*,#36859,.F.) ;
#48100 = ORIENTED_EDGE('',*,*,#36580,.F.) ;
#48101 = ORIENTED_EDGE('',*,*,#36851,.T.) ;
#48102 = ORIENTED_EDGE('',*,*,#36860,.F.) ;
#48103 = ORIENTED_EDGE('',*,*,#36573,.F.) ;
#48104 = ORIENTED_EDGE('',*,*,#36852,.T.) ;
#48105 = ORIENTED_EDGE('',*,*,#36861,.F.) ;
#48106 = ORIENTED_EDGE('',*,*,#36855,.T.) ;
#48107 = ORIENTED_EDGE('',*,*,#36854,.T.) ;
#48108 = ORIENTED_EDGE('',*,*,#36569,.F.) ;
#48109 = ORIENTED_EDGE('',*,*,#36856,.T.) ;
#48110 = ORIENTED_EDGE('',*,*,#36862,.F.) ;
#48111 = ORIENTED_EDGE('',*,*,#36863,.F.) ;
#48112 = ORIENTED_EDGE('',*,*,#36857,.T.) ;
#48113 = ORIENTED_EDGE('',*,*,#36612,.F.) ;
#48114 = ORIENTED_EDGE('',*,*,#36864,.F.) ;
#48115 = ORIENTED_EDGE('',*,*,#36584,.F.) ;
#48116 = ORIENTED_EDGE('',*,*,#36859,.T.) ;
#48117 = ORIENTED_EDGE('',*,*,#36586,.F.) ;
#48118 = ORIENTED_EDGE('',*,*,#36865,.F.) ;
#48119 = ORIENTED_EDGE('',*,*,#36866,.F.) ;
#48120 = ORIENTED_EDGE('',*,*,#36860,.T.) ;
#48121 = ORIENTED_EDGE('',*,*,#36858,.T.) ;
#48122 = ORIENTED_EDGE('',*,*,#36867,.F.) ;
#48123 = ORIENTED_EDGE('',*,*,#36574,.T.) ;
#48124 = ORIENTED_EDGE('',*,*,#36861,.T.) ;
#48125 = ORIENTED_EDGE('',*,*,#36568,.T.) ;
#48126 = ORIENTED_EDGE('',*,*,#36868,.F.) ;
#48127 = ORIENTED_EDGE('',*,*,#36862,.T.) ;
#48128 = ORIENTED_EDGE('',*,*,#36869,.F.) ;
#48129 = ORIENTED_EDGE('',*,*,#36870,.F.) ;
#48130 = ORIENTED_EDGE('',*,*,#36611,.F.) ;
#48131 = ORIENTED_EDGE('',*,*,#36863,.T.) ;
#48132 = ORIENTED_EDGE('',*,*,#36870,.T.) ;
#48133 = ORIENTED_EDGE('',*,*,#36578,.T.) ;
#48134 = ORIENTED_EDGE('',*,*,#36871,.F.) ;
#48135 = ORIENTED_EDGE('',*,*,#36864,.T.) ;
#48136 = ORIENTED_EDGE('',*,*,#36872,.F.) ;
#48137 = ORIENTED_EDGE('',*,*,#36865,.T.) ;
#48138 = ORIENTED_EDGE('',*,*,#36873,.F.) ;
#48139 = ORIENTED_EDGE('',*,*,#36867,.T.) ;
#48140 = ORIENTED_EDGE('',*,*,#36866,.T.) ;
#48141 = ORIENTED_EDGE('',*,*,#36874,.F.) ;
#48142 = ORIENTED_EDGE('',*,*,#36575,.F.) ;
#48143 = ORIENTED_EDGE('',*,*,#36868,.T.) ;
#48144 = ORIENTED_EDGE('',*,*,#36567,.F.) ;
#48145 = ORIENTED_EDGE('',*,*,#36875,.F.) ;
#48146 = ORIENTED_EDGE('',*,*,#36576,.F.) ;
#48147 = ORIENTED_EDGE('',*,*,#36869,.T.) ;
#48148 = ORIENTED_EDGE('',*,*,#36585,.F.) ;
#48149 = ORIENTED_EDGE('',*,*,#36871,.T.) ;
#48150 = ORIENTED_EDGE('',*,*,#36876,.F.) ;
#48151 = ORIENTED_EDGE('',*,*,#36873,.T.) ;
#48152 = ORIENTED_EDGE('',*,*,#36874,.T.) ;
#48153 = ORIENTED_EDGE('',*,*,#36872,.T.) ;
#48154 = ORIENTED_EDGE('',*,*,#36877,.F.) ;
#48155 = ORIENTED_EDGE('',*,*,#36570,.T.) ;
#48156 = ORIENTED_EDGE('',*,*,#36875,.T.) ;
#48157 = ORIENTED_EDGE('',*,*,#36571,.F.) ;
#48158 = ORIENTED_EDGE('',*,*,#36877,.T.) ;
#48159 = ORIENTED_EDGE('',*,*,#36876,.T.) ;
#48160 = ORIENTED_EDGE('',*,*,#36577,.F.) ;
#48161 = ORIENTED_EDGE('',*,*,#36878,.F.) ;
#48162 = ORIENTED_EDGE('',*,*,#36626,.F.) ;
#48163 = ORIENTED_EDGE('',*,*,#36461,.F.) ;
#48164 = ORIENTED_EDGE('',*,*,#36632,.F.) ;
#48165 = ORIENTED_EDGE('',*,*,#36879,.F.) ;
#48166 = ORIENTED_EDGE('',*,*,#36878,.T.) ;
#48167 = ORIENTED_EDGE('',*,*,#36880,.F.) ;
#48168 = ORIENTED_EDGE('',*,*,#36459,.F.) ;
#48169 = ORIENTED_EDGE('',*,*,#36541,.F.) ;
#48170 = ORIENTED_EDGE('',*,*,#36881,.F.) ;
#48171 = ORIENTED_EDGE('',*,*,#36630,.F.) ;
#48172 = ORIENTED_EDGE('',*,*,#36880,.T.) ;
#48173 = ORIENTED_EDGE('',*,*,#36631,.F.) ;
#48174 = ORIENTED_EDGE('',*,*,#36882,.F.) ;
#48175 = ORIENTED_EDGE('',*,*,#36637,.F.) ;
#48176 = ORIENTED_EDGE('',*,*,#36879,.T.) ;
#48177 = ORIENTED_EDGE('',*,*,#36636,.F.) ;
#48178 = ORIENTED_EDGE('',*,*,#36883,.F.) ;
#48179 = ORIENTED_EDGE('',*,*,#36627,.F.) ;
#48180 = ORIENTED_EDGE('',*,*,#36463,.F.) ;
#48181 = ORIENTED_EDGE('',*,*,#36625,.F.) ;
#48182 = ORIENTED_EDGE('',*,*,#36884,.F.) ;
#48183 = ORIENTED_EDGE('',*,*,#36436,.F.) ;
#48184 = ORIENTED_EDGE('',*,*,#36404,.F.) ;
#48185 = ORIENTED_EDGE('',*,*,#36885,.T.) ;
#48186 = ORIENTED_EDGE('',*,*,#36433,.F.) ;
#48187 = ORIENTED_EDGE('',*,*,#36886,.F.) ;
#48188 = ORIENTED_EDGE('',*,*,#36881,.T.) ;
#48189 = ORIENTED_EDGE('',*,*,#36540,.T.) ;
#48190 = ORIENTED_EDGE('',*,*,#36887,.F.) ;
#48191 = ORIENTED_EDGE('',*,*,#36882,.T.) ;
#48192 = ORIENTED_EDGE('',*,*,#36888,.F.) ;
#48193 = ORIENTED_EDGE('',*,*,#36883,.T.) ;
#48194 = ORIENTED_EDGE('',*,*,#36889,.F.) ;
#48195 = ORIENTED_EDGE('',*,*,#36884,.T.) ;
#48196 = ORIENTED_EDGE('',*,*,#36624,.T.) ;
#48197 = ORIENTED_EDGE('',*,*,#36890,.F.) ;
#48198 = ORIENTED_EDGE('',*,*,#36886,.T.) ;
#48199 = ORIENTED_EDGE('',*,*,#36887,.T.) ;
#48200 = ORIENTED_EDGE('',*,*,#36561,.F.) ;
#48201 = ORIENTED_EDGE('',*,*,#36891,.F.) ;
#48202 = ORIENTED_EDGE('',*,*,#36638,.F.) ;
#48203 = ORIENTED_EDGE('',*,*,#36889,.T.) ;
#48204 = ORIENTED_EDGE('',*,*,#36639,.F.) ;
#48205 = ORIENTED_EDGE('',*,*,#36892,.F.) ;
#48206 = ORIENTED_EDGE('',*,*,#36633,.F.) ;
#48207 = ORIENTED_EDGE('',*,*,#36888,.T.) ;
#48208 = ORIENTED_EDGE('',*,*,#36635,.F.) ;
#48209 = ORIENTED_EDGE('',*,*,#36893,.F.) ;
#48210 = ORIENTED_EDGE('',*,*,#36628,.F.) ;
#48211 = ORIENTED_EDGE('',*,*,#36890,.T.) ;
#48212 = ORIENTED_EDGE('',*,*,#36629,.F.) ;
#48213 = ORIENTED_EDGE('',*,*,#36894,.F.) ;
#48214 = ORIENTED_EDGE('',*,*,#36405,.F.) ;
#48215 = ORIENTED_EDGE('',*,*,#36439,.F.) ;
#48216 = ORIENTED_EDGE('',*,*,#36895,.T.) ;
#48217 = ORIENTED_EDGE('',*,*,#36410,.F.) ;
#48218 = ORIENTED_EDGE('',*,*,#36896,.F.) ;
#48219 = ORIENTED_EDGE('',*,*,#36489,.F.) ;
#48220 = ORIENTED_EDGE('',*,*,#36440,.F.) ;
#48221 = ORIENTED_EDGE('',*,*,#36897,.F.) ;
#48222 = ORIENTED_EDGE('',*,*,#36652,.F.) ;
#48223 = ORIENTED_EDGE('',*,*,#36491,.F.) ;
#48224 = ORIENTED_EDGE('',*,*,#36651,.F.) ;
#48225 = ORIENTED_EDGE('',*,*,#36898,.F.) ;
#48226 = ORIENTED_EDGE('',*,*,#36649,.F.) ;
#48227 = ORIENTED_EDGE('',*,*,#36891,.T.) ;
#48228 = ORIENTED_EDGE('',*,*,#36560,.T.) ;
#48229 = ORIENTED_EDGE('',*,*,#36899,.F.) ;
#48230 = ORIENTED_EDGE('',*,*,#36892,.T.) ;
#48231 = ORIENTED_EDGE('',*,*,#36894,.T.) ;
#48232 = ORIENTED_EDGE('',*,*,#36893,.T.) ;
#48233 = ORIENTED_EDGE('',*,*,#36397,.F.) ;
#48234 = ORIENTED_EDGE('',*,*,#36897,.T.) ;
#48235 = ORIENTED_EDGE('',*,*,#36896,.T.) ;
#48236 = ORIENTED_EDGE('',*,*,#36900,.F.) ;
#48237 = ORIENTED_EDGE('',*,*,#36653,.T.) ;
#48238 = ORIENTED_EDGE('',*,*,#36901,.F.) ;
#48239 = ORIENTED_EDGE('',*,*,#36898,.T.) ;
#48240 = ORIENTED_EDGE('',*,*,#36902,.F.) ;
#48241 = ORIENTED_EDGE('',*,*,#36899,.T.) ;
#48242 = ORIENTED_EDGE('',*,*,#36559,.F.) ;
#48243 = ORIENTED_EDGE('',*,*,#36903,.F.) ;
#48244 = ORIENTED_EDGE('',*,*,#36634,.F.) ;
#48245 = ORIENTED_EDGE('',*,*,#36900,.T.) ;
#48246 = ORIENTED_EDGE('',*,*,#36409,.F.) ;
#48247 = ORIENTED_EDGE('',*,*,#36904,.F.) ;
#48248 = ORIENTED_EDGE('',*,*,#36654,.F.) ;
#48249 = ORIENTED_EDGE('',*,*,#36905,.F.) ;
#48250 = ORIENTED_EDGE('',*,*,#36655,.F.) ;
#48251 = ORIENTED_EDGE('',*,*,#36906,.F.) ;
#48252 = ORIENTED_EDGE('',*,*,#36646,.F.) ;
#48253 = ORIENTED_EDGE('',*,*,#36902,.T.) ;
#48254 = ORIENTED_EDGE('',*,*,#36650,.F.) ;
#48255 = ORIENTED_EDGE('',*,*,#36907,.F.) ;
#48256 = ORIENTED_EDGE('',*,*,#36640,.F.) ;
#48257 = ORIENTED_EDGE('',*,*,#36901,.T.) ;
#48258 = ORIENTED_EDGE('',*,*,#36643,.F.) ;
#48259 = ORIENTED_EDGE('',*,*,#36908,.F.) ;
#48260 = ORIENTED_EDGE('',*,*,#36647,.F.) ;
#48261 = ORIENTED_EDGE('',*,*,#36493,.F.) ;
#48262 = ORIENTED_EDGE('',*,*,#36648,.F.) ;
#48263 = ORIENTED_EDGE('',*,*,#36909,.F.) ;
#48264 = ORIENTED_EDGE('',*,*,#36553,.F.) ;
#48265 = ORIENTED_EDGE('',*,*,#36395,.T.) ;
#48266 = ORIENTED_EDGE('',*,*,#36903,.T.) ;
#48267 = ORIENTED_EDGE('',*,*,#36910,.F.) ;
#48268 = ORIENTED_EDGE('',*,*,#36406,.T.) ;
#48269 = ORIENTED_EDGE('',*,*,#36906,.T.) ;
#48270 = ORIENTED_EDGE('',*,*,#36904,.T.) ;
#48271 = ORIENTED_EDGE('',*,*,#36393,.F.) ;
#48272 = ORIENTED_EDGE('',*,*,#36911,.F.) ;
#48273 = ORIENTED_EDGE('',*,*,#36911,.T.) ;
#48274 = ORIENTED_EDGE('',*,*,#36392,.F.) ;
#48275 = ORIENTED_EDGE('',*,*,#36907,.T.) ;
#48276 = ORIENTED_EDGE('',*,*,#36905,.T.) ;
#48277 = ORIENTED_EDGE('',*,*,#36912,.F.) ;
#48278 = ORIENTED_EDGE('',*,*,#36909,.T.) ;
#48279 = ORIENTED_EDGE('',*,*,#36908,.T.) ;
#48280 = ORIENTED_EDGE('',*,*,#36913,.F.) ;
#48281 = ORIENTED_EDGE('',*,*,#36554,.T.) ;
#48282 = ORIENTED_EDGE('',*,*,#36910,.T.) ;
#48283 = ORIENTED_EDGE('',*,*,#36558,.F.) ;
#48284 = ORIENTED_EDGE('',*,*,#36914,.F.) ;
#48285 = ORIENTED_EDGE('',*,*,#36407,.F.) ;
#48286 = ORIENTED_EDGE('',*,*,#36912,.T.) ;
#48287 = ORIENTED_EDGE('',*,*,#36645,.F.) ;
#48288 = ORIENTED_EDGE('',*,*,#36915,.F.) ;
#48289 = ORIENTED_EDGE('',*,*,#36641,.F.) ;
#48290 = ORIENTED_EDGE('',*,*,#36913,.T.) ;
#48291 = ORIENTED_EDGE('',*,*,#36642,.F.) ;
#48292 = ORIENTED_EDGE('',*,*,#36916,.F.) ;
#48293 = ORIENTED_EDGE('',*,*,#36555,.F.) ;
#48294 = ORIENTED_EDGE('',*,*,#36408,.T.) ;
#48295 = ORIENTED_EDGE('',*,*,#36914,.T.) ;
#48296 = ORIENTED_EDGE('',*,*,#36917,.F.) ;
#48297 = ORIENTED_EDGE('',*,*,#36390,.T.) ;
#48298 = ORIENTED_EDGE('',*,*,#36916,.T.) ;
#48299 = ORIENTED_EDGE('',*,*,#36915,.T.) ;
#48300 = ORIENTED_EDGE('',*,*,#36918,.F.) ;
#48301 = ORIENTED_EDGE('',*,*,#36556,.T.) ;
#48302 = ORIENTED_EDGE('',*,*,#36917,.T.) ;
#48303 = ORIENTED_EDGE('',*,*,#36557,.F.) ;
#48304 = ORIENTED_EDGE('',*,*,#36918,.T.) ;
#48305 = ORIENTED_EDGE('',*,*,#36644,.F.) ;
#48306 = ORIENTED_EDGE('',*,*,#36413,.F.) ;
#48307 = ORIENTED_EDGE('',*,*,#36919,.T.) ;
#48308 = ORIENTED_EDGE('',*,*,#36734,.F.) ;
#48309 = ORIENTED_EDGE('',*,*,#36920,.F.) ;
#48310 = ORIENTED_EDGE('',*,*,#36739,.F.) ;
#48311 = ORIENTED_EDGE('',*,*,#36733,.F.) ;
#48312 = ORIENTED_EDGE('',*,*,#36921,.T.) ;
#48313 = ORIENTED_EDGE('',*,*,#36740,.F.) ;
#48314 = ORIENTED_EDGE('',*,*,#36920,.T.) ;
#48315 = ORIENTED_EDGE('',*,*,#36736,.F.) ;
#48316 = ORIENTED_EDGE('',*,*,#36922,.T.) ;
#48317 = ORIENTED_EDGE('',*,*,#36602,.F.) ;
#48318 = ORIENTED_EDGE('',*,*,#36760,.F.) ;
#48319 = ORIENTED_EDGE('',*,*,#36923,.F.) ;
#48320 = ORIENTED_EDGE('',*,*,#36745,.F.) ;
#48321 = ORIENTED_EDGE('',*,*,#36924,.T.) ;
#48322 = ORIENTED_EDGE('',*,*,#36773,.F.) ;
#48323 = ORIENTED_EDGE('',*,*,#36925,.F.) ;
#48324 = ORIENTED_EDGE('',*,*,#36730,.F.) ;
#48325 = ORIENTED_EDGE('',*,*,#36926,.T.) ;
#48326 = ORIENTED_EDGE('',*,*,#36415,.F.) ;
#48327 = ORIENTED_EDGE('',*,*,#36738,.F.) ;
#48328 = ORIENTED_EDGE('',*,*,#36927,.F.) ;
#48329 = ORIENTED_EDGE('',*,*,#36757,.F.) ;
#48330 = ORIENTED_EDGE('',*,*,#36928,.T.) ;
#48331 = ORIENTED_EDGE('',*,*,#36731,.F.) ;
#48332 = ORIENTED_EDGE('',*,*,#36923,.T.) ;
#48333 = ORIENTED_EDGE('',*,*,#36929,.F.) ;
#48334 = ORIENTED_EDGE('',*,*,#36925,.T.) ;
#48335 = ORIENTED_EDGE('',*,*,#36930,.F.) ;
#48336 = ORIENTED_EDGE('',*,*,#36742,.F.) ;
#48337 = ORIENTED_EDGE('',*,*,#36931,.T.) ;
#48338 = ORIENTED_EDGE('',*,*,#36725,.F.) ;
#48339 = ORIENTED_EDGE('',*,*,#36927,.T.) ;
#48340 = ORIENTED_EDGE('',*,*,#36775,.F.) ;
#48341 = ORIENTED_EDGE('',*,*,#36932,.T.) ;
#48342 = ORIENTED_EDGE('',*,*,#36751,.F.) ;
#48343 = ORIENTED_EDGE('',*,*,#36933,.F.) ;
#48344 = ORIENTED_EDGE('',*,*,#36930,.T.) ;
#48345 = ORIENTED_EDGE('',*,*,#36776,.F.) ;
#48346 = ORIENTED_EDGE('',*,*,#36934,.F.) ;
#48347 = ORIENTED_EDGE('',*,*,#36750,.F.) ;
#48348 = ORIENTED_EDGE('',*,*,#36929,.T.) ;
#48349 = ORIENTED_EDGE('',*,*,#36749,.F.) ;
#48350 = ORIENTED_EDGE('',*,*,#36935,.F.) ;
#48351 = ORIENTED_EDGE('',*,*,#36746,.F.) ;
#48352 = ORIENTED_EDGE('',*,*,#36771,.F.) ;
#48353 = ORIENTED_EDGE('',*,*,#36936,.T.) ;
#48354 = ORIENTED_EDGE('',*,*,#36743,.F.) ;
#48355 = ORIENTED_EDGE('',*,*,#36937,.F.) ;
#48356 = ORIENTED_EDGE('',*,*,#36934,.T.) ;
#48357 = ORIENTED_EDGE('',*,*,#36933,.T.) ;
#48358 = ORIENTED_EDGE('',*,*,#36938,.F.) ;
#48359 = ORIENTED_EDGE('',*,*,#36937,.T.) ;
#48360 = ORIENTED_EDGE('',*,*,#36935,.T.) ;
#48361 = ORIENTED_EDGE('',*,*,#36939,.F.) ;
#48362 = ORIENTED_EDGE('',*,*,#36938,.T.) ;
#48363 = ORIENTED_EDGE('',*,*,#36754,.F.) ;
#48364 = ORIENTED_EDGE('',*,*,#36940,.F.) ;
#48365 = ORIENTED_EDGE('',*,*,#36747,.F.) ;
#48366 = ORIENTED_EDGE('',*,*,#36939,.T.) ;
#48367 = ORIENTED_EDGE('',*,*,#36748,.F.) ;
#48368 = ORIENTED_EDGE('',*,*,#36941,.F.) ;
#48369 = ORIENTED_EDGE('',*,*,#36772,.F.) ;
#48370 = ORIENTED_EDGE('',*,*,#36941,.T.) ;
#48371 = ORIENTED_EDGE('',*,*,#36940,.T.) ;
#48372 = ORIENTED_EDGE('',*,*,#36942,.F.) ;
#48373 = ORIENTED_EDGE('',*,*,#36753,.F.) ;
#48374 = ORIENTED_EDGE('',*,*,#36943,.T.) ;
#48375 = ORIENTED_EDGE('',*,*,#36769,.F.) ;
#48376 = ORIENTED_EDGE('',*,*,#36942,.T.) ;
#48377 = ORIENTED_EDGE('',*,*,#36727,.F.) ;
#48378 = ORIENTED_EDGE('',*,*,#36944,.T.) ;
#48379 = ORIENTED_EDGE('',*,*,#36755,.F.) ;
#48380 = ORIENTED_EDGE('',*,*,#36945,.F.) ;
#48381 = ORIENTED_EDGE('',*,*,#36606,.F.) ;
#48382 = ORIENTED_EDGE('',*,*,#36946,.T.) ;
#48383 = ORIENTED_EDGE('',*,*,#36728,.F.) ;
#48384 = ORIENTED_EDGE('',*,*,#36945,.T.) ;
#48385 = ORIENTED_EDGE('',*,*,#36759,.F.) ;
#48386 = ORIENTED_EDGE('',*,*,#36718,.F.) ;
#48387 = ORIENTED_EDGE('',*,*,#36947,.T.) ;
#48388 = ORIENTED_EDGE('',*,*,#36719,.F.) ;
#48389 = ORIENTED_EDGE('',*,*,#36621,.F.) ;
#48390 = ORIENTED_EDGE('',*,*,#36724,.F.) ;
#48391 = ORIENTED_EDGE('',*,*,#36948,.T.) ;
#48392 = ORIENTED_EDGE('',*,*,#36716,.F.) ;
#48393 = ORIENTED_EDGE('',*,*,#36619,.F.) ;
#48394 = ORIENTED_EDGE('',*,*,#36703,.F.) ;
#48395 = ORIENTED_EDGE('',*,*,#36949,.T.) ;
#48396 = ORIENTED_EDGE('',*,*,#36761,.F.) ;
#48397 = ORIENTED_EDGE('',*,*,#36950,.F.) ;
#48398 = ORIENTED_EDGE('',*,*,#36763,.F.) ;
#48399 = ORIENTED_EDGE('',*,*,#36951,.T.) ;
#48400 = ORIENTED_EDGE('',*,*,#36709,.F.) ;
#48401 = ORIENTED_EDGE('',*,*,#36952,.F.) ;
#48402 = ORIENTED_EDGE('',*,*,#36953,.F.) ;
#48403 = ORIENTED_EDGE('',*,*,#36764,.F.) ;
#48404 = ORIENTED_EDGE('',*,*,#36954,.F.) ;
#48405 = ORIENTED_EDGE('',*,*,#36708,.F.) ;
#48406 = ORIENTED_EDGE('',*,*,#36950,.T.) ;
#48407 = ORIENTED_EDGE('',*,*,#36953,.T.) ;
#48408 = ORIENTED_EDGE('',*,*,#36955,.F.) ;
#48409 = ORIENTED_EDGE('',*,*,#36721,.F.) ;
#48410 = ORIENTED_EDGE('',*,*,#36956,.T.) ;
#48411 = ORIENTED_EDGE('',*,*,#36713,.F.) ;
#48412 = ORIENTED_EDGE('',*,*,#36623,.F.) ;
#48413 = ORIENTED_EDGE('',*,*,#36715,.F.) ;
#48414 = ORIENTED_EDGE('',*,*,#36957,.T.) ;
#48415 = ORIENTED_EDGE('',*,*,#36722,.F.) ;
#48416 = ORIENTED_EDGE('',*,*,#36617,.F.) ;
#48417 = ORIENTED_EDGE('',*,*,#36954,.T.) ;
#48418 = ORIENTED_EDGE('',*,*,#36952,.T.) ;
#48419 = ORIENTED_EDGE('',*,*,#36958,.F.) ;
#48420 = ORIENTED_EDGE('',*,*,#36955,.T.) ;
#48421 = ORIENTED_EDGE('',*,*,#36707,.F.) ;
#48422 = ORIENTED_EDGE('',*,*,#36959,.F.) ;
#48423 = ORIENTED_EDGE('',*,*,#36704,.F.) ;
#48424 = ORIENTED_EDGE('',*,*,#36767,.F.) ;
#48425 = ORIENTED_EDGE('',*,*,#36960,.T.) ;
#48426 = ORIENTED_EDGE('',*,*,#36701,.F.) ;
#48427 = ORIENTED_EDGE('',*,*,#36961,.F.) ;
#48428 = ORIENTED_EDGE('',*,*,#36711,.F.) ;
#48429 = ORIENTED_EDGE('',*,*,#36962,.T.) ;
#48430 = ORIENTED_EDGE('',*,*,#36765,.F.) ;
#48431 = ORIENTED_EDGE('',*,*,#36963,.F.) ;
#48432 = ORIENTED_EDGE('',*,*,#36958,.T.) ;
#48433 = ORIENTED_EDGE('',*,*,#36712,.F.) ;
#48434 = ORIENTED_EDGE('',*,*,#36964,.F.) ;
#48435 = ORIENTED_EDGE('',*,*,#36705,.F.) ;
#48436 = ORIENTED_EDGE('',*,*,#36961,.T.) ;
#48437 = ORIENTED_EDGE('',*,*,#36959,.T.) ;
#48438 = ORIENTED_EDGE('',*,*,#36965,.F.) ;
#48439 = ORIENTED_EDGE('',*,*,#36964,.T.) ;
#48440 = ORIENTED_EDGE('',*,*,#36963,.T.) ;
#48441 = ORIENTED_EDGE('',*,*,#36966,.F.) ;
#48442 = ORIENTED_EDGE('',*,*,#36965,.T.) ;
#48443 = ORIENTED_EDGE('',*,*,#36706,.F.) ;
#48444 = ORIENTED_EDGE('',*,*,#36966,.T.) ;
#48445 = ORIENTED_EDGE('',*,*,#36768,.F.) ;
#48446 = ORIENTED_EDGE('',*,*,#36450,.F.) ;
#48447 = ORIENTED_EDGE('',*,*,#36426,.F.) ;
#48448 = ORIENTED_EDGE('',*,*,#36967,.F.) ;
#48449 = ORIENTED_EDGE('',*,*,#36432,.F.) ;
#48450 = ORIENTED_EDGE('',*,*,#36688,.F.) ;
#48451 = ORIENTED_EDGE('',*,*,#36968,.T.) ;
#48452 = ORIENTED_EDGE('',*,*,#36427,.F.) ;
#48453 = ORIENTED_EDGE('',*,*,#36969,.F.) ;
#48454 = ORIENTED_EDGE('',*,*,#36969,.T.) ;
#48455 = ORIENTED_EDGE('',*,*,#36967,.T.) ;
#48456 = ORIENTED_EDGE('',*,*,#36970,.F.) ;
#48457 = ORIENTED_EDGE('',*,*,#36449,.F.) ;
#48458 = ORIENTED_EDGE('',*,*,#36422,.F.) ;
#48459 = ORIENTED_EDGE('',*,*,#36971,.F.) ;
#48460 = ORIENTED_EDGE('',*,*,#36424,.F.) ;
#48461 = ORIENTED_EDGE('',*,*,#36970,.T.) ;
#48462 = ORIENTED_EDGE('',*,*,#36425,.F.) ;
#48463 = ORIENTED_EDGE('',*,*,#36972,.F.) ;
#48464 = ORIENTED_EDGE('',*,*,#36689,.F.) ;
#48465 = ORIENTED_EDGE('',*,*,#36972,.T.) ;
#48466 = ORIENTED_EDGE('',*,*,#36971,.T.) ;
#48467 = ORIENTED_EDGE('',*,*,#36973,.F.) ;
#48468 = ORIENTED_EDGE('',*,*,#36421,.F.) ;
#48469 = ORIENTED_EDGE('',*,*,#36974,.T.) ;
#48470 = ORIENTED_EDGE('',*,*,#36686,.F.) ;
#48471 = ORIENTED_EDGE('',*,*,#36973,.T.) ;
#48472 = ORIENTED_EDGE('',*,*,#36525,.F.) ;
#48473 = ORIENTED_EDGE('',*,*,#36377,.T.) ;
#48474 = ORIENTED_EDGE('',*,*,#36975,.T.) ;
#48475 = ORIENTED_EDGE('',*,*,#36697,.F.) ;
#48476 = ORIENTED_EDGE('',*,*,#36976,.F.) ;
#48477 = ORIENTED_EDGE('',*,*,#36503,.F.) ;
#48478 = ORIENTED_EDGE('',*,*,#36526,.F.) ;
#48479 = ORIENTED_EDGE('',*,*,#36977,.F.) ;
#48480 = ORIENTED_EDGE('',*,*,#36523,.F.) ;
#48481 = ORIENTED_EDGE('',*,*,#36977,.T.) ;
#48482 = ORIENTED_EDGE('',*,*,#36976,.T.) ;
#48483 = ORIENTED_EDGE('',*,*,#36978,.F.) ;
#48484 = ORIENTED_EDGE('',*,*,#36978,.T.) ;
#48485 = ORIENTED_EDGE('',*,*,#36700,.F.) ;
#48486 = ORIENTED_EDGE('',*,*,#36979,.F.) ;
#48487 = ORIENTED_EDGE('',*,*,#36521,.F.) ;
#48488 = ORIENTED_EDGE('',*,*,#36505,.F.) ;
#48489 = ORIENTED_EDGE('',*,*,#36522,.F.) ;
#48490 = ORIENTED_EDGE('',*,*,#36980,.F.) ;
#48491 = ORIENTED_EDGE('',*,*,#36519,.F.) ;
#48492 = ORIENTED_EDGE('',*,*,#36980,.T.) ;
#48493 = ORIENTED_EDGE('',*,*,#36979,.T.) ;
#48494 = ORIENTED_EDGE('',*,*,#36981,.F.) ;
#48495 = ORIENTED_EDGE('',*,*,#36699,.F.) ;
#48496 = ORIENTED_EDGE('',*,*,#36381,.T.) ;
#48497 = ORIENTED_EDGE('',*,*,#36982,.T.) ;
#48498 = ORIENTED_EDGE('',*,*,#36520,.F.) ;
#48499 = ORIENTED_EDGE('',*,*,#36981,.T.) ;
#48500 = ORIENTED_EDGE('',*,*,#36600,.F.) ;
#48501 = ORIENTED_EDGE('',*,*,#36983,.T.) ;
#48502 = ORIENTED_EDGE('',*,*,#36411,.F.) ;
#48503 = ORIENTED_EDGE('',*,*,#36984,.T.) ;
#48504 = ORIENTED_EDGE('',*,*,#36470,.F.) ;
#48505 = ORIENTED_EDGE('',*,*,#36572,.F.) ;
#48506 = ORIENTED_EDGE('',*,*,#36482,.F.) ;
#48507 = ORIENTED_EDGE('',*,*,#36506,.F.) ;
#48508 = ORIENTED_EDGE('',*,*,#36472,.F.) ;
#48509 = ORIENTED_EDGE('',*,*,#36507,.F.) ;
#48510 = ORIENTED_EDGE('',*,*,#36480,.F.) ;
#48511 = ORIENTED_EDGE('',*,*,#36508,.F.) ;
#48512 = ORIENTED_EDGE('',*,*,#36474,.F.) ;
#48513 = ORIENTED_EDGE('',*,*,#36509,.F.) ;
#48514 = ORIENTED_EDGE('',*,*,#36478,.F.) ;
#48515 = ORIENTED_EDGE('',*,*,#36512,.F.) ;
#48516 = ORIENTED_EDGE('',*,*,#36467,.F.) ;
#48517 = ORIENTED_EDGE('',*,*,#36442,.F.) ;
#48518 = ORIENTED_EDGE('',*,*,#36485,.F.) ;
#48519 = ORIENTED_EDGE('',*,*,#36565,.F.) ;
#48520 = ORIENTED_EDGE('',*,*,#36785,.F.) ;
#48521 = ORIENTED_EDGE('',*,*,#36985,.T.) ;
#48522 = ORIENTED_EDGE('',*,*,#36444,.F.) ;
#48523 = ORIENTED_EDGE('',*,*,#36466,.F.) ;
#48524 = ORIENTED_EDGE('',*,*,#36780,.F.) ;
#48525 = ORIENTED_EDGE('',*,*,#36986,.T.) ;
#48526 = ORIENTED_EDGE('',*,*,#36445,.F.) ;
#48527 = ORIENTED_EDGE('',*,*,#36987,.T.) ;
#48528 = ORIENTED_EDGE('',*,*,#36446,.F.) ;
#48529 = ORIENTED_EDGE('',*,*,#36988,.T.) ;
#48530 = ORIENTED_EDGE('',*,*,#36777,.F.) ;
#48531 = ORIENTED_EDGE('',*,*,#36486,.F.) ;
#48532 = ORIENTED_EDGE('',*,*,#36825,.F.) ;
#48533 = ORIENTED_EDGE('',*,*,#36831,.F.) ;
#48534 = ORIENTED_EDGE('',*,*,#36830,.F.) ;
#48535 = ORIENTED_EDGE('',*,*,#36989,.F.) ;
#48536 = ORIENTED_EDGE('',*,*,#36826,.F.) ;
#48537 = ORIENTED_EDGE('',*,*,#36919,.F.) ;
#48538 = ORIENTED_EDGE('',*,*,#36412,.F.) ;
#48539 = ORIENTED_EDGE('',*,*,#36990,.F.) ;
#48540 = ORIENTED_EDGE('',*,*,#36594,.F.) ;
#48541 = ORIENTED_EDGE('',*,*,#36989,.T.) ;
#48542 = ORIENTED_EDGE('',*,*,#36603,.F.) ;
#48543 = ORIENTED_EDGE('',*,*,#36922,.F.) ;
#48544 = ORIENTED_EDGE('',*,*,#36735,.F.) ;
#48545 = ORIENTED_EDGE('',*,*,#36990,.T.) ;
#48546 = ORIENTED_EDGE('',*,*,#36983,.F.) ;
#48547 = ORIENTED_EDGE('',*,*,#36991,.F.) ;
#48548 = ORIENTED_EDGE('',*,*,#36991,.T.) ;
#48549 = ORIENTED_EDGE('',*,*,#36599,.F.) ;
#48550 = ORIENTED_EDGE('',*,*,#36992,.F.) ;
#48551 = ORIENTED_EDGE('',*,*,#36595,.F.) ;
#48552 = ORIENTED_EDGE('',*,*,#36834,.F.) ;
#48553 = ORIENTED_EDGE('',*,*,#36828,.F.) ;
#48554 = ORIENTED_EDGE('',*,*,#36827,.F.) ;
#48555 = ORIENTED_EDGE('',*,*,#36992,.T.) ;
#48556 = ORIENTED_EDGE('',*,*,#36835,.F.) ;
#48557 = ORIENTED_EDGE('',*,*,#36847,.F.) ;
#48558 = ORIENTED_EDGE('',*,*,#36837,.F.) ;
#48559 = ORIENTED_EDGE('',*,*,#36836,.F.) ;
#48560 = ORIENTED_EDGE('',*,*,#36993,.F.) ;
#48561 = ORIENTED_EDGE('',*,*,#36848,.F.) ;
#48562 = ORIENTED_EDGE('',*,*,#36993,.T.) ;
#48563 = ORIENTED_EDGE('',*,*,#36601,.F.) ;
#48564 = ORIENTED_EDGE('',*,*,#36994,.F.) ;
#48565 = ORIENTED_EDGE('',*,*,#36591,.F.) ;
#48566 = ORIENTED_EDGE('',*,*,#36994,.T.) ;
#48567 = ORIENTED_EDGE('',*,*,#36984,.F.) ;
#48568 = ORIENTED_EDGE('',*,*,#36995,.F.) ;
#48569 = ORIENTED_EDGE('',*,*,#36946,.F.) ;
#48570 = ORIENTED_EDGE('',*,*,#36605,.F.) ;
#48571 = ORIENTED_EDGE('',*,*,#36996,.F.) ;
#48572 = ORIENTED_EDGE('',*,*,#36592,.F.) ;
#48573 = ORIENTED_EDGE('',*,*,#36995,.T.) ;
#48574 = ORIENTED_EDGE('',*,*,#36416,.F.) ;
#48575 = ORIENTED_EDGE('',*,*,#36926,.F.) ;
#48576 = ORIENTED_EDGE('',*,*,#36729,.F.) ;
#48577 = ORIENTED_EDGE('',*,*,#36996,.T.) ;
#48578 = ORIENTED_EDGE('',*,*,#36833,.F.) ;
#48579 = ORIENTED_EDGE('',*,*,#36832,.F.) ;
#48580 = ORIENTED_EDGE('',*,*,#36845,.F.) ;
#48581 = ORIENTED_EDGE('',*,*,#36844,.F.) ;
#48582 = ORIENTED_EDGE('',*,*,#36420,.F.) ;
#48583 = ORIENTED_EDGE('',*,*,#36997,.T.) ;
#48584 = ORIENTED_EDGE('',*,*,#36690,.F.) ;
#48585 = ORIENTED_EDGE('',*,*,#36998,.F.) ;
#48586 = ORIENTED_EDGE('',*,*,#36974,.F.) ;
#48587 = ORIENTED_EDGE('',*,*,#36998,.T.) ;
#48588 = ORIENTED_EDGE('',*,*,#36696,.F.) ;
#48589 = ORIENTED_EDGE('',*,*,#36999,.F.) ;
#48590 = ORIENTED_EDGE('',*,*,#36687,.F.) ;
#48591 = ORIENTED_EDGE('',*,*,#36999,.T.) ;
#48592 = ORIENTED_EDGE('',*,*,#36695,.F.) ;
#48593 = ORIENTED_EDGE('',*,*,#37000,.F.) ;
#48594 = ORIENTED_EDGE('',*,*,#37001,.F.) ;
#48595 = ORIENTED_EDGE('',*,*,#37002,.F.) ;
#48596 = ORIENTED_EDGE('',*,*,#37003,.F.) ;
#48597 = ORIENTED_EDGE('',*,*,#36428,.F.) ;
#48598 = ORIENTED_EDGE('',*,*,#36968,.F.) ;
#48599 = ORIENTED_EDGE('',*,*,#36451,.F.) ;
#48600 = ORIENTED_EDGE('',*,*,#36430,.F.) ;
#48601 = ORIENTED_EDGE('',*,*,#37004,.F.) ;
#48602 = ORIENTED_EDGE('',*,*,#36528,.F.) ;
#48603 = ORIENTED_EDGE('',*,*,#36429,.F.) ;
#48604 = ORIENTED_EDGE('',*,*,#37003,.T.) ;
#48605 = ORIENTED_EDGE('',*,*,#37002,.T.) ;
#48606 = ORIENTED_EDGE('',*,*,#37001,.T.) ;
#48607 = ORIENTED_EDGE('',*,*,#37000,.T.) ;
#48608 = ORIENTED_EDGE('',*,*,#37005,.F.) ;
#48609 = ORIENTED_EDGE('',*,*,#36529,.F.) ;
#48610 = ORIENTED_EDGE('',*,*,#37004,.T.) ;
#48611 = ORIENTED_EDGE('',*,*,#36380,.F.) ;
#48612 = ORIENTED_EDGE('',*,*,#37006,.T.) ;
#48613 = ORIENTED_EDGE('',*,*,#36516,.F.) ;
#48614 = ORIENTED_EDGE('',*,*,#36982,.F.) ;
#48615 = ORIENTED_EDGE('',*,*,#37005,.T.) ;
#48616 = ORIENTED_EDGE('',*,*,#36694,.F.) ;
#48617 = ORIENTED_EDGE('',*,*,#37007,.F.) ;
#48618 = ORIENTED_EDGE('',*,*,#36530,.F.) ;
#48619 = ORIENTED_EDGE('',*,*,#36501,.F.) ;
#48620 = ORIENTED_EDGE('',*,*,#36532,.F.) ;
#48621 = ORIENTED_EDGE('',*,*,#37008,.F.) ;
#48622 = ORIENTED_EDGE('',*,*,#36527,.F.) ;
#48623 = ORIENTED_EDGE('',*,*,#36382,.T.) ;
#48624 = ORIENTED_EDGE('',*,*,#36698,.F.) ;
#48625 = ORIENTED_EDGE('',*,*,#37009,.F.) ;
#48626 = ORIENTED_EDGE('',*,*,#36692,.F.) ;
#48627 = ORIENTED_EDGE('',*,*,#36531,.F.) ;
#48628 = ORIENTED_EDGE('',*,*,#37007,.T.) ;
#48629 = ORIENTED_EDGE('',*,*,#37010,.F.) ;
#48630 = ORIENTED_EDGE('',*,*,#37011,.F.) ;
#48631 = ORIENTED_EDGE('',*,*,#37012,.F.) ;
#48632 = ORIENTED_EDGE('',*,*,#36375,.F.) ;
#48633 = ORIENTED_EDGE('',*,*,#36374,.F.) ;
#48634 = ORIENTED_EDGE('',*,*,#36524,.F.) ;
#48635 = ORIENTED_EDGE('',*,*,#37008,.T.) ;
#48636 = ORIENTED_EDGE('',*,*,#36376,.F.) ;
#48637 = ORIENTED_EDGE('',*,*,#37012,.T.) ;
#48638 = ORIENTED_EDGE('',*,*,#37011,.T.) ;
#48639 = ORIENTED_EDGE('',*,*,#37010,.T.) ;
#48640 = ORIENTED_EDGE('',*,*,#36693,.F.) ;
#48641 = ORIENTED_EDGE('',*,*,#37009,.T.) ;
#48642 = ORIENTED_EDGE('',*,*,#36975,.F.) ;
#48643 = ORIENTED_EDGE('',*,*,#37013,.F.) ;
#48644 = ORIENTED_EDGE('',*,*,#36438,.F.) ;
#48645 = ORIENTED_EDGE('',*,*,#36488,.F.) ;
#48646 = ORIENTED_EDGE('',*,*,#36779,.F.) ;
#48647 = ORIENTED_EDGE('',*,*,#36895,.F.) ;
#48648 = ORIENTED_EDGE('',*,*,#37013,.T.) ;
#48649 = ORIENTED_EDGE('',*,*,#37014,.F.) ;
#48650 = ORIENTED_EDGE('',*,*,#36400,.F.) ;
#48651 = ORIENTED_EDGE('',*,*,#37014,.T.) ;
#48652 = ORIENTED_EDGE('',*,*,#36778,.F.) ;
#48653 = ORIENTED_EDGE('',*,*,#37015,.F.) ;
#48654 = ORIENTED_EDGE('',*,*,#36782,.F.) ;
#48655 = ORIENTED_EDGE('',*,*,#36988,.F.) ;
#48656 = ORIENTED_EDGE('',*,*,#36986,.F.) ;
#48657 = ORIENTED_EDGE('',*,*,#37015,.T.) ;
#48658 = ORIENTED_EDGE('',*,*,#37016,.T.) ;
#48659 = ORIENTED_EDGE('',*,*,#36921,.F.) ;
#48660 = ORIENTED_EDGE('',*,*,#37017,.F.) ;
#48661 = ORIENTED_EDGE('',*,*,#36924,.F.) ;
#48662 = ORIENTED_EDGE('',*,*,#37016,.F.) ;
#48663 = ORIENTED_EDGE('',*,*,#36744,.F.) ;
#48664 = ORIENTED_EDGE('',*,*,#37018,.F.) ;
#48665 = ORIENTED_EDGE('',*,*,#36741,.F.) ;
#48666 = ORIENTED_EDGE('',*,*,#37017,.T.) ;
#48667 = ORIENTED_EDGE('',*,*,#36732,.F.) ;
#48668 = ORIENTED_EDGE('',*,*,#37019,.F.) ;
#48669 = ORIENTED_EDGE('',*,*,#36774,.F.) ;
#48670 = ORIENTED_EDGE('',*,*,#37018,.T.) ;
#48671 = ORIENTED_EDGE('',*,*,#36936,.F.) ;
#48672 = ORIENTED_EDGE('',*,*,#37020,.F.) ;
#48673 = ORIENTED_EDGE('',*,*,#36931,.F.) ;
#48674 = ORIENTED_EDGE('',*,*,#37019,.T.) ;
#48675 = ORIENTED_EDGE('',*,*,#36928,.F.) ;
#48676 = ORIENTED_EDGE('',*,*,#37021,.F.) ;
#48677 = ORIENTED_EDGE('',*,*,#36932,.F.) ;
#48678 = ORIENTED_EDGE('',*,*,#37020,.T.) ;
#48679 = ORIENTED_EDGE('',*,*,#36770,.F.) ;
#48680 = ORIENTED_EDGE('',*,*,#37022,.F.) ;
#48681 = ORIENTED_EDGE('',*,*,#36726,.F.) ;
#48682 = ORIENTED_EDGE('',*,*,#37021,.T.) ;
#48683 = ORIENTED_EDGE('',*,*,#36756,.F.) ;
#48684 = ORIENTED_EDGE('',*,*,#37023,.F.) ;
#48685 = ORIENTED_EDGE('',*,*,#36752,.F.) ;
#48686 = ORIENTED_EDGE('',*,*,#37022,.T.) ;
#48687 = ORIENTED_EDGE('',*,*,#36943,.F.) ;
#48688 = ORIENTED_EDGE('',*,*,#37023,.T.) ;
#48689 = ORIENTED_EDGE('',*,*,#36944,.F.) ;
#48690 = ORIENTED_EDGE('',*,*,#37024,.T.) ;
#48691 = ORIENTED_EDGE('',*,*,#36947,.F.) ;
#48692 = ORIENTED_EDGE('',*,*,#37025,.F.) ;
#48693 = ORIENTED_EDGE('',*,*,#36949,.F.) ;
#48694 = ORIENTED_EDGE('',*,*,#37024,.F.) ;
#48695 = ORIENTED_EDGE('',*,*,#36702,.F.) ;
#48696 = ORIENTED_EDGE('',*,*,#37026,.F.) ;
#48697 = ORIENTED_EDGE('',*,*,#36720,.F.) ;
#48698 = ORIENTED_EDGE('',*,*,#37025,.T.) ;
#48699 = ORIENTED_EDGE('',*,*,#36717,.F.) ;
#48700 = ORIENTED_EDGE('',*,*,#37027,.F.) ;
#48701 = ORIENTED_EDGE('',*,*,#36762,.F.) ;
#48702 = ORIENTED_EDGE('',*,*,#37026,.T.) ;
#48703 = ORIENTED_EDGE('',*,*,#36960,.F.) ;
#48704 = ORIENTED_EDGE('',*,*,#37028,.F.) ;
#48705 = ORIENTED_EDGE('',*,*,#36956,.F.) ;
#48706 = ORIENTED_EDGE('',*,*,#37027,.T.) ;
#48707 = ORIENTED_EDGE('',*,*,#36948,.F.) ;
#48708 = ORIENTED_EDGE('',*,*,#37029,.F.) ;
#48709 = ORIENTED_EDGE('',*,*,#36951,.F.) ;
#48710 = ORIENTED_EDGE('',*,*,#37028,.T.) ;
#48711 = ORIENTED_EDGE('',*,*,#36766,.F.) ;
#48712 = ORIENTED_EDGE('',*,*,#37030,.F.) ;
#48713 = ORIENTED_EDGE('',*,*,#36714,.F.) ;
#48714 = ORIENTED_EDGE('',*,*,#37029,.T.) ;
#48715 = ORIENTED_EDGE('',*,*,#36723,.F.) ;
#48716 = ORIENTED_EDGE('',*,*,#37031,.F.) ;
#48717 = ORIENTED_EDGE('',*,*,#36710,.F.) ;
#48718 = ORIENTED_EDGE('',*,*,#37030,.T.) ;
#48719 = ORIENTED_EDGE('',*,*,#36962,.F.) ;
#48720 = ORIENTED_EDGE('',*,*,#37031,.T.) ;
#48721 = ORIENTED_EDGE('',*,*,#36957,.F.) ;
#48722 = ORIENTED_EDGE('',*,*,#36464,.F.) ;
#48723 = ORIENTED_EDGE('',*,*,#36434,.F.) ;
#48724 = ORIENTED_EDGE('',*,*,#37032,.F.) ;
#48725 = ORIENTED_EDGE('',*,*,#36783,.F.) ;
#48726 = ORIENTED_EDGE('',*,*,#37032,.T.) ;
#48727 = ORIENTED_EDGE('',*,*,#36885,.F.) ;
#48728 = ORIENTED_EDGE('',*,*,#36402,.F.) ;
#48729 = ORIENTED_EDGE('',*,*,#37033,.F.) ;
#48730 = ORIENTED_EDGE('',*,*,#37033,.T.) ;
#48731 = ORIENTED_EDGE('',*,*,#36781,.F.) ;
#48732 = ORIENTED_EDGE('',*,*,#37034,.F.) ;
#48733 = ORIENTED_EDGE('',*,*,#36784,.F.) ;
#48734 = ORIENTED_EDGE('',*,*,#36987,.F.) ;
#48735 = ORIENTED_EDGE('',*,*,#36985,.F.) ;
#48736 = ORIENTED_EDGE('',*,*,#37034,.T.) ;
#48737 = ORIENTED_EDGE('',*,*,#36518,.F.) ;
#48738 = ORIENTED_EDGE('',*,*,#37035,.F.) ;
#48739 = ORIENTED_EDGE('',*,*,#36513,.F.) ;
#48740 = ORIENTED_EDGE('',*,*,#36476,.F.) ;
#48741 = ORIENTED_EDGE('',*,*,#36517,.F.) ;
#48742 = ORIENTED_EDGE('',*,*,#37006,.F.) ;
#48743 = ORIENTED_EDGE('',*,*,#36379,.F.) ;
#48744 = ORIENTED_EDGE('',*,*,#37036,.F.) ;
#48745 = ORIENTED_EDGE('',*,*,#36514,.F.) ;
#48746 = ORIENTED_EDGE('',*,*,#37035,.T.) ;
#48747 = ORIENTED_EDGE('',*,*,#37036,.T.) ;
#48748 = ORIENTED_EDGE('',*,*,#36691,.F.) ;
#48749 = ORIENTED_EDGE('',*,*,#37037,.F.) ;
#48750 = ORIENTED_EDGE('',*,*,#36515,.F.) ;
#48751 = ORIENTED_EDGE('',*,*,#36997,.F.) ;
#48752 = ORIENTED_EDGE('',*,*,#36419,.F.) ;
#48753 = ORIENTED_EDGE('',*,*,#37038,.F.) ;
#48754 = ORIENTED_EDGE('',*,*,#36510,.F.) ;
#48755 = ORIENTED_EDGE('',*,*,#37037,.T.) ;
#48756 = ORIENTED_EDGE('',*,*,#36448,.F.) ;
#48757 = ORIENTED_EDGE('',*,*,#36511,.F.) ;
#48758 = ORIENTED_EDGE('',*,*,#37038,.T.) ;
#48759 = ORIENTED_EDGE('',*,*,#36418,.F.) ;
#48760 = ORIENTED_EDGE('',*,*,#37039,.T.) ;
#48761 = ORIENTED_EDGE('',*,*,#37040,.T.) ;
#48762 = ORIENTED_EDGE('',*,*,#37041,.T.) ;
#48763 = ORIENTED_EDGE('',*,*,#37042,.F.) ;
#48764 = ORIENTED_EDGE('',*,*,#37043,.F.) ;
#48765 = ORIENTED_EDGE('',*,*,#37044,.T.) ;
#48766 = ORIENTED_EDGE('',*,*,#37045,.T.) ;
#48767 = ORIENTED_EDGE('',*,*,#37046,.F.) ;
#48768 = ORIENTED_EDGE('',*,*,#37047,.F.) ;
#48769 = ORIENTED_EDGE('',*,*,#37048,.F.) ;
#48770 = ORIENTED_EDGE('',*,*,#37049,.F.) ;
#48771 = ORIENTED_EDGE('',*,*,#37050,.T.) ;
#48772 = ORIENTED_EDGE('',*,*,#37051,.F.) ;
#48773 = ORIENTED_EDGE('',*,*,#37050,.F.) ;
#48774 = ORIENTED_EDGE('',*,*,#37052,.F.) ;
#48775 = ORIENTED_EDGE('',*,*,#37053,.T.) ;
#48776 = ORIENTED_EDGE('',*,*,#37054,.F.) ;
#48777 = ORIENTED_EDGE('',*,*,#37053,.F.) ;
#48778 = ORIENTED_EDGE('',*,*,#37055,.F.) ;
#48779 = ORIENTED_EDGE('',*,*,#37056,.F.) ;
#48780 = ORIENTED_EDGE('',*,*,#37057,.T.) ;
#48781 = ORIENTED_EDGE('',*,*,#37058,.T.) ;
#48782 = ORIENTED_EDGE('',*,*,#37059,.F.) ;
#48783 = ORIENTED_EDGE('',*,*,#37060,.F.) ;
#48784 = ORIENTED_EDGE('',*,*,#37061,.F.) ;
#48785 = ORIENTED_EDGE('',*,*,#37062,.T.) ;
#48786 = ORIENTED_EDGE('',*,*,#37063,.F.) ;
#48787 = ORIENTED_EDGE('',*,*,#37064,.F.) ;
#48788 = ORIENTED_EDGE('',*,*,#37065,.T.) ;
#48789 = ORIENTED_EDGE('',*,*,#37066,.F.) ;
#48790 = ORIENTED_EDGE('',*,*,#37067,.T.) ;
#48791 = ORIENTED_EDGE('',*,*,#37051,.T.) ;
#48792 = ORIENTED_EDGE('',*,*,#37068,.T.) ;
#48793 = ORIENTED_EDGE('',*,*,#37052,.T.) ;
#48794 = ORIENTED_EDGE('',*,*,#37068,.F.) ;
#48795 = ORIENTED_EDGE('',*,*,#37064,.T.) ;
#48796 = ORIENTED_EDGE('',*,*,#37069,.T.) ;
#48797 = ORIENTED_EDGE('',*,*,#37070,.T.) ;
#48798 = ORIENTED_EDGE('',*,*,#37061,.T.) ;
#48799 = ORIENTED_EDGE('',*,*,#37071,.F.) ;
#48800 = ORIENTED_EDGE('',*,*,#37072,.T.) ;
#48801 = ORIENTED_EDGE('',*,*,#37073,.F.) ;
#48802 = ORIENTED_EDGE('',*,*,#37059,.T.) ;
#48803 = ORIENTED_EDGE('',*,*,#37074,.T.) ;
#48804 = ORIENTED_EDGE('',*,*,#37075,.T.) ;
#48805 = ORIENTED_EDGE('',*,*,#37076,.T.) ;
#48806 = ORIENTED_EDGE('',*,*,#37077,.T.) ;
#48807 = ORIENTED_EDGE('',*,*,#37078,.T.) ;
#48808 = ORIENTED_EDGE('',*,*,#37079,.T.) ;
#48809 = ORIENTED_EDGE('',*,*,#37080,.T.) ;
#48810 = ORIENTED_EDGE('',*,*,#37081,.T.) ;
#48811 = ORIENTED_EDGE('',*,*,#37082,.T.) ;
#48812 = ORIENTED_EDGE('',*,*,#37083,.T.) ;
#48813 = ORIENTED_EDGE('',*,*,#37084,.T.) ;
#48814 = ORIENTED_EDGE('',*,*,#37085,.T.) ;
#48815 = ORIENTED_EDGE('',*,*,#37086,.T.) ;
#48816 = ORIENTED_EDGE('',*,*,#37087,.T.) ;
#48817 = ORIENTED_EDGE('',*,*,#37088,.T.) ;
#48818 = ORIENTED_EDGE('',*,*,#37089,.T.) ;
#48819 = ORIENTED_EDGE('',*,*,#37090,.T.) ;
#48820 = ORIENTED_EDGE('',*,*,#37091,.T.) ;
#48821 = ORIENTED_EDGE('',*,*,#37092,.T.) ;
#48822 = ORIENTED_EDGE('',*,*,#37093,.T.) ;
#48823 = ORIENTED_EDGE('',*,*,#37094,.T.) ;
#48824 = ORIENTED_EDGE('',*,*,#37095,.T.) ;
#48825 = ORIENTED_EDGE('',*,*,#37096,.T.) ;
#48826 = ORIENTED_EDGE('',*,*,#37097,.T.) ;
#48827 = ORIENTED_EDGE('',*,*,#37098,.T.) ;
#48828 = ORIENTED_EDGE('',*,*,#37099,.T.) ;
#48829 = ORIENTED_EDGE('',*,*,#37100,.T.) ;
#48830 = ORIENTED_EDGE('',*,*,#37101,.T.) ;
#48831 = ORIENTED_EDGE('',*,*,#37102,.F.) ;
#48832 = ORIENTED_EDGE('',*,*,#37103,.T.) ;
#48833 = ORIENTED_EDGE('',*,*,#37104,.T.) ;
#48834 = ORIENTED_EDGE('',*,*,#37105,.T.) ;
#48835 = ORIENTED_EDGE('',*,*,#37106,.F.) ;
#48836 = ORIENTED_EDGE('',*,*,#37107,.T.) ;
#48837 = ORIENTED_EDGE('',*,*,#37108,.T.) ;
#48838 = ORIENTED_EDGE('',*,*,#37109,.T.) ;
#48839 = ORIENTED_EDGE('',*,*,#37110,.T.) ;
#48840 = ORIENTED_EDGE('',*,*,#37111,.T.) ;
#48841 = ORIENTED_EDGE('',*,*,#37112,.F.) ;
#48842 = ORIENTED_EDGE('',*,*,#37113,.T.) ;
#48843 = ORIENTED_EDGE('',*,*,#37082,.F.) ;
#48844 = ORIENTED_EDGE('',*,*,#37114,.T.) ;
#48845 = ORIENTED_EDGE('',*,*,#37088,.F.) ;
#48846 = ORIENTED_EDGE('',*,*,#37115,.T.) ;
#48847 = ORIENTED_EDGE('',*,*,#37096,.F.) ;
#48848 = ORIENTED_EDGE('',*,*,#37116,.T.) ;
#48849 = ORIENTED_EDGE('',*,*,#37117,.F.) ;
#48850 = ORIENTED_EDGE('',*,*,#37118,.T.) ;
#48851 = ORIENTED_EDGE('',*,*,#37119,.F.) ;
#48852 = ORIENTED_EDGE('',*,*,#37120,.T.) ;
#48853 = ORIENTED_EDGE('',*,*,#37121,.T.) ;
#48854 = ORIENTED_EDGE('',*,*,#37122,.T.) ;
#48855 = ORIENTED_EDGE('',*,*,#37123,.F.) ;
#48856 = ORIENTED_EDGE('',*,*,#37124,.T.) ;
#48857 = ORIENTED_EDGE('',*,*,#37125,.T.) ;
#48858 = ORIENTED_EDGE('',*,*,#37126,.T.) ;
#48859 = ORIENTED_EDGE('',*,*,#37127,.F.) ;
#48860 = ORIENTED_EDGE('',*,*,#37128,.T.) ;
#48861 = ORIENTED_EDGE('',*,*,#37100,.F.) ;
#48862 = ORIENTED_EDGE('',*,*,#37129,.T.) ;
#48863 = ORIENTED_EDGE('',*,*,#37130,.T.) ;
#48864 = ORIENTED_EDGE('',*,*,#37131,.T.) ;
#48865 = ORIENTED_EDGE('',*,*,#37108,.F.) ;
#48866 = ORIENTED_EDGE('',*,*,#37132,.T.) ;
#48867 = ORIENTED_EDGE('',*,*,#37133,.F.) ;
#48868 = ORIENTED_EDGE('',*,*,#37134,.F.) ;
#48869 = ORIENTED_EDGE('',*,*,#37135,.T.) ;
#48870 = ORIENTED_EDGE('',*,*,#37136,.F.) ;
#48871 = ORIENTED_EDGE('',*,*,#37137,.T.) ;
#48872 = ORIENTED_EDGE('',*,*,#37138,.F.) ;
#48873 = ORIENTED_EDGE('',*,*,#37139,.T.) ;
#48874 = ORIENTED_EDGE('',*,*,#37140,.T.) ;
#48875 = ORIENTED_EDGE('',*,*,#37141,.T.) ;
#48876 = ORIENTED_EDGE('',*,*,#37142,.T.) ;
#48877 = ORIENTED_EDGE('',*,*,#37143,.T.) ;
#48878 = ORIENTED_EDGE('',*,*,#37144,.T.) ;
#48879 = ORIENTED_EDGE('',*,*,#37145,.T.) ;
#48880 = ORIENTED_EDGE('',*,*,#37146,.T.) ;
#48881 = ORIENTED_EDGE('',*,*,#37147,.T.) ;
#48882 = ORIENTED_EDGE('',*,*,#37148,.T.) ;
#48883 = ORIENTED_EDGE('',*,*,#37149,.T.) ;
#48884 = ORIENTED_EDGE('',*,*,#37150,.T.) ;
#48885 = ORIENTED_EDGE('',*,*,#37106,.T.) ;
#48886 = ORIENTED_EDGE('',*,*,#37151,.T.) ;
#48887 = ORIENTED_EDGE('',*,*,#37152,.T.) ;
#48888 = ORIENTED_EDGE('',*,*,#37153,.T.) ;
#48889 = ORIENTED_EDGE('',*,*,#37102,.T.) ;
#48890 = ORIENTED_EDGE('',*,*,#37154,.T.) ;
#48891 = ORIENTED_EDGE('',*,*,#37155,.F.) ;
#48892 = ORIENTED_EDGE('',*,*,#37156,.T.) ;
#48893 = ORIENTED_EDGE('',*,*,#37157,.F.) ;
#48894 = ORIENTED_EDGE('',*,*,#37158,.T.) ;
#48895 = ORIENTED_EDGE('',*,*,#37159,.T.) ;
#48896 = ORIENTED_EDGE('',*,*,#37160,.T.) ;
#48897 = ORIENTED_EDGE('',*,*,#37161,.F.) ;
#48898 = ORIENTED_EDGE('',*,*,#37162,.T.) ;
#48899 = ORIENTED_EDGE('',*,*,#37163,.F.) ;
#48900 = ORIENTED_EDGE('',*,*,#37164,.T.) ;
#48901 = ORIENTED_EDGE('',*,*,#37165,.T.) ;
#48902 = ORIENTED_EDGE('',*,*,#37166,.T.) ;
#48903 = ORIENTED_EDGE('',*,*,#37167,.T.) ;
#48904 = ORIENTED_EDGE('',*,*,#37168,.T.) ;
#48905 = ORIENTED_EDGE('',*,*,#37169,.T.) ;
#48906 = ORIENTED_EDGE('',*,*,#37170,.T.) ;
#48907 = ORIENTED_EDGE('',*,*,#37136,.T.) ;
#48908 = ORIENTED_EDGE('',*,*,#37171,.T.) ;
#48909 = ORIENTED_EDGE('',*,*,#37146,.F.) ;
#48910 = ORIENTED_EDGE('',*,*,#37172,.T.) ;
#48911 = ORIENTED_EDGE('',*,*,#37138,.T.) ;
#48912 = ORIENTED_EDGE('',*,*,#37173,.T.) ;
#48913 = ORIENTED_EDGE('',*,*,#37144,.F.) ;
#48914 = ORIENTED_EDGE('',*,*,#37174,.T.) ;
#48915 = ORIENTED_EDGE('',*,*,#37175,.T.) ;
#48916 = ORIENTED_EDGE('',*,*,#37176,.T.) ;
#48917 = ORIENTED_EDGE('',*,*,#37112,.T.) ;
#48918 = ORIENTED_EDGE('',*,*,#37177,.T.) ;
#48919 = ORIENTED_EDGE('',*,*,#37142,.F.) ;
#48920 = ORIENTED_EDGE('',*,*,#37178,.T.) ;
#48921 = ORIENTED_EDGE('',*,*,#37179,.T.) ;
#48922 = ORIENTED_EDGE('',*,*,#37180,.T.) ;
#48923 = ORIENTED_EDGE('',*,*,#37181,.T.) ;
#48924 = ORIENTED_EDGE('',*,*,#37182,.T.) ;
#48925 = ORIENTED_EDGE('',*,*,#37183,.T.) ;
#48926 = ORIENTED_EDGE('',*,*,#37140,.F.) ;
#48927 = ORIENTED_EDGE('',*,*,#37184,.T.) ;
#48928 = ORIENTED_EDGE('',*,*,#37185,.T.) ;
#48929 = ORIENTED_EDGE('',*,*,#37186,.T.) ;
#48930 = ORIENTED_EDGE('',*,*,#37187,.T.) ;
#48931 = ORIENTED_EDGE('',*,*,#37169,.F.) ;
#48932 = ORIENTED_EDGE('',*,*,#37188,.T.) ;
#48933 = ORIENTED_EDGE('',*,*,#37189,.T.) ;
#48934 = ORIENTED_EDGE('',*,*,#37043,.T.) ;
#48935 = ORIENTED_EDGE('',*,*,#37190,.T.) ;
#48936 = ORIENTED_EDGE('',*,*,#37191,.T.) ;
#48937 = ORIENTED_EDGE('',*,*,#37167,.F.) ;
#48938 = ORIENTED_EDGE('',*,*,#37192,.T.) ;
#48939 = ORIENTED_EDGE('',*,*,#37193,.T.) ;
#48940 = ORIENTED_EDGE('',*,*,#37194,.T.) ;
#48941 = ORIENTED_EDGE('',*,*,#37195,.T.) ;
#48942 = ORIENTED_EDGE('',*,*,#37196,.T.) ;
#48943 = ORIENTED_EDGE('',*,*,#37197,.T.) ;
#48944 = ORIENTED_EDGE('',*,*,#37165,.F.) ;
#48945 = ORIENTED_EDGE('',*,*,#37198,.T.) ;
#48946 = ORIENTED_EDGE('',*,*,#37199,.T.) ;
#48947 = ORIENTED_EDGE('',*,*,#37200,.F.) ;
#48948 = ORIENTED_EDGE('',*,*,#37201,.T.) ;
#48949 = ORIENTED_EDGE('',*,*,#37202,.F.) ;
#48950 = ORIENTED_EDGE('',*,*,#37203,.T.) ;
#48951 = ORIENTED_EDGE('',*,*,#37204,.T.) ;
#48952 = ORIENTED_EDGE('',*,*,#37117,.T.) ;
#48953 = ORIENTED_EDGE('',*,*,#37205,.F.) ;
#48954 = ORIENTED_EDGE('',*,*,#37206,.T.) ;
#48955 = ORIENTED_EDGE('',*,*,#37123,.T.) ;
#48956 = ORIENTED_EDGE('',*,*,#37207,.T.) ;
#48957 = ORIENTED_EDGE('',*,*,#37208,.F.) ;
#48958 = ORIENTED_EDGE('',*,*,#37209,.T.) ;
#48959 = ORIENTED_EDGE('',*,*,#37210,.F.) ;
#48960 = ORIENTED_EDGE('',*,*,#37211,.T.) ;
#48961 = ORIENTED_EDGE('',*,*,#37212,.T.) ;
#48962 = ORIENTED_EDGE('',*,*,#37213,.T.) ;
#48963 = ORIENTED_EDGE('',*,*,#37214,.F.) ;
#48964 = ORIENTED_EDGE('',*,*,#37215,.T.) ;
#48965 = ORIENTED_EDGE('',*,*,#37216,.F.) ;
#48966 = ORIENTED_EDGE('',*,*,#37217,.T.) ;
#48967 = ORIENTED_EDGE('',*,*,#37159,.F.) ;
#48968 = ORIENTED_EDGE('',*,*,#37218,.T.) ;
#48969 = ORIENTED_EDGE('',*,*,#37219,.F.) ;
#48970 = ORIENTED_EDGE('',*,*,#37220,.T.) ;
#48971 = ORIENTED_EDGE('',*,*,#37221,.F.) ;
#48972 = ORIENTED_EDGE('',*,*,#37222,.T.) ;
#48973 = ORIENTED_EDGE('',*,*,#37223,.T.) ;
#48974 = ORIENTED_EDGE('',*,*,#37224,.T.) ;
#48975 = ORIENTED_EDGE('',*,*,#37225,.F.) ;
#48976 = ORIENTED_EDGE('',*,*,#37226,.T.) ;
#48977 = ORIENTED_EDGE('',*,*,#37054,.T.) ;
#48978 = ORIENTED_EDGE('',*,*,#37227,.F.) ;
#48979 = ORIENTED_EDGE('',*,*,#37228,.T.) ;
#48980 = ORIENTED_EDGE('',*,*,#37229,.F.) ;
#48981 = ORIENTED_EDGE('',*,*,#37133,.T.) ;
#48982 = ORIENTED_EDGE('',*,*,#37230,.T.) ;
#48983 = ORIENTED_EDGE('',*,*,#37149,.F.) ;
#48984 = ORIENTED_EDGE('',*,*,#37231,.F.) ;
#48985 = ORIENTED_EDGE('',*,*,#37232,.T.) ;
#48986 = ORIENTED_EDGE('',*,*,#37233,.F.) ;
#48987 = ORIENTED_EDGE('',*,*,#37234,.T.) ;
#48988 = ORIENTED_EDGE('',*,*,#37235,.F.) ;
#48989 = ORIENTED_EDGE('',*,*,#37236,.T.) ;
#48990 = ORIENTED_EDGE('',*,*,#37231,.T.) ;
#48991 = ORIENTED_EDGE('',*,*,#37148,.F.) ;
#48992 = ORIENTED_EDGE('',*,*,#37237,.T.) ;
#48993 = ORIENTED_EDGE('',*,*,#37134,.T.) ;
#48994 = ORIENTED_EDGE('',*,*,#37229,.T.) ;
#48995 = ORIENTED_EDGE('',*,*,#37238,.T.) ;
#48996 = ORIENTED_EDGE('',*,*,#37239,.F.) ;
#48997 = ORIENTED_EDGE('',*,*,#37240,.T.) ;
#48998 = ORIENTED_EDGE('',*,*,#37241,.T.) ;
#48999 = ORIENTED_EDGE('',*,*,#37242,.T.) ;
#49000 = ORIENTED_EDGE('',*,*,#37243,.F.) ;
#49001 = ORIENTED_EDGE('',*,*,#37244,.F.) ;
#49002 = ORIENTED_EDGE('',*,*,#37245,.T.) ;
#49003 = ORIENTED_EDGE('',*,*,#37246,.T.) ;
#49004 = ORIENTED_EDGE('',*,*,#37247,.T.) ;
#49005 = ORIENTED_EDGE('',*,*,#37248,.T.) ;
#49006 = ORIENTED_EDGE('',*,*,#37249,.T.) ;
#49007 = ORIENTED_EDGE('',*,*,#37250,.T.) ;
#49008 = ORIENTED_EDGE('',*,*,#37251,.T.) ;
#49009 = ORIENTED_EDGE('',*,*,#37252,.T.) ;
#49010 = ORIENTED_EDGE('',*,*,#37253,.T.) ;
#49011 = ORIENTED_EDGE('',*,*,#37254,.T.) ;
#49012 = ORIENTED_EDGE('',*,*,#37255,.T.) ;
#49013 = ORIENTED_EDGE('',*,*,#37256,.T.) ;
#49014 = ORIENTED_EDGE('',*,*,#37257,.T.) ;
#49015 = ORIENTED_EDGE('',*,*,#37258,.T.) ;
#49016 = ORIENTED_EDGE('',*,*,#37259,.T.) ;
#49017 = ORIENTED_EDGE('',*,*,#37260,.T.) ;
#49018 = ORIENTED_EDGE('',*,*,#37261,.T.) ;
#49019 = ORIENTED_EDGE('',*,*,#37262,.T.) ;
#49020 = ORIENTED_EDGE('',*,*,#37263,.T.) ;
#49021 = ORIENTED_EDGE('',*,*,#37264,.T.) ;
#49022 = ORIENTED_EDGE('',*,*,#37265,.T.) ;
#49023 = ORIENTED_EDGE('',*,*,#37266,.T.) ;
#49024 = ORIENTED_EDGE('',*,*,#37267,.T.) ;
#49025 = ORIENTED_EDGE('',*,*,#37268,.T.) ;
#49026 = ORIENTED_EDGE('',*,*,#37269,.T.) ;
#49027 = ORIENTED_EDGE('',*,*,#37270,.T.) ;
#49028 = ORIENTED_EDGE('',*,*,#37271,.T.) ;
#49029 = ORIENTED_EDGE('',*,*,#37272,.T.) ;
#49030 = ORIENTED_EDGE('',*,*,#37273,.T.) ;
#49031 = ORIENTED_EDGE('',*,*,#37274,.T.) ;
#49032 = ORIENTED_EDGE('',*,*,#37275,.T.) ;
#49033 = ORIENTED_EDGE('',*,*,#37276,.T.) ;
#49034 = ORIENTED_EDGE('',*,*,#37277,.T.) ;
#49035 = ORIENTED_EDGE('',*,*,#37278,.T.) ;
#49036 = ORIENTED_EDGE('',*,*,#37279,.T.) ;
#49037 = ORIENTED_EDGE('',*,*,#37280,.T.) ;
#49038 = ORIENTED_EDGE('',*,*,#37049,.T.) ;
#49039 = ORIENTED_EDGE('',*,*,#37281,.F.) ;
#49040 = ORIENTED_EDGE('',*,*,#37282,.T.) ;
#49041 = ORIENTED_EDGE('',*,*,#37283,.T.) ;
#49042 = ORIENTED_EDGE('',*,*,#37284,.T.) ;
#49043 = ORIENTED_EDGE('',*,*,#37285,.T.) ;
#49044 = ORIENTED_EDGE('',*,*,#37286,.T.) ;
#49045 = ORIENTED_EDGE('',*,*,#37287,.T.) ;
#49046 = ORIENTED_EDGE('',*,*,#37288,.T.) ;
#49047 = ORIENTED_EDGE('',*,*,#37289,.F.) ;
#49048 = ORIENTED_EDGE('',*,*,#37290,.T.) ;
#49049 = ORIENTED_EDGE('',*,*,#37127,.T.) ;
#49050 = ORIENTED_EDGE('',*,*,#37291,.T.) ;
#49051 = ORIENTED_EDGE('',*,*,#37292,.T.) ;
#49052 = ORIENTED_EDGE('',*,*,#37293,.T.) ;
#49053 = ORIENTED_EDGE('',*,*,#37294,.T.) ;
#49054 = ORIENTED_EDGE('',*,*,#37125,.F.) ;
#49055 = ORIENTED_EDGE('',*,*,#37295,.T.) ;
#49056 = ORIENTED_EDGE('',*,*,#37296,.T.) ;
#49057 = ORIENTED_EDGE('',*,*,#37297,.T.) ;
#49058 = ORIENTED_EDGE('',*,*,#37298,.T.) ;
#49059 = ORIENTED_EDGE('',*,*,#37299,.T.) ;
#49060 = ORIENTED_EDGE('',*,*,#37063,.T.) ;
#49061 = ORIENTED_EDGE('',*,*,#37300,.T.) ;
#49062 = ORIENTED_EDGE('',*,*,#37301,.T.) ;
#49063 = ORIENTED_EDGE('',*,*,#37302,.T.) ;
#49064 = ORIENTED_EDGE('',*,*,#37303,.T.) ;
#49065 = ORIENTED_EDGE('',*,*,#37304,.T.) ;
#49066 = ORIENTED_EDGE('',*,*,#37305,.T.) ;
#49067 = ORIENTED_EDGE('',*,*,#37306,.T.) ;
#49068 = ORIENTED_EDGE('',*,*,#37307,.T.) ;
#49069 = ORIENTED_EDGE('',*,*,#37308,.T.) ;
#49070 = ORIENTED_EDGE('',*,*,#37056,.T.) ;
#49071 = ORIENTED_EDGE('',*,*,#37309,.T.) ;
#49072 = ORIENTED_EDGE('',*,*,#37310,.T.) ;
#49073 = ORIENTED_EDGE('',*,*,#37311,.T.) ;
#49074 = ORIENTED_EDGE('',*,*,#37312,.T.) ;
#49075 = ORIENTED_EDGE('',*,*,#37313,.T.) ;
#49076 = ORIENTED_EDGE('',*,*,#37157,.T.) ;
#49077 = ORIENTED_EDGE('',*,*,#37314,.T.) ;
#49078 = ORIENTED_EDGE('',*,*,#37315,.T.) ;
#49079 = ORIENTED_EDGE('',*,*,#37316,.T.) ;
#49080 = ORIENTED_EDGE('',*,*,#37155,.T.) ;
#49081 = ORIENTED_EDGE('',*,*,#37317,.T.) ;
#49082 = ORIENTED_EDGE('',*,*,#37318,.F.) ;
#49083 = ORIENTED_EDGE('',*,*,#37319,.T.) ;
#49084 = ORIENTED_EDGE('',*,*,#37320,.T.) ;
#49085 = ORIENTED_EDGE('',*,*,#37321,.T.) ;
#49086 = ORIENTED_EDGE('',*,*,#37322,.T.) ;
#49087 = ORIENTED_EDGE('',*,*,#37119,.T.) ;
#49088 = ORIENTED_EDGE('',*,*,#37323,.T.) ;
#49089 = ORIENTED_EDGE('',*,*,#37324,.T.) ;
#49090 = ORIENTED_EDGE('',*,*,#37325,.T.) ;
#49091 = ORIENTED_EDGE('',*,*,#37326,.T.) ;
#49092 = ORIENTED_EDGE('',*,*,#37121,.F.) ;
#49093 = ORIENTED_EDGE('',*,*,#37327,.T.) ;
#49094 = ORIENTED_EDGE('',*,*,#37328,.T.) ;
#49095 = ORIENTED_EDGE('',*,*,#37329,.T.) ;
#49096 = ORIENTED_EDGE('',*,*,#37330,.T.) ;
#49097 = ORIENTED_EDGE('',*,*,#37331,.T.) ;
#49098 = ORIENTED_EDGE('',*,*,#37332,.T.) ;
#49099 = ORIENTED_EDGE('',*,*,#37333,.T.) ;
#49100 = ORIENTED_EDGE('',*,*,#37334,.T.) ;
#49101 = ORIENTED_EDGE('',*,*,#37335,.T.) ;
#49102 = ORIENTED_EDGE('',*,*,#37336,.T.) ;
#49103 = ORIENTED_EDGE('',*,*,#37337,.T.) ;
#49104 = ORIENTED_EDGE('',*,*,#37338,.T.) ;
#49105 = ORIENTED_EDGE('',*,*,#37339,.T.) ;
#49106 = ORIENTED_EDGE('',*,*,#37161,.T.) ;
#49107 = ORIENTED_EDGE('',*,*,#37340,.T.) ;
#49108 = ORIENTED_EDGE('',*,*,#37341,.T.) ;
#49109 = ORIENTED_EDGE('',*,*,#37342,.T.) ;
#49110 = ORIENTED_EDGE('',*,*,#37343,.T.) ;
#49111 = ORIENTED_EDGE('',*,*,#37344,.T.) ;
#49112 = ORIENTED_EDGE('',*,*,#37345,.T.) ;
#49113 = ORIENTED_EDGE('',*,*,#37346,.T.) ;
#49114 = ORIENTED_EDGE('',*,*,#37347,.T.) ;
#49115 = ORIENTED_EDGE('',*,*,#37348,.T.) ;
#49116 = ORIENTED_EDGE('',*,*,#37163,.T.) ;
#49117 = ORIENTED_EDGE('',*,*,#37349,.T.) ;
#49118 = ORIENTED_EDGE('',*,*,#37350,.T.) ;
#49119 = ORIENTED_EDGE('',*,*,#37351,.T.) ;
#49120 = ORIENTED_EDGE('',*,*,#37352,.T.) ;
#49121 = ORIENTED_EDGE('',*,*,#37353,.T.) ;
#49122 = ORIENTED_EDGE('',*,*,#37354,.T.) ;
#49123 = ORIENTED_EDGE('',*,*,#37355,.T.) ;
#49124 = ORIENTED_EDGE('',*,*,#37356,.T.) ;
#49125 = ORIENTED_EDGE('',*,*,#37048,.T.) ;
#49126 = ORIENTED_EDGE('',*,*,#37357,.T.) ;
#49127 = ORIENTED_EDGE('',*,*,#37358,.T.) ;
#49128 = ORIENTED_EDGE('',*,*,#37359,.T.) ;
#49129 = ORIENTED_EDGE('',*,*,#37360,.T.) ;
#49130 = ORIENTED_EDGE('',*,*,#37361,.T.) ;
#49131 = ORIENTED_EDGE('',*,*,#37362,.T.) ;
#49132 = ORIENTED_EDGE('',*,*,#37363,.T.) ;
#49133 = ORIENTED_EDGE('',*,*,#37364,.T.) ;
#49134 = ORIENTED_EDGE('',*,*,#37365,.T.) ;
#49135 = ORIENTED_EDGE('',*,*,#37366,.T.) ;
#49136 = ORIENTED_EDGE('',*,*,#37367,.T.) ;
#49137 = ORIENTED_EDGE('',*,*,#37368,.T.) ;
#49138 = ORIENTED_EDGE('',*,*,#37369,.T.) ;
#49139 = ORIENTED_EDGE('',*,*,#37370,.T.) ;
#49140 = ORIENTED_EDGE('',*,*,#37371,.T.) ;
#49141 = ORIENTED_EDGE('',*,*,#37372,.T.) ;
#49142 = ORIENTED_EDGE('',*,*,#37373,.T.) ;
#49143 = ORIENTED_EDGE('',*,*,#37374,.T.) ;
#49144 = ORIENTED_EDGE('',*,*,#37375,.T.) ;
#49145 = ORIENTED_EDGE('',*,*,#37376,.T.) ;
#49146 = ORIENTED_EDGE('',*,*,#37377,.T.) ;
#49147 = ORIENTED_EDGE('',*,*,#37378,.T.) ;
#49148 = ORIENTED_EDGE('',*,*,#37379,.T.) ;
#49149 = ORIENTED_EDGE('',*,*,#37380,.T.) ;
#49150 = ORIENTED_EDGE('',*,*,#37281,.T.) ;
#49151 = ORIENTED_EDGE('',*,*,#37381,.T.) ;
#49152 = ORIENTED_EDGE('',*,*,#37382,.T.) ;
#49153 = ORIENTED_EDGE('',*,*,#37383,.T.) ;
#49154 = ORIENTED_EDGE('',*,*,#37285,.F.) ;
#49155 = ORIENTED_EDGE('',*,*,#37384,.T.) ;
#49156 = ORIENTED_EDGE('',*,*,#37385,.T.) ;
#49157 = ORIENTED_EDGE('',*,*,#37386,.T.) ;
#49158 = ORIENTED_EDGE('',*,*,#37287,.F.) ;
#49159 = ORIENTED_EDGE('',*,*,#37387,.T.) ;
#49160 = ORIENTED_EDGE('',*,*,#37388,.T.) ;
#49161 = ORIENTED_EDGE('',*,*,#37389,.T.) ;
#49162 = ORIENTED_EDGE('',*,*,#37283,.F.) ;
#49163 = ORIENTED_EDGE('',*,*,#37390,.T.) ;
#49164 = ORIENTED_EDGE('',*,*,#37391,.T.) ;
#49165 = ORIENTED_EDGE('',*,*,#37392,.T.) ;
#49166 = ORIENTED_EDGE('',*,*,#37393,.T.) ;
#49167 = ORIENTED_EDGE('',*,*,#37394,.T.) ;
#49168 = ORIENTED_EDGE('',*,*,#37395,.T.) ;
#49169 = ORIENTED_EDGE('',*,*,#37396,.T.) ;
#49170 = ORIENTED_EDGE('',*,*,#37397,.T.) ;
#49171 = ORIENTED_EDGE('',*,*,#37398,.T.) ;
#49172 = ORIENTED_EDGE('',*,*,#37399,.T.) ;
#49173 = ORIENTED_EDGE('',*,*,#37400,.T.) ;
#49174 = ORIENTED_EDGE('',*,*,#37401,.T.) ;
#49175 = ORIENTED_EDGE('',*,*,#37402,.F.) ;
#49176 = ORIENTED_EDGE('',*,*,#37403,.T.) ;
#49177 = ORIENTED_EDGE('',*,*,#37079,.F.) ;
#49178 = ORIENTED_EDGE('',*,*,#37404,.T.) ;
#49179 = ORIENTED_EDGE('',*,*,#37405,.T.) ;
#49180 = ORIENTED_EDGE('',*,*,#37406,.T.) ;
#49181 = ORIENTED_EDGE('',*,*,#37407,.T.) ;
#49182 = ORIENTED_EDGE('',*,*,#37402,.T.) ;
#49183 = ORIENTED_EDGE('',*,*,#37408,.T.) ;
#49184 = ORIENTED_EDGE('',*,*,#37409,.T.) ;
#49185 = ORIENTED_EDGE('',*,*,#37410,.T.) ;
#49186 = ORIENTED_EDGE('',*,*,#37411,.T.) ;
#49187 = ORIENTED_EDGE('',*,*,#37412,.T.) ;
#49188 = ORIENTED_EDGE('',*,*,#37413,.T.) ;
#49189 = ORIENTED_EDGE('',*,*,#37414,.T.) ;
#49190 = ORIENTED_EDGE('',*,*,#37415,.T.) ;
#49191 = ORIENTED_EDGE('',*,*,#37416,.T.) ;
#49192 = ORIENTED_EDGE('',*,*,#37417,.T.) ;
#49193 = ORIENTED_EDGE('',*,*,#37418,.T.) ;
#49194 = ORIENTED_EDGE('',*,*,#37419,.T.) ;
#49195 = ORIENTED_EDGE('',*,*,#37420,.T.) ;
#49196 = ORIENTED_EDGE('',*,*,#37421,.T.) ;
#49197 = ORIENTED_EDGE('',*,*,#37422,.T.) ;
#49198 = ORIENTED_EDGE('',*,*,#37423,.F.) ;
#49199 = ORIENTED_EDGE('',*,*,#37272,.F.) ;
#49200 = ORIENTED_EDGE('',*,*,#37424,.T.) ;
#49201 = ORIENTED_EDGE('',*,*,#37423,.T.) ;
#49202 = ORIENTED_EDGE('',*,*,#37425,.T.) ;
#49203 = ORIENTED_EDGE('',*,*,#37426,.T.) ;
#49204 = ORIENTED_EDGE('',*,*,#37427,.T.) ;
#49205 = ORIENTED_EDGE('',*,*,#37428,.T.) ;
#49206 = ORIENTED_EDGE('',*,*,#37429,.T.) ;
#49207 = ORIENTED_EDGE('',*,*,#37430,.T.) ;
#49208 = ORIENTED_EDGE('',*,*,#37431,.T.) ;
#49209 = ORIENTED_EDGE('',*,*,#37432,.T.) ;
#49210 = ORIENTED_EDGE('',*,*,#37433,.T.) ;
#49211 = ORIENTED_EDGE('',*,*,#37434,.T.) ;
#49212 = ORIENTED_EDGE('',*,*,#37435,.T.) ;
#49213 = ORIENTED_EDGE('',*,*,#37436,.T.) ;
#49214 = ORIENTED_EDGE('',*,*,#37437,.T.) ;
#49215 = ORIENTED_EDGE('',*,*,#37438,.T.) ;
#49216 = ORIENTED_EDGE('',*,*,#37439,.T.) ;
#49217 = ORIENTED_EDGE('',*,*,#37440,.T.) ;
#49218 = ORIENTED_EDGE('',*,*,#37441,.T.) ;
#49219 = ORIENTED_EDGE('',*,*,#37442,.T.) ;
#49220 = ORIENTED_EDGE('',*,*,#37443,.T.) ;
#49221 = ORIENTED_EDGE('',*,*,#37444,.T.) ;
#49222 = ORIENTED_EDGE('',*,*,#37152,.F.) ;
#49223 = ORIENTED_EDGE('',*,*,#37445,.T.) ;
#49224 = ORIENTED_EDGE('',*,*,#37446,.T.) ;
#49225 = ORIENTED_EDGE('',*,*,#37066,.T.) ;
#49226 = ORIENTED_EDGE('',*,*,#37447,.T.) ;
#49227 = ORIENTED_EDGE('',*,*,#37130,.F.) ;
#49228 = ORIENTED_EDGE('',*,*,#37448,.T.) ;
#49229 = ORIENTED_EDGE('',*,*,#37449,.T.) ;
#49230 = ORIENTED_EDGE('',*,*,#37450,.T.) ;
#49231 = ORIENTED_EDGE('',*,*,#37451,.F.) ;
#49232 = ORIENTED_EDGE('',*,*,#37349,.F.) ;
#49233 = ORIENTED_EDGE('',*,*,#37162,.F.) ;
#49234 = ORIENTED_EDGE('',*,*,#37342,.F.) ;
#49235 = ORIENTED_EDGE('',*,*,#37452,.F.) ;
#49236 = ORIENTED_EDGE('',*,*,#37451,.T.) ;
#49237 = ORIENTED_EDGE('',*,*,#37453,.F.) ;
#49238 = ORIENTED_EDGE('',*,*,#37160,.F.) ;
#49239 = ORIENTED_EDGE('',*,*,#37217,.F.) ;
#49240 = ORIENTED_EDGE('',*,*,#37454,.F.) ;
#49241 = ORIENTED_EDGE('',*,*,#37340,.F.) ;
#49242 = ORIENTED_EDGE('',*,*,#37453,.T.) ;
#49243 = ORIENTED_EDGE('',*,*,#37341,.F.) ;
#49244 = ORIENTED_EDGE('',*,*,#37455,.F.) ;
#49245 = ORIENTED_EDGE('',*,*,#37337,.F.) ;
#49246 = ORIENTED_EDGE('',*,*,#37452,.T.) ;
#49247 = ORIENTED_EDGE('',*,*,#37336,.F.) ;
#49248 = ORIENTED_EDGE('',*,*,#37456,.F.) ;
#49249 = ORIENTED_EDGE('',*,*,#37350,.F.) ;
#49250 = ORIENTED_EDGE('',*,*,#37454,.T.) ;
#49251 = ORIENTED_EDGE('',*,*,#37216,.T.) ;
#49252 = ORIENTED_EDGE('',*,*,#37457,.F.) ;
#49253 = ORIENTED_EDGE('',*,*,#37455,.T.) ;
#49254 = ORIENTED_EDGE('',*,*,#37458,.F.) ;
#49255 = ORIENTED_EDGE('',*,*,#37456,.T.) ;
#49256 = ORIENTED_EDGE('',*,*,#37459,.F.) ;
#49257 = ORIENTED_EDGE('',*,*,#37120,.F.) ;
#49258 = ORIENTED_EDGE('',*,*,#37322,.F.) ;
#49259 = ORIENTED_EDGE('',*,*,#37460,.F.) ;
#49260 = ORIENTED_EDGE('',*,*,#37327,.F.) ;
#49261 = ORIENTED_EDGE('',*,*,#37461,.F.) ;
#49262 = ORIENTED_EDGE('',*,*,#37325,.F.) ;
#49263 = ORIENTED_EDGE('',*,*,#37462,.F.) ;
#49264 = ORIENTED_EDGE('',*,*,#37331,.F.) ;
#49265 = ORIENTED_EDGE('',*,*,#37122,.F.) ;
#49266 = ORIENTED_EDGE('',*,*,#37326,.F.) ;
#49267 = ORIENTED_EDGE('',*,*,#37463,.F.) ;
#49268 = ORIENTED_EDGE('',*,*,#37207,.F.) ;
#49269 = ORIENTED_EDGE('',*,*,#37457,.T.) ;
#49270 = ORIENTED_EDGE('',*,*,#37215,.F.) ;
#49271 = ORIENTED_EDGE('',*,*,#37464,.F.) ;
#49272 = ORIENTED_EDGE('',*,*,#37338,.F.) ;
#49273 = ORIENTED_EDGE('',*,*,#37459,.T.) ;
#49274 = ORIENTED_EDGE('',*,*,#37339,.F.) ;
#49275 = ORIENTED_EDGE('',*,*,#37465,.F.) ;
#49276 = ORIENTED_EDGE('',*,*,#37346,.F.) ;
#49277 = ORIENTED_EDGE('',*,*,#37458,.T.) ;
#49278 = ORIENTED_EDGE('',*,*,#37345,.F.) ;
#49279 = ORIENTED_EDGE('',*,*,#37466,.F.) ;
#49280 = ORIENTED_EDGE('',*,*,#37347,.F.) ;
#49281 = ORIENTED_EDGE('',*,*,#37164,.F.) ;
#49282 = ORIENTED_EDGE('',*,*,#37348,.F.) ;
#49283 = ORIENTED_EDGE('',*,*,#37467,.F.) ;
#49284 = ORIENTED_EDGE('',*,*,#37198,.F.) ;
#49285 = ORIENTED_EDGE('',*,*,#37462,.T.) ;
#49286 = ORIENTED_EDGE('',*,*,#37460,.T.) ;
#49287 = ORIENTED_EDGE('',*,*,#37468,.F.) ;
#49288 = ORIENTED_EDGE('',*,*,#37463,.T.) ;
#49289 = ORIENTED_EDGE('',*,*,#37461,.T.) ;
#49290 = ORIENTED_EDGE('',*,*,#37469,.F.) ;
#49291 = ORIENTED_EDGE('',*,*,#37208,.T.) ;
#49292 = ORIENTED_EDGE('',*,*,#37464,.T.) ;
#49293 = ORIENTED_EDGE('',*,*,#37214,.T.) ;
#49294 = ORIENTED_EDGE('',*,*,#37470,.F.) ;
#49295 = ORIENTED_EDGE('',*,*,#37465,.T.) ;
#49296 = ORIENTED_EDGE('',*,*,#37467,.T.) ;
#49297 = ORIENTED_EDGE('',*,*,#37466,.T.) ;
#49298 = ORIENTED_EDGE('',*,*,#37471,.F.) ;
#49299 = ORIENTED_EDGE('',*,*,#37468,.T.) ;
#49300 = ORIENTED_EDGE('',*,*,#37321,.F.) ;
#49301 = ORIENTED_EDGE('',*,*,#37472,.F.) ;
#49302 = ORIENTED_EDGE('',*,*,#37328,.F.) ;
#49303 = ORIENTED_EDGE('',*,*,#37473,.F.) ;
#49304 = ORIENTED_EDGE('',*,*,#37329,.F.) ;
#49305 = ORIENTED_EDGE('',*,*,#37474,.F.) ;
#49306 = ORIENTED_EDGE('',*,*,#37335,.F.) ;
#49307 = ORIENTED_EDGE('',*,*,#37469,.T.) ;
#49308 = ORIENTED_EDGE('',*,*,#37330,.F.) ;
#49309 = ORIENTED_EDGE('',*,*,#37475,.F.) ;
#49310 = ORIENTED_EDGE('',*,*,#37209,.F.) ;
#49311 = ORIENTED_EDGE('',*,*,#37470,.T.) ;
#49312 = ORIENTED_EDGE('',*,*,#37213,.F.) ;
#49313 = ORIENTED_EDGE('',*,*,#37476,.F.) ;
#49314 = ORIENTED_EDGE('',*,*,#37343,.F.) ;
#49315 = ORIENTED_EDGE('',*,*,#37471,.T.) ;
#49316 = ORIENTED_EDGE('',*,*,#37344,.F.) ;
#49317 = ORIENTED_EDGE('',*,*,#37477,.F.) ;
#49318 = ORIENTED_EDGE('',*,*,#37199,.F.) ;
#49319 = ORIENTED_EDGE('',*,*,#37474,.T.) ;
#49320 = ORIENTED_EDGE('',*,*,#37472,.T.) ;
#49321 = ORIENTED_EDGE('',*,*,#37478,.F.) ;
#49322 = ORIENTED_EDGE('',*,*,#37475,.T.) ;
#49323 = ORIENTED_EDGE('',*,*,#37473,.T.) ;
#49324 = ORIENTED_EDGE('',*,*,#37479,.F.) ;
#49325 = ORIENTED_EDGE('',*,*,#37210,.T.) ;
#49326 = ORIENTED_EDGE('',*,*,#37477,.T.) ;
#49327 = ORIENTED_EDGE('',*,*,#37476,.T.) ;
#49328 = ORIENTED_EDGE('',*,*,#37480,.F.) ;
#49329 = ORIENTED_EDGE('',*,*,#37200,.T.) ;
#49330 = ORIENTED_EDGE('',*,*,#37118,.F.) ;
#49331 = ORIENTED_EDGE('',*,*,#37204,.F.) ;
#49332 = ORIENTED_EDGE('',*,*,#37481,.F.) ;
#49333 = ORIENTED_EDGE('',*,*,#37323,.F.) ;
#49334 = ORIENTED_EDGE('',*,*,#37478,.T.) ;
#49335 = ORIENTED_EDGE('',*,*,#37324,.F.) ;
#49336 = ORIENTED_EDGE('',*,*,#37482,.F.) ;
#49337 = ORIENTED_EDGE('',*,*,#37332,.F.) ;
#49338 = ORIENTED_EDGE('',*,*,#37479,.T.) ;
#49339 = ORIENTED_EDGE('',*,*,#37334,.F.) ;
#49340 = ORIENTED_EDGE('',*,*,#37483,.F.) ;
#49341 = ORIENTED_EDGE('',*,*,#37211,.F.) ;
#49342 = ORIENTED_EDGE('',*,*,#37480,.T.) ;
#49343 = ORIENTED_EDGE('',*,*,#37212,.F.) ;
#49344 = ORIENTED_EDGE('',*,*,#37484,.F.) ;
#49345 = ORIENTED_EDGE('',*,*,#37201,.F.) ;
#49346 = ORIENTED_EDGE('',*,*,#37482,.T.) ;
#49347 = ORIENTED_EDGE('',*,*,#37481,.T.) ;
#49348 = ORIENTED_EDGE('',*,*,#37485,.F.) ;
#49349 = ORIENTED_EDGE('',*,*,#37484,.T.) ;
#49350 = ORIENTED_EDGE('',*,*,#37483,.T.) ;
#49351 = ORIENTED_EDGE('',*,*,#37486,.F.) ;
#49352 = ORIENTED_EDGE('',*,*,#37202,.T.) ;
#49353 = ORIENTED_EDGE('',*,*,#37485,.T.) ;
#49354 = ORIENTED_EDGE('',*,*,#37203,.F.) ;
#49355 = ORIENTED_EDGE('',*,*,#37486,.T.) ;
#49356 = ORIENTED_EDGE('',*,*,#37333,.F.) ;
#49357 = ORIENTED_EDGE('',*,*,#37487,.F.) ;
#49358 = ORIENTED_EDGE('',*,*,#37488,.F.) ;
#49359 = ORIENTED_EDGE('',*,*,#37489,.F.) ;
#49360 = ORIENTED_EDGE('',*,*,#37280,.F.) ;
#49361 = ORIENTED_EDGE('',*,*,#37490,.T.) ;
#49362 = ORIENTED_EDGE('',*,*,#37491,.T.) ;
#49363 = ORIENTED_EDGE('',*,*,#37262,.F.) ;
#49364 = ORIENTED_EDGE('',*,*,#37488,.T.) ;
#49365 = ORIENTED_EDGE('',*,*,#37261,.F.) ;
#49366 = ORIENTED_EDGE('',*,*,#37492,.T.) ;
#49367 = ORIENTED_EDGE('',*,*,#37493,.T.) ;
#49368 = ORIENTED_EDGE('',*,*,#37254,.F.) ;
#49369 = ORIENTED_EDGE('',*,*,#37489,.T.) ;
#49370 = ORIENTED_EDGE('',*,*,#37487,.T.) ;
#49371 = ORIENTED_EDGE('',*,*,#37253,.F.) ;
#49372 = ORIENTED_EDGE('',*,*,#37494,.F.) ;
#49373 = ORIENTED_EDGE('',*,*,#37273,.F.) ;
#49374 = ORIENTED_EDGE('',*,*,#37269,.F.) ;
#49375 = ORIENTED_EDGE('',*,*,#37495,.T.) ;
#49376 = ORIENTED_EDGE('',*,*,#37496,.T.) ;
#49377 = ORIENTED_EDGE('',*,*,#37279,.F.) ;
#49378 = ORIENTED_EDGE('',*,*,#37497,.T.) ;
#49379 = ORIENTED_EDGE('',*,*,#37498,.T.) ;
#49380 = ORIENTED_EDGE('',*,*,#37247,.F.) ;
#49381 = ORIENTED_EDGE('',*,*,#37499,.T.) ;
#49382 = ORIENTED_EDGE('',*,*,#37500,.T.) ;
#49383 = ORIENTED_EDGE('',*,*,#37263,.F.) ;
#49384 = ORIENTED_EDGE('',*,*,#37501,.T.) ;
#49385 = ORIENTED_EDGE('',*,*,#37502,.T.) ;
#49386 = ORIENTED_EDGE('',*,*,#37503,.F.) ;
#49387 = ORIENTED_EDGE('',*,*,#37494,.T.) ;
#49388 = ORIENTED_EDGE('',*,*,#37504,.F.) ;
#49389 = ORIENTED_EDGE('',*,*,#37244,.T.) ;
#49390 = ORIENTED_EDGE('',*,*,#37505,.F.) ;
#49391 = ORIENTED_EDGE('',*,*,#37506,.F.) ;
#49392 = ORIENTED_EDGE('',*,*,#37274,.F.) ;
#49393 = ORIENTED_EDGE('',*,*,#37503,.T.) ;
#49394 = ORIENTED_EDGE('',*,*,#37506,.T.) ;
#49395 = ORIENTED_EDGE('',*,*,#37507,.F.) ;
#49396 = ORIENTED_EDGE('',*,*,#37508,.F.) ;
#49397 = ORIENTED_EDGE('',*,*,#37258,.F.) ;
#49398 = ORIENTED_EDGE('',*,*,#37509,.T.) ;
#49399 = ORIENTED_EDGE('',*,*,#37510,.T.) ;
#49400 = ORIENTED_EDGE('',*,*,#37278,.F.) ;
#49401 = ORIENTED_EDGE('',*,*,#37511,.F.) ;
#49402 = ORIENTED_EDGE('',*,*,#37248,.F.) ;
#49403 = ORIENTED_EDGE('',*,*,#37512,.T.) ;
#49404 = ORIENTED_EDGE('',*,*,#37513,.T.) ;
#49405 = ORIENTED_EDGE('',*,*,#37255,.F.) ;
#49406 = ORIENTED_EDGE('',*,*,#37514,.F.) ;
#49407 = ORIENTED_EDGE('',*,*,#37504,.T.) ;
#49408 = ORIENTED_EDGE('',*,*,#37252,.F.) ;
#49409 = ORIENTED_EDGE('',*,*,#37515,.F.) ;
#49410 = ORIENTED_EDGE('',*,*,#37516,.F.) ;
#49411 = ORIENTED_EDGE('',*,*,#37517,.F.) ;
#49412 = ORIENTED_EDGE('',*,*,#37228,.F.) ;
#49413 = ORIENTED_EDGE('',*,*,#37518,.F.) ;
#49414 = ORIENTED_EDGE('',*,*,#37505,.T.) ;
#49415 = ORIENTED_EDGE('',*,*,#37246,.F.) ;
#49416 = ORIENTED_EDGE('',*,*,#37518,.T.) ;
#49417 = ORIENTED_EDGE('',*,*,#37227,.T.) ;
#49418 = ORIENTED_EDGE('',*,*,#37519,.F.) ;
#49419 = ORIENTED_EDGE('',*,*,#37507,.T.) ;
#49420 = ORIENTED_EDGE('',*,*,#37275,.F.) ;
#49421 = ORIENTED_EDGE('',*,*,#37508,.T.) ;
#49422 = ORIENTED_EDGE('',*,*,#37520,.F.) ;
#49423 = ORIENTED_EDGE('',*,*,#37521,.F.) ;
#49424 = ORIENTED_EDGE('',*,*,#37514,.T.) ;
#49425 = ORIENTED_EDGE('',*,*,#37511,.T.) ;
#49426 = ORIENTED_EDGE('',*,*,#37522,.F.) ;
#49427 = ORIENTED_EDGE('',*,*,#37523,.F.) ;
#49428 = ORIENTED_EDGE('',*,*,#37515,.T.) ;
#49429 = ORIENTED_EDGE('',*,*,#37524,.F.) ;
#49430 = ORIENTED_EDGE('',*,*,#37245,.F.) ;
#49431 = ORIENTED_EDGE('',*,*,#37516,.T.) ;
#49432 = ORIENTED_EDGE('',*,*,#37525,.F.) ;
#49433 = ORIENTED_EDGE('',*,*,#37238,.F.) ;
#49434 = ORIENTED_EDGE('',*,*,#37517,.T.) ;
#49435 = ORIENTED_EDGE('',*,*,#37526,.F.) ;
#49436 = ORIENTED_EDGE('',*,*,#37520,.T.) ;
#49437 = ORIENTED_EDGE('',*,*,#37519,.T.) ;
#49438 = ORIENTED_EDGE('',*,*,#37234,.F.) ;
#49439 = ORIENTED_EDGE('',*,*,#37521,.T.) ;
#49440 = ORIENTED_EDGE('',*,*,#37527,.F.) ;
#49441 = ORIENTED_EDGE('',*,*,#37528,.F.) ;
#49442 = ORIENTED_EDGE('',*,*,#37522,.T.) ;
#49443 = ORIENTED_EDGE('',*,*,#37277,.F.) ;
#49444 = ORIENTED_EDGE('',*,*,#37529,.F.) ;
#49445 = ORIENTED_EDGE('',*,*,#37249,.F.) ;
#49446 = ORIENTED_EDGE('',*,*,#37524,.T.) ;
#49447 = ORIENTED_EDGE('',*,*,#37251,.F.) ;
#49448 = ORIENTED_EDGE('',*,*,#37530,.F.) ;
#49449 = ORIENTED_EDGE('',*,*,#37531,.F.) ;
#49450 = ORIENTED_EDGE('',*,*,#37525,.T.) ;
#49451 = ORIENTED_EDGE('',*,*,#37523,.T.) ;
#49452 = ORIENTED_EDGE('',*,*,#37532,.F.) ;
#49453 = ORIENTED_EDGE('',*,*,#37239,.T.) ;
#49454 = ORIENTED_EDGE('',*,*,#37526,.T.) ;
#49455 = ORIENTED_EDGE('',*,*,#37233,.T.) ;
#49456 = ORIENTED_EDGE('',*,*,#37533,.F.) ;
#49457 = ORIENTED_EDGE('',*,*,#37527,.T.) ;
#49458 = ORIENTED_EDGE('',*,*,#37534,.F.) ;
#49459 = ORIENTED_EDGE('',*,*,#37535,.F.) ;
#49460 = ORIENTED_EDGE('',*,*,#37276,.F.) ;
#49461 = ORIENTED_EDGE('',*,*,#37528,.T.) ;
#49462 = ORIENTED_EDGE('',*,*,#37535,.T.) ;
#49463 = ORIENTED_EDGE('',*,*,#37243,.T.) ;
#49464 = ORIENTED_EDGE('',*,*,#37536,.F.) ;
#49465 = ORIENTED_EDGE('',*,*,#37529,.T.) ;
#49466 = ORIENTED_EDGE('',*,*,#37537,.F.) ;
#49467 = ORIENTED_EDGE('',*,*,#37530,.T.) ;
#49468 = ORIENTED_EDGE('',*,*,#37538,.F.) ;
#49469 = ORIENTED_EDGE('',*,*,#37532,.T.) ;
#49470 = ORIENTED_EDGE('',*,*,#37531,.T.) ;
#49471 = ORIENTED_EDGE('',*,*,#37539,.F.) ;
#49472 = ORIENTED_EDGE('',*,*,#37240,.F.) ;
#49473 = ORIENTED_EDGE('',*,*,#37533,.T.) ;
#49474 = ORIENTED_EDGE('',*,*,#37232,.F.) ;
#49475 = ORIENTED_EDGE('',*,*,#37540,.F.) ;
#49476 = ORIENTED_EDGE('',*,*,#37241,.F.) ;
#49477 = ORIENTED_EDGE('',*,*,#37534,.T.) ;
#49478 = ORIENTED_EDGE('',*,*,#37250,.F.) ;
#49479 = ORIENTED_EDGE('',*,*,#37536,.T.) ;
#49480 = ORIENTED_EDGE('',*,*,#37541,.F.) ;
#49481 = ORIENTED_EDGE('',*,*,#37538,.T.) ;
#49482 = ORIENTED_EDGE('',*,*,#37539,.T.) ;
#49483 = ORIENTED_EDGE('',*,*,#37537,.T.) ;
#49484 = ORIENTED_EDGE('',*,*,#37542,.F.) ;
#49485 = ORIENTED_EDGE('',*,*,#37235,.T.) ;
#49486 = ORIENTED_EDGE('',*,*,#37540,.T.) ;
#49487 = ORIENTED_EDGE('',*,*,#37236,.F.) ;
#49488 = ORIENTED_EDGE('',*,*,#37542,.T.) ;
#49489 = ORIENTED_EDGE('',*,*,#37541,.T.) ;
#49490 = ORIENTED_EDGE('',*,*,#37242,.F.) ;
#49491 = ORIENTED_EDGE('',*,*,#37543,.F.) ;
#49492 = ORIENTED_EDGE('',*,*,#37291,.F.) ;
#49493 = ORIENTED_EDGE('',*,*,#37126,.F.) ;
#49494 = ORIENTED_EDGE('',*,*,#37297,.F.) ;
#49495 = ORIENTED_EDGE('',*,*,#37544,.F.) ;
#49496 = ORIENTED_EDGE('',*,*,#37543,.T.) ;
#49497 = ORIENTED_EDGE('',*,*,#37545,.F.) ;
#49498 = ORIENTED_EDGE('',*,*,#37124,.F.) ;
#49499 = ORIENTED_EDGE('',*,*,#37206,.F.) ;
#49500 = ORIENTED_EDGE('',*,*,#37546,.F.) ;
#49501 = ORIENTED_EDGE('',*,*,#37295,.F.) ;
#49502 = ORIENTED_EDGE('',*,*,#37545,.T.) ;
#49503 = ORIENTED_EDGE('',*,*,#37296,.F.) ;
#49504 = ORIENTED_EDGE('',*,*,#37547,.F.) ;
#49505 = ORIENTED_EDGE('',*,*,#37302,.F.) ;
#49506 = ORIENTED_EDGE('',*,*,#37544,.T.) ;
#49507 = ORIENTED_EDGE('',*,*,#37301,.F.) ;
#49508 = ORIENTED_EDGE('',*,*,#37548,.F.) ;
#49509 = ORIENTED_EDGE('',*,*,#37292,.F.) ;
#49510 = ORIENTED_EDGE('',*,*,#37128,.F.) ;
#49511 = ORIENTED_EDGE('',*,*,#37290,.F.) ;
#49512 = ORIENTED_EDGE('',*,*,#37549,.F.) ;
#49513 = ORIENTED_EDGE('',*,*,#37101,.F.) ;
#49514 = ORIENTED_EDGE('',*,*,#37069,.F.) ;
#49515 = ORIENTED_EDGE('',*,*,#37550,.T.) ;
#49516 = ORIENTED_EDGE('',*,*,#37098,.F.) ;
#49517 = ORIENTED_EDGE('',*,*,#37551,.F.) ;
#49518 = ORIENTED_EDGE('',*,*,#37546,.T.) ;
#49519 = ORIENTED_EDGE('',*,*,#37205,.T.) ;
#49520 = ORIENTED_EDGE('',*,*,#37552,.F.) ;
#49521 = ORIENTED_EDGE('',*,*,#37547,.T.) ;
#49522 = ORIENTED_EDGE('',*,*,#37553,.F.) ;
#49523 = ORIENTED_EDGE('',*,*,#37548,.T.) ;
#49524 = ORIENTED_EDGE('',*,*,#37554,.F.) ;
#49525 = ORIENTED_EDGE('',*,*,#37549,.T.) ;
#49526 = ORIENTED_EDGE('',*,*,#37289,.T.) ;
#49527 = ORIENTED_EDGE('',*,*,#37555,.F.) ;
#49528 = ORIENTED_EDGE('',*,*,#37551,.T.) ;
#49529 = ORIENTED_EDGE('',*,*,#37552,.T.) ;
#49530 = ORIENTED_EDGE('',*,*,#37226,.F.) ;
#49531 = ORIENTED_EDGE('',*,*,#37556,.F.) ;
#49532 = ORIENTED_EDGE('',*,*,#37303,.F.) ;
#49533 = ORIENTED_EDGE('',*,*,#37554,.T.) ;
#49534 = ORIENTED_EDGE('',*,*,#37304,.F.) ;
#49535 = ORIENTED_EDGE('',*,*,#37557,.F.) ;
#49536 = ORIENTED_EDGE('',*,*,#37298,.F.) ;
#49537 = ORIENTED_EDGE('',*,*,#37553,.T.) ;
#49538 = ORIENTED_EDGE('',*,*,#37300,.F.) ;
#49539 = ORIENTED_EDGE('',*,*,#37558,.F.) ;
#49540 = ORIENTED_EDGE('',*,*,#37293,.F.) ;
#49541 = ORIENTED_EDGE('',*,*,#37555,.T.) ;
#49542 = ORIENTED_EDGE('',*,*,#37294,.F.) ;
#49543 = ORIENTED_EDGE('',*,*,#37559,.F.) ;
#49544 = ORIENTED_EDGE('',*,*,#37070,.F.) ;
#49545 = ORIENTED_EDGE('',*,*,#37104,.F.) ;
#49546 = ORIENTED_EDGE('',*,*,#37560,.T.) ;
#49547 = ORIENTED_EDGE('',*,*,#37075,.F.) ;
#49548 = ORIENTED_EDGE('',*,*,#37561,.F.) ;
#49549 = ORIENTED_EDGE('',*,*,#37154,.F.) ;
#49550 = ORIENTED_EDGE('',*,*,#37105,.F.) ;
#49551 = ORIENTED_EDGE('',*,*,#37562,.F.) ;
#49552 = ORIENTED_EDGE('',*,*,#37317,.F.) ;
#49553 = ORIENTED_EDGE('',*,*,#37156,.F.) ;
#49554 = ORIENTED_EDGE('',*,*,#37316,.F.) ;
#49555 = ORIENTED_EDGE('',*,*,#37563,.F.) ;
#49556 = ORIENTED_EDGE('',*,*,#37314,.F.) ;
#49557 = ORIENTED_EDGE('',*,*,#37556,.T.) ;
#49558 = ORIENTED_EDGE('',*,*,#37225,.T.) ;
#49559 = ORIENTED_EDGE('',*,*,#37564,.F.) ;
#49560 = ORIENTED_EDGE('',*,*,#37557,.T.) ;
#49561 = ORIENTED_EDGE('',*,*,#37559,.T.) ;
#49562 = ORIENTED_EDGE('',*,*,#37558,.T.) ;
#49563 = ORIENTED_EDGE('',*,*,#37062,.F.) ;
#49564 = ORIENTED_EDGE('',*,*,#37562,.T.) ;
#49565 = ORIENTED_EDGE('',*,*,#37561,.T.) ;
#49566 = ORIENTED_EDGE('',*,*,#37565,.F.) ;
#49567 = ORIENTED_EDGE('',*,*,#37318,.T.) ;
#49568 = ORIENTED_EDGE('',*,*,#37566,.F.) ;
#49569 = ORIENTED_EDGE('',*,*,#37563,.T.) ;
#49570 = ORIENTED_EDGE('',*,*,#37567,.F.) ;
#49571 = ORIENTED_EDGE('',*,*,#37564,.T.) ;
#49572 = ORIENTED_EDGE('',*,*,#37224,.F.) ;
#49573 = ORIENTED_EDGE('',*,*,#37568,.F.) ;
#49574 = ORIENTED_EDGE('',*,*,#37299,.F.) ;
#49575 = ORIENTED_EDGE('',*,*,#37565,.T.) ;
#49576 = ORIENTED_EDGE('',*,*,#37074,.F.) ;
#49577 = ORIENTED_EDGE('',*,*,#37569,.F.) ;
#49578 = ORIENTED_EDGE('',*,*,#37319,.F.) ;
#49579 = ORIENTED_EDGE('',*,*,#37570,.F.) ;
#49580 = ORIENTED_EDGE('',*,*,#37320,.F.) ;
#49581 = ORIENTED_EDGE('',*,*,#37571,.F.) ;
#49582 = ORIENTED_EDGE('',*,*,#37311,.F.) ;
#49583 = ORIENTED_EDGE('',*,*,#37567,.T.) ;
#49584 = ORIENTED_EDGE('',*,*,#37315,.F.) ;
#49585 = ORIENTED_EDGE('',*,*,#37572,.F.) ;
#49586 = ORIENTED_EDGE('',*,*,#37305,.F.) ;
#49587 = ORIENTED_EDGE('',*,*,#37566,.T.) ;
#49588 = ORIENTED_EDGE('',*,*,#37308,.F.) ;
#49589 = ORIENTED_EDGE('',*,*,#37573,.F.) ;
#49590 = ORIENTED_EDGE('',*,*,#37312,.F.) ;
#49591 = ORIENTED_EDGE('',*,*,#37158,.F.) ;
#49592 = ORIENTED_EDGE('',*,*,#37313,.F.) ;
#49593 = ORIENTED_EDGE('',*,*,#37574,.F.) ;
#49594 = ORIENTED_EDGE('',*,*,#37218,.F.) ;
#49595 = ORIENTED_EDGE('',*,*,#37060,.T.) ;
#49596 = ORIENTED_EDGE('',*,*,#37568,.T.) ;
#49597 = ORIENTED_EDGE('',*,*,#37575,.F.) ;
#49598 = ORIENTED_EDGE('',*,*,#37071,.T.) ;
#49599 = ORIENTED_EDGE('',*,*,#37571,.T.) ;
#49600 = ORIENTED_EDGE('',*,*,#37569,.T.) ;
#49601 = ORIENTED_EDGE('',*,*,#37058,.F.) ;
#49602 = ORIENTED_EDGE('',*,*,#37576,.F.) ;
#49603 = ORIENTED_EDGE('',*,*,#37576,.T.) ;
#49604 = ORIENTED_EDGE('',*,*,#37057,.F.) ;
#49605 = ORIENTED_EDGE('',*,*,#37572,.T.) ;
#49606 = ORIENTED_EDGE('',*,*,#37570,.T.) ;
#49607 = ORIENTED_EDGE('',*,*,#37577,.F.) ;
#49608 = ORIENTED_EDGE('',*,*,#37574,.T.) ;
#49609 = ORIENTED_EDGE('',*,*,#37573,.T.) ;
#49610 = ORIENTED_EDGE('',*,*,#37578,.F.) ;
#49611 = ORIENTED_EDGE('',*,*,#37219,.T.) ;
#49612 = ORIENTED_EDGE('',*,*,#37575,.T.) ;
#49613 = ORIENTED_EDGE('',*,*,#37223,.F.) ;
#49614 = ORIENTED_EDGE('',*,*,#37579,.F.) ;
#49615 = ORIENTED_EDGE('',*,*,#37072,.F.) ;
#49616 = ORIENTED_EDGE('',*,*,#37577,.T.) ;
#49617 = ORIENTED_EDGE('',*,*,#37310,.F.) ;
#49618 = ORIENTED_EDGE('',*,*,#37580,.F.) ;
#49619 = ORIENTED_EDGE('',*,*,#37306,.F.) ;
#49620 = ORIENTED_EDGE('',*,*,#37578,.T.) ;
#49621 = ORIENTED_EDGE('',*,*,#37307,.F.) ;
#49622 = ORIENTED_EDGE('',*,*,#37581,.F.) ;
#49623 = ORIENTED_EDGE('',*,*,#37220,.F.) ;
#49624 = ORIENTED_EDGE('',*,*,#37073,.T.) ;
#49625 = ORIENTED_EDGE('',*,*,#37579,.T.) ;
#49626 = ORIENTED_EDGE('',*,*,#37582,.F.) ;
#49627 = ORIENTED_EDGE('',*,*,#37055,.T.) ;
#49628 = ORIENTED_EDGE('',*,*,#37581,.T.) ;
#49629 = ORIENTED_EDGE('',*,*,#37580,.T.) ;
#49630 = ORIENTED_EDGE('',*,*,#37583,.F.) ;
#49631 = ORIENTED_EDGE('',*,*,#37221,.T.) ;
#49632 = ORIENTED_EDGE('',*,*,#37582,.T.) ;
#49633 = ORIENTED_EDGE('',*,*,#37222,.F.) ;
#49634 = ORIENTED_EDGE('',*,*,#37583,.T.) ;
#49635 = ORIENTED_EDGE('',*,*,#37309,.F.) ;
#49636 = ORIENTED_EDGE('',*,*,#37078,.F.) ;
#49637 = ORIENTED_EDGE('',*,*,#37584,.T.) ;
#49638 = ORIENTED_EDGE('',*,*,#37399,.F.) ;
#49639 = ORIENTED_EDGE('',*,*,#37585,.F.) ;
#49640 = ORIENTED_EDGE('',*,*,#37404,.F.) ;
#49641 = ORIENTED_EDGE('',*,*,#37398,.F.) ;
#49642 = ORIENTED_EDGE('',*,*,#37586,.T.) ;
#49643 = ORIENTED_EDGE('',*,*,#37405,.F.) ;
#49644 = ORIENTED_EDGE('',*,*,#37585,.T.) ;
#49645 = ORIENTED_EDGE('',*,*,#37401,.F.) ;
#49646 = ORIENTED_EDGE('',*,*,#37587,.T.) ;
#49647 = ORIENTED_EDGE('',*,*,#37267,.F.) ;
#49648 = ORIENTED_EDGE('',*,*,#37425,.F.) ;
#49649 = ORIENTED_EDGE('',*,*,#37588,.F.) ;
#49650 = ORIENTED_EDGE('',*,*,#37410,.F.) ;
#49651 = ORIENTED_EDGE('',*,*,#37589,.T.) ;
#49652 = ORIENTED_EDGE('',*,*,#37438,.F.) ;
#49653 = ORIENTED_EDGE('',*,*,#37590,.F.) ;
#49654 = ORIENTED_EDGE('',*,*,#37395,.F.) ;
#49655 = ORIENTED_EDGE('',*,*,#37591,.T.) ;
#49656 = ORIENTED_EDGE('',*,*,#37080,.F.) ;
#49657 = ORIENTED_EDGE('',*,*,#37403,.F.) ;
#49658 = ORIENTED_EDGE('',*,*,#37592,.F.) ;
#49659 = ORIENTED_EDGE('',*,*,#37422,.F.) ;
#49660 = ORIENTED_EDGE('',*,*,#37593,.T.) ;
#49661 = ORIENTED_EDGE('',*,*,#37396,.F.) ;
#49662 = ORIENTED_EDGE('',*,*,#37588,.T.) ;
#49663 = ORIENTED_EDGE('',*,*,#37594,.F.) ;
#49664 = ORIENTED_EDGE('',*,*,#37590,.T.) ;
#49665 = ORIENTED_EDGE('',*,*,#37595,.F.) ;
#49666 = ORIENTED_EDGE('',*,*,#37407,.F.) ;
#49667 = ORIENTED_EDGE('',*,*,#37596,.T.) ;
#49668 = ORIENTED_EDGE('',*,*,#37390,.F.) ;
#49669 = ORIENTED_EDGE('',*,*,#37592,.T.) ;
#49670 = ORIENTED_EDGE('',*,*,#37440,.F.) ;
#49671 = ORIENTED_EDGE('',*,*,#37597,.T.) ;
#49672 = ORIENTED_EDGE('',*,*,#37416,.F.) ;
#49673 = ORIENTED_EDGE('',*,*,#37598,.F.) ;
#49674 = ORIENTED_EDGE('',*,*,#37595,.T.) ;
#49675 = ORIENTED_EDGE('',*,*,#37441,.F.) ;
#49676 = ORIENTED_EDGE('',*,*,#37599,.F.) ;
#49677 = ORIENTED_EDGE('',*,*,#37415,.F.) ;
#49678 = ORIENTED_EDGE('',*,*,#37594,.T.) ;
#49679 = ORIENTED_EDGE('',*,*,#37414,.F.) ;
#49680 = ORIENTED_EDGE('',*,*,#37600,.F.) ;
#49681 = ORIENTED_EDGE('',*,*,#37411,.F.) ;
#49682 = ORIENTED_EDGE('',*,*,#37436,.F.) ;
#49683 = ORIENTED_EDGE('',*,*,#37601,.T.) ;
#49684 = ORIENTED_EDGE('',*,*,#37408,.F.) ;
#49685 = ORIENTED_EDGE('',*,*,#37602,.F.) ;
#49686 = ORIENTED_EDGE('',*,*,#37599,.T.) ;
#49687 = ORIENTED_EDGE('',*,*,#37598,.T.) ;
#49688 = ORIENTED_EDGE('',*,*,#37603,.F.) ;
#49689 = ORIENTED_EDGE('',*,*,#37602,.T.) ;
#49690 = ORIENTED_EDGE('',*,*,#37600,.T.) ;
#49691 = ORIENTED_EDGE('',*,*,#37604,.F.) ;
#49692 = ORIENTED_EDGE('',*,*,#37603,.T.) ;
#49693 = ORIENTED_EDGE('',*,*,#37419,.F.) ;
#49694 = ORIENTED_EDGE('',*,*,#37605,.F.) ;
#49695 = ORIENTED_EDGE('',*,*,#37412,.F.) ;
#49696 = ORIENTED_EDGE('',*,*,#37604,.T.) ;
#49697 = ORIENTED_EDGE('',*,*,#37413,.F.) ;
#49698 = ORIENTED_EDGE('',*,*,#37606,.F.) ;
#49699 = ORIENTED_EDGE('',*,*,#37437,.F.) ;
#49700 = ORIENTED_EDGE('',*,*,#37606,.T.) ;
#49701 = ORIENTED_EDGE('',*,*,#37605,.T.) ;
#49702 = ORIENTED_EDGE('',*,*,#37607,.F.) ;
#49703 = ORIENTED_EDGE('',*,*,#37418,.F.) ;
#49704 = ORIENTED_EDGE('',*,*,#37608,.T.) ;
#49705 = ORIENTED_EDGE('',*,*,#37434,.F.) ;
#49706 = ORIENTED_EDGE('',*,*,#37607,.T.) ;
#49707 = ORIENTED_EDGE('',*,*,#37392,.F.) ;
#49708 = ORIENTED_EDGE('',*,*,#37609,.T.) ;
#49709 = ORIENTED_EDGE('',*,*,#37420,.F.) ;
#49710 = ORIENTED_EDGE('',*,*,#37610,.F.) ;
#49711 = ORIENTED_EDGE('',*,*,#37271,.F.) ;
#49712 = ORIENTED_EDGE('',*,*,#37611,.T.) ;
#49713 = ORIENTED_EDGE('',*,*,#37393,.F.) ;
#49714 = ORIENTED_EDGE('',*,*,#37610,.T.) ;
#49715 = ORIENTED_EDGE('',*,*,#37424,.F.) ;
#49716 = ORIENTED_EDGE('',*,*,#37383,.F.) ;
#49717 = ORIENTED_EDGE('',*,*,#37612,.T.) ;
#49718 = ORIENTED_EDGE('',*,*,#37384,.F.) ;
#49719 = ORIENTED_EDGE('',*,*,#37286,.F.) ;
#49720 = ORIENTED_EDGE('',*,*,#37389,.F.) ;
#49721 = ORIENTED_EDGE('',*,*,#37613,.T.) ;
#49722 = ORIENTED_EDGE('',*,*,#37381,.F.) ;
#49723 = ORIENTED_EDGE('',*,*,#37284,.F.) ;
#49724 = ORIENTED_EDGE('',*,*,#37368,.F.) ;
#49725 = ORIENTED_EDGE('',*,*,#37614,.T.) ;
#49726 = ORIENTED_EDGE('',*,*,#37426,.F.) ;
#49727 = ORIENTED_EDGE('',*,*,#37615,.F.) ;
#49728 = ORIENTED_EDGE('',*,*,#37428,.F.) ;
#49729 = ORIENTED_EDGE('',*,*,#37616,.T.) ;
#49730 = ORIENTED_EDGE('',*,*,#37374,.F.) ;
#49731 = ORIENTED_EDGE('',*,*,#37617,.F.) ;
#49732 = ORIENTED_EDGE('',*,*,#37618,.F.) ;
#49733 = ORIENTED_EDGE('',*,*,#37429,.F.) ;
#49734 = ORIENTED_EDGE('',*,*,#37619,.F.) ;
#49735 = ORIENTED_EDGE('',*,*,#37373,.F.) ;
#49736 = ORIENTED_EDGE('',*,*,#37615,.T.) ;
#49737 = ORIENTED_EDGE('',*,*,#37618,.T.) ;
#49738 = ORIENTED_EDGE('',*,*,#37620,.F.) ;
#49739 = ORIENTED_EDGE('',*,*,#37386,.F.) ;
#49740 = ORIENTED_EDGE('',*,*,#37621,.T.) ;
#49741 = ORIENTED_EDGE('',*,*,#37378,.F.) ;
#49742 = ORIENTED_EDGE('',*,*,#37288,.F.) ;
#49743 = ORIENTED_EDGE('',*,*,#37380,.F.) ;
#49744 = ORIENTED_EDGE('',*,*,#37622,.T.) ;
#49745 = ORIENTED_EDGE('',*,*,#37387,.F.) ;
#49746 = ORIENTED_EDGE('',*,*,#37282,.F.) ;
#49747 = ORIENTED_EDGE('',*,*,#37619,.T.) ;
#49748 = ORIENTED_EDGE('',*,*,#37617,.T.) ;
#49749 = ORIENTED_EDGE('',*,*,#37623,.F.) ;
#49750 = ORIENTED_EDGE('',*,*,#37620,.T.) ;
#49751 = ORIENTED_EDGE('',*,*,#37372,.F.) ;
#49752 = ORIENTED_EDGE('',*,*,#37624,.F.) ;
#49753 = ORIENTED_EDGE('',*,*,#37369,.F.) ;
#49754 = ORIENTED_EDGE('',*,*,#37432,.F.) ;
#49755 = ORIENTED_EDGE('',*,*,#37625,.T.) ;
#49756 = ORIENTED_EDGE('',*,*,#37366,.F.) ;
#49757 = ORIENTED_EDGE('',*,*,#37626,.F.) ;
#49758 = ORIENTED_EDGE('',*,*,#37376,.F.) ;
#49759 = ORIENTED_EDGE('',*,*,#37627,.T.) ;
#49760 = ORIENTED_EDGE('',*,*,#37430,.F.) ;
#49761 = ORIENTED_EDGE('',*,*,#37628,.F.) ;
#49762 = ORIENTED_EDGE('',*,*,#37623,.T.) ;
#49763 = ORIENTED_EDGE('',*,*,#37377,.F.) ;
#49764 = ORIENTED_EDGE('',*,*,#37629,.F.) ;
#49765 = ORIENTED_EDGE('',*,*,#37370,.F.) ;
#49766 = ORIENTED_EDGE('',*,*,#37626,.T.) ;
#49767 = ORIENTED_EDGE('',*,*,#37624,.T.) ;
#49768 = ORIENTED_EDGE('',*,*,#37630,.F.) ;
#49769 = ORIENTED_EDGE('',*,*,#37629,.T.) ;
#49770 = ORIENTED_EDGE('',*,*,#37628,.T.) ;
#49771 = ORIENTED_EDGE('',*,*,#37631,.F.) ;
#49772 = ORIENTED_EDGE('',*,*,#37630,.T.) ;
#49773 = ORIENTED_EDGE('',*,*,#37371,.F.) ;
#49774 = ORIENTED_EDGE('',*,*,#37631,.T.) ;
#49775 = ORIENTED_EDGE('',*,*,#37433,.F.) ;
#49776 = ORIENTED_EDGE('',*,*,#37115,.F.) ;
#49777 = ORIENTED_EDGE('',*,*,#37091,.F.) ;
#49778 = ORIENTED_EDGE('',*,*,#37632,.F.) ;
#49779 = ORIENTED_EDGE('',*,*,#37097,.F.) ;
#49780 = ORIENTED_EDGE('',*,*,#37353,.F.) ;
#49781 = ORIENTED_EDGE('',*,*,#37633,.T.) ;
#49782 = ORIENTED_EDGE('',*,*,#37092,.F.) ;
#49783 = ORIENTED_EDGE('',*,*,#37634,.F.) ;
#49784 = ORIENTED_EDGE('',*,*,#37634,.T.) ;
#49785 = ORIENTED_EDGE('',*,*,#37632,.T.) ;
#49786 = ORIENTED_EDGE('',*,*,#37635,.F.) ;
#49787 = ORIENTED_EDGE('',*,*,#37114,.F.) ;
#49788 = ORIENTED_EDGE('',*,*,#37087,.F.) ;
#49789 = ORIENTED_EDGE('',*,*,#37636,.F.) ;
#49790 = ORIENTED_EDGE('',*,*,#37089,.F.) ;
#49791 = ORIENTED_EDGE('',*,*,#37635,.T.) ;
#49792 = ORIENTED_EDGE('',*,*,#37090,.F.) ;
#49793 = ORIENTED_EDGE('',*,*,#37637,.F.) ;
#49794 = ORIENTED_EDGE('',*,*,#37354,.F.) ;
#49795 = ORIENTED_EDGE('',*,*,#37637,.T.) ;
#49796 = ORIENTED_EDGE('',*,*,#37636,.T.) ;
#49797 = ORIENTED_EDGE('',*,*,#37638,.F.) ;
#49798 = ORIENTED_EDGE('',*,*,#37086,.F.) ;
#49799 = ORIENTED_EDGE('',*,*,#37639,.T.) ;
#49800 = ORIENTED_EDGE('',*,*,#37351,.F.) ;
#49801 = ORIENTED_EDGE('',*,*,#37638,.T.) ;
#49802 = ORIENTED_EDGE('',*,*,#37190,.F.) ;
#49803 = ORIENTED_EDGE('',*,*,#37042,.T.) ;
#49804 = ORIENTED_EDGE('',*,*,#37640,.T.) ;
#49805 = ORIENTED_EDGE('',*,*,#37362,.F.) ;
#49806 = ORIENTED_EDGE('',*,*,#37641,.F.) ;
#49807 = ORIENTED_EDGE('',*,*,#37168,.F.) ;
#49808 = ORIENTED_EDGE('',*,*,#37191,.F.) ;
#49809 = ORIENTED_EDGE('',*,*,#37642,.F.) ;
#49810 = ORIENTED_EDGE('',*,*,#37188,.F.) ;
#49811 = ORIENTED_EDGE('',*,*,#37642,.T.) ;
#49812 = ORIENTED_EDGE('',*,*,#37641,.T.) ;
#49813 = ORIENTED_EDGE('',*,*,#37643,.F.) ;
#49814 = ORIENTED_EDGE('',*,*,#37643,.T.) ;
#49815 = ORIENTED_EDGE('',*,*,#37365,.F.) ;
#49816 = ORIENTED_EDGE('',*,*,#37644,.F.) ;
#49817 = ORIENTED_EDGE('',*,*,#37186,.F.) ;
#49818 = ORIENTED_EDGE('',*,*,#37170,.F.) ;
#49819 = ORIENTED_EDGE('',*,*,#37187,.F.) ;
#49820 = ORIENTED_EDGE('',*,*,#37645,.F.) ;
#49821 = ORIENTED_EDGE('',*,*,#37184,.F.) ;
#49822 = ORIENTED_EDGE('',*,*,#37645,.T.) ;
#49823 = ORIENTED_EDGE('',*,*,#37644,.T.) ;
#49824 = ORIENTED_EDGE('',*,*,#37646,.F.) ;
#49825 = ORIENTED_EDGE('',*,*,#37364,.F.) ;
#49826 = ORIENTED_EDGE('',*,*,#37046,.T.) ;
#49827 = ORIENTED_EDGE('',*,*,#37647,.T.) ;
#49828 = ORIENTED_EDGE('',*,*,#37185,.F.) ;
#49829 = ORIENTED_EDGE('',*,*,#37646,.T.) ;
#49830 = ORIENTED_EDGE('',*,*,#37265,.F.) ;
#49831 = ORIENTED_EDGE('',*,*,#37648,.T.) ;
#49832 = ORIENTED_EDGE('',*,*,#37076,.F.) ;
#49833 = ORIENTED_EDGE('',*,*,#37649,.T.) ;
#49834 = ORIENTED_EDGE('',*,*,#37135,.F.) ;
#49835 = ORIENTED_EDGE('',*,*,#37237,.F.) ;
#49836 = ORIENTED_EDGE('',*,*,#37147,.F.) ;
#49837 = ORIENTED_EDGE('',*,*,#37171,.F.) ;
#49838 = ORIENTED_EDGE('',*,*,#37137,.F.) ;
#49839 = ORIENTED_EDGE('',*,*,#37172,.F.) ;
#49840 = ORIENTED_EDGE('',*,*,#37145,.F.) ;
#49841 = ORIENTED_EDGE('',*,*,#37173,.F.) ;
#49842 = ORIENTED_EDGE('',*,*,#37139,.F.) ;
#49843 = ORIENTED_EDGE('',*,*,#37174,.F.) ;
#49844 = ORIENTED_EDGE('',*,*,#37143,.F.) ;
#49845 = ORIENTED_EDGE('',*,*,#37177,.F.) ;
#49846 = ORIENTED_EDGE('',*,*,#37132,.F.) ;
#49847 = ORIENTED_EDGE('',*,*,#37107,.F.) ;
#49848 = ORIENTED_EDGE('',*,*,#37150,.F.) ;
#49849 = ORIENTED_EDGE('',*,*,#37230,.F.) ;
#49850 = ORIENTED_EDGE('',*,*,#37450,.F.) ;
#49851 = ORIENTED_EDGE('',*,*,#37650,.T.) ;
#49852 = ORIENTED_EDGE('',*,*,#37109,.F.) ;
#49853 = ORIENTED_EDGE('',*,*,#37131,.F.) ;
#49854 = ORIENTED_EDGE('',*,*,#37445,.F.) ;
#49855 = ORIENTED_EDGE('',*,*,#37651,.T.) ;
#49856 = ORIENTED_EDGE('',*,*,#37110,.F.) ;
#49857 = ORIENTED_EDGE('',*,*,#37652,.T.) ;
#49858 = ORIENTED_EDGE('',*,*,#37111,.F.) ;
#49859 = ORIENTED_EDGE('',*,*,#37653,.T.) ;
#49860 = ORIENTED_EDGE('',*,*,#37442,.F.) ;
#49861 = ORIENTED_EDGE('',*,*,#37151,.F.) ;
#49862 = ORIENTED_EDGE('',*,*,#37490,.F.) ;
#49863 = ORIENTED_EDGE('',*,*,#37496,.F.) ;
#49864 = ORIENTED_EDGE('',*,*,#37495,.F.) ;
#49865 = ORIENTED_EDGE('',*,*,#37654,.F.) ;
#49866 = ORIENTED_EDGE('',*,*,#37491,.F.) ;
#49867 = ORIENTED_EDGE('',*,*,#37584,.F.) ;
#49868 = ORIENTED_EDGE('',*,*,#37077,.F.) ;
#49869 = ORIENTED_EDGE('',*,*,#37655,.F.) ;
#49870 = ORIENTED_EDGE('',*,*,#37259,.F.) ;
#49871 = ORIENTED_EDGE('',*,*,#37654,.T.) ;
#49872 = ORIENTED_EDGE('',*,*,#37268,.F.) ;
#49873 = ORIENTED_EDGE('',*,*,#37587,.F.) ;
#49874 = ORIENTED_EDGE('',*,*,#37400,.F.) ;
#49875 = ORIENTED_EDGE('',*,*,#37655,.T.) ;
#49876 = ORIENTED_EDGE('',*,*,#37648,.F.) ;
#49877 = ORIENTED_EDGE('',*,*,#37656,.F.) ;
#49878 = ORIENTED_EDGE('',*,*,#37656,.T.) ;
#49879 = ORIENTED_EDGE('',*,*,#37264,.F.) ;
#49880 = ORIENTED_EDGE('',*,*,#37657,.F.) ;
#49881 = ORIENTED_EDGE('',*,*,#37260,.F.) ;
#49882 = ORIENTED_EDGE('',*,*,#37499,.F.) ;
#49883 = ORIENTED_EDGE('',*,*,#37493,.F.) ;
#49884 = ORIENTED_EDGE('',*,*,#37492,.F.) ;
#49885 = ORIENTED_EDGE('',*,*,#37657,.T.) ;
#49886 = ORIENTED_EDGE('',*,*,#37500,.F.) ;
#49887 = ORIENTED_EDGE('',*,*,#37512,.F.) ;
#49888 = ORIENTED_EDGE('',*,*,#37502,.F.) ;
#49889 = ORIENTED_EDGE('',*,*,#37501,.F.) ;
#49890 = ORIENTED_EDGE('',*,*,#37658,.F.) ;
#49891 = ORIENTED_EDGE('',*,*,#37513,.F.) ;
#49892 = ORIENTED_EDGE('',*,*,#37658,.T.) ;
#49893 = ORIENTED_EDGE('',*,*,#37266,.F.) ;
#49894 = ORIENTED_EDGE('',*,*,#37659,.F.) ;
#49895 = ORIENTED_EDGE('',*,*,#37256,.F.) ;
#49896 = ORIENTED_EDGE('',*,*,#37659,.T.) ;
#49897 = ORIENTED_EDGE('',*,*,#37649,.F.) ;
#49898 = ORIENTED_EDGE('',*,*,#37660,.F.) ;
#49899 = ORIENTED_EDGE('',*,*,#37611,.F.) ;
#49900 = ORIENTED_EDGE('',*,*,#37270,.F.) ;
#49901 = ORIENTED_EDGE('',*,*,#37661,.F.) ;
#49902 = ORIENTED_EDGE('',*,*,#37257,.F.) ;
#49903 = ORIENTED_EDGE('',*,*,#37660,.T.) ;
#49904 = ORIENTED_EDGE('',*,*,#37081,.F.) ;
#49905 = ORIENTED_EDGE('',*,*,#37591,.F.) ;
#49906 = ORIENTED_EDGE('',*,*,#37394,.F.) ;
#49907 = ORIENTED_EDGE('',*,*,#37661,.T.) ;
#49908 = ORIENTED_EDGE('',*,*,#37498,.F.) ;
#49909 = ORIENTED_EDGE('',*,*,#37497,.F.) ;
#49910 = ORIENTED_EDGE('',*,*,#37510,.F.) ;
#49911 = ORIENTED_EDGE('',*,*,#37509,.F.) ;
#49912 = ORIENTED_EDGE('',*,*,#37085,.F.) ;
#49913 = ORIENTED_EDGE('',*,*,#37662,.T.) ;
#49914 = ORIENTED_EDGE('',*,*,#37355,.F.) ;
#49915 = ORIENTED_EDGE('',*,*,#37663,.F.) ;
#49916 = ORIENTED_EDGE('',*,*,#37639,.F.) ;
#49917 = ORIENTED_EDGE('',*,*,#37663,.T.) ;
#49918 = ORIENTED_EDGE('',*,*,#37361,.F.) ;
#49919 = ORIENTED_EDGE('',*,*,#37664,.F.) ;
#49920 = ORIENTED_EDGE('',*,*,#37352,.F.) ;
#49921 = ORIENTED_EDGE('',*,*,#37664,.T.) ;
#49922 = ORIENTED_EDGE('',*,*,#37360,.F.) ;
#49923 = ORIENTED_EDGE('',*,*,#37665,.F.) ;
#49924 = ORIENTED_EDGE('',*,*,#37666,.F.) ;
#49925 = ORIENTED_EDGE('',*,*,#37667,.F.) ;
#49926 = ORIENTED_EDGE('',*,*,#37668,.F.) ;
#49927 = ORIENTED_EDGE('',*,*,#37093,.F.) ;
#49928 = ORIENTED_EDGE('',*,*,#37633,.F.) ;
#49929 = ORIENTED_EDGE('',*,*,#37116,.F.) ;
#49930 = ORIENTED_EDGE('',*,*,#37095,.F.) ;
#49931 = ORIENTED_EDGE('',*,*,#37669,.F.) ;
#49932 = ORIENTED_EDGE('',*,*,#37193,.F.) ;
#49933 = ORIENTED_EDGE('',*,*,#37094,.F.) ;
#49934 = ORIENTED_EDGE('',*,*,#37668,.T.) ;
#49935 = ORIENTED_EDGE('',*,*,#37667,.T.) ;
#49936 = ORIENTED_EDGE('',*,*,#37666,.T.) ;
#49937 = ORIENTED_EDGE('',*,*,#37665,.T.) ;
#49938 = ORIENTED_EDGE('',*,*,#37670,.F.) ;
#49939 = ORIENTED_EDGE('',*,*,#37194,.F.) ;
#49940 = ORIENTED_EDGE('',*,*,#37669,.T.) ;
#49941 = ORIENTED_EDGE('',*,*,#37045,.F.) ;
#49942 = ORIENTED_EDGE('',*,*,#37671,.T.) ;
#49943 = ORIENTED_EDGE('',*,*,#37181,.F.) ;
#49944 = ORIENTED_EDGE('',*,*,#37647,.F.) ;
#49945 = ORIENTED_EDGE('',*,*,#37670,.T.) ;
#49946 = ORIENTED_EDGE('',*,*,#37359,.F.) ;
#49947 = ORIENTED_EDGE('',*,*,#37672,.F.) ;
#49948 = ORIENTED_EDGE('',*,*,#37195,.F.) ;
#49949 = ORIENTED_EDGE('',*,*,#37166,.F.) ;
#49950 = ORIENTED_EDGE('',*,*,#37197,.F.) ;
#49951 = ORIENTED_EDGE('',*,*,#37673,.F.) ;
#49952 = ORIENTED_EDGE('',*,*,#37192,.F.) ;
#49953 = ORIENTED_EDGE('',*,*,#37047,.T.) ;
#49954 = ORIENTED_EDGE('',*,*,#37363,.F.) ;
#49955 = ORIENTED_EDGE('',*,*,#37674,.F.) ;
#49956 = ORIENTED_EDGE('',*,*,#37357,.F.) ;
#49957 = ORIENTED_EDGE('',*,*,#37196,.F.) ;
#49958 = ORIENTED_EDGE('',*,*,#37672,.T.) ;
#49959 = ORIENTED_EDGE('',*,*,#37675,.F.) ;
#49960 = ORIENTED_EDGE('',*,*,#37676,.F.) ;
#49961 = ORIENTED_EDGE('',*,*,#37677,.F.) ;
#49962 = ORIENTED_EDGE('',*,*,#37040,.F.) ;
#49963 = ORIENTED_EDGE('',*,*,#37039,.F.) ;
#49964 = ORIENTED_EDGE('',*,*,#37189,.F.) ;
#49965 = ORIENTED_EDGE('',*,*,#37673,.T.) ;
#49966 = ORIENTED_EDGE('',*,*,#37041,.F.) ;
#49967 = ORIENTED_EDGE('',*,*,#37677,.T.) ;
#49968 = ORIENTED_EDGE('',*,*,#37676,.T.) ;
#49969 = ORIENTED_EDGE('',*,*,#37675,.T.) ;
#49970 = ORIENTED_EDGE('',*,*,#37358,.F.) ;
#49971 = ORIENTED_EDGE('',*,*,#37674,.T.) ;
#49972 = ORIENTED_EDGE('',*,*,#37640,.F.) ;
#49973 = ORIENTED_EDGE('',*,*,#37678,.F.) ;
#49974 = ORIENTED_EDGE('',*,*,#37103,.F.) ;
#49975 = ORIENTED_EDGE('',*,*,#37153,.F.) ;
#49976 = ORIENTED_EDGE('',*,*,#37444,.F.) ;
#49977 = ORIENTED_EDGE('',*,*,#37560,.F.) ;
#49978 = ORIENTED_EDGE('',*,*,#37678,.T.) ;
#49979 = ORIENTED_EDGE('',*,*,#37679,.F.) ;
#49980 = ORIENTED_EDGE('',*,*,#37065,.F.) ;
#49981 = ORIENTED_EDGE('',*,*,#37679,.T.) ;
#49982 = ORIENTED_EDGE('',*,*,#37443,.F.) ;
#49983 = ORIENTED_EDGE('',*,*,#37680,.F.) ;
#49984 = ORIENTED_EDGE('',*,*,#37447,.F.) ;
#49985 = ORIENTED_EDGE('',*,*,#37653,.F.) ;
#49986 = ORIENTED_EDGE('',*,*,#37651,.F.) ;
#49987 = ORIENTED_EDGE('',*,*,#37680,.T.) ;
#49988 = ORIENTED_EDGE('',*,*,#37681,.T.) ;
#49989 = ORIENTED_EDGE('',*,*,#37586,.F.) ;
#49990 = ORIENTED_EDGE('',*,*,#37682,.F.) ;
#49991 = ORIENTED_EDGE('',*,*,#37589,.F.) ;
#49992 = ORIENTED_EDGE('',*,*,#37681,.F.) ;
#49993 = ORIENTED_EDGE('',*,*,#37409,.F.) ;
#49994 = ORIENTED_EDGE('',*,*,#37683,.F.) ;
#49995 = ORIENTED_EDGE('',*,*,#37406,.F.) ;
#49996 = ORIENTED_EDGE('',*,*,#37682,.T.) ;
#49997 = ORIENTED_EDGE('',*,*,#37397,.F.) ;
#49998 = ORIENTED_EDGE('',*,*,#37684,.F.) ;
#49999 = ORIENTED_EDGE('',*,*,#37439,.F.) ;
#50000 = ORIENTED_EDGE('',*,*,#37683,.T.) ;
#50001 = ORIENTED_EDGE('',*,*,#37601,.F.) ;
#50002 = ORIENTED_EDGE('',*,*,#37685,.F.) ;
#50003 = ORIENTED_EDGE('',*,*,#37596,.F.) ;
#50004 = ORIENTED_EDGE('',*,*,#37684,.T.) ;
#50005 = ORIENTED_EDGE('',*,*,#37593,.F.) ;
#50006 = ORIENTED_EDGE('',*,*,#37686,.F.) ;
#50007 = ORIENTED_EDGE('',*,*,#37597,.F.) ;
#50008 = ORIENTED_EDGE('',*,*,#37685,.T.) ;
#50009 = ORIENTED_EDGE('',*,*,#37435,.F.) ;
#50010 = ORIENTED_EDGE('',*,*,#37687,.F.) ;
#50011 = ORIENTED_EDGE('',*,*,#37391,.F.) ;
#50012 = ORIENTED_EDGE('',*,*,#37686,.T.) ;
#50013 = ORIENTED_EDGE('',*,*,#37421,.F.) ;
#50014 = ORIENTED_EDGE('',*,*,#37688,.F.) ;
#50015 = ORIENTED_EDGE('',*,*,#37417,.F.) ;
#50016 = ORIENTED_EDGE('',*,*,#37687,.T.) ;
#50017 = ORIENTED_EDGE('',*,*,#37608,.F.) ;
#50018 = ORIENTED_EDGE('',*,*,#37688,.T.) ;
#50019 = ORIENTED_EDGE('',*,*,#37609,.F.) ;
#50020 = ORIENTED_EDGE('',*,*,#37689,.T.) ;
#50021 = ORIENTED_EDGE('',*,*,#37612,.F.) ;
#50022 = ORIENTED_EDGE('',*,*,#37690,.F.) ;
#50023 = ORIENTED_EDGE('',*,*,#37614,.F.) ;
#50024 = ORIENTED_EDGE('',*,*,#37689,.F.) ;
#50025 = ORIENTED_EDGE('',*,*,#37367,.F.) ;
#50026 = ORIENTED_EDGE('',*,*,#37691,.F.) ;
#50027 = ORIENTED_EDGE('',*,*,#37385,.F.) ;
#50028 = ORIENTED_EDGE('',*,*,#37690,.T.) ;
#50029 = ORIENTED_EDGE('',*,*,#37382,.F.) ;
#50030 = ORIENTED_EDGE('',*,*,#37692,.F.) ;
#50031 = ORIENTED_EDGE('',*,*,#37427,.F.) ;
#50032 = ORIENTED_EDGE('',*,*,#37691,.T.) ;
#50033 = ORIENTED_EDGE('',*,*,#37625,.F.) ;
#50034 = ORIENTED_EDGE('',*,*,#37693,.F.) ;
#50035 = ORIENTED_EDGE('',*,*,#37621,.F.) ;
#50036 = ORIENTED_EDGE('',*,*,#37692,.T.) ;
#50037 = ORIENTED_EDGE('',*,*,#37613,.F.) ;
#50038 = ORIENTED_EDGE('',*,*,#37694,.F.) ;
#50039 = ORIENTED_EDGE('',*,*,#37616,.F.) ;
#50040 = ORIENTED_EDGE('',*,*,#37693,.T.) ;
#50041 = ORIENTED_EDGE('',*,*,#37431,.F.) ;
#50042 = ORIENTED_EDGE('',*,*,#37695,.F.) ;
#50043 = ORIENTED_EDGE('',*,*,#37379,.F.) ;
#50044 = ORIENTED_EDGE('',*,*,#37694,.T.) ;
#50045 = ORIENTED_EDGE('',*,*,#37388,.F.) ;
#50046 = ORIENTED_EDGE('',*,*,#37696,.F.) ;
#50047 = ORIENTED_EDGE('',*,*,#37375,.F.) ;
#50048 = ORIENTED_EDGE('',*,*,#37695,.T.) ;
#50049 = ORIENTED_EDGE('',*,*,#37627,.F.) ;
#50050 = ORIENTED_EDGE('',*,*,#37696,.T.) ;
#50051 = ORIENTED_EDGE('',*,*,#37622,.F.) ;
#50052 = ORIENTED_EDGE('',*,*,#37129,.F.) ;
#50053 = ORIENTED_EDGE('',*,*,#37099,.F.) ;
#50054 = ORIENTED_EDGE('',*,*,#37697,.F.) ;
#50055 = ORIENTED_EDGE('',*,*,#37448,.F.) ;
#50056 = ORIENTED_EDGE('',*,*,#37697,.T.) ;
#50057 = ORIENTED_EDGE('',*,*,#37550,.F.) ;
#50058 = ORIENTED_EDGE('',*,*,#37067,.F.) ;
#50059 = ORIENTED_EDGE('',*,*,#37698,.F.) ;
#50060 = ORIENTED_EDGE('',*,*,#37698,.T.) ;
#50061 = ORIENTED_EDGE('',*,*,#37446,.F.) ;
#50062 = ORIENTED_EDGE('',*,*,#37699,.F.) ;
#50063 = ORIENTED_EDGE('',*,*,#37449,.F.) ;
#50064 = ORIENTED_EDGE('',*,*,#37652,.F.) ;
#50065 = ORIENTED_EDGE('',*,*,#37650,.F.) ;
#50066 = ORIENTED_EDGE('',*,*,#37699,.T.) ;
#50067 = ORIENTED_EDGE('',*,*,#37183,.F.) ;
#50068 = ORIENTED_EDGE('',*,*,#37700,.F.) ;
#50069 = ORIENTED_EDGE('',*,*,#37178,.F.) ;
#50070 = ORIENTED_EDGE('',*,*,#37141,.F.) ;
#50071 = ORIENTED_EDGE('',*,*,#37182,.F.) ;
#50072 = ORIENTED_EDGE('',*,*,#37671,.F.) ;
#50073 = ORIENTED_EDGE('',*,*,#37044,.F.) ;
#50074 = ORIENTED_EDGE('',*,*,#37701,.F.) ;
#50075 = ORIENTED_EDGE('',*,*,#37179,.F.) ;
#50076 = ORIENTED_EDGE('',*,*,#37700,.T.) ;
#50077 = ORIENTED_EDGE('',*,*,#37701,.T.) ;
#50078 = ORIENTED_EDGE('',*,*,#37356,.F.) ;
#50079 = ORIENTED_EDGE('',*,*,#37702,.F.) ;
#50080 = ORIENTED_EDGE('',*,*,#37180,.F.) ;
#50081 = ORIENTED_EDGE('',*,*,#37662,.F.) ;
#50082 = ORIENTED_EDGE('',*,*,#37084,.F.) ;
#50083 = ORIENTED_EDGE('',*,*,#37703,.F.) ;
#50084 = ORIENTED_EDGE('',*,*,#37175,.F.) ;
#50085 = ORIENTED_EDGE('',*,*,#37702,.T.) ;
#50086 = ORIENTED_EDGE('',*,*,#37113,.F.) ;
#50087 = ORIENTED_EDGE('',*,*,#37176,.F.) ;
#50088 = ORIENTED_EDGE('',*,*,#37703,.T.) ;
#50089 = ORIENTED_EDGE('',*,*,#37083,.F.) ;
#50090 = ORIENTED_EDGE('',*,*,#37704,.T.) ;
#50091 = ORIENTED_EDGE('',*,*,#37705,.T.) ;
#50092 = ORIENTED_EDGE('',*,*,#37706,.T.) ;
#50093 = ORIENTED_EDGE('',*,*,#37707,.F.) ;
#50094 = ORIENTED_EDGE('',*,*,#37708,.F.) ;
#50095 = ORIENTED_EDGE('',*,*,#37709,.T.) ;
#50096 = ORIENTED_EDGE('',*,*,#37710,.T.) ;
#50097 = ORIENTED_EDGE('',*,*,#37711,.F.) ;
#50098 = ORIENTED_EDGE('',*,*,#37712,.F.) ;
#50099 = ORIENTED_EDGE('',*,*,#37713,.F.) ;
#50100 = ORIENTED_EDGE('',*,*,#37714,.F.) ;
#50101 = ORIENTED_EDGE('',*,*,#37715,.T.) ;
#50102 = ORIENTED_EDGE('',*,*,#37716,.F.) ;
#50103 = ORIENTED_EDGE('',*,*,#37715,.F.) ;
#50104 = ORIENTED_EDGE('',*,*,#37717,.F.) ;
#50105 = ORIENTED_EDGE('',*,*,#37718,.T.) ;
#50106 = ORIENTED_EDGE('',*,*,#37719,.F.) ;
#50107 = ORIENTED_EDGE('',*,*,#37718,.F.) ;
#50108 = ORIENTED_EDGE('',*,*,#37720,.F.) ;
#50109 = ORIENTED_EDGE('',*,*,#37721,.F.) ;
#50110 = ORIENTED_EDGE('',*,*,#37722,.T.) ;
#50111 = ORIENTED_EDGE('',*,*,#37723,.T.) ;
#50112 = ORIENTED_EDGE('',*,*,#37724,.F.) ;
#50113 = ORIENTED_EDGE('',*,*,#37725,.F.) ;
#50114 = ORIENTED_EDGE('',*,*,#37726,.F.) ;
#50115 = ORIENTED_EDGE('',*,*,#37727,.T.) ;
#50116 = ORIENTED_EDGE('',*,*,#37728,.F.) ;
#50117 = ORIENTED_EDGE('',*,*,#37729,.F.) ;
#50118 = ORIENTED_EDGE('',*,*,#37730,.T.) ;
#50119 = ORIENTED_EDGE('',*,*,#37731,.F.) ;
#50120 = ORIENTED_EDGE('',*,*,#37732,.T.) ;
#50121 = ORIENTED_EDGE('',*,*,#37716,.T.) ;
#50122 = ORIENTED_EDGE('',*,*,#37733,.T.) ;
#50123 = ORIENTED_EDGE('',*,*,#37717,.T.) ;
#50124 = ORIENTED_EDGE('',*,*,#37733,.F.) ;
#50125 = ORIENTED_EDGE('',*,*,#37729,.T.) ;
#50126 = ORIENTED_EDGE('',*,*,#37734,.T.) ;
#50127 = ORIENTED_EDGE('',*,*,#37735,.T.) ;
#50128 = ORIENTED_EDGE('',*,*,#37726,.T.) ;
#50129 = ORIENTED_EDGE('',*,*,#37736,.F.) ;
#50130 = ORIENTED_EDGE('',*,*,#37737,.T.) ;
#50131 = ORIENTED_EDGE('',*,*,#37738,.F.) ;
#50132 = ORIENTED_EDGE('',*,*,#37724,.T.) ;
#50133 = ORIENTED_EDGE('',*,*,#37739,.T.) ;
#50134 = ORIENTED_EDGE('',*,*,#37740,.T.) ;
#50135 = ORIENTED_EDGE('',*,*,#37741,.T.) ;
#50136 = ORIENTED_EDGE('',*,*,#37742,.T.) ;
#50137 = ORIENTED_EDGE('',*,*,#37743,.T.) ;
#50138 = ORIENTED_EDGE('',*,*,#37744,.T.) ;
#50139 = ORIENTED_EDGE('',*,*,#37745,.T.) ;
#50140 = ORIENTED_EDGE('',*,*,#37746,.T.) ;
#50141 = ORIENTED_EDGE('',*,*,#37747,.T.) ;
#50142 = ORIENTED_EDGE('',*,*,#37748,.T.) ;
#50143 = ORIENTED_EDGE('',*,*,#37749,.T.) ;
#50144 = ORIENTED_EDGE('',*,*,#37750,.T.) ;
#50145 = ORIENTED_EDGE('',*,*,#37751,.T.) ;
#50146 = ORIENTED_EDGE('',*,*,#37752,.T.) ;
#50147 = ORIENTED_EDGE('',*,*,#37753,.T.) ;
#50148 = ORIENTED_EDGE('',*,*,#37754,.T.) ;
#50149 = ORIENTED_EDGE('',*,*,#37755,.T.) ;
#50150 = ORIENTED_EDGE('',*,*,#37756,.T.) ;
#50151 = ORIENTED_EDGE('',*,*,#37757,.T.) ;
#50152 = ORIENTED_EDGE('',*,*,#37758,.T.) ;
#50153 = ORIENTED_EDGE('',*,*,#37759,.T.) ;
#50154 = ORIENTED_EDGE('',*,*,#37760,.T.) ;
#50155 = ORIENTED_EDGE('',*,*,#37761,.T.) ;
#50156 = ORIENTED_EDGE('',*,*,#37762,.T.) ;
#50157 = ORIENTED_EDGE('',*,*,#37763,.T.) ;
#50158 = ORIENTED_EDGE('',*,*,#37764,.T.) ;
#50159 = ORIENTED_EDGE('',*,*,#37765,.T.) ;
#50160 = ORIENTED_EDGE('',*,*,#37766,.T.) ;
#50161 = ORIENTED_EDGE('',*,*,#37767,.F.) ;
#50162 = ORIENTED_EDGE('',*,*,#37768,.T.) ;
#50163 = ORIENTED_EDGE('',*,*,#37769,.T.) ;
#50164 = ORIENTED_EDGE('',*,*,#37770,.T.) ;
#50165 = ORIENTED_EDGE('',*,*,#37771,.F.) ;
#50166 = ORIENTED_EDGE('',*,*,#37772,.T.) ;
#50167 = ORIENTED_EDGE('',*,*,#37773,.T.) ;
#50168 = ORIENTED_EDGE('',*,*,#37774,.T.) ;
#50169 = ORIENTED_EDGE('',*,*,#37775,.T.) ;
#50170 = ORIENTED_EDGE('',*,*,#37776,.T.) ;
#50171 = ORIENTED_EDGE('',*,*,#37777,.F.) ;
#50172 = ORIENTED_EDGE('',*,*,#37778,.T.) ;
#50173 = ORIENTED_EDGE('',*,*,#37747,.F.) ;
#50174 = ORIENTED_EDGE('',*,*,#37779,.T.) ;
#50175 = ORIENTED_EDGE('',*,*,#37753,.F.) ;
#50176 = ORIENTED_EDGE('',*,*,#37780,.T.) ;
#50177 = ORIENTED_EDGE('',*,*,#37761,.F.) ;
#50178 = ORIENTED_EDGE('',*,*,#37781,.T.) ;
#50179 = ORIENTED_EDGE('',*,*,#37782,.F.) ;
#50180 = ORIENTED_EDGE('',*,*,#37783,.T.) ;
#50181 = ORIENTED_EDGE('',*,*,#37784,.F.) ;
#50182 = ORIENTED_EDGE('',*,*,#37785,.T.) ;
#50183 = ORIENTED_EDGE('',*,*,#37786,.T.) ;
#50184 = ORIENTED_EDGE('',*,*,#37787,.T.) ;
#50185 = ORIENTED_EDGE('',*,*,#37788,.F.) ;
#50186 = ORIENTED_EDGE('',*,*,#37789,.T.) ;
#50187 = ORIENTED_EDGE('',*,*,#37790,.T.) ;
#50188 = ORIENTED_EDGE('',*,*,#37791,.T.) ;
#50189 = ORIENTED_EDGE('',*,*,#37792,.F.) ;
#50190 = ORIENTED_EDGE('',*,*,#37793,.T.) ;
#50191 = ORIENTED_EDGE('',*,*,#37765,.F.) ;
#50192 = ORIENTED_EDGE('',*,*,#37794,.T.) ;
#50193 = ORIENTED_EDGE('',*,*,#37795,.T.) ;
#50194 = ORIENTED_EDGE('',*,*,#37796,.T.) ;
#50195 = ORIENTED_EDGE('',*,*,#37773,.F.) ;
#50196 = ORIENTED_EDGE('',*,*,#37797,.T.) ;
#50197 = ORIENTED_EDGE('',*,*,#37798,.F.) ;
#50198 = ORIENTED_EDGE('',*,*,#37799,.F.) ;
#50199 = ORIENTED_EDGE('',*,*,#37800,.T.) ;
#50200 = ORIENTED_EDGE('',*,*,#37801,.F.) ;
#50201 = ORIENTED_EDGE('',*,*,#37802,.T.) ;
#50202 = ORIENTED_EDGE('',*,*,#37803,.F.) ;
#50203 = ORIENTED_EDGE('',*,*,#37804,.T.) ;
#50204 = ORIENTED_EDGE('',*,*,#37805,.T.) ;
#50205 = ORIENTED_EDGE('',*,*,#37806,.T.) ;
#50206 = ORIENTED_EDGE('',*,*,#37807,.T.) ;
#50207 = ORIENTED_EDGE('',*,*,#37808,.T.) ;
#50208 = ORIENTED_EDGE('',*,*,#37809,.T.) ;
#50209 = ORIENTED_EDGE('',*,*,#37810,.T.) ;
#50210 = ORIENTED_EDGE('',*,*,#37811,.T.) ;
#50211 = ORIENTED_EDGE('',*,*,#37812,.T.) ;
#50212 = ORIENTED_EDGE('',*,*,#37813,.T.) ;
#50213 = ORIENTED_EDGE('',*,*,#37814,.T.) ;
#50214 = ORIENTED_EDGE('',*,*,#37815,.T.) ;
#50215 = ORIENTED_EDGE('',*,*,#37771,.T.) ;
#50216 = ORIENTED_EDGE('',*,*,#37816,.T.) ;
#50217 = ORIENTED_EDGE('',*,*,#37817,.T.) ;
#50218 = ORIENTED_EDGE('',*,*,#37818,.T.) ;
#50219 = ORIENTED_EDGE('',*,*,#37767,.T.) ;
#50220 = ORIENTED_EDGE('',*,*,#37819,.T.) ;
#50221 = ORIENTED_EDGE('',*,*,#37820,.F.) ;
#50222 = ORIENTED_EDGE('',*,*,#37821,.T.) ;
#50223 = ORIENTED_EDGE('',*,*,#37822,.F.) ;
#50224 = ORIENTED_EDGE('',*,*,#37823,.T.) ;
#50225 = ORIENTED_EDGE('',*,*,#37824,.T.) ;
#50226 = ORIENTED_EDGE('',*,*,#37825,.T.) ;
#50227 = ORIENTED_EDGE('',*,*,#37826,.F.) ;
#50228 = ORIENTED_EDGE('',*,*,#37827,.T.) ;
#50229 = ORIENTED_EDGE('',*,*,#37828,.F.) ;
#50230 = ORIENTED_EDGE('',*,*,#37829,.T.) ;
#50231 = ORIENTED_EDGE('',*,*,#37830,.T.) ;
#50232 = ORIENTED_EDGE('',*,*,#37831,.T.) ;
#50233 = ORIENTED_EDGE('',*,*,#37832,.T.) ;
#50234 = ORIENTED_EDGE('',*,*,#37833,.T.) ;
#50235 = ORIENTED_EDGE('',*,*,#37834,.T.) ;
#50236 = ORIENTED_EDGE('',*,*,#37835,.T.) ;
#50237 = ORIENTED_EDGE('',*,*,#37801,.T.) ;
#50238 = ORIENTED_EDGE('',*,*,#37836,.T.) ;
#50239 = ORIENTED_EDGE('',*,*,#37811,.F.) ;
#50240 = ORIENTED_EDGE('',*,*,#37837,.T.) ;
#50241 = ORIENTED_EDGE('',*,*,#37803,.T.) ;
#50242 = ORIENTED_EDGE('',*,*,#37838,.T.) ;
#50243 = ORIENTED_EDGE('',*,*,#37809,.F.) ;
#50244 = ORIENTED_EDGE('',*,*,#37839,.T.) ;
#50245 = ORIENTED_EDGE('',*,*,#37840,.T.) ;
#50246 = ORIENTED_EDGE('',*,*,#37841,.T.) ;
#50247 = ORIENTED_EDGE('',*,*,#37777,.T.) ;
#50248 = ORIENTED_EDGE('',*,*,#37842,.T.) ;
#50249 = ORIENTED_EDGE('',*,*,#37807,.F.) ;
#50250 = ORIENTED_EDGE('',*,*,#37843,.T.) ;
#50251 = ORIENTED_EDGE('',*,*,#37844,.T.) ;
#50252 = ORIENTED_EDGE('',*,*,#37845,.T.) ;
#50253 = ORIENTED_EDGE('',*,*,#37846,.T.) ;
#50254 = ORIENTED_EDGE('',*,*,#37847,.T.) ;
#50255 = ORIENTED_EDGE('',*,*,#37848,.T.) ;
#50256 = ORIENTED_EDGE('',*,*,#37805,.F.) ;
#50257 = ORIENTED_EDGE('',*,*,#37849,.T.) ;
#50258 = ORIENTED_EDGE('',*,*,#37850,.T.) ;
#50259 = ORIENTED_EDGE('',*,*,#37851,.T.) ;
#50260 = ORIENTED_EDGE('',*,*,#37852,.T.) ;
#50261 = ORIENTED_EDGE('',*,*,#37834,.F.) ;
#50262 = ORIENTED_EDGE('',*,*,#37853,.T.) ;
#50263 = ORIENTED_EDGE('',*,*,#37854,.T.) ;
#50264 = ORIENTED_EDGE('',*,*,#37708,.T.) ;
#50265 = ORIENTED_EDGE('',*,*,#37855,.T.) ;
#50266 = ORIENTED_EDGE('',*,*,#37856,.T.) ;
#50267 = ORIENTED_EDGE('',*,*,#37832,.F.) ;
#50268 = ORIENTED_EDGE('',*,*,#37857,.T.) ;
#50269 = ORIENTED_EDGE('',*,*,#37858,.T.) ;
#50270 = ORIENTED_EDGE('',*,*,#37859,.T.) ;
#50271 = ORIENTED_EDGE('',*,*,#37860,.T.) ;
#50272 = ORIENTED_EDGE('',*,*,#37861,.T.) ;
#50273 = ORIENTED_EDGE('',*,*,#37862,.T.) ;
#50274 = ORIENTED_EDGE('',*,*,#37830,.F.) ;
#50275 = ORIENTED_EDGE('',*,*,#37863,.T.) ;
#50276 = ORIENTED_EDGE('',*,*,#37864,.T.) ;
#50277 = ORIENTED_EDGE('',*,*,#37865,.F.) ;
#50278 = ORIENTED_EDGE('',*,*,#37866,.T.) ;
#50279 = ORIENTED_EDGE('',*,*,#37867,.F.) ;
#50280 = ORIENTED_EDGE('',*,*,#37868,.T.) ;
#50281 = ORIENTED_EDGE('',*,*,#37869,.T.) ;
#50282 = ORIENTED_EDGE('',*,*,#37782,.T.) ;
#50283 = ORIENTED_EDGE('',*,*,#37870,.F.) ;
#50284 = ORIENTED_EDGE('',*,*,#37871,.T.) ;
#50285 = ORIENTED_EDGE('',*,*,#37788,.T.) ;
#50286 = ORIENTED_EDGE('',*,*,#37872,.T.) ;
#50287 = ORIENTED_EDGE('',*,*,#37873,.F.) ;
#50288 = ORIENTED_EDGE('',*,*,#37874,.T.) ;
#50289 = ORIENTED_EDGE('',*,*,#37875,.F.) ;
#50290 = ORIENTED_EDGE('',*,*,#37876,.T.) ;
#50291 = ORIENTED_EDGE('',*,*,#37877,.T.) ;
#50292 = ORIENTED_EDGE('',*,*,#37878,.T.) ;
#50293 = ORIENTED_EDGE('',*,*,#37879,.F.) ;
#50294 = ORIENTED_EDGE('',*,*,#37880,.T.) ;
#50295 = ORIENTED_EDGE('',*,*,#37881,.F.) ;
#50296 = ORIENTED_EDGE('',*,*,#37882,.T.) ;
#50297 = ORIENTED_EDGE('',*,*,#37824,.F.) ;
#50298 = ORIENTED_EDGE('',*,*,#37883,.T.) ;
#50299 = ORIENTED_EDGE('',*,*,#37884,.F.) ;
#50300 = ORIENTED_EDGE('',*,*,#37885,.T.) ;
#50301 = ORIENTED_EDGE('',*,*,#37886,.F.) ;
#50302 = ORIENTED_EDGE('',*,*,#37887,.T.) ;
#50303 = ORIENTED_EDGE('',*,*,#37888,.T.) ;
#50304 = ORIENTED_EDGE('',*,*,#37889,.T.) ;
#50305 = ORIENTED_EDGE('',*,*,#37890,.F.) ;
#50306 = ORIENTED_EDGE('',*,*,#37891,.T.) ;
#50307 = ORIENTED_EDGE('',*,*,#37719,.T.) ;
#50308 = ORIENTED_EDGE('',*,*,#37892,.F.) ;
#50309 = ORIENTED_EDGE('',*,*,#37893,.T.) ;
#50310 = ORIENTED_EDGE('',*,*,#37894,.F.) ;
#50311 = ORIENTED_EDGE('',*,*,#37798,.T.) ;
#50312 = ORIENTED_EDGE('',*,*,#37895,.T.) ;
#50313 = ORIENTED_EDGE('',*,*,#37814,.F.) ;
#50314 = ORIENTED_EDGE('',*,*,#37896,.F.) ;
#50315 = ORIENTED_EDGE('',*,*,#37897,.T.) ;
#50316 = ORIENTED_EDGE('',*,*,#37898,.F.) ;
#50317 = ORIENTED_EDGE('',*,*,#37899,.T.) ;
#50318 = ORIENTED_EDGE('',*,*,#37900,.F.) ;
#50319 = ORIENTED_EDGE('',*,*,#37901,.T.) ;
#50320 = ORIENTED_EDGE('',*,*,#37896,.T.) ;
#50321 = ORIENTED_EDGE('',*,*,#37813,.F.) ;
#50322 = ORIENTED_EDGE('',*,*,#37902,.T.) ;
#50323 = ORIENTED_EDGE('',*,*,#37799,.T.) ;
#50324 = ORIENTED_EDGE('',*,*,#37894,.T.) ;
#50325 = ORIENTED_EDGE('',*,*,#37903,.T.) ;
#50326 = ORIENTED_EDGE('',*,*,#37904,.F.) ;
#50327 = ORIENTED_EDGE('',*,*,#37905,.T.) ;
#50328 = ORIENTED_EDGE('',*,*,#37906,.T.) ;
#50329 = ORIENTED_EDGE('',*,*,#37907,.T.) ;
#50330 = ORIENTED_EDGE('',*,*,#37908,.F.) ;
#50331 = ORIENTED_EDGE('',*,*,#37909,.F.) ;
#50332 = ORIENTED_EDGE('',*,*,#37910,.T.) ;
#50333 = ORIENTED_EDGE('',*,*,#37911,.T.) ;
#50334 = ORIENTED_EDGE('',*,*,#37912,.T.) ;
#50335 = ORIENTED_EDGE('',*,*,#37913,.T.) ;
#50336 = ORIENTED_EDGE('',*,*,#37914,.T.) ;
#50337 = ORIENTED_EDGE('',*,*,#37915,.T.) ;
#50338 = ORIENTED_EDGE('',*,*,#37916,.T.) ;
#50339 = ORIENTED_EDGE('',*,*,#37917,.T.) ;
#50340 = ORIENTED_EDGE('',*,*,#37918,.T.) ;
#50341 = ORIENTED_EDGE('',*,*,#37919,.T.) ;
#50342 = ORIENTED_EDGE('',*,*,#37920,.T.) ;
#50343 = ORIENTED_EDGE('',*,*,#37921,.T.) ;
#50344 = ORIENTED_EDGE('',*,*,#37922,.T.) ;
#50345 = ORIENTED_EDGE('',*,*,#37923,.T.) ;
#50346 = ORIENTED_EDGE('',*,*,#37924,.T.) ;
#50347 = ORIENTED_EDGE('',*,*,#37925,.T.) ;
#50348 = ORIENTED_EDGE('',*,*,#37926,.T.) ;
#50349 = ORIENTED_EDGE('',*,*,#37927,.T.) ;
#50350 = ORIENTED_EDGE('',*,*,#37928,.T.) ;
#50351 = ORIENTED_EDGE('',*,*,#37929,.T.) ;
#50352 = ORIENTED_EDGE('',*,*,#37930,.T.) ;
#50353 = ORIENTED_EDGE('',*,*,#37931,.T.) ;
#50354 = ORIENTED_EDGE('',*,*,#37932,.T.) ;
#50355 = ORIENTED_EDGE('',*,*,#37933,.T.) ;
#50356 = ORIENTED_EDGE('',*,*,#37934,.T.) ;
#50357 = ORIENTED_EDGE('',*,*,#37935,.T.) ;
#50358 = ORIENTED_EDGE('',*,*,#37936,.T.) ;
#50359 = ORIENTED_EDGE('',*,*,#37937,.T.) ;
#50360 = ORIENTED_EDGE('',*,*,#37938,.T.) ;
#50361 = ORIENTED_EDGE('',*,*,#37939,.T.) ;
#50362 = ORIENTED_EDGE('',*,*,#37940,.T.) ;
#50363 = ORIENTED_EDGE('',*,*,#37941,.T.) ;
#50364 = ORIENTED_EDGE('',*,*,#37942,.T.) ;
#50365 = ORIENTED_EDGE('',*,*,#37943,.T.) ;
#50366 = ORIENTED_EDGE('',*,*,#37944,.T.) ;
#50367 = ORIENTED_EDGE('',*,*,#37945,.T.) ;
#50368 = ORIENTED_EDGE('',*,*,#37714,.T.) ;
#50369 = ORIENTED_EDGE('',*,*,#37946,.F.) ;
#50370 = ORIENTED_EDGE('',*,*,#37947,.T.) ;
#50371 = ORIENTED_EDGE('',*,*,#37948,.T.) ;
#50372 = ORIENTED_EDGE('',*,*,#37949,.T.) ;
#50373 = ORIENTED_EDGE('',*,*,#37950,.T.) ;
#50374 = ORIENTED_EDGE('',*,*,#37951,.T.) ;
#50375 = ORIENTED_EDGE('',*,*,#37952,.T.) ;
#50376 = ORIENTED_EDGE('',*,*,#37953,.T.) ;
#50377 = ORIENTED_EDGE('',*,*,#37954,.F.) ;
#50378 = ORIENTED_EDGE('',*,*,#37955,.T.) ;
#50379 = ORIENTED_EDGE('',*,*,#37792,.T.) ;
#50380 = ORIENTED_EDGE('',*,*,#37956,.T.) ;
#50381 = ORIENTED_EDGE('',*,*,#37957,.T.) ;
#50382 = ORIENTED_EDGE('',*,*,#37958,.T.) ;
#50383 = ORIENTED_EDGE('',*,*,#37959,.T.) ;
#50384 = ORIENTED_EDGE('',*,*,#37790,.F.) ;
#50385 = ORIENTED_EDGE('',*,*,#37960,.T.) ;
#50386 = ORIENTED_EDGE('',*,*,#37961,.T.) ;
#50387 = ORIENTED_EDGE('',*,*,#37962,.T.) ;
#50388 = ORIENTED_EDGE('',*,*,#37963,.T.) ;
#50389 = ORIENTED_EDGE('',*,*,#37964,.T.) ;
#50390 = ORIENTED_EDGE('',*,*,#37728,.T.) ;
#50391 = ORIENTED_EDGE('',*,*,#37965,.T.) ;
#50392 = ORIENTED_EDGE('',*,*,#37966,.T.) ;
#50393 = ORIENTED_EDGE('',*,*,#37967,.T.) ;
#50394 = ORIENTED_EDGE('',*,*,#37968,.T.) ;
#50395 = ORIENTED_EDGE('',*,*,#37969,.T.) ;
#50396 = ORIENTED_EDGE('',*,*,#37970,.T.) ;
#50397 = ORIENTED_EDGE('',*,*,#37971,.T.) ;
#50398 = ORIENTED_EDGE('',*,*,#37972,.T.) ;
#50399 = ORIENTED_EDGE('',*,*,#37973,.T.) ;
#50400 = ORIENTED_EDGE('',*,*,#37721,.T.) ;
#50401 = ORIENTED_EDGE('',*,*,#37974,.T.) ;
#50402 = ORIENTED_EDGE('',*,*,#37975,.T.) ;
#50403 = ORIENTED_EDGE('',*,*,#37976,.T.) ;
#50404 = ORIENTED_EDGE('',*,*,#37977,.T.) ;
#50405 = ORIENTED_EDGE('',*,*,#37978,.T.) ;
#50406 = ORIENTED_EDGE('',*,*,#37822,.T.) ;
#50407 = ORIENTED_EDGE('',*,*,#37979,.T.) ;
#50408 = ORIENTED_EDGE('',*,*,#37980,.T.) ;
#50409 = ORIENTED_EDGE('',*,*,#37981,.T.) ;
#50410 = ORIENTED_EDGE('',*,*,#37820,.T.) ;
#50411 = ORIENTED_EDGE('',*,*,#37982,.T.) ;
#50412 = ORIENTED_EDGE('',*,*,#37983,.F.) ;
#50413 = ORIENTED_EDGE('',*,*,#37984,.T.) ;
#50414 = ORIENTED_EDGE('',*,*,#37985,.T.) ;
#50415 = ORIENTED_EDGE('',*,*,#37986,.T.) ;
#50416 = ORIENTED_EDGE('',*,*,#37987,.T.) ;
#50417 = ORIENTED_EDGE('',*,*,#37784,.T.) ;
#50418 = ORIENTED_EDGE('',*,*,#37988,.T.) ;
#50419 = ORIENTED_EDGE('',*,*,#37989,.T.) ;
#50420 = ORIENTED_EDGE('',*,*,#37990,.T.) ;
#50421 = ORIENTED_EDGE('',*,*,#37991,.T.) ;
#50422 = ORIENTED_EDGE('',*,*,#37786,.F.) ;
#50423 = ORIENTED_EDGE('',*,*,#37992,.T.) ;
#50424 = ORIENTED_EDGE('',*,*,#37993,.T.) ;
#50425 = ORIENTED_EDGE('',*,*,#37994,.T.) ;
#50426 = ORIENTED_EDGE('',*,*,#37995,.T.) ;
#50427 = ORIENTED_EDGE('',*,*,#37996,.T.) ;
#50428 = ORIENTED_EDGE('',*,*,#37997,.T.) ;
#50429 = ORIENTED_EDGE('',*,*,#37998,.T.) ;
#50430 = ORIENTED_EDGE('',*,*,#37999,.T.) ;
#50431 = ORIENTED_EDGE('',*,*,#38000,.T.) ;
#50432 = ORIENTED_EDGE('',*,*,#38001,.T.) ;
#50433 = ORIENTED_EDGE('',*,*,#38002,.T.) ;
#50434 = ORIENTED_EDGE('',*,*,#38003,.T.) ;
#50435 = ORIENTED_EDGE('',*,*,#38004,.T.) ;
#50436 = ORIENTED_EDGE('',*,*,#37826,.T.) ;
#50437 = ORIENTED_EDGE('',*,*,#38005,.T.) ;
#50438 = ORIENTED_EDGE('',*,*,#38006,.T.) ;
#50439 = ORIENTED_EDGE('',*,*,#38007,.T.) ;
#50440 = ORIENTED_EDGE('',*,*,#38008,.T.) ;
#50441 = ORIENTED_EDGE('',*,*,#38009,.T.) ;
#50442 = ORIENTED_EDGE('',*,*,#38010,.T.) ;
#50443 = ORIENTED_EDGE('',*,*,#38011,.T.) ;
#50444 = ORIENTED_EDGE('',*,*,#38012,.T.) ;
#50445 = ORIENTED_EDGE('',*,*,#38013,.T.) ;
#50446 = ORIENTED_EDGE('',*,*,#37828,.T.) ;
#50447 = ORIENTED_EDGE('',*,*,#38014,.T.) ;
#50448 = ORIENTED_EDGE('',*,*,#38015,.T.) ;
#50449 = ORIENTED_EDGE('',*,*,#38016,.T.) ;
#50450 = ORIENTED_EDGE('',*,*,#38017,.T.) ;
#50451 = ORIENTED_EDGE('',*,*,#38018,.T.) ;
#50452 = ORIENTED_EDGE('',*,*,#38019,.T.) ;
#50453 = ORIENTED_EDGE('',*,*,#38020,.T.) ;
#50454 = ORIENTED_EDGE('',*,*,#38021,.T.) ;
#50455 = ORIENTED_EDGE('',*,*,#37713,.T.) ;
#50456 = ORIENTED_EDGE('',*,*,#38022,.T.) ;
#50457 = ORIENTED_EDGE('',*,*,#38023,.T.) ;
#50458 = ORIENTED_EDGE('',*,*,#38024,.T.) ;
#50459 = ORIENTED_EDGE('',*,*,#38025,.T.) ;
#50460 = ORIENTED_EDGE('',*,*,#38026,.T.) ;
#50461 = ORIENTED_EDGE('',*,*,#38027,.T.) ;
#50462 = ORIENTED_EDGE('',*,*,#38028,.T.) ;
#50463 = ORIENTED_EDGE('',*,*,#38029,.T.) ;
#50464 = ORIENTED_EDGE('',*,*,#38030,.T.) ;
#50465 = ORIENTED_EDGE('',*,*,#38031,.T.) ;
#50466 = ORIENTED_EDGE('',*,*,#38032,.T.) ;
#50467 = ORIENTED_EDGE('',*,*,#38033,.T.) ;
#50468 = ORIENTED_EDGE('',*,*,#38034,.T.) ;
#50469 = ORIENTED_EDGE('',*,*,#38035,.T.) ;
#50470 = ORIENTED_EDGE('',*,*,#38036,.T.) ;
#50471 = ORIENTED_EDGE('',*,*,#38037,.T.) ;
#50472 = ORIENTED_EDGE('',*,*,#38038,.T.) ;
#50473 = ORIENTED_EDGE('',*,*,#38039,.T.) ;
#50474 = ORIENTED_EDGE('',*,*,#38040,.T.) ;
#50475 = ORIENTED_EDGE('',*,*,#38041,.T.) ;
#50476 = ORIENTED_EDGE('',*,*,#38042,.T.) ;
#50477 = ORIENTED_EDGE('',*,*,#38043,.T.) ;
#50478 = ORIENTED_EDGE('',*,*,#38044,.T.) ;
#50479 = ORIENTED_EDGE('',*,*,#38045,.T.) ;
#50480 = ORIENTED_EDGE('',*,*,#37946,.T.) ;
#50481 = ORIENTED_EDGE('',*,*,#38046,.T.) ;
#50482 = ORIENTED_EDGE('',*,*,#38047,.T.) ;
#50483 = ORIENTED_EDGE('',*,*,#38048,.T.) ;
#50484 = ORIENTED_EDGE('',*,*,#37950,.F.) ;
#50485 = ORIENTED_EDGE('',*,*,#38049,.T.) ;
#50486 = ORIENTED_EDGE('',*,*,#38050,.T.) ;
#50487 = ORIENTED_EDGE('',*,*,#38051,.T.) ;
#50488 = ORIENTED_EDGE('',*,*,#37952,.F.) ;
#50489 = ORIENTED_EDGE('',*,*,#38052,.T.) ;
#50490 = ORIENTED_EDGE('',*,*,#38053,.T.) ;
#50491 = ORIENTED_EDGE('',*,*,#38054,.T.) ;
#50492 = ORIENTED_EDGE('',*,*,#37948,.F.) ;
#50493 = ORIENTED_EDGE('',*,*,#38055,.T.) ;
#50494 = ORIENTED_EDGE('',*,*,#38056,.T.) ;
#50495 = ORIENTED_EDGE('',*,*,#38057,.T.) ;
#50496 = ORIENTED_EDGE('',*,*,#38058,.T.) ;
#50497 = ORIENTED_EDGE('',*,*,#38059,.T.) ;
#50498 = ORIENTED_EDGE('',*,*,#38060,.T.) ;
#50499 = ORIENTED_EDGE('',*,*,#38061,.T.) ;
#50500 = ORIENTED_EDGE('',*,*,#38062,.T.) ;
#50501 = ORIENTED_EDGE('',*,*,#38063,.T.) ;
#50502 = ORIENTED_EDGE('',*,*,#38064,.T.) ;
#50503 = ORIENTED_EDGE('',*,*,#38065,.T.) ;
#50504 = ORIENTED_EDGE('',*,*,#38066,.T.) ;
#50505 = ORIENTED_EDGE('',*,*,#38067,.F.) ;
#50506 = ORIENTED_EDGE('',*,*,#38068,.T.) ;
#50507 = ORIENTED_EDGE('',*,*,#37744,.F.) ;
#50508 = ORIENTED_EDGE('',*,*,#38069,.T.) ;
#50509 = ORIENTED_EDGE('',*,*,#38070,.T.) ;
#50510 = ORIENTED_EDGE('',*,*,#38071,.T.) ;
#50511 = ORIENTED_EDGE('',*,*,#38072,.T.) ;
#50512 = ORIENTED_EDGE('',*,*,#38067,.T.) ;
#50513 = ORIENTED_EDGE('',*,*,#38073,.T.) ;
#50514 = ORIENTED_EDGE('',*,*,#38074,.T.) ;
#50515 = ORIENTED_EDGE('',*,*,#38075,.T.) ;
#50516 = ORIENTED_EDGE('',*,*,#38076,.T.) ;
#50517 = ORIENTED_EDGE('',*,*,#38077,.T.) ;
#50518 = ORIENTED_EDGE('',*,*,#38078,.T.) ;
#50519 = ORIENTED_EDGE('',*,*,#38079,.T.) ;
#50520 = ORIENTED_EDGE('',*,*,#38080,.T.) ;
#50521 = ORIENTED_EDGE('',*,*,#38081,.T.) ;
#50522 = ORIENTED_EDGE('',*,*,#38082,.T.) ;
#50523 = ORIENTED_EDGE('',*,*,#38083,.T.) ;
#50524 = ORIENTED_EDGE('',*,*,#38084,.T.) ;
#50525 = ORIENTED_EDGE('',*,*,#38085,.T.) ;
#50526 = ORIENTED_EDGE('',*,*,#38086,.T.) ;
#50527 = ORIENTED_EDGE('',*,*,#38087,.T.) ;
#50528 = ORIENTED_EDGE('',*,*,#38088,.F.) ;
#50529 = ORIENTED_EDGE('',*,*,#37937,.F.) ;
#50530 = ORIENTED_EDGE('',*,*,#38089,.T.) ;
#50531 = ORIENTED_EDGE('',*,*,#38088,.T.) ;
#50532 = ORIENTED_EDGE('',*,*,#38090,.T.) ;
#50533 = ORIENTED_EDGE('',*,*,#38091,.T.) ;
#50534 = ORIENTED_EDGE('',*,*,#38092,.T.) ;
#50535 = ORIENTED_EDGE('',*,*,#38093,.T.) ;
#50536 = ORIENTED_EDGE('',*,*,#38094,.T.) ;
#50537 = ORIENTED_EDGE('',*,*,#38095,.T.) ;
#50538 = ORIENTED_EDGE('',*,*,#38096,.T.) ;
#50539 = ORIENTED_EDGE('',*,*,#38097,.T.) ;
#50540 = ORIENTED_EDGE('',*,*,#38098,.T.) ;
#50541 = ORIENTED_EDGE('',*,*,#38099,.T.) ;
#50542 = ORIENTED_EDGE('',*,*,#38100,.T.) ;
#50543 = ORIENTED_EDGE('',*,*,#38101,.T.) ;
#50544 = ORIENTED_EDGE('',*,*,#38102,.T.) ;
#50545 = ORIENTED_EDGE('',*,*,#38103,.T.) ;
#50546 = ORIENTED_EDGE('',*,*,#38104,.T.) ;
#50547 = ORIENTED_EDGE('',*,*,#38105,.T.) ;
#50548 = ORIENTED_EDGE('',*,*,#38106,.T.) ;
#50549 = ORIENTED_EDGE('',*,*,#38107,.T.) ;
#50550 = ORIENTED_EDGE('',*,*,#38108,.T.) ;
#50551 = ORIENTED_EDGE('',*,*,#38109,.T.) ;
#50552 = ORIENTED_EDGE('',*,*,#37817,.F.) ;
#50553 = ORIENTED_EDGE('',*,*,#38110,.T.) ;
#50554 = ORIENTED_EDGE('',*,*,#38111,.T.) ;
#50555 = ORIENTED_EDGE('',*,*,#37731,.T.) ;
#50556 = ORIENTED_EDGE('',*,*,#38112,.T.) ;
#50557 = ORIENTED_EDGE('',*,*,#37795,.F.) ;
#50558 = ORIENTED_EDGE('',*,*,#38113,.T.) ;
#50559 = ORIENTED_EDGE('',*,*,#38114,.T.) ;
#50560 = ORIENTED_EDGE('',*,*,#38115,.T.) ;
#50561 = ORIENTED_EDGE('',*,*,#38116,.F.) ;
#50562 = ORIENTED_EDGE('',*,*,#38014,.F.) ;
#50563 = ORIENTED_EDGE('',*,*,#37827,.F.) ;
#50564 = ORIENTED_EDGE('',*,*,#38007,.F.) ;
#50565 = ORIENTED_EDGE('',*,*,#38117,.F.) ;
#50566 = ORIENTED_EDGE('',*,*,#38116,.T.) ;
#50567 = ORIENTED_EDGE('',*,*,#38118,.F.) ;
#50568 = ORIENTED_EDGE('',*,*,#37825,.F.) ;
#50569 = ORIENTED_EDGE('',*,*,#37882,.F.) ;
#50570 = ORIENTED_EDGE('',*,*,#38119,.F.) ;
#50571 = ORIENTED_EDGE('',*,*,#38005,.F.) ;
#50572 = ORIENTED_EDGE('',*,*,#38118,.T.) ;
#50573 = ORIENTED_EDGE('',*,*,#38006,.F.) ;
#50574 = ORIENTED_EDGE('',*,*,#38120,.F.) ;
#50575 = ORIENTED_EDGE('',*,*,#38002,.F.) ;
#50576 = ORIENTED_EDGE('',*,*,#38117,.T.) ;
#50577 = ORIENTED_EDGE('',*,*,#38001,.F.) ;
#50578 = ORIENTED_EDGE('',*,*,#38121,.F.) ;
#50579 = ORIENTED_EDGE('',*,*,#38015,.F.) ;
#50580 = ORIENTED_EDGE('',*,*,#38119,.T.) ;
#50581 = ORIENTED_EDGE('',*,*,#37881,.T.) ;
#50582 = ORIENTED_EDGE('',*,*,#38122,.F.) ;
#50583 = ORIENTED_EDGE('',*,*,#38120,.T.) ;
#50584 = ORIENTED_EDGE('',*,*,#38123,.F.) ;
#50585 = ORIENTED_EDGE('',*,*,#38121,.T.) ;
#50586 = ORIENTED_EDGE('',*,*,#38124,.F.) ;
#50587 = ORIENTED_EDGE('',*,*,#37785,.F.) ;
#50588 = ORIENTED_EDGE('',*,*,#37987,.F.) ;
#50589 = ORIENTED_EDGE('',*,*,#38125,.F.) ;
#50590 = ORIENTED_EDGE('',*,*,#37992,.F.) ;
#50591 = ORIENTED_EDGE('',*,*,#38126,.F.) ;
#50592 = ORIENTED_EDGE('',*,*,#37990,.F.) ;
#50593 = ORIENTED_EDGE('',*,*,#38127,.F.) ;
#50594 = ORIENTED_EDGE('',*,*,#37996,.F.) ;
#50595 = ORIENTED_EDGE('',*,*,#37787,.F.) ;
#50596 = ORIENTED_EDGE('',*,*,#37991,.F.) ;
#50597 = ORIENTED_EDGE('',*,*,#38128,.F.) ;
#50598 = ORIENTED_EDGE('',*,*,#37872,.F.) ;
#50599 = ORIENTED_EDGE('',*,*,#38122,.T.) ;
#50600 = ORIENTED_EDGE('',*,*,#37880,.F.) ;
#50601 = ORIENTED_EDGE('',*,*,#38129,.F.) ;
#50602 = ORIENTED_EDGE('',*,*,#38003,.F.) ;
#50603 = ORIENTED_EDGE('',*,*,#38124,.T.) ;
#50604 = ORIENTED_EDGE('',*,*,#38004,.F.) ;
#50605 = ORIENTED_EDGE('',*,*,#38130,.F.) ;
#50606 = ORIENTED_EDGE('',*,*,#38011,.F.) ;
#50607 = ORIENTED_EDGE('',*,*,#38123,.T.) ;
#50608 = ORIENTED_EDGE('',*,*,#38010,.F.) ;
#50609 = ORIENTED_EDGE('',*,*,#38131,.F.) ;
#50610 = ORIENTED_EDGE('',*,*,#38012,.F.) ;
#50611 = ORIENTED_EDGE('',*,*,#37829,.F.) ;
#50612 = ORIENTED_EDGE('',*,*,#38013,.F.) ;
#50613 = ORIENTED_EDGE('',*,*,#38132,.F.) ;
#50614 = ORIENTED_EDGE('',*,*,#37863,.F.) ;
#50615 = ORIENTED_EDGE('',*,*,#38127,.T.) ;
#50616 = ORIENTED_EDGE('',*,*,#38125,.T.) ;
#50617 = ORIENTED_EDGE('',*,*,#38133,.F.) ;
#50618 = ORIENTED_EDGE('',*,*,#38128,.T.) ;
#50619 = ORIENTED_EDGE('',*,*,#38126,.T.) ;
#50620 = ORIENTED_EDGE('',*,*,#38134,.F.) ;
#50621 = ORIENTED_EDGE('',*,*,#37873,.T.) ;
#50622 = ORIENTED_EDGE('',*,*,#38129,.T.) ;
#50623 = ORIENTED_EDGE('',*,*,#37879,.T.) ;
#50624 = ORIENTED_EDGE('',*,*,#38135,.F.) ;
#50625 = ORIENTED_EDGE('',*,*,#38130,.T.) ;
#50626 = ORIENTED_EDGE('',*,*,#38132,.T.) ;
#50627 = ORIENTED_EDGE('',*,*,#38131,.T.) ;
#50628 = ORIENTED_EDGE('',*,*,#38136,.F.) ;
#50629 = ORIENTED_EDGE('',*,*,#38133,.T.) ;
#50630 = ORIENTED_EDGE('',*,*,#37986,.F.) ;
#50631 = ORIENTED_EDGE('',*,*,#38137,.F.) ;
#50632 = ORIENTED_EDGE('',*,*,#37993,.F.) ;
#50633 = ORIENTED_EDGE('',*,*,#38138,.F.) ;
#50634 = ORIENTED_EDGE('',*,*,#37994,.F.) ;
#50635 = ORIENTED_EDGE('',*,*,#38139,.F.) ;
#50636 = ORIENTED_EDGE('',*,*,#38000,.F.) ;
#50637 = ORIENTED_EDGE('',*,*,#38134,.T.) ;
#50638 = ORIENTED_EDGE('',*,*,#37995,.F.) ;
#50639 = ORIENTED_EDGE('',*,*,#38140,.F.) ;
#50640 = ORIENTED_EDGE('',*,*,#37874,.F.) ;
#50641 = ORIENTED_EDGE('',*,*,#38135,.T.) ;
#50642 = ORIENTED_EDGE('',*,*,#37878,.F.) ;
#50643 = ORIENTED_EDGE('',*,*,#38141,.F.) ;
#50644 = ORIENTED_EDGE('',*,*,#38008,.F.) ;
#50645 = ORIENTED_EDGE('',*,*,#38136,.T.) ;
#50646 = ORIENTED_EDGE('',*,*,#38009,.F.) ;
#50647 = ORIENTED_EDGE('',*,*,#38142,.F.) ;
#50648 = ORIENTED_EDGE('',*,*,#37864,.F.) ;
#50649 = ORIENTED_EDGE('',*,*,#38139,.T.) ;
#50650 = ORIENTED_EDGE('',*,*,#38137,.T.) ;
#50651 = ORIENTED_EDGE('',*,*,#38143,.F.) ;
#50652 = ORIENTED_EDGE('',*,*,#38140,.T.) ;
#50653 = ORIENTED_EDGE('',*,*,#38138,.T.) ;
#50654 = ORIENTED_EDGE('',*,*,#38144,.F.) ;
#50655 = ORIENTED_EDGE('',*,*,#37875,.T.) ;
#50656 = ORIENTED_EDGE('',*,*,#38142,.T.) ;
#50657 = ORIENTED_EDGE('',*,*,#38141,.T.) ;
#50658 = ORIENTED_EDGE('',*,*,#38145,.F.) ;
#50659 = ORIENTED_EDGE('',*,*,#37865,.T.) ;
#50660 = ORIENTED_EDGE('',*,*,#37783,.F.) ;
#50661 = ORIENTED_EDGE('',*,*,#37869,.F.) ;
#50662 = ORIENTED_EDGE('',*,*,#38146,.F.) ;
#50663 = ORIENTED_EDGE('',*,*,#37988,.F.) ;
#50664 = ORIENTED_EDGE('',*,*,#38143,.T.) ;
#50665 = ORIENTED_EDGE('',*,*,#37989,.F.) ;
#50666 = ORIENTED_EDGE('',*,*,#38147,.F.) ;
#50667 = ORIENTED_EDGE('',*,*,#37997,.F.) ;
#50668 = ORIENTED_EDGE('',*,*,#38144,.T.) ;
#50669 = ORIENTED_EDGE('',*,*,#37999,.F.) ;
#50670 = ORIENTED_EDGE('',*,*,#38148,.F.) ;
#50671 = ORIENTED_EDGE('',*,*,#37876,.F.) ;
#50672 = ORIENTED_EDGE('',*,*,#38145,.T.) ;
#50673 = ORIENTED_EDGE('',*,*,#37877,.F.) ;
#50674 = ORIENTED_EDGE('',*,*,#38149,.F.) ;
#50675 = ORIENTED_EDGE('',*,*,#37866,.F.) ;
#50676 = ORIENTED_EDGE('',*,*,#38147,.T.) ;
#50677 = ORIENTED_EDGE('',*,*,#38146,.T.) ;
#50678 = ORIENTED_EDGE('',*,*,#38150,.F.) ;
#50679 = ORIENTED_EDGE('',*,*,#38149,.T.) ;
#50680 = ORIENTED_EDGE('',*,*,#38148,.T.) ;
#50681 = ORIENTED_EDGE('',*,*,#38151,.F.) ;
#50682 = ORIENTED_EDGE('',*,*,#37867,.T.) ;
#50683 = ORIENTED_EDGE('',*,*,#38150,.T.) ;
#50684 = ORIENTED_EDGE('',*,*,#37868,.F.) ;
#50685 = ORIENTED_EDGE('',*,*,#38151,.T.) ;
#50686 = ORIENTED_EDGE('',*,*,#37998,.F.) ;
#50687 = ORIENTED_EDGE('',*,*,#38152,.F.) ;
#50688 = ORIENTED_EDGE('',*,*,#38153,.F.) ;
#50689 = ORIENTED_EDGE('',*,*,#38154,.F.) ;
#50690 = ORIENTED_EDGE('',*,*,#37945,.F.) ;
#50691 = ORIENTED_EDGE('',*,*,#38155,.T.) ;
#50692 = ORIENTED_EDGE('',*,*,#38156,.T.) ;
#50693 = ORIENTED_EDGE('',*,*,#37927,.F.) ;
#50694 = ORIENTED_EDGE('',*,*,#38153,.T.) ;
#50695 = ORIENTED_EDGE('',*,*,#37926,.F.) ;
#50696 = ORIENTED_EDGE('',*,*,#38157,.T.) ;
#50697 = ORIENTED_EDGE('',*,*,#38158,.T.) ;
#50698 = ORIENTED_EDGE('',*,*,#37919,.F.) ;
#50699 = ORIENTED_EDGE('',*,*,#38154,.T.) ;
#50700 = ORIENTED_EDGE('',*,*,#38152,.T.) ;
#50701 = ORIENTED_EDGE('',*,*,#37918,.F.) ;
#50702 = ORIENTED_EDGE('',*,*,#38159,.F.) ;
#50703 = ORIENTED_EDGE('',*,*,#37938,.F.) ;
#50704 = ORIENTED_EDGE('',*,*,#37934,.F.) ;
#50705 = ORIENTED_EDGE('',*,*,#38160,.T.) ;
#50706 = ORIENTED_EDGE('',*,*,#38161,.T.) ;
#50707 = ORIENTED_EDGE('',*,*,#37944,.F.) ;
#50708 = ORIENTED_EDGE('',*,*,#38162,.T.) ;
#50709 = ORIENTED_EDGE('',*,*,#38163,.T.) ;
#50710 = ORIENTED_EDGE('',*,*,#37912,.F.) ;
#50711 = ORIENTED_EDGE('',*,*,#38164,.T.) ;
#50712 = ORIENTED_EDGE('',*,*,#38165,.T.) ;
#50713 = ORIENTED_EDGE('',*,*,#37928,.F.) ;
#50714 = ORIENTED_EDGE('',*,*,#38166,.T.) ;
#50715 = ORIENTED_EDGE('',*,*,#38167,.T.) ;
#50716 = ORIENTED_EDGE('',*,*,#38168,.F.) ;
#50717 = ORIENTED_EDGE('',*,*,#38159,.T.) ;
#50718 = ORIENTED_EDGE('',*,*,#38169,.F.) ;
#50719 = ORIENTED_EDGE('',*,*,#37909,.T.) ;
#50720 = ORIENTED_EDGE('',*,*,#38170,.F.) ;
#50721 = ORIENTED_EDGE('',*,*,#38171,.F.) ;
#50722 = ORIENTED_EDGE('',*,*,#37939,.F.) ;
#50723 = ORIENTED_EDGE('',*,*,#38168,.T.) ;
#50724 = ORIENTED_EDGE('',*,*,#38171,.T.) ;
#50725 = ORIENTED_EDGE('',*,*,#38172,.F.) ;
#50726 = ORIENTED_EDGE('',*,*,#38173,.F.) ;
#50727 = ORIENTED_EDGE('',*,*,#37923,.F.) ;
#50728 = ORIENTED_EDGE('',*,*,#38174,.T.) ;
#50729 = ORIENTED_EDGE('',*,*,#38175,.T.) ;
#50730 = ORIENTED_EDGE('',*,*,#37943,.F.) ;
#50731 = ORIENTED_EDGE('',*,*,#38176,.F.) ;
#50732 = ORIENTED_EDGE('',*,*,#37913,.F.) ;
#50733 = ORIENTED_EDGE('',*,*,#38177,.T.) ;
#50734 = ORIENTED_EDGE('',*,*,#38178,.T.) ;
#50735 = ORIENTED_EDGE('',*,*,#37920,.F.) ;
#50736 = ORIENTED_EDGE('',*,*,#38179,.F.) ;
#50737 = ORIENTED_EDGE('',*,*,#38169,.T.) ;
#50738 = ORIENTED_EDGE('',*,*,#37917,.F.) ;
#50739 = ORIENTED_EDGE('',*,*,#38180,.F.) ;
#50740 = ORIENTED_EDGE('',*,*,#38181,.F.) ;
#50741 = ORIENTED_EDGE('',*,*,#38182,.F.) ;
#50742 = ORIENTED_EDGE('',*,*,#37893,.F.) ;
#50743 = ORIENTED_EDGE('',*,*,#38183,.F.) ;
#50744 = ORIENTED_EDGE('',*,*,#38170,.T.) ;
#50745 = ORIENTED_EDGE('',*,*,#37911,.F.) ;
#50746 = ORIENTED_EDGE('',*,*,#38183,.T.) ;
#50747 = ORIENTED_EDGE('',*,*,#37892,.T.) ;
#50748 = ORIENTED_EDGE('',*,*,#38184,.F.) ;
#50749 = ORIENTED_EDGE('',*,*,#38172,.T.) ;
#50750 = ORIENTED_EDGE('',*,*,#37940,.F.) ;
#50751 = ORIENTED_EDGE('',*,*,#38173,.T.) ;
#50752 = ORIENTED_EDGE('',*,*,#38185,.F.) ;
#50753 = ORIENTED_EDGE('',*,*,#38186,.F.) ;
#50754 = ORIENTED_EDGE('',*,*,#38179,.T.) ;
#50755 = ORIENTED_EDGE('',*,*,#38176,.T.) ;
#50756 = ORIENTED_EDGE('',*,*,#38187,.F.) ;
#50757 = ORIENTED_EDGE('',*,*,#38188,.F.) ;
#50758 = ORIENTED_EDGE('',*,*,#38180,.T.) ;
#50759 = ORIENTED_EDGE('',*,*,#38189,.F.) ;
#50760 = ORIENTED_EDGE('',*,*,#37910,.F.) ;
#50761 = ORIENTED_EDGE('',*,*,#38181,.T.) ;
#50762 = ORIENTED_EDGE('',*,*,#38190,.F.) ;
#50763 = ORIENTED_EDGE('',*,*,#37903,.F.) ;
#50764 = ORIENTED_EDGE('',*,*,#38182,.T.) ;
#50765 = ORIENTED_EDGE('',*,*,#38191,.F.) ;
#50766 = ORIENTED_EDGE('',*,*,#38185,.T.) ;
#50767 = ORIENTED_EDGE('',*,*,#38184,.T.) ;
#50768 = ORIENTED_EDGE('',*,*,#37899,.F.) ;
#50769 = ORIENTED_EDGE('',*,*,#38186,.T.) ;
#50770 = ORIENTED_EDGE('',*,*,#38192,.F.) ;
#50771 = ORIENTED_EDGE('',*,*,#38193,.F.) ;
#50772 = ORIENTED_EDGE('',*,*,#38187,.T.) ;
#50773 = ORIENTED_EDGE('',*,*,#37942,.F.) ;
#50774 = ORIENTED_EDGE('',*,*,#38194,.F.) ;
#50775 = ORIENTED_EDGE('',*,*,#37914,.F.) ;
#50776 = ORIENTED_EDGE('',*,*,#38189,.T.) ;
#50777 = ORIENTED_EDGE('',*,*,#37916,.F.) ;
#50778 = ORIENTED_EDGE('',*,*,#38195,.F.) ;
#50779 = ORIENTED_EDGE('',*,*,#38196,.F.) ;
#50780 = ORIENTED_EDGE('',*,*,#38190,.T.) ;
#50781 = ORIENTED_EDGE('',*,*,#38188,.T.) ;
#50782 = ORIENTED_EDGE('',*,*,#38197,.F.) ;
#50783 = ORIENTED_EDGE('',*,*,#37904,.T.) ;
#50784 = ORIENTED_EDGE('',*,*,#38191,.T.) ;
#50785 = ORIENTED_EDGE('',*,*,#37898,.T.) ;
#50786 = ORIENTED_EDGE('',*,*,#38198,.F.) ;
#50787 = ORIENTED_EDGE('',*,*,#38192,.T.) ;
#50788 = ORIENTED_EDGE('',*,*,#38199,.F.) ;
#50789 = ORIENTED_EDGE('',*,*,#38200,.F.) ;
#50790 = ORIENTED_EDGE('',*,*,#37941,.F.) ;
#50791 = ORIENTED_EDGE('',*,*,#38193,.T.) ;
#50792 = ORIENTED_EDGE('',*,*,#38200,.T.) ;
#50793 = ORIENTED_EDGE('',*,*,#37908,.T.) ;
#50794 = ORIENTED_EDGE('',*,*,#38201,.F.) ;
#50795 = ORIENTED_EDGE('',*,*,#38194,.T.) ;
#50796 = ORIENTED_EDGE('',*,*,#38202,.F.) ;
#50797 = ORIENTED_EDGE('',*,*,#38195,.T.) ;
#50798 = ORIENTED_EDGE('',*,*,#38203,.F.) ;
#50799 = ORIENTED_EDGE('',*,*,#38197,.T.) ;
#50800 = ORIENTED_EDGE('',*,*,#38196,.T.) ;
#50801 = ORIENTED_EDGE('',*,*,#38204,.F.) ;
#50802 = ORIENTED_EDGE('',*,*,#37905,.F.) ;
#50803 = ORIENTED_EDGE('',*,*,#38198,.T.) ;
#50804 = ORIENTED_EDGE('',*,*,#37897,.F.) ;
#50805 = ORIENTED_EDGE('',*,*,#38205,.F.) ;
#50806 = ORIENTED_EDGE('',*,*,#37906,.F.) ;
#50807 = ORIENTED_EDGE('',*,*,#38199,.T.) ;
#50808 = ORIENTED_EDGE('',*,*,#37915,.F.) ;
#50809 = ORIENTED_EDGE('',*,*,#38201,.T.) ;
#50810 = ORIENTED_EDGE('',*,*,#38206,.F.) ;
#50811 = ORIENTED_EDGE('',*,*,#38203,.T.) ;
#50812 = ORIENTED_EDGE('',*,*,#38204,.T.) ;
#50813 = ORIENTED_EDGE('',*,*,#38202,.T.) ;
#50814 = ORIENTED_EDGE('',*,*,#38207,.F.) ;
#50815 = ORIENTED_EDGE('',*,*,#37900,.T.) ;
#50816 = ORIENTED_EDGE('',*,*,#38205,.T.) ;
#50817 = ORIENTED_EDGE('',*,*,#37901,.F.) ;
#50818 = ORIENTED_EDGE('',*,*,#38207,.T.) ;
#50819 = ORIENTED_EDGE('',*,*,#38206,.T.) ;
#50820 = ORIENTED_EDGE('',*,*,#37907,.F.) ;
#50821 = ORIENTED_EDGE('',*,*,#38208,.F.) ;
#50822 = ORIENTED_EDGE('',*,*,#37956,.F.) ;
#50823 = ORIENTED_EDGE('',*,*,#37791,.F.) ;
#50824 = ORIENTED_EDGE('',*,*,#37962,.F.) ;
#50825 = ORIENTED_EDGE('',*,*,#38209,.F.) ;
#50826 = ORIENTED_EDGE('',*,*,#38208,.T.) ;
#50827 = ORIENTED_EDGE('',*,*,#38210,.F.) ;
#50828 = ORIENTED_EDGE('',*,*,#37789,.F.) ;
#50829 = ORIENTED_EDGE('',*,*,#37871,.F.) ;
#50830 = ORIENTED_EDGE('',*,*,#38211,.F.) ;
#50831 = ORIENTED_EDGE('',*,*,#37960,.F.) ;
#50832 = ORIENTED_EDGE('',*,*,#38210,.T.) ;
#50833 = ORIENTED_EDGE('',*,*,#37961,.F.) ;
#50834 = ORIENTED_EDGE('',*,*,#38212,.F.) ;
#50835 = ORIENTED_EDGE('',*,*,#37967,.F.) ;
#50836 = ORIENTED_EDGE('',*,*,#38209,.T.) ;
#50837 = ORIENTED_EDGE('',*,*,#37966,.F.) ;
#50838 = ORIENTED_EDGE('',*,*,#38213,.F.) ;
#50839 = ORIENTED_EDGE('',*,*,#37957,.F.) ;
#50840 = ORIENTED_EDGE('',*,*,#37793,.F.) ;
#50841 = ORIENTED_EDGE('',*,*,#37955,.F.) ;
#50842 = ORIENTED_EDGE('',*,*,#38214,.F.) ;
#50843 = ORIENTED_EDGE('',*,*,#37766,.F.) ;
#50844 = ORIENTED_EDGE('',*,*,#37734,.F.) ;
#50845 = ORIENTED_EDGE('',*,*,#38215,.T.) ;
#50846 = ORIENTED_EDGE('',*,*,#37763,.F.) ;
#50847 = ORIENTED_EDGE('',*,*,#38216,.F.) ;
#50848 = ORIENTED_EDGE('',*,*,#38211,.T.) ;
#50849 = ORIENTED_EDGE('',*,*,#37870,.T.) ;
#50850 = ORIENTED_EDGE('',*,*,#38217,.F.) ;
#50851 = ORIENTED_EDGE('',*,*,#38212,.T.) ;
#50852 = ORIENTED_EDGE('',*,*,#38218,.F.) ;
#50853 = ORIENTED_EDGE('',*,*,#38213,.T.) ;
#50854 = ORIENTED_EDGE('',*,*,#38219,.F.) ;
#50855 = ORIENTED_EDGE('',*,*,#38214,.T.) ;
#50856 = ORIENTED_EDGE('',*,*,#37954,.T.) ;
#50857 = ORIENTED_EDGE('',*,*,#38220,.F.) ;
#50858 = ORIENTED_EDGE('',*,*,#38216,.T.) ;
#50859 = ORIENTED_EDGE('',*,*,#38217,.T.) ;
#50860 = ORIENTED_EDGE('',*,*,#37891,.F.) ;
#50861 = ORIENTED_EDGE('',*,*,#38221,.F.) ;
#50862 = ORIENTED_EDGE('',*,*,#37968,.F.) ;
#50863 = ORIENTED_EDGE('',*,*,#38219,.T.) ;
#50864 = ORIENTED_EDGE('',*,*,#37969,.F.) ;
#50865 = ORIENTED_EDGE('',*,*,#38222,.F.) ;
#50866 = ORIENTED_EDGE('',*,*,#37963,.F.) ;
#50867 = ORIENTED_EDGE('',*,*,#38218,.T.) ;
#50868 = ORIENTED_EDGE('',*,*,#37965,.F.) ;
#50869 = ORIENTED_EDGE('',*,*,#38223,.F.) ;
#50870 = ORIENTED_EDGE('',*,*,#37958,.F.) ;
#50871 = ORIENTED_EDGE('',*,*,#38220,.T.) ;
#50872 = ORIENTED_EDGE('',*,*,#37959,.F.) ;
#50873 = ORIENTED_EDGE('',*,*,#38224,.F.) ;
#50874 = ORIENTED_EDGE('',*,*,#37735,.F.) ;
#50875 = ORIENTED_EDGE('',*,*,#37769,.F.) ;
#50876 = ORIENTED_EDGE('',*,*,#38225,.T.) ;
#50877 = ORIENTED_EDGE('',*,*,#37740,.F.) ;
#50878 = ORIENTED_EDGE('',*,*,#38226,.F.) ;
#50879 = ORIENTED_EDGE('',*,*,#37819,.F.) ;
#50880 = ORIENTED_EDGE('',*,*,#37770,.F.) ;
#50881 = ORIENTED_EDGE('',*,*,#38227,.F.) ;
#50882 = ORIENTED_EDGE('',*,*,#37982,.F.) ;
#50883 = ORIENTED_EDGE('',*,*,#37821,.F.) ;
#50884 = ORIENTED_EDGE('',*,*,#37981,.F.) ;
#50885 = ORIENTED_EDGE('',*,*,#38228,.F.) ;
#50886 = ORIENTED_EDGE('',*,*,#37979,.F.) ;
#50887 = ORIENTED_EDGE('',*,*,#38221,.T.) ;
#50888 = ORIENTED_EDGE('',*,*,#37890,.T.) ;
#50889 = ORIENTED_EDGE('',*,*,#38229,.F.) ;
#50890 = ORIENTED_EDGE('',*,*,#38222,.T.) ;
#50891 = ORIENTED_EDGE('',*,*,#38224,.T.) ;
#50892 = ORIENTED_EDGE('',*,*,#38223,.T.) ;
#50893 = ORIENTED_EDGE('',*,*,#37727,.F.) ;
#50894 = ORIENTED_EDGE('',*,*,#38227,.T.) ;
#50895 = ORIENTED_EDGE('',*,*,#38226,.T.) ;
#50896 = ORIENTED_EDGE('',*,*,#38230,.F.) ;
#50897 = ORIENTED_EDGE('',*,*,#37983,.T.) ;
#50898 = ORIENTED_EDGE('',*,*,#38231,.F.) ;
#50899 = ORIENTED_EDGE('',*,*,#38228,.T.) ;
#50900 = ORIENTED_EDGE('',*,*,#38232,.F.) ;
#50901 = ORIENTED_EDGE('',*,*,#38229,.T.) ;
#50902 = ORIENTED_EDGE('',*,*,#37889,.F.) ;
#50903 = ORIENTED_EDGE('',*,*,#38233,.F.) ;
#50904 = ORIENTED_EDGE('',*,*,#37964,.F.) ;
#50905 = ORIENTED_EDGE('',*,*,#38230,.T.) ;
#50906 = ORIENTED_EDGE('',*,*,#37739,.F.) ;
#50907 = ORIENTED_EDGE('',*,*,#38234,.F.) ;
#50908 = ORIENTED_EDGE('',*,*,#37984,.F.) ;
#50909 = ORIENTED_EDGE('',*,*,#38235,.F.) ;
#50910 = ORIENTED_EDGE('',*,*,#37985,.F.) ;
#50911 = ORIENTED_EDGE('',*,*,#38236,.F.) ;
#50912 = ORIENTED_EDGE('',*,*,#37976,.F.) ;
#50913 = ORIENTED_EDGE('',*,*,#38232,.T.) ;
#50914 = ORIENTED_EDGE('',*,*,#37980,.F.) ;
#50915 = ORIENTED_EDGE('',*,*,#38237,.F.) ;
#50916 = ORIENTED_EDGE('',*,*,#37970,.F.) ;
#50917 = ORIENTED_EDGE('',*,*,#38231,.T.) ;
#50918 = ORIENTED_EDGE('',*,*,#37973,.F.) ;
#50919 = ORIENTED_EDGE('',*,*,#38238,.F.) ;
#50920 = ORIENTED_EDGE('',*,*,#37977,.F.) ;
#50921 = ORIENTED_EDGE('',*,*,#37823,.F.) ;
#50922 = ORIENTED_EDGE('',*,*,#37978,.F.) ;
#50923 = ORIENTED_EDGE('',*,*,#38239,.F.) ;
#50924 = ORIENTED_EDGE('',*,*,#37883,.F.) ;
#50925 = ORIENTED_EDGE('',*,*,#37725,.T.) ;
#50926 = ORIENTED_EDGE('',*,*,#38233,.T.) ;
#50927 = ORIENTED_EDGE('',*,*,#38240,.F.) ;
#50928 = ORIENTED_EDGE('',*,*,#37736,.T.) ;
#50929 = ORIENTED_EDGE('',*,*,#38236,.T.) ;
#50930 = ORIENTED_EDGE('',*,*,#38234,.T.) ;
#50931 = ORIENTED_EDGE('',*,*,#37723,.F.) ;
#50932 = ORIENTED_EDGE('',*,*,#38241,.F.) ;
#50933 = ORIENTED_EDGE('',*,*,#38241,.T.) ;
#50934 = ORIENTED_EDGE('',*,*,#37722,.F.) ;
#50935 = ORIENTED_EDGE('',*,*,#38237,.T.) ;
#50936 = ORIENTED_EDGE('',*,*,#38235,.T.) ;
#50937 = ORIENTED_EDGE('',*,*,#38242,.F.) ;
#50938 = ORIENTED_EDGE('',*,*,#38239,.T.) ;
#50939 = ORIENTED_EDGE('',*,*,#38238,.T.) ;
#50940 = ORIENTED_EDGE('',*,*,#38243,.F.) ;
#50941 = ORIENTED_EDGE('',*,*,#37884,.T.) ;
#50942 = ORIENTED_EDGE('',*,*,#38240,.T.) ;
#50943 = ORIENTED_EDGE('',*,*,#37888,.F.) ;
#50944 = ORIENTED_EDGE('',*,*,#38244,.F.) ;
#50945 = ORIENTED_EDGE('',*,*,#37737,.F.) ;
#50946 = ORIENTED_EDGE('',*,*,#38242,.T.) ;
#50947 = ORIENTED_EDGE('',*,*,#37975,.F.) ;
#50948 = ORIENTED_EDGE('',*,*,#38245,.F.) ;
#50949 = ORIENTED_EDGE('',*,*,#37971,.F.) ;
#50950 = ORIENTED_EDGE('',*,*,#38243,.T.) ;
#50951 = ORIENTED_EDGE('',*,*,#37972,.F.) ;
#50952 = ORIENTED_EDGE('',*,*,#38246,.F.) ;
#50953 = ORIENTED_EDGE('',*,*,#37885,.F.) ;
#50954 = ORIENTED_EDGE('',*,*,#37738,.T.) ;
#50955 = ORIENTED_EDGE('',*,*,#38244,.T.) ;
#50956 = ORIENTED_EDGE('',*,*,#38247,.F.) ;
#50957 = ORIENTED_EDGE('',*,*,#37720,.T.) ;
#50958 = ORIENTED_EDGE('',*,*,#38246,.T.) ;
#50959 = ORIENTED_EDGE('',*,*,#38245,.T.) ;
#50960 = ORIENTED_EDGE('',*,*,#38248,.F.) ;
#50961 = ORIENTED_EDGE('',*,*,#37886,.T.) ;
#50962 = ORIENTED_EDGE('',*,*,#38247,.T.) ;
#50963 = ORIENTED_EDGE('',*,*,#37887,.F.) ;
#50964 = ORIENTED_EDGE('',*,*,#38248,.T.) ;
#50965 = ORIENTED_EDGE('',*,*,#37974,.F.) ;
#50966 = ORIENTED_EDGE('',*,*,#37743,.F.) ;
#50967 = ORIENTED_EDGE('',*,*,#38249,.T.) ;
#50968 = ORIENTED_EDGE('',*,*,#38064,.F.) ;
#50969 = ORIENTED_EDGE('',*,*,#38250,.F.) ;
#50970 = ORIENTED_EDGE('',*,*,#38069,.F.) ;
#50971 = ORIENTED_EDGE('',*,*,#38063,.F.) ;
#50972 = ORIENTED_EDGE('',*,*,#38251,.T.) ;
#50973 = ORIENTED_EDGE('',*,*,#38070,.F.) ;
#50974 = ORIENTED_EDGE('',*,*,#38250,.T.) ;
#50975 = ORIENTED_EDGE('',*,*,#38066,.F.) ;
#50976 = ORIENTED_EDGE('',*,*,#38252,.T.) ;
#50977 = ORIENTED_EDGE('',*,*,#37932,.F.) ;
#50978 = ORIENTED_EDGE('',*,*,#38090,.F.) ;
#50979 = ORIENTED_EDGE('',*,*,#38253,.F.) ;
#50980 = ORIENTED_EDGE('',*,*,#38075,.F.) ;
#50981 = ORIENTED_EDGE('',*,*,#38254,.T.) ;
#50982 = ORIENTED_EDGE('',*,*,#38103,.F.) ;
#50983 = ORIENTED_EDGE('',*,*,#38255,.F.) ;
#50984 = ORIENTED_EDGE('',*,*,#38060,.F.) ;
#50985 = ORIENTED_EDGE('',*,*,#38256,.T.) ;
#50986 = ORIENTED_EDGE('',*,*,#37745,.F.) ;
#50987 = ORIENTED_EDGE('',*,*,#38068,.F.) ;
#50988 = ORIENTED_EDGE('',*,*,#38257,.F.) ;
#50989 = ORIENTED_EDGE('',*,*,#38087,.F.) ;
#50990 = ORIENTED_EDGE('',*,*,#38258,.T.) ;
#50991 = ORIENTED_EDGE('',*,*,#38061,.F.) ;
#50992 = ORIENTED_EDGE('',*,*,#38253,.T.) ;
#50993 = ORIENTED_EDGE('',*,*,#38259,.F.) ;
#50994 = ORIENTED_EDGE('',*,*,#38255,.T.) ;
#50995 = ORIENTED_EDGE('',*,*,#38260,.F.) ;
#50996 = ORIENTED_EDGE('',*,*,#38072,.F.) ;
#50997 = ORIENTED_EDGE('',*,*,#38261,.T.) ;
#50998 = ORIENTED_EDGE('',*,*,#38055,.F.) ;
#50999 = ORIENTED_EDGE('',*,*,#38257,.T.) ;
#51000 = ORIENTED_EDGE('',*,*,#38105,.F.) ;
#51001 = ORIENTED_EDGE('',*,*,#38262,.T.) ;
#51002 = ORIENTED_EDGE('',*,*,#38081,.F.) ;
#51003 = ORIENTED_EDGE('',*,*,#38263,.F.) ;
#51004 = ORIENTED_EDGE('',*,*,#38260,.T.) ;
#51005 = ORIENTED_EDGE('',*,*,#38106,.F.) ;
#51006 = ORIENTED_EDGE('',*,*,#38264,.F.) ;
#51007 = ORIENTED_EDGE('',*,*,#38080,.F.) ;
#51008 = ORIENTED_EDGE('',*,*,#38259,.T.) ;
#51009 = ORIENTED_EDGE('',*,*,#38079,.F.) ;
#51010 = ORIENTED_EDGE('',*,*,#38265,.F.) ;
#51011 = ORIENTED_EDGE('',*,*,#38076,.F.) ;
#51012 = ORIENTED_EDGE('',*,*,#38101,.F.) ;
#51013 = ORIENTED_EDGE('',*,*,#38266,.T.) ;
#51014 = ORIENTED_EDGE('',*,*,#38073,.F.) ;
#51015 = ORIENTED_EDGE('',*,*,#38267,.F.) ;
#51016 = ORIENTED_EDGE('',*,*,#38264,.T.) ;
#51017 = ORIENTED_EDGE('',*,*,#38263,.T.) ;
#51018 = ORIENTED_EDGE('',*,*,#38268,.F.) ;
#51019 = ORIENTED_EDGE('',*,*,#38267,.T.) ;
#51020 = ORIENTED_EDGE('',*,*,#38265,.T.) ;
#51021 = ORIENTED_EDGE('',*,*,#38269,.F.) ;
#51022 = ORIENTED_EDGE('',*,*,#38268,.T.) ;
#51023 = ORIENTED_EDGE('',*,*,#38084,.F.) ;
#51024 = ORIENTED_EDGE('',*,*,#38270,.F.) ;
#51025 = ORIENTED_EDGE('',*,*,#38077,.F.) ;
#51026 = ORIENTED_EDGE('',*,*,#38269,.T.) ;
#51027 = ORIENTED_EDGE('',*,*,#38078,.F.) ;
#51028 = ORIENTED_EDGE('',*,*,#38271,.F.) ;
#51029 = ORIENTED_EDGE('',*,*,#38102,.F.) ;
#51030 = ORIENTED_EDGE('',*,*,#38271,.T.) ;
#51031 = ORIENTED_EDGE('',*,*,#38270,.T.) ;
#51032 = ORIENTED_EDGE('',*,*,#38272,.F.) ;
#51033 = ORIENTED_EDGE('',*,*,#38083,.F.) ;
#51034 = ORIENTED_EDGE('',*,*,#38273,.T.) ;
#51035 = ORIENTED_EDGE('',*,*,#38099,.F.) ;
#51036 = ORIENTED_EDGE('',*,*,#38272,.T.) ;
#51037 = ORIENTED_EDGE('',*,*,#38057,.F.) ;
#51038 = ORIENTED_EDGE('',*,*,#38274,.T.) ;
#51039 = ORIENTED_EDGE('',*,*,#38085,.F.) ;
#51040 = ORIENTED_EDGE('',*,*,#38275,.F.) ;
#51041 = ORIENTED_EDGE('',*,*,#37936,.F.) ;
#51042 = ORIENTED_EDGE('',*,*,#38276,.T.) ;
#51043 = ORIENTED_EDGE('',*,*,#38058,.F.) ;
#51044 = ORIENTED_EDGE('',*,*,#38275,.T.) ;
#51045 = ORIENTED_EDGE('',*,*,#38089,.F.) ;
#51046 = ORIENTED_EDGE('',*,*,#38048,.F.) ;
#51047 = ORIENTED_EDGE('',*,*,#38277,.T.) ;
#51048 = ORIENTED_EDGE('',*,*,#38049,.F.) ;
#51049 = ORIENTED_EDGE('',*,*,#37951,.F.) ;
#51050 = ORIENTED_EDGE('',*,*,#38054,.F.) ;
#51051 = ORIENTED_EDGE('',*,*,#38278,.T.) ;
#51052 = ORIENTED_EDGE('',*,*,#38046,.F.) ;
#51053 = ORIENTED_EDGE('',*,*,#37949,.F.) ;
#51054 = ORIENTED_EDGE('',*,*,#38033,.F.) ;
#51055 = ORIENTED_EDGE('',*,*,#38279,.T.) ;
#51056 = ORIENTED_EDGE('',*,*,#38091,.F.) ;
#51057 = ORIENTED_EDGE('',*,*,#38280,.F.) ;
#51058 = ORIENTED_EDGE('',*,*,#38093,.F.) ;
#51059 = ORIENTED_EDGE('',*,*,#38281,.T.) ;
#51060 = ORIENTED_EDGE('',*,*,#38039,.F.) ;
#51061 = ORIENTED_EDGE('',*,*,#38282,.F.) ;
#51062 = ORIENTED_EDGE('',*,*,#38283,.F.) ;
#51063 = ORIENTED_EDGE('',*,*,#38094,.F.) ;
#51064 = ORIENTED_EDGE('',*,*,#38284,.F.) ;
#51065 = ORIENTED_EDGE('',*,*,#38038,.F.) ;
#51066 = ORIENTED_EDGE('',*,*,#38280,.T.) ;
#51067 = ORIENTED_EDGE('',*,*,#38283,.T.) ;
#51068 = ORIENTED_EDGE('',*,*,#38285,.F.) ;
#51069 = ORIENTED_EDGE('',*,*,#38051,.F.) ;
#51070 = ORIENTED_EDGE('',*,*,#38286,.T.) ;
#51071 = ORIENTED_EDGE('',*,*,#38043,.F.) ;
#51072 = ORIENTED_EDGE('',*,*,#37953,.F.) ;
#51073 = ORIENTED_EDGE('',*,*,#38045,.F.) ;
#51074 = ORIENTED_EDGE('',*,*,#38287,.T.) ;
#51075 = ORIENTED_EDGE('',*,*,#38052,.F.) ;
#51076 = ORIENTED_EDGE('',*,*,#37947,.F.) ;
#51077 = ORIENTED_EDGE('',*,*,#38284,.T.) ;
#51078 = ORIENTED_EDGE('',*,*,#38282,.T.) ;
#51079 = ORIENTED_EDGE('',*,*,#38288,.F.) ;
#51080 = ORIENTED_EDGE('',*,*,#38285,.T.) ;
#51081 = ORIENTED_EDGE('',*,*,#38037,.F.) ;
#51082 = ORIENTED_EDGE('',*,*,#38289,.F.) ;
#51083 = ORIENTED_EDGE('',*,*,#38034,.F.) ;
#51084 = ORIENTED_EDGE('',*,*,#38097,.F.) ;
#51085 = ORIENTED_EDGE('',*,*,#38290,.T.) ;
#51086 = ORIENTED_EDGE('',*,*,#38031,.F.) ;
#51087 = ORIENTED_EDGE('',*,*,#38291,.F.) ;
#51088 = ORIENTED_EDGE('',*,*,#38041,.F.) ;
#51089 = ORIENTED_EDGE('',*,*,#38292,.T.) ;
#51090 = ORIENTED_EDGE('',*,*,#38095,.F.) ;
#51091 = ORIENTED_EDGE('',*,*,#38293,.F.) ;
#51092 = ORIENTED_EDGE('',*,*,#38288,.T.) ;
#51093 = ORIENTED_EDGE('',*,*,#38042,.F.) ;
#51094 = ORIENTED_EDGE('',*,*,#38294,.F.) ;
#51095 = ORIENTED_EDGE('',*,*,#38035,.F.) ;
#51096 = ORIENTED_EDGE('',*,*,#38291,.T.) ;
#51097 = ORIENTED_EDGE('',*,*,#38289,.T.) ;
#51098 = ORIENTED_EDGE('',*,*,#38295,.F.) ;
#51099 = ORIENTED_EDGE('',*,*,#38294,.T.) ;
#51100 = ORIENTED_EDGE('',*,*,#38293,.T.) ;
#51101 = ORIENTED_EDGE('',*,*,#38296,.F.) ;
#51102 = ORIENTED_EDGE('',*,*,#38295,.T.) ;
#51103 = ORIENTED_EDGE('',*,*,#38036,.F.) ;
#51104 = ORIENTED_EDGE('',*,*,#38296,.T.) ;
#51105 = ORIENTED_EDGE('',*,*,#38098,.F.) ;
#51106 = ORIENTED_EDGE('',*,*,#37780,.F.) ;
#51107 = ORIENTED_EDGE('',*,*,#37756,.F.) ;
#51108 = ORIENTED_EDGE('',*,*,#38297,.F.) ;
#51109 = ORIENTED_EDGE('',*,*,#37762,.F.) ;
#51110 = ORIENTED_EDGE('',*,*,#38018,.F.) ;
#51111 = ORIENTED_EDGE('',*,*,#38298,.T.) ;
#51112 = ORIENTED_EDGE('',*,*,#37757,.F.) ;
#51113 = ORIENTED_EDGE('',*,*,#38299,.F.) ;
#51114 = ORIENTED_EDGE('',*,*,#38299,.T.) ;
#51115 = ORIENTED_EDGE('',*,*,#38297,.T.) ;
#51116 = ORIENTED_EDGE('',*,*,#38300,.F.) ;
#51117 = ORIENTED_EDGE('',*,*,#37779,.F.) ;
#51118 = ORIENTED_EDGE('',*,*,#37752,.F.) ;
#51119 = ORIENTED_EDGE('',*,*,#38301,.F.) ;
#51120 = ORIENTED_EDGE('',*,*,#37754,.F.) ;
#51121 = ORIENTED_EDGE('',*,*,#38300,.T.) ;
#51122 = ORIENTED_EDGE('',*,*,#37755,.F.) ;
#51123 = ORIENTED_EDGE('',*,*,#38302,.F.) ;
#51124 = ORIENTED_EDGE('',*,*,#38019,.F.) ;
#51125 = ORIENTED_EDGE('',*,*,#38302,.T.) ;
#51126 = ORIENTED_EDGE('',*,*,#38301,.T.) ;
#51127 = ORIENTED_EDGE('',*,*,#38303,.F.) ;
#51128 = ORIENTED_EDGE('',*,*,#37751,.F.) ;
#51129 = ORIENTED_EDGE('',*,*,#38304,.T.) ;
#51130 = ORIENTED_EDGE('',*,*,#38016,.F.) ;
#51131 = ORIENTED_EDGE('',*,*,#38303,.T.) ;
#51132 = ORIENTED_EDGE('',*,*,#37855,.F.) ;
#51133 = ORIENTED_EDGE('',*,*,#37707,.T.) ;
#51134 = ORIENTED_EDGE('',*,*,#38305,.T.) ;
#51135 = ORIENTED_EDGE('',*,*,#38027,.F.) ;
#51136 = ORIENTED_EDGE('',*,*,#38306,.F.) ;
#51137 = ORIENTED_EDGE('',*,*,#37833,.F.) ;
#51138 = ORIENTED_EDGE('',*,*,#37856,.F.) ;
#51139 = ORIENTED_EDGE('',*,*,#38307,.F.) ;
#51140 = ORIENTED_EDGE('',*,*,#37853,.F.) ;
#51141 = ORIENTED_EDGE('',*,*,#38307,.T.) ;
#51142 = ORIENTED_EDGE('',*,*,#38306,.T.) ;
#51143 = ORIENTED_EDGE('',*,*,#38308,.F.) ;
#51144 = ORIENTED_EDGE('',*,*,#38308,.T.) ;
#51145 = ORIENTED_EDGE('',*,*,#38030,.F.) ;
#51146 = ORIENTED_EDGE('',*,*,#38309,.F.) ;
#51147 = ORIENTED_EDGE('',*,*,#37851,.F.) ;
#51148 = ORIENTED_EDGE('',*,*,#37835,.F.) ;
#51149 = ORIENTED_EDGE('',*,*,#37852,.F.) ;
#51150 = ORIENTED_EDGE('',*,*,#38310,.F.) ;
#51151 = ORIENTED_EDGE('',*,*,#37849,.F.) ;
#51152 = ORIENTED_EDGE('',*,*,#38310,.T.) ;
#51153 = ORIENTED_EDGE('',*,*,#38309,.T.) ;
#51154 = ORIENTED_EDGE('',*,*,#38311,.F.) ;
#51155 = ORIENTED_EDGE('',*,*,#38029,.F.) ;
#51156 = ORIENTED_EDGE('',*,*,#37711,.T.) ;
#51157 = ORIENTED_EDGE('',*,*,#38312,.T.) ;
#51158 = ORIENTED_EDGE('',*,*,#37850,.F.) ;
#51159 = ORIENTED_EDGE('',*,*,#38311,.T.) ;
#51160 = ORIENTED_EDGE('',*,*,#37930,.F.) ;
#51161 = ORIENTED_EDGE('',*,*,#38313,.T.) ;
#51162 = ORIENTED_EDGE('',*,*,#37741,.F.) ;
#51163 = ORIENTED_EDGE('',*,*,#38314,.T.) ;
#51164 = ORIENTED_EDGE('',*,*,#37800,.F.) ;
#51165 = ORIENTED_EDGE('',*,*,#37902,.F.) ;
#51166 = ORIENTED_EDGE('',*,*,#37812,.F.) ;
#51167 = ORIENTED_EDGE('',*,*,#37836,.F.) ;
#51168 = ORIENTED_EDGE('',*,*,#37802,.F.) ;
#51169 = ORIENTED_EDGE('',*,*,#37837,.F.) ;
#51170 = ORIENTED_EDGE('',*,*,#37810,.F.) ;
#51171 = ORIENTED_EDGE('',*,*,#37838,.F.) ;
#51172 = ORIENTED_EDGE('',*,*,#37804,.F.) ;
#51173 = ORIENTED_EDGE('',*,*,#37839,.F.) ;
#51174 = ORIENTED_EDGE('',*,*,#37808,.F.) ;
#51175 = ORIENTED_EDGE('',*,*,#37842,.F.) ;
#51176 = ORIENTED_EDGE('',*,*,#37797,.F.) ;
#51177 = ORIENTED_EDGE('',*,*,#37772,.F.) ;
#51178 = ORIENTED_EDGE('',*,*,#37815,.F.) ;
#51179 = ORIENTED_EDGE('',*,*,#37895,.F.) ;
#51180 = ORIENTED_EDGE('',*,*,#38115,.F.) ;
#51181 = ORIENTED_EDGE('',*,*,#38315,.T.) ;
#51182 = ORIENTED_EDGE('',*,*,#37774,.F.) ;
#51183 = ORIENTED_EDGE('',*,*,#37796,.F.) ;
#51184 = ORIENTED_EDGE('',*,*,#38110,.F.) ;
#51185 = ORIENTED_EDGE('',*,*,#38316,.T.) ;
#51186 = ORIENTED_EDGE('',*,*,#37775,.F.) ;
#51187 = ORIENTED_EDGE('',*,*,#38317,.T.) ;
#51188 = ORIENTED_EDGE('',*,*,#37776,.F.) ;
#51189 = ORIENTED_EDGE('',*,*,#38318,.T.) ;
#51190 = ORIENTED_EDGE('',*,*,#38107,.F.) ;
#51191 = ORIENTED_EDGE('',*,*,#37816,.F.) ;
#51192 = ORIENTED_EDGE('',*,*,#38155,.F.) ;
#51193 = ORIENTED_EDGE('',*,*,#38161,.F.) ;
#51194 = ORIENTED_EDGE('',*,*,#38160,.F.) ;
#51195 = ORIENTED_EDGE('',*,*,#38319,.F.) ;
#51196 = ORIENTED_EDGE('',*,*,#38156,.F.) ;
#51197 = ORIENTED_EDGE('',*,*,#38249,.F.) ;
#51198 = ORIENTED_EDGE('',*,*,#37742,.F.) ;
#51199 = ORIENTED_EDGE('',*,*,#38320,.F.) ;
#51200 = ORIENTED_EDGE('',*,*,#37924,.F.) ;
#51201 = ORIENTED_EDGE('',*,*,#38319,.T.) ;
#51202 = ORIENTED_EDGE('',*,*,#37933,.F.) ;
#51203 = ORIENTED_EDGE('',*,*,#38252,.F.) ;
#51204 = ORIENTED_EDGE('',*,*,#38065,.F.) ;
#51205 = ORIENTED_EDGE('',*,*,#38320,.T.) ;
#51206 = ORIENTED_EDGE('',*,*,#38313,.F.) ;
#51207 = ORIENTED_EDGE('',*,*,#38321,.F.) ;
#51208 = ORIENTED_EDGE('',*,*,#38321,.T.) ;
#51209 = ORIENTED_EDGE('',*,*,#37929,.F.) ;
#51210 = ORIENTED_EDGE('',*,*,#38322,.F.) ;
#51211 = ORIENTED_EDGE('',*,*,#37925,.F.) ;
#51212 = ORIENTED_EDGE('',*,*,#38164,.F.) ;
#51213 = ORIENTED_EDGE('',*,*,#38158,.F.) ;
#51214 = ORIENTED_EDGE('',*,*,#38157,.F.) ;
#51215 = ORIENTED_EDGE('',*,*,#38322,.T.) ;
#51216 = ORIENTED_EDGE('',*,*,#38165,.F.) ;
#51217 = ORIENTED_EDGE('',*,*,#38177,.F.) ;
#51218 = ORIENTED_EDGE('',*,*,#38167,.F.) ;
#51219 = ORIENTED_EDGE('',*,*,#38166,.F.) ;
#51220 = ORIENTED_EDGE('',*,*,#38323,.F.) ;
#51221 = ORIENTED_EDGE('',*,*,#38178,.F.) ;
#51222 = ORIENTED_EDGE('',*,*,#38323,.T.) ;
#51223 = ORIENTED_EDGE('',*,*,#37931,.F.) ;
#51224 = ORIENTED_EDGE('',*,*,#38324,.F.) ;
#51225 = ORIENTED_EDGE('',*,*,#37921,.F.) ;
#51226 = ORIENTED_EDGE('',*,*,#38324,.T.) ;
#51227 = ORIENTED_EDGE('',*,*,#38314,.F.) ;
#51228 = ORIENTED_EDGE('',*,*,#38325,.F.) ;
#51229 = ORIENTED_EDGE('',*,*,#38276,.F.) ;
#51230 = ORIENTED_EDGE('',*,*,#37935,.F.) ;
#51231 = ORIENTED_EDGE('',*,*,#38326,.F.) ;
#51232 = ORIENTED_EDGE('',*,*,#37922,.F.) ;
#51233 = ORIENTED_EDGE('',*,*,#38325,.T.) ;
#51234 = ORIENTED_EDGE('',*,*,#37746,.F.) ;
#51235 = ORIENTED_EDGE('',*,*,#38256,.F.) ;
#51236 = ORIENTED_EDGE('',*,*,#38059,.F.) ;
#51237 = ORIENTED_EDGE('',*,*,#38326,.T.) ;
#51238 = ORIENTED_EDGE('',*,*,#38163,.F.) ;
#51239 = ORIENTED_EDGE('',*,*,#38162,.F.) ;
#51240 = ORIENTED_EDGE('',*,*,#38175,.F.) ;
#51241 = ORIENTED_EDGE('',*,*,#38174,.F.) ;
#51242 = ORIENTED_EDGE('',*,*,#37750,.F.) ;
#51243 = ORIENTED_EDGE('',*,*,#38327,.T.) ;
#51244 = ORIENTED_EDGE('',*,*,#38020,.F.) ;
#51245 = ORIENTED_EDGE('',*,*,#38328,.F.) ;
#51246 = ORIENTED_EDGE('',*,*,#38304,.F.) ;
#51247 = ORIENTED_EDGE('',*,*,#38328,.T.) ;
#51248 = ORIENTED_EDGE('',*,*,#38026,.F.) ;
#51249 = ORIENTED_EDGE('',*,*,#38329,.F.) ;
#51250 = ORIENTED_EDGE('',*,*,#38017,.F.) ;
#51251 = ORIENTED_EDGE('',*,*,#38329,.T.) ;
#51252 = ORIENTED_EDGE('',*,*,#38025,.F.) ;
#51253 = ORIENTED_EDGE('',*,*,#38330,.F.) ;
#51254 = ORIENTED_EDGE('',*,*,#38331,.F.) ;
#51255 = ORIENTED_EDGE('',*,*,#38332,.F.) ;
#51256 = ORIENTED_EDGE('',*,*,#38333,.F.) ;
#51257 = ORIENTED_EDGE('',*,*,#37758,.F.) ;
#51258 = ORIENTED_EDGE('',*,*,#38298,.F.) ;
#51259 = ORIENTED_EDGE('',*,*,#37781,.F.) ;
#51260 = ORIENTED_EDGE('',*,*,#37760,.F.) ;
#51261 = ORIENTED_EDGE('',*,*,#38334,.F.) ;
#51262 = ORIENTED_EDGE('',*,*,#37858,.F.) ;
#51263 = ORIENTED_EDGE('',*,*,#37759,.F.) ;
#51264 = ORIENTED_EDGE('',*,*,#38333,.T.) ;
#51265 = ORIENTED_EDGE('',*,*,#38332,.T.) ;
#51266 = ORIENTED_EDGE('',*,*,#38331,.T.) ;
#51267 = ORIENTED_EDGE('',*,*,#38330,.T.) ;
#51268 = ORIENTED_EDGE('',*,*,#38335,.F.) ;
#51269 = ORIENTED_EDGE('',*,*,#37859,.F.) ;
#51270 = ORIENTED_EDGE('',*,*,#38334,.T.) ;
#51271 = ORIENTED_EDGE('',*,*,#37710,.F.) ;
#51272 = ORIENTED_EDGE('',*,*,#38336,.T.) ;
#51273 = ORIENTED_EDGE('',*,*,#37846,.F.) ;
#51274 = ORIENTED_EDGE('',*,*,#38312,.F.) ;
#51275 = ORIENTED_EDGE('',*,*,#38335,.T.) ;
#51276 = ORIENTED_EDGE('',*,*,#38024,.F.) ;
#51277 = ORIENTED_EDGE('',*,*,#38337,.F.) ;
#51278 = ORIENTED_EDGE('',*,*,#37860,.F.) ;
#51279 = ORIENTED_EDGE('',*,*,#37831,.F.) ;
#51280 = ORIENTED_EDGE('',*,*,#37862,.F.) ;
#51281 = ORIENTED_EDGE('',*,*,#38338,.F.) ;
#51282 = ORIENTED_EDGE('',*,*,#37857,.F.) ;
#51283 = ORIENTED_EDGE('',*,*,#37712,.T.) ;
#51284 = ORIENTED_EDGE('',*,*,#38028,.F.) ;
#51285 = ORIENTED_EDGE('',*,*,#38339,.F.) ;
#51286 = ORIENTED_EDGE('',*,*,#38022,.F.) ;
#51287 = ORIENTED_EDGE('',*,*,#37861,.F.) ;
#51288 = ORIENTED_EDGE('',*,*,#38337,.T.) ;
#51289 = ORIENTED_EDGE('',*,*,#38340,.F.) ;
#51290 = ORIENTED_EDGE('',*,*,#38341,.F.) ;
#51291 = ORIENTED_EDGE('',*,*,#38342,.F.) ;
#51292 = ORIENTED_EDGE('',*,*,#37705,.F.) ;
#51293 = ORIENTED_EDGE('',*,*,#37704,.F.) ;
#51294 = ORIENTED_EDGE('',*,*,#37854,.F.) ;
#51295 = ORIENTED_EDGE('',*,*,#38338,.T.) ;
#51296 = ORIENTED_EDGE('',*,*,#37706,.F.) ;
#51297 = ORIENTED_EDGE('',*,*,#38342,.T.) ;
#51298 = ORIENTED_EDGE('',*,*,#38341,.T.) ;
#51299 = ORIENTED_EDGE('',*,*,#38340,.T.) ;
#51300 = ORIENTED_EDGE('',*,*,#38023,.F.) ;
#51301 = ORIENTED_EDGE('',*,*,#38339,.T.) ;
#51302 = ORIENTED_EDGE('',*,*,#38305,.F.) ;
#51303 = ORIENTED_EDGE('',*,*,#38343,.F.) ;
#51304 = ORIENTED_EDGE('',*,*,#37768,.F.) ;
#51305 = ORIENTED_EDGE('',*,*,#37818,.F.) ;
#51306 = ORIENTED_EDGE('',*,*,#38109,.F.) ;
#51307 = ORIENTED_EDGE('',*,*,#38225,.F.) ;
#51308 = ORIENTED_EDGE('',*,*,#38343,.T.) ;
#51309 = ORIENTED_EDGE('',*,*,#38344,.F.) ;
#51310 = ORIENTED_EDGE('',*,*,#37730,.F.) ;
#51311 = ORIENTED_EDGE('',*,*,#38344,.T.) ;
#51312 = ORIENTED_EDGE('',*,*,#38108,.F.) ;
#51313 = ORIENTED_EDGE('',*,*,#38345,.F.) ;
#51314 = ORIENTED_EDGE('',*,*,#38112,.F.) ;
#51315 = ORIENTED_EDGE('',*,*,#38318,.F.) ;
#51316 = ORIENTED_EDGE('',*,*,#38316,.F.) ;
#51317 = ORIENTED_EDGE('',*,*,#38345,.T.) ;
#51318 = ORIENTED_EDGE('',*,*,#38346,.T.) ;
#51319 = ORIENTED_EDGE('',*,*,#38251,.F.) ;
#51320 = ORIENTED_EDGE('',*,*,#38347,.F.) ;
#51321 = ORIENTED_EDGE('',*,*,#38254,.F.) ;
#51322 = ORIENTED_EDGE('',*,*,#38346,.F.) ;
#51323 = ORIENTED_EDGE('',*,*,#38074,.F.) ;
#51324 = ORIENTED_EDGE('',*,*,#38348,.F.) ;
#51325 = ORIENTED_EDGE('',*,*,#38071,.F.) ;
#51326 = ORIENTED_EDGE('',*,*,#38347,.T.) ;
#51327 = ORIENTED_EDGE('',*,*,#38062,.F.) ;
#51328 = ORIENTED_EDGE('',*,*,#38349,.F.) ;
#51329 = ORIENTED_EDGE('',*,*,#38104,.F.) ;
#51330 = ORIENTED_EDGE('',*,*,#38348,.T.) ;
#51331 = ORIENTED_EDGE('',*,*,#38266,.F.) ;
#51332 = ORIENTED_EDGE('',*,*,#38350,.F.) ;
#51333 = ORIENTED_EDGE('',*,*,#38261,.F.) ;
#51334 = ORIENTED_EDGE('',*,*,#38349,.T.) ;
#51335 = ORIENTED_EDGE('',*,*,#38258,.F.) ;
#51336 = ORIENTED_EDGE('',*,*,#38351,.F.) ;
#51337 = ORIENTED_EDGE('',*,*,#38262,.F.) ;
#51338 = ORIENTED_EDGE('',*,*,#38350,.T.) ;
#51339 = ORIENTED_EDGE('',*,*,#38100,.F.) ;
#51340 = ORIENTED_EDGE('',*,*,#38352,.F.) ;
#51341 = ORIENTED_EDGE('',*,*,#38056,.F.) ;
#51342 = ORIENTED_EDGE('',*,*,#38351,.T.) ;
#51343 = ORIENTED_EDGE('',*,*,#38086,.F.) ;
#51344 = ORIENTED_EDGE('',*,*,#38353,.F.) ;
#51345 = ORIENTED_EDGE('',*,*,#38082,.F.) ;
#51346 = ORIENTED_EDGE('',*,*,#38352,.T.) ;
#51347 = ORIENTED_EDGE('',*,*,#38273,.F.) ;
#51348 = ORIENTED_EDGE('',*,*,#38353,.T.) ;
#51349 = ORIENTED_EDGE('',*,*,#38274,.F.) ;
#51350 = ORIENTED_EDGE('',*,*,#38354,.T.) ;
#51351 = ORIENTED_EDGE('',*,*,#38277,.F.) ;
#51352 = ORIENTED_EDGE('',*,*,#38355,.F.) ;
#51353 = ORIENTED_EDGE('',*,*,#38279,.F.) ;
#51354 = ORIENTED_EDGE('',*,*,#38354,.F.) ;
#51355 = ORIENTED_EDGE('',*,*,#38032,.F.) ;
#51356 = ORIENTED_EDGE('',*,*,#38356,.F.) ;
#51357 = ORIENTED_EDGE('',*,*,#38050,.F.) ;
#51358 = ORIENTED_EDGE('',*,*,#38355,.T.) ;
#51359 = ORIENTED_EDGE('',*,*,#38047,.F.) ;
#51360 = ORIENTED_EDGE('',*,*,#38357,.F.) ;
#51361 = ORIENTED_EDGE('',*,*,#38092,.F.) ;
#51362 = ORIENTED_EDGE('',*,*,#38356,.T.) ;
#51363 = ORIENTED_EDGE('',*,*,#38290,.F.) ;
#51364 = ORIENTED_EDGE('',*,*,#38358,.F.) ;
#51365 = ORIENTED_EDGE('',*,*,#38286,.F.) ;
#51366 = ORIENTED_EDGE('',*,*,#38357,.T.) ;
#51367 = ORIENTED_EDGE('',*,*,#38278,.F.) ;
#51368 = ORIENTED_EDGE('',*,*,#38359,.F.) ;
#51369 = ORIENTED_EDGE('',*,*,#38281,.F.) ;
#51370 = ORIENTED_EDGE('',*,*,#38358,.T.) ;
#51371 = ORIENTED_EDGE('',*,*,#38096,.F.) ;
#51372 = ORIENTED_EDGE('',*,*,#38360,.F.) ;
#51373 = ORIENTED_EDGE('',*,*,#38044,.F.) ;
#51374 = ORIENTED_EDGE('',*,*,#38359,.T.) ;
#51375 = ORIENTED_EDGE('',*,*,#38053,.F.) ;
#51376 = ORIENTED_EDGE('',*,*,#38361,.F.) ;
#51377 = ORIENTED_EDGE('',*,*,#38040,.F.) ;
#51378 = ORIENTED_EDGE('',*,*,#38360,.T.) ;
#51379 = ORIENTED_EDGE('',*,*,#38292,.F.) ;
#51380 = ORIENTED_EDGE('',*,*,#38361,.T.) ;
#51381 = ORIENTED_EDGE('',*,*,#38287,.F.) ;
#51382 = ORIENTED_EDGE('',*,*,#37794,.F.) ;
#51383 = ORIENTED_EDGE('',*,*,#37764,.F.) ;
#51384 = ORIENTED_EDGE('',*,*,#38362,.F.) ;
#51385 = ORIENTED_EDGE('',*,*,#38113,.F.) ;
#51386 = ORIENTED_EDGE('',*,*,#38362,.T.) ;
#51387 = ORIENTED_EDGE('',*,*,#38215,.F.) ;
#51388 = ORIENTED_EDGE('',*,*,#37732,.F.) ;
#51389 = ORIENTED_EDGE('',*,*,#38363,.F.) ;
#51390 = ORIENTED_EDGE('',*,*,#38363,.T.) ;
#51391 = ORIENTED_EDGE('',*,*,#38111,.F.) ;
#51392 = ORIENTED_EDGE('',*,*,#38364,.F.) ;
#51393 = ORIENTED_EDGE('',*,*,#38114,.F.) ;
#51394 = ORIENTED_EDGE('',*,*,#38317,.F.) ;
#51395 = ORIENTED_EDGE('',*,*,#38315,.F.) ;
#51396 = ORIENTED_EDGE('',*,*,#38364,.T.) ;
#51397 = ORIENTED_EDGE('',*,*,#37848,.F.) ;
#51398 = ORIENTED_EDGE('',*,*,#38365,.F.) ;
#51399 = ORIENTED_EDGE('',*,*,#37843,.F.) ;
#51400 = ORIENTED_EDGE('',*,*,#37806,.F.) ;
#51401 = ORIENTED_EDGE('',*,*,#37847,.F.) ;
#51402 = ORIENTED_EDGE('',*,*,#38336,.F.) ;
#51403 = ORIENTED_EDGE('',*,*,#37709,.F.) ;
#51404 = ORIENTED_EDGE('',*,*,#38366,.F.) ;
#51405 = ORIENTED_EDGE('',*,*,#37844,.F.) ;
#51406 = ORIENTED_EDGE('',*,*,#38365,.T.) ;
#51407 = ORIENTED_EDGE('',*,*,#38366,.T.) ;
#51408 = ORIENTED_EDGE('',*,*,#38021,.F.) ;
#51409 = ORIENTED_EDGE('',*,*,#38367,.F.) ;
#51410 = ORIENTED_EDGE('',*,*,#37845,.F.) ;
#51411 = ORIENTED_EDGE('',*,*,#38327,.F.) ;
#51412 = ORIENTED_EDGE('',*,*,#37749,.F.) ;
#51413 = ORIENTED_EDGE('',*,*,#38368,.F.) ;
#51414 = ORIENTED_EDGE('',*,*,#37840,.F.) ;
#51415 = ORIENTED_EDGE('',*,*,#38367,.T.) ;
#51416 = ORIENTED_EDGE('',*,*,#37778,.F.) ;
#51417 = ORIENTED_EDGE('',*,*,#37841,.F.) ;
#51418 = ORIENTED_EDGE('',*,*,#38368,.T.) ;
#51419 = ORIENTED_EDGE('',*,*,#37748,.F.) ;
#51420 = ORIENTED_EDGE('',*,*,#38369,.T.) ;
#51421 = ORIENTED_EDGE('',*,*,#38370,.T.) ;
#51422 = ORIENTED_EDGE('',*,*,#38371,.T.) ;
#51423 = ORIENTED_EDGE('',*,*,#38372,.F.) ;
#51424 = ORIENTED_EDGE('',*,*,#38373,.F.) ;
#51425 = ORIENTED_EDGE('',*,*,#38374,.T.) ;
#51426 = ORIENTED_EDGE('',*,*,#38375,.T.) ;
#51427 = ORIENTED_EDGE('',*,*,#38376,.F.) ;
#51428 = ORIENTED_EDGE('',*,*,#38377,.F.) ;
#51429 = ORIENTED_EDGE('',*,*,#38378,.F.) ;
#51430 = ORIENTED_EDGE('',*,*,#38379,.F.) ;
#51431 = ORIENTED_EDGE('',*,*,#38380,.T.) ;
#51432 = ORIENTED_EDGE('',*,*,#38381,.F.) ;
#51433 = ORIENTED_EDGE('',*,*,#38380,.F.) ;
#51434 = ORIENTED_EDGE('',*,*,#38382,.F.) ;
#51435 = ORIENTED_EDGE('',*,*,#38383,.T.) ;
#51436 = ORIENTED_EDGE('',*,*,#38384,.F.) ;
#51437 = ORIENTED_EDGE('',*,*,#38383,.F.) ;
#51438 = ORIENTED_EDGE('',*,*,#38385,.F.) ;
#51439 = ORIENTED_EDGE('',*,*,#38386,.F.) ;
#51440 = ORIENTED_EDGE('',*,*,#38387,.T.) ;
#51441 = ORIENTED_EDGE('',*,*,#38388,.T.) ;
#51442 = ORIENTED_EDGE('',*,*,#38389,.F.) ;
#51443 = ORIENTED_EDGE('',*,*,#38390,.F.) ;
#51444 = ORIENTED_EDGE('',*,*,#38391,.F.) ;
#51445 = ORIENTED_EDGE('',*,*,#38392,.T.) ;
#51446 = ORIENTED_EDGE('',*,*,#38393,.F.) ;
#51447 = ORIENTED_EDGE('',*,*,#38394,.F.) ;
#51448 = ORIENTED_EDGE('',*,*,#38395,.T.) ;
#51449 = ORIENTED_EDGE('',*,*,#38396,.F.) ;
#51450 = ORIENTED_EDGE('',*,*,#38397,.T.) ;
#51451 = ORIENTED_EDGE('',*,*,#38381,.T.) ;
#51452 = ORIENTED_EDGE('',*,*,#38398,.T.) ;
#51453 = ORIENTED_EDGE('',*,*,#38382,.T.) ;
#51454 = ORIENTED_EDGE('',*,*,#38398,.F.) ;
#51455 = ORIENTED_EDGE('',*,*,#38394,.T.) ;
#51456 = ORIENTED_EDGE('',*,*,#38399,.T.) ;
#51457 = ORIENTED_EDGE('',*,*,#38400,.T.) ;
#51458 = ORIENTED_EDGE('',*,*,#38391,.T.) ;
#51459 = ORIENTED_EDGE('',*,*,#38401,.F.) ;
#51460 = ORIENTED_EDGE('',*,*,#38402,.T.) ;
#51461 = ORIENTED_EDGE('',*,*,#38403,.F.) ;
#51462 = ORIENTED_EDGE('',*,*,#38389,.T.) ;
#51463 = ORIENTED_EDGE('',*,*,#38404,.T.) ;
#51464 = ORIENTED_EDGE('',*,*,#38405,.T.) ;
#51465 = ORIENTED_EDGE('',*,*,#38406,.T.) ;
#51466 = ORIENTED_EDGE('',*,*,#38407,.T.) ;
#51467 = ORIENTED_EDGE('',*,*,#38408,.T.) ;
#51468 = ORIENTED_EDGE('',*,*,#38409,.T.) ;
#51469 = ORIENTED_EDGE('',*,*,#38410,.T.) ;
#51470 = ORIENTED_EDGE('',*,*,#38411,.T.) ;
#51471 = ORIENTED_EDGE('',*,*,#38412,.T.) ;
#51472 = ORIENTED_EDGE('',*,*,#38413,.T.) ;
#51473 = ORIENTED_EDGE('',*,*,#38414,.T.) ;
#51474 = ORIENTED_EDGE('',*,*,#38415,.T.) ;
#51475 = ORIENTED_EDGE('',*,*,#38416,.T.) ;
#51476 = ORIENTED_EDGE('',*,*,#38417,.T.) ;
#51477 = ORIENTED_EDGE('',*,*,#38418,.T.) ;
#51478 = ORIENTED_EDGE('',*,*,#38419,.T.) ;
#51479 = ORIENTED_EDGE('',*,*,#38420,.T.) ;
#51480 = ORIENTED_EDGE('',*,*,#38421,.T.) ;
#51481 = ORIENTED_EDGE('',*,*,#38422,.T.) ;
#51482 = ORIENTED_EDGE('',*,*,#38423,.T.) ;
#51483 = ORIENTED_EDGE('',*,*,#38424,.T.) ;
#51484 = ORIENTED_EDGE('',*,*,#38425,.T.) ;
#51485 = ORIENTED_EDGE('',*,*,#38426,.T.) ;
#51486 = ORIENTED_EDGE('',*,*,#38427,.T.) ;
#51487 = ORIENTED_EDGE('',*,*,#38428,.T.) ;
#51488 = ORIENTED_EDGE('',*,*,#38429,.T.) ;
#51489 = ORIENTED_EDGE('',*,*,#38430,.T.) ;
#51490 = ORIENTED_EDGE('',*,*,#38431,.T.) ;
#51491 = ORIENTED_EDGE('',*,*,#38432,.F.) ;
#51492 = ORIENTED_EDGE('',*,*,#38433,.T.) ;
#51493 = ORIENTED_EDGE('',*,*,#38434,.T.) ;
#51494 = ORIENTED_EDGE('',*,*,#38435,.T.) ;
#51495 = ORIENTED_EDGE('',*,*,#38436,.F.) ;
#51496 = ORIENTED_EDGE('',*,*,#38437,.T.) ;
#51497 = ORIENTED_EDGE('',*,*,#38438,.T.) ;
#51498 = ORIENTED_EDGE('',*,*,#38439,.T.) ;
#51499 = ORIENTED_EDGE('',*,*,#38440,.T.) ;
#51500 = ORIENTED_EDGE('',*,*,#38441,.T.) ;
#51501 = ORIENTED_EDGE('',*,*,#38442,.F.) ;
#51502 = ORIENTED_EDGE('',*,*,#38443,.T.) ;
#51503 = ORIENTED_EDGE('',*,*,#38412,.F.) ;
#51504 = ORIENTED_EDGE('',*,*,#38444,.T.) ;
#51505 = ORIENTED_EDGE('',*,*,#38418,.F.) ;
#51506 = ORIENTED_EDGE('',*,*,#38445,.T.) ;
#51507 = ORIENTED_EDGE('',*,*,#38426,.F.) ;
#51508 = ORIENTED_EDGE('',*,*,#38446,.T.) ;
#51509 = ORIENTED_EDGE('',*,*,#38447,.F.) ;
#51510 = ORIENTED_EDGE('',*,*,#38448,.T.) ;
#51511 = ORIENTED_EDGE('',*,*,#38449,.F.) ;
#51512 = ORIENTED_EDGE('',*,*,#38450,.T.) ;
#51513 = ORIENTED_EDGE('',*,*,#38451,.T.) ;
#51514 = ORIENTED_EDGE('',*,*,#38452,.T.) ;
#51515 = ORIENTED_EDGE('',*,*,#38453,.F.) ;
#51516 = ORIENTED_EDGE('',*,*,#38454,.T.) ;
#51517 = ORIENTED_EDGE('',*,*,#38455,.T.) ;
#51518 = ORIENTED_EDGE('',*,*,#38456,.T.) ;
#51519 = ORIENTED_EDGE('',*,*,#38457,.F.) ;
#51520 = ORIENTED_EDGE('',*,*,#38458,.T.) ;
#51521 = ORIENTED_EDGE('',*,*,#38430,.F.) ;
#51522 = ORIENTED_EDGE('',*,*,#38459,.T.) ;
#51523 = ORIENTED_EDGE('',*,*,#38460,.T.) ;
#51524 = ORIENTED_EDGE('',*,*,#38461,.T.) ;
#51525 = ORIENTED_EDGE('',*,*,#38438,.F.) ;
#51526 = ORIENTED_EDGE('',*,*,#38462,.T.) ;
#51527 = ORIENTED_EDGE('',*,*,#38463,.F.) ;
#51528 = ORIENTED_EDGE('',*,*,#38464,.F.) ;
#51529 = ORIENTED_EDGE('',*,*,#38465,.T.) ;
#51530 = ORIENTED_EDGE('',*,*,#38466,.F.) ;
#51531 = ORIENTED_EDGE('',*,*,#38467,.T.) ;
#51532 = ORIENTED_EDGE('',*,*,#38468,.F.) ;
#51533 = ORIENTED_EDGE('',*,*,#38469,.T.) ;
#51534 = ORIENTED_EDGE('',*,*,#38470,.T.) ;
#51535 = ORIENTED_EDGE('',*,*,#38471,.T.) ;
#51536 = ORIENTED_EDGE('',*,*,#38472,.T.) ;
#51537 = ORIENTED_EDGE('',*,*,#38473,.T.) ;
#51538 = ORIENTED_EDGE('',*,*,#38474,.T.) ;
#51539 = ORIENTED_EDGE('',*,*,#38475,.T.) ;
#51540 = ORIENTED_EDGE('',*,*,#38476,.T.) ;
#51541 = ORIENTED_EDGE('',*,*,#38477,.T.) ;
#51542 = ORIENTED_EDGE('',*,*,#38478,.T.) ;
#51543 = ORIENTED_EDGE('',*,*,#38479,.T.) ;
#51544 = ORIENTED_EDGE('',*,*,#38480,.T.) ;
#51545 = ORIENTED_EDGE('',*,*,#38436,.T.) ;
#51546 = ORIENTED_EDGE('',*,*,#38481,.T.) ;
#51547 = ORIENTED_EDGE('',*,*,#38482,.T.) ;
#51548 = ORIENTED_EDGE('',*,*,#38483,.T.) ;
#51549 = ORIENTED_EDGE('',*,*,#38432,.T.) ;
#51550 = ORIENTED_EDGE('',*,*,#38484,.T.) ;
#51551 = ORIENTED_EDGE('',*,*,#38485,.F.) ;
#51552 = ORIENTED_EDGE('',*,*,#38486,.T.) ;
#51553 = ORIENTED_EDGE('',*,*,#38487,.F.) ;
#51554 = ORIENTED_EDGE('',*,*,#38488,.T.) ;
#51555 = ORIENTED_EDGE('',*,*,#38489,.T.) ;
#51556 = ORIENTED_EDGE('',*,*,#38490,.T.) ;
#51557 = ORIENTED_EDGE('',*,*,#38491,.F.) ;
#51558 = ORIENTED_EDGE('',*,*,#38492,.T.) ;
#51559 = ORIENTED_EDGE('',*,*,#38493,.F.) ;
#51560 = ORIENTED_EDGE('',*,*,#38494,.T.) ;
#51561 = ORIENTED_EDGE('',*,*,#38495,.T.) ;
#51562 = ORIENTED_EDGE('',*,*,#38496,.T.) ;
#51563 = ORIENTED_EDGE('',*,*,#38497,.T.) ;
#51564 = ORIENTED_EDGE('',*,*,#38498,.T.) ;
#51565 = ORIENTED_EDGE('',*,*,#38499,.T.) ;
#51566 = ORIENTED_EDGE('',*,*,#38500,.T.) ;
#51567 = ORIENTED_EDGE('',*,*,#38466,.T.) ;
#51568 = ORIENTED_EDGE('',*,*,#38501,.T.) ;
#51569 = ORIENTED_EDGE('',*,*,#38476,.F.) ;
#51570 = ORIENTED_EDGE('',*,*,#38502,.T.) ;
#51571 = ORIENTED_EDGE('',*,*,#38468,.T.) ;
#51572 = ORIENTED_EDGE('',*,*,#38503,.T.) ;
#51573 = ORIENTED_EDGE('',*,*,#38474,.F.) ;
#51574 = ORIENTED_EDGE('',*,*,#38504,.T.) ;
#51575 = ORIENTED_EDGE('',*,*,#38505,.T.) ;
#51576 = ORIENTED_EDGE('',*,*,#38506,.T.) ;
#51577 = ORIENTED_EDGE('',*,*,#38442,.T.) ;
#51578 = ORIENTED_EDGE('',*,*,#38507,.T.) ;
#51579 = ORIENTED_EDGE('',*,*,#38472,.F.) ;
#51580 = ORIENTED_EDGE('',*,*,#38508,.T.) ;
#51581 = ORIENTED_EDGE('',*,*,#38509,.T.) ;
#51582 = ORIENTED_EDGE('',*,*,#38510,.T.) ;
#51583 = ORIENTED_EDGE('',*,*,#38511,.T.) ;
#51584 = ORIENTED_EDGE('',*,*,#38512,.T.) ;
#51585 = ORIENTED_EDGE('',*,*,#38513,.T.) ;
#51586 = ORIENTED_EDGE('',*,*,#38470,.F.) ;
#51587 = ORIENTED_EDGE('',*,*,#38514,.T.) ;
#51588 = ORIENTED_EDGE('',*,*,#38515,.T.) ;
#51589 = ORIENTED_EDGE('',*,*,#38516,.T.) ;
#51590 = ORIENTED_EDGE('',*,*,#38517,.T.) ;
#51591 = ORIENTED_EDGE('',*,*,#38499,.F.) ;
#51592 = ORIENTED_EDGE('',*,*,#38518,.T.) ;
#51593 = ORIENTED_EDGE('',*,*,#38519,.T.) ;
#51594 = ORIENTED_EDGE('',*,*,#38373,.T.) ;
#51595 = ORIENTED_EDGE('',*,*,#38520,.T.) ;
#51596 = ORIENTED_EDGE('',*,*,#38521,.T.) ;
#51597 = ORIENTED_EDGE('',*,*,#38497,.F.) ;
#51598 = ORIENTED_EDGE('',*,*,#38522,.T.) ;
#51599 = ORIENTED_EDGE('',*,*,#38523,.T.) ;
#51600 = ORIENTED_EDGE('',*,*,#38524,.T.) ;
#51601 = ORIENTED_EDGE('',*,*,#38525,.T.) ;
#51602 = ORIENTED_EDGE('',*,*,#38526,.T.) ;
#51603 = ORIENTED_EDGE('',*,*,#38527,.T.) ;
#51604 = ORIENTED_EDGE('',*,*,#38495,.F.) ;
#51605 = ORIENTED_EDGE('',*,*,#38528,.T.) ;
#51606 = ORIENTED_EDGE('',*,*,#38529,.T.) ;
#51607 = ORIENTED_EDGE('',*,*,#38530,.F.) ;
#51608 = ORIENTED_EDGE('',*,*,#38531,.T.) ;
#51609 = ORIENTED_EDGE('',*,*,#38532,.F.) ;
#51610 = ORIENTED_EDGE('',*,*,#38533,.T.) ;
#51611 = ORIENTED_EDGE('',*,*,#38534,.T.) ;
#51612 = ORIENTED_EDGE('',*,*,#38447,.T.) ;
#51613 = ORIENTED_EDGE('',*,*,#38535,.F.) ;
#51614 = ORIENTED_EDGE('',*,*,#38536,.T.) ;
#51615 = ORIENTED_EDGE('',*,*,#38453,.T.) ;
#51616 = ORIENTED_EDGE('',*,*,#38537,.T.) ;
#51617 = ORIENTED_EDGE('',*,*,#38538,.F.) ;
#51618 = ORIENTED_EDGE('',*,*,#38539,.T.) ;
#51619 = ORIENTED_EDGE('',*,*,#38540,.F.) ;
#51620 = ORIENTED_EDGE('',*,*,#38541,.T.) ;
#51621 = ORIENTED_EDGE('',*,*,#38542,.T.) ;
#51622 = ORIENTED_EDGE('',*,*,#38543,.T.) ;
#51623 = ORIENTED_EDGE('',*,*,#38544,.F.) ;
#51624 = ORIENTED_EDGE('',*,*,#38545,.T.) ;
#51625 = ORIENTED_EDGE('',*,*,#38546,.F.) ;
#51626 = ORIENTED_EDGE('',*,*,#38547,.T.) ;
#51627 = ORIENTED_EDGE('',*,*,#38489,.F.) ;
#51628 = ORIENTED_EDGE('',*,*,#38548,.T.) ;
#51629 = ORIENTED_EDGE('',*,*,#38549,.F.) ;
#51630 = ORIENTED_EDGE('',*,*,#38550,.T.) ;
#51631 = ORIENTED_EDGE('',*,*,#38551,.F.) ;
#51632 = ORIENTED_EDGE('',*,*,#38552,.T.) ;
#51633 = ORIENTED_EDGE('',*,*,#38553,.T.) ;
#51634 = ORIENTED_EDGE('',*,*,#38554,.T.) ;
#51635 = ORIENTED_EDGE('',*,*,#38555,.F.) ;
#51636 = ORIENTED_EDGE('',*,*,#38556,.T.) ;
#51637 = ORIENTED_EDGE('',*,*,#38384,.T.) ;
#51638 = ORIENTED_EDGE('',*,*,#38557,.F.) ;
#51639 = ORIENTED_EDGE('',*,*,#38558,.T.) ;
#51640 = ORIENTED_EDGE('',*,*,#38559,.F.) ;
#51641 = ORIENTED_EDGE('',*,*,#38463,.T.) ;
#51642 = ORIENTED_EDGE('',*,*,#38560,.T.) ;
#51643 = ORIENTED_EDGE('',*,*,#38479,.F.) ;
#51644 = ORIENTED_EDGE('',*,*,#38561,.F.) ;
#51645 = ORIENTED_EDGE('',*,*,#38562,.T.) ;
#51646 = ORIENTED_EDGE('',*,*,#38563,.F.) ;
#51647 = ORIENTED_EDGE('',*,*,#38564,.T.) ;
#51648 = ORIENTED_EDGE('',*,*,#38565,.F.) ;
#51649 = ORIENTED_EDGE('',*,*,#38566,.T.) ;
#51650 = ORIENTED_EDGE('',*,*,#38561,.T.) ;
#51651 = ORIENTED_EDGE('',*,*,#38478,.F.) ;
#51652 = ORIENTED_EDGE('',*,*,#38567,.T.) ;
#51653 = ORIENTED_EDGE('',*,*,#38464,.T.) ;
#51654 = ORIENTED_EDGE('',*,*,#38559,.T.) ;
#51655 = ORIENTED_EDGE('',*,*,#38568,.T.) ;
#51656 = ORIENTED_EDGE('',*,*,#38569,.F.) ;
#51657 = ORIENTED_EDGE('',*,*,#38570,.T.) ;
#51658 = ORIENTED_EDGE('',*,*,#38571,.T.) ;
#51659 = ORIENTED_EDGE('',*,*,#38572,.T.) ;
#51660 = ORIENTED_EDGE('',*,*,#38573,.F.) ;
#51661 = ORIENTED_EDGE('',*,*,#38574,.F.) ;
#51662 = ORIENTED_EDGE('',*,*,#38575,.T.) ;
#51663 = ORIENTED_EDGE('',*,*,#38576,.T.) ;
#51664 = ORIENTED_EDGE('',*,*,#38577,.T.) ;
#51665 = ORIENTED_EDGE('',*,*,#38578,.T.) ;
#51666 = ORIENTED_EDGE('',*,*,#38579,.T.) ;
#51667 = ORIENTED_EDGE('',*,*,#38580,.T.) ;
#51668 = ORIENTED_EDGE('',*,*,#38581,.T.) ;
#51669 = ORIENTED_EDGE('',*,*,#38582,.T.) ;
#51670 = ORIENTED_EDGE('',*,*,#38583,.T.) ;
#51671 = ORIENTED_EDGE('',*,*,#38584,.T.) ;
#51672 = ORIENTED_EDGE('',*,*,#38585,.T.) ;
#51673 = ORIENTED_EDGE('',*,*,#38586,.T.) ;
#51674 = ORIENTED_EDGE('',*,*,#38587,.T.) ;
#51675 = ORIENTED_EDGE('',*,*,#38588,.T.) ;
#51676 = ORIENTED_EDGE('',*,*,#38589,.T.) ;
#51677 = ORIENTED_EDGE('',*,*,#38590,.T.) ;
#51678 = ORIENTED_EDGE('',*,*,#38591,.T.) ;
#51679 = ORIENTED_EDGE('',*,*,#38592,.T.) ;
#51680 = ORIENTED_EDGE('',*,*,#38593,.T.) ;
#51681 = ORIENTED_EDGE('',*,*,#38594,.T.) ;
#51682 = ORIENTED_EDGE('',*,*,#38595,.T.) ;
#51683 = ORIENTED_EDGE('',*,*,#38596,.T.) ;
#51684 = ORIENTED_EDGE('',*,*,#38597,.T.) ;
#51685 = ORIENTED_EDGE('',*,*,#38598,.T.) ;
#51686 = ORIENTED_EDGE('',*,*,#38599,.T.) ;
#51687 = ORIENTED_EDGE('',*,*,#38600,.T.) ;
#51688 = ORIENTED_EDGE('',*,*,#38601,.T.) ;
#51689 = ORIENTED_EDGE('',*,*,#38602,.T.) ;
#51690 = ORIENTED_EDGE('',*,*,#38603,.T.) ;
#51691 = ORIENTED_EDGE('',*,*,#38604,.T.) ;
#51692 = ORIENTED_EDGE('',*,*,#38605,.T.) ;
#51693 = ORIENTED_EDGE('',*,*,#38606,.T.) ;
#51694 = ORIENTED_EDGE('',*,*,#38607,.T.) ;
#51695 = ORIENTED_EDGE('',*,*,#38608,.T.) ;
#51696 = ORIENTED_EDGE('',*,*,#38609,.T.) ;
#51697 = ORIENTED_EDGE('',*,*,#38610,.T.) ;
#51698 = ORIENTED_EDGE('',*,*,#38379,.T.) ;
#51699 = ORIENTED_EDGE('',*,*,#38611,.F.) ;
#51700 = ORIENTED_EDGE('',*,*,#38612,.T.) ;
#51701 = ORIENTED_EDGE('',*,*,#38613,.T.) ;
#51702 = ORIENTED_EDGE('',*,*,#38614,.T.) ;
#51703 = ORIENTED_EDGE('',*,*,#38615,.T.) ;
#51704 = ORIENTED_EDGE('',*,*,#38616,.T.) ;
#51705 = ORIENTED_EDGE('',*,*,#38617,.T.) ;
#51706 = ORIENTED_EDGE('',*,*,#38618,.T.) ;
#51707 = ORIENTED_EDGE('',*,*,#38619,.F.) ;
#51708 = ORIENTED_EDGE('',*,*,#38620,.T.) ;
#51709 = ORIENTED_EDGE('',*,*,#38457,.T.) ;
#51710 = ORIENTED_EDGE('',*,*,#38621,.T.) ;
#51711 = ORIENTED_EDGE('',*,*,#38622,.T.) ;
#51712 = ORIENTED_EDGE('',*,*,#38623,.T.) ;
#51713 = ORIENTED_EDGE('',*,*,#38624,.T.) ;
#51714 = ORIENTED_EDGE('',*,*,#38455,.F.) ;
#51715 = ORIENTED_EDGE('',*,*,#38625,.T.) ;
#51716 = ORIENTED_EDGE('',*,*,#38626,.T.) ;
#51717 = ORIENTED_EDGE('',*,*,#38627,.T.) ;
#51718 = ORIENTED_EDGE('',*,*,#38628,.T.) ;
#51719 = ORIENTED_EDGE('',*,*,#38629,.T.) ;
#51720 = ORIENTED_EDGE('',*,*,#38393,.T.) ;
#51721 = ORIENTED_EDGE('',*,*,#38630,.T.) ;
#51722 = ORIENTED_EDGE('',*,*,#38631,.T.) ;
#51723 = ORIENTED_EDGE('',*,*,#38632,.T.) ;
#51724 = ORIENTED_EDGE('',*,*,#38633,.T.) ;
#51725 = ORIENTED_EDGE('',*,*,#38634,.T.) ;
#51726 = ORIENTED_EDGE('',*,*,#38635,.T.) ;
#51727 = ORIENTED_EDGE('',*,*,#38636,.T.) ;
#51728 = ORIENTED_EDGE('',*,*,#38637,.T.) ;
#51729 = ORIENTED_EDGE('',*,*,#38638,.T.) ;
#51730 = ORIENTED_EDGE('',*,*,#38386,.T.) ;
#51731 = ORIENTED_EDGE('',*,*,#38639,.T.) ;
#51732 = ORIENTED_EDGE('',*,*,#38640,.T.) ;
#51733 = ORIENTED_EDGE('',*,*,#38641,.T.) ;
#51734 = ORIENTED_EDGE('',*,*,#38642,.T.) ;
#51735 = ORIENTED_EDGE('',*,*,#38643,.T.) ;
#51736 = ORIENTED_EDGE('',*,*,#38487,.T.) ;
#51737 = ORIENTED_EDGE('',*,*,#38644,.T.) ;
#51738 = ORIENTED_EDGE('',*,*,#38645,.T.) ;
#51739 = ORIENTED_EDGE('',*,*,#38646,.T.) ;
#51740 = ORIENTED_EDGE('',*,*,#38485,.T.) ;
#51741 = ORIENTED_EDGE('',*,*,#38647,.T.) ;
#51742 = ORIENTED_EDGE('',*,*,#38648,.F.) ;
#51743 = ORIENTED_EDGE('',*,*,#38649,.T.) ;
#51744 = ORIENTED_EDGE('',*,*,#38650,.T.) ;
#51745 = ORIENTED_EDGE('',*,*,#38651,.T.) ;
#51746 = ORIENTED_EDGE('',*,*,#38652,.T.) ;
#51747 = ORIENTED_EDGE('',*,*,#38449,.T.) ;
#51748 = ORIENTED_EDGE('',*,*,#38653,.T.) ;
#51749 = ORIENTED_EDGE('',*,*,#38654,.T.) ;
#51750 = ORIENTED_EDGE('',*,*,#38655,.T.) ;
#51751 = ORIENTED_EDGE('',*,*,#38656,.T.) ;
#51752 = ORIENTED_EDGE('',*,*,#38451,.F.) ;
#51753 = ORIENTED_EDGE('',*,*,#38657,.T.) ;
#51754 = ORIENTED_EDGE('',*,*,#38658,.T.) ;
#51755 = ORIENTED_EDGE('',*,*,#38659,.T.) ;
#51756 = ORIENTED_EDGE('',*,*,#38660,.T.) ;
#51757 = ORIENTED_EDGE('',*,*,#38661,.T.) ;
#51758 = ORIENTED_EDGE('',*,*,#38662,.T.) ;
#51759 = ORIENTED_EDGE('',*,*,#38663,.T.) ;
#51760 = ORIENTED_EDGE('',*,*,#38664,.T.) ;
#51761 = ORIENTED_EDGE('',*,*,#38665,.T.) ;
#51762 = ORIENTED_EDGE('',*,*,#38666,.T.) ;
#51763 = ORIENTED_EDGE('',*,*,#38667,.T.) ;
#51764 = ORIENTED_EDGE('',*,*,#38668,.T.) ;
#51765 = ORIENTED_EDGE('',*,*,#38669,.T.) ;
#51766 = ORIENTED_EDGE('',*,*,#38491,.T.) ;
#51767 = ORIENTED_EDGE('',*,*,#38670,.T.) ;
#51768 = ORIENTED_EDGE('',*,*,#38671,.T.) ;
#51769 = ORIENTED_EDGE('',*,*,#38672,.T.) ;
#51770 = ORIENTED_EDGE('',*,*,#38673,.T.) ;
#51771 = ORIENTED_EDGE('',*,*,#38674,.T.) ;
#51772 = ORIENTED_EDGE('',*,*,#38675,.T.) ;
#51773 = ORIENTED_EDGE('',*,*,#38676,.T.) ;
#51774 = ORIENTED_EDGE('',*,*,#38677,.T.) ;
#51775 = ORIENTED_EDGE('',*,*,#38678,.T.) ;
#51776 = ORIENTED_EDGE('',*,*,#38493,.T.) ;
#51777 = ORIENTED_EDGE('',*,*,#38679,.T.) ;
#51778 = ORIENTED_EDGE('',*,*,#38680,.T.) ;
#51779 = ORIENTED_EDGE('',*,*,#38681,.T.) ;
#51780 = ORIENTED_EDGE('',*,*,#38682,.T.) ;
#51781 = ORIENTED_EDGE('',*,*,#38683,.T.) ;
#51782 = ORIENTED_EDGE('',*,*,#38684,.T.) ;
#51783 = ORIENTED_EDGE('',*,*,#38685,.T.) ;
#51784 = ORIENTED_EDGE('',*,*,#38686,.T.) ;
#51785 = ORIENTED_EDGE('',*,*,#38378,.T.) ;
#51786 = ORIENTED_EDGE('',*,*,#38687,.T.) ;
#51787 = ORIENTED_EDGE('',*,*,#38688,.T.) ;
#51788 = ORIENTED_EDGE('',*,*,#38689,.T.) ;
#51789 = ORIENTED_EDGE('',*,*,#38690,.T.) ;
#51790 = ORIENTED_EDGE('',*,*,#38691,.T.) ;
#51791 = ORIENTED_EDGE('',*,*,#38692,.T.) ;
#51792 = ORIENTED_EDGE('',*,*,#38693,.T.) ;
#51793 = ORIENTED_EDGE('',*,*,#38694,.T.) ;
#51794 = ORIENTED_EDGE('',*,*,#38695,.T.) ;
#51795 = ORIENTED_EDGE('',*,*,#38696,.T.) ;
#51796 = ORIENTED_EDGE('',*,*,#38697,.T.) ;
#51797 = ORIENTED_EDGE('',*,*,#38698,.T.) ;
#51798 = ORIENTED_EDGE('',*,*,#38699,.T.) ;
#51799 = ORIENTED_EDGE('',*,*,#38700,.T.) ;
#51800 = ORIENTED_EDGE('',*,*,#38701,.T.) ;
#51801 = ORIENTED_EDGE('',*,*,#38702,.T.) ;
#51802 = ORIENTED_EDGE('',*,*,#38703,.T.) ;
#51803 = ORIENTED_EDGE('',*,*,#38704,.T.) ;
#51804 = ORIENTED_EDGE('',*,*,#38705,.T.) ;
#51805 = ORIENTED_EDGE('',*,*,#38706,.T.) ;
#51806 = ORIENTED_EDGE('',*,*,#38707,.T.) ;
#51807 = ORIENTED_EDGE('',*,*,#38708,.T.) ;
#51808 = ORIENTED_EDGE('',*,*,#38709,.T.) ;
#51809 = ORIENTED_EDGE('',*,*,#38710,.T.) ;
#51810 = ORIENTED_EDGE('',*,*,#38611,.T.) ;
#51811 = ORIENTED_EDGE('',*,*,#38711,.T.) ;
#51812 = ORIENTED_EDGE('',*,*,#38712,.T.) ;
#51813 = ORIENTED_EDGE('',*,*,#38713,.T.) ;
#51814 = ORIENTED_EDGE('',*,*,#38615,.F.) ;
#51815 = ORIENTED_EDGE('',*,*,#38714,.T.) ;
#51816 = ORIENTED_EDGE('',*,*,#38715,.T.) ;
#51817 = ORIENTED_EDGE('',*,*,#38716,.T.) ;
#51818 = ORIENTED_EDGE('',*,*,#38617,.F.) ;
#51819 = ORIENTED_EDGE('',*,*,#38717,.T.) ;
#51820 = ORIENTED_EDGE('',*,*,#38718,.T.) ;
#51821 = ORIENTED_EDGE('',*,*,#38719,.T.) ;
#51822 = ORIENTED_EDGE('',*,*,#38613,.F.) ;
#51823 = ORIENTED_EDGE('',*,*,#38720,.T.) ;
#51824 = ORIENTED_EDGE('',*,*,#38721,.T.) ;
#51825 = ORIENTED_EDGE('',*,*,#38722,.T.) ;
#51826 = ORIENTED_EDGE('',*,*,#38723,.T.) ;
#51827 = ORIENTED_EDGE('',*,*,#38724,.T.) ;
#51828 = ORIENTED_EDGE('',*,*,#38725,.T.) ;
#51829 = ORIENTED_EDGE('',*,*,#38726,.T.) ;
#51830 = ORIENTED_EDGE('',*,*,#38727,.T.) ;
#51831 = ORIENTED_EDGE('',*,*,#38728,.T.) ;
#51832 = ORIENTED_EDGE('',*,*,#38729,.T.) ;
#51833 = ORIENTED_EDGE('',*,*,#38730,.T.) ;
#51834 = ORIENTED_EDGE('',*,*,#38731,.T.) ;
#51835 = ORIENTED_EDGE('',*,*,#38732,.F.) ;
#51836 = ORIENTED_EDGE('',*,*,#38733,.T.) ;
#51837 = ORIENTED_EDGE('',*,*,#38409,.F.) ;
#51838 = ORIENTED_EDGE('',*,*,#38734,.T.) ;
#51839 = ORIENTED_EDGE('',*,*,#38735,.T.) ;
#51840 = ORIENTED_EDGE('',*,*,#38736,.T.) ;
#51841 = ORIENTED_EDGE('',*,*,#38737,.T.) ;
#51842 = ORIENTED_EDGE('',*,*,#38732,.T.) ;
#51843 = ORIENTED_EDGE('',*,*,#38738,.T.) ;
#51844 = ORIENTED_EDGE('',*,*,#38739,.T.) ;
#51845 = ORIENTED_EDGE('',*,*,#38740,.T.) ;
#51846 = ORIENTED_EDGE('',*,*,#38741,.T.) ;
#51847 = ORIENTED_EDGE('',*,*,#38742,.T.) ;
#51848 = ORIENTED_EDGE('',*,*,#38743,.T.) ;
#51849 = ORIENTED_EDGE('',*,*,#38744,.T.) ;
#51850 = ORIENTED_EDGE('',*,*,#38745,.T.) ;
#51851 = ORIENTED_EDGE('',*,*,#38746,.T.) ;
#51852 = ORIENTED_EDGE('',*,*,#38747,.T.) ;
#51853 = ORIENTED_EDGE('',*,*,#38748,.T.) ;
#51854 = ORIENTED_EDGE('',*,*,#38749,.T.) ;
#51855 = ORIENTED_EDGE('',*,*,#38750,.T.) ;
#51856 = ORIENTED_EDGE('',*,*,#38751,.T.) ;
#51857 = ORIENTED_EDGE('',*,*,#38752,.T.) ;
#51858 = ORIENTED_EDGE('',*,*,#38753,.F.) ;
#51859 = ORIENTED_EDGE('',*,*,#38602,.F.) ;
#51860 = ORIENTED_EDGE('',*,*,#38754,.T.) ;
#51861 = ORIENTED_EDGE('',*,*,#38753,.T.) ;
#51862 = ORIENTED_EDGE('',*,*,#38755,.T.) ;
#51863 = ORIENTED_EDGE('',*,*,#38756,.T.) ;
#51864 = ORIENTED_EDGE('',*,*,#38757,.T.) ;
#51865 = ORIENTED_EDGE('',*,*,#38758,.T.) ;
#51866 = ORIENTED_EDGE('',*,*,#38759,.T.) ;
#51867 = ORIENTED_EDGE('',*,*,#38760,.T.) ;
#51868 = ORIENTED_EDGE('',*,*,#38761,.T.) ;
#51869 = ORIENTED_EDGE('',*,*,#38762,.T.) ;
#51870 = ORIENTED_EDGE('',*,*,#38763,.T.) ;
#51871 = ORIENTED_EDGE('',*,*,#38764,.T.) ;
#51872 = ORIENTED_EDGE('',*,*,#38765,.T.) ;
#51873 = ORIENTED_EDGE('',*,*,#38766,.T.) ;
#51874 = ORIENTED_EDGE('',*,*,#38767,.T.) ;
#51875 = ORIENTED_EDGE('',*,*,#38768,.T.) ;
#51876 = ORIENTED_EDGE('',*,*,#38769,.T.) ;
#51877 = ORIENTED_EDGE('',*,*,#38770,.T.) ;
#51878 = ORIENTED_EDGE('',*,*,#38771,.T.) ;
#51879 = ORIENTED_EDGE('',*,*,#38772,.T.) ;
#51880 = ORIENTED_EDGE('',*,*,#38773,.T.) ;
#51881 = ORIENTED_EDGE('',*,*,#38774,.T.) ;
#51882 = ORIENTED_EDGE('',*,*,#38482,.F.) ;
#51883 = ORIENTED_EDGE('',*,*,#38775,.T.) ;
#51884 = ORIENTED_EDGE('',*,*,#38776,.T.) ;
#51885 = ORIENTED_EDGE('',*,*,#38396,.T.) ;
#51886 = ORIENTED_EDGE('',*,*,#38777,.T.) ;
#51887 = ORIENTED_EDGE('',*,*,#38460,.F.) ;
#51888 = ORIENTED_EDGE('',*,*,#38778,.T.) ;
#51889 = ORIENTED_EDGE('',*,*,#38779,.T.) ;
#51890 = ORIENTED_EDGE('',*,*,#38780,.T.) ;
#51891 = ORIENTED_EDGE('',*,*,#38781,.F.) ;
#51892 = ORIENTED_EDGE('',*,*,#38679,.F.) ;
#51893 = ORIENTED_EDGE('',*,*,#38492,.F.) ;
#51894 = ORIENTED_EDGE('',*,*,#38672,.F.) ;
#51895 = ORIENTED_EDGE('',*,*,#38782,.F.) ;
#51896 = ORIENTED_EDGE('',*,*,#38781,.T.) ;
#51897 = ORIENTED_EDGE('',*,*,#38783,.F.) ;
#51898 = ORIENTED_EDGE('',*,*,#38490,.F.) ;
#51899 = ORIENTED_EDGE('',*,*,#38547,.F.) ;
#51900 = ORIENTED_EDGE('',*,*,#38784,.F.) ;
#51901 = ORIENTED_EDGE('',*,*,#38670,.F.) ;
#51902 = ORIENTED_EDGE('',*,*,#38783,.T.) ;
#51903 = ORIENTED_EDGE('',*,*,#38671,.F.) ;
#51904 = ORIENTED_EDGE('',*,*,#38785,.F.) ;
#51905 = ORIENTED_EDGE('',*,*,#38667,.F.) ;
#51906 = ORIENTED_EDGE('',*,*,#38782,.T.) ;
#51907 = ORIENTED_EDGE('',*,*,#38666,.F.) ;
#51908 = ORIENTED_EDGE('',*,*,#38786,.F.) ;
#51909 = ORIENTED_EDGE('',*,*,#38680,.F.) ;
#51910 = ORIENTED_EDGE('',*,*,#38784,.T.) ;
#51911 = ORIENTED_EDGE('',*,*,#38546,.T.) ;
#51912 = ORIENTED_EDGE('',*,*,#38787,.F.) ;
#51913 = ORIENTED_EDGE('',*,*,#38785,.T.) ;
#51914 = ORIENTED_EDGE('',*,*,#38788,.F.) ;
#51915 = ORIENTED_EDGE('',*,*,#38786,.T.) ;
#51916 = ORIENTED_EDGE('',*,*,#38789,.F.) ;
#51917 = ORIENTED_EDGE('',*,*,#38450,.F.) ;
#51918 = ORIENTED_EDGE('',*,*,#38652,.F.) ;
#51919 = ORIENTED_EDGE('',*,*,#38790,.F.) ;
#51920 = ORIENTED_EDGE('',*,*,#38657,.F.) ;
#51921 = ORIENTED_EDGE('',*,*,#38791,.F.) ;
#51922 = ORIENTED_EDGE('',*,*,#38655,.F.) ;
#51923 = ORIENTED_EDGE('',*,*,#38792,.F.) ;
#51924 = ORIENTED_EDGE('',*,*,#38661,.F.) ;
#51925 = ORIENTED_EDGE('',*,*,#38452,.F.) ;
#51926 = ORIENTED_EDGE('',*,*,#38656,.F.) ;
#51927 = ORIENTED_EDGE('',*,*,#38793,.F.) ;
#51928 = ORIENTED_EDGE('',*,*,#38537,.F.) ;
#51929 = ORIENTED_EDGE('',*,*,#38787,.T.) ;
#51930 = ORIENTED_EDGE('',*,*,#38545,.F.) ;
#51931 = ORIENTED_EDGE('',*,*,#38794,.F.) ;
#51932 = ORIENTED_EDGE('',*,*,#38668,.F.) ;
#51933 = ORIENTED_EDGE('',*,*,#38789,.T.) ;
#51934 = ORIENTED_EDGE('',*,*,#38669,.F.) ;
#51935 = ORIENTED_EDGE('',*,*,#38795,.F.) ;
#51936 = ORIENTED_EDGE('',*,*,#38676,.F.) ;
#51937 = ORIENTED_EDGE('',*,*,#38788,.T.) ;
#51938 = ORIENTED_EDGE('',*,*,#38675,.F.) ;
#51939 = ORIENTED_EDGE('',*,*,#38796,.F.) ;
#51940 = ORIENTED_EDGE('',*,*,#38677,.F.) ;
#51941 = ORIENTED_EDGE('',*,*,#38494,.F.) ;
#51942 = ORIENTED_EDGE('',*,*,#38678,.F.) ;
#51943 = ORIENTED_EDGE('',*,*,#38797,.F.) ;
#51944 = ORIENTED_EDGE('',*,*,#38528,.F.) ;
#51945 = ORIENTED_EDGE('',*,*,#38792,.T.) ;
#51946 = ORIENTED_EDGE('',*,*,#38790,.T.) ;
#51947 = ORIENTED_EDGE('',*,*,#38798,.F.) ;
#51948 = ORIENTED_EDGE('',*,*,#38793,.T.) ;
#51949 = ORIENTED_EDGE('',*,*,#38791,.T.) ;
#51950 = ORIENTED_EDGE('',*,*,#38799,.F.) ;
#51951 = ORIENTED_EDGE('',*,*,#38538,.T.) ;
#51952 = ORIENTED_EDGE('',*,*,#38794,.T.) ;
#51953 = ORIENTED_EDGE('',*,*,#38544,.T.) ;
#51954 = ORIENTED_EDGE('',*,*,#38800,.F.) ;
#51955 = ORIENTED_EDGE('',*,*,#38795,.T.) ;
#51956 = ORIENTED_EDGE('',*,*,#38797,.T.) ;
#51957 = ORIENTED_EDGE('',*,*,#38796,.T.) ;
#51958 = ORIENTED_EDGE('',*,*,#38801,.F.) ;
#51959 = ORIENTED_EDGE('',*,*,#38798,.T.) ;
#51960 = ORIENTED_EDGE('',*,*,#38651,.F.) ;
#51961 = ORIENTED_EDGE('',*,*,#38802,.F.) ;
#51962 = ORIENTED_EDGE('',*,*,#38658,.F.) ;
#51963 = ORIENTED_EDGE('',*,*,#38803,.F.) ;
#51964 = ORIENTED_EDGE('',*,*,#38659,.F.) ;
#51965 = ORIENTED_EDGE('',*,*,#38804,.F.) ;
#51966 = ORIENTED_EDGE('',*,*,#38665,.F.) ;
#51967 = ORIENTED_EDGE('',*,*,#38799,.T.) ;
#51968 = ORIENTED_EDGE('',*,*,#38660,.F.) ;
#51969 = ORIENTED_EDGE('',*,*,#38805,.F.) ;
#51970 = ORIENTED_EDGE('',*,*,#38539,.F.) ;
#51971 = ORIENTED_EDGE('',*,*,#38800,.T.) ;
#51972 = ORIENTED_EDGE('',*,*,#38543,.F.) ;
#51973 = ORIENTED_EDGE('',*,*,#38806,.F.) ;
#51974 = ORIENTED_EDGE('',*,*,#38673,.F.) ;
#51975 = ORIENTED_EDGE('',*,*,#38801,.T.) ;
#51976 = ORIENTED_EDGE('',*,*,#38674,.F.) ;
#51977 = ORIENTED_EDGE('',*,*,#38807,.F.) ;
#51978 = ORIENTED_EDGE('',*,*,#38529,.F.) ;
#51979 = ORIENTED_EDGE('',*,*,#38804,.T.) ;
#51980 = ORIENTED_EDGE('',*,*,#38802,.T.) ;
#51981 = ORIENTED_EDGE('',*,*,#38808,.F.) ;
#51982 = ORIENTED_EDGE('',*,*,#38805,.T.) ;
#51983 = ORIENTED_EDGE('',*,*,#38803,.T.) ;
#51984 = ORIENTED_EDGE('',*,*,#38809,.F.) ;
#51985 = ORIENTED_EDGE('',*,*,#38540,.T.) ;
#51986 = ORIENTED_EDGE('',*,*,#38807,.T.) ;
#51987 = ORIENTED_EDGE('',*,*,#38806,.T.) ;
#51988 = ORIENTED_EDGE('',*,*,#38810,.F.) ;
#51989 = ORIENTED_EDGE('',*,*,#38530,.T.) ;
#51990 = ORIENTED_EDGE('',*,*,#38448,.F.) ;
#51991 = ORIENTED_EDGE('',*,*,#38534,.F.) ;
#51992 = ORIENTED_EDGE('',*,*,#38811,.F.) ;
#51993 = ORIENTED_EDGE('',*,*,#38653,.F.) ;
#51994 = ORIENTED_EDGE('',*,*,#38808,.T.) ;
#51995 = ORIENTED_EDGE('',*,*,#38654,.F.) ;
#51996 = ORIENTED_EDGE('',*,*,#38812,.F.) ;
#51997 = ORIENTED_EDGE('',*,*,#38662,.F.) ;
#51998 = ORIENTED_EDGE('',*,*,#38809,.T.) ;
#51999 = ORIENTED_EDGE('',*,*,#38664,.F.) ;
#52000 = ORIENTED_EDGE('',*,*,#38813,.F.) ;
#52001 = ORIENTED_EDGE('',*,*,#38541,.F.) ;
#52002 = ORIENTED_EDGE('',*,*,#38810,.T.) ;
#52003 = ORIENTED_EDGE('',*,*,#38542,.F.) ;
#52004 = ORIENTED_EDGE('',*,*,#38814,.F.) ;
#52005 = ORIENTED_EDGE('',*,*,#38531,.F.) ;
#52006 = ORIENTED_EDGE('',*,*,#38812,.T.) ;
#52007 = ORIENTED_EDGE('',*,*,#38811,.T.) ;
#52008 = ORIENTED_EDGE('',*,*,#38815,.F.) ;
#52009 = ORIENTED_EDGE('',*,*,#38814,.T.) ;
#52010 = ORIENTED_EDGE('',*,*,#38813,.T.) ;
#52011 = ORIENTED_EDGE('',*,*,#38816,.F.) ;
#52012 = ORIENTED_EDGE('',*,*,#38532,.T.) ;
#52013 = ORIENTED_EDGE('',*,*,#38815,.T.) ;
#52014 = ORIENTED_EDGE('',*,*,#38533,.F.) ;
#52015 = ORIENTED_EDGE('',*,*,#38816,.T.) ;
#52016 = ORIENTED_EDGE('',*,*,#38663,.F.) ;
#52017 = ORIENTED_EDGE('',*,*,#38817,.F.) ;
#52018 = ORIENTED_EDGE('',*,*,#38818,.F.) ;
#52019 = ORIENTED_EDGE('',*,*,#38819,.F.) ;
#52020 = ORIENTED_EDGE('',*,*,#38610,.F.) ;
#52021 = ORIENTED_EDGE('',*,*,#38820,.T.) ;
#52022 = ORIENTED_EDGE('',*,*,#38821,.T.) ;
#52023 = ORIENTED_EDGE('',*,*,#38592,.F.) ;
#52024 = ORIENTED_EDGE('',*,*,#38818,.T.) ;
#52025 = ORIENTED_EDGE('',*,*,#38591,.F.) ;
#52026 = ORIENTED_EDGE('',*,*,#38822,.T.) ;
#52027 = ORIENTED_EDGE('',*,*,#38823,.T.) ;
#52028 = ORIENTED_EDGE('',*,*,#38584,.F.) ;
#52029 = ORIENTED_EDGE('',*,*,#38819,.T.) ;
#52030 = ORIENTED_EDGE('',*,*,#38817,.T.) ;
#52031 = ORIENTED_EDGE('',*,*,#38583,.F.) ;
#52032 = ORIENTED_EDGE('',*,*,#38824,.F.) ;
#52033 = ORIENTED_EDGE('',*,*,#38603,.F.) ;
#52034 = ORIENTED_EDGE('',*,*,#38599,.F.) ;
#52035 = ORIENTED_EDGE('',*,*,#38825,.T.) ;
#52036 = ORIENTED_EDGE('',*,*,#38826,.T.) ;
#52037 = ORIENTED_EDGE('',*,*,#38609,.F.) ;
#52038 = ORIENTED_EDGE('',*,*,#38827,.T.) ;
#52039 = ORIENTED_EDGE('',*,*,#38828,.T.) ;
#52040 = ORIENTED_EDGE('',*,*,#38577,.F.) ;
#52041 = ORIENTED_EDGE('',*,*,#38829,.T.) ;
#52042 = ORIENTED_EDGE('',*,*,#38830,.T.) ;
#52043 = ORIENTED_EDGE('',*,*,#38593,.F.) ;
#52044 = ORIENTED_EDGE('',*,*,#38831,.T.) ;
#52045 = ORIENTED_EDGE('',*,*,#38832,.T.) ;
#52046 = ORIENTED_EDGE('',*,*,#38833,.F.) ;
#52047 = ORIENTED_EDGE('',*,*,#38824,.T.) ;
#52048 = ORIENTED_EDGE('',*,*,#38834,.F.) ;
#52049 = ORIENTED_EDGE('',*,*,#38574,.T.) ;
#52050 = ORIENTED_EDGE('',*,*,#38835,.F.) ;
#52051 = ORIENTED_EDGE('',*,*,#38836,.F.) ;
#52052 = ORIENTED_EDGE('',*,*,#38604,.F.) ;
#52053 = ORIENTED_EDGE('',*,*,#38833,.T.) ;
#52054 = ORIENTED_EDGE('',*,*,#38836,.T.) ;
#52055 = ORIENTED_EDGE('',*,*,#38837,.F.) ;
#52056 = ORIENTED_EDGE('',*,*,#38838,.F.) ;
#52057 = ORIENTED_EDGE('',*,*,#38588,.F.) ;
#52058 = ORIENTED_EDGE('',*,*,#38839,.T.) ;
#52059 = ORIENTED_EDGE('',*,*,#38840,.T.) ;
#52060 = ORIENTED_EDGE('',*,*,#38608,.F.) ;
#52061 = ORIENTED_EDGE('',*,*,#38841,.F.) ;
#52062 = ORIENTED_EDGE('',*,*,#38578,.F.) ;
#52063 = ORIENTED_EDGE('',*,*,#38842,.T.) ;
#52064 = ORIENTED_EDGE('',*,*,#38843,.T.) ;
#52065 = ORIENTED_EDGE('',*,*,#38585,.F.) ;
#52066 = ORIENTED_EDGE('',*,*,#38844,.F.) ;
#52067 = ORIENTED_EDGE('',*,*,#38834,.T.) ;
#52068 = ORIENTED_EDGE('',*,*,#38582,.F.) ;
#52069 = ORIENTED_EDGE('',*,*,#38845,.F.) ;
#52070 = ORIENTED_EDGE('',*,*,#38846,.F.) ;
#52071 = ORIENTED_EDGE('',*,*,#38847,.F.) ;
#52072 = ORIENTED_EDGE('',*,*,#38558,.F.) ;
#52073 = ORIENTED_EDGE('',*,*,#38848,.F.) ;
#52074 = ORIENTED_EDGE('',*,*,#38835,.T.) ;
#52075 = ORIENTED_EDGE('',*,*,#38576,.F.) ;
#52076 = ORIENTED_EDGE('',*,*,#38848,.T.) ;
#52077 = ORIENTED_EDGE('',*,*,#38557,.T.) ;
#52078 = ORIENTED_EDGE('',*,*,#38849,.F.) ;
#52079 = ORIENTED_EDGE('',*,*,#38837,.T.) ;
#52080 = ORIENTED_EDGE('',*,*,#38605,.F.) ;
#52081 = ORIENTED_EDGE('',*,*,#38838,.T.) ;
#52082 = ORIENTED_EDGE('',*,*,#38850,.F.) ;
#52083 = ORIENTED_EDGE('',*,*,#38851,.F.) ;
#52084 = ORIENTED_EDGE('',*,*,#38844,.T.) ;
#52085 = ORIENTED_EDGE('',*,*,#38841,.T.) ;
#52086 = ORIENTED_EDGE('',*,*,#38852,.F.) ;
#52087 = ORIENTED_EDGE('',*,*,#38853,.F.) ;
#52088 = ORIENTED_EDGE('',*,*,#38845,.T.) ;
#52089 = ORIENTED_EDGE('',*,*,#38854,.F.) ;
#52090 = ORIENTED_EDGE('',*,*,#38575,.F.) ;
#52091 = ORIENTED_EDGE('',*,*,#38846,.T.) ;
#52092 = ORIENTED_EDGE('',*,*,#38855,.F.) ;
#52093 = ORIENTED_EDGE('',*,*,#38568,.F.) ;
#52094 = ORIENTED_EDGE('',*,*,#38847,.T.) ;
#52095 = ORIENTED_EDGE('',*,*,#38856,.F.) ;
#52096 = ORIENTED_EDGE('',*,*,#38850,.T.) ;
#52097 = ORIENTED_EDGE('',*,*,#38849,.T.) ;
#52098 = ORIENTED_EDGE('',*,*,#38564,.F.) ;
#52099 = ORIENTED_EDGE('',*,*,#38851,.T.) ;
#52100 = ORIENTED_EDGE('',*,*,#38857,.F.) ;
#52101 = ORIENTED_EDGE('',*,*,#38858,.F.) ;
#52102 = ORIENTED_EDGE('',*,*,#38852,.T.) ;
#52103 = ORIENTED_EDGE('',*,*,#38607,.F.) ;
#52104 = ORIENTED_EDGE('',*,*,#38859,.F.) ;
#52105 = ORIENTED_EDGE('',*,*,#38579,.F.) ;
#52106 = ORIENTED_EDGE('',*,*,#38854,.T.) ;
#52107 = ORIENTED_EDGE('',*,*,#38581,.F.) ;
#52108 = ORIENTED_EDGE('',*,*,#38860,.F.) ;
#52109 = ORIENTED_EDGE('',*,*,#38861,.F.) ;
#52110 = ORIENTED_EDGE('',*,*,#38855,.T.) ;
#52111 = ORIENTED_EDGE('',*,*,#38853,.T.) ;
#52112 = ORIENTED_EDGE('',*,*,#38862,.F.) ;
#52113 = ORIENTED_EDGE('',*,*,#38569,.T.) ;
#52114 = ORIENTED_EDGE('',*,*,#38856,.T.) ;
#52115 = ORIENTED_EDGE('',*,*,#38563,.T.) ;
#52116 = ORIENTED_EDGE('',*,*,#38863,.F.) ;
#52117 = ORIENTED_EDGE('',*,*,#38857,.T.) ;
#52118 = ORIENTED_EDGE('',*,*,#38864,.F.) ;
#52119 = ORIENTED_EDGE('',*,*,#38865,.F.) ;
#52120 = ORIENTED_EDGE('',*,*,#38606,.F.) ;
#52121 = ORIENTED_EDGE('',*,*,#38858,.T.) ;
#52122 = ORIENTED_EDGE('',*,*,#38865,.T.) ;
#52123 = ORIENTED_EDGE('',*,*,#38573,.T.) ;
#52124 = ORIENTED_EDGE('',*,*,#38866,.F.) ;
#52125 = ORIENTED_EDGE('',*,*,#38859,.T.) ;
#52126 = ORIENTED_EDGE('',*,*,#38867,.F.) ;
#52127 = ORIENTED_EDGE('',*,*,#38860,.T.) ;
#52128 = ORIENTED_EDGE('',*,*,#38868,.F.) ;
#52129 = ORIENTED_EDGE('',*,*,#38862,.T.) ;
#52130 = ORIENTED_EDGE('',*,*,#38861,.T.) ;
#52131 = ORIENTED_EDGE('',*,*,#38869,.F.) ;
#52132 = ORIENTED_EDGE('',*,*,#38570,.F.) ;
#52133 = ORIENTED_EDGE('',*,*,#38863,.T.) ;
#52134 = ORIENTED_EDGE('',*,*,#38562,.F.) ;
#52135 = ORIENTED_EDGE('',*,*,#38870,.F.) ;
#52136 = ORIENTED_EDGE('',*,*,#38571,.F.) ;
#52137 = ORIENTED_EDGE('',*,*,#38864,.T.) ;
#52138 = ORIENTED_EDGE('',*,*,#38580,.F.) ;
#52139 = ORIENTED_EDGE('',*,*,#38866,.T.) ;
#52140 = ORIENTED_EDGE('',*,*,#38871,.F.) ;
#52141 = ORIENTED_EDGE('',*,*,#38868,.T.) ;
#52142 = ORIENTED_EDGE('',*,*,#38869,.T.) ;
#52143 = ORIENTED_EDGE('',*,*,#38867,.T.) ;
#52144 = ORIENTED_EDGE('',*,*,#38872,.F.) ;
#52145 = ORIENTED_EDGE('',*,*,#38565,.T.) ;
#52146 = ORIENTED_EDGE('',*,*,#38870,.T.) ;
#52147 = ORIENTED_EDGE('',*,*,#38566,.F.) ;
#52148 = ORIENTED_EDGE('',*,*,#38872,.T.) ;
#52149 = ORIENTED_EDGE('',*,*,#38871,.T.) ;
#52150 = ORIENTED_EDGE('',*,*,#38572,.F.) ;
#52151 = ORIENTED_EDGE('',*,*,#38873,.F.) ;
#52152 = ORIENTED_EDGE('',*,*,#38621,.F.) ;
#52153 = ORIENTED_EDGE('',*,*,#38456,.F.) ;
#52154 = ORIENTED_EDGE('',*,*,#38627,.F.) ;
#52155 = ORIENTED_EDGE('',*,*,#38874,.F.) ;
#52156 = ORIENTED_EDGE('',*,*,#38873,.T.) ;
#52157 = ORIENTED_EDGE('',*,*,#38875,.F.) ;
#52158 = ORIENTED_EDGE('',*,*,#38454,.F.) ;
#52159 = ORIENTED_EDGE('',*,*,#38536,.F.) ;
#52160 = ORIENTED_EDGE('',*,*,#38876,.F.) ;
#52161 = ORIENTED_EDGE('',*,*,#38625,.F.) ;
#52162 = ORIENTED_EDGE('',*,*,#38875,.T.) ;
#52163 = ORIENTED_EDGE('',*,*,#38626,.F.) ;
#52164 = ORIENTED_EDGE('',*,*,#38877,.F.) ;
#52165 = ORIENTED_EDGE('',*,*,#38632,.F.) ;
#52166 = ORIENTED_EDGE('',*,*,#38874,.T.) ;
#52167 = ORIENTED_EDGE('',*,*,#38631,.F.) ;
#52168 = ORIENTED_EDGE('',*,*,#38878,.F.) ;
#52169 = ORIENTED_EDGE('',*,*,#38622,.F.) ;
#52170 = ORIENTED_EDGE('',*,*,#38458,.F.) ;
#52171 = ORIENTED_EDGE('',*,*,#38620,.F.) ;
#52172 = ORIENTED_EDGE('',*,*,#38879,.F.) ;
#52173 = ORIENTED_EDGE('',*,*,#38431,.F.) ;
#52174 = ORIENTED_EDGE('',*,*,#38399,.F.) ;
#52175 = ORIENTED_EDGE('',*,*,#38880,.T.) ;
#52176 = ORIENTED_EDGE('',*,*,#38428,.F.) ;
#52177 = ORIENTED_EDGE('',*,*,#38881,.F.) ;
#52178 = ORIENTED_EDGE('',*,*,#38876,.T.) ;
#52179 = ORIENTED_EDGE('',*,*,#38535,.T.) ;
#52180 = ORIENTED_EDGE('',*,*,#38882,.F.) ;
#52181 = ORIENTED_EDGE('',*,*,#38877,.T.) ;
#52182 = ORIENTED_EDGE('',*,*,#38883,.F.) ;
#52183 = ORIENTED_EDGE('',*,*,#38878,.T.) ;
#52184 = ORIENTED_EDGE('',*,*,#38884,.F.) ;
#52185 = ORIENTED_EDGE('',*,*,#38879,.T.) ;
#52186 = ORIENTED_EDGE('',*,*,#38619,.T.) ;
#52187 = ORIENTED_EDGE('',*,*,#38885,.F.) ;
#52188 = ORIENTED_EDGE('',*,*,#38881,.T.) ;
#52189 = ORIENTED_EDGE('',*,*,#38882,.T.) ;
#52190 = ORIENTED_EDGE('',*,*,#38556,.F.) ;
#52191 = ORIENTED_EDGE('',*,*,#38886,.F.) ;
#52192 = ORIENTED_EDGE('',*,*,#38633,.F.) ;
#52193 = ORIENTED_EDGE('',*,*,#38884,.T.) ;
#52194 = ORIENTED_EDGE('',*,*,#38634,.F.) ;
#52195 = ORIENTED_EDGE('',*,*,#38887,.F.) ;
#52196 = ORIENTED_EDGE('',*,*,#38628,.F.) ;
#52197 = ORIENTED_EDGE('',*,*,#38883,.T.) ;
#52198 = ORIENTED_EDGE('',*,*,#38630,.F.) ;
#52199 = ORIENTED_EDGE('',*,*,#38888,.F.) ;
#52200 = ORIENTED_EDGE('',*,*,#38623,.F.) ;
#52201 = ORIENTED_EDGE('',*,*,#38885,.T.) ;
#52202 = ORIENTED_EDGE('',*,*,#38624,.F.) ;
#52203 = ORIENTED_EDGE('',*,*,#38889,.F.) ;
#52204 = ORIENTED_EDGE('',*,*,#38400,.F.) ;
#52205 = ORIENTED_EDGE('',*,*,#38434,.F.) ;
#52206 = ORIENTED_EDGE('',*,*,#38890,.T.) ;
#52207 = ORIENTED_EDGE('',*,*,#38405,.F.) ;
#52208 = ORIENTED_EDGE('',*,*,#38891,.F.) ;
#52209 = ORIENTED_EDGE('',*,*,#38484,.F.) ;
#52210 = ORIENTED_EDGE('',*,*,#38435,.F.) ;
#52211 = ORIENTED_EDGE('',*,*,#38892,.F.) ;
#52212 = ORIENTED_EDGE('',*,*,#38647,.F.) ;
#52213 = ORIENTED_EDGE('',*,*,#38486,.F.) ;
#52214 = ORIENTED_EDGE('',*,*,#38646,.F.) ;
#52215 = ORIENTED_EDGE('',*,*,#38893,.F.) ;
#52216 = ORIENTED_EDGE('',*,*,#38644,.F.) ;
#52217 = ORIENTED_EDGE('',*,*,#38886,.T.) ;
#52218 = ORIENTED_EDGE('',*,*,#38555,.T.) ;
#52219 = ORIENTED_EDGE('',*,*,#38894,.F.) ;
#52220 = ORIENTED_EDGE('',*,*,#38887,.T.) ;
#52221 = ORIENTED_EDGE('',*,*,#38889,.T.) ;
#52222 = ORIENTED_EDGE('',*,*,#38888,.T.) ;
#52223 = ORIENTED_EDGE('',*,*,#38392,.F.) ;
#52224 = ORIENTED_EDGE('',*,*,#38892,.T.) ;
#52225 = ORIENTED_EDGE('',*,*,#38891,.T.) ;
#52226 = ORIENTED_EDGE('',*,*,#38895,.F.) ;
#52227 = ORIENTED_EDGE('',*,*,#38648,.T.) ;
#52228 = ORIENTED_EDGE('',*,*,#38896,.F.) ;
#52229 = ORIENTED_EDGE('',*,*,#38893,.T.) ;
#52230 = ORIENTED_EDGE('',*,*,#38897,.F.) ;
#52231 = ORIENTED_EDGE('',*,*,#38894,.T.) ;
#52232 = ORIENTED_EDGE('',*,*,#38554,.F.) ;
#52233 = ORIENTED_EDGE('',*,*,#38898,.F.) ;
#52234 = ORIENTED_EDGE('',*,*,#38629,.F.) ;
#52235 = ORIENTED_EDGE('',*,*,#38895,.T.) ;
#52236 = ORIENTED_EDGE('',*,*,#38404,.F.) ;
#52237 = ORIENTED_EDGE('',*,*,#38899,.F.) ;
#52238 = ORIENTED_EDGE('',*,*,#38649,.F.) ;
#52239 = ORIENTED_EDGE('',*,*,#38900,.F.) ;
#52240 = ORIENTED_EDGE('',*,*,#38650,.F.) ;
#52241 = ORIENTED_EDGE('',*,*,#38901,.F.) ;
#52242 = ORIENTED_EDGE('',*,*,#38641,.F.) ;
#52243 = ORIENTED_EDGE('',*,*,#38897,.T.) ;
#52244 = ORIENTED_EDGE('',*,*,#38645,.F.) ;
#52245 = ORIENTED_EDGE('',*,*,#38902,.F.) ;
#52246 = ORIENTED_EDGE('',*,*,#38635,.F.) ;
#52247 = ORIENTED_EDGE('',*,*,#38896,.T.) ;
#52248 = ORIENTED_EDGE('',*,*,#38638,.F.) ;
#52249 = ORIENTED_EDGE('',*,*,#38903,.F.) ;
#52250 = ORIENTED_EDGE('',*,*,#38642,.F.) ;
#52251 = ORIENTED_EDGE('',*,*,#38488,.F.) ;
#52252 = ORIENTED_EDGE('',*,*,#38643,.F.) ;
#52253 = ORIENTED_EDGE('',*,*,#38904,.F.) ;
#52254 = ORIENTED_EDGE('',*,*,#38548,.F.) ;
#52255 = ORIENTED_EDGE('',*,*,#38390,.T.) ;
#52256 = ORIENTED_EDGE('',*,*,#38898,.T.) ;
#52257 = ORIENTED_EDGE('',*,*,#38905,.F.) ;
#52258 = ORIENTED_EDGE('',*,*,#38401,.T.) ;
#52259 = ORIENTED_EDGE('',*,*,#38901,.T.) ;
#52260 = ORIENTED_EDGE('',*,*,#38899,.T.) ;
#52261 = ORIENTED_EDGE('',*,*,#38388,.F.) ;
#52262 = ORIENTED_EDGE('',*,*,#38906,.F.) ;
#52263 = ORIENTED_EDGE('',*,*,#38906,.T.) ;
#52264 = ORIENTED_EDGE('',*,*,#38387,.F.) ;
#52265 = ORIENTED_EDGE('',*,*,#38902,.T.) ;
#52266 = ORIENTED_EDGE('',*,*,#38900,.T.) ;
#52267 = ORIENTED_EDGE('',*,*,#38907,.F.) ;
#52268 = ORIENTED_EDGE('',*,*,#38904,.T.) ;
#52269 = ORIENTED_EDGE('',*,*,#38903,.T.) ;
#52270 = ORIENTED_EDGE('',*,*,#38908,.F.) ;
#52271 = ORIENTED_EDGE('',*,*,#38549,.T.) ;
#52272 = ORIENTED_EDGE('',*,*,#38905,.T.) ;
#52273 = ORIENTED_EDGE('',*,*,#38553,.F.) ;
#52274 = ORIENTED_EDGE('',*,*,#38909,.F.) ;
#52275 = ORIENTED_EDGE('',*,*,#38402,.F.) ;
#52276 = ORIENTED_EDGE('',*,*,#38907,.T.) ;
#52277 = ORIENTED_EDGE('',*,*,#38640,.F.) ;
#52278 = ORIENTED_EDGE('',*,*,#38910,.F.) ;
#52279 = ORIENTED_EDGE('',*,*,#38636,.F.) ;
#52280 = ORIENTED_EDGE('',*,*,#38908,.T.) ;
#52281 = ORIENTED_EDGE('',*,*,#38637,.F.) ;
#52282 = ORIENTED_EDGE('',*,*,#38911,.F.) ;
#52283 = ORIENTED_EDGE('',*,*,#38550,.F.) ;
#52284 = ORIENTED_EDGE('',*,*,#38403,.T.) ;
#52285 = ORIENTED_EDGE('',*,*,#38909,.T.) ;
#52286 = ORIENTED_EDGE('',*,*,#38912,.F.) ;
#52287 = ORIENTED_EDGE('',*,*,#38385,.T.) ;
#52288 = ORIENTED_EDGE('',*,*,#38911,.T.) ;
#52289 = ORIENTED_EDGE('',*,*,#38910,.T.) ;
#52290 = ORIENTED_EDGE('',*,*,#38913,.F.) ;
#52291 = ORIENTED_EDGE('',*,*,#38551,.T.) ;
#52292 = ORIENTED_EDGE('',*,*,#38912,.T.) ;
#52293 = ORIENTED_EDGE('',*,*,#38552,.F.) ;
#52294 = ORIENTED_EDGE('',*,*,#38913,.T.) ;
#52295 = ORIENTED_EDGE('',*,*,#38639,.F.) ;
#52296 = ORIENTED_EDGE('',*,*,#38408,.F.) ;
#52297 = ORIENTED_EDGE('',*,*,#38914,.T.) ;
#52298 = ORIENTED_EDGE('',*,*,#38729,.F.) ;
#52299 = ORIENTED_EDGE('',*,*,#38915,.F.) ;
#52300 = ORIENTED_EDGE('',*,*,#38734,.F.) ;
#52301 = ORIENTED_EDGE('',*,*,#38728,.F.) ;
#52302 = ORIENTED_EDGE('',*,*,#38916,.T.) ;
#52303 = ORIENTED_EDGE('',*,*,#38735,.F.) ;
#52304 = ORIENTED_EDGE('',*,*,#38915,.T.) ;
#52305 = ORIENTED_EDGE('',*,*,#38731,.F.) ;
#52306 = ORIENTED_EDGE('',*,*,#38917,.T.) ;
#52307 = ORIENTED_EDGE('',*,*,#38597,.F.) ;
#52308 = ORIENTED_EDGE('',*,*,#38755,.F.) ;
#52309 = ORIENTED_EDGE('',*,*,#38918,.F.) ;
#52310 = ORIENTED_EDGE('',*,*,#38740,.F.) ;
#52311 = ORIENTED_EDGE('',*,*,#38919,.T.) ;
#52312 = ORIENTED_EDGE('',*,*,#38768,.F.) ;
#52313 = ORIENTED_EDGE('',*,*,#38920,.F.) ;
#52314 = ORIENTED_EDGE('',*,*,#38725,.F.) ;
#52315 = ORIENTED_EDGE('',*,*,#38921,.T.) ;
#52316 = ORIENTED_EDGE('',*,*,#38410,.F.) ;
#52317 = ORIENTED_EDGE('',*,*,#38733,.F.) ;
#52318 = ORIENTED_EDGE('',*,*,#38922,.F.) ;
#52319 = ORIENTED_EDGE('',*,*,#38752,.F.) ;
#52320 = ORIENTED_EDGE('',*,*,#38923,.T.) ;
#52321 = ORIENTED_EDGE('',*,*,#38726,.F.) ;
#52322 = ORIENTED_EDGE('',*,*,#38918,.T.) ;
#52323 = ORIENTED_EDGE('',*,*,#38924,.F.) ;
#52324 = ORIENTED_EDGE('',*,*,#38920,.T.) ;
#52325 = ORIENTED_EDGE('',*,*,#38925,.F.) ;
#52326 = ORIENTED_EDGE('',*,*,#38737,.F.) ;
#52327 = ORIENTED_EDGE('',*,*,#38926,.T.) ;
#52328 = ORIENTED_EDGE('',*,*,#38720,.F.) ;
#52329 = ORIENTED_EDGE('',*,*,#38922,.T.) ;
#52330 = ORIENTED_EDGE('',*,*,#38770,.F.) ;
#52331 = ORIENTED_EDGE('',*,*,#38927,.T.) ;
#52332 = ORIENTED_EDGE('',*,*,#38746,.F.) ;
#52333 = ORIENTED_EDGE('',*,*,#38928,.F.) ;
#52334 = ORIENTED_EDGE('',*,*,#38925,.T.) ;
#52335 = ORIENTED_EDGE('',*,*,#38771,.F.) ;
#52336 = ORIENTED_EDGE('',*,*,#38929,.F.) ;
#52337 = ORIENTED_EDGE('',*,*,#38745,.F.) ;
#52338 = ORIENTED_EDGE('',*,*,#38924,.T.) ;
#52339 = ORIENTED_EDGE('',*,*,#38744,.F.) ;
#52340 = ORIENTED_EDGE('',*,*,#38930,.F.) ;
#52341 = ORIENTED_EDGE('',*,*,#38741,.F.) ;
#52342 = ORIENTED_EDGE('',*,*,#38766,.F.) ;
#52343 = ORIENTED_EDGE('',*,*,#38931,.T.) ;
#52344 = ORIENTED_EDGE('',*,*,#38738,.F.) ;
#52345 = ORIENTED_EDGE('',*,*,#38932,.F.) ;
#52346 = ORIENTED_EDGE('',*,*,#38929,.T.) ;
#52347 = ORIENTED_EDGE('',*,*,#38928,.T.) ;
#52348 = ORIENTED_EDGE('',*,*,#38933,.F.) ;
#52349 = ORIENTED_EDGE('',*,*,#38932,.T.) ;
#52350 = ORIENTED_EDGE('',*,*,#38930,.T.) ;
#52351 = ORIENTED_EDGE('',*,*,#38934,.F.) ;
#52352 = ORIENTED_EDGE('',*,*,#38933,.T.) ;
#52353 = ORIENTED_EDGE('',*,*,#38749,.F.) ;
#52354 = ORIENTED_EDGE('',*,*,#38935,.F.) ;
#52355 = ORIENTED_EDGE('',*,*,#38742,.F.) ;
#52356 = ORIENTED_EDGE('',*,*,#38934,.T.) ;
#52357 = ORIENTED_EDGE('',*,*,#38743,.F.) ;
#52358 = ORIENTED_EDGE('',*,*,#38936,.F.) ;
#52359 = ORIENTED_EDGE('',*,*,#38767,.F.) ;
#52360 = ORIENTED_EDGE('',*,*,#38936,.T.) ;
#52361 = ORIENTED_EDGE('',*,*,#38935,.T.) ;
#52362 = ORIENTED_EDGE('',*,*,#38937,.F.) ;
#52363 = ORIENTED_EDGE('',*,*,#38748,.F.) ;
#52364 = ORIENTED_EDGE('',*,*,#38938,.T.) ;
#52365 = ORIENTED_EDGE('',*,*,#38764,.F.) ;
#52366 = ORIENTED_EDGE('',*,*,#38937,.T.) ;
#52367 = ORIENTED_EDGE('',*,*,#38722,.F.) ;
#52368 = ORIENTED_EDGE('',*,*,#38939,.T.) ;
#52369 = ORIENTED_EDGE('',*,*,#38750,.F.) ;
#52370 = ORIENTED_EDGE('',*,*,#38940,.F.) ;
#52371 = ORIENTED_EDGE('',*,*,#38601,.F.) ;
#52372 = ORIENTED_EDGE('',*,*,#38941,.T.) ;
#52373 = ORIENTED_EDGE('',*,*,#38723,.F.) ;
#52374 = ORIENTED_EDGE('',*,*,#38940,.T.) ;
#52375 = ORIENTED_EDGE('',*,*,#38754,.F.) ;
#52376 = ORIENTED_EDGE('',*,*,#38713,.F.) ;
#52377 = ORIENTED_EDGE('',*,*,#38942,.T.) ;
#52378 = ORIENTED_EDGE('',*,*,#38714,.F.) ;
#52379 = ORIENTED_EDGE('',*,*,#38616,.F.) ;
#52380 = ORIENTED_EDGE('',*,*,#38719,.F.) ;
#52381 = ORIENTED_EDGE('',*,*,#38943,.T.) ;
#52382 = ORIENTED_EDGE('',*,*,#38711,.F.) ;
#52383 = ORIENTED_EDGE('',*,*,#38614,.F.) ;
#52384 = ORIENTED_EDGE('',*,*,#38698,.F.) ;
#52385 = ORIENTED_EDGE('',*,*,#38944,.T.) ;
#52386 = ORIENTED_EDGE('',*,*,#38756,.F.) ;
#52387 = ORIENTED_EDGE('',*,*,#38945,.F.) ;
#52388 = ORIENTED_EDGE('',*,*,#38758,.F.) ;
#52389 = ORIENTED_EDGE('',*,*,#38946,.T.) ;
#52390 = ORIENTED_EDGE('',*,*,#38704,.F.) ;
#52391 = ORIENTED_EDGE('',*,*,#38947,.F.) ;
#52392 = ORIENTED_EDGE('',*,*,#38948,.F.) ;
#52393 = ORIENTED_EDGE('',*,*,#38759,.F.) ;
#52394 = ORIENTED_EDGE('',*,*,#38949,.F.) ;
#52395 = ORIENTED_EDGE('',*,*,#38703,.F.) ;
#52396 = ORIENTED_EDGE('',*,*,#38945,.T.) ;
#52397 = ORIENTED_EDGE('',*,*,#38948,.T.) ;
#52398 = ORIENTED_EDGE('',*,*,#38950,.F.) ;
#52399 = ORIENTED_EDGE('',*,*,#38716,.F.) ;
#52400 = ORIENTED_EDGE('',*,*,#38951,.T.) ;
#52401 = ORIENTED_EDGE('',*,*,#38708,.F.) ;
#52402 = ORIENTED_EDGE('',*,*,#38618,.F.) ;
#52403 = ORIENTED_EDGE('',*,*,#38710,.F.) ;
#52404 = ORIENTED_EDGE('',*,*,#38952,.T.) ;
#52405 = ORIENTED_EDGE('',*,*,#38717,.F.) ;
#52406 = ORIENTED_EDGE('',*,*,#38612,.F.) ;
#52407 = ORIENTED_EDGE('',*,*,#38949,.T.) ;
#52408 = ORIENTED_EDGE('',*,*,#38947,.T.) ;
#52409 = ORIENTED_EDGE('',*,*,#38953,.F.) ;
#52410 = ORIENTED_EDGE('',*,*,#38950,.T.) ;
#52411 = ORIENTED_EDGE('',*,*,#38702,.F.) ;
#52412 = ORIENTED_EDGE('',*,*,#38954,.F.) ;
#52413 = ORIENTED_EDGE('',*,*,#38699,.F.) ;
#52414 = ORIENTED_EDGE('',*,*,#38762,.F.) ;
#52415 = ORIENTED_EDGE('',*,*,#38955,.T.) ;
#52416 = ORIENTED_EDGE('',*,*,#38696,.F.) ;
#52417 = ORIENTED_EDGE('',*,*,#38956,.F.) ;
#52418 = ORIENTED_EDGE('',*,*,#38706,.F.) ;
#52419 = ORIENTED_EDGE('',*,*,#38957,.T.) ;
#52420 = ORIENTED_EDGE('',*,*,#38760,.F.) ;
#52421 = ORIENTED_EDGE('',*,*,#38958,.F.) ;
#52422 = ORIENTED_EDGE('',*,*,#38953,.T.) ;
#52423 = ORIENTED_EDGE('',*,*,#38707,.F.) ;
#52424 = ORIENTED_EDGE('',*,*,#38959,.F.) ;
#52425 = ORIENTED_EDGE('',*,*,#38700,.F.) ;
#52426 = ORIENTED_EDGE('',*,*,#38956,.T.) ;
#52427 = ORIENTED_EDGE('',*,*,#38954,.T.) ;
#52428 = ORIENTED_EDGE('',*,*,#38960,.F.) ;
#52429 = ORIENTED_EDGE('',*,*,#38959,.T.) ;
#52430 = ORIENTED_EDGE('',*,*,#38958,.T.) ;
#52431 = ORIENTED_EDGE('',*,*,#38961,.F.) ;
#52432 = ORIENTED_EDGE('',*,*,#38960,.T.) ;
#52433 = ORIENTED_EDGE('',*,*,#38701,.F.) ;
#52434 = ORIENTED_EDGE('',*,*,#38961,.T.) ;
#52435 = ORIENTED_EDGE('',*,*,#38763,.F.) ;
#52436 = ORIENTED_EDGE('',*,*,#38445,.F.) ;
#52437 = ORIENTED_EDGE('',*,*,#38421,.F.) ;
#52438 = ORIENTED_EDGE('',*,*,#38962,.F.) ;
#52439 = ORIENTED_EDGE('',*,*,#38427,.F.) ;
#52440 = ORIENTED_EDGE('',*,*,#38683,.F.) ;
#52441 = ORIENTED_EDGE('',*,*,#38963,.T.) ;
#52442 = ORIENTED_EDGE('',*,*,#38422,.F.) ;
#52443 = ORIENTED_EDGE('',*,*,#38964,.F.) ;
#52444 = ORIENTED_EDGE('',*,*,#38964,.T.) ;
#52445 = ORIENTED_EDGE('',*,*,#38962,.T.) ;
#52446 = ORIENTED_EDGE('',*,*,#38965,.F.) ;
#52447 = ORIENTED_EDGE('',*,*,#38444,.F.) ;
#52448 = ORIENTED_EDGE('',*,*,#38417,.F.) ;
#52449 = ORIENTED_EDGE('',*,*,#38966,.F.) ;
#52450 = ORIENTED_EDGE('',*,*,#38419,.F.) ;
#52451 = ORIENTED_EDGE('',*,*,#38965,.T.) ;
#52452 = ORIENTED_EDGE('',*,*,#38420,.F.) ;
#52453 = ORIENTED_EDGE('',*,*,#38967,.F.) ;
#52454 = ORIENTED_EDGE('',*,*,#38684,.F.) ;
#52455 = ORIENTED_EDGE('',*,*,#38967,.T.) ;
#52456 = ORIENTED_EDGE('',*,*,#38966,.T.) ;
#52457 = ORIENTED_EDGE('',*,*,#38968,.F.) ;
#52458 = ORIENTED_EDGE('',*,*,#38416,.F.) ;
#52459 = ORIENTED_EDGE('',*,*,#38969,.T.) ;
#52460 = ORIENTED_EDGE('',*,*,#38681,.F.) ;
#52461 = ORIENTED_EDGE('',*,*,#38968,.T.) ;
#52462 = ORIENTED_EDGE('',*,*,#38520,.F.) ;
#52463 = ORIENTED_EDGE('',*,*,#38372,.T.) ;
#52464 = ORIENTED_EDGE('',*,*,#38970,.T.) ;
#52465 = ORIENTED_EDGE('',*,*,#38692,.F.) ;
#52466 = ORIENTED_EDGE('',*,*,#38971,.F.) ;
#52467 = ORIENTED_EDGE('',*,*,#38498,.F.) ;
#52468 = ORIENTED_EDGE('',*,*,#38521,.F.) ;
#52469 = ORIENTED_EDGE('',*,*,#38972,.F.) ;
#52470 = ORIENTED_EDGE('',*,*,#38518,.F.) ;
#52471 = ORIENTED_EDGE('',*,*,#38972,.T.) ;
#52472 = ORIENTED_EDGE('',*,*,#38971,.T.) ;
#52473 = ORIENTED_EDGE('',*,*,#38973,.F.) ;
#52474 = ORIENTED_EDGE('',*,*,#38973,.T.) ;
#52475 = ORIENTED_EDGE('',*,*,#38695,.F.) ;
#52476 = ORIENTED_EDGE('',*,*,#38974,.F.) ;
#52477 = ORIENTED_EDGE('',*,*,#38516,.F.) ;
#52478 = ORIENTED_EDGE('',*,*,#38500,.F.) ;
#52479 = ORIENTED_EDGE('',*,*,#38517,.F.) ;
#52480 = ORIENTED_EDGE('',*,*,#38975,.F.) ;
#52481 = ORIENTED_EDGE('',*,*,#38514,.F.) ;
#52482 = ORIENTED_EDGE('',*,*,#38975,.T.) ;
#52483 = ORIENTED_EDGE('',*,*,#38974,.T.) ;
#52484 = ORIENTED_EDGE('',*,*,#38976,.F.) ;
#52485 = ORIENTED_EDGE('',*,*,#38694,.F.) ;
#52486 = ORIENTED_EDGE('',*,*,#38376,.T.) ;
#52487 = ORIENTED_EDGE('',*,*,#38977,.T.) ;
#52488 = ORIENTED_EDGE('',*,*,#38515,.F.) ;
#52489 = ORIENTED_EDGE('',*,*,#38976,.T.) ;
#52490 = ORIENTED_EDGE('',*,*,#38595,.F.) ;
#52491 = ORIENTED_EDGE('',*,*,#38978,.T.) ;
#52492 = ORIENTED_EDGE('',*,*,#38406,.F.) ;
#52493 = ORIENTED_EDGE('',*,*,#38979,.T.) ;
#52494 = ORIENTED_EDGE('',*,*,#38465,.F.) ;
#52495 = ORIENTED_EDGE('',*,*,#38567,.F.) ;
#52496 = ORIENTED_EDGE('',*,*,#38477,.F.) ;
#52497 = ORIENTED_EDGE('',*,*,#38501,.F.) ;
#52498 = ORIENTED_EDGE('',*,*,#38467,.F.) ;
#52499 = ORIENTED_EDGE('',*,*,#38502,.F.) ;
#52500 = ORIENTED_EDGE('',*,*,#38475,.F.) ;
#52501 = ORIENTED_EDGE('',*,*,#38503,.F.) ;
#52502 = ORIENTED_EDGE('',*,*,#38469,.F.) ;
#52503 = ORIENTED_EDGE('',*,*,#38504,.F.) ;
#52504 = ORIENTED_EDGE('',*,*,#38473,.F.) ;
#52505 = ORIENTED_EDGE('',*,*,#38507,.F.) ;
#52506 = ORIENTED_EDGE('',*,*,#38462,.F.) ;
#52507 = ORIENTED_EDGE('',*,*,#38437,.F.) ;
#52508 = ORIENTED_EDGE('',*,*,#38480,.F.) ;
#52509 = ORIENTED_EDGE('',*,*,#38560,.F.) ;
#52510 = ORIENTED_EDGE('',*,*,#38780,.F.) ;
#52511 = ORIENTED_EDGE('',*,*,#38980,.T.) ;
#52512 = ORIENTED_EDGE('',*,*,#38439,.F.) ;
#52513 = ORIENTED_EDGE('',*,*,#38461,.F.) ;
#52514 = ORIENTED_EDGE('',*,*,#38775,.F.) ;
#52515 = ORIENTED_EDGE('',*,*,#38981,.T.) ;
#52516 = ORIENTED_EDGE('',*,*,#38440,.F.) ;
#52517 = ORIENTED_EDGE('',*,*,#38982,.T.) ;
#52518 = ORIENTED_EDGE('',*,*,#38441,.F.) ;
#52519 = ORIENTED_EDGE('',*,*,#38983,.T.) ;
#52520 = ORIENTED_EDGE('',*,*,#38772,.F.) ;
#52521 = ORIENTED_EDGE('',*,*,#38481,.F.) ;
#52522 = ORIENTED_EDGE('',*,*,#38820,.F.) ;
#52523 = ORIENTED_EDGE('',*,*,#38826,.F.) ;
#52524 = ORIENTED_EDGE('',*,*,#38825,.F.) ;
#52525 = ORIENTED_EDGE('',*,*,#38984,.F.) ;
#52526 = ORIENTED_EDGE('',*,*,#38821,.F.) ;
#52527 = ORIENTED_EDGE('',*,*,#38914,.F.) ;
#52528 = ORIENTED_EDGE('',*,*,#38407,.F.) ;
#52529 = ORIENTED_EDGE('',*,*,#38985,.F.) ;
#52530 = ORIENTED_EDGE('',*,*,#38589,.F.) ;
#52531 = ORIENTED_EDGE('',*,*,#38984,.T.) ;
#52532 = ORIENTED_EDGE('',*,*,#38598,.F.) ;
#52533 = ORIENTED_EDGE('',*,*,#38917,.F.) ;
#52534 = ORIENTED_EDGE('',*,*,#38730,.F.) ;
#52535 = ORIENTED_EDGE('',*,*,#38985,.T.) ;
#52536 = ORIENTED_EDGE('',*,*,#38978,.F.) ;
#52537 = ORIENTED_EDGE('',*,*,#38986,.F.) ;
#52538 = ORIENTED_EDGE('',*,*,#38986,.T.) ;
#52539 = ORIENTED_EDGE('',*,*,#38594,.F.) ;
#52540 = ORIENTED_EDGE('',*,*,#38987,.F.) ;
#52541 = ORIENTED_EDGE('',*,*,#38590,.F.) ;
#52542 = ORIENTED_EDGE('',*,*,#38829,.F.) ;
#52543 = ORIENTED_EDGE('',*,*,#38823,.F.) ;
#52544 = ORIENTED_EDGE('',*,*,#38822,.F.) ;
#52545 = ORIENTED_EDGE('',*,*,#38987,.T.) ;
#52546 = ORIENTED_EDGE('',*,*,#38830,.F.) ;
#52547 = ORIENTED_EDGE('',*,*,#38842,.F.) ;
#52548 = ORIENTED_EDGE('',*,*,#38832,.F.) ;
#52549 = ORIENTED_EDGE('',*,*,#38831,.F.) ;
#52550 = ORIENTED_EDGE('',*,*,#38988,.F.) ;
#52551 = ORIENTED_EDGE('',*,*,#38843,.F.) ;
#52552 = ORIENTED_EDGE('',*,*,#38988,.T.) ;
#52553 = ORIENTED_EDGE('',*,*,#38596,.F.) ;
#52554 = ORIENTED_EDGE('',*,*,#38989,.F.) ;
#52555 = ORIENTED_EDGE('',*,*,#38586,.F.) ;
#52556 = ORIENTED_EDGE('',*,*,#38989,.T.) ;
#52557 = ORIENTED_EDGE('',*,*,#38979,.F.) ;
#52558 = ORIENTED_EDGE('',*,*,#38990,.F.) ;
#52559 = ORIENTED_EDGE('',*,*,#38941,.F.) ;
#52560 = ORIENTED_EDGE('',*,*,#38600,.F.) ;
#52561 = ORIENTED_EDGE('',*,*,#38991,.F.) ;
#52562 = ORIENTED_EDGE('',*,*,#38587,.F.) ;
#52563 = ORIENTED_EDGE('',*,*,#38990,.T.) ;
#52564 = ORIENTED_EDGE('',*,*,#38411,.F.) ;
#52565 = ORIENTED_EDGE('',*,*,#38921,.F.) ;
#52566 = ORIENTED_EDGE('',*,*,#38724,.F.) ;
#52567 = ORIENTED_EDGE('',*,*,#38991,.T.) ;
#52568 = ORIENTED_EDGE('',*,*,#38828,.F.) ;
#52569 = ORIENTED_EDGE('',*,*,#38827,.F.) ;
#52570 = ORIENTED_EDGE('',*,*,#38840,.F.) ;
#52571 = ORIENTED_EDGE('',*,*,#38839,.F.) ;
#52572 = ORIENTED_EDGE('',*,*,#38415,.F.) ;
#52573 = ORIENTED_EDGE('',*,*,#38992,.T.) ;
#52574 = ORIENTED_EDGE('',*,*,#38685,.F.) ;
#52575 = ORIENTED_EDGE('',*,*,#38993,.F.) ;
#52576 = ORIENTED_EDGE('',*,*,#38969,.F.) ;
#52577 = ORIENTED_EDGE('',*,*,#38993,.T.) ;
#52578 = ORIENTED_EDGE('',*,*,#38691,.F.) ;
#52579 = ORIENTED_EDGE('',*,*,#38994,.F.) ;
#52580 = ORIENTED_EDGE('',*,*,#38682,.F.) ;
#52581 = ORIENTED_EDGE('',*,*,#38994,.T.) ;
#52582 = ORIENTED_EDGE('',*,*,#38690,.F.) ;
#52583 = ORIENTED_EDGE('',*,*,#38995,.F.) ;
#52584 = ORIENTED_EDGE('',*,*,#38996,.F.) ;
#52585 = ORIENTED_EDGE('',*,*,#38997,.F.) ;
#52586 = ORIENTED_EDGE('',*,*,#38998,.F.) ;
#52587 = ORIENTED_EDGE('',*,*,#38423,.F.) ;
#52588 = ORIENTED_EDGE('',*,*,#38963,.F.) ;
#52589 = ORIENTED_EDGE('',*,*,#38446,.F.) ;
#52590 = ORIENTED_EDGE('',*,*,#38425,.F.) ;
#52591 = ORIENTED_EDGE('',*,*,#38999,.F.) ;
#52592 = ORIENTED_EDGE('',*,*,#38523,.F.) ;
#52593 = ORIENTED_EDGE('',*,*,#38424,.F.) ;
#52594 = ORIENTED_EDGE('',*,*,#38998,.T.) ;
#52595 = ORIENTED_EDGE('',*,*,#38997,.T.) ;
#52596 = ORIENTED_EDGE('',*,*,#38996,.T.) ;
#52597 = ORIENTED_EDGE('',*,*,#38995,.T.) ;
#52598 = ORIENTED_EDGE('',*,*,#39000,.F.) ;
#52599 = ORIENTED_EDGE('',*,*,#38524,.F.) ;
#52600 = ORIENTED_EDGE('',*,*,#38999,.T.) ;
#52601 = ORIENTED_EDGE('',*,*,#38375,.F.) ;
#52602 = ORIENTED_EDGE('',*,*,#39001,.T.) ;
#52603 = ORIENTED_EDGE('',*,*,#38511,.F.) ;
#52604 = ORIENTED_EDGE('',*,*,#38977,.F.) ;
#52605 = ORIENTED_EDGE('',*,*,#39000,.T.) ;
#52606 = ORIENTED_EDGE('',*,*,#38689,.F.) ;
#52607 = ORIENTED_EDGE('',*,*,#39002,.F.) ;
#52608 = ORIENTED_EDGE('',*,*,#38525,.F.) ;
#52609 = ORIENTED_EDGE('',*,*,#38496,.F.) ;
#52610 = ORIENTED_EDGE('',*,*,#38527,.F.) ;
#52611 = ORIENTED_EDGE('',*,*,#39003,.F.) ;
#52612 = ORIENTED_EDGE('',*,*,#38522,.F.) ;
#52613 = ORIENTED_EDGE('',*,*,#38377,.T.) ;
#52614 = ORIENTED_EDGE('',*,*,#38693,.F.) ;
#52615 = ORIENTED_EDGE('',*,*,#39004,.F.) ;
#52616 = ORIENTED_EDGE('',*,*,#38687,.F.) ;
#52617 = ORIENTED_EDGE('',*,*,#38526,.F.) ;
#52618 = ORIENTED_EDGE('',*,*,#39002,.T.) ;
#52619 = ORIENTED_EDGE('',*,*,#39005,.F.) ;
#52620 = ORIENTED_EDGE('',*,*,#39006,.F.) ;
#52621 = ORIENTED_EDGE('',*,*,#39007,.F.) ;
#52622 = ORIENTED_EDGE('',*,*,#38370,.F.) ;
#52623 = ORIENTED_EDGE('',*,*,#38369,.F.) ;
#52624 = ORIENTED_EDGE('',*,*,#38519,.F.) ;
#52625 = ORIENTED_EDGE('',*,*,#39003,.T.) ;
#52626 = ORIENTED_EDGE('',*,*,#38371,.F.) ;
#52627 = ORIENTED_EDGE('',*,*,#39007,.T.) ;
#52628 = ORIENTED_EDGE('',*,*,#39006,.T.) ;
#52629 = ORIENTED_EDGE('',*,*,#39005,.T.) ;
#52630 = ORIENTED_EDGE('',*,*,#38688,.F.) ;
#52631 = ORIENTED_EDGE('',*,*,#39004,.T.) ;
#52632 = ORIENTED_EDGE('',*,*,#38970,.F.) ;
#52633 = ORIENTED_EDGE('',*,*,#39008,.F.) ;
#52634 = ORIENTED_EDGE('',*,*,#38433,.F.) ;
#52635 = ORIENTED_EDGE('',*,*,#38483,.F.) ;
#52636 = ORIENTED_EDGE('',*,*,#38774,.F.) ;
#52637 = ORIENTED_EDGE('',*,*,#38890,.F.) ;
#52638 = ORIENTED_EDGE('',*,*,#39008,.T.) ;
#52639 = ORIENTED_EDGE('',*,*,#39009,.F.) ;
#52640 = ORIENTED_EDGE('',*,*,#38395,.F.) ;
#52641 = ORIENTED_EDGE('',*,*,#39009,.T.) ;
#52642 = ORIENTED_EDGE('',*,*,#38773,.F.) ;
#52643 = ORIENTED_EDGE('',*,*,#39010,.F.) ;
#52644 = ORIENTED_EDGE('',*,*,#38777,.F.) ;
#52645 = ORIENTED_EDGE('',*,*,#38983,.F.) ;
#52646 = ORIENTED_EDGE('',*,*,#38981,.F.) ;
#52647 = ORIENTED_EDGE('',*,*,#39010,.T.) ;
#52648 = ORIENTED_EDGE('',*,*,#39011,.T.) ;
#52649 = ORIENTED_EDGE('',*,*,#38916,.F.) ;
#52650 = ORIENTED_EDGE('',*,*,#39012,.F.) ;
#52651 = ORIENTED_EDGE('',*,*,#38919,.F.) ;
#52652 = ORIENTED_EDGE('',*,*,#39011,.F.) ;
#52653 = ORIENTED_EDGE('',*,*,#38739,.F.) ;
#52654 = ORIENTED_EDGE('',*,*,#39013,.F.) ;
#52655 = ORIENTED_EDGE('',*,*,#38736,.F.) ;
#52656 = ORIENTED_EDGE('',*,*,#39012,.T.) ;
#52657 = ORIENTED_EDGE('',*,*,#38727,.F.) ;
#52658 = ORIENTED_EDGE('',*,*,#39014,.F.) ;
#52659 = ORIENTED_EDGE('',*,*,#38769,.F.) ;
#52660 = ORIENTED_EDGE('',*,*,#39013,.T.) ;
#52661 = ORIENTED_EDGE('',*,*,#38931,.F.) ;
#52662 = ORIENTED_EDGE('',*,*,#39015,.F.) ;
#52663 = ORIENTED_EDGE('',*,*,#38926,.F.) ;
#52664 = ORIENTED_EDGE('',*,*,#39014,.T.) ;
#52665 = ORIENTED_EDGE('',*,*,#38923,.F.) ;
#52666 = ORIENTED_EDGE('',*,*,#39016,.F.) ;
#52667 = ORIENTED_EDGE('',*,*,#38927,.F.) ;
#52668 = ORIENTED_EDGE('',*,*,#39015,.T.) ;
#52669 = ORIENTED_EDGE('',*,*,#38765,.F.) ;
#52670 = ORIENTED_EDGE('',*,*,#39017,.F.) ;
#52671 = ORIENTED_EDGE('',*,*,#38721,.F.) ;
#52672 = ORIENTED_EDGE('',*,*,#39016,.T.) ;
#52673 = ORIENTED_EDGE('',*,*,#38751,.F.) ;
#52674 = ORIENTED_EDGE('',*,*,#39018,.F.) ;
#52675 = ORIENTED_EDGE('',*,*,#38747,.F.) ;
#52676 = ORIENTED_EDGE('',*,*,#39017,.T.) ;
#52677 = ORIENTED_EDGE('',*,*,#38938,.F.) ;
#52678 = ORIENTED_EDGE('',*,*,#39018,.T.) ;
#52679 = ORIENTED_EDGE('',*,*,#38939,.F.) ;
#52680 = ORIENTED_EDGE('',*,*,#39019,.T.) ;
#52681 = ORIENTED_EDGE('',*,*,#38942,.F.) ;
#52682 = ORIENTED_EDGE('',*,*,#39020,.F.) ;
#52683 = ORIENTED_EDGE('',*,*,#38944,.F.) ;
#52684 = ORIENTED_EDGE('',*,*,#39019,.F.) ;
#52685 = ORIENTED_EDGE('',*,*,#38697,.F.) ;
#52686 = ORIENTED_EDGE('',*,*,#39021,.F.) ;
#52687 = ORIENTED_EDGE('',*,*,#38715,.F.) ;
#52688 = ORIENTED_EDGE('',*,*,#39020,.T.) ;
#52689 = ORIENTED_EDGE('',*,*,#38712,.F.) ;
#52690 = ORIENTED_EDGE('',*,*,#39022,.F.) ;
#52691 = ORIENTED_EDGE('',*,*,#38757,.F.) ;
#52692 = ORIENTED_EDGE('',*,*,#39021,.T.) ;
#52693 = ORIENTED_EDGE('',*,*,#38955,.F.) ;
#52694 = ORIENTED_EDGE('',*,*,#39023,.F.) ;
#52695 = ORIENTED_EDGE('',*,*,#38951,.F.) ;
#52696 = ORIENTED_EDGE('',*,*,#39022,.T.) ;
#52697 = ORIENTED_EDGE('',*,*,#38943,.F.) ;
#52698 = ORIENTED_EDGE('',*,*,#39024,.F.) ;
#52699 = ORIENTED_EDGE('',*,*,#38946,.F.) ;
#52700 = ORIENTED_EDGE('',*,*,#39023,.T.) ;
#52701 = ORIENTED_EDGE('',*,*,#38761,.F.) ;
#52702 = ORIENTED_EDGE('',*,*,#39025,.F.) ;
#52703 = ORIENTED_EDGE('',*,*,#38709,.F.) ;
#52704 = ORIENTED_EDGE('',*,*,#39024,.T.) ;
#52705 = ORIENTED_EDGE('',*,*,#38718,.F.) ;
#52706 = ORIENTED_EDGE('',*,*,#39026,.F.) ;
#52707 = ORIENTED_EDGE('',*,*,#38705,.F.) ;
#52708 = ORIENTED_EDGE('',*,*,#39025,.T.) ;
#52709 = ORIENTED_EDGE('',*,*,#38957,.F.) ;
#52710 = ORIENTED_EDGE('',*,*,#39026,.T.) ;
#52711 = ORIENTED_EDGE('',*,*,#38952,.F.) ;
#52712 = ORIENTED_EDGE('',*,*,#38459,.F.) ;
#52713 = ORIENTED_EDGE('',*,*,#38429,.F.) ;
#52714 = ORIENTED_EDGE('',*,*,#39027,.F.) ;
#52715 = ORIENTED_EDGE('',*,*,#38778,.F.) ;
#52716 = ORIENTED_EDGE('',*,*,#39027,.T.) ;
#52717 = ORIENTED_EDGE('',*,*,#38880,.F.) ;
#52718 = ORIENTED_EDGE('',*,*,#38397,.F.) ;
#52719 = ORIENTED_EDGE('',*,*,#39028,.F.) ;
#52720 = ORIENTED_EDGE('',*,*,#39028,.T.) ;
#52721 = ORIENTED_EDGE('',*,*,#38776,.F.) ;
#52722 = ORIENTED_EDGE('',*,*,#39029,.F.) ;
#52723 = ORIENTED_EDGE('',*,*,#38779,.F.) ;
#52724 = ORIENTED_EDGE('',*,*,#38982,.F.) ;
#52725 = ORIENTED_EDGE('',*,*,#38980,.F.) ;
#52726 = ORIENTED_EDGE('',*,*,#39029,.T.) ;
#52727 = ORIENTED_EDGE('',*,*,#38513,.F.) ;
#52728 = ORIENTED_EDGE('',*,*,#39030,.F.) ;
#52729 = ORIENTED_EDGE('',*,*,#38508,.F.) ;
#52730 = ORIENTED_EDGE('',*,*,#38471,.F.) ;
#52731 = ORIENTED_EDGE('',*,*,#38512,.F.) ;
#52732 = ORIENTED_EDGE('',*,*,#39001,.F.) ;
#52733 = ORIENTED_EDGE('',*,*,#38374,.F.) ;
#52734 = ORIENTED_EDGE('',*,*,#39031,.F.) ;
#52735 = ORIENTED_EDGE('',*,*,#38509,.F.) ;
#52736 = ORIENTED_EDGE('',*,*,#39030,.T.) ;
#52737 = ORIENTED_EDGE('',*,*,#39031,.T.) ;
#52738 = ORIENTED_EDGE('',*,*,#38686,.F.) ;
#52739 = ORIENTED_EDGE('',*,*,#39032,.F.) ;
#52740 = ORIENTED_EDGE('',*,*,#38510,.F.) ;
#52741 = ORIENTED_EDGE('',*,*,#38992,.F.) ;
#52742 = ORIENTED_EDGE('',*,*,#38414,.F.) ;
#52743 = ORIENTED_EDGE('',*,*,#39033,.F.) ;
#52744 = ORIENTED_EDGE('',*,*,#38505,.F.) ;
#52745 = ORIENTED_EDGE('',*,*,#39032,.T.) ;
#52746 = ORIENTED_EDGE('',*,*,#38443,.F.) ;
#52747 = ORIENTED_EDGE('',*,*,#38506,.F.) ;
#52748 = ORIENTED_EDGE('',*,*,#39033,.T.) ;
#52749 = ORIENTED_EDGE('',*,*,#38413,.F.) ;
#52750 = ORIENTED_EDGE('',*,*,#39034,.T.) ;
#52751 = ORIENTED_EDGE('',*,*,#39035,.T.) ;
#52752 = ORIENTED_EDGE('',*,*,#39036,.T.) ;
#52753 = ORIENTED_EDGE('',*,*,#39037,.T.) ;
#52754 = ORIENTED_EDGE('',*,*,#39035,.F.) ;
#52755 = ORIENTED_EDGE('',*,*,#39038,.F.) ;
#52756 = ORIENTED_EDGE('',*,*,#39039,.T.) ;
#52757 = ORIENTED_EDGE('',*,*,#39040,.T.) ;
#52758 = ORIENTED_EDGE('',*,*,#39041,.F.) ;
#52759 = ORIENTED_EDGE('',*,*,#39042,.T.) ;
#52760 = ORIENTED_EDGE('',*,*,#39043,.F.) ;
#52761 = ORIENTED_EDGE('',*,*,#39044,.F.) ;
#52762 = ORIENTED_EDGE('',*,*,#39045,.T.) ;
#52763 = ORIENTED_EDGE('',*,*,#39046,.T.) ;
#52764 = ORIENTED_EDGE('',*,*,#39047,.F.) ;
#52765 = ORIENTED_EDGE('',*,*,#39048,.T.) ;
#52766 = ORIENTED_EDGE('',*,*,#39049,.F.) ;
#52767 = ORIENTED_EDGE('',*,*,#39050,.T.) ;
#52768 = ORIENTED_EDGE('',*,*,#39051,.T.) ;
#52769 = ORIENTED_EDGE('',*,*,#39052,.F.) ;
#52770 = ORIENTED_EDGE('',*,*,#39053,.F.) ;
#52771 = ORIENTED_EDGE('',*,*,#39054,.F.) ;
#52772 = ORIENTED_EDGE('',*,*,#39055,.T.) ;
#52773 = ORIENTED_EDGE('',*,*,#39046,.F.) ;
#52774 = ORIENTED_EDGE('',*,*,#39056,.T.) ;
#52775 = ORIENTED_EDGE('',*,*,#39054,.T.) ;
#52776 = ORIENTED_EDGE('',*,*,#39057,.F.) ;
#52777 = ORIENTED_EDGE('',*,*,#39058,.F.) ;
#52778 = ORIENTED_EDGE('',*,*,#39059,.F.) ;
#52779 = ORIENTED_EDGE('',*,*,#39060,.T.) ;
#52780 = ORIENTED_EDGE('',*,*,#39061,.F.) ;
#52781 = ORIENTED_EDGE('',*,*,#39062,.F.) ;
#52782 = ORIENTED_EDGE('',*,*,#39063,.F.) ;
#52783 = ORIENTED_EDGE('',*,*,#39064,.T.) ;
#52784 = ORIENTED_EDGE('',*,*,#39065,.F.) ;
#52785 = ORIENTED_EDGE('',*,*,#39066,.T.) ;
#52786 = ORIENTED_EDGE('',*,*,#39063,.T.) ;
#52787 = ORIENTED_EDGE('',*,*,#39067,.F.) ;
#52788 = ORIENTED_EDGE('',*,*,#39068,.T.) ;
#52789 = ORIENTED_EDGE('',*,*,#39069,.T.) ;
#52790 = ORIENTED_EDGE('',*,*,#39070,.F.) ;
#52791 = ORIENTED_EDGE('',*,*,#39071,.T.) ;
#52792 = ORIENTED_EDGE('',*,*,#39065,.T.) ;
#52793 = ORIENTED_EDGE('',*,*,#39072,.F.) ;
#52794 = ORIENTED_EDGE('',*,*,#39073,.T.) ;
#52795 = ORIENTED_EDGE('',*,*,#39052,.T.) ;
#52796 = ORIENTED_EDGE('',*,*,#39074,.T.) ;
#52797 = ORIENTED_EDGE('',*,*,#39048,.F.) ;
#52798 = ORIENTED_EDGE('',*,*,#39075,.F.) ;
#52799 = ORIENTED_EDGE('',*,*,#39057,.T.) ;
#52800 = ORIENTED_EDGE('',*,*,#39053,.T.) ;
#52801 = ORIENTED_EDGE('',*,*,#39075,.T.) ;
#52802 = ORIENTED_EDGE('',*,*,#39047,.T.) ;
#52803 = ORIENTED_EDGE('',*,*,#39061,.T.) ;
#52804 = ORIENTED_EDGE('',*,*,#39076,.T.) ;
#52805 = ORIENTED_EDGE('',*,*,#39073,.F.) ;
#52806 = ORIENTED_EDGE('',*,*,#39077,.F.) ;
#52807 = ORIENTED_EDGE('',*,*,#39067,.T.) ;
#52808 = ORIENTED_EDGE('',*,*,#39062,.T.) ;
#52809 = ORIENTED_EDGE('',*,*,#39077,.T.) ;
#52810 = ORIENTED_EDGE('',*,*,#39072,.T.) ;
#52811 = ORIENTED_EDGE('',*,*,#39055,.F.) ;
#52812 = ORIENTED_EDGE('',*,*,#39056,.F.) ;
#52813 = ORIENTED_EDGE('',*,*,#39045,.F.) ;
#52814 = ORIENTED_EDGE('',*,*,#39078,.F.) ;
#52815 = ORIENTED_EDGE('',*,*,#39064,.F.) ;
#52816 = ORIENTED_EDGE('',*,*,#39066,.F.) ;
#52817 = ORIENTED_EDGE('',*,*,#39071,.F.) ;
#52818 = ORIENTED_EDGE('',*,*,#39079,.F.) ;
#52819 = ORIENTED_EDGE('',*,*,#39051,.F.) ;
#52820 = ORIENTED_EDGE('',*,*,#39080,.F.) ;
#52821 = ORIENTED_EDGE('',*,*,#39042,.F.) ;
#52822 = ORIENTED_EDGE('',*,*,#39074,.F.) ;
#52823 = ORIENTED_EDGE('',*,*,#39060,.F.) ;
#52824 = ORIENTED_EDGE('',*,*,#39081,.F.) ;
#52825 = ORIENTED_EDGE('',*,*,#39068,.F.) ;
#52826 = ORIENTED_EDGE('',*,*,#39076,.F.) ;
#52827 = ORIENTED_EDGE('',*,*,#39082,.F.) ;
#52828 = ORIENTED_EDGE('',*,*,#39040,.F.) ;
#52829 = ORIENTED_EDGE('',*,*,#39083,.F.) ;
#52830 = ORIENTED_EDGE('',*,*,#39049,.T.) ;
#52831 = ORIENTED_EDGE('',*,*,#39078,.T.) ;
#52832 = ORIENTED_EDGE('',*,*,#39044,.T.) ;
#52833 = ORIENTED_EDGE('',*,*,#39070,.T.) ;
#52834 = ORIENTED_EDGE('',*,*,#39084,.T.) ;
#52835 = ORIENTED_EDGE('',*,*,#39058,.T.) ;
#52836 = ORIENTED_EDGE('',*,*,#39079,.T.) ;
#52837 = ORIENTED_EDGE('',*,*,#39082,.T.) ;
#52838 = ORIENTED_EDGE('',*,*,#39039,.F.) ;
#52839 = ORIENTED_EDGE('',*,*,#39085,.F.) ;
#52840 = ORIENTED_EDGE('',*,*,#39086,.F.) ;
#52841 = ORIENTED_EDGE('',*,*,#39041,.T.) ;
#52842 = ORIENTED_EDGE('',*,*,#39086,.T.) ;
#52843 = ORIENTED_EDGE('',*,*,#39034,.F.) ;
#52844 = ORIENTED_EDGE('',*,*,#39085,.T.) ;
#52845 = ORIENTED_EDGE('',*,*,#39038,.T.) ;
#52846 = ORIENTED_EDGE('',*,*,#39037,.F.) ;
#52847 = ORIENTED_EDGE('',*,*,#39087,.F.) ;
#52848 = ORIENTED_EDGE('',*,*,#39087,.T.) ;
#52849 = ORIENTED_EDGE('',*,*,#39036,.F.) ;
#52850 = ORIENTED_EDGE('',*,*,#39083,.T.) ;
#52851 = ORIENTED_EDGE('',*,*,#39043,.T.) ;
#52852 = ORIENTED_EDGE('',*,*,#39080,.T.) ;
#52853 = ORIENTED_EDGE('',*,*,#39050,.F.) ;
#52854 = ORIENTED_EDGE('',*,*,#39081,.T.) ;
#52855 = ORIENTED_EDGE('',*,*,#39059,.T.) ;
#52856 = ORIENTED_EDGE('',*,*,#39084,.F.) ;
#52857 = ORIENTED_EDGE('',*,*,#39069,.F.) ;
#52858 = ORIENTED_EDGE('',*,*,#39088,.F.) ;
#52859 = ORIENTED_EDGE('',*,*,#39089,.T.) ;
#52860 = ORIENTED_EDGE('',*,*,#39090,.F.) ;
#52861 = ORIENTED_EDGE('',*,*,#39091,.F.) ;
#52862 = ORIENTED_EDGE('',*,*,#39089,.F.) ;
#52863 = ORIENTED_EDGE('',*,*,#39092,.F.) ;
#52864 = ORIENTED_EDGE('',*,*,#39093,.T.) ;
#52865 = ORIENTED_EDGE('',*,*,#39094,.F.) ;
#52866 = ORIENTED_EDGE('',*,*,#39093,.F.) ;
#52867 = ORIENTED_EDGE('',*,*,#39095,.F.) ;
#52868 = ORIENTED_EDGE('',*,*,#39096,.F.) ;
#52869 = ORIENTED_EDGE('',*,*,#39097,.T.) ;
#52870 = ORIENTED_EDGE('',*,*,#39098,.F.) ;
#52871 = ORIENTED_EDGE('',*,*,#39099,.T.) ;
#52872 = ORIENTED_EDGE('',*,*,#39100,.F.) ;
#52873 = ORIENTED_EDGE('',*,*,#39101,.F.) ;
#52874 = ORIENTED_EDGE('',*,*,#39102,.F.) ;
#52875 = ORIENTED_EDGE('',*,*,#39103,.F.) ;
#52876 = ORIENTED_EDGE('',*,*,#39104,.T.) ;
#52877 = ORIENTED_EDGE('',*,*,#39105,.F.) ;
#52878 = ORIENTED_EDGE('',*,*,#39106,.T.) ;
#52879 = ORIENTED_EDGE('',*,*,#39107,.F.) ;
#52880 = ORIENTED_EDGE('',*,*,#39108,.F.) ;
#52881 = ORIENTED_EDGE('',*,*,#39106,.F.) ;
#52882 = ORIENTED_EDGE('',*,*,#39109,.F.) ;
#52883 = ORIENTED_EDGE('',*,*,#39110,.T.) ;
#52884 = ORIENTED_EDGE('',*,*,#39111,.F.) ;
#52885 = ORIENTED_EDGE('',*,*,#39110,.F.) ;
#52886 = ORIENTED_EDGE('',*,*,#39112,.F.) ;
#52887 = ORIENTED_EDGE('',*,*,#39113,.F.) ;
#52888 = ORIENTED_EDGE('',*,*,#39114,.T.) ;
#52889 = ORIENTED_EDGE('',*,*,#39115,.F.) ;
#52890 = ORIENTED_EDGE('',*,*,#39116,.T.) ;
#52891 = ORIENTED_EDGE('',*,*,#39117,.F.) ;
#52892 = ORIENTED_EDGE('',*,*,#39118,.F.) ;
#52893 = ORIENTED_EDGE('',*,*,#39119,.F.) ;
#52894 = ORIENTED_EDGE('',*,*,#39120,.F.) ;
#52895 = ORIENTED_EDGE('',*,*,#39121,.T.) ;
#52896 = ORIENTED_EDGE('',*,*,#39122,.F.) ;
#52897 = ORIENTED_EDGE('',*,*,#39123,.T.) ;
#52898 = ORIENTED_EDGE('',*,*,#39124,.F.) ;
#52899 = ORIENTED_EDGE('',*,*,#39125,.F.) ;
#52900 = ORIENTED_EDGE('',*,*,#39123,.F.) ;
#52901 = ORIENTED_EDGE('',*,*,#39126,.F.) ;
#52902 = ORIENTED_EDGE('',*,*,#39127,.T.) ;
#52903 = ORIENTED_EDGE('',*,*,#39128,.F.) ;
#52904 = ORIENTED_EDGE('',*,*,#39127,.F.) ;
#52905 = ORIENTED_EDGE('',*,*,#39129,.F.) ;
#52906 = ORIENTED_EDGE('',*,*,#39130,.F.) ;
#52907 = ORIENTED_EDGE('',*,*,#39131,.T.) ;
#52908 = ORIENTED_EDGE('',*,*,#39132,.F.) ;
#52909 = ORIENTED_EDGE('',*,*,#39133,.T.) ;
#52910 = ORIENTED_EDGE('',*,*,#39134,.F.) ;
#52911 = ORIENTED_EDGE('',*,*,#39135,.F.) ;
#52912 = ORIENTED_EDGE('',*,*,#39136,.F.) ;
#52913 = ORIENTED_EDGE('',*,*,#39137,.F.) ;
#52914 = ORIENTED_EDGE('',*,*,#39138,.T.) ;
#52915 = ORIENTED_EDGE('',*,*,#39139,.F.) ;
#52916 = ORIENTED_EDGE('',*,*,#39140,.T.) ;
#52917 = ORIENTED_EDGE('',*,*,#39141,.F.) ;
#52918 = ORIENTED_EDGE('',*,*,#39142,.F.) ;
#52919 = ORIENTED_EDGE('',*,*,#39140,.F.) ;
#52920 = ORIENTED_EDGE('',*,*,#39143,.F.) ;
#52921 = ORIENTED_EDGE('',*,*,#39144,.T.) ;
#52922 = ORIENTED_EDGE('',*,*,#39145,.F.) ;
#52923 = ORIENTED_EDGE('',*,*,#39144,.F.) ;
#52924 = ORIENTED_EDGE('',*,*,#39146,.F.) ;
#52925 = ORIENTED_EDGE('',*,*,#39147,.F.) ;
#52926 = ORIENTED_EDGE('',*,*,#39148,.T.) ;
#52927 = ORIENTED_EDGE('',*,*,#39149,.F.) ;
#52928 = ORIENTED_EDGE('',*,*,#39150,.T.) ;
#52929 = ORIENTED_EDGE('',*,*,#39151,.F.) ;
#52930 = ORIENTED_EDGE('',*,*,#39152,.F.) ;
#52931 = ORIENTED_EDGE('',*,*,#39153,.F.) ;
#52932 = ORIENTED_EDGE('',*,*,#39154,.F.) ;
#52933 = ORIENTED_EDGE('',*,*,#39155,.T.) ;
#52934 = ORIENTED_EDGE('',*,*,#39156,.F.) ;
#52935 = ORIENTED_EDGE('',*,*,#39157,.T.) ;
#52936 = ORIENTED_EDGE('',*,*,#39158,.F.) ;
#52937 = ORIENTED_EDGE('',*,*,#39159,.F.) ;
#52938 = ORIENTED_EDGE('',*,*,#39157,.F.) ;
#52939 = ORIENTED_EDGE('',*,*,#39160,.F.) ;
#52940 = ORIENTED_EDGE('',*,*,#39161,.T.) ;
#52941 = ORIENTED_EDGE('',*,*,#39162,.F.) ;
#52942 = ORIENTED_EDGE('',*,*,#39161,.F.) ;
#52943 = ORIENTED_EDGE('',*,*,#39163,.F.) ;
#52944 = ORIENTED_EDGE('',*,*,#39164,.F.) ;
#52945 = ORIENTED_EDGE('',*,*,#39165,.T.) ;
#52946 = ORIENTED_EDGE('',*,*,#39166,.F.) ;
#52947 = ORIENTED_EDGE('',*,*,#39167,.T.) ;
#52948 = ORIENTED_EDGE('',*,*,#39168,.F.) ;
#52949 = ORIENTED_EDGE('',*,*,#39169,.F.) ;
#52950 = ORIENTED_EDGE('',*,*,#39170,.F.) ;
#52951 = ORIENTED_EDGE('',*,*,#39171,.F.) ;
#52952 = ORIENTED_EDGE('',*,*,#39172,.T.) ;
#52953 = ORIENTED_EDGE('',*,*,#39173,.F.) ;
#52954 = ORIENTED_EDGE('',*,*,#39174,.T.) ;
#52955 = ORIENTED_EDGE('',*,*,#39175,.F.) ;
#52956 = ORIENTED_EDGE('',*,*,#39176,.F.) ;
#52957 = ORIENTED_EDGE('',*,*,#39174,.F.) ;
#52958 = ORIENTED_EDGE('',*,*,#39177,.F.) ;
#52959 = ORIENTED_EDGE('',*,*,#39178,.T.) ;
#52960 = ORIENTED_EDGE('',*,*,#39179,.F.) ;
#52961 = ORIENTED_EDGE('',*,*,#39178,.F.) ;
#52962 = ORIENTED_EDGE('',*,*,#39180,.F.) ;
#52963 = ORIENTED_EDGE('',*,*,#39181,.F.) ;
#52964 = ORIENTED_EDGE('',*,*,#39182,.T.) ;
#52965 = ORIENTED_EDGE('',*,*,#39183,.F.) ;
#52966 = ORIENTED_EDGE('',*,*,#39184,.T.) ;
#52967 = ORIENTED_EDGE('',*,*,#39185,.F.) ;
#52968 = ORIENTED_EDGE('',*,*,#39186,.F.) ;
#52969 = ORIENTED_EDGE('',*,*,#39187,.F.) ;
#52970 = ORIENTED_EDGE('',*,*,#39188,.F.) ;
#52971 = ORIENTED_EDGE('',*,*,#39189,.T.) ;
#52972 = ORIENTED_EDGE('',*,*,#39190,.F.) ;
#52973 = ORIENTED_EDGE('',*,*,#39191,.T.) ;
#52974 = ORIENTED_EDGE('',*,*,#39192,.F.) ;
#52975 = ORIENTED_EDGE('',*,*,#39193,.F.) ;
#52976 = ORIENTED_EDGE('',*,*,#39191,.F.) ;
#52977 = ORIENTED_EDGE('',*,*,#39194,.F.) ;
#52978 = ORIENTED_EDGE('',*,*,#39195,.T.) ;
#52979 = ORIENTED_EDGE('',*,*,#39196,.F.) ;
#52980 = ORIENTED_EDGE('',*,*,#39195,.F.) ;
#52981 = ORIENTED_EDGE('',*,*,#39197,.F.) ;
#52982 = ORIENTED_EDGE('',*,*,#39198,.F.) ;
#52983 = ORIENTED_EDGE('',*,*,#39199,.T.) ;
#52984 = ORIENTED_EDGE('',*,*,#39200,.F.) ;
#52985 = ORIENTED_EDGE('',*,*,#39201,.T.) ;
#52986 = ORIENTED_EDGE('',*,*,#39202,.F.) ;
#52987 = ORIENTED_EDGE('',*,*,#39203,.F.) ;
#52988 = ORIENTED_EDGE('',*,*,#39204,.F.) ;
#52989 = ORIENTED_EDGE('',*,*,#39205,.F.) ;
#52990 = ORIENTED_EDGE('',*,*,#39206,.T.) ;
#52991 = ORIENTED_EDGE('',*,*,#39207,.F.) ;
#52992 = ORIENTED_EDGE('',*,*,#39208,.T.) ;
#52993 = ORIENTED_EDGE('',*,*,#39209,.F.) ;
#52994 = ORIENTED_EDGE('',*,*,#39210,.F.) ;
#52995 = ORIENTED_EDGE('',*,*,#39208,.F.) ;
#52996 = ORIENTED_EDGE('',*,*,#39211,.F.) ;
#52997 = ORIENTED_EDGE('',*,*,#39212,.T.) ;
#52998 = ORIENTED_EDGE('',*,*,#39213,.F.) ;
#52999 = ORIENTED_EDGE('',*,*,#39212,.F.) ;
#53000 = ORIENTED_EDGE('',*,*,#39214,.F.) ;
#53001 = ORIENTED_EDGE('',*,*,#39215,.F.) ;
#53002 = ORIENTED_EDGE('',*,*,#39216,.T.) ;
#53003 = ORIENTED_EDGE('',*,*,#39217,.F.) ;
#53004 = ORIENTED_EDGE('',*,*,#39218,.T.) ;
#53005 = ORIENTED_EDGE('',*,*,#39219,.F.) ;
#53006 = ORIENTED_EDGE('',*,*,#39220,.F.) ;
#53007 = ORIENTED_EDGE('',*,*,#39221,.F.) ;
#53008 = ORIENTED_EDGE('',*,*,#39222,.F.) ;
#53009 = ORIENTED_EDGE('',*,*,#39223,.T.) ;
#53010 = ORIENTED_EDGE('',*,*,#39224,.F.) ;
#53011 = ORIENTED_EDGE('',*,*,#39225,.T.) ;
#53012 = ORIENTED_EDGE('',*,*,#39226,.F.) ;
#53013 = ORIENTED_EDGE('',*,*,#39227,.F.) ;
#53014 = ORIENTED_EDGE('',*,*,#39225,.F.) ;
#53015 = ORIENTED_EDGE('',*,*,#39228,.F.) ;
#53016 = ORIENTED_EDGE('',*,*,#39229,.F.) ;
#53017 = ORIENTED_EDGE('',*,*,#39230,.F.) ;
#53018 = ORIENTED_EDGE('',*,*,#39231,.T.) ;
#53019 = ORIENTED_EDGE('',*,*,#39232,.F.) ;
#53020 = ORIENTED_EDGE('',*,*,#39233,.F.) ;
#53021 = ORIENTED_EDGE('',*,*,#39234,.F.) ;
#53022 = ORIENTED_EDGE('',*,*,#39235,.T.) ;
#53023 = ORIENTED_EDGE('',*,*,#39236,.F.) ;
#53024 = ORIENTED_EDGE('',*,*,#39237,.F.) ;
#53025 = ORIENTED_EDGE('',*,*,#39238,.F.) ;
#53026 = ORIENTED_EDGE('',*,*,#39239,.T.) ;
#53027 = ORIENTED_EDGE('',*,*,#39240,.F.) ;
#53028 = ORIENTED_EDGE('',*,*,#39241,.F.) ;
#53029 = ORIENTED_EDGE('',*,*,#39242,.F.) ;
#53030 = ORIENTED_EDGE('',*,*,#39243,.T.) ;
#53031 = ORIENTED_EDGE('',*,*,#39244,.F.) ;
#53032 = ORIENTED_EDGE('',*,*,#39245,.F.) ;
#53033 = ORIENTED_EDGE('',*,*,#39246,.F.) ;
#53034 = ORIENTED_EDGE('',*,*,#39247,.T.) ;
#53035 = ORIENTED_EDGE('',*,*,#39248,.F.) ;
#53036 = ORIENTED_EDGE('',*,*,#39249,.F.) ;
#53037 = ORIENTED_EDGE('',*,*,#39250,.F.) ;
#53038 = ORIENTED_EDGE('',*,*,#39251,.T.) ;
#53039 = ORIENTED_EDGE('',*,*,#39252,.F.) ;
#53040 = ORIENTED_EDGE('',*,*,#39253,.F.) ;
#53041 = ORIENTED_EDGE('',*,*,#39254,.F.) ;
#53042 = ORIENTED_EDGE('',*,*,#39255,.T.) ;
#53043 = ORIENTED_EDGE('',*,*,#39256,.F.) ;
#53044 = ORIENTED_EDGE('',*,*,#39257,.F.) ;
#53045 = ORIENTED_EDGE('',*,*,#39258,.F.) ;
#53046 = ORIENTED_EDGE('',*,*,#39259,.T.) ;
#53047 = ORIENTED_EDGE('',*,*,#39260,.F.) ;
#53048 = ORIENTED_EDGE('',*,*,#39261,.F.) ;
#53049 = ORIENTED_EDGE('',*,*,#39262,.F.) ;
#53050 = ORIENTED_EDGE('',*,*,#39263,.T.) ;
#53051 = ORIENTED_EDGE('',*,*,#39264,.F.) ;
#53052 = ORIENTED_EDGE('',*,*,#39265,.T.) ;
#53053 = ORIENTED_EDGE('',*,*,#39266,.F.) ;
#53054 = ORIENTED_EDGE('',*,*,#39265,.F.) ;
#53055 = ORIENTED_EDGE('',*,*,#39267,.F.) ;
#53056 = ORIENTED_EDGE('',*,*,#39268,.F.) ;
#53057 = ORIENTED_EDGE('',*,*,#39269,.T.) ;
#53058 = ORIENTED_EDGE('',*,*,#39270,.F.) ;
#53059 = ORIENTED_EDGE('',*,*,#39271,.T.) ;
#53060 = ORIENTED_EDGE('',*,*,#39272,.F.) ;
#53061 = ORIENTED_EDGE('',*,*,#39273,.F.) ;
#53062 = ORIENTED_EDGE('',*,*,#39274,.F.) ;
#53063 = ORIENTED_EDGE('',*,*,#39275,.F.) ;
#53064 = ORIENTED_EDGE('',*,*,#39276,.T.) ;
#53065 = ORIENTED_EDGE('',*,*,#39094,.T.) ;
#53066 = ORIENTED_EDGE('',*,*,#39277,.T.) ;
#53067 = ORIENTED_EDGE('',*,*,#39090,.T.) ;
#53068 = ORIENTED_EDGE('',*,*,#39091,.T.) ;
#53069 = ORIENTED_EDGE('',*,*,#39277,.F.) ;
#53070 = ORIENTED_EDGE('',*,*,#39111,.T.) ;
#53071 = ORIENTED_EDGE('',*,*,#39278,.T.) ;
#53072 = ORIENTED_EDGE('',*,*,#39107,.T.) ;
#53073 = ORIENTED_EDGE('',*,*,#39108,.T.) ;
#53074 = ORIENTED_EDGE('',*,*,#39278,.F.) ;
#53075 = ORIENTED_EDGE('',*,*,#39128,.T.) ;
#53076 = ORIENTED_EDGE('',*,*,#39279,.T.) ;
#53077 = ORIENTED_EDGE('',*,*,#39124,.T.) ;
#53078 = ORIENTED_EDGE('',*,*,#39125,.T.) ;
#53079 = ORIENTED_EDGE('',*,*,#39279,.F.) ;
#53080 = ORIENTED_EDGE('',*,*,#39145,.T.) ;
#53081 = ORIENTED_EDGE('',*,*,#39280,.T.) ;
#53082 = ORIENTED_EDGE('',*,*,#39141,.T.) ;
#53083 = ORIENTED_EDGE('',*,*,#39142,.T.) ;
#53084 = ORIENTED_EDGE('',*,*,#39280,.F.) ;
#53085 = ORIENTED_EDGE('',*,*,#39162,.T.) ;
#53086 = ORIENTED_EDGE('',*,*,#39281,.T.) ;
#53087 = ORIENTED_EDGE('',*,*,#39158,.T.) ;
#53088 = ORIENTED_EDGE('',*,*,#39159,.T.) ;
#53089 = ORIENTED_EDGE('',*,*,#39281,.F.) ;
#53090 = ORIENTED_EDGE('',*,*,#39179,.T.) ;
#53091 = ORIENTED_EDGE('',*,*,#39282,.T.) ;
#53092 = ORIENTED_EDGE('',*,*,#39175,.T.) ;
#53093 = ORIENTED_EDGE('',*,*,#39176,.T.) ;
#53094 = ORIENTED_EDGE('',*,*,#39282,.F.) ;
#53095 = ORIENTED_EDGE('',*,*,#39196,.T.) ;
#53096 = ORIENTED_EDGE('',*,*,#39283,.T.) ;
#53097 = ORIENTED_EDGE('',*,*,#39192,.T.) ;
#53098 = ORIENTED_EDGE('',*,*,#39193,.T.) ;
#53099 = ORIENTED_EDGE('',*,*,#39283,.F.) ;
#53100 = ORIENTED_EDGE('',*,*,#39213,.T.) ;
#53101 = ORIENTED_EDGE('',*,*,#39284,.T.) ;
#53102 = ORIENTED_EDGE('',*,*,#39209,.T.) ;
#53103 = ORIENTED_EDGE('',*,*,#39210,.T.) ;
#53104 = ORIENTED_EDGE('',*,*,#39284,.F.) ;
#53105 = ORIENTED_EDGE('',*,*,#39266,.T.) ;
#53106 = ORIENTED_EDGE('',*,*,#39285,.T.) ;
#53107 = ORIENTED_EDGE('',*,*,#39226,.T.) ;
#53108 = ORIENTED_EDGE('',*,*,#39227,.T.) ;
#53109 = ORIENTED_EDGE('',*,*,#39285,.F.) ;
#53110 = ORIENTED_EDGE('',*,*,#39286,.T.) ;
#53111 = ORIENTED_EDGE('',*,*,#39287,.T.) ;
#53112 = ORIENTED_EDGE('',*,*,#39230,.T.) ;
#53113 = ORIENTED_EDGE('',*,*,#39288,.F.) ;
#53114 = ORIENTED_EDGE('',*,*,#39289,.T.) ;
#53115 = ORIENTED_EDGE('',*,*,#39290,.T.) ;
#53116 = ORIENTED_EDGE('',*,*,#39234,.T.) ;
#53117 = ORIENTED_EDGE('',*,*,#39291,.F.) ;
#53118 = ORIENTED_EDGE('',*,*,#39292,.T.) ;
#53119 = ORIENTED_EDGE('',*,*,#39293,.T.) ;
#53120 = ORIENTED_EDGE('',*,*,#39238,.T.) ;
#53121 = ORIENTED_EDGE('',*,*,#39294,.F.) ;
#53122 = ORIENTED_EDGE('',*,*,#39295,.T.) ;
#53123 = ORIENTED_EDGE('',*,*,#39296,.T.) ;
#53124 = ORIENTED_EDGE('',*,*,#39242,.T.) ;
#53125 = ORIENTED_EDGE('',*,*,#39297,.F.) ;
#53126 = ORIENTED_EDGE('',*,*,#39298,.T.) ;
#53127 = ORIENTED_EDGE('',*,*,#39299,.T.) ;
#53128 = ORIENTED_EDGE('',*,*,#39246,.T.) ;
#53129 = ORIENTED_EDGE('',*,*,#39300,.F.) ;
#53130 = ORIENTED_EDGE('',*,*,#39301,.T.) ;
#53131 = ORIENTED_EDGE('',*,*,#39302,.T.) ;
#53132 = ORIENTED_EDGE('',*,*,#39250,.T.) ;
#53133 = ORIENTED_EDGE('',*,*,#39303,.F.) ;
#53134 = ORIENTED_EDGE('',*,*,#39304,.T.) ;
#53135 = ORIENTED_EDGE('',*,*,#39305,.T.) ;
#53136 = ORIENTED_EDGE('',*,*,#39254,.T.) ;
#53137 = ORIENTED_EDGE('',*,*,#39306,.F.) ;
#53138 = ORIENTED_EDGE('',*,*,#39307,.T.) ;
#53139 = ORIENTED_EDGE('',*,*,#39308,.T.) ;
#53140 = ORIENTED_EDGE('',*,*,#39258,.T.) ;
#53141 = ORIENTED_EDGE('',*,*,#39309,.F.) ;
#53142 = ORIENTED_EDGE('',*,*,#39310,.T.) ;
#53143 = ORIENTED_EDGE('',*,*,#39311,.T.) ;
#53144 = ORIENTED_EDGE('',*,*,#39262,.T.) ;
#53145 = ORIENTED_EDGE('',*,*,#39312,.F.) ;
#53146 = ORIENTED_EDGE('',*,*,#39313,.F.) ;
#53147 = ORIENTED_EDGE('',*,*,#39314,.T.) ;
#53148 = ORIENTED_EDGE('',*,*,#39315,.F.) ;
#53149 = ORIENTED_EDGE('',*,*,#39316,.F.) ;
#53150 = ORIENTED_EDGE('',*,*,#39314,.F.) ;
#53151 = ORIENTED_EDGE('',*,*,#39317,.F.) ;
#53152 = ORIENTED_EDGE('',*,*,#39318,.F.) ;
#53153 = ORIENTED_EDGE('',*,*,#39319,.F.) ;
#53154 = ORIENTED_EDGE('',*,*,#39320,.T.) ;
#53155 = ORIENTED_EDGE('',*,*,#39321,.F.) ;
#53156 = ORIENTED_EDGE('',*,*,#39322,.T.) ;
#53157 = ORIENTED_EDGE('',*,*,#39323,.F.) ;
#53158 = ORIENTED_EDGE('',*,*,#39322,.F.) ;
#53159 = ORIENTED_EDGE('',*,*,#39324,.F.) ;
#53160 = ORIENTED_EDGE('',*,*,#39325,.F.) ;
#53161 = ORIENTED_EDGE('',*,*,#39326,.T.) ;
#53162 = ORIENTED_EDGE('',*,*,#39327,.F.) ;
#53163 = ORIENTED_EDGE('',*,*,#39328,.T.) ;
#53164 = ORIENTED_EDGE('',*,*,#39329,.F.) ;
#53165 = ORIENTED_EDGE('',*,*,#39330,.F.) ;
#53166 = ORIENTED_EDGE('',*,*,#39331,.F.) ;
#53167 = ORIENTED_EDGE('',*,*,#39332,.F.) ;
#53168 = ORIENTED_EDGE('',*,*,#39333,.T.) ;
#53169 = ORIENTED_EDGE('',*,*,#39323,.T.) ;
#53170 = ORIENTED_EDGE('',*,*,#39334,.T.) ;
#53171 = ORIENTED_EDGE('',*,*,#39315,.T.) ;
#53172 = ORIENTED_EDGE('',*,*,#39316,.T.) ;
#53173 = ORIENTED_EDGE('',*,*,#39334,.F.) ;
#53174 = ORIENTED_EDGE('',*,*,#39335,.T.) ;
#53175 = ORIENTED_EDGE('',*,*,#39336,.T.) ;
#53176 = ORIENTED_EDGE('',*,*,#39319,.T.) ;
#53177 = ORIENTED_EDGE('',*,*,#39337,.F.) ;
#53178 = ORIENTED_EDGE('',*,*,#39338,.T.) ;
#53179 = ORIENTED_EDGE('',*,*,#39339,.T.) ;
#53180 = ORIENTED_EDGE('',*,*,#39340,.T.) ;
#53181 = ORIENTED_EDGE('',*,*,#39341,.T.) ;
#53182 = ORIENTED_EDGE('',*,*,#39102,.T.) ;
#53183 = ORIENTED_EDGE('',*,*,#39342,.F.) ;
#53184 = ORIENTED_EDGE('',*,*,#39343,.T.) ;
#53185 = ORIENTED_EDGE('',*,*,#39344,.T.) ;
#53186 = ORIENTED_EDGE('',*,*,#39345,.T.) ;
#53187 = ORIENTED_EDGE('',*,*,#39346,.T.) ;
#53188 = ORIENTED_EDGE('',*,*,#39347,.T.) ;
#53189 = ORIENTED_EDGE('',*,*,#39348,.F.) ;
#53190 = ORIENTED_EDGE('',*,*,#39349,.T.) ;
#53191 = ORIENTED_EDGE('',*,*,#39350,.T.) ;
#53192 = ORIENTED_EDGE('',*,*,#39351,.T.) ;
#53193 = ORIENTED_EDGE('',*,*,#39352,.T.) ;
#53194 = ORIENTED_EDGE('',*,*,#39119,.T.) ;
#53195 = ORIENTED_EDGE('',*,*,#39353,.F.) ;
#53196 = ORIENTED_EDGE('',*,*,#39354,.T.) ;
#53197 = ORIENTED_EDGE('',*,*,#39355,.T.) ;
#53198 = ORIENTED_EDGE('',*,*,#39356,.T.) ;
#53199 = ORIENTED_EDGE('',*,*,#39357,.T.) ;
#53200 = ORIENTED_EDGE('',*,*,#39358,.T.) ;
#53201 = ORIENTED_EDGE('',*,*,#39359,.F.) ;
#53202 = ORIENTED_EDGE('',*,*,#39360,.T.) ;
#53203 = ORIENTED_EDGE('',*,*,#39361,.T.) ;
#53204 = ORIENTED_EDGE('',*,*,#39362,.T.) ;
#53205 = ORIENTED_EDGE('',*,*,#39363,.T.) ;
#53206 = ORIENTED_EDGE('',*,*,#39136,.T.) ;
#53207 = ORIENTED_EDGE('',*,*,#39364,.F.) ;
#53208 = ORIENTED_EDGE('',*,*,#39365,.T.) ;
#53209 = ORIENTED_EDGE('',*,*,#39366,.T.) ;
#53210 = ORIENTED_EDGE('',*,*,#39367,.T.) ;
#53211 = ORIENTED_EDGE('',*,*,#39368,.T.) ;
#53212 = ORIENTED_EDGE('',*,*,#39369,.T.) ;
#53213 = ORIENTED_EDGE('',*,*,#39370,.F.) ;
#53214 = ORIENTED_EDGE('',*,*,#39371,.T.) ;
#53215 = ORIENTED_EDGE('',*,*,#39372,.T.) ;
#53216 = ORIENTED_EDGE('',*,*,#39373,.T.) ;
#53217 = ORIENTED_EDGE('',*,*,#39374,.T.) ;
#53218 = ORIENTED_EDGE('',*,*,#39153,.T.) ;
#53219 = ORIENTED_EDGE('',*,*,#39375,.F.) ;
#53220 = ORIENTED_EDGE('',*,*,#39376,.T.) ;
#53221 = ORIENTED_EDGE('',*,*,#39377,.T.) ;
#53222 = ORIENTED_EDGE('',*,*,#39378,.T.) ;
#53223 = ORIENTED_EDGE('',*,*,#39379,.T.) ;
#53224 = ORIENTED_EDGE('',*,*,#39380,.T.) ;
#53225 = ORIENTED_EDGE('',*,*,#39381,.F.) ;
#53226 = ORIENTED_EDGE('',*,*,#39382,.T.) ;
#53227 = ORIENTED_EDGE('',*,*,#39383,.T.) ;
#53228 = ORIENTED_EDGE('',*,*,#39384,.T.) ;
#53229 = ORIENTED_EDGE('',*,*,#39385,.T.) ;
#53230 = ORIENTED_EDGE('',*,*,#39170,.T.) ;
#53231 = ORIENTED_EDGE('',*,*,#39386,.F.) ;
#53232 = ORIENTED_EDGE('',*,*,#39387,.T.) ;
#53233 = ORIENTED_EDGE('',*,*,#39388,.T.) ;
#53234 = ORIENTED_EDGE('',*,*,#39389,.T.) ;
#53235 = ORIENTED_EDGE('',*,*,#39390,.T.) ;
#53236 = ORIENTED_EDGE('',*,*,#39391,.T.) ;
#53237 = ORIENTED_EDGE('',*,*,#39392,.F.) ;
#53238 = ORIENTED_EDGE('',*,*,#39393,.T.) ;
#53239 = ORIENTED_EDGE('',*,*,#39394,.T.) ;
#53240 = ORIENTED_EDGE('',*,*,#39395,.T.) ;
#53241 = ORIENTED_EDGE('',*,*,#39396,.T.) ;
#53242 = ORIENTED_EDGE('',*,*,#39187,.T.) ;
#53243 = ORIENTED_EDGE('',*,*,#39397,.F.) ;
#53244 = ORIENTED_EDGE('',*,*,#39398,.T.) ;
#53245 = ORIENTED_EDGE('',*,*,#39399,.T.) ;
#53246 = ORIENTED_EDGE('',*,*,#39400,.T.) ;
#53247 = ORIENTED_EDGE('',*,*,#39401,.T.) ;
#53248 = ORIENTED_EDGE('',*,*,#39402,.T.) ;
#53249 = ORIENTED_EDGE('',*,*,#39403,.F.) ;
#53250 = ORIENTED_EDGE('',*,*,#39404,.T.) ;
#53251 = ORIENTED_EDGE('',*,*,#39405,.T.) ;
#53252 = ORIENTED_EDGE('',*,*,#39406,.T.) ;
#53253 = ORIENTED_EDGE('',*,*,#39407,.T.) ;
#53254 = ORIENTED_EDGE('',*,*,#39204,.T.) ;
#53255 = ORIENTED_EDGE('',*,*,#39408,.F.) ;
#53256 = ORIENTED_EDGE('',*,*,#39409,.T.) ;
#53257 = ORIENTED_EDGE('',*,*,#39410,.T.) ;
#53258 = ORIENTED_EDGE('',*,*,#39411,.T.) ;
#53259 = ORIENTED_EDGE('',*,*,#39412,.T.) ;
#53260 = ORIENTED_EDGE('',*,*,#39413,.T.) ;
#53261 = ORIENTED_EDGE('',*,*,#39414,.F.) ;
#53262 = ORIENTED_EDGE('',*,*,#39415,.T.) ;
#53263 = ORIENTED_EDGE('',*,*,#39416,.T.) ;
#53264 = ORIENTED_EDGE('',*,*,#39417,.T.) ;
#53265 = ORIENTED_EDGE('',*,*,#39418,.T.) ;
#53266 = ORIENTED_EDGE('',*,*,#39221,.T.) ;
#53267 = ORIENTED_EDGE('',*,*,#39419,.F.) ;
#53268 = ORIENTED_EDGE('',*,*,#39420,.T.) ;
#53269 = ORIENTED_EDGE('',*,*,#39421,.T.) ;
#53270 = ORIENTED_EDGE('',*,*,#39422,.T.) ;
#53271 = ORIENTED_EDGE('',*,*,#39423,.T.) ;
#53272 = ORIENTED_EDGE('',*,*,#39424,.T.) ;
#53273 = ORIENTED_EDGE('',*,*,#39425,.F.) ;
#53274 = ORIENTED_EDGE('',*,*,#39426,.T.) ;
#53275 = ORIENTED_EDGE('',*,*,#39427,.T.) ;
#53276 = ORIENTED_EDGE('',*,*,#39428,.T.) ;
#53277 = ORIENTED_EDGE('',*,*,#39429,.T.) ;
#53278 = ORIENTED_EDGE('',*,*,#39274,.T.) ;
#53279 = ORIENTED_EDGE('',*,*,#39430,.F.) ;
#53280 = ORIENTED_EDGE('',*,*,#39431,.T.) ;
#53281 = ORIENTED_EDGE('',*,*,#39432,.T.) ;
#53282 = ORIENTED_EDGE('',*,*,#39433,.T.) ;
#53283 = ORIENTED_EDGE('',*,*,#39434,.T.) ;
#53284 = ORIENTED_EDGE('',*,*,#39435,.T.) ;
#53285 = ORIENTED_EDGE('',*,*,#39436,.F.) ;
#53286 = ORIENTED_EDGE('',*,*,#39437,.F.) ;
#53287 = ORIENTED_EDGE('',*,*,#39438,.T.) ;
#53288 = ORIENTED_EDGE('',*,*,#39439,.T.) ;
#53289 = ORIENTED_EDGE('',*,*,#39440,.T.) ;
#53290 = ORIENTED_EDGE('',*,*,#39441,.T.) ;
#53291 = ORIENTED_EDGE('',*,*,#39442,.F.) ;
#53292 = ORIENTED_EDGE('',*,*,#39443,.T.) ;
#53293 = ORIENTED_EDGE('',*,*,#39444,.T.) ;
#53294 = ORIENTED_EDGE('',*,*,#39445,.T.) ;
#53295 = ORIENTED_EDGE('',*,*,#39446,.T.) ;
#53296 = ORIENTED_EDGE('',*,*,#39447,.F.) ;
#53297 = ORIENTED_EDGE('',*,*,#39448,.T.) ;
#53298 = ORIENTED_EDGE('',*,*,#39449,.T.) ;
#53299 = ORIENTED_EDGE('',*,*,#39450,.T.) ;
#53300 = ORIENTED_EDGE('',*,*,#39451,.T.) ;
#53301 = ORIENTED_EDGE('',*,*,#39452,.F.) ;
#53302 = ORIENTED_EDGE('',*,*,#39453,.T.) ;
#53303 = ORIENTED_EDGE('',*,*,#39454,.T.) ;
#53304 = ORIENTED_EDGE('',*,*,#39455,.T.) ;
#53305 = ORIENTED_EDGE('',*,*,#39456,.T.) ;
#53306 = ORIENTED_EDGE('',*,*,#39457,.F.) ;
#53307 = ORIENTED_EDGE('',*,*,#39458,.T.) ;
#53308 = ORIENTED_EDGE('',*,*,#39459,.T.) ;
#53309 = ORIENTED_EDGE('',*,*,#39460,.T.) ;
#53310 = ORIENTED_EDGE('',*,*,#39461,.T.) ;
#53311 = ORIENTED_EDGE('',*,*,#39462,.F.) ;
#53312 = ORIENTED_EDGE('',*,*,#39463,.T.) ;
#53313 = ORIENTED_EDGE('',*,*,#39464,.T.) ;
#53314 = ORIENTED_EDGE('',*,*,#39465,.T.) ;
#53315 = ORIENTED_EDGE('',*,*,#39466,.T.) ;
#53316 = ORIENTED_EDGE('',*,*,#39467,.F.) ;
#53317 = ORIENTED_EDGE('',*,*,#39468,.T.) ;
#53318 = ORIENTED_EDGE('',*,*,#39469,.T.) ;
#53319 = ORIENTED_EDGE('',*,*,#39470,.T.) ;
#53320 = ORIENTED_EDGE('',*,*,#39471,.T.) ;
#53321 = ORIENTED_EDGE('',*,*,#39472,.F.) ;
#53322 = ORIENTED_EDGE('',*,*,#39473,.T.) ;
#53323 = ORIENTED_EDGE('',*,*,#39474,.T.) ;
#53324 = ORIENTED_EDGE('',*,*,#39475,.T.) ;
#53325 = ORIENTED_EDGE('',*,*,#39476,.T.) ;
#53326 = ORIENTED_EDGE('',*,*,#39477,.F.) ;
#53327 = ORIENTED_EDGE('',*,*,#39478,.T.) ;
#53328 = ORIENTED_EDGE('',*,*,#39479,.T.) ;
#53329 = ORIENTED_EDGE('',*,*,#39480,.T.) ;
#53330 = ORIENTED_EDGE('',*,*,#39481,.T.) ;
#53331 = ORIENTED_EDGE('',*,*,#39482,.F.) ;
#53332 = ORIENTED_EDGE('',*,*,#39483,.T.) ;
#53333 = ORIENTED_EDGE('',*,*,#39484,.T.) ;
#53334 = ORIENTED_EDGE('',*,*,#39485,.T.) ;
#53335 = ORIENTED_EDGE('',*,*,#39486,.T.) ;
#53336 = ORIENTED_EDGE('',*,*,#39487,.F.) ;
#53337 = ORIENTED_EDGE('',*,*,#39488,.T.) ;
#53338 = ORIENTED_EDGE('',*,*,#39489,.T.) ;
#53339 = ORIENTED_EDGE('',*,*,#39490,.T.) ;
#53340 = ORIENTED_EDGE('',*,*,#39491,.T.) ;
#53341 = ORIENTED_EDGE('',*,*,#39492,.F.) ;
#53342 = ORIENTED_EDGE('',*,*,#39493,.T.) ;
#53343 = ORIENTED_EDGE('',*,*,#39494,.T.) ;
#53344 = ORIENTED_EDGE('',*,*,#39495,.T.) ;
#53345 = ORIENTED_EDGE('',*,*,#39496,.T.) ;
#53346 = ORIENTED_EDGE('',*,*,#39497,.F.) ;
#53347 = ORIENTED_EDGE('',*,*,#39498,.T.) ;
#53348 = ORIENTED_EDGE('',*,*,#39499,.T.) ;
#53349 = ORIENTED_EDGE('',*,*,#39500,.T.) ;
#53350 = ORIENTED_EDGE('',*,*,#39501,.T.) ;
#53351 = ORIENTED_EDGE('',*,*,#39502,.F.) ;
#53352 = ORIENTED_EDGE('',*,*,#39503,.T.) ;
#53353 = ORIENTED_EDGE('',*,*,#39504,.T.) ;
#53354 = ORIENTED_EDGE('',*,*,#39505,.T.) ;
#53355 = ORIENTED_EDGE('',*,*,#39506,.T.) ;
#53356 = ORIENTED_EDGE('',*,*,#39507,.F.) ;
#53357 = ORIENTED_EDGE('',*,*,#39508,.T.) ;
#53358 = ORIENTED_EDGE('',*,*,#39509,.T.) ;
#53359 = ORIENTED_EDGE('',*,*,#39510,.T.) ;
#53360 = ORIENTED_EDGE('',*,*,#39511,.T.) ;
#53361 = ORIENTED_EDGE('',*,*,#39512,.F.) ;
#53362 = ORIENTED_EDGE('',*,*,#39513,.T.) ;
#53363 = ORIENTED_EDGE('',*,*,#39514,.T.) ;
#53364 = ORIENTED_EDGE('',*,*,#39515,.T.) ;
#53365 = ORIENTED_EDGE('',*,*,#39516,.T.) ;
#53366 = ORIENTED_EDGE('',*,*,#39517,.F.) ;
#53367 = ORIENTED_EDGE('',*,*,#39518,.T.) ;
#53368 = ORIENTED_EDGE('',*,*,#39519,.T.) ;
#53369 = ORIENTED_EDGE('',*,*,#39520,.T.) ;
#53370 = ORIENTED_EDGE('',*,*,#39521,.T.) ;
#53371 = ORIENTED_EDGE('',*,*,#39522,.F.) ;
#53372 = ORIENTED_EDGE('',*,*,#39523,.T.) ;
#53373 = ORIENTED_EDGE('',*,*,#39524,.T.) ;
#53374 = ORIENTED_EDGE('',*,*,#39525,.T.) ;
#53375 = ORIENTED_EDGE('',*,*,#39526,.T.) ;
#53376 = ORIENTED_EDGE('',*,*,#39527,.F.) ;
#53377 = ORIENTED_EDGE('',*,*,#39528,.T.) ;
#53378 = ORIENTED_EDGE('',*,*,#39529,.T.) ;
#53379 = ORIENTED_EDGE('',*,*,#39530,.T.) ;
#53380 = ORIENTED_EDGE('',*,*,#39531,.F.) ;
#53381 = ORIENTED_EDGE('',*,*,#39532,.T.) ;
#53382 = ORIENTED_EDGE('',*,*,#39533,.T.) ;
#53383 = ORIENTED_EDGE('',*,*,#39534,.T.) ;
#53384 = ORIENTED_EDGE('',*,*,#39535,.F.) ;
#53385 = ORIENTED_EDGE('',*,*,#39536,.T.) ;
#53386 = ORIENTED_EDGE('',*,*,#39537,.T.) ;
#53387 = ORIENTED_EDGE('',*,*,#39538,.T.) ;
#53388 = ORIENTED_EDGE('',*,*,#39539,.F.) ;
#53389 = ORIENTED_EDGE('',*,*,#39540,.T.) ;
#53390 = ORIENTED_EDGE('',*,*,#39541,.T.) ;
#53391 = ORIENTED_EDGE('',*,*,#39542,.T.) ;
#53392 = ORIENTED_EDGE('',*,*,#39543,.F.) ;
#53393 = ORIENTED_EDGE('',*,*,#39544,.T.) ;
#53394 = ORIENTED_EDGE('',*,*,#39545,.T.) ;
#53395 = ORIENTED_EDGE('',*,*,#39546,.T.) ;
#53396 = ORIENTED_EDGE('',*,*,#39547,.F.) ;
#53397 = ORIENTED_EDGE('',*,*,#39548,.T.) ;
#53398 = ORIENTED_EDGE('',*,*,#39549,.T.) ;
#53399 = ORIENTED_EDGE('',*,*,#39550,.T.) ;
#53400 = ORIENTED_EDGE('',*,*,#39551,.F.) ;
#53401 = ORIENTED_EDGE('',*,*,#39552,.T.) ;
#53402 = ORIENTED_EDGE('',*,*,#39553,.T.) ;
#53403 = ORIENTED_EDGE('',*,*,#39554,.T.) ;
#53404 = ORIENTED_EDGE('',*,*,#39555,.F.) ;
#53405 = ORIENTED_EDGE('',*,*,#39556,.T.) ;
#53406 = ORIENTED_EDGE('',*,*,#39557,.T.) ;
#53407 = ORIENTED_EDGE('',*,*,#39558,.T.) ;
#53408 = ORIENTED_EDGE('',*,*,#39559,.F.) ;
#53409 = ORIENTED_EDGE('',*,*,#39560,.T.) ;
#53410 = ORIENTED_EDGE('',*,*,#39561,.T.) ;
#53411 = ORIENTED_EDGE('',*,*,#39562,.T.) ;
#53412 = ORIENTED_EDGE('',*,*,#39563,.T.) ;
#53413 = ORIENTED_EDGE('',*,*,#39564,.T.) ;
#53414 = ORIENTED_EDGE('',*,*,#39565,.T.) ;
#53415 = ORIENTED_EDGE('',*,*,#39566,.T.) ;
#53416 = ORIENTED_EDGE('',*,*,#39331,.T.) ;
#53417 = ORIENTED_EDGE('',*,*,#39567,.F.) ;
#53418 = ORIENTED_EDGE('',*,*,#39568,.T.) ;
#53419 = ORIENTED_EDGE('',*,*,#39569,.T.) ;
#53420 = ORIENTED_EDGE('',*,*,#39570,.T.) ;
#53421 = ORIENTED_EDGE('',*,*,#39571,.T.) ;
#53422 = ORIENTED_EDGE('',*,*,#39572,.T.) ;
#53423 = ORIENTED_EDGE('',*,*,#39573,.F.) ;
#53424 = ORIENTED_EDGE('',*,*,#39574,.F.) ;
#53425 = ORIENTED_EDGE('',*,*,#39575,.T.) ;
#53426 = ORIENTED_EDGE('',*,*,#39576,.T.) ;
#53427 = ORIENTED_EDGE('',*,*,#39577,.T.) ;
#53428 = ORIENTED_EDGE('',*,*,#39578,.T.) ;
#53429 = ORIENTED_EDGE('',*,*,#39579,.F.) ;
#53430 = ORIENTED_EDGE('',*,*,#39580,.T.) ;
#53431 = ORIENTED_EDGE('',*,*,#39581,.T.) ;
#53432 = ORIENTED_EDGE('',*,*,#39582,.T.) ;
#53433 = ORIENTED_EDGE('',*,*,#39583,.T.) ;
#53434 = ORIENTED_EDGE('',*,*,#39584,.F.) ;
#53435 = ORIENTED_EDGE('',*,*,#39585,.T.) ;
#53436 = ORIENTED_EDGE('',*,*,#39586,.T.) ;
#53437 = ORIENTED_EDGE('',*,*,#39587,.T.) ;
#53438 = ORIENTED_EDGE('',*,*,#39588,.F.) ;
#53439 = ORIENTED_EDGE('',*,*,#39589,.T.) ;
#53440 = ORIENTED_EDGE('',*,*,#39590,.T.) ;
#53441 = ORIENTED_EDGE('',*,*,#39591,.T.) ;
#53442 = ORIENTED_EDGE('',*,*,#39592,.F.) ;
#53443 = ORIENTED_EDGE('',*,*,#39593,.T.) ;
#53444 = ORIENTED_EDGE('',*,*,#39594,.F.) ;
#53445 = ORIENTED_EDGE('',*,*,#39595,.T.) ;
#53446 = ORIENTED_EDGE('',*,*,#39588,.T.) ;
#53447 = ORIENTED_EDGE('',*,*,#39596,.T.) ;
#53448 = ORIENTED_EDGE('',*,*,#39586,.F.) ;
#53449 = ORIENTED_EDGE('',*,*,#39597,.T.) ;
#53450 = ORIENTED_EDGE('',*,*,#39598,.F.) ;
#53451 = ORIENTED_EDGE('',*,*,#39599,.T.) ;
#53452 = ORIENTED_EDGE('',*,*,#39600,.F.) ;
#53453 = ORIENTED_EDGE('',*,*,#39601,.T.) ;
#53454 = ORIENTED_EDGE('',*,*,#39529,.F.) ;
#53455 = ORIENTED_EDGE('',*,*,#39602,.T.) ;
#53456 = ORIENTED_EDGE('',*,*,#39603,.F.) ;
#53457 = ORIENTED_EDGE('',*,*,#39604,.T.) ;
#53458 = ORIENTED_EDGE('',*,*,#39605,.F.) ;
#53459 = ORIENTED_EDGE('',*,*,#39606,.T.) ;
#53460 = ORIENTED_EDGE('',*,*,#39533,.F.) ;
#53461 = ORIENTED_EDGE('',*,*,#39607,.T.) ;
#53462 = ORIENTED_EDGE('',*,*,#39608,.F.) ;
#53463 = ORIENTED_EDGE('',*,*,#39609,.T.) ;
#53464 = ORIENTED_EDGE('',*,*,#39610,.F.) ;
#53465 = ORIENTED_EDGE('',*,*,#39611,.T.) ;
#53466 = ORIENTED_EDGE('',*,*,#39537,.F.) ;
#53467 = ORIENTED_EDGE('',*,*,#39612,.T.) ;
#53468 = ORIENTED_EDGE('',*,*,#39613,.F.) ;
#53469 = ORIENTED_EDGE('',*,*,#39614,.T.) ;
#53470 = ORIENTED_EDGE('',*,*,#39615,.F.) ;
#53471 = ORIENTED_EDGE('',*,*,#39616,.T.) ;
#53472 = ORIENTED_EDGE('',*,*,#39541,.F.) ;
#53473 = ORIENTED_EDGE('',*,*,#39617,.T.) ;
#53474 = ORIENTED_EDGE('',*,*,#39618,.F.) ;
#53475 = ORIENTED_EDGE('',*,*,#39619,.T.) ;
#53476 = ORIENTED_EDGE('',*,*,#39620,.F.) ;
#53477 = ORIENTED_EDGE('',*,*,#39621,.T.) ;
#53478 = ORIENTED_EDGE('',*,*,#39545,.F.) ;
#53479 = ORIENTED_EDGE('',*,*,#39622,.T.) ;
#53480 = ORIENTED_EDGE('',*,*,#39623,.F.) ;
#53481 = ORIENTED_EDGE('',*,*,#39624,.T.) ;
#53482 = ORIENTED_EDGE('',*,*,#39625,.F.) ;
#53483 = ORIENTED_EDGE('',*,*,#39626,.T.) ;
#53484 = ORIENTED_EDGE('',*,*,#39549,.F.) ;
#53485 = ORIENTED_EDGE('',*,*,#39627,.T.) ;
#53486 = ORIENTED_EDGE('',*,*,#39628,.F.) ;
#53487 = ORIENTED_EDGE('',*,*,#39629,.T.) ;
#53488 = ORIENTED_EDGE('',*,*,#39630,.F.) ;
#53489 = ORIENTED_EDGE('',*,*,#39631,.T.) ;
#53490 = ORIENTED_EDGE('',*,*,#39553,.F.) ;
#53491 = ORIENTED_EDGE('',*,*,#39632,.T.) ;
#53492 = ORIENTED_EDGE('',*,*,#39633,.F.) ;
#53493 = ORIENTED_EDGE('',*,*,#39634,.T.) ;
#53494 = ORIENTED_EDGE('',*,*,#39635,.F.) ;
#53495 = ORIENTED_EDGE('',*,*,#39636,.T.) ;
#53496 = ORIENTED_EDGE('',*,*,#39557,.F.) ;
#53497 = ORIENTED_EDGE('',*,*,#39637,.T.) ;
#53498 = ORIENTED_EDGE('',*,*,#39638,.F.) ;
#53499 = ORIENTED_EDGE('',*,*,#39639,.T.) ;
#53500 = ORIENTED_EDGE('',*,*,#39640,.F.) ;
#53501 = ORIENTED_EDGE('',*,*,#39641,.T.) ;
#53502 = ORIENTED_EDGE('',*,*,#39561,.F.) ;
#53503 = ORIENTED_EDGE('',*,*,#39642,.T.) ;
#53504 = ORIENTED_EDGE('',*,*,#39643,.F.) ;
#53505 = ORIENTED_EDGE('',*,*,#39644,.T.) ;
#53506 = ORIENTED_EDGE('',*,*,#39594,.T.) ;
#53507 = ORIENTED_EDGE('',*,*,#39645,.T.) ;
#53508 = ORIENTED_EDGE('',*,*,#39646,.F.) ;
#53509 = ORIENTED_EDGE('',*,*,#39647,.T.) ;
#53510 = ORIENTED_EDGE('',*,*,#39648,.F.) ;
#53511 = ORIENTED_EDGE('',*,*,#39649,.T.) ;
#53512 = ORIENTED_EDGE('',*,*,#39559,.T.) ;
#53513 = ORIENTED_EDGE('',*,*,#39650,.T.) ;
#53514 = ORIENTED_EDGE('',*,*,#39651,.F.) ;
#53515 = ORIENTED_EDGE('',*,*,#39652,.T.) ;
#53516 = ORIENTED_EDGE('',*,*,#39653,.F.) ;
#53517 = ORIENTED_EDGE('',*,*,#39654,.T.) ;
#53518 = ORIENTED_EDGE('',*,*,#39555,.T.) ;
#53519 = ORIENTED_EDGE('',*,*,#39655,.T.) ;
#53520 = ORIENTED_EDGE('',*,*,#39656,.F.) ;
#53521 = ORIENTED_EDGE('',*,*,#39657,.T.) ;
#53522 = ORIENTED_EDGE('',*,*,#39658,.F.) ;
#53523 = ORIENTED_EDGE('',*,*,#39659,.T.) ;
#53524 = ORIENTED_EDGE('',*,*,#39551,.T.) ;
#53525 = ORIENTED_EDGE('',*,*,#39660,.T.) ;
#53526 = ORIENTED_EDGE('',*,*,#39661,.F.) ;
#53527 = ORIENTED_EDGE('',*,*,#39662,.T.) ;
#53528 = ORIENTED_EDGE('',*,*,#39663,.F.) ;
#53529 = ORIENTED_EDGE('',*,*,#39664,.T.) ;
#53530 = ORIENTED_EDGE('',*,*,#39547,.T.) ;
#53531 = ORIENTED_EDGE('',*,*,#39665,.T.) ;
#53532 = ORIENTED_EDGE('',*,*,#39666,.F.) ;
#53533 = ORIENTED_EDGE('',*,*,#39667,.T.) ;
#53534 = ORIENTED_EDGE('',*,*,#39668,.F.) ;
#53535 = ORIENTED_EDGE('',*,*,#39669,.T.) ;
#53536 = ORIENTED_EDGE('',*,*,#39543,.T.) ;
#53537 = ORIENTED_EDGE('',*,*,#39670,.T.) ;
#53538 = ORIENTED_EDGE('',*,*,#39671,.F.) ;
#53539 = ORIENTED_EDGE('',*,*,#39672,.T.) ;
#53540 = ORIENTED_EDGE('',*,*,#39673,.F.) ;
#53541 = ORIENTED_EDGE('',*,*,#39674,.T.) ;
#53542 = ORIENTED_EDGE('',*,*,#39539,.T.) ;
#53543 = ORIENTED_EDGE('',*,*,#39675,.T.) ;
#53544 = ORIENTED_EDGE('',*,*,#39676,.F.) ;
#53545 = ORIENTED_EDGE('',*,*,#39677,.T.) ;
#53546 = ORIENTED_EDGE('',*,*,#39678,.F.) ;
#53547 = ORIENTED_EDGE('',*,*,#39679,.T.) ;
#53548 = ORIENTED_EDGE('',*,*,#39535,.T.) ;
#53549 = ORIENTED_EDGE('',*,*,#39680,.T.) ;
#53550 = ORIENTED_EDGE('',*,*,#39681,.F.) ;
#53551 = ORIENTED_EDGE('',*,*,#39682,.T.) ;
#53552 = ORIENTED_EDGE('',*,*,#39683,.F.) ;
#53553 = ORIENTED_EDGE('',*,*,#39684,.T.) ;
#53554 = ORIENTED_EDGE('',*,*,#39531,.T.) ;
#53555 = ORIENTED_EDGE('',*,*,#39685,.T.) ;
#53556 = ORIENTED_EDGE('',*,*,#39686,.F.) ;
#53557 = ORIENTED_EDGE('',*,*,#39687,.T.) ;
#53558 = ORIENTED_EDGE('',*,*,#39688,.F.) ;
#53559 = ORIENTED_EDGE('',*,*,#39689,.T.) ;
#53560 = ORIENTED_EDGE('',*,*,#39527,.T.) ;
#53561 = ORIENTED_EDGE('',*,*,#39690,.T.) ;
#53562 = ORIENTED_EDGE('',*,*,#39691,.F.) ;
#53563 = ORIENTED_EDGE('',*,*,#39692,.T.) ;
#53564 = ORIENTED_EDGE('',*,*,#39693,.F.) ;
#53565 = ORIENTED_EDGE('',*,*,#39694,.T.) ;
#53566 = ORIENTED_EDGE('',*,*,#39584,.T.) ;
#53567 = ORIENTED_EDGE('',*,*,#39695,.T.) ;
#53568 = ORIENTED_EDGE('',*,*,#39696,.F.) ;
#53569 = ORIENTED_EDGE('',*,*,#39697,.T.) ;
#53570 = ORIENTED_EDGE('',*,*,#39646,.T.) ;
#53571 = ORIENTED_EDGE('',*,*,#39698,.T.) ;
#53572 = ORIENTED_EDGE('',*,*,#39699,.F.) ;
#53573 = ORIENTED_EDGE('',*,*,#39700,.T.) ;
#53574 = ORIENTED_EDGE('',*,*,#39701,.F.) ;
#53575 = ORIENTED_EDGE('',*,*,#39702,.T.) ;
#53576 = ORIENTED_EDGE('',*,*,#39696,.T.) ;
#53577 = ORIENTED_EDGE('',*,*,#39703,.T.) ;
#53578 = ORIENTED_EDGE('',*,*,#39704,.F.) ;
#53579 = ORIENTED_EDGE('',*,*,#39705,.T.) ;
#53580 = ORIENTED_EDGE('',*,*,#39701,.T.) ;
#53581 = ORIENTED_EDGE('',*,*,#39706,.T.) ;
#53582 = ORIENTED_EDGE('',*,*,#39707,.F.) ;
#53583 = ORIENTED_EDGE('',*,*,#39708,.T.) ;
#53584 = ORIENTED_EDGE('',*,*,#39704,.T.) ;
#53585 = ORIENTED_EDGE('',*,*,#39709,.T.) ;
#53586 = ORIENTED_EDGE('',*,*,#39710,.F.) ;
#53587 = ORIENTED_EDGE('',*,*,#39711,.T.) ;
#53588 = ORIENTED_EDGE('',*,*,#39707,.T.) ;
#53589 = ORIENTED_EDGE('',*,*,#39712,.T.) ;
#53590 = ORIENTED_EDGE('',*,*,#39713,.F.) ;
#53591 = ORIENTED_EDGE('',*,*,#39714,.T.) ;
#53592 = ORIENTED_EDGE('',*,*,#39710,.T.) ;
#53593 = ORIENTED_EDGE('',*,*,#39715,.T.) ;
#53594 = ORIENTED_EDGE('',*,*,#39716,.F.) ;
#53595 = ORIENTED_EDGE('',*,*,#39717,.T.) ;
#53596 = ORIENTED_EDGE('',*,*,#39713,.T.) ;
#53597 = ORIENTED_EDGE('',*,*,#39718,.T.) ;
#53598 = ORIENTED_EDGE('',*,*,#39719,.F.) ;
#53599 = ORIENTED_EDGE('',*,*,#39720,.T.) ;
#53600 = ORIENTED_EDGE('',*,*,#39716,.T.) ;
#53601 = ORIENTED_EDGE('',*,*,#39721,.T.) ;
#53602 = ORIENTED_EDGE('',*,*,#39722,.F.) ;
#53603 = ORIENTED_EDGE('',*,*,#39723,.T.) ;
#53604 = ORIENTED_EDGE('',*,*,#39719,.T.) ;
#53605 = ORIENTED_EDGE('',*,*,#39724,.T.) ;
#53606 = ORIENTED_EDGE('',*,*,#39725,.F.) ;
#53607 = ORIENTED_EDGE('',*,*,#39726,.T.) ;
#53608 = ORIENTED_EDGE('',*,*,#39722,.T.) ;
#53609 = ORIENTED_EDGE('',*,*,#39727,.T.) ;
#53610 = ORIENTED_EDGE('',*,*,#39728,.F.) ;
#53611 = ORIENTED_EDGE('',*,*,#39729,.T.) ;
#53612 = ORIENTED_EDGE('',*,*,#39725,.T.) ;
#53613 = ORIENTED_EDGE('',*,*,#39730,.T.) ;
#53614 = ORIENTED_EDGE('',*,*,#39731,.F.) ;
#53615 = ORIENTED_EDGE('',*,*,#39732,.T.) ;
#53616 = ORIENTED_EDGE('',*,*,#39728,.T.) ;
#53617 = ORIENTED_EDGE('',*,*,#39733,.T.) ;
#53618 = ORIENTED_EDGE('',*,*,#39590,.F.) ;
#53619 = ORIENTED_EDGE('',*,*,#39734,.T.) ;
#53620 = ORIENTED_EDGE('',*,*,#39731,.T.) ;
#53621 = ORIENTED_EDGE('',*,*,#39735,.T.) ;
#53622 = ORIENTED_EDGE('',*,*,#39736,.T.) ;
#53623 = ORIENTED_EDGE('',*,*,#39737,.T.) ;
#53624 = ORIENTED_EDGE('',*,*,#39738,.T.) ;
#53625 = ORIENTED_EDGE('',*,*,#39739,.T.) ;
#53626 = ORIENTED_EDGE('',*,*,#39740,.T.) ;
#53627 = ORIENTED_EDGE('',*,*,#39741,.T.) ;
#53628 = ORIENTED_EDGE('',*,*,#39742,.T.) ;
#53629 = ORIENTED_EDGE('',*,*,#39743,.T.) ;
#53630 = ORIENTED_EDGE('',*,*,#39260,.T.) ;
#53631 = ORIENTED_EDGE('',*,*,#39744,.T.) ;
#53632 = ORIENTED_EDGE('',*,*,#39745,.T.) ;
#53633 = ORIENTED_EDGE('',*,*,#39746,.T.) ;
#53634 = ORIENTED_EDGE('',*,*,#39747,.T.) ;
#53635 = ORIENTED_EDGE('',*,*,#39748,.T.) ;
#53636 = ORIENTED_EDGE('',*,*,#39749,.T.) ;
#53637 = ORIENTED_EDGE('',*,*,#39750,.T.) ;
#53638 = ORIENTED_EDGE('',*,*,#39751,.T.) ;
#53639 = ORIENTED_EDGE('',*,*,#39752,.T.) ;
#53640 = ORIENTED_EDGE('',*,*,#39753,.T.) ;
#53641 = ORIENTED_EDGE('',*,*,#39754,.T.) ;
#53642 = ORIENTED_EDGE('',*,*,#39755,.T.) ;
#53643 = ORIENTED_EDGE('',*,*,#39756,.T.) ;
#53644 = ORIENTED_EDGE('',*,*,#39757,.T.) ;
#53645 = ORIENTED_EDGE('',*,*,#39758,.T.) ;
#53646 = ORIENTED_EDGE('',*,*,#39759,.T.) ;
#53647 = ORIENTED_EDGE('',*,*,#39760,.T.) ;
#53648 = ORIENTED_EDGE('',*,*,#39761,.T.) ;
#53649 = ORIENTED_EDGE('',*,*,#39762,.T.) ;
#53650 = ORIENTED_EDGE('',*,*,#39763,.T.) ;
#53651 = ORIENTED_EDGE('',*,*,#39764,.T.) ;
#53652 = ORIENTED_EDGE('',*,*,#39765,.T.) ;
#53653 = ORIENTED_EDGE('',*,*,#39766,.T.) ;
#53654 = ORIENTED_EDGE('',*,*,#39256,.T.) ;
#53655 = ORIENTED_EDGE('',*,*,#39767,.T.) ;
#53656 = ORIENTED_EDGE('',*,*,#39768,.T.) ;
#53657 = ORIENTED_EDGE('',*,*,#39769,.T.) ;
#53658 = ORIENTED_EDGE('',*,*,#39770,.T.) ;
#53659 = ORIENTED_EDGE('',*,*,#39771,.T.) ;
#53660 = ORIENTED_EDGE('',*,*,#39772,.T.) ;
#53661 = ORIENTED_EDGE('',*,*,#39773,.T.) ;
#53662 = ORIENTED_EDGE('',*,*,#39774,.T.) ;
#53663 = ORIENTED_EDGE('',*,*,#39775,.T.) ;
#53664 = ORIENTED_EDGE('',*,*,#39776,.T.) ;
#53665 = ORIENTED_EDGE('',*,*,#39777,.T.) ;
#53666 = ORIENTED_EDGE('',*,*,#39778,.T.) ;
#53667 = ORIENTED_EDGE('',*,*,#39779,.T.) ;
#53668 = ORIENTED_EDGE('',*,*,#39780,.T.) ;
#53669 = ORIENTED_EDGE('',*,*,#39781,.T.) ;
#53670 = ORIENTED_EDGE('',*,*,#39782,.T.) ;
#53671 = ORIENTED_EDGE('',*,*,#39783,.T.) ;
#53672 = ORIENTED_EDGE('',*,*,#39784,.T.) ;
#53673 = ORIENTED_EDGE('',*,*,#39785,.T.) ;
#53674 = ORIENTED_EDGE('',*,*,#39786,.T.) ;
#53675 = ORIENTED_EDGE('',*,*,#39787,.T.) ;
#53676 = ORIENTED_EDGE('',*,*,#39788,.T.) ;
#53677 = ORIENTED_EDGE('',*,*,#39789,.T.) ;
#53678 = ORIENTED_EDGE('',*,*,#39252,.T.) ;
#53679 = ORIENTED_EDGE('',*,*,#39790,.T.) ;
#53680 = ORIENTED_EDGE('',*,*,#39791,.T.) ;
#53681 = ORIENTED_EDGE('',*,*,#39792,.T.) ;
#53682 = ORIENTED_EDGE('',*,*,#39793,.T.) ;
#53683 = ORIENTED_EDGE('',*,*,#39794,.T.) ;
#53684 = ORIENTED_EDGE('',*,*,#39795,.T.) ;
#53685 = ORIENTED_EDGE('',*,*,#39796,.T.) ;
#53686 = ORIENTED_EDGE('',*,*,#39797,.T.) ;
#53687 = ORIENTED_EDGE('',*,*,#39798,.T.) ;
#53688 = ORIENTED_EDGE('',*,*,#39799,.T.) ;
#53689 = ORIENTED_EDGE('',*,*,#39800,.T.) ;
#53690 = ORIENTED_EDGE('',*,*,#39801,.T.) ;
#53691 = ORIENTED_EDGE('',*,*,#39802,.T.) ;
#53692 = ORIENTED_EDGE('',*,*,#39803,.T.) ;
#53693 = ORIENTED_EDGE('',*,*,#39804,.T.) ;
#53694 = ORIENTED_EDGE('',*,*,#39805,.T.) ;
#53695 = ORIENTED_EDGE('',*,*,#39806,.T.) ;
#53696 = ORIENTED_EDGE('',*,*,#39807,.T.) ;
#53697 = ORIENTED_EDGE('',*,*,#39808,.T.) ;
#53698 = ORIENTED_EDGE('',*,*,#39809,.T.) ;
#53699 = ORIENTED_EDGE('',*,*,#39810,.T.) ;
#53700 = ORIENTED_EDGE('',*,*,#39811,.T.) ;
#53701 = ORIENTED_EDGE('',*,*,#39812,.T.) ;
#53702 = ORIENTED_EDGE('',*,*,#39248,.T.) ;
#53703 = ORIENTED_EDGE('',*,*,#39813,.T.) ;
#53704 = ORIENTED_EDGE('',*,*,#39814,.T.) ;
#53705 = ORIENTED_EDGE('',*,*,#39815,.T.) ;
#53706 = ORIENTED_EDGE('',*,*,#39816,.T.) ;
#53707 = ORIENTED_EDGE('',*,*,#39817,.T.) ;
#53708 = ORIENTED_EDGE('',*,*,#39818,.T.) ;
#53709 = ORIENTED_EDGE('',*,*,#39819,.T.) ;
#53710 = ORIENTED_EDGE('',*,*,#39820,.T.) ;
#53711 = ORIENTED_EDGE('',*,*,#39821,.T.) ;
#53712 = ORIENTED_EDGE('',*,*,#39822,.T.) ;
#53713 = ORIENTED_EDGE('',*,*,#39823,.T.) ;
#53714 = ORIENTED_EDGE('',*,*,#39824,.T.) ;
#53715 = ORIENTED_EDGE('',*,*,#39825,.T.) ;
#53716 = ORIENTED_EDGE('',*,*,#39826,.T.) ;
#53717 = ORIENTED_EDGE('',*,*,#39827,.T.) ;
#53718 = ORIENTED_EDGE('',*,*,#39828,.T.) ;
#53719 = ORIENTED_EDGE('',*,*,#39829,.T.) ;
#53720 = ORIENTED_EDGE('',*,*,#39830,.T.) ;
#53721 = ORIENTED_EDGE('',*,*,#39831,.T.) ;
#53722 = ORIENTED_EDGE('',*,*,#39832,.T.) ;
#53723 = ORIENTED_EDGE('',*,*,#39833,.T.) ;
#53724 = ORIENTED_EDGE('',*,*,#39834,.T.) ;
#53725 = ORIENTED_EDGE('',*,*,#39835,.T.) ;
#53726 = ORIENTED_EDGE('',*,*,#39244,.T.) ;
#53727 = ORIENTED_EDGE('',*,*,#39836,.T.) ;
#53728 = ORIENTED_EDGE('',*,*,#39837,.T.) ;
#53729 = ORIENTED_EDGE('',*,*,#39838,.T.) ;
#53730 = ORIENTED_EDGE('',*,*,#39839,.T.) ;
#53731 = ORIENTED_EDGE('',*,*,#39840,.T.) ;
#53732 = ORIENTED_EDGE('',*,*,#39841,.T.) ;
#53733 = ORIENTED_EDGE('',*,*,#39842,.T.) ;
#53734 = ORIENTED_EDGE('',*,*,#39843,.T.) ;
#53735 = ORIENTED_EDGE('',*,*,#39844,.T.) ;
#53736 = ORIENTED_EDGE('',*,*,#39845,.T.) ;
#53737 = ORIENTED_EDGE('',*,*,#39846,.T.) ;
#53738 = ORIENTED_EDGE('',*,*,#39847,.T.) ;
#53739 = ORIENTED_EDGE('',*,*,#39848,.T.) ;
#53740 = ORIENTED_EDGE('',*,*,#39849,.T.) ;
#53741 = ORIENTED_EDGE('',*,*,#39850,.T.) ;
#53742 = ORIENTED_EDGE('',*,*,#39851,.T.) ;
#53743 = ORIENTED_EDGE('',*,*,#39852,.T.) ;
#53744 = ORIENTED_EDGE('',*,*,#39853,.T.) ;
#53745 = ORIENTED_EDGE('',*,*,#39854,.T.) ;
#53746 = ORIENTED_EDGE('',*,*,#39855,.T.) ;
#53747 = ORIENTED_EDGE('',*,*,#39856,.T.) ;
#53748 = ORIENTED_EDGE('',*,*,#39857,.T.) ;
#53749 = ORIENTED_EDGE('',*,*,#39858,.T.) ;
#53750 = ORIENTED_EDGE('',*,*,#39240,.T.) ;
#53751 = ORIENTED_EDGE('',*,*,#39859,.T.) ;
#53752 = ORIENTED_EDGE('',*,*,#39860,.T.) ;
#53753 = ORIENTED_EDGE('',*,*,#39861,.T.) ;
#53754 = ORIENTED_EDGE('',*,*,#39862,.T.) ;
#53755 = ORIENTED_EDGE('',*,*,#39863,.T.) ;
#53756 = ORIENTED_EDGE('',*,*,#39864,.T.) ;
#53757 = ORIENTED_EDGE('',*,*,#39865,.T.) ;
#53758 = ORIENTED_EDGE('',*,*,#39866,.T.) ;
#53759 = ORIENTED_EDGE('',*,*,#39867,.T.) ;
#53760 = ORIENTED_EDGE('',*,*,#39868,.T.) ;
#53761 = ORIENTED_EDGE('',*,*,#39869,.T.) ;
#53762 = ORIENTED_EDGE('',*,*,#39870,.T.) ;
#53763 = ORIENTED_EDGE('',*,*,#39871,.T.) ;
#53764 = ORIENTED_EDGE('',*,*,#39872,.T.) ;
#53765 = ORIENTED_EDGE('',*,*,#39873,.T.) ;
#53766 = ORIENTED_EDGE('',*,*,#39874,.T.) ;
#53767 = ORIENTED_EDGE('',*,*,#39875,.T.) ;
#53768 = ORIENTED_EDGE('',*,*,#39876,.T.) ;
#53769 = ORIENTED_EDGE('',*,*,#39877,.T.) ;
#53770 = ORIENTED_EDGE('',*,*,#39878,.T.) ;
#53771 = ORIENTED_EDGE('',*,*,#39879,.T.) ;
#53772 = ORIENTED_EDGE('',*,*,#39880,.T.) ;
#53773 = ORIENTED_EDGE('',*,*,#39881,.T.) ;
#53774 = ORIENTED_EDGE('',*,*,#39236,.T.) ;
#53775 = ORIENTED_EDGE('',*,*,#39882,.T.) ;
#53776 = ORIENTED_EDGE('',*,*,#39883,.T.) ;
#53777 = ORIENTED_EDGE('',*,*,#39884,.T.) ;
#53778 = ORIENTED_EDGE('',*,*,#39885,.T.) ;
#53779 = ORIENTED_EDGE('',*,*,#39886,.T.) ;
#53780 = ORIENTED_EDGE('',*,*,#39887,.T.) ;
#53781 = ORIENTED_EDGE('',*,*,#39888,.T.) ;
#53782 = ORIENTED_EDGE('',*,*,#39889,.T.) ;
#53783 = ORIENTED_EDGE('',*,*,#39890,.T.) ;
#53784 = ORIENTED_EDGE('',*,*,#39891,.T.) ;
#53785 = ORIENTED_EDGE('',*,*,#39892,.T.) ;
#53786 = ORIENTED_EDGE('',*,*,#39893,.T.) ;
#53787 = ORIENTED_EDGE('',*,*,#39894,.T.) ;
#53788 = ORIENTED_EDGE('',*,*,#39895,.T.) ;
#53789 = ORIENTED_EDGE('',*,*,#39896,.T.) ;
#53790 = ORIENTED_EDGE('',*,*,#39897,.T.) ;
#53791 = ORIENTED_EDGE('',*,*,#39898,.T.) ;
#53792 = ORIENTED_EDGE('',*,*,#39899,.T.) ;
#53793 = ORIENTED_EDGE('',*,*,#39900,.T.) ;
#53794 = ORIENTED_EDGE('',*,*,#39901,.T.) ;
#53795 = ORIENTED_EDGE('',*,*,#39902,.T.) ;
#53796 = ORIENTED_EDGE('',*,*,#39903,.T.) ;
#53797 = ORIENTED_EDGE('',*,*,#39904,.T.) ;
#53798 = ORIENTED_EDGE('',*,*,#39232,.T.) ;
#53799 = ORIENTED_EDGE('',*,*,#39905,.T.) ;
#53800 = ORIENTED_EDGE('',*,*,#39906,.T.) ;
#53801 = ORIENTED_EDGE('',*,*,#39907,.T.) ;
#53802 = ORIENTED_EDGE('',*,*,#39908,.T.) ;
#53803 = ORIENTED_EDGE('',*,*,#39909,.T.) ;
#53804 = ORIENTED_EDGE('',*,*,#39910,.T.) ;
#53805 = ORIENTED_EDGE('',*,*,#39911,.T.) ;
#53806 = ORIENTED_EDGE('',*,*,#39912,.T.) ;
#53807 = ORIENTED_EDGE('',*,*,#39913,.T.) ;
#53808 = ORIENTED_EDGE('',*,*,#39914,.T.) ;
#53809 = ORIENTED_EDGE('',*,*,#39915,.T.) ;
#53810 = ORIENTED_EDGE('',*,*,#39916,.T.) ;
#53811 = ORIENTED_EDGE('',*,*,#39917,.T.) ;
#53812 = ORIENTED_EDGE('',*,*,#39918,.T.) ;
#53813 = ORIENTED_EDGE('',*,*,#39919,.T.) ;
#53814 = ORIENTED_EDGE('',*,*,#39920,.T.) ;
#53815 = ORIENTED_EDGE('',*,*,#39921,.T.) ;
#53816 = ORIENTED_EDGE('',*,*,#39922,.T.) ;
#53817 = ORIENTED_EDGE('',*,*,#39923,.T.) ;
#53818 = ORIENTED_EDGE('',*,*,#39924,.T.) ;
#53819 = ORIENTED_EDGE('',*,*,#39925,.T.) ;
#53820 = ORIENTED_EDGE('',*,*,#39926,.T.) ;
#53821 = ORIENTED_EDGE('',*,*,#39927,.T.) ;
#53822 = ORIENTED_EDGE('',*,*,#39228,.T.) ;
#53823 = ORIENTED_EDGE('',*,*,#39928,.T.) ;
#53824 = ORIENTED_EDGE('',*,*,#39929,.T.) ;
#53825 = ORIENTED_EDGE('',*,*,#39930,.T.) ;
#53826 = ORIENTED_EDGE('',*,*,#39931,.T.) ;
#53827 = ORIENTED_EDGE('',*,*,#39932,.T.) ;
#53828 = ORIENTED_EDGE('',*,*,#39933,.T.) ;
#53829 = ORIENTED_EDGE('',*,*,#39934,.T.) ;
#53830 = ORIENTED_EDGE('',*,*,#39935,.T.) ;
#53831 = ORIENTED_EDGE('',*,*,#39936,.T.) ;
#53832 = ORIENTED_EDGE('',*,*,#39937,.T.) ;
#53833 = ORIENTED_EDGE('',*,*,#39938,.T.) ;
#53834 = ORIENTED_EDGE('',*,*,#39939,.T.) ;
#53835 = ORIENTED_EDGE('',*,*,#39940,.T.) ;
#53836 = ORIENTED_EDGE('',*,*,#39941,.T.) ;
#53837 = ORIENTED_EDGE('',*,*,#39942,.T.) ;
#53838 = ORIENTED_EDGE('',*,*,#39943,.T.) ;
#53839 = ORIENTED_EDGE('',*,*,#39944,.T.) ;
#53840 = ORIENTED_EDGE('',*,*,#39945,.T.) ;
#53841 = ORIENTED_EDGE('',*,*,#39946,.T.) ;
#53842 = ORIENTED_EDGE('',*,*,#39947,.T.) ;
#53843 = ORIENTED_EDGE('',*,*,#39948,.T.) ;
#53844 = ORIENTED_EDGE('',*,*,#39949,.T.) ;
#53845 = ORIENTED_EDGE('',*,*,#39950,.T.) ;
#53846 = ORIENTED_EDGE('',*,*,#39317,.T.) ;
#53847 = ORIENTED_EDGE('',*,*,#39951,.T.) ;
#53848 = ORIENTED_EDGE('',*,*,#39952,.T.) ;
#53849 = ORIENTED_EDGE('',*,*,#39953,.T.) ;
#53850 = ORIENTED_EDGE('',*,*,#39954,.T.) ;
#53851 = ORIENTED_EDGE('',*,*,#39955,.T.) ;
#53852 = ORIENTED_EDGE('',*,*,#39956,.T.) ;
#53853 = ORIENTED_EDGE('',*,*,#39957,.T.) ;
#53854 = ORIENTED_EDGE('',*,*,#39958,.T.) ;
#53855 = ORIENTED_EDGE('',*,*,#39959,.T.) ;
#53856 = ORIENTED_EDGE('',*,*,#39960,.T.) ;
#53857 = ORIENTED_EDGE('',*,*,#39961,.T.) ;
#53858 = ORIENTED_EDGE('',*,*,#39962,.T.) ;
#53859 = ORIENTED_EDGE('',*,*,#39963,.T.) ;
#53860 = ORIENTED_EDGE('',*,*,#39964,.T.) ;
#53861 = ORIENTED_EDGE('',*,*,#39965,.T.) ;
#53862 = ORIENTED_EDGE('',*,*,#39966,.T.) ;
#53863 = ORIENTED_EDGE('',*,*,#39967,.T.) ;
#53864 = ORIENTED_EDGE('',*,*,#39968,.T.) ;
#53865 = ORIENTED_EDGE('',*,*,#39969,.T.) ;
#53866 = ORIENTED_EDGE('',*,*,#39970,.T.) ;
#53867 = ORIENTED_EDGE('',*,*,#39971,.T.) ;
#53868 = ORIENTED_EDGE('',*,*,#39972,.T.) ;
#53869 = ORIENTED_EDGE('',*,*,#39973,.T.) ;
#53870 = ORIENTED_EDGE('',*,*,#39974,.T.) ;
#53871 = ORIENTED_EDGE('',*,*,#39975,.T.) ;
#53872 = ORIENTED_EDGE('',*,*,#39976,.T.) ;
#53873 = ORIENTED_EDGE('',*,*,#39977,.T.) ;
#53874 = ORIENTED_EDGE('',*,*,#39978,.T.) ;
#53875 = ORIENTED_EDGE('',*,*,#39979,.T.) ;
#53876 = ORIENTED_EDGE('',*,*,#39980,.T.) ;
#53877 = ORIENTED_EDGE('',*,*,#39981,.T.) ;
#53878 = ORIENTED_EDGE('',*,*,#39982,.T.) ;
#53879 = ORIENTED_EDGE('',*,*,#39983,.T.) ;
#53880 = ORIENTED_EDGE('',*,*,#39984,.T.) ;
#53881 = ORIENTED_EDGE('',*,*,#39985,.T.) ;
#53882 = ORIENTED_EDGE('',*,*,#39986,.T.) ;
#53883 = ORIENTED_EDGE('',*,*,#39987,.T.) ;
#53884 = ORIENTED_EDGE('',*,*,#39988,.T.) ;
#53885 = ORIENTED_EDGE('',*,*,#39989,.T.) ;
#53886 = ORIENTED_EDGE('',*,*,#39990,.T.) ;
#53887 = ORIENTED_EDGE('',*,*,#39991,.T.) ;
#53888 = ORIENTED_EDGE('',*,*,#39992,.F.) ;
#53889 = ORIENTED_EDGE('',*,*,#39993,.T.) ;
#53890 = ORIENTED_EDGE('',*,*,#39994,.F.) ;
#53891 = ORIENTED_EDGE('',*,*,#39995,.T.) ;
#53892 = ORIENTED_EDGE('',*,*,#39996,.T.) ;
#53893 = ORIENTED_EDGE('',*,*,#39997,.T.) ;
#53894 = ORIENTED_EDGE('',*,*,#39998,.T.) ;
#53895 = ORIENTED_EDGE('',*,*,#39999,.T.) ;
#53896 = ORIENTED_EDGE('',*,*,#40000,.T.) ;
#53897 = ORIENTED_EDGE('',*,*,#40001,.T.) ;
#53898 = ORIENTED_EDGE('',*,*,#40002,.T.) ;
#53899 = ORIENTED_EDGE('',*,*,#39329,.T.) ;
#53900 = ORIENTED_EDGE('',*,*,#40003,.T.) ;
#53901 = ORIENTED_EDGE('',*,*,#40004,.T.) ;
#53902 = ORIENTED_EDGE('',*,*,#40005,.T.) ;
#53903 = ORIENTED_EDGE('',*,*,#40006,.T.) ;
#53904 = ORIENTED_EDGE('',*,*,#40007,.T.) ;
#53905 = ORIENTED_EDGE('',*,*,#40008,.T.) ;
#53906 = ORIENTED_EDGE('',*,*,#40009,.T.) ;
#53907 = ORIENTED_EDGE('',*,*,#40010,.T.) ;
#53908 = ORIENTED_EDGE('',*,*,#40011,.T.) ;
#53909 = ORIENTED_EDGE('',*,*,#40012,.T.) ;
#53910 = ORIENTED_EDGE('',*,*,#40013,.T.) ;
#53911 = ORIENTED_EDGE('',*,*,#40014,.T.) ;
#53912 = ORIENTED_EDGE('',*,*,#40015,.F.) ;
#53913 = ORIENTED_EDGE('',*,*,#40016,.T.) ;
#53914 = ORIENTED_EDGE('',*,*,#40017,.T.) ;
#53915 = ORIENTED_EDGE('',*,*,#40018,.T.) ;
#53916 = ORIENTED_EDGE('',*,*,#40017,.F.) ;
#53917 = ORIENTED_EDGE('',*,*,#40019,.T.) ;
#53918 = ORIENTED_EDGE('',*,*,#40020,.T.) ;
#53919 = ORIENTED_EDGE('',*,*,#40021,.T.) ;
#53920 = ORIENTED_EDGE('',*,*,#40020,.F.) ;
#53921 = ORIENTED_EDGE('',*,*,#40022,.T.) ;
#53922 = ORIENTED_EDGE('',*,*,#40023,.T.) ;
#53923 = ORIENTED_EDGE('',*,*,#40024,.T.) ;
#53924 = ORIENTED_EDGE('',*,*,#40023,.F.) ;
#53925 = ORIENTED_EDGE('',*,*,#40025,.T.) ;
#53926 = ORIENTED_EDGE('',*,*,#40026,.T.) ;
#53927 = ORIENTED_EDGE('',*,*,#40027,.T.) ;
#53928 = ORIENTED_EDGE('',*,*,#40026,.F.) ;
#53929 = ORIENTED_EDGE('',*,*,#40028,.T.) ;
#53930 = ORIENTED_EDGE('',*,*,#40029,.T.) ;
#53931 = ORIENTED_EDGE('',*,*,#40030,.T.) ;
#53932 = ORIENTED_EDGE('',*,*,#40029,.F.) ;
#53933 = ORIENTED_EDGE('',*,*,#40031,.T.) ;
#53934 = ORIENTED_EDGE('',*,*,#40032,.T.) ;
#53935 = ORIENTED_EDGE('',*,*,#40033,.T.) ;
#53936 = ORIENTED_EDGE('',*,*,#40032,.F.) ;
#53937 = ORIENTED_EDGE('',*,*,#39324,.T.) ;
#53938 = ORIENTED_EDGE('',*,*,#40034,.T.) ;
#53939 = ORIENTED_EDGE('',*,*,#40035,.T.) ;
#53940 = ORIENTED_EDGE('',*,*,#40034,.F.) ;
#53941 = ORIENTED_EDGE('',*,*,#40036,.T.) ;
#53942 = ORIENTED_EDGE('',*,*,#39337,.T.) ;
#53943 = ORIENTED_EDGE('',*,*,#40037,.T.) ;
#53944 = ORIENTED_EDGE('',*,*,#39336,.F.) ;
#53945 = ORIENTED_EDGE('',*,*,#40038,.T.) ;
#53946 = ORIENTED_EDGE('',*,*,#40039,.T.) ;
#53947 = ORIENTED_EDGE('',*,*,#40040,.T.) ;
#53948 = ORIENTED_EDGE('',*,*,#40039,.F.) ;
#53949 = ORIENTED_EDGE('',*,*,#40041,.T.) ;
#53950 = ORIENTED_EDGE('',*,*,#40042,.T.) ;
#53951 = ORIENTED_EDGE('',*,*,#40043,.T.) ;
#53952 = ORIENTED_EDGE('',*,*,#40042,.F.) ;
#53953 = ORIENTED_EDGE('',*,*,#40044,.T.) ;
#53954 = ORIENTED_EDGE('',*,*,#40045,.T.) ;
#53955 = ORIENTED_EDGE('',*,*,#40046,.T.) ;
#53956 = ORIENTED_EDGE('',*,*,#40045,.F.) ;
#53957 = ORIENTED_EDGE('',*,*,#40047,.T.) ;
#53958 = ORIENTED_EDGE('',*,*,#40048,.T.) ;
#53959 = ORIENTED_EDGE('',*,*,#40049,.T.) ;
#53960 = ORIENTED_EDGE('',*,*,#40048,.F.) ;
#53961 = ORIENTED_EDGE('',*,*,#40050,.T.) ;
#53962 = ORIENTED_EDGE('',*,*,#40051,.T.) ;
#53963 = ORIENTED_EDGE('',*,*,#40052,.T.) ;
#53964 = ORIENTED_EDGE('',*,*,#40051,.F.) ;
#53965 = ORIENTED_EDGE('',*,*,#40053,.T.) ;
#53966 = ORIENTED_EDGE('',*,*,#40054,.T.) ;
#53967 = ORIENTED_EDGE('',*,*,#40055,.T.) ;
#53968 = ORIENTED_EDGE('',*,*,#40054,.F.) ;
#53969 = ORIENTED_EDGE('',*,*,#40056,.T.) ;
#53970 = ORIENTED_EDGE('',*,*,#40057,.T.) ;
#53971 = ORIENTED_EDGE('',*,*,#40058,.T.) ;
#53972 = ORIENTED_EDGE('',*,*,#40057,.F.) ;
#53973 = ORIENTED_EDGE('',*,*,#40059,.T.) ;
#53974 = ORIENTED_EDGE('',*,*,#40060,.T.) ;
#53975 = ORIENTED_EDGE('',*,*,#40061,.T.) ;
#53976 = ORIENTED_EDGE('',*,*,#40060,.F.) ;
#53977 = ORIENTED_EDGE('',*,*,#40062,.T.) ;
#53978 = ORIENTED_EDGE('',*,*,#40063,.T.) ;
#53979 = ORIENTED_EDGE('',*,*,#40064,.T.) ;
#53980 = ORIENTED_EDGE('',*,*,#40063,.F.) ;
#53981 = ORIENTED_EDGE('',*,*,#40065,.T.) ;
#53982 = ORIENTED_EDGE('',*,*,#40066,.T.) ;
#53983 = ORIENTED_EDGE('',*,*,#40067,.T.) ;
#53984 = ORIENTED_EDGE('',*,*,#40066,.F.) ;
#53985 = ORIENTED_EDGE('',*,*,#40068,.T.) ;
#53986 = ORIENTED_EDGE('',*,*,#40069,.T.) ;
#53987 = ORIENTED_EDGE('',*,*,#40070,.T.) ;
#53988 = ORIENTED_EDGE('',*,*,#40069,.F.) ;
#53989 = ORIENTED_EDGE('',*,*,#40071,.T.) ;
#53990 = ORIENTED_EDGE('',*,*,#40072,.T.) ;
#53991 = ORIENTED_EDGE('',*,*,#40073,.T.) ;
#53992 = ORIENTED_EDGE('',*,*,#40072,.F.) ;
#53993 = ORIENTED_EDGE('',*,*,#40074,.T.) ;
#53994 = ORIENTED_EDGE('',*,*,#40075,.T.) ;
#53995 = ORIENTED_EDGE('',*,*,#40076,.T.) ;
#53996 = ORIENTED_EDGE('',*,*,#40075,.F.) ;
#53997 = ORIENTED_EDGE('',*,*,#40077,.T.) ;
#53998 = ORIENTED_EDGE('',*,*,#40078,.T.) ;
#53999 = ORIENTED_EDGE('',*,*,#40079,.T.) ;
#54000 = ORIENTED_EDGE('',*,*,#40078,.F.) ;
#54001 = ORIENTED_EDGE('',*,*,#40080,.T.) ;
#54002 = ORIENTED_EDGE('',*,*,#40081,.T.) ;
#54003 = ORIENTED_EDGE('',*,*,#40082,.T.) ;
#54004 = ORIENTED_EDGE('',*,*,#40081,.F.) ;
#54005 = ORIENTED_EDGE('',*,*,#40083,.T.) ;
#54006 = ORIENTED_EDGE('',*,*,#40084,.T.) ;
#54007 = ORIENTED_EDGE('',*,*,#40085,.T.) ;
#54008 = ORIENTED_EDGE('',*,*,#40084,.F.) ;
#54009 = ORIENTED_EDGE('',*,*,#40086,.T.) ;
#54010 = ORIENTED_EDGE('',*,*,#40087,.T.) ;
#54011 = ORIENTED_EDGE('',*,*,#40088,.T.) ;
#54012 = ORIENTED_EDGE('',*,*,#40087,.F.) ;
#54013 = ORIENTED_EDGE('',*,*,#40089,.T.) ;
#54014 = ORIENTED_EDGE('',*,*,#40090,.T.) ;
#54015 = ORIENTED_EDGE('',*,*,#40091,.T.) ;
#54016 = ORIENTED_EDGE('',*,*,#40090,.F.) ;
#54017 = ORIENTED_EDGE('',*,*,#40092,.T.) ;
#54018 = ORIENTED_EDGE('',*,*,#40015,.T.) ;
#54019 = ORIENTED_EDGE('',*,*,#40093,.T.) ;
#54020 = ORIENTED_EDGE('',*,*,#40094,.T.) ;
#54021 = ORIENTED_EDGE('',*,*,#40095,.T.) ;
#54022 = ORIENTED_EDGE('',*,*,#40096,.T.) ;
#54023 = ORIENTED_EDGE('',*,*,#40097,.T.) ;
#54024 = ORIENTED_EDGE('',*,*,#40098,.T.) ;
#54025 = ORIENTED_EDGE('',*,*,#40099,.T.) ;
#54026 = ORIENTED_EDGE('',*,*,#40100,.T.) ;
#54027 = ORIENTED_EDGE('',*,*,#40101,.T.) ;
#54028 = ORIENTED_EDGE('',*,*,#40102,.T.) ;
#54029 = ORIENTED_EDGE('',*,*,#40103,.T.) ;
#54030 = ORIENTED_EDGE('',*,*,#40104,.T.) ;
#54031 = ORIENTED_EDGE('',*,*,#40105,.T.) ;
#54032 = ORIENTED_EDGE('',*,*,#40106,.T.) ;
#54033 = ORIENTED_EDGE('',*,*,#40107,.T.) ;
#54034 = ORIENTED_EDGE('',*,*,#40108,.T.) ;
#54035 = ORIENTED_EDGE('',*,*,#40109,.T.) ;
#54036 = ORIENTED_EDGE('',*,*,#40110,.T.) ;
#54037 = ORIENTED_EDGE('',*,*,#40111,.T.) ;
#54038 = ORIENTED_EDGE('',*,*,#39321,.T.) ;
#54039 = ORIENTED_EDGE('',*,*,#39313,.T.) ;
#54040 = ORIENTED_EDGE('',*,*,#40112,.F.) ;
#54041 = ORIENTED_EDGE('',*,*,#40113,.T.) ;
#54042 = ORIENTED_EDGE('',*,*,#40114,.T.) ;
#54043 = ORIENTED_EDGE('',*,*,#40115,.T.) ;
#54044 = ORIENTED_EDGE('',*,*,#40116,.T.) ;
#54045 = ORIENTED_EDGE('',*,*,#40117,.T.) ;
#54046 = ORIENTED_EDGE('',*,*,#40118,.T.) ;
#54047 = ORIENTED_EDGE('',*,*,#40119,.T.) ;
#54048 = ORIENTED_EDGE('',*,*,#40120,.F.) ;
#54049 = ORIENTED_EDGE('',*,*,#40008,.F.) ;
#54050 = ORIENTED_EDGE('',*,*,#40121,.F.) ;
#54051 = ORIENTED_EDGE('',*,*,#39995,.F.) ;
#54052 = ORIENTED_EDGE('',*,*,#40122,.F.) ;
#54053 = ORIENTED_EDGE('',*,*,#40009,.F.) ;
#54054 = ORIENTED_EDGE('',*,*,#40123,.F.) ;
#54055 = ORIENTED_EDGE('',*,*,#40003,.F.) ;
#54056 = ORIENTED_EDGE('',*,*,#40124,.F.) ;
#54057 = ORIENTED_EDGE('',*,*,#40122,.T.) ;
#54058 = ORIENTED_EDGE('',*,*,#40125,.F.) ;
#54059 = ORIENTED_EDGE('',*,*,#40126,.F.) ;
#54060 = ORIENTED_EDGE('',*,*,#40121,.T.) ;
#54061 = ORIENTED_EDGE('',*,*,#40127,.F.) ;
#54062 = ORIENTED_EDGE('',*,*,#40120,.T.) ;
#54063 = ORIENTED_EDGE('',*,*,#39994,.T.) ;
#54064 = ORIENTED_EDGE('',*,*,#40128,.F.) ;
#54065 = ORIENTED_EDGE('',*,*,#40123,.T.) ;
#54066 = ORIENTED_EDGE('',*,*,#40125,.T.) ;
#54067 = ORIENTED_EDGE('',*,*,#40006,.F.) ;
#54068 = ORIENTED_EDGE('',*,*,#40129,.F.) ;
#54069 = ORIENTED_EDGE('',*,*,#39327,.T.) ;
#54070 = ORIENTED_EDGE('',*,*,#40130,.T.) ;
#54071 = ORIENTED_EDGE('',*,*,#40131,.F.) ;
#54072 = ORIENTED_EDGE('',*,*,#40124,.T.) ;
#54073 = ORIENTED_EDGE('',*,*,#40132,.F.) ;
#54074 = ORIENTED_EDGE('',*,*,#40133,.T.) ;
#54075 = ORIENTED_EDGE('',*,*,#40134,.F.) ;
#54076 = ORIENTED_EDGE('',*,*,#39563,.F.) ;
#54077 = ORIENTED_EDGE('',*,*,#40135,.F.) ;
#54078 = ORIENTED_EDGE('',*,*,#40010,.F.) ;
#54079 = ORIENTED_EDGE('',*,*,#40127,.T.) ;
#54080 = ORIENTED_EDGE('',*,*,#40007,.F.) ;
#54081 = ORIENTED_EDGE('',*,*,#40136,.F.) ;
#54082 = ORIENTED_EDGE('',*,*,#40013,.F.) ;
#54083 = ORIENTED_EDGE('',*,*,#40126,.T.) ;
#54084 = ORIENTED_EDGE('',*,*,#40012,.F.) ;
#54085 = ORIENTED_EDGE('',*,*,#40137,.F.) ;
#54086 = ORIENTED_EDGE('',*,*,#39986,.F.) ;
#54087 = ORIENTED_EDGE('',*,*,#40128,.T.) ;
#54088 = ORIENTED_EDGE('',*,*,#39993,.F.) ;
#54089 = ORIENTED_EDGE('',*,*,#40138,.F.) ;
#54090 = ORIENTED_EDGE('',*,*,#40004,.F.) ;
#54091 = ORIENTED_EDGE('',*,*,#40139,.F.) ;
#54092 = ORIENTED_EDGE('',*,*,#40005,.F.) ;
#54093 = ORIENTED_EDGE('',*,*,#40140,.F.) ;
#54094 = ORIENTED_EDGE('',*,*,#40000,.F.) ;
#54095 = ORIENTED_EDGE('',*,*,#40129,.T.) ;
#54096 = ORIENTED_EDGE('',*,*,#40139,.T.) ;
#54097 = ORIENTED_EDGE('',*,*,#39328,.F.) ;
#54098 = ORIENTED_EDGE('',*,*,#40135,.T.) ;
#54099 = ORIENTED_EDGE('',*,*,#39573,.T.) ;
#54100 = ORIENTED_EDGE('',*,*,#40141,.F.) ;
#54101 = ORIENTED_EDGE('',*,*,#40136,.T.) ;
#54102 = ORIENTED_EDGE('',*,*,#40142,.F.) ;
#54103 = ORIENTED_EDGE('',*,*,#40137,.T.) ;
#54104 = ORIENTED_EDGE('',*,*,#40143,.F.) ;
#54105 = ORIENTED_EDGE('',*,*,#39579,.T.) ;
#54106 = ORIENTED_EDGE('',*,*,#40138,.T.) ;
#54107 = ORIENTED_EDGE('',*,*,#39992,.T.) ;
#54108 = ORIENTED_EDGE('',*,*,#40144,.F.) ;
#54109 = ORIENTED_EDGE('',*,*,#40140,.T.) ;
#54110 = ORIENTED_EDGE('',*,*,#40141,.T.) ;
#54111 = ORIENTED_EDGE('',*,*,#39572,.F.) ;
#54112 = ORIENTED_EDGE('',*,*,#40145,.F.) ;
#54113 = ORIENTED_EDGE('',*,*,#40014,.F.) ;
#54114 = ORIENTED_EDGE('',*,*,#40143,.T.) ;
#54115 = ORIENTED_EDGE('',*,*,#40011,.F.) ;
#54116 = ORIENTED_EDGE('',*,*,#40146,.F.) ;
#54117 = ORIENTED_EDGE('',*,*,#39580,.F.) ;
#54118 = ORIENTED_EDGE('',*,*,#39987,.F.) ;
#54119 = ORIENTED_EDGE('',*,*,#40142,.T.) ;
#54120 = ORIENTED_EDGE('',*,*,#40147,.F.) ;
#54121 = ORIENTED_EDGE('',*,*,#40148,.F.) ;
#54122 = ORIENTED_EDGE('',*,*,#40144,.T.) ;
#54123 = ORIENTED_EDGE('',*,*,#39991,.F.) ;
#54124 = ORIENTED_EDGE('',*,*,#40149,.F.) ;
#54125 = ORIENTED_EDGE('',*,*,#40001,.F.) ;
#54126 = ORIENTED_EDGE('',*,*,#40150,.F.) ;
#54127 = ORIENTED_EDGE('',*,*,#40002,.F.) ;
#54128 = ORIENTED_EDGE('',*,*,#40151,.F.) ;
#54129 = ORIENTED_EDGE('',*,*,#39996,.F.) ;
#54130 = ORIENTED_EDGE('',*,*,#39330,.T.) ;
#54131 = ORIENTED_EDGE('',*,*,#40150,.T.) ;
#54132 = ORIENTED_EDGE('',*,*,#40152,.F.) ;
#54133 = ORIENTED_EDGE('',*,*,#39567,.T.) ;
#54134 = ORIENTED_EDGE('',*,*,#40146,.T.) ;
#54135 = ORIENTED_EDGE('',*,*,#40145,.T.) ;
#54136 = ORIENTED_EDGE('',*,*,#40153,.F.) ;
#54137 = ORIENTED_EDGE('',*,*,#40154,.F.) ;
#54138 = ORIENTED_EDGE('',*,*,#39585,.F.) ;
#54139 = ORIENTED_EDGE('',*,*,#40155,.F.) ;
#54140 = ORIENTED_EDGE('',*,*,#40156,.F.) ;
#54141 = ORIENTED_EDGE('',*,*,#40147,.T.) ;
#54142 = ORIENTED_EDGE('',*,*,#39583,.F.) ;
#54143 = ORIENTED_EDGE('',*,*,#40155,.T.) ;
#54144 = ORIENTED_EDGE('',*,*,#39694,.F.) ;
#54145 = ORIENTED_EDGE('',*,*,#40148,.T.) ;
#54146 = ORIENTED_EDGE('',*,*,#40157,.F.) ;
#54147 = ORIENTED_EDGE('',*,*,#40158,.F.) ;
#54148 = ORIENTED_EDGE('',*,*,#40151,.T.) ;
#54149 = ORIENTED_EDGE('',*,*,#40149,.T.) ;
#54150 = ORIENTED_EDGE('',*,*,#40159,.F.) ;
#54151 = ORIENTED_EDGE('',*,*,#40152,.T.) ;
#54152 = ORIENTED_EDGE('',*,*,#39999,.F.) ;
#54153 = ORIENTED_EDGE('',*,*,#40160,.F.) ;
#54154 = ORIENTED_EDGE('',*,*,#39568,.F.) ;
#54155 = ORIENTED_EDGE('',*,*,#40153,.T.) ;
#54156 = ORIENTED_EDGE('',*,*,#39571,.F.) ;
#54157 = ORIENTED_EDGE('',*,*,#40161,.F.) ;
#54158 = ORIENTED_EDGE('',*,*,#39581,.F.) ;
#54159 = ORIENTED_EDGE('',*,*,#40154,.T.) ;
#54160 = ORIENTED_EDGE('',*,*,#39582,.F.) ;
#54161 = ORIENTED_EDGE('',*,*,#40162,.F.) ;
#54162 = ORIENTED_EDGE('',*,*,#39597,.F.) ;
#54163 = ORIENTED_EDGE('',*,*,#40156,.T.) ;
#54164 = ORIENTED_EDGE('',*,*,#39693,.T.) ;
#54165 = ORIENTED_EDGE('',*,*,#40163,.F.) ;
#54166 = ORIENTED_EDGE('',*,*,#40157,.T.) ;
#54167 = ORIENTED_EDGE('',*,*,#39988,.F.) ;
#54168 = ORIENTED_EDGE('',*,*,#40158,.T.) ;
#54169 = ORIENTED_EDGE('',*,*,#40164,.F.) ;
#54170 = ORIENTED_EDGE('',*,*,#40165,.F.) ;
#54171 = ORIENTED_EDGE('',*,*,#40159,.T.) ;
#54172 = ORIENTED_EDGE('',*,*,#39990,.F.) ;
#54173 = ORIENTED_EDGE('',*,*,#40166,.F.) ;
#54174 = ORIENTED_EDGE('',*,*,#39997,.F.) ;
#54175 = ORIENTED_EDGE('',*,*,#40167,.F.) ;
#54176 = ORIENTED_EDGE('',*,*,#39998,.F.) ;
#54177 = ORIENTED_EDGE('',*,*,#40168,.F.) ;
#54178 = ORIENTED_EDGE('',*,*,#39578,.F.) ;
#54179 = ORIENTED_EDGE('',*,*,#40160,.T.) ;
#54180 = ORIENTED_EDGE('',*,*,#40167,.T.) ;
#54181 = ORIENTED_EDGE('',*,*,#40169,.F.) ;
#54182 = ORIENTED_EDGE('',*,*,#40162,.T.) ;
#54183 = ORIENTED_EDGE('',*,*,#40161,.T.) ;
#54184 = ORIENTED_EDGE('',*,*,#40170,.F.) ;
#54185 = ORIENTED_EDGE('',*,*,#39598,.T.) ;
#54186 = ORIENTED_EDGE('',*,*,#40171,.F.) ;
#54187 = ORIENTED_EDGE('',*,*,#40164,.T.) ;
#54188 = ORIENTED_EDGE('',*,*,#40163,.T.) ;
#54189 = ORIENTED_EDGE('',*,*,#39692,.F.) ;
#54190 = ORIENTED_EDGE('',*,*,#40165,.T.) ;
#54191 = ORIENTED_EDGE('',*,*,#40172,.F.) ;
#54192 = ORIENTED_EDGE('',*,*,#40173,.F.) ;
#54193 = ORIENTED_EDGE('',*,*,#40168,.T.) ;
#54194 = ORIENTED_EDGE('',*,*,#40166,.T.) ;
#54195 = ORIENTED_EDGE('',*,*,#40174,.F.) ;
#54196 = ORIENTED_EDGE('',*,*,#39574,.T.) ;
#54197 = ORIENTED_EDGE('',*,*,#40169,.T.) ;
#54198 = ORIENTED_EDGE('',*,*,#39577,.F.) ;
#54199 = ORIENTED_EDGE('',*,*,#40175,.F.) ;
#54200 = ORIENTED_EDGE('',*,*,#39569,.F.) ;
#54201 = ORIENTED_EDGE('',*,*,#40170,.T.) ;
#54202 = ORIENTED_EDGE('',*,*,#39570,.F.) ;
#54203 = ORIENTED_EDGE('',*,*,#40176,.F.) ;
#54204 = ORIENTED_EDGE('',*,*,#39599,.F.) ;
#54205 = ORIENTED_EDGE('',*,*,#40171,.T.) ;
#54206 = ORIENTED_EDGE('',*,*,#39691,.T.) ;
#54207 = ORIENTED_EDGE('',*,*,#40177,.F.) ;
#54208 = ORIENTED_EDGE('',*,*,#40172,.T.) ;
#54209 = ORIENTED_EDGE('',*,*,#39989,.F.) ;
#54210 = ORIENTED_EDGE('',*,*,#40173,.T.) ;
#54211 = ORIENTED_EDGE('',*,*,#40178,.F.) ;
#54212 = ORIENTED_EDGE('',*,*,#40174,.T.) ;
#54213 = ORIENTED_EDGE('',*,*,#40176,.T.) ;
#54214 = ORIENTED_EDGE('',*,*,#40175,.T.) ;
#54215 = ORIENTED_EDGE('',*,*,#40179,.F.) ;
#54216 = ORIENTED_EDGE('',*,*,#39600,.T.) ;
#54217 = ORIENTED_EDGE('',*,*,#40177,.T.) ;
#54218 = ORIENTED_EDGE('',*,*,#39690,.F.) ;
#54219 = ORIENTED_EDGE('',*,*,#40180,.F.) ;
#54220 = ORIENTED_EDGE('',*,*,#39575,.F.) ;
#54221 = ORIENTED_EDGE('',*,*,#40178,.T.) ;
#54222 = ORIENTED_EDGE('',*,*,#40179,.T.) ;
#54223 = ORIENTED_EDGE('',*,*,#39576,.F.) ;
#54224 = ORIENTED_EDGE('',*,*,#40181,.F.) ;
#54225 = ORIENTED_EDGE('',*,*,#39601,.F.) ;
#54226 = ORIENTED_EDGE('',*,*,#40180,.T.) ;
#54227 = ORIENTED_EDGE('',*,*,#39530,.F.) ;
#54228 = ORIENTED_EDGE('',*,*,#40181,.T.) ;
#54229 = ORIENTED_EDGE('',*,*,#40182,.F.) ;
#54230 = ORIENTED_EDGE('',*,*,#40183,.F.) ;
#54231 = ORIENTED_EDGE('',*,*,#39714,.F.) ;
#54232 = ORIENTED_EDGE('',*,*,#40183,.T.) ;
#54233 = ORIENTED_EDGE('',*,*,#39971,.F.) ;
#54234 = ORIENTED_EDGE('',*,*,#40184,.F.) ;
#54235 = ORIENTED_EDGE('',*,*,#39711,.F.) ;
#54236 = ORIENTED_EDGE('',*,*,#40182,.T.) ;
#54237 = ORIENTED_EDGE('',*,*,#39717,.F.) ;
#54238 = ORIENTED_EDGE('',*,*,#40185,.F.) ;
#54239 = ORIENTED_EDGE('',*,*,#39972,.F.) ;
#54240 = ORIENTED_EDGE('',*,*,#40184,.T.) ;
#54241 = ORIENTED_EDGE('',*,*,#39970,.F.) ;
#54242 = ORIENTED_EDGE('',*,*,#40186,.F.) ;
#54243 = ORIENTED_EDGE('',*,*,#39708,.F.) ;
#54244 = ORIENTED_EDGE('',*,*,#40185,.T.) ;
#54245 = ORIENTED_EDGE('',*,*,#39720,.F.) ;
#54246 = ORIENTED_EDGE('',*,*,#40187,.F.) ;
#54247 = ORIENTED_EDGE('',*,*,#40186,.T.) ;
#54248 = ORIENTED_EDGE('',*,*,#39969,.F.) ;
#54249 = ORIENTED_EDGE('',*,*,#40188,.F.) ;
#54250 = ORIENTED_EDGE('',*,*,#39705,.F.) ;
#54251 = ORIENTED_EDGE('',*,*,#40187,.T.) ;
#54252 = ORIENTED_EDGE('',*,*,#39723,.F.) ;
#54253 = ORIENTED_EDGE('',*,*,#40189,.F.) ;
#54254 = ORIENTED_EDGE('',*,*,#39973,.F.) ;
#54255 = ORIENTED_EDGE('',*,*,#39702,.F.) ;
#54256 = ORIENTED_EDGE('',*,*,#40188,.T.) ;
#54257 = ORIENTED_EDGE('',*,*,#40190,.F.) ;
#54258 = ORIENTED_EDGE('',*,*,#40189,.T.) ;
#54259 = ORIENTED_EDGE('',*,*,#39726,.F.) ;
#54260 = ORIENTED_EDGE('',*,*,#40191,.F.) ;
#54261 = ORIENTED_EDGE('',*,*,#39974,.F.) ;
#54262 = ORIENTED_EDGE('',*,*,#40190,.T.) ;
#54263 = ORIENTED_EDGE('',*,*,#39968,.F.) ;
#54264 = ORIENTED_EDGE('',*,*,#40192,.F.) ;
#54265 = ORIENTED_EDGE('',*,*,#39697,.F.) ;
#54266 = ORIENTED_EDGE('',*,*,#40191,.T.) ;
#54267 = ORIENTED_EDGE('',*,*,#39729,.F.) ;
#54268 = ORIENTED_EDGE('',*,*,#40193,.F.) ;
#54269 = ORIENTED_EDGE('',*,*,#39975,.F.) ;
#54270 = ORIENTED_EDGE('',*,*,#39647,.F.) ;
#54271 = ORIENTED_EDGE('',*,*,#40192,.T.) ;
#54272 = ORIENTED_EDGE('',*,*,#40194,.F.) ;
#54273 = ORIENTED_EDGE('',*,*,#40193,.T.) ;
#54274 = ORIENTED_EDGE('',*,*,#39732,.F.) ;
#54275 = ORIENTED_EDGE('',*,*,#40195,.F.) ;
#54276 = ORIENTED_EDGE('',*,*,#40194,.T.) ;
#54277 = ORIENTED_EDGE('',*,*,#39967,.F.) ;
#54278 = ORIENTED_EDGE('',*,*,#40196,.F.) ;
#54279 = ORIENTED_EDGE('',*,*,#39595,.F.) ;
#54280 = ORIENTED_EDGE('',*,*,#40195,.T.) ;
#54281 = ORIENTED_EDGE('',*,*,#39734,.F.) ;
#54282 = ORIENTED_EDGE('',*,*,#40197,.F.) ;
#54283 = ORIENTED_EDGE('',*,*,#39966,.F.) ;
#54284 = ORIENTED_EDGE('',*,*,#39589,.F.) ;
#54285 = ORIENTED_EDGE('',*,*,#40196,.T.) ;
#54286 = ORIENTED_EDGE('',*,*,#40197,.T.) ;
#54287 = ORIENTED_EDGE('',*,*,#40198,.F.) ;
#54288 = ORIENTED_EDGE('',*,*,#39715,.F.) ;
#54289 = ORIENTED_EDGE('',*,*,#40199,.F.) ;
#54290 = ORIENTED_EDGE('',*,*,#40199,.T.) ;
#54291 = ORIENTED_EDGE('',*,*,#39712,.F.) ;
#54292 = ORIENTED_EDGE('',*,*,#40200,.F.) ;
#54293 = ORIENTED_EDGE('',*,*,#39983,.F.) ;
#54294 = ORIENTED_EDGE('',*,*,#40198,.T.) ;
#54295 = ORIENTED_EDGE('',*,*,#39982,.F.) ;
#54296 = ORIENTED_EDGE('',*,*,#40201,.F.) ;
#54297 = ORIENTED_EDGE('',*,*,#39718,.F.) ;
#54298 = ORIENTED_EDGE('',*,*,#40200,.T.) ;
#54299 = ORIENTED_EDGE('',*,*,#39709,.F.) ;
#54300 = ORIENTED_EDGE('',*,*,#40202,.F.) ;
#54301 = ORIENTED_EDGE('',*,*,#39984,.F.) ;
#54302 = ORIENTED_EDGE('',*,*,#39721,.F.) ;
#54303 = ORIENTED_EDGE('',*,*,#40201,.T.) ;
#54304 = ORIENTED_EDGE('',*,*,#40203,.F.) ;
#54305 = ORIENTED_EDGE('',*,*,#40202,.T.) ;
#54306 = ORIENTED_EDGE('',*,*,#39706,.F.) ;
#54307 = ORIENTED_EDGE('',*,*,#40204,.F.) ;
#54308 = ORIENTED_EDGE('',*,*,#39985,.F.) ;
#54309 = ORIENTED_EDGE('',*,*,#40203,.T.) ;
#54310 = ORIENTED_EDGE('',*,*,#39981,.F.) ;
#54311 = ORIENTED_EDGE('',*,*,#40205,.F.) ;
#54312 = ORIENTED_EDGE('',*,*,#39724,.F.) ;
#54313 = ORIENTED_EDGE('',*,*,#40204,.T.) ;
#54314 = ORIENTED_EDGE('',*,*,#39703,.F.) ;
#54315 = ORIENTED_EDGE('',*,*,#40206,.F.) ;
#54316 = ORIENTED_EDGE('',*,*,#40205,.T.) ;
#54317 = ORIENTED_EDGE('',*,*,#39980,.F.) ;
#54318 = ORIENTED_EDGE('',*,*,#40207,.F.) ;
#54319 = ORIENTED_EDGE('',*,*,#39727,.F.) ;
#54320 = ORIENTED_EDGE('',*,*,#40206,.T.) ;
#54321 = ORIENTED_EDGE('',*,*,#39695,.F.) ;
#54322 = ORIENTED_EDGE('',*,*,#40208,.F.) ;
#54323 = ORIENTED_EDGE('',*,*,#39976,.F.) ;
#54324 = ORIENTED_EDGE('',*,*,#40207,.T.) ;
#54325 = ORIENTED_EDGE('',*,*,#39979,.F.) ;
#54326 = ORIENTED_EDGE('',*,*,#40209,.F.) ;
#54327 = ORIENTED_EDGE('',*,*,#39730,.F.) ;
#54328 = ORIENTED_EDGE('',*,*,#40208,.T.) ;
#54329 = ORIENTED_EDGE('',*,*,#39587,.F.) ;
#54330 = ORIENTED_EDGE('',*,*,#40210,.F.) ;
#54331 = ORIENTED_EDGE('',*,*,#39733,.F.) ;
#54332 = ORIENTED_EDGE('',*,*,#40209,.T.) ;
#54333 = ORIENTED_EDGE('',*,*,#40211,.F.) ;
#54334 = ORIENTED_EDGE('',*,*,#40210,.T.) ;
#54335 = ORIENTED_EDGE('',*,*,#39596,.F.) ;
#54336 = ORIENTED_EDGE('',*,*,#40212,.F.) ;
#54337 = ORIENTED_EDGE('',*,*,#39977,.F.) ;
#54338 = ORIENTED_EDGE('',*,*,#40211,.T.) ;
#54339 = ORIENTED_EDGE('',*,*,#39978,.F.) ;
#54340 = ORIENTED_EDGE('',*,*,#40213,.F.) ;
#54341 = ORIENTED_EDGE('',*,*,#39735,.F.) ;
#54342 = ORIENTED_EDGE('',*,*,#40212,.T.) ;
#54343 = ORIENTED_EDGE('',*,*,#39591,.F.) ;
#54344 = ORIENTED_EDGE('',*,*,#40213,.T.) ;
#54345 = ORIENTED_EDGE('',*,*,#40214,.F.) ;
#54346 = ORIENTED_EDGE('',*,*,#40056,.F.) ;
#54347 = ORIENTED_EDGE('',*,*,#40215,.F.) ;
#54348 = ORIENTED_EDGE('',*,*,#40103,.F.) ;
#54349 = ORIENTED_EDGE('',*,*,#40215,.T.) ;
#54350 = ORIENTED_EDGE('',*,*,#40053,.F.) ;
#54351 = ORIENTED_EDGE('',*,*,#40216,.F.) ;
#54352 = ORIENTED_EDGE('',*,*,#40104,.F.) ;
#54353 = ORIENTED_EDGE('',*,*,#40059,.F.) ;
#54354 = ORIENTED_EDGE('',*,*,#40214,.T.) ;
#54355 = ORIENTED_EDGE('',*,*,#40217,.F.) ;
#54356 = ORIENTED_EDGE('',*,*,#40216,.T.) ;
#54357 = ORIENTED_EDGE('',*,*,#40050,.F.) ;
#54358 = ORIENTED_EDGE('',*,*,#40218,.F.) ;
#54359 = ORIENTED_EDGE('',*,*,#40105,.F.) ;
#54360 = ORIENTED_EDGE('',*,*,#40217,.T.) ;
#54361 = ORIENTED_EDGE('',*,*,#40102,.F.) ;
#54362 = ORIENTED_EDGE('',*,*,#40219,.F.) ;
#54363 = ORIENTED_EDGE('',*,*,#40062,.F.) ;
#54364 = ORIENTED_EDGE('',*,*,#40218,.T.) ;
#54365 = ORIENTED_EDGE('',*,*,#40047,.F.) ;
#54366 = ORIENTED_EDGE('',*,*,#40220,.F.) ;
#54367 = ORIENTED_EDGE('',*,*,#40106,.F.) ;
#54368 = ORIENTED_EDGE('',*,*,#40065,.F.) ;
#54369 = ORIENTED_EDGE('',*,*,#40219,.T.) ;
#54370 = ORIENTED_EDGE('',*,*,#40221,.F.) ;
#54371 = ORIENTED_EDGE('',*,*,#40220,.T.) ;
#54372 = ORIENTED_EDGE('',*,*,#40044,.F.) ;
#54373 = ORIENTED_EDGE('',*,*,#40222,.F.) ;
#54374 = ORIENTED_EDGE('',*,*,#40107,.F.) ;
#54375 = ORIENTED_EDGE('',*,*,#40221,.T.) ;
#54376 = ORIENTED_EDGE('',*,*,#40101,.F.) ;
#54377 = ORIENTED_EDGE('',*,*,#40223,.F.) ;
#54378 = ORIENTED_EDGE('',*,*,#40068,.F.) ;
#54379 = ORIENTED_EDGE('',*,*,#40222,.T.) ;
#54380 = ORIENTED_EDGE('',*,*,#40041,.F.) ;
#54381 = ORIENTED_EDGE('',*,*,#40224,.F.) ;
#54382 = ORIENTED_EDGE('',*,*,#40071,.F.) ;
#54383 = ORIENTED_EDGE('',*,*,#40223,.T.) ;
#54384 = ORIENTED_EDGE('',*,*,#40225,.F.) ;
#54385 = ORIENTED_EDGE('',*,*,#40224,.T.) ;
#54386 = ORIENTED_EDGE('',*,*,#40038,.F.) ;
#54387 = ORIENTED_EDGE('',*,*,#40226,.F.) ;
#54388 = ORIENTED_EDGE('',*,*,#40108,.F.) ;
#54389 = ORIENTED_EDGE('',*,*,#40225,.T.) ;
#54390 = ORIENTED_EDGE('',*,*,#40100,.F.) ;
#54391 = ORIENTED_EDGE('',*,*,#40227,.F.) ;
#54392 = ORIENTED_EDGE('',*,*,#40074,.F.) ;
#54393 = ORIENTED_EDGE('',*,*,#40226,.T.) ;
#54394 = ORIENTED_EDGE('',*,*,#39335,.F.) ;
#54395 = ORIENTED_EDGE('',*,*,#40228,.F.) ;
#54396 = ORIENTED_EDGE('',*,*,#40077,.F.) ;
#54397 = ORIENTED_EDGE('',*,*,#40227,.T.) ;
#54398 = ORIENTED_EDGE('',*,*,#40229,.F.) ;
#54399 = ORIENTED_EDGE('',*,*,#40228,.T.) ;
#54400 = ORIENTED_EDGE('',*,*,#40036,.F.) ;
#54401 = ORIENTED_EDGE('',*,*,#39326,.F.) ;
#54402 = ORIENTED_EDGE('',*,*,#40109,.F.) ;
#54403 = ORIENTED_EDGE('',*,*,#40229,.T.) ;
#54404 = ORIENTED_EDGE('',*,*,#40099,.F.) ;
#54405 = ORIENTED_EDGE('',*,*,#40230,.F.) ;
#54406 = ORIENTED_EDGE('',*,*,#40080,.F.) ;
#54407 = ORIENTED_EDGE('',*,*,#40083,.F.) ;
#54408 = ORIENTED_EDGE('',*,*,#40230,.T.) ;
#54409 = ORIENTED_EDGE('',*,*,#40231,.F.) ;
#54410 = ORIENTED_EDGE('',*,*,#39325,.T.) ;
#54411 = ORIENTED_EDGE('',*,*,#40031,.F.) ;
#54412 = ORIENTED_EDGE('',*,*,#40232,.F.) ;
#54413 = ORIENTED_EDGE('',*,*,#40110,.F.) ;
#54414 = ORIENTED_EDGE('',*,*,#40231,.T.) ;
#54415 = ORIENTED_EDGE('',*,*,#40098,.F.) ;
#54416 = ORIENTED_EDGE('',*,*,#40233,.F.) ;
#54417 = ORIENTED_EDGE('',*,*,#40086,.F.) ;
#54418 = ORIENTED_EDGE('',*,*,#40232,.T.) ;
#54419 = ORIENTED_EDGE('',*,*,#40028,.F.) ;
#54420 = ORIENTED_EDGE('',*,*,#40234,.F.) ;
#54421 = ORIENTED_EDGE('',*,*,#40089,.F.) ;
#54422 = ORIENTED_EDGE('',*,*,#40233,.T.) ;
#54423 = ORIENTED_EDGE('',*,*,#40235,.F.) ;
#54424 = ORIENTED_EDGE('',*,*,#40234,.T.) ;
#54425 = ORIENTED_EDGE('',*,*,#40025,.F.) ;
#54426 = ORIENTED_EDGE('',*,*,#40236,.F.) ;
#54427 = ORIENTED_EDGE('',*,*,#40111,.F.) ;
#54428 = ORIENTED_EDGE('',*,*,#40235,.T.) ;
#54429 = ORIENTED_EDGE('',*,*,#40097,.F.) ;
#54430 = ORIENTED_EDGE('',*,*,#40237,.F.) ;
#54431 = ORIENTED_EDGE('',*,*,#40092,.F.) ;
#54432 = ORIENTED_EDGE('',*,*,#40236,.T.) ;
#54433 = ORIENTED_EDGE('',*,*,#40022,.F.) ;
#54434 = ORIENTED_EDGE('',*,*,#40238,.F.) ;
#54435 = ORIENTED_EDGE('',*,*,#40094,.F.) ;
#54436 = ORIENTED_EDGE('',*,*,#40237,.T.) ;
#54437 = ORIENTED_EDGE('',*,*,#40096,.F.) ;
#54438 = ORIENTED_EDGE('',*,*,#40239,.F.) ;
#54439 = ORIENTED_EDGE('',*,*,#40016,.F.) ;
#54440 = ORIENTED_EDGE('',*,*,#40238,.T.) ;
#54441 = ORIENTED_EDGE('',*,*,#40019,.F.) ;
#54442 = ORIENTED_EDGE('',*,*,#40239,.T.) ;
#54443 = ORIENTED_EDGE('',*,*,#40095,.F.) ;
#54444 = ORIENTED_EDGE('',*,*,#40240,.F.) ;
#54445 = ORIENTED_EDGE('',*,*,#40052,.F.) ;
#54446 = ORIENTED_EDGE('',*,*,#40241,.F.) ;
#54447 = ORIENTED_EDGE('',*,*,#39954,.F.) ;
#54448 = ORIENTED_EDGE('',*,*,#40049,.F.) ;
#54449 = ORIENTED_EDGE('',*,*,#40240,.T.) ;
#54450 = ORIENTED_EDGE('',*,*,#40242,.F.) ;
#54451 = ORIENTED_EDGE('',*,*,#40241,.T.) ;
#54452 = ORIENTED_EDGE('',*,*,#40055,.F.) ;
#54453 = ORIENTED_EDGE('',*,*,#40243,.F.) ;
#54454 = ORIENTED_EDGE('',*,*,#40242,.T.) ;
#54455 = ORIENTED_EDGE('',*,*,#39953,.F.) ;
#54456 = ORIENTED_EDGE('',*,*,#40244,.F.) ;
#54457 = ORIENTED_EDGE('',*,*,#40046,.F.) ;
#54458 = ORIENTED_EDGE('',*,*,#40243,.T.) ;
#54459 = ORIENTED_EDGE('',*,*,#40058,.F.) ;
#54460 = ORIENTED_EDGE('',*,*,#40245,.F.) ;
#54461 = ORIENTED_EDGE('',*,*,#39955,.F.) ;
#54462 = ORIENTED_EDGE('',*,*,#40244,.T.) ;
#54463 = ORIENTED_EDGE('',*,*,#39952,.F.) ;
#54464 = ORIENTED_EDGE('',*,*,#40246,.F.) ;
#54465 = ORIENTED_EDGE('',*,*,#40043,.F.) ;
#54466 = ORIENTED_EDGE('',*,*,#40245,.T.) ;
#54467 = ORIENTED_EDGE('',*,*,#40061,.F.) ;
#54468 = ORIENTED_EDGE('',*,*,#40247,.F.) ;
#54469 = ORIENTED_EDGE('',*,*,#39956,.F.) ;
#54470 = ORIENTED_EDGE('',*,*,#40246,.T.) ;
#54471 = ORIENTED_EDGE('',*,*,#39951,.F.) ;
#54472 = ORIENTED_EDGE('',*,*,#39320,.F.) ;
#54473 = ORIENTED_EDGE('',*,*,#40040,.F.) ;
#54474 = ORIENTED_EDGE('',*,*,#40247,.T.) ;
#54475 = ORIENTED_EDGE('',*,*,#40064,.F.) ;
#54476 = ORIENTED_EDGE('',*,*,#40248,.F.) ;
#54477 = ORIENTED_EDGE('',*,*,#39957,.F.) ;
#54478 = ORIENTED_EDGE('',*,*,#40248,.T.) ;
#54479 = ORIENTED_EDGE('',*,*,#40067,.F.) ;
#54480 = ORIENTED_EDGE('',*,*,#40249,.F.) ;
#54481 = ORIENTED_EDGE('',*,*,#39958,.F.) ;
#54482 = ORIENTED_EDGE('',*,*,#39318,.T.) ;
#54483 = ORIENTED_EDGE('',*,*,#39950,.F.) ;
#54484 = ORIENTED_EDGE('',*,*,#40250,.F.) ;
#54485 = ORIENTED_EDGE('',*,*,#40037,.F.) ;
#54486 = ORIENTED_EDGE('',*,*,#40249,.T.) ;
#54487 = ORIENTED_EDGE('',*,*,#40070,.F.) ;
#54488 = ORIENTED_EDGE('',*,*,#40251,.F.) ;
#54489 = ORIENTED_EDGE('',*,*,#39959,.F.) ;
#54490 = ORIENTED_EDGE('',*,*,#40250,.T.) ;
#54491 = ORIENTED_EDGE('',*,*,#39949,.F.) ;
#54492 = ORIENTED_EDGE('',*,*,#40252,.F.) ;
#54493 = ORIENTED_EDGE('',*,*,#40035,.F.) ;
#54494 = ORIENTED_EDGE('',*,*,#40251,.T.) ;
#54495 = ORIENTED_EDGE('',*,*,#40073,.F.) ;
#54496 = ORIENTED_EDGE('',*,*,#40253,.F.) ;
#54497 = ORIENTED_EDGE('',*,*,#39960,.F.) ;
#54498 = ORIENTED_EDGE('',*,*,#40252,.T.) ;
#54499 = ORIENTED_EDGE('',*,*,#39948,.F.) ;
#54500 = ORIENTED_EDGE('',*,*,#40254,.F.) ;
#54501 = ORIENTED_EDGE('',*,*,#40033,.F.) ;
#54502 = ORIENTED_EDGE('',*,*,#40253,.T.) ;
#54503 = ORIENTED_EDGE('',*,*,#40076,.F.) ;
#54504 = ORIENTED_EDGE('',*,*,#40255,.F.) ;
#54505 = ORIENTED_EDGE('',*,*,#39961,.F.) ;
#54506 = ORIENTED_EDGE('',*,*,#40254,.T.) ;
#54507 = ORIENTED_EDGE('',*,*,#39947,.F.) ;
#54508 = ORIENTED_EDGE('',*,*,#40256,.F.) ;
#54509 = ORIENTED_EDGE('',*,*,#40030,.F.) ;
#54510 = ORIENTED_EDGE('',*,*,#40255,.T.) ;
#54511 = ORIENTED_EDGE('',*,*,#40079,.F.) ;
#54512 = ORIENTED_EDGE('',*,*,#40257,.F.) ;
#54513 = ORIENTED_EDGE('',*,*,#39962,.F.) ;
#54514 = ORIENTED_EDGE('',*,*,#40256,.T.) ;
#54515 = ORIENTED_EDGE('',*,*,#39946,.F.) ;
#54516 = ORIENTED_EDGE('',*,*,#40258,.F.) ;
#54517 = ORIENTED_EDGE('',*,*,#40027,.F.) ;
#54518 = ORIENTED_EDGE('',*,*,#40257,.T.) ;
#54519 = ORIENTED_EDGE('',*,*,#40082,.F.) ;
#54520 = ORIENTED_EDGE('',*,*,#40259,.F.) ;
#54521 = ORIENTED_EDGE('',*,*,#39963,.F.) ;
#54522 = ORIENTED_EDGE('',*,*,#40024,.F.) ;
#54523 = ORIENTED_EDGE('',*,*,#40258,.T.) ;
#54524 = ORIENTED_EDGE('',*,*,#40260,.F.) ;
#54525 = ORIENTED_EDGE('',*,*,#40259,.T.) ;
#54526 = ORIENTED_EDGE('',*,*,#40085,.F.) ;
#54527 = ORIENTED_EDGE('',*,*,#40261,.F.) ;
#54528 = ORIENTED_EDGE('',*,*,#39964,.F.) ;
#54529 = ORIENTED_EDGE('',*,*,#40260,.T.) ;
#54530 = ORIENTED_EDGE('',*,*,#39945,.F.) ;
#54531 = ORIENTED_EDGE('',*,*,#40262,.F.) ;
#54532 = ORIENTED_EDGE('',*,*,#40021,.F.) ;
#54533 = ORIENTED_EDGE('',*,*,#40261,.T.) ;
#54534 = ORIENTED_EDGE('',*,*,#40088,.F.) ;
#54535 = ORIENTED_EDGE('',*,*,#40263,.F.) ;
#54536 = ORIENTED_EDGE('',*,*,#39965,.F.) ;
#54537 = ORIENTED_EDGE('',*,*,#40018,.F.) ;
#54538 = ORIENTED_EDGE('',*,*,#40262,.T.) ;
#54539 = ORIENTED_EDGE('',*,*,#40264,.F.) ;
#54540 = ORIENTED_EDGE('',*,*,#40263,.T.) ;
#54541 = ORIENTED_EDGE('',*,*,#40091,.F.) ;
#54542 = ORIENTED_EDGE('',*,*,#40265,.F.) ;
#54543 = ORIENTED_EDGE('',*,*,#39943,.F.) ;
#54544 = ORIENTED_EDGE('',*,*,#40264,.T.) ;
#54545 = ORIENTED_EDGE('',*,*,#39944,.F.) ;
#54546 = ORIENTED_EDGE('',*,*,#40265,.T.) ;
#54547 = ORIENTED_EDGE('',*,*,#40093,.F.) ;
#54548 = ORIENTED_EDGE('',*,*,#40266,.T.) ;
#54549 = ORIENTED_EDGE('',*,*,#40267,.T.) ;
#54550 = ORIENTED_EDGE('',*,*,#40268,.T.) ;
#54551 = ORIENTED_EDGE('',*,*,#40269,.T.) ;
#54552 = ORIENTED_EDGE('',*,*,#40270,.T.) ;
#54553 = ORIENTED_EDGE('',*,*,#40271,.T.) ;
#54554 = ORIENTED_EDGE('',*,*,#40272,.T.) ;
#54555 = ORIENTED_EDGE('',*,*,#40273,.T.) ;
#54556 = ORIENTED_EDGE('',*,*,#40274,.T.) ;
#54557 = ORIENTED_EDGE('',*,*,#40275,.T.) ;
#54558 = ORIENTED_EDGE('',*,*,#40276,.T.) ;
#54559 = ORIENTED_EDGE('',*,*,#40277,.T.) ;
#54560 = ORIENTED_EDGE('',*,*,#40278,.T.) ;
#54561 = ORIENTED_EDGE('',*,*,#40279,.T.) ;
#54562 = ORIENTED_EDGE('',*,*,#40280,.T.) ;
#54563 = ORIENTED_EDGE('',*,*,#40281,.T.) ;
#54564 = ORIENTED_EDGE('',*,*,#40282,.T.) ;
#54565 = ORIENTED_EDGE('',*,*,#40283,.T.) ;
#54566 = ORIENTED_EDGE('',*,*,#40284,.F.) ;
#54567 = ORIENTED_EDGE('',*,*,#40285,.T.) ;
#54568 = ORIENTED_EDGE('',*,*,#40286,.T.) ;
#54569 = ORIENTED_EDGE('',*,*,#40287,.T.) ;
#54570 = ORIENTED_EDGE('',*,*,#40134,.T.) ;
#54571 = ORIENTED_EDGE('',*,*,#40288,.T.) ;
#54572 = ORIENTED_EDGE('',*,*,#40289,.T.) ;
#54573 = ORIENTED_EDGE('',*,*,#40290,.T.) ;
#54574 = ORIENTED_EDGE('',*,*,#40291,.T.) ;
#54575 = ORIENTED_EDGE('',*,*,#40292,.T.) ;
#54576 = ORIENTED_EDGE('',*,*,#39332,.T.) ;
#54577 = ORIENTED_EDGE('',*,*,#40293,.T.) ;
#54578 = ORIENTED_EDGE('',*,*,#40294,.T.) ;
#54579 = ORIENTED_EDGE('',*,*,#40295,.T.) ;
#54580 = ORIENTED_EDGE('',*,*,#40131,.T.) ;
#54581 = ORIENTED_EDGE('',*,*,#40296,.T.) ;
#54582 = ORIENTED_EDGE('',*,*,#40266,.F.) ;
#54583 = ORIENTED_EDGE('',*,*,#40297,.T.) ;
#54584 = ORIENTED_EDGE('',*,*,#40132,.T.) ;
#54585 = ORIENTED_EDGE('',*,*,#40284,.T.) ;
#54586 = ORIENTED_EDGE('',*,*,#40298,.T.) ;
#54587 = ORIENTED_EDGE('',*,*,#39565,.F.) ;
#54588 = ORIENTED_EDGE('',*,*,#40299,.T.) ;
#54589 = ORIENTED_EDGE('',*,*,#40300,.T.) ;
#54590 = ORIENTED_EDGE('',*,*,#40301,.T.) ;
#54591 = ORIENTED_EDGE('',*,*,#40302,.T.) ;
#54592 = ORIENTED_EDGE('',*,*,#40303,.T.) ;
#54593 = ORIENTED_EDGE('',*,*,#40304,.T.) ;
#54594 = ORIENTED_EDGE('',*,*,#40305,.T.) ;
#54595 = ORIENTED_EDGE('',*,*,#40114,.F.) ;
#54596 = ORIENTED_EDGE('',*,*,#40306,.T.) ;
#54597 = ORIENTED_EDGE('',*,*,#40118,.F.) ;
#54598 = ORIENTED_EDGE('',*,*,#40307,.T.) ;
#54599 = ORIENTED_EDGE('',*,*,#40308,.T.) ;
#54600 = ORIENTED_EDGE('',*,*,#40309,.T.) ;
#54601 = ORIENTED_EDGE('',*,*,#40310,.T.) ;
#54602 = ORIENTED_EDGE('',*,*,#40311,.T.) ;
#54603 = ORIENTED_EDGE('',*,*,#40312,.T.) ;
#54604 = ORIENTED_EDGE('',*,*,#40313,.T.) ;
#54605 = ORIENTED_EDGE('',*,*,#40314,.T.) ;
#54606 = ORIENTED_EDGE('',*,*,#40315,.T.) ;
#54607 = ORIENTED_EDGE('',*,*,#40316,.T.) ;
#54608 = ORIENTED_EDGE('',*,*,#40317,.T.) ;
#54609 = ORIENTED_EDGE('',*,*,#40318,.T.) ;
#54610 = ORIENTED_EDGE('',*,*,#40319,.T.) ;
#54611 = ORIENTED_EDGE('',*,*,#40112,.T.) ;
#54612 = ORIENTED_EDGE('',*,*,#40320,.T.) ;
#54613 = ORIENTED_EDGE('',*,*,#40116,.F.) ;
#54614 = ORIENTED_EDGE('',*,*,#40321,.T.) ;
#54615 = ORIENTED_EDGE('',*,*,#40322,.T.) ;
#54616 = ORIENTED_EDGE('',*,*,#40323,.T.) ;
#54617 = ORIENTED_EDGE('',*,*,#40324,.T.) ;
#54618 = ORIENTED_EDGE('',*,*,#40325,.T.) ;
#54619 = ORIENTED_EDGE('',*,*,#40326,.T.) ;
#54620 = ORIENTED_EDGE('',*,*,#40327,.T.) ;
#54621 = ORIENTED_EDGE('',*,*,#40328,.T.) ;
#54622 = ORIENTED_EDGE('',*,*,#40329,.T.) ;
#54623 = ORIENTED_EDGE('',*,*,#40330,.T.) ;
#54624 = ORIENTED_EDGE('',*,*,#40331,.T.) ;
#54625 = ORIENTED_EDGE('',*,*,#40332,.T.) ;
#54626 = ORIENTED_EDGE('',*,*,#40333,.T.) ;
#54627 = ORIENTED_EDGE('',*,*,#40334,.T.) ;
#54628 = ORIENTED_EDGE('',*,*,#40335,.T.) ;
#54629 = ORIENTED_EDGE('',*,*,#40336,.T.) ;
#54630 = ORIENTED_EDGE('',*,*,#40337,.T.) ;
#54631 = ORIENTED_EDGE('',*,*,#40338,.T.) ;
#54632 = ORIENTED_EDGE('',*,*,#40339,.T.) ;
#54633 = ORIENTED_EDGE('',*,*,#40326,.F.) ;
#54634 = ORIENTED_EDGE('',*,*,#40340,.T.) ;
#54635 = ORIENTED_EDGE('',*,*,#40281,.F.) ;
#54636 = ORIENTED_EDGE('',*,*,#40341,.F.) ;
#54637 = ORIENTED_EDGE('',*,*,#40278,.F.) ;
#54638 = ORIENTED_EDGE('',*,*,#40342,.T.) ;
#54639 = ORIENTED_EDGE('',*,*,#40282,.F.) ;
#54640 = ORIENTED_EDGE('',*,*,#40343,.T.) ;
#54641 = ORIENTED_EDGE('',*,*,#40344,.F.) ;
#54642 = ORIENTED_EDGE('',*,*,#40341,.T.) ;
#54643 = ORIENTED_EDGE('',*,*,#40345,.F.) ;
#54644 = ORIENTED_EDGE('',*,*,#40279,.F.) ;
#54645 = ORIENTED_EDGE('',*,*,#40346,.T.) ;
#54646 = ORIENTED_EDGE('',*,*,#40328,.F.) ;
#54647 = ORIENTED_EDGE('',*,*,#40347,.F.) ;
#54648 = ORIENTED_EDGE('',*,*,#40345,.T.) ;
#54649 = ORIENTED_EDGE('',*,*,#40280,.F.) ;
#54650 = ORIENTED_EDGE('',*,*,#40348,.F.) ;
#54651 = ORIENTED_EDGE('',*,*,#40274,.F.) ;
#54652 = ORIENTED_EDGE('',*,*,#40344,.T.) ;
#54653 = ORIENTED_EDGE('',*,*,#40277,.F.) ;
#54654 = ORIENTED_EDGE('',*,*,#40349,.F.) ;
#54655 = ORIENTED_EDGE('',*,*,#40327,.F.) ;
#54656 = ORIENTED_EDGE('',*,*,#40348,.T.) ;
#54657 = ORIENTED_EDGE('',*,*,#40347,.T.) ;
#54658 = ORIENTED_EDGE('',*,*,#40350,.F.) ;
#54659 = ORIENTED_EDGE('',*,*,#40351,.F.) ;
#54660 = ORIENTED_EDGE('',*,*,#40349,.T.) ;
#54661 = ORIENTED_EDGE('',*,*,#40352,.F.) ;
#54662 = ORIENTED_EDGE('',*,*,#40350,.T.) ;
#54663 = ORIENTED_EDGE('',*,*,#40331,.F.) ;
#54664 = ORIENTED_EDGE('',*,*,#40353,.F.) ;
#54665 = ORIENTED_EDGE('',*,*,#40275,.F.) ;
#54666 = ORIENTED_EDGE('',*,*,#40352,.T.) ;
#54667 = ORIENTED_EDGE('',*,*,#40276,.F.) ;
#54668 = ORIENTED_EDGE('',*,*,#40354,.F.) ;
#54669 = ORIENTED_EDGE('',*,*,#40270,.F.) ;
#54670 = ORIENTED_EDGE('',*,*,#40273,.F.) ;
#54671 = ORIENTED_EDGE('',*,*,#40355,.T.) ;
#54672 = ORIENTED_EDGE('',*,*,#40324,.F.) ;
#54673 = ORIENTED_EDGE('',*,*,#40351,.T.) ;
#54674 = ORIENTED_EDGE('',*,*,#40354,.T.) ;
#54675 = ORIENTED_EDGE('',*,*,#40353,.T.) ;
#54676 = ORIENTED_EDGE('',*,*,#40356,.F.) ;
#54677 = ORIENTED_EDGE('',*,*,#40268,.F.) ;
#54678 = ORIENTED_EDGE('',*,*,#40357,.T.) ;
#54679 = ORIENTED_EDGE('',*,*,#40272,.F.) ;
#54680 = ORIENTED_EDGE('',*,*,#40358,.T.) ;
#54681 = ORIENTED_EDGE('',*,*,#40330,.F.) ;
#54682 = ORIENTED_EDGE('',*,*,#40359,.T.) ;
#54683 = ORIENTED_EDGE('',*,*,#40271,.F.) ;
#54684 = ORIENTED_EDGE('',*,*,#40356,.T.) ;
#54685 = ORIENTED_EDGE('',*,*,#40334,.F.) ;
#54686 = ORIENTED_EDGE('',*,*,#40360,.T.) ;
#54687 = ORIENTED_EDGE('',*,*,#40303,.F.) ;
#54688 = ORIENTED_EDGE('',*,*,#40361,.F.) ;
#54689 = ORIENTED_EDGE('',*,*,#40300,.F.) ;
#54690 = ORIENTED_EDGE('',*,*,#40362,.T.) ;
#54691 = ORIENTED_EDGE('',*,*,#40304,.F.) ;
#54692 = ORIENTED_EDGE('',*,*,#40363,.T.) ;
#54693 = ORIENTED_EDGE('',*,*,#40364,.F.) ;
#54694 = ORIENTED_EDGE('',*,*,#40361,.T.) ;
#54695 = ORIENTED_EDGE('',*,*,#40365,.F.) ;
#54696 = ORIENTED_EDGE('',*,*,#40301,.F.) ;
#54697 = ORIENTED_EDGE('',*,*,#40366,.T.) ;
#54698 = ORIENTED_EDGE('',*,*,#40336,.F.) ;
#54699 = ORIENTED_EDGE('',*,*,#40367,.F.) ;
#54700 = ORIENTED_EDGE('',*,*,#40365,.T.) ;
#54701 = ORIENTED_EDGE('',*,*,#40302,.F.) ;
#54702 = ORIENTED_EDGE('',*,*,#40368,.F.) ;
#54703 = ORIENTED_EDGE('',*,*,#40316,.F.) ;
#54704 = ORIENTED_EDGE('',*,*,#40364,.T.) ;
#54705 = ORIENTED_EDGE('',*,*,#40315,.F.) ;
#54706 = ORIENTED_EDGE('',*,*,#40369,.F.) ;
#54707 = ORIENTED_EDGE('',*,*,#40335,.F.) ;
#54708 = ORIENTED_EDGE('',*,*,#40368,.T.) ;
#54709 = ORIENTED_EDGE('',*,*,#40367,.T.) ;
#54710 = ORIENTED_EDGE('',*,*,#40370,.F.) ;
#54711 = ORIENTED_EDGE('',*,*,#40371,.F.) ;
#54712 = ORIENTED_EDGE('',*,*,#40369,.T.) ;
#54713 = ORIENTED_EDGE('',*,*,#40372,.F.) ;
#54714 = ORIENTED_EDGE('',*,*,#40370,.T.) ;
#54715 = ORIENTED_EDGE('',*,*,#40339,.F.) ;
#54716 = ORIENTED_EDGE('',*,*,#40373,.F.) ;
#54717 = ORIENTED_EDGE('',*,*,#40317,.F.) ;
#54718 = ORIENTED_EDGE('',*,*,#40372,.T.) ;
#54719 = ORIENTED_EDGE('',*,*,#40314,.F.) ;
#54720 = ORIENTED_EDGE('',*,*,#40374,.F.) ;
#54721 = ORIENTED_EDGE('',*,*,#40310,.F.) ;
#54722 = ORIENTED_EDGE('',*,*,#40313,.F.) ;
#54723 = ORIENTED_EDGE('',*,*,#40375,.T.) ;
#54724 = ORIENTED_EDGE('',*,*,#40332,.F.) ;
#54725 = ORIENTED_EDGE('',*,*,#40371,.T.) ;
#54726 = ORIENTED_EDGE('',*,*,#40374,.T.) ;
#54727 = ORIENTED_EDGE('',*,*,#40373,.T.) ;
#54728 = ORIENTED_EDGE('',*,*,#40376,.F.) ;
#54729 = ORIENTED_EDGE('',*,*,#40308,.F.) ;
#54730 = ORIENTED_EDGE('',*,*,#40377,.T.) ;
#54731 = ORIENTED_EDGE('',*,*,#40312,.F.) ;
#54732 = ORIENTED_EDGE('',*,*,#40378,.T.) ;
#54733 = ORIENTED_EDGE('',*,*,#40338,.F.) ;
#54734 = ORIENTED_EDGE('',*,*,#40379,.T.) ;
#54735 = ORIENTED_EDGE('',*,*,#40311,.F.) ;
#54736 = ORIENTED_EDGE('',*,*,#40376,.T.) ;
#54737 = ORIENTED_EDGE('',*,*,#39566,.F.) ;
#54738 = ORIENTED_EDGE('',*,*,#40298,.F.) ;
#54739 = ORIENTED_EDGE('',*,*,#40380,.F.) ;
#54740 = ORIENTED_EDGE('',*,*,#40293,.F.) ;
#54741 = ORIENTED_EDGE('',*,*,#40380,.T.) ;
#54742 = ORIENTED_EDGE('',*,*,#40283,.F.) ;
#54743 = ORIENTED_EDGE('',*,*,#40381,.F.) ;
#54744 = ORIENTED_EDGE('',*,*,#40294,.F.) ;
#54745 = ORIENTED_EDGE('',*,*,#40381,.T.) ;
#54746 = ORIENTED_EDGE('',*,*,#40342,.F.) ;
#54747 = ORIENTED_EDGE('',*,*,#40340,.F.) ;
#54748 = ORIENTED_EDGE('',*,*,#40382,.F.) ;
#54749 = ORIENTED_EDGE('',*,*,#40382,.T.) ;
#54750 = ORIENTED_EDGE('',*,*,#40325,.F.) ;
#54751 = ORIENTED_EDGE('',*,*,#40383,.F.) ;
#54752 = ORIENTED_EDGE('',*,*,#40295,.F.) ;
#54753 = ORIENTED_EDGE('',*,*,#40383,.T.) ;
#54754 = ORIENTED_EDGE('',*,*,#40355,.F.) ;
#54755 = ORIENTED_EDGE('',*,*,#40357,.F.) ;
#54756 = ORIENTED_EDGE('',*,*,#40384,.F.) ;
#54757 = ORIENTED_EDGE('',*,*,#40384,.T.) ;
#54758 = ORIENTED_EDGE('',*,*,#40267,.F.) ;
#54759 = ORIENTED_EDGE('',*,*,#40385,.F.) ;
#54760 = ORIENTED_EDGE('',*,*,#40291,.F.) ;
#54761 = ORIENTED_EDGE('',*,*,#39333,.F.) ;
#54762 = ORIENTED_EDGE('',*,*,#40292,.F.) ;
#54763 = ORIENTED_EDGE('',*,*,#40385,.T.) ;
#54764 = ORIENTED_EDGE('',*,*,#40296,.F.) ;
#54765 = ORIENTED_EDGE('',*,*,#40130,.F.) ;
#54766 = ORIENTED_EDGE('',*,*,#40133,.F.) ;
#54767 = ORIENTED_EDGE('',*,*,#40297,.F.) ;
#54768 = ORIENTED_EDGE('',*,*,#40386,.F.) ;
#54769 = ORIENTED_EDGE('',*,*,#40288,.F.) ;
#54770 = ORIENTED_EDGE('',*,*,#40386,.T.) ;
#54771 = ORIENTED_EDGE('',*,*,#40269,.F.) ;
#54772 = ORIENTED_EDGE('',*,*,#40387,.F.) ;
#54773 = ORIENTED_EDGE('',*,*,#40289,.F.) ;
#54774 = ORIENTED_EDGE('',*,*,#40387,.T.) ;
#54775 = ORIENTED_EDGE('',*,*,#40358,.F.) ;
#54776 = ORIENTED_EDGE('',*,*,#40359,.F.) ;
#54777 = ORIENTED_EDGE('',*,*,#40388,.F.) ;
#54778 = ORIENTED_EDGE('',*,*,#40388,.T.) ;
#54779 = ORIENTED_EDGE('',*,*,#40329,.F.) ;
#54780 = ORIENTED_EDGE('',*,*,#40389,.F.) ;
#54781 = ORIENTED_EDGE('',*,*,#40290,.F.) ;
#54782 = ORIENTED_EDGE('',*,*,#40389,.T.) ;
#54783 = ORIENTED_EDGE('',*,*,#40346,.F.) ;
#54784 = ORIENTED_EDGE('',*,*,#40343,.F.) ;
#54785 = ORIENTED_EDGE('',*,*,#40390,.F.) ;
#54786 = ORIENTED_EDGE('',*,*,#40390,.T.) ;
#54787 = ORIENTED_EDGE('',*,*,#40285,.F.) ;
#54788 = ORIENTED_EDGE('',*,*,#40391,.F.) ;
#54789 = ORIENTED_EDGE('',*,*,#40286,.F.) ;
#54790 = ORIENTED_EDGE('',*,*,#40391,.T.) ;
#54791 = ORIENTED_EDGE('',*,*,#40299,.F.) ;
#54792 = ORIENTED_EDGE('',*,*,#39564,.F.) ;
#54793 = ORIENTED_EDGE('',*,*,#40287,.F.) ;
#54794 = ORIENTED_EDGE('',*,*,#40115,.F.) ;
#54795 = ORIENTED_EDGE('',*,*,#40305,.F.) ;
#54796 = ORIENTED_EDGE('',*,*,#40392,.F.) ;
#54797 = ORIENTED_EDGE('',*,*,#40321,.F.) ;
#54798 = ORIENTED_EDGE('',*,*,#40392,.T.) ;
#54799 = ORIENTED_EDGE('',*,*,#40362,.F.) ;
#54800 = ORIENTED_EDGE('',*,*,#40360,.F.) ;
#54801 = ORIENTED_EDGE('',*,*,#40393,.F.) ;
#54802 = ORIENTED_EDGE('',*,*,#40393,.T.) ;
#54803 = ORIENTED_EDGE('',*,*,#40333,.F.) ;
#54804 = ORIENTED_EDGE('',*,*,#40394,.F.) ;
#54805 = ORIENTED_EDGE('',*,*,#40322,.F.) ;
#54806 = ORIENTED_EDGE('',*,*,#40394,.T.) ;
#54807 = ORIENTED_EDGE('',*,*,#40375,.F.) ;
#54808 = ORIENTED_EDGE('',*,*,#40377,.F.) ;
#54809 = ORIENTED_EDGE('',*,*,#40395,.F.) ;
#54810 = ORIENTED_EDGE('',*,*,#40117,.F.) ;
#54811 = ORIENTED_EDGE('',*,*,#40323,.F.) ;
#54812 = ORIENTED_EDGE('',*,*,#40395,.T.) ;
#54813 = ORIENTED_EDGE('',*,*,#40307,.F.) ;
#54814 = ORIENTED_EDGE('',*,*,#40396,.F.) ;
#54815 = ORIENTED_EDGE('',*,*,#40306,.F.) ;
#54816 = ORIENTED_EDGE('',*,*,#40113,.F.) ;
#54817 = ORIENTED_EDGE('',*,*,#40319,.F.) ;
#54818 = ORIENTED_EDGE('',*,*,#40363,.F.) ;
#54819 = ORIENTED_EDGE('',*,*,#40396,.T.) ;
#54820 = ORIENTED_EDGE('',*,*,#40397,.F.) ;
#54821 = ORIENTED_EDGE('',*,*,#40366,.F.) ;
#54822 = ORIENTED_EDGE('',*,*,#40397,.T.) ;
#54823 = ORIENTED_EDGE('',*,*,#40318,.F.) ;
#54824 = ORIENTED_EDGE('',*,*,#40398,.F.) ;
#54825 = ORIENTED_EDGE('',*,*,#40337,.F.) ;
#54826 = ORIENTED_EDGE('',*,*,#40119,.F.) ;
#54827 = ORIENTED_EDGE('',*,*,#40309,.F.) ;
#54828 = ORIENTED_EDGE('',*,*,#40399,.F.) ;
#54829 = ORIENTED_EDGE('',*,*,#40320,.F.) ;
#54830 = ORIENTED_EDGE('',*,*,#40379,.F.) ;
#54831 = ORIENTED_EDGE('',*,*,#40398,.T.) ;
#54832 = ORIENTED_EDGE('',*,*,#40399,.T.) ;
#54833 = ORIENTED_EDGE('',*,*,#40378,.F.) ;
#54834 = ORIENTED_EDGE('',*,*,#40400,.T.) ;
#54835 = ORIENTED_EDGE('',*,*,#40401,.T.) ;
#54836 = ORIENTED_EDGE('',*,*,#40402,.T.) ;
#54837 = ORIENTED_EDGE('',*,*,#40403,.T.) ;
#54838 = ORIENTED_EDGE('',*,*,#40404,.T.) ;
#54839 = ORIENTED_EDGE('',*,*,#40405,.T.) ;
#54840 = ORIENTED_EDGE('',*,*,#40406,.F.) ;
#54841 = ORIENTED_EDGE('',*,*,#40407,.T.) ;
#54842 = ORIENTED_EDGE('',*,*,#40408,.F.) ;
#54843 = ORIENTED_EDGE('',*,*,#40409,.T.) ;
#54844 = ORIENTED_EDGE('',*,*,#40410,.T.) ;
#54845 = ORIENTED_EDGE('',*,*,#40411,.T.) ;
#54846 = ORIENTED_EDGE('',*,*,#40412,.T.) ;
#54847 = ORIENTED_EDGE('',*,*,#40413,.T.) ;
#54848 = ORIENTED_EDGE('',*,*,#40414,.T.) ;
#54849 = ORIENTED_EDGE('',*,*,#40415,.T.) ;
#54850 = ORIENTED_EDGE('',*,*,#40416,.F.) ;
#54851 = ORIENTED_EDGE('',*,*,#40417,.T.) ;
#54852 = ORIENTED_EDGE('',*,*,#40418,.F.) ;
#54853 = ORIENTED_EDGE('',*,*,#40419,.T.) ;
#54854 = ORIENTED_EDGE('',*,*,#40420,.T.) ;
#54855 = ORIENTED_EDGE('',*,*,#40421,.T.) ;
#54856 = ORIENTED_EDGE('',*,*,#40422,.T.) ;
#54857 = ORIENTED_EDGE('',*,*,#40423,.T.) ;
#54858 = ORIENTED_EDGE('',*,*,#40424,.T.) ;
#54859 = ORIENTED_EDGE('',*,*,#40425,.T.) ;
#54860 = ORIENTED_EDGE('',*,*,#40426,.F.) ;
#54861 = ORIENTED_EDGE('',*,*,#40427,.T.) ;
#54862 = ORIENTED_EDGE('',*,*,#40428,.F.) ;
#54863 = ORIENTED_EDGE('',*,*,#40429,.T.) ;
#54864 = ORIENTED_EDGE('',*,*,#40430,.T.) ;
#54865 = ORIENTED_EDGE('',*,*,#40431,.T.) ;
#54866 = ORIENTED_EDGE('',*,*,#40432,.T.) ;
#54867 = ORIENTED_EDGE('',*,*,#40433,.T.) ;
#54868 = ORIENTED_EDGE('',*,*,#40434,.T.) ;
#54869 = ORIENTED_EDGE('',*,*,#40435,.T.) ;
#54870 = ORIENTED_EDGE('',*,*,#40436,.F.) ;
#54871 = ORIENTED_EDGE('',*,*,#40437,.T.) ;
#54872 = ORIENTED_EDGE('',*,*,#40438,.F.) ;
#54873 = ORIENTED_EDGE('',*,*,#40439,.T.) ;
#54874 = ORIENTED_EDGE('',*,*,#40440,.T.) ;
#54875 = ORIENTED_EDGE('',*,*,#40441,.T.) ;
#54876 = ORIENTED_EDGE('',*,*,#40442,.T.) ;
#54877 = ORIENTED_EDGE('',*,*,#40443,.T.) ;
#54878 = ORIENTED_EDGE('',*,*,#40444,.T.) ;
#54879 = ORIENTED_EDGE('',*,*,#40445,.T.) ;
#54880 = ORIENTED_EDGE('',*,*,#40446,.F.) ;
#54881 = ORIENTED_EDGE('',*,*,#40447,.T.) ;
#54882 = ORIENTED_EDGE('',*,*,#40448,.F.) ;
#54883 = ORIENTED_EDGE('',*,*,#40449,.T.) ;
#54884 = ORIENTED_EDGE('',*,*,#40450,.T.) ;
#54885 = ORIENTED_EDGE('',*,*,#40451,.T.) ;
#54886 = ORIENTED_EDGE('',*,*,#40452,.T.) ;
#54887 = ORIENTED_EDGE('',*,*,#40453,.T.) ;
#54888 = ORIENTED_EDGE('',*,*,#40454,.T.) ;
#54889 = ORIENTED_EDGE('',*,*,#40455,.T.) ;
#54890 = ORIENTED_EDGE('',*,*,#40456,.F.) ;
#54891 = ORIENTED_EDGE('',*,*,#40457,.T.) ;
#54892 = ORIENTED_EDGE('',*,*,#40458,.F.) ;
#54893 = ORIENTED_EDGE('',*,*,#40459,.T.) ;
#54894 = ORIENTED_EDGE('',*,*,#40460,.T.) ;
#54895 = ORIENTED_EDGE('',*,*,#40461,.T.) ;
#54896 = ORIENTED_EDGE('',*,*,#40462,.T.) ;
#54897 = ORIENTED_EDGE('',*,*,#40463,.T.) ;
#54898 = ORIENTED_EDGE('',*,*,#40464,.T.) ;
#54899 = ORIENTED_EDGE('',*,*,#40465,.T.) ;
#54900 = ORIENTED_EDGE('',*,*,#40466,.F.) ;
#54901 = ORIENTED_EDGE('',*,*,#40467,.T.) ;
#54902 = ORIENTED_EDGE('',*,*,#40468,.F.) ;
#54903 = ORIENTED_EDGE('',*,*,#40469,.T.) ;
#54904 = ORIENTED_EDGE('',*,*,#40470,.T.) ;
#54905 = ORIENTED_EDGE('',*,*,#40471,.T.) ;
#54906 = ORIENTED_EDGE('',*,*,#40472,.T.) ;
#54907 = ORIENTED_EDGE('',*,*,#40473,.T.) ;
#54908 = ORIENTED_EDGE('',*,*,#40474,.T.) ;
#54909 = ORIENTED_EDGE('',*,*,#40475,.T.) ;
#54910 = ORIENTED_EDGE('',*,*,#40476,.F.) ;
#54911 = ORIENTED_EDGE('',*,*,#40477,.T.) ;
#54912 = ORIENTED_EDGE('',*,*,#40478,.F.) ;
#54913 = ORIENTED_EDGE('',*,*,#40479,.T.) ;
#54914 = ORIENTED_EDGE('',*,*,#40480,.T.) ;
#54915 = ORIENTED_EDGE('',*,*,#40481,.T.) ;
#54916 = ORIENTED_EDGE('',*,*,#40482,.T.) ;
#54917 = ORIENTED_EDGE('',*,*,#40483,.T.) ;
#54918 = ORIENTED_EDGE('',*,*,#40484,.T.) ;
#54919 = ORIENTED_EDGE('',*,*,#40485,.T.) ;
#54920 = ORIENTED_EDGE('',*,*,#40486,.F.) ;
#54921 = ORIENTED_EDGE('',*,*,#40487,.T.) ;
#54922 = ORIENTED_EDGE('',*,*,#40488,.F.) ;
#54923 = ORIENTED_EDGE('',*,*,#40489,.T.) ;
#54924 = ORIENTED_EDGE('',*,*,#40490,.T.) ;
#54925 = ORIENTED_EDGE('',*,*,#40491,.T.) ;
#54926 = ORIENTED_EDGE('',*,*,#40492,.T.) ;
#54927 = ORIENTED_EDGE('',*,*,#40493,.T.) ;
#54928 = ORIENTED_EDGE('',*,*,#40494,.T.) ;
#54929 = ORIENTED_EDGE('',*,*,#40495,.T.) ;
#54930 = ORIENTED_EDGE('',*,*,#40496,.T.) ;
#54931 = ORIENTED_EDGE('',*,*,#39272,.T.) ;
#54932 = ORIENTED_EDGE('',*,*,#40497,.T.) ;
#54933 = ORIENTED_EDGE('',*,*,#40498,.T.) ;
#54934 = ORIENTED_EDGE('',*,*,#40499,.T.) ;
#54935 = ORIENTED_EDGE('',*,*,#40500,.T.) ;
#54936 = ORIENTED_EDGE('',*,*,#40501,.T.) ;
#54937 = ORIENTED_EDGE('',*,*,#40502,.T.) ;
#54938 = ORIENTED_EDGE('',*,*,#40503,.T.) ;
#54939 = ORIENTED_EDGE('',*,*,#40504,.T.) ;
#54940 = ORIENTED_EDGE('',*,*,#40505,.T.) ;
#54941 = ORIENTED_EDGE('',*,*,#40506,.T.) ;
#54942 = ORIENTED_EDGE('',*,*,#40507,.T.) ;
#54943 = ORIENTED_EDGE('',*,*,#40508,.T.) ;
#54944 = ORIENTED_EDGE('',*,*,#40509,.T.) ;
#54945 = ORIENTED_EDGE('',*,*,#40510,.T.) ;
#54946 = ORIENTED_EDGE('',*,*,#40511,.T.) ;
#54947 = ORIENTED_EDGE('',*,*,#40512,.T.) ;
#54948 = ORIENTED_EDGE('',*,*,#40513,.T.) ;
#54949 = ORIENTED_EDGE('',*,*,#40514,.T.) ;
#54950 = ORIENTED_EDGE('',*,*,#40515,.T.) ;
#54951 = ORIENTED_EDGE('',*,*,#39219,.T.) ;
#54952 = ORIENTED_EDGE('',*,*,#40516,.T.) ;
#54953 = ORIENTED_EDGE('',*,*,#40517,.T.) ;
#54954 = ORIENTED_EDGE('',*,*,#40518,.T.) ;
#54955 = ORIENTED_EDGE('',*,*,#40519,.T.) ;
#54956 = ORIENTED_EDGE('',*,*,#40520,.T.) ;
#54957 = ORIENTED_EDGE('',*,*,#40521,.T.) ;
#54958 = ORIENTED_EDGE('',*,*,#40522,.T.) ;
#54959 = ORIENTED_EDGE('',*,*,#40523,.T.) ;
#54960 = ORIENTED_EDGE('',*,*,#40524,.T.) ;
#54961 = ORIENTED_EDGE('',*,*,#40525,.T.) ;
#54962 = ORIENTED_EDGE('',*,*,#40526,.T.) ;
#54963 = ORIENTED_EDGE('',*,*,#40527,.T.) ;
#54964 = ORIENTED_EDGE('',*,*,#40528,.T.) ;
#54965 = ORIENTED_EDGE('',*,*,#40529,.T.) ;
#54966 = ORIENTED_EDGE('',*,*,#40530,.T.) ;
#54967 = ORIENTED_EDGE('',*,*,#40531,.T.) ;
#54968 = ORIENTED_EDGE('',*,*,#40532,.T.) ;
#54969 = ORIENTED_EDGE('',*,*,#40533,.T.) ;
#54970 = ORIENTED_EDGE('',*,*,#40534,.T.) ;
#54971 = ORIENTED_EDGE('',*,*,#39202,.T.) ;
#54972 = ORIENTED_EDGE('',*,*,#40535,.T.) ;
#54973 = ORIENTED_EDGE('',*,*,#40536,.T.) ;
#54974 = ORIENTED_EDGE('',*,*,#40537,.T.) ;
#54975 = ORIENTED_EDGE('',*,*,#40538,.T.) ;
#54976 = ORIENTED_EDGE('',*,*,#40539,.T.) ;
#54977 = ORIENTED_EDGE('',*,*,#40540,.T.) ;
#54978 = ORIENTED_EDGE('',*,*,#40541,.T.) ;
#54979 = ORIENTED_EDGE('',*,*,#40542,.T.) ;
#54980 = ORIENTED_EDGE('',*,*,#40543,.T.) ;
#54981 = ORIENTED_EDGE('',*,*,#40544,.T.) ;
#54982 = ORIENTED_EDGE('',*,*,#40545,.T.) ;
#54983 = ORIENTED_EDGE('',*,*,#40546,.T.) ;
#54984 = ORIENTED_EDGE('',*,*,#40547,.T.) ;
#54985 = ORIENTED_EDGE('',*,*,#40548,.T.) ;
#54986 = ORIENTED_EDGE('',*,*,#40549,.T.) ;
#54987 = ORIENTED_EDGE('',*,*,#40550,.T.) ;
#54988 = ORIENTED_EDGE('',*,*,#40551,.T.) ;
#54989 = ORIENTED_EDGE('',*,*,#40552,.T.) ;
#54990 = ORIENTED_EDGE('',*,*,#40553,.T.) ;
#54991 = ORIENTED_EDGE('',*,*,#39185,.T.) ;
#54992 = ORIENTED_EDGE('',*,*,#40554,.T.) ;
#54993 = ORIENTED_EDGE('',*,*,#40555,.T.) ;
#54994 = ORIENTED_EDGE('',*,*,#40556,.T.) ;
#54995 = ORIENTED_EDGE('',*,*,#40557,.T.) ;
#54996 = ORIENTED_EDGE('',*,*,#40558,.T.) ;
#54997 = ORIENTED_EDGE('',*,*,#40559,.T.) ;
#54998 = ORIENTED_EDGE('',*,*,#40560,.T.) ;
#54999 = ORIENTED_EDGE('',*,*,#40561,.T.) ;
#55000 = ORIENTED_EDGE('',*,*,#40562,.T.) ;
#55001 = ORIENTED_EDGE('',*,*,#40563,.T.) ;
#55002 = ORIENTED_EDGE('',*,*,#40564,.T.) ;
#55003 = ORIENTED_EDGE('',*,*,#40565,.T.) ;
#55004 = ORIENTED_EDGE('',*,*,#40566,.T.) ;
#55005 = ORIENTED_EDGE('',*,*,#40567,.T.) ;
#55006 = ORIENTED_EDGE('',*,*,#40568,.T.) ;
#55007 = ORIENTED_EDGE('',*,*,#40569,.T.) ;
#55008 = ORIENTED_EDGE('',*,*,#40570,.T.) ;
#55009 = ORIENTED_EDGE('',*,*,#40571,.T.) ;
#55010 = ORIENTED_EDGE('',*,*,#40572,.T.) ;
#55011 = ORIENTED_EDGE('',*,*,#39168,.T.) ;
#55012 = ORIENTED_EDGE('',*,*,#40573,.T.) ;
#55013 = ORIENTED_EDGE('',*,*,#40574,.T.) ;
#55014 = ORIENTED_EDGE('',*,*,#40575,.T.) ;
#55015 = ORIENTED_EDGE('',*,*,#40576,.T.) ;
#55016 = ORIENTED_EDGE('',*,*,#40577,.T.) ;
#55017 = ORIENTED_EDGE('',*,*,#40578,.T.) ;
#55018 = ORIENTED_EDGE('',*,*,#40579,.T.) ;
#55019 = ORIENTED_EDGE('',*,*,#40580,.T.) ;
#55020 = ORIENTED_EDGE('',*,*,#40581,.T.) ;
#55021 = ORIENTED_EDGE('',*,*,#40582,.T.) ;
#55022 = ORIENTED_EDGE('',*,*,#40583,.T.) ;
#55023 = ORIENTED_EDGE('',*,*,#40584,.T.) ;
#55024 = ORIENTED_EDGE('',*,*,#40585,.T.) ;
#55025 = ORIENTED_EDGE('',*,*,#40586,.T.) ;
#55026 = ORIENTED_EDGE('',*,*,#40587,.T.) ;
#55027 = ORIENTED_EDGE('',*,*,#40588,.T.) ;
#55028 = ORIENTED_EDGE('',*,*,#40589,.T.) ;
#55029 = ORIENTED_EDGE('',*,*,#40590,.T.) ;
#55030 = ORIENTED_EDGE('',*,*,#40591,.T.) ;
#55031 = ORIENTED_EDGE('',*,*,#39151,.T.) ;
#55032 = ORIENTED_EDGE('',*,*,#40592,.T.) ;
#55033 = ORIENTED_EDGE('',*,*,#40593,.T.) ;
#55034 = ORIENTED_EDGE('',*,*,#40594,.T.) ;
#55035 = ORIENTED_EDGE('',*,*,#40595,.T.) ;
#55036 = ORIENTED_EDGE('',*,*,#40596,.T.) ;
#55037 = ORIENTED_EDGE('',*,*,#40597,.T.) ;
#55038 = ORIENTED_EDGE('',*,*,#40598,.T.) ;
#55039 = ORIENTED_EDGE('',*,*,#40599,.T.) ;
#55040 = ORIENTED_EDGE('',*,*,#40600,.T.) ;
#55041 = ORIENTED_EDGE('',*,*,#40601,.T.) ;
#55042 = ORIENTED_EDGE('',*,*,#40602,.T.) ;
#55043 = ORIENTED_EDGE('',*,*,#40603,.T.) ;
#55044 = ORIENTED_EDGE('',*,*,#40604,.T.) ;
#55045 = ORIENTED_EDGE('',*,*,#40605,.T.) ;
#55046 = ORIENTED_EDGE('',*,*,#40606,.T.) ;
#55047 = ORIENTED_EDGE('',*,*,#40607,.T.) ;
#55048 = ORIENTED_EDGE('',*,*,#40608,.T.) ;
#55049 = ORIENTED_EDGE('',*,*,#40609,.T.) ;
#55050 = ORIENTED_EDGE('',*,*,#40610,.T.) ;
#55051 = ORIENTED_EDGE('',*,*,#39134,.T.) ;
#55052 = ORIENTED_EDGE('',*,*,#40611,.T.) ;
#55053 = ORIENTED_EDGE('',*,*,#40612,.T.) ;
#55054 = ORIENTED_EDGE('',*,*,#40613,.T.) ;
#55055 = ORIENTED_EDGE('',*,*,#40614,.T.) ;
#55056 = ORIENTED_EDGE('',*,*,#40615,.T.) ;
#55057 = ORIENTED_EDGE('',*,*,#40616,.T.) ;
#55058 = ORIENTED_EDGE('',*,*,#40617,.T.) ;
#55059 = ORIENTED_EDGE('',*,*,#40618,.T.) ;
#55060 = ORIENTED_EDGE('',*,*,#40619,.T.) ;
#55061 = ORIENTED_EDGE('',*,*,#40620,.T.) ;
#55062 = ORIENTED_EDGE('',*,*,#40621,.T.) ;
#55063 = ORIENTED_EDGE('',*,*,#40622,.T.) ;
#55064 = ORIENTED_EDGE('',*,*,#40623,.T.) ;
#55065 = ORIENTED_EDGE('',*,*,#40624,.T.) ;
#55066 = ORIENTED_EDGE('',*,*,#40625,.T.) ;
#55067 = ORIENTED_EDGE('',*,*,#40626,.T.) ;
#55068 = ORIENTED_EDGE('',*,*,#40627,.T.) ;
#55069 = ORIENTED_EDGE('',*,*,#40628,.T.) ;
#55070 = ORIENTED_EDGE('',*,*,#40629,.T.) ;
#55071 = ORIENTED_EDGE('',*,*,#39117,.T.) ;
#55072 = ORIENTED_EDGE('',*,*,#40630,.T.) ;
#55073 = ORIENTED_EDGE('',*,*,#40631,.T.) ;
#55074 = ORIENTED_EDGE('',*,*,#40632,.T.) ;
#55075 = ORIENTED_EDGE('',*,*,#40633,.T.) ;
#55076 = ORIENTED_EDGE('',*,*,#40634,.T.) ;
#55077 = ORIENTED_EDGE('',*,*,#40635,.T.) ;
#55078 = ORIENTED_EDGE('',*,*,#40636,.T.) ;
#55079 = ORIENTED_EDGE('',*,*,#40637,.T.) ;
#55080 = ORIENTED_EDGE('',*,*,#40638,.T.) ;
#55081 = ORIENTED_EDGE('',*,*,#40639,.T.) ;
#55082 = ORIENTED_EDGE('',*,*,#40640,.T.) ;
#55083 = ORIENTED_EDGE('',*,*,#40641,.T.) ;
#55084 = ORIENTED_EDGE('',*,*,#40642,.T.) ;
#55085 = ORIENTED_EDGE('',*,*,#40643,.T.) ;
#55086 = ORIENTED_EDGE('',*,*,#40644,.T.) ;
#55087 = ORIENTED_EDGE('',*,*,#40645,.T.) ;
#55088 = ORIENTED_EDGE('',*,*,#40646,.T.) ;
#55089 = ORIENTED_EDGE('',*,*,#40647,.T.) ;
#55090 = ORIENTED_EDGE('',*,*,#40648,.T.) ;
#55091 = ORIENTED_EDGE('',*,*,#39100,.T.) ;
#55092 = ORIENTED_EDGE('',*,*,#40649,.T.) ;
#55093 = ORIENTED_EDGE('',*,*,#40650,.T.) ;
#55094 = ORIENTED_EDGE('',*,*,#40651,.T.) ;
#55095 = ORIENTED_EDGE('',*,*,#40652,.T.) ;
#55096 = ORIENTED_EDGE('',*,*,#40653,.T.) ;
#55097 = ORIENTED_EDGE('',*,*,#40654,.T.) ;
#55098 = ORIENTED_EDGE('',*,*,#40655,.T.) ;
#55099 = ORIENTED_EDGE('',*,*,#40656,.T.) ;
#55100 = ORIENTED_EDGE('',*,*,#40657,.T.) ;
#55101 = ORIENTED_EDGE('',*,*,#40658,.T.) ;
#55102 = ORIENTED_EDGE('',*,*,#40659,.T.) ;
#55103 = ORIENTED_EDGE('',*,*,#40660,.T.) ;
#55104 = ORIENTED_EDGE('',*,*,#40661,.F.) ;
#55105 = ORIENTED_EDGE('',*,*,#40662,.T.) ;
#55106 = ORIENTED_EDGE('',*,*,#40663,.T.) ;
#55107 = ORIENTED_EDGE('',*,*,#40664,.T.) ;
#55108 = ORIENTED_EDGE('',*,*,#40663,.F.) ;
#55109 = ORIENTED_EDGE('',*,*,#40665,.T.) ;
#55110 = ORIENTED_EDGE('',*,*,#40666,.T.) ;
#55111 = ORIENTED_EDGE('',*,*,#40667,.T.) ;
#55112 = ORIENTED_EDGE('',*,*,#40666,.F.) ;
#55113 = ORIENTED_EDGE('',*,*,#40668,.T.) ;
#55114 = ORIENTED_EDGE('',*,*,#40669,.T.) ;
#55115 = ORIENTED_EDGE('',*,*,#40670,.T.) ;
#55116 = ORIENTED_EDGE('',*,*,#40669,.F.) ;
#55117 = ORIENTED_EDGE('',*,*,#40671,.T.) ;
#55118 = ORIENTED_EDGE('',*,*,#40672,.T.) ;
#55119 = ORIENTED_EDGE('',*,*,#40673,.T.) ;
#55120 = ORIENTED_EDGE('',*,*,#40672,.F.) ;
#55121 = ORIENTED_EDGE('',*,*,#40674,.T.) ;
#55122 = ORIENTED_EDGE('',*,*,#40675,.T.) ;
#55123 = ORIENTED_EDGE('',*,*,#40676,.T.) ;
#55124 = ORIENTED_EDGE('',*,*,#40675,.F.) ;
#55125 = ORIENTED_EDGE('',*,*,#40677,.T.) ;
#55126 = ORIENTED_EDGE('',*,*,#40678,.T.) ;
#55127 = ORIENTED_EDGE('',*,*,#40679,.T.) ;
#55128 = ORIENTED_EDGE('',*,*,#40678,.F.) ;
#55129 = ORIENTED_EDGE('',*,*,#39095,.T.) ;
#55130 = ORIENTED_EDGE('',*,*,#40680,.T.) ;
#55131 = ORIENTED_EDGE('',*,*,#40681,.T.) ;
#55132 = ORIENTED_EDGE('',*,*,#40680,.F.) ;
#55133 = ORIENTED_EDGE('',*,*,#40682,.T.) ;
#55134 = ORIENTED_EDGE('',*,*,#39312,.T.) ;
#55135 = ORIENTED_EDGE('',*,*,#40683,.T.) ;
#55136 = ORIENTED_EDGE('',*,*,#39311,.F.) ;
#55137 = ORIENTED_EDGE('',*,*,#40684,.T.) ;
#55138 = ORIENTED_EDGE('',*,*,#40685,.T.) ;
#55139 = ORIENTED_EDGE('',*,*,#40686,.T.) ;
#55140 = ORIENTED_EDGE('',*,*,#40685,.F.) ;
#55141 = ORIENTED_EDGE('',*,*,#40687,.T.) ;
#55142 = ORIENTED_EDGE('',*,*,#40688,.T.) ;
#55143 = ORIENTED_EDGE('',*,*,#40689,.T.) ;
#55144 = ORIENTED_EDGE('',*,*,#40688,.F.) ;
#55145 = ORIENTED_EDGE('',*,*,#40690,.T.) ;
#55146 = ORIENTED_EDGE('',*,*,#40691,.T.) ;
#55147 = ORIENTED_EDGE('',*,*,#40692,.T.) ;
#55148 = ORIENTED_EDGE('',*,*,#40691,.F.) ;
#55149 = ORIENTED_EDGE('',*,*,#40693,.T.) ;
#55150 = ORIENTED_EDGE('',*,*,#40694,.T.) ;
#55151 = ORIENTED_EDGE('',*,*,#40695,.T.) ;
#55152 = ORIENTED_EDGE('',*,*,#40694,.F.) ;
#55153 = ORIENTED_EDGE('',*,*,#40696,.T.) ;
#55154 = ORIENTED_EDGE('',*,*,#40697,.T.) ;
#55155 = ORIENTED_EDGE('',*,*,#40698,.T.) ;
#55156 = ORIENTED_EDGE('',*,*,#40697,.F.) ;
#55157 = ORIENTED_EDGE('',*,*,#40699,.T.) ;
#55158 = ORIENTED_EDGE('',*,*,#40700,.T.) ;
#55159 = ORIENTED_EDGE('',*,*,#40701,.T.) ;
#55160 = ORIENTED_EDGE('',*,*,#40700,.F.) ;
#55161 = ORIENTED_EDGE('',*,*,#40702,.T.) ;
#55162 = ORIENTED_EDGE('',*,*,#40703,.T.) ;
#55163 = ORIENTED_EDGE('',*,*,#40704,.T.) ;
#55164 = ORIENTED_EDGE('',*,*,#40703,.F.) ;
#55165 = ORIENTED_EDGE('',*,*,#40705,.T.) ;
#55166 = ORIENTED_EDGE('',*,*,#40706,.T.) ;
#55167 = ORIENTED_EDGE('',*,*,#40707,.T.) ;
#55168 = ORIENTED_EDGE('',*,*,#40706,.F.) ;
#55169 = ORIENTED_EDGE('',*,*,#40708,.T.) ;
#55170 = ORIENTED_EDGE('',*,*,#40709,.T.) ;
#55171 = ORIENTED_EDGE('',*,*,#40710,.T.) ;
#55172 = ORIENTED_EDGE('',*,*,#40709,.F.) ;
#55173 = ORIENTED_EDGE('',*,*,#40711,.T.) ;
#55174 = ORIENTED_EDGE('',*,*,#40712,.T.) ;
#55175 = ORIENTED_EDGE('',*,*,#40713,.T.) ;
#55176 = ORIENTED_EDGE('',*,*,#40712,.F.) ;
#55177 = ORIENTED_EDGE('',*,*,#40714,.T.) ;
#55178 = ORIENTED_EDGE('',*,*,#40715,.T.) ;
#55179 = ORIENTED_EDGE('',*,*,#40716,.T.) ;
#55180 = ORIENTED_EDGE('',*,*,#40715,.F.) ;
#55181 = ORIENTED_EDGE('',*,*,#40717,.T.) ;
#55182 = ORIENTED_EDGE('',*,*,#40718,.T.) ;
#55183 = ORIENTED_EDGE('',*,*,#40719,.T.) ;
#55184 = ORIENTED_EDGE('',*,*,#40718,.F.) ;
#55185 = ORIENTED_EDGE('',*,*,#40720,.T.) ;
#55186 = ORIENTED_EDGE('',*,*,#40721,.T.) ;
#55187 = ORIENTED_EDGE('',*,*,#40722,.T.) ;
#55188 = ORIENTED_EDGE('',*,*,#40721,.F.) ;
#55189 = ORIENTED_EDGE('',*,*,#40723,.T.) ;
#55190 = ORIENTED_EDGE('',*,*,#40724,.T.) ;
#55191 = ORIENTED_EDGE('',*,*,#40725,.T.) ;
#55192 = ORIENTED_EDGE('',*,*,#40724,.F.) ;
#55193 = ORIENTED_EDGE('',*,*,#40726,.T.) ;
#55194 = ORIENTED_EDGE('',*,*,#40727,.T.) ;
#55195 = ORIENTED_EDGE('',*,*,#40728,.T.) ;
#55196 = ORIENTED_EDGE('',*,*,#40727,.F.) ;
#55197 = ORIENTED_EDGE('',*,*,#40729,.T.) ;
#55198 = ORIENTED_EDGE('',*,*,#40730,.T.) ;
#55199 = ORIENTED_EDGE('',*,*,#40731,.T.) ;
#55200 = ORIENTED_EDGE('',*,*,#40730,.F.) ;
#55201 = ORIENTED_EDGE('',*,*,#40732,.T.) ;
#55202 = ORIENTED_EDGE('',*,*,#40733,.T.) ;
#55203 = ORIENTED_EDGE('',*,*,#40734,.T.) ;
#55204 = ORIENTED_EDGE('',*,*,#40733,.F.) ;
#55205 = ORIENTED_EDGE('',*,*,#40735,.T.) ;
#55206 = ORIENTED_EDGE('',*,*,#40736,.T.) ;
#55207 = ORIENTED_EDGE('',*,*,#40737,.T.) ;
#55208 = ORIENTED_EDGE('',*,*,#40736,.F.) ;
#55209 = ORIENTED_EDGE('',*,*,#40738,.T.) ;
#55210 = ORIENTED_EDGE('',*,*,#40661,.T.) ;
#55211 = ORIENTED_EDGE('',*,*,#40739,.T.) ;
#55212 = ORIENTED_EDGE('',*,*,#40740,.T.) ;
#55213 = ORIENTED_EDGE('',*,*,#40741,.T.) ;
#55214 = ORIENTED_EDGE('',*,*,#40742,.T.) ;
#55215 = ORIENTED_EDGE('',*,*,#40743,.T.) ;
#55216 = ORIENTED_EDGE('',*,*,#40744,.T.) ;
#55217 = ORIENTED_EDGE('',*,*,#40745,.T.) ;
#55218 = ORIENTED_EDGE('',*,*,#40746,.T.) ;
#55219 = ORIENTED_EDGE('',*,*,#40747,.T.) ;
#55220 = ORIENTED_EDGE('',*,*,#40748,.T.) ;
#55221 = ORIENTED_EDGE('',*,*,#40749,.T.) ;
#55222 = ORIENTED_EDGE('',*,*,#40750,.T.) ;
#55223 = ORIENTED_EDGE('',*,*,#40751,.T.) ;
#55224 = ORIENTED_EDGE('',*,*,#40752,.T.) ;
#55225 = ORIENTED_EDGE('',*,*,#40753,.T.) ;
#55226 = ORIENTED_EDGE('',*,*,#40754,.T.) ;
#55227 = ORIENTED_EDGE('',*,*,#40755,.T.) ;
#55228 = ORIENTED_EDGE('',*,*,#40756,.T.) ;
#55229 = ORIENTED_EDGE('',*,*,#40757,.T.) ;
#55230 = ORIENTED_EDGE('',*,*,#39092,.T.) ;
#55231 = ORIENTED_EDGE('',*,*,#40758,.F.) ;
#55232 = ORIENTED_EDGE('',*,*,#40759,.T.) ;
#55233 = ORIENTED_EDGE('',*,*,#40760,.T.) ;
#55234 = ORIENTED_EDGE('',*,*,#40761,.T.) ;
#55235 = ORIENTED_EDGE('',*,*,#40760,.F.) ;
#55236 = ORIENTED_EDGE('',*,*,#40762,.T.) ;
#55237 = ORIENTED_EDGE('',*,*,#40763,.T.) ;
#55238 = ORIENTED_EDGE('',*,*,#40764,.T.) ;
#55239 = ORIENTED_EDGE('',*,*,#40763,.F.) ;
#55240 = ORIENTED_EDGE('',*,*,#40765,.T.) ;
#55241 = ORIENTED_EDGE('',*,*,#40766,.T.) ;
#55242 = ORIENTED_EDGE('',*,*,#40767,.T.) ;
#55243 = ORIENTED_EDGE('',*,*,#40766,.F.) ;
#55244 = ORIENTED_EDGE('',*,*,#40768,.T.) ;
#55245 = ORIENTED_EDGE('',*,*,#40769,.T.) ;
#55246 = ORIENTED_EDGE('',*,*,#40770,.T.) ;
#55247 = ORIENTED_EDGE('',*,*,#40769,.F.) ;
#55248 = ORIENTED_EDGE('',*,*,#40771,.T.) ;
#55249 = ORIENTED_EDGE('',*,*,#40772,.T.) ;
#55250 = ORIENTED_EDGE('',*,*,#40773,.T.) ;
#55251 = ORIENTED_EDGE('',*,*,#40772,.F.) ;
#55252 = ORIENTED_EDGE('',*,*,#40774,.T.) ;
#55253 = ORIENTED_EDGE('',*,*,#40775,.T.) ;
#55254 = ORIENTED_EDGE('',*,*,#40776,.T.) ;
#55255 = ORIENTED_EDGE('',*,*,#40775,.F.) ;
#55256 = ORIENTED_EDGE('',*,*,#39112,.T.) ;
#55257 = ORIENTED_EDGE('',*,*,#40777,.T.) ;
#55258 = ORIENTED_EDGE('',*,*,#40778,.T.) ;
#55259 = ORIENTED_EDGE('',*,*,#40777,.F.) ;
#55260 = ORIENTED_EDGE('',*,*,#40779,.T.) ;
#55261 = ORIENTED_EDGE('',*,*,#39309,.T.) ;
#55262 = ORIENTED_EDGE('',*,*,#40780,.T.) ;
#55263 = ORIENTED_EDGE('',*,*,#39308,.F.) ;
#55264 = ORIENTED_EDGE('',*,*,#40781,.T.) ;
#55265 = ORIENTED_EDGE('',*,*,#40782,.T.) ;
#55266 = ORIENTED_EDGE('',*,*,#40783,.T.) ;
#55267 = ORIENTED_EDGE('',*,*,#40782,.F.) ;
#55268 = ORIENTED_EDGE('',*,*,#40784,.T.) ;
#55269 = ORIENTED_EDGE('',*,*,#40785,.T.) ;
#55270 = ORIENTED_EDGE('',*,*,#40786,.T.) ;
#55271 = ORIENTED_EDGE('',*,*,#40785,.F.) ;
#55272 = ORIENTED_EDGE('',*,*,#40787,.T.) ;
#55273 = ORIENTED_EDGE('',*,*,#40788,.T.) ;
#55274 = ORIENTED_EDGE('',*,*,#40789,.T.) ;
#55275 = ORIENTED_EDGE('',*,*,#40788,.F.) ;
#55276 = ORIENTED_EDGE('',*,*,#40790,.T.) ;
#55277 = ORIENTED_EDGE('',*,*,#40791,.T.) ;
#55278 = ORIENTED_EDGE('',*,*,#40792,.T.) ;
#55279 = ORIENTED_EDGE('',*,*,#40791,.F.) ;
#55280 = ORIENTED_EDGE('',*,*,#40793,.T.) ;
#55281 = ORIENTED_EDGE('',*,*,#40794,.T.) ;
#55282 = ORIENTED_EDGE('',*,*,#40795,.T.) ;
#55283 = ORIENTED_EDGE('',*,*,#40794,.F.) ;
#55284 = ORIENTED_EDGE('',*,*,#40796,.T.) ;
#55285 = ORIENTED_EDGE('',*,*,#40797,.T.) ;
#55286 = ORIENTED_EDGE('',*,*,#40798,.T.) ;
#55287 = ORIENTED_EDGE('',*,*,#40797,.F.) ;
#55288 = ORIENTED_EDGE('',*,*,#40799,.T.) ;
#55289 = ORIENTED_EDGE('',*,*,#40800,.T.) ;
#55290 = ORIENTED_EDGE('',*,*,#40801,.T.) ;
#55291 = ORIENTED_EDGE('',*,*,#40800,.F.) ;
#55292 = ORIENTED_EDGE('',*,*,#40802,.T.) ;
#55293 = ORIENTED_EDGE('',*,*,#40803,.T.) ;
#55294 = ORIENTED_EDGE('',*,*,#40804,.T.) ;
#55295 = ORIENTED_EDGE('',*,*,#40803,.F.) ;
#55296 = ORIENTED_EDGE('',*,*,#40805,.T.) ;
#55297 = ORIENTED_EDGE('',*,*,#40806,.T.) ;
#55298 = ORIENTED_EDGE('',*,*,#40807,.T.) ;
#55299 = ORIENTED_EDGE('',*,*,#40806,.F.) ;
#55300 = ORIENTED_EDGE('',*,*,#40808,.T.) ;
#55301 = ORIENTED_EDGE('',*,*,#40809,.T.) ;
#55302 = ORIENTED_EDGE('',*,*,#40810,.T.) ;
#55303 = ORIENTED_EDGE('',*,*,#40809,.F.) ;
#55304 = ORIENTED_EDGE('',*,*,#40811,.T.) ;
#55305 = ORIENTED_EDGE('',*,*,#40812,.T.) ;
#55306 = ORIENTED_EDGE('',*,*,#40813,.T.) ;
#55307 = ORIENTED_EDGE('',*,*,#40812,.F.) ;
#55308 = ORIENTED_EDGE('',*,*,#40814,.T.) ;
#55309 = ORIENTED_EDGE('',*,*,#40815,.T.) ;
#55310 = ORIENTED_EDGE('',*,*,#40816,.T.) ;
#55311 = ORIENTED_EDGE('',*,*,#40815,.F.) ;
#55312 = ORIENTED_EDGE('',*,*,#40817,.T.) ;
#55313 = ORIENTED_EDGE('',*,*,#40818,.T.) ;
#55314 = ORIENTED_EDGE('',*,*,#40819,.T.) ;
#55315 = ORIENTED_EDGE('',*,*,#40818,.F.) ;
#55316 = ORIENTED_EDGE('',*,*,#40820,.T.) ;
#55317 = ORIENTED_EDGE('',*,*,#40821,.T.) ;
#55318 = ORIENTED_EDGE('',*,*,#40822,.T.) ;
#55319 = ORIENTED_EDGE('',*,*,#40821,.F.) ;
#55320 = ORIENTED_EDGE('',*,*,#40823,.T.) ;
#55321 = ORIENTED_EDGE('',*,*,#40824,.T.) ;
#55322 = ORIENTED_EDGE('',*,*,#40825,.T.) ;
#55323 = ORIENTED_EDGE('',*,*,#40824,.F.) ;
#55324 = ORIENTED_EDGE('',*,*,#40826,.T.) ;
#55325 = ORIENTED_EDGE('',*,*,#40827,.T.) ;
#55326 = ORIENTED_EDGE('',*,*,#40828,.T.) ;
#55327 = ORIENTED_EDGE('',*,*,#40827,.F.) ;
#55328 = ORIENTED_EDGE('',*,*,#40829,.T.) ;
#55329 = ORIENTED_EDGE('',*,*,#40830,.T.) ;
#55330 = ORIENTED_EDGE('',*,*,#40831,.T.) ;
#55331 = ORIENTED_EDGE('',*,*,#40830,.F.) ;
#55332 = ORIENTED_EDGE('',*,*,#40832,.T.) ;
#55333 = ORIENTED_EDGE('',*,*,#40833,.T.) ;
#55334 = ORIENTED_EDGE('',*,*,#40834,.T.) ;
#55335 = ORIENTED_EDGE('',*,*,#40833,.F.) ;
#55336 = ORIENTED_EDGE('',*,*,#40835,.T.) ;
#55337 = ORIENTED_EDGE('',*,*,#40758,.T.) ;
#55338 = ORIENTED_EDGE('',*,*,#40836,.T.) ;
#55339 = ORIENTED_EDGE('',*,*,#40837,.T.) ;
#55340 = ORIENTED_EDGE('',*,*,#40838,.T.) ;
#55341 = ORIENTED_EDGE('',*,*,#40839,.T.) ;
#55342 = ORIENTED_EDGE('',*,*,#40840,.T.) ;
#55343 = ORIENTED_EDGE('',*,*,#40841,.T.) ;
#55344 = ORIENTED_EDGE('',*,*,#40842,.T.) ;
#55345 = ORIENTED_EDGE('',*,*,#40843,.T.) ;
#55346 = ORIENTED_EDGE('',*,*,#40844,.T.) ;
#55347 = ORIENTED_EDGE('',*,*,#40845,.T.) ;
#55348 = ORIENTED_EDGE('',*,*,#40846,.T.) ;
#55349 = ORIENTED_EDGE('',*,*,#40847,.T.) ;
#55350 = ORIENTED_EDGE('',*,*,#40848,.T.) ;
#55351 = ORIENTED_EDGE('',*,*,#40849,.T.) ;
#55352 = ORIENTED_EDGE('',*,*,#40850,.T.) ;
#55353 = ORIENTED_EDGE('',*,*,#40851,.T.) ;
#55354 = ORIENTED_EDGE('',*,*,#40852,.T.) ;
#55355 = ORIENTED_EDGE('',*,*,#40853,.T.) ;
#55356 = ORIENTED_EDGE('',*,*,#40854,.T.) ;
#55357 = ORIENTED_EDGE('',*,*,#39109,.T.) ;
#55358 = ORIENTED_EDGE('',*,*,#40855,.F.) ;
#55359 = ORIENTED_EDGE('',*,*,#40856,.T.) ;
#55360 = ORIENTED_EDGE('',*,*,#40857,.T.) ;
#55361 = ORIENTED_EDGE('',*,*,#40858,.T.) ;
#55362 = ORIENTED_EDGE('',*,*,#40857,.F.) ;
#55363 = ORIENTED_EDGE('',*,*,#40859,.T.) ;
#55364 = ORIENTED_EDGE('',*,*,#40860,.T.) ;
#55365 = ORIENTED_EDGE('',*,*,#40861,.T.) ;
#55366 = ORIENTED_EDGE('',*,*,#40860,.F.) ;
#55367 = ORIENTED_EDGE('',*,*,#40862,.T.) ;
#55368 = ORIENTED_EDGE('',*,*,#40863,.T.) ;
#55369 = ORIENTED_EDGE('',*,*,#40864,.T.) ;
#55370 = ORIENTED_EDGE('',*,*,#40863,.F.) ;
#55371 = ORIENTED_EDGE('',*,*,#40865,.T.) ;
#55372 = ORIENTED_EDGE('',*,*,#40866,.T.) ;
#55373 = ORIENTED_EDGE('',*,*,#40867,.T.) ;
#55374 = ORIENTED_EDGE('',*,*,#40866,.F.) ;
#55375 = ORIENTED_EDGE('',*,*,#40868,.T.) ;
#55376 = ORIENTED_EDGE('',*,*,#40869,.T.) ;
#55377 = ORIENTED_EDGE('',*,*,#40870,.T.) ;
#55378 = ORIENTED_EDGE('',*,*,#40869,.F.) ;
#55379 = ORIENTED_EDGE('',*,*,#40871,.T.) ;
#55380 = ORIENTED_EDGE('',*,*,#40872,.T.) ;
#55381 = ORIENTED_EDGE('',*,*,#40873,.T.) ;
#55382 = ORIENTED_EDGE('',*,*,#40872,.F.) ;
#55383 = ORIENTED_EDGE('',*,*,#39129,.T.) ;
#55384 = ORIENTED_EDGE('',*,*,#40874,.T.) ;
#55385 = ORIENTED_EDGE('',*,*,#40875,.T.) ;
#55386 = ORIENTED_EDGE('',*,*,#40874,.F.) ;
#55387 = ORIENTED_EDGE('',*,*,#40876,.T.) ;
#55388 = ORIENTED_EDGE('',*,*,#39306,.T.) ;
#55389 = ORIENTED_EDGE('',*,*,#40877,.T.) ;
#55390 = ORIENTED_EDGE('',*,*,#39305,.F.) ;
#55391 = ORIENTED_EDGE('',*,*,#40878,.T.) ;
#55392 = ORIENTED_EDGE('',*,*,#40879,.T.) ;
#55393 = ORIENTED_EDGE('',*,*,#40880,.T.) ;
#55394 = ORIENTED_EDGE('',*,*,#40879,.F.) ;
#55395 = ORIENTED_EDGE('',*,*,#40881,.T.) ;
#55396 = ORIENTED_EDGE('',*,*,#40882,.T.) ;
#55397 = ORIENTED_EDGE('',*,*,#40883,.T.) ;
#55398 = ORIENTED_EDGE('',*,*,#40882,.F.) ;
#55399 = ORIENTED_EDGE('',*,*,#40884,.T.) ;
#55400 = ORIENTED_EDGE('',*,*,#40885,.T.) ;
#55401 = ORIENTED_EDGE('',*,*,#40886,.T.) ;
#55402 = ORIENTED_EDGE('',*,*,#40885,.F.) ;
#55403 = ORIENTED_EDGE('',*,*,#40887,.T.) ;
#55404 = ORIENTED_EDGE('',*,*,#40888,.T.) ;
#55405 = ORIENTED_EDGE('',*,*,#40889,.T.) ;
#55406 = ORIENTED_EDGE('',*,*,#40888,.F.) ;
#55407 = ORIENTED_EDGE('',*,*,#40890,.T.) ;
#55408 = ORIENTED_EDGE('',*,*,#40891,.T.) ;
#55409 = ORIENTED_EDGE('',*,*,#40892,.T.) ;
#55410 = ORIENTED_EDGE('',*,*,#40891,.F.) ;
#55411 = ORIENTED_EDGE('',*,*,#40893,.T.) ;
#55412 = ORIENTED_EDGE('',*,*,#40894,.T.) ;
#55413 = ORIENTED_EDGE('',*,*,#40895,.T.) ;
#55414 = ORIENTED_EDGE('',*,*,#40894,.F.) ;
#55415 = ORIENTED_EDGE('',*,*,#40896,.T.) ;
#55416 = ORIENTED_EDGE('',*,*,#40897,.T.) ;
#55417 = ORIENTED_EDGE('',*,*,#40898,.T.) ;
#55418 = ORIENTED_EDGE('',*,*,#40897,.F.) ;
#55419 = ORIENTED_EDGE('',*,*,#40899,.T.) ;
#55420 = ORIENTED_EDGE('',*,*,#40900,.T.) ;
#55421 = ORIENTED_EDGE('',*,*,#40901,.T.) ;
#55422 = ORIENTED_EDGE('',*,*,#40900,.F.) ;
#55423 = ORIENTED_EDGE('',*,*,#40902,.T.) ;
#55424 = ORIENTED_EDGE('',*,*,#40903,.T.) ;
#55425 = ORIENTED_EDGE('',*,*,#40904,.T.) ;
#55426 = ORIENTED_EDGE('',*,*,#40903,.F.) ;
#55427 = ORIENTED_EDGE('',*,*,#40905,.T.) ;
#55428 = ORIENTED_EDGE('',*,*,#40906,.T.) ;
#55429 = ORIENTED_EDGE('',*,*,#40907,.T.) ;
#55430 = ORIENTED_EDGE('',*,*,#40906,.F.) ;
#55431 = ORIENTED_EDGE('',*,*,#40908,.T.) ;
#55432 = ORIENTED_EDGE('',*,*,#40909,.T.) ;
#55433 = ORIENTED_EDGE('',*,*,#40910,.T.) ;
#55434 = ORIENTED_EDGE('',*,*,#40909,.F.) ;
#55435 = ORIENTED_EDGE('',*,*,#40911,.T.) ;
#55436 = ORIENTED_EDGE('',*,*,#40912,.T.) ;
#55437 = ORIENTED_EDGE('',*,*,#40913,.T.) ;
#55438 = ORIENTED_EDGE('',*,*,#40912,.F.) ;
#55439 = ORIENTED_EDGE('',*,*,#40914,.T.) ;
#55440 = ORIENTED_EDGE('',*,*,#40915,.T.) ;
#55441 = ORIENTED_EDGE('',*,*,#40916,.T.) ;
#55442 = ORIENTED_EDGE('',*,*,#40915,.F.) ;
#55443 = ORIENTED_EDGE('',*,*,#40917,.T.) ;
#55444 = ORIENTED_EDGE('',*,*,#40918,.T.) ;
#55445 = ORIENTED_EDGE('',*,*,#40919,.T.) ;
#55446 = ORIENTED_EDGE('',*,*,#40918,.F.) ;
#55447 = ORIENTED_EDGE('',*,*,#40920,.T.) ;
#55448 = ORIENTED_EDGE('',*,*,#40921,.T.) ;
#55449 = ORIENTED_EDGE('',*,*,#40922,.T.) ;
#55450 = ORIENTED_EDGE('',*,*,#40921,.F.) ;
#55451 = ORIENTED_EDGE('',*,*,#40923,.T.) ;
#55452 = ORIENTED_EDGE('',*,*,#40924,.T.) ;
#55453 = ORIENTED_EDGE('',*,*,#40925,.T.) ;
#55454 = ORIENTED_EDGE('',*,*,#40924,.F.) ;
#55455 = ORIENTED_EDGE('',*,*,#40926,.T.) ;
#55456 = ORIENTED_EDGE('',*,*,#40927,.T.) ;
#55457 = ORIENTED_EDGE('',*,*,#40928,.T.) ;
#55458 = ORIENTED_EDGE('',*,*,#40927,.F.) ;
#55459 = ORIENTED_EDGE('',*,*,#40929,.T.) ;
#55460 = ORIENTED_EDGE('',*,*,#40930,.T.) ;
#55461 = ORIENTED_EDGE('',*,*,#40931,.T.) ;
#55462 = ORIENTED_EDGE('',*,*,#40930,.F.) ;
#55463 = ORIENTED_EDGE('',*,*,#40932,.T.) ;
#55464 = ORIENTED_EDGE('',*,*,#40855,.T.) ;
#55465 = ORIENTED_EDGE('',*,*,#40933,.T.) ;
#55466 = ORIENTED_EDGE('',*,*,#40934,.T.) ;
#55467 = ORIENTED_EDGE('',*,*,#40935,.T.) ;
#55468 = ORIENTED_EDGE('',*,*,#40936,.T.) ;
#55469 = ORIENTED_EDGE('',*,*,#40937,.T.) ;
#55470 = ORIENTED_EDGE('',*,*,#40938,.T.) ;
#55471 = ORIENTED_EDGE('',*,*,#40939,.T.) ;
#55472 = ORIENTED_EDGE('',*,*,#40940,.T.) ;
#55473 = ORIENTED_EDGE('',*,*,#40941,.T.) ;
#55474 = ORIENTED_EDGE('',*,*,#40942,.T.) ;
#55475 = ORIENTED_EDGE('',*,*,#40943,.T.) ;
#55476 = ORIENTED_EDGE('',*,*,#40944,.T.) ;
#55477 = ORIENTED_EDGE('',*,*,#40945,.T.) ;
#55478 = ORIENTED_EDGE('',*,*,#40946,.T.) ;
#55479 = ORIENTED_EDGE('',*,*,#40947,.T.) ;
#55480 = ORIENTED_EDGE('',*,*,#40948,.T.) ;
#55481 = ORIENTED_EDGE('',*,*,#40949,.T.) ;
#55482 = ORIENTED_EDGE('',*,*,#40950,.T.) ;
#55483 = ORIENTED_EDGE('',*,*,#40951,.T.) ;
#55484 = ORIENTED_EDGE('',*,*,#39126,.T.) ;
#55485 = ORIENTED_EDGE('',*,*,#40952,.F.) ;
#55486 = ORIENTED_EDGE('',*,*,#40953,.T.) ;
#55487 = ORIENTED_EDGE('',*,*,#40954,.T.) ;
#55488 = ORIENTED_EDGE('',*,*,#40955,.T.) ;
#55489 = ORIENTED_EDGE('',*,*,#40954,.F.) ;
#55490 = ORIENTED_EDGE('',*,*,#40956,.T.) ;
#55491 = ORIENTED_EDGE('',*,*,#40957,.T.) ;
#55492 = ORIENTED_EDGE('',*,*,#40958,.T.) ;
#55493 = ORIENTED_EDGE('',*,*,#40957,.F.) ;
#55494 = ORIENTED_EDGE('',*,*,#40959,.T.) ;
#55495 = ORIENTED_EDGE('',*,*,#40960,.T.) ;
#55496 = ORIENTED_EDGE('',*,*,#40961,.T.) ;
#55497 = ORIENTED_EDGE('',*,*,#40960,.F.) ;
#55498 = ORIENTED_EDGE('',*,*,#40962,.T.) ;
#55499 = ORIENTED_EDGE('',*,*,#40963,.T.) ;
#55500 = ORIENTED_EDGE('',*,*,#40964,.T.) ;
#55501 = ORIENTED_EDGE('',*,*,#40963,.F.) ;
#55502 = ORIENTED_EDGE('',*,*,#40965,.T.) ;
#55503 = ORIENTED_EDGE('',*,*,#40966,.T.) ;
#55504 = ORIENTED_EDGE('',*,*,#40967,.T.) ;
#55505 = ORIENTED_EDGE('',*,*,#40966,.F.) ;
#55506 = ORIENTED_EDGE('',*,*,#40968,.T.) ;
#55507 = ORIENTED_EDGE('',*,*,#40969,.T.) ;
#55508 = ORIENTED_EDGE('',*,*,#40970,.T.) ;
#55509 = ORIENTED_EDGE('',*,*,#40969,.F.) ;
#55510 = ORIENTED_EDGE('',*,*,#39146,.T.) ;
#55511 = ORIENTED_EDGE('',*,*,#40971,.T.) ;
#55512 = ORIENTED_EDGE('',*,*,#40972,.T.) ;
#55513 = ORIENTED_EDGE('',*,*,#40971,.F.) ;
#55514 = ORIENTED_EDGE('',*,*,#40973,.T.) ;
#55515 = ORIENTED_EDGE('',*,*,#39303,.T.) ;
#55516 = ORIENTED_EDGE('',*,*,#40974,.T.) ;
#55517 = ORIENTED_EDGE('',*,*,#39302,.F.) ;
#55518 = ORIENTED_EDGE('',*,*,#40975,.T.) ;
#55519 = ORIENTED_EDGE('',*,*,#40976,.T.) ;
#55520 = ORIENTED_EDGE('',*,*,#40977,.T.) ;
#55521 = ORIENTED_EDGE('',*,*,#40976,.F.) ;
#55522 = ORIENTED_EDGE('',*,*,#40978,.T.) ;
#55523 = ORIENTED_EDGE('',*,*,#40979,.T.) ;
#55524 = ORIENTED_EDGE('',*,*,#40980,.T.) ;
#55525 = ORIENTED_EDGE('',*,*,#40979,.F.) ;
#55526 = ORIENTED_EDGE('',*,*,#40981,.T.) ;
#55527 = ORIENTED_EDGE('',*,*,#40982,.T.) ;
#55528 = ORIENTED_EDGE('',*,*,#40983,.T.) ;
#55529 = ORIENTED_EDGE('',*,*,#40982,.F.) ;
#55530 = ORIENTED_EDGE('',*,*,#40984,.T.) ;
#55531 = ORIENTED_EDGE('',*,*,#40985,.T.) ;
#55532 = ORIENTED_EDGE('',*,*,#40986,.T.) ;
#55533 = ORIENTED_EDGE('',*,*,#40985,.F.) ;
#55534 = ORIENTED_EDGE('',*,*,#40987,.T.) ;
#55535 = ORIENTED_EDGE('',*,*,#40988,.T.) ;
#55536 = ORIENTED_EDGE('',*,*,#40989,.T.) ;
#55537 = ORIENTED_EDGE('',*,*,#40988,.F.) ;
#55538 = ORIENTED_EDGE('',*,*,#40990,.T.) ;
#55539 = ORIENTED_EDGE('',*,*,#40991,.T.) ;
#55540 = ORIENTED_EDGE('',*,*,#40992,.T.) ;
#55541 = ORIENTED_EDGE('',*,*,#40991,.F.) ;
#55542 = ORIENTED_EDGE('',*,*,#40993,.T.) ;
#55543 = ORIENTED_EDGE('',*,*,#40994,.T.) ;
#55544 = ORIENTED_EDGE('',*,*,#40995,.T.) ;
#55545 = ORIENTED_EDGE('',*,*,#40994,.F.) ;
#55546 = ORIENTED_EDGE('',*,*,#40996,.T.) ;
#55547 = ORIENTED_EDGE('',*,*,#40997,.T.) ;
#55548 = ORIENTED_EDGE('',*,*,#40998,.T.) ;
#55549 = ORIENTED_EDGE('',*,*,#40997,.F.) ;
#55550 = ORIENTED_EDGE('',*,*,#40999,.T.) ;
#55551 = ORIENTED_EDGE('',*,*,#41000,.T.) ;
#55552 = ORIENTED_EDGE('',*,*,#41001,.T.) ;
#55553 = ORIENTED_EDGE('',*,*,#41000,.F.) ;
#55554 = ORIENTED_EDGE('',*,*,#41002,.T.) ;
#55555 = ORIENTED_EDGE('',*,*,#41003,.T.) ;
#55556 = ORIENTED_EDGE('',*,*,#41004,.T.) ;
#55557 = ORIENTED_EDGE('',*,*,#41003,.F.) ;
#55558 = ORIENTED_EDGE('',*,*,#41005,.T.) ;
#55559 = ORIENTED_EDGE('',*,*,#41006,.T.) ;
#55560 = ORIENTED_EDGE('',*,*,#41007,.T.) ;
#55561 = ORIENTED_EDGE('',*,*,#41006,.F.) ;
#55562 = ORIENTED_EDGE('',*,*,#41008,.T.) ;
#55563 = ORIENTED_EDGE('',*,*,#41009,.T.) ;
#55564 = ORIENTED_EDGE('',*,*,#41010,.T.) ;
#55565 = ORIENTED_EDGE('',*,*,#41009,.F.) ;
#55566 = ORIENTED_EDGE('',*,*,#41011,.T.) ;
#55567 = ORIENTED_EDGE('',*,*,#41012,.T.) ;
#55568 = ORIENTED_EDGE('',*,*,#41013,.T.) ;
#55569 = ORIENTED_EDGE('',*,*,#41012,.F.) ;
#55570 = ORIENTED_EDGE('',*,*,#41014,.T.) ;
#55571 = ORIENTED_EDGE('',*,*,#41015,.T.) ;
#55572 = ORIENTED_EDGE('',*,*,#41016,.T.) ;
#55573 = ORIENTED_EDGE('',*,*,#41015,.F.) ;
#55574 = ORIENTED_EDGE('',*,*,#41017,.T.) ;
#55575 = ORIENTED_EDGE('',*,*,#41018,.T.) ;
#55576 = ORIENTED_EDGE('',*,*,#41019,.T.) ;
#55577 = ORIENTED_EDGE('',*,*,#41018,.F.) ;
#55578 = ORIENTED_EDGE('',*,*,#41020,.T.) ;
#55579 = ORIENTED_EDGE('',*,*,#41021,.T.) ;
#55580 = ORIENTED_EDGE('',*,*,#41022,.T.) ;
#55581 = ORIENTED_EDGE('',*,*,#41021,.F.) ;
#55582 = ORIENTED_EDGE('',*,*,#41023,.T.) ;
#55583 = ORIENTED_EDGE('',*,*,#41024,.T.) ;
#55584 = ORIENTED_EDGE('',*,*,#41025,.T.) ;
#55585 = ORIENTED_EDGE('',*,*,#41024,.F.) ;
#55586 = ORIENTED_EDGE('',*,*,#41026,.T.) ;
#55587 = ORIENTED_EDGE('',*,*,#41027,.T.) ;
#55588 = ORIENTED_EDGE('',*,*,#41028,.T.) ;
#55589 = ORIENTED_EDGE('',*,*,#41027,.F.) ;
#55590 = ORIENTED_EDGE('',*,*,#41029,.T.) ;
#55591 = ORIENTED_EDGE('',*,*,#40952,.T.) ;
#55592 = ORIENTED_EDGE('',*,*,#41030,.T.) ;
#55593 = ORIENTED_EDGE('',*,*,#41031,.T.) ;
#55594 = ORIENTED_EDGE('',*,*,#41032,.T.) ;
#55595 = ORIENTED_EDGE('',*,*,#41033,.T.) ;
#55596 = ORIENTED_EDGE('',*,*,#41034,.T.) ;
#55597 = ORIENTED_EDGE('',*,*,#41035,.T.) ;
#55598 = ORIENTED_EDGE('',*,*,#41036,.T.) ;
#55599 = ORIENTED_EDGE('',*,*,#41037,.T.) ;
#55600 = ORIENTED_EDGE('',*,*,#41038,.T.) ;
#55601 = ORIENTED_EDGE('',*,*,#41039,.T.) ;
#55602 = ORIENTED_EDGE('',*,*,#41040,.T.) ;
#55603 = ORIENTED_EDGE('',*,*,#41041,.T.) ;
#55604 = ORIENTED_EDGE('',*,*,#41042,.T.) ;
#55605 = ORIENTED_EDGE('',*,*,#41043,.T.) ;
#55606 = ORIENTED_EDGE('',*,*,#41044,.T.) ;
#55607 = ORIENTED_EDGE('',*,*,#41045,.T.) ;
#55608 = ORIENTED_EDGE('',*,*,#41046,.T.) ;
#55609 = ORIENTED_EDGE('',*,*,#41047,.T.) ;
#55610 = ORIENTED_EDGE('',*,*,#41048,.T.) ;
#55611 = ORIENTED_EDGE('',*,*,#39143,.T.) ;
#55612 = ORIENTED_EDGE('',*,*,#41049,.F.) ;
#55613 = ORIENTED_EDGE('',*,*,#41050,.T.) ;
#55614 = ORIENTED_EDGE('',*,*,#41051,.T.) ;
#55615 = ORIENTED_EDGE('',*,*,#41052,.T.) ;
#55616 = ORIENTED_EDGE('',*,*,#41051,.F.) ;
#55617 = ORIENTED_EDGE('',*,*,#41053,.T.) ;
#55618 = ORIENTED_EDGE('',*,*,#41054,.T.) ;
#55619 = ORIENTED_EDGE('',*,*,#41055,.T.) ;
#55620 = ORIENTED_EDGE('',*,*,#41054,.F.) ;
#55621 = ORIENTED_EDGE('',*,*,#41056,.T.) ;
#55622 = ORIENTED_EDGE('',*,*,#41057,.T.) ;
#55623 = ORIENTED_EDGE('',*,*,#41058,.T.) ;
#55624 = ORIENTED_EDGE('',*,*,#41057,.F.) ;
#55625 = ORIENTED_EDGE('',*,*,#41059,.T.) ;
#55626 = ORIENTED_EDGE('',*,*,#41060,.T.) ;
#55627 = ORIENTED_EDGE('',*,*,#41061,.T.) ;
#55628 = ORIENTED_EDGE('',*,*,#41060,.F.) ;
#55629 = ORIENTED_EDGE('',*,*,#41062,.T.) ;
#55630 = ORIENTED_EDGE('',*,*,#41063,.T.) ;
#55631 = ORIENTED_EDGE('',*,*,#41064,.T.) ;
#55632 = ORIENTED_EDGE('',*,*,#41063,.F.) ;
#55633 = ORIENTED_EDGE('',*,*,#41065,.T.) ;
#55634 = ORIENTED_EDGE('',*,*,#41066,.T.) ;
#55635 = ORIENTED_EDGE('',*,*,#41067,.T.) ;
#55636 = ORIENTED_EDGE('',*,*,#41066,.F.) ;
#55637 = ORIENTED_EDGE('',*,*,#39163,.T.) ;
#55638 = ORIENTED_EDGE('',*,*,#41068,.T.) ;
#55639 = ORIENTED_EDGE('',*,*,#41069,.T.) ;
#55640 = ORIENTED_EDGE('',*,*,#41068,.F.) ;
#55641 = ORIENTED_EDGE('',*,*,#41070,.T.) ;
#55642 = ORIENTED_EDGE('',*,*,#39300,.T.) ;
#55643 = ORIENTED_EDGE('',*,*,#41071,.T.) ;
#55644 = ORIENTED_EDGE('',*,*,#39299,.F.) ;
#55645 = ORIENTED_EDGE('',*,*,#41072,.T.) ;
#55646 = ORIENTED_EDGE('',*,*,#41073,.T.) ;
#55647 = ORIENTED_EDGE('',*,*,#41074,.T.) ;
#55648 = ORIENTED_EDGE('',*,*,#41073,.F.) ;
#55649 = ORIENTED_EDGE('',*,*,#41075,.T.) ;
#55650 = ORIENTED_EDGE('',*,*,#41076,.T.) ;
#55651 = ORIENTED_EDGE('',*,*,#41077,.T.) ;
#55652 = ORIENTED_EDGE('',*,*,#41076,.F.) ;
#55653 = ORIENTED_EDGE('',*,*,#41078,.T.) ;
#55654 = ORIENTED_EDGE('',*,*,#41079,.T.) ;
#55655 = ORIENTED_EDGE('',*,*,#41080,.T.) ;
#55656 = ORIENTED_EDGE('',*,*,#41079,.F.) ;
#55657 = ORIENTED_EDGE('',*,*,#41081,.T.) ;
#55658 = ORIENTED_EDGE('',*,*,#41082,.T.) ;
#55659 = ORIENTED_EDGE('',*,*,#41083,.T.) ;
#55660 = ORIENTED_EDGE('',*,*,#41082,.F.) ;
#55661 = ORIENTED_EDGE('',*,*,#41084,.T.) ;
#55662 = ORIENTED_EDGE('',*,*,#41085,.T.) ;
#55663 = ORIENTED_EDGE('',*,*,#41086,.T.) ;
#55664 = ORIENTED_EDGE('',*,*,#41085,.F.) ;
#55665 = ORIENTED_EDGE('',*,*,#41087,.T.) ;
#55666 = ORIENTED_EDGE('',*,*,#41088,.T.) ;
#55667 = ORIENTED_EDGE('',*,*,#41089,.T.) ;
#55668 = ORIENTED_EDGE('',*,*,#41088,.F.) ;
#55669 = ORIENTED_EDGE('',*,*,#41090,.T.) ;
#55670 = ORIENTED_EDGE('',*,*,#41091,.T.) ;
#55671 = ORIENTED_EDGE('',*,*,#41092,.T.) ;
#55672 = ORIENTED_EDGE('',*,*,#41091,.F.) ;
#55673 = ORIENTED_EDGE('',*,*,#41093,.T.) ;
#55674 = ORIENTED_EDGE('',*,*,#41094,.T.) ;
#55675 = ORIENTED_EDGE('',*,*,#41095,.T.) ;
#55676 = ORIENTED_EDGE('',*,*,#41094,.F.) ;
#55677 = ORIENTED_EDGE('',*,*,#41096,.T.) ;
#55678 = ORIENTED_EDGE('',*,*,#41097,.T.) ;
#55679 = ORIENTED_EDGE('',*,*,#41098,.T.) ;
#55680 = ORIENTED_EDGE('',*,*,#41097,.F.) ;
#55681 = ORIENTED_EDGE('',*,*,#41099,.T.) ;
#55682 = ORIENTED_EDGE('',*,*,#41100,.T.) ;
#55683 = ORIENTED_EDGE('',*,*,#41101,.T.) ;
#55684 = ORIENTED_EDGE('',*,*,#41100,.F.) ;
#55685 = ORIENTED_EDGE('',*,*,#41102,.T.) ;
#55686 = ORIENTED_EDGE('',*,*,#41103,.T.) ;
#55687 = ORIENTED_EDGE('',*,*,#41104,.T.) ;
#55688 = ORIENTED_EDGE('',*,*,#41103,.F.) ;
#55689 = ORIENTED_EDGE('',*,*,#41105,.T.) ;
#55690 = ORIENTED_EDGE('',*,*,#41106,.T.) ;
#55691 = ORIENTED_EDGE('',*,*,#41107,.T.) ;
#55692 = ORIENTED_EDGE('',*,*,#41106,.F.) ;
#55693 = ORIENTED_EDGE('',*,*,#41108,.T.) ;
#55694 = ORIENTED_EDGE('',*,*,#41109,.T.) ;
#55695 = ORIENTED_EDGE('',*,*,#41110,.T.) ;
#55696 = ORIENTED_EDGE('',*,*,#41109,.F.) ;
#55697 = ORIENTED_EDGE('',*,*,#41111,.T.) ;
#55698 = ORIENTED_EDGE('',*,*,#41112,.T.) ;
#55699 = ORIENTED_EDGE('',*,*,#41113,.T.) ;
#55700 = ORIENTED_EDGE('',*,*,#41112,.F.) ;
#55701 = ORIENTED_EDGE('',*,*,#41114,.T.) ;
#55702 = ORIENTED_EDGE('',*,*,#41115,.T.) ;
#55703 = ORIENTED_EDGE('',*,*,#41116,.T.) ;
#55704 = ORIENTED_EDGE('',*,*,#41115,.F.) ;
#55705 = ORIENTED_EDGE('',*,*,#41117,.T.) ;
#55706 = ORIENTED_EDGE('',*,*,#41118,.T.) ;
#55707 = ORIENTED_EDGE('',*,*,#41119,.T.) ;
#55708 = ORIENTED_EDGE('',*,*,#41118,.F.) ;
#55709 = ORIENTED_EDGE('',*,*,#41120,.T.) ;
#55710 = ORIENTED_EDGE('',*,*,#41121,.T.) ;
#55711 = ORIENTED_EDGE('',*,*,#41122,.T.) ;
#55712 = ORIENTED_EDGE('',*,*,#41121,.F.) ;
#55713 = ORIENTED_EDGE('',*,*,#41123,.T.) ;
#55714 = ORIENTED_EDGE('',*,*,#41124,.T.) ;
#55715 = ORIENTED_EDGE('',*,*,#41125,.T.) ;
#55716 = ORIENTED_EDGE('',*,*,#41124,.F.) ;
#55717 = ORIENTED_EDGE('',*,*,#41126,.T.) ;
#55718 = ORIENTED_EDGE('',*,*,#41049,.T.) ;
#55719 = ORIENTED_EDGE('',*,*,#41127,.T.) ;
#55720 = ORIENTED_EDGE('',*,*,#41128,.T.) ;
#55721 = ORIENTED_EDGE('',*,*,#41129,.T.) ;
#55722 = ORIENTED_EDGE('',*,*,#41130,.T.) ;
#55723 = ORIENTED_EDGE('',*,*,#41131,.T.) ;
#55724 = ORIENTED_EDGE('',*,*,#41132,.T.) ;
#55725 = ORIENTED_EDGE('',*,*,#41133,.T.) ;
#55726 = ORIENTED_EDGE('',*,*,#41134,.T.) ;
#55727 = ORIENTED_EDGE('',*,*,#41135,.T.) ;
#55728 = ORIENTED_EDGE('',*,*,#41136,.T.) ;
#55729 = ORIENTED_EDGE('',*,*,#41137,.T.) ;
#55730 = ORIENTED_EDGE('',*,*,#41138,.T.) ;
#55731 = ORIENTED_EDGE('',*,*,#41139,.T.) ;
#55732 = ORIENTED_EDGE('',*,*,#41140,.T.) ;
#55733 = ORIENTED_EDGE('',*,*,#41141,.T.) ;
#55734 = ORIENTED_EDGE('',*,*,#41142,.T.) ;
#55735 = ORIENTED_EDGE('',*,*,#41143,.T.) ;
#55736 = ORIENTED_EDGE('',*,*,#41144,.T.) ;
#55737 = ORIENTED_EDGE('',*,*,#41145,.T.) ;
#55738 = ORIENTED_EDGE('',*,*,#39160,.T.) ;
#55739 = ORIENTED_EDGE('',*,*,#41146,.F.) ;
#55740 = ORIENTED_EDGE('',*,*,#41147,.T.) ;
#55741 = ORIENTED_EDGE('',*,*,#41148,.T.) ;
#55742 = ORIENTED_EDGE('',*,*,#41149,.T.) ;
#55743 = ORIENTED_EDGE('',*,*,#41148,.F.) ;
#55744 = ORIENTED_EDGE('',*,*,#41150,.T.) ;
#55745 = ORIENTED_EDGE('',*,*,#41151,.T.) ;
#55746 = ORIENTED_EDGE('',*,*,#41152,.T.) ;
#55747 = ORIENTED_EDGE('',*,*,#41151,.F.) ;
#55748 = ORIENTED_EDGE('',*,*,#41153,.T.) ;
#55749 = ORIENTED_EDGE('',*,*,#41154,.T.) ;
#55750 = ORIENTED_EDGE('',*,*,#41155,.T.) ;
#55751 = ORIENTED_EDGE('',*,*,#41154,.F.) ;
#55752 = ORIENTED_EDGE('',*,*,#41156,.T.) ;
#55753 = ORIENTED_EDGE('',*,*,#41157,.T.) ;
#55754 = ORIENTED_EDGE('',*,*,#41158,.T.) ;
#55755 = ORIENTED_EDGE('',*,*,#41157,.F.) ;
#55756 = ORIENTED_EDGE('',*,*,#41159,.T.) ;
#55757 = ORIENTED_EDGE('',*,*,#41160,.T.) ;
#55758 = ORIENTED_EDGE('',*,*,#41161,.T.) ;
#55759 = ORIENTED_EDGE('',*,*,#41160,.F.) ;
#55760 = ORIENTED_EDGE('',*,*,#41162,.T.) ;
#55761 = ORIENTED_EDGE('',*,*,#41163,.T.) ;
#55762 = ORIENTED_EDGE('',*,*,#41164,.T.) ;
#55763 = ORIENTED_EDGE('',*,*,#41163,.F.) ;
#55764 = ORIENTED_EDGE('',*,*,#39180,.T.) ;
#55765 = ORIENTED_EDGE('',*,*,#41165,.T.) ;
#55766 = ORIENTED_EDGE('',*,*,#41166,.T.) ;
#55767 = ORIENTED_EDGE('',*,*,#41165,.F.) ;
#55768 = ORIENTED_EDGE('',*,*,#41167,.T.) ;
#55769 = ORIENTED_EDGE('',*,*,#39297,.T.) ;
#55770 = ORIENTED_EDGE('',*,*,#41168,.T.) ;
#55771 = ORIENTED_EDGE('',*,*,#39296,.F.) ;
#55772 = ORIENTED_EDGE('',*,*,#41169,.T.) ;
#55773 = ORIENTED_EDGE('',*,*,#41170,.T.) ;
#55774 = ORIENTED_EDGE('',*,*,#41171,.T.) ;
#55775 = ORIENTED_EDGE('',*,*,#41170,.F.) ;
#55776 = ORIENTED_EDGE('',*,*,#41172,.T.) ;
#55777 = ORIENTED_EDGE('',*,*,#41173,.T.) ;
#55778 = ORIENTED_EDGE('',*,*,#41174,.T.) ;
#55779 = ORIENTED_EDGE('',*,*,#41173,.F.) ;
#55780 = ORIENTED_EDGE('',*,*,#41175,.T.) ;
#55781 = ORIENTED_EDGE('',*,*,#41176,.T.) ;
#55782 = ORIENTED_EDGE('',*,*,#41177,.T.) ;
#55783 = ORIENTED_EDGE('',*,*,#41176,.F.) ;
#55784 = ORIENTED_EDGE('',*,*,#41178,.T.) ;
#55785 = ORIENTED_EDGE('',*,*,#41179,.T.) ;
#55786 = ORIENTED_EDGE('',*,*,#41180,.T.) ;
#55787 = ORIENTED_EDGE('',*,*,#41179,.F.) ;
#55788 = ORIENTED_EDGE('',*,*,#41181,.T.) ;
#55789 = ORIENTED_EDGE('',*,*,#41182,.T.) ;
#55790 = ORIENTED_EDGE('',*,*,#41183,.T.) ;
#55791 = ORIENTED_EDGE('',*,*,#41182,.F.) ;
#55792 = ORIENTED_EDGE('',*,*,#41184,.T.) ;
#55793 = ORIENTED_EDGE('',*,*,#41185,.T.) ;
#55794 = ORIENTED_EDGE('',*,*,#41186,.T.) ;
#55795 = ORIENTED_EDGE('',*,*,#41185,.F.) ;
#55796 = ORIENTED_EDGE('',*,*,#41187,.T.) ;
#55797 = ORIENTED_EDGE('',*,*,#41188,.T.) ;
#55798 = ORIENTED_EDGE('',*,*,#41189,.T.) ;
#55799 = ORIENTED_EDGE('',*,*,#41188,.F.) ;
#55800 = ORIENTED_EDGE('',*,*,#41190,.T.) ;
#55801 = ORIENTED_EDGE('',*,*,#41191,.T.) ;
#55802 = ORIENTED_EDGE('',*,*,#41192,.T.) ;
#55803 = ORIENTED_EDGE('',*,*,#41191,.F.) ;
#55804 = ORIENTED_EDGE('',*,*,#41193,.T.) ;
#55805 = ORIENTED_EDGE('',*,*,#41194,.T.) ;
#55806 = ORIENTED_EDGE('',*,*,#41195,.T.) ;
#55807 = ORIENTED_EDGE('',*,*,#41194,.F.) ;
#55808 = ORIENTED_EDGE('',*,*,#41196,.T.) ;
#55809 = ORIENTED_EDGE('',*,*,#41197,.T.) ;
#55810 = ORIENTED_EDGE('',*,*,#41198,.T.) ;
#55811 = ORIENTED_EDGE('',*,*,#41197,.F.) ;
#55812 = ORIENTED_EDGE('',*,*,#41199,.T.) ;
#55813 = ORIENTED_EDGE('',*,*,#41200,.T.) ;
#55814 = ORIENTED_EDGE('',*,*,#41201,.T.) ;
#55815 = ORIENTED_EDGE('',*,*,#41200,.F.) ;
#55816 = ORIENTED_EDGE('',*,*,#41202,.T.) ;
#55817 = ORIENTED_EDGE('',*,*,#41203,.T.) ;
#55818 = ORIENTED_EDGE('',*,*,#41204,.T.) ;
#55819 = ORIENTED_EDGE('',*,*,#41203,.F.) ;
#55820 = ORIENTED_EDGE('',*,*,#41205,.T.) ;
#55821 = ORIENTED_EDGE('',*,*,#41206,.T.) ;
#55822 = ORIENTED_EDGE('',*,*,#41207,.T.) ;
#55823 = ORIENTED_EDGE('',*,*,#41206,.F.) ;
#55824 = ORIENTED_EDGE('',*,*,#41208,.T.) ;
#55825 = ORIENTED_EDGE('',*,*,#41209,.T.) ;
#55826 = ORIENTED_EDGE('',*,*,#41210,.T.) ;
#55827 = ORIENTED_EDGE('',*,*,#41209,.F.) ;
#55828 = ORIENTED_EDGE('',*,*,#41211,.T.) ;
#55829 = ORIENTED_EDGE('',*,*,#41212,.T.) ;
#55830 = ORIENTED_EDGE('',*,*,#41213,.T.) ;
#55831 = ORIENTED_EDGE('',*,*,#41212,.F.) ;
#55832 = ORIENTED_EDGE('',*,*,#41214,.T.) ;
#55833 = ORIENTED_EDGE('',*,*,#41215,.T.) ;
#55834 = ORIENTED_EDGE('',*,*,#41216,.T.) ;
#55835 = ORIENTED_EDGE('',*,*,#41215,.F.) ;
#55836 = ORIENTED_EDGE('',*,*,#41217,.T.) ;
#55837 = ORIENTED_EDGE('',*,*,#41218,.T.) ;
#55838 = ORIENTED_EDGE('',*,*,#41219,.T.) ;
#55839 = ORIENTED_EDGE('',*,*,#41218,.F.) ;
#55840 = ORIENTED_EDGE('',*,*,#41220,.T.) ;
#55841 = ORIENTED_EDGE('',*,*,#41221,.T.) ;
#55842 = ORIENTED_EDGE('',*,*,#41222,.T.) ;
#55843 = ORIENTED_EDGE('',*,*,#41221,.F.) ;
#55844 = ORIENTED_EDGE('',*,*,#41223,.T.) ;
#55845 = ORIENTED_EDGE('',*,*,#41146,.T.) ;
#55846 = ORIENTED_EDGE('',*,*,#41224,.T.) ;
#55847 = ORIENTED_EDGE('',*,*,#41225,.T.) ;
#55848 = ORIENTED_EDGE('',*,*,#41226,.T.) ;
#55849 = ORIENTED_EDGE('',*,*,#41227,.T.) ;
#55850 = ORIENTED_EDGE('',*,*,#41228,.T.) ;
#55851 = ORIENTED_EDGE('',*,*,#41229,.T.) ;
#55852 = ORIENTED_EDGE('',*,*,#41230,.T.) ;
#55853 = ORIENTED_EDGE('',*,*,#41231,.T.) ;
#55854 = ORIENTED_EDGE('',*,*,#41232,.T.) ;
#55855 = ORIENTED_EDGE('',*,*,#41233,.T.) ;
#55856 = ORIENTED_EDGE('',*,*,#41234,.T.) ;
#55857 = ORIENTED_EDGE('',*,*,#41235,.T.) ;
#55858 = ORIENTED_EDGE('',*,*,#41236,.T.) ;
#55859 = ORIENTED_EDGE('',*,*,#41237,.T.) ;
#55860 = ORIENTED_EDGE('',*,*,#41238,.T.) ;
#55861 = ORIENTED_EDGE('',*,*,#41239,.T.) ;
#55862 = ORIENTED_EDGE('',*,*,#41240,.T.) ;
#55863 = ORIENTED_EDGE('',*,*,#41241,.T.) ;
#55864 = ORIENTED_EDGE('',*,*,#41242,.T.) ;
#55865 = ORIENTED_EDGE('',*,*,#39177,.T.) ;
#55866 = ORIENTED_EDGE('',*,*,#41243,.F.) ;
#55867 = ORIENTED_EDGE('',*,*,#41244,.T.) ;
#55868 = ORIENTED_EDGE('',*,*,#41245,.T.) ;
#55869 = ORIENTED_EDGE('',*,*,#41246,.T.) ;
#55870 = ORIENTED_EDGE('',*,*,#41245,.F.) ;
#55871 = ORIENTED_EDGE('',*,*,#41247,.T.) ;
#55872 = ORIENTED_EDGE('',*,*,#41248,.T.) ;
#55873 = ORIENTED_EDGE('',*,*,#41249,.T.) ;
#55874 = ORIENTED_EDGE('',*,*,#41248,.F.) ;
#55875 = ORIENTED_EDGE('',*,*,#41250,.T.) ;
#55876 = ORIENTED_EDGE('',*,*,#41251,.T.) ;
#55877 = ORIENTED_EDGE('',*,*,#41252,.T.) ;
#55878 = ORIENTED_EDGE('',*,*,#41251,.F.) ;
#55879 = ORIENTED_EDGE('',*,*,#41253,.T.) ;
#55880 = ORIENTED_EDGE('',*,*,#41254,.T.) ;
#55881 = ORIENTED_EDGE('',*,*,#41255,.T.) ;
#55882 = ORIENTED_EDGE('',*,*,#41254,.F.) ;
#55883 = ORIENTED_EDGE('',*,*,#41256,.T.) ;
#55884 = ORIENTED_EDGE('',*,*,#41257,.T.) ;
#55885 = ORIENTED_EDGE('',*,*,#41258,.T.) ;
#55886 = ORIENTED_EDGE('',*,*,#41257,.F.) ;
#55887 = ORIENTED_EDGE('',*,*,#41259,.T.) ;
#55888 = ORIENTED_EDGE('',*,*,#41260,.T.) ;
#55889 = ORIENTED_EDGE('',*,*,#41261,.T.) ;
#55890 = ORIENTED_EDGE('',*,*,#41260,.F.) ;
#55891 = ORIENTED_EDGE('',*,*,#39197,.T.) ;
#55892 = ORIENTED_EDGE('',*,*,#41262,.T.) ;
#55893 = ORIENTED_EDGE('',*,*,#41263,.T.) ;
#55894 = ORIENTED_EDGE('',*,*,#41262,.F.) ;
#55895 = ORIENTED_EDGE('',*,*,#41264,.T.) ;
#55896 = ORIENTED_EDGE('',*,*,#39294,.T.) ;
#55897 = ORIENTED_EDGE('',*,*,#41265,.T.) ;
#55898 = ORIENTED_EDGE('',*,*,#39293,.F.) ;
#55899 = ORIENTED_EDGE('',*,*,#41266,.T.) ;
#55900 = ORIENTED_EDGE('',*,*,#41267,.T.) ;
#55901 = ORIENTED_EDGE('',*,*,#41268,.T.) ;
#55902 = ORIENTED_EDGE('',*,*,#41267,.F.) ;
#55903 = ORIENTED_EDGE('',*,*,#41269,.T.) ;
#55904 = ORIENTED_EDGE('',*,*,#41270,.T.) ;
#55905 = ORIENTED_EDGE('',*,*,#41271,.T.) ;
#55906 = ORIENTED_EDGE('',*,*,#41270,.F.) ;
#55907 = ORIENTED_EDGE('',*,*,#41272,.T.) ;
#55908 = ORIENTED_EDGE('',*,*,#41273,.T.) ;
#55909 = ORIENTED_EDGE('',*,*,#41274,.T.) ;
#55910 = ORIENTED_EDGE('',*,*,#41273,.F.) ;
#55911 = ORIENTED_EDGE('',*,*,#41275,.T.) ;
#55912 = ORIENTED_EDGE('',*,*,#41276,.T.) ;
#55913 = ORIENTED_EDGE('',*,*,#41277,.T.) ;
#55914 = ORIENTED_EDGE('',*,*,#41276,.F.) ;
#55915 = ORIENTED_EDGE('',*,*,#41278,.T.) ;
#55916 = ORIENTED_EDGE('',*,*,#41279,.T.) ;
#55917 = ORIENTED_EDGE('',*,*,#41280,.T.) ;
#55918 = ORIENTED_EDGE('',*,*,#41279,.F.) ;
#55919 = ORIENTED_EDGE('',*,*,#41281,.T.) ;
#55920 = ORIENTED_EDGE('',*,*,#41282,.T.) ;
#55921 = ORIENTED_EDGE('',*,*,#41283,.T.) ;
#55922 = ORIENTED_EDGE('',*,*,#41282,.F.) ;
#55923 = ORIENTED_EDGE('',*,*,#41284,.T.) ;
#55924 = ORIENTED_EDGE('',*,*,#41285,.T.) ;
#55925 = ORIENTED_EDGE('',*,*,#41286,.T.) ;
#55926 = ORIENTED_EDGE('',*,*,#41285,.F.) ;
#55927 = ORIENTED_EDGE('',*,*,#41287,.T.) ;
#55928 = ORIENTED_EDGE('',*,*,#41288,.T.) ;
#55929 = ORIENTED_EDGE('',*,*,#41289,.T.) ;
#55930 = ORIENTED_EDGE('',*,*,#41288,.F.) ;
#55931 = ORIENTED_EDGE('',*,*,#41290,.T.) ;
#55932 = ORIENTED_EDGE('',*,*,#41291,.T.) ;
#55933 = ORIENTED_EDGE('',*,*,#41292,.T.) ;
#55934 = ORIENTED_EDGE('',*,*,#41291,.F.) ;
#55935 = ORIENTED_EDGE('',*,*,#41293,.T.) ;
#55936 = ORIENTED_EDGE('',*,*,#41294,.T.) ;
#55937 = ORIENTED_EDGE('',*,*,#41295,.T.) ;
#55938 = ORIENTED_EDGE('',*,*,#41294,.F.) ;
#55939 = ORIENTED_EDGE('',*,*,#41296,.T.) ;
#55940 = ORIENTED_EDGE('',*,*,#41297,.T.) ;
#55941 = ORIENTED_EDGE('',*,*,#41298,.T.) ;
#55942 = ORIENTED_EDGE('',*,*,#41297,.F.) ;
#55943 = ORIENTED_EDGE('',*,*,#41299,.T.) ;
#55944 = ORIENTED_EDGE('',*,*,#41300,.T.) ;
#55945 = ORIENTED_EDGE('',*,*,#41301,.T.) ;
#55946 = ORIENTED_EDGE('',*,*,#41300,.F.) ;
#55947 = ORIENTED_EDGE('',*,*,#41302,.T.) ;
#55948 = ORIENTED_EDGE('',*,*,#41303,.T.) ;
#55949 = ORIENTED_EDGE('',*,*,#41304,.T.) ;
#55950 = ORIENTED_EDGE('',*,*,#41303,.F.) ;
#55951 = ORIENTED_EDGE('',*,*,#41305,.T.) ;
#55952 = ORIENTED_EDGE('',*,*,#41306,.T.) ;
#55953 = ORIENTED_EDGE('',*,*,#41307,.T.) ;
#55954 = ORIENTED_EDGE('',*,*,#41306,.F.) ;
#55955 = ORIENTED_EDGE('',*,*,#41308,.T.) ;
#55956 = ORIENTED_EDGE('',*,*,#41309,.T.) ;
#55957 = ORIENTED_EDGE('',*,*,#41310,.T.) ;
#55958 = ORIENTED_EDGE('',*,*,#41309,.F.) ;
#55959 = ORIENTED_EDGE('',*,*,#41311,.T.) ;
#55960 = ORIENTED_EDGE('',*,*,#41312,.T.) ;
#55961 = ORIENTED_EDGE('',*,*,#41313,.T.) ;
#55962 = ORIENTED_EDGE('',*,*,#41312,.F.) ;
#55963 = ORIENTED_EDGE('',*,*,#41314,.T.) ;
#55964 = ORIENTED_EDGE('',*,*,#41315,.T.) ;
#55965 = ORIENTED_EDGE('',*,*,#41316,.T.) ;
#55966 = ORIENTED_EDGE('',*,*,#41315,.F.) ;
#55967 = ORIENTED_EDGE('',*,*,#41317,.T.) ;
#55968 = ORIENTED_EDGE('',*,*,#41318,.T.) ;
#55969 = ORIENTED_EDGE('',*,*,#41319,.T.) ;
#55970 = ORIENTED_EDGE('',*,*,#41318,.F.) ;
#55971 = ORIENTED_EDGE('',*,*,#41320,.T.) ;
#55972 = ORIENTED_EDGE('',*,*,#41243,.T.) ;
#55973 = ORIENTED_EDGE('',*,*,#41321,.T.) ;
#55974 = ORIENTED_EDGE('',*,*,#41322,.T.) ;
#55975 = ORIENTED_EDGE('',*,*,#41323,.T.) ;
#55976 = ORIENTED_EDGE('',*,*,#41324,.T.) ;
#55977 = ORIENTED_EDGE('',*,*,#41325,.T.) ;
#55978 = ORIENTED_EDGE('',*,*,#41326,.T.) ;
#55979 = ORIENTED_EDGE('',*,*,#41327,.T.) ;
#55980 = ORIENTED_EDGE('',*,*,#41328,.T.) ;
#55981 = ORIENTED_EDGE('',*,*,#41329,.T.) ;
#55982 = ORIENTED_EDGE('',*,*,#41330,.T.) ;
#55983 = ORIENTED_EDGE('',*,*,#41331,.T.) ;
#55984 = ORIENTED_EDGE('',*,*,#41332,.T.) ;
#55985 = ORIENTED_EDGE('',*,*,#41333,.T.) ;
#55986 = ORIENTED_EDGE('',*,*,#41334,.T.) ;
#55987 = ORIENTED_EDGE('',*,*,#41335,.T.) ;
#55988 = ORIENTED_EDGE('',*,*,#41336,.T.) ;
#55989 = ORIENTED_EDGE('',*,*,#41337,.T.) ;
#55990 = ORIENTED_EDGE('',*,*,#41338,.T.) ;
#55991 = ORIENTED_EDGE('',*,*,#41339,.T.) ;
#55992 = ORIENTED_EDGE('',*,*,#39194,.T.) ;
#55993 = ORIENTED_EDGE('',*,*,#41340,.F.) ;
#55994 = ORIENTED_EDGE('',*,*,#41341,.T.) ;
#55995 = ORIENTED_EDGE('',*,*,#41342,.T.) ;
#55996 = ORIENTED_EDGE('',*,*,#41343,.T.) ;
#55997 = ORIENTED_EDGE('',*,*,#41342,.F.) ;
#55998 = ORIENTED_EDGE('',*,*,#41344,.T.) ;
#55999 = ORIENTED_EDGE('',*,*,#41345,.T.) ;
#56000 = ORIENTED_EDGE('',*,*,#41346,.T.) ;
#56001 = ORIENTED_EDGE('',*,*,#41345,.F.) ;
#56002 = ORIENTED_EDGE('',*,*,#41347,.T.) ;
#56003 = ORIENTED_EDGE('',*,*,#41348,.T.) ;
#56004 = ORIENTED_EDGE('',*,*,#41349,.T.) ;
#56005 = ORIENTED_EDGE('',*,*,#41348,.F.) ;
#56006 = ORIENTED_EDGE('',*,*,#41350,.T.) ;
#56007 = ORIENTED_EDGE('',*,*,#41351,.T.) ;
#56008 = ORIENTED_EDGE('',*,*,#41352,.T.) ;
#56009 = ORIENTED_EDGE('',*,*,#41351,.F.) ;
#56010 = ORIENTED_EDGE('',*,*,#41353,.T.) ;
#56011 = ORIENTED_EDGE('',*,*,#41354,.T.) ;
#56012 = ORIENTED_EDGE('',*,*,#41355,.T.) ;
#56013 = ORIENTED_EDGE('',*,*,#41354,.F.) ;
#56014 = ORIENTED_EDGE('',*,*,#41356,.T.) ;
#56015 = ORIENTED_EDGE('',*,*,#41357,.T.) ;
#56016 = ORIENTED_EDGE('',*,*,#41358,.T.) ;
#56017 = ORIENTED_EDGE('',*,*,#41357,.F.) ;
#56018 = ORIENTED_EDGE('',*,*,#39214,.T.) ;
#56019 = ORIENTED_EDGE('',*,*,#41359,.T.) ;
#56020 = ORIENTED_EDGE('',*,*,#41360,.T.) ;
#56021 = ORIENTED_EDGE('',*,*,#41359,.F.) ;
#56022 = ORIENTED_EDGE('',*,*,#41361,.T.) ;
#56023 = ORIENTED_EDGE('',*,*,#39291,.T.) ;
#56024 = ORIENTED_EDGE('',*,*,#41362,.T.) ;
#56025 = ORIENTED_EDGE('',*,*,#39290,.F.) ;
#56026 = ORIENTED_EDGE('',*,*,#41363,.T.) ;
#56027 = ORIENTED_EDGE('',*,*,#41364,.T.) ;
#56028 = ORIENTED_EDGE('',*,*,#41365,.T.) ;
#56029 = ORIENTED_EDGE('',*,*,#41364,.F.) ;
#56030 = ORIENTED_EDGE('',*,*,#41366,.T.) ;
#56031 = ORIENTED_EDGE('',*,*,#41367,.T.) ;
#56032 = ORIENTED_EDGE('',*,*,#41368,.T.) ;
#56033 = ORIENTED_EDGE('',*,*,#41367,.F.) ;
#56034 = ORIENTED_EDGE('',*,*,#41369,.T.) ;
#56035 = ORIENTED_EDGE('',*,*,#41370,.T.) ;
#56036 = ORIENTED_EDGE('',*,*,#41371,.T.) ;
#56037 = ORIENTED_EDGE('',*,*,#41370,.F.) ;
#56038 = ORIENTED_EDGE('',*,*,#41372,.T.) ;
#56039 = ORIENTED_EDGE('',*,*,#41373,.T.) ;
#56040 = ORIENTED_EDGE('',*,*,#41374,.T.) ;
#56041 = ORIENTED_EDGE('',*,*,#41373,.F.) ;
#56042 = ORIENTED_EDGE('',*,*,#41375,.T.) ;
#56043 = ORIENTED_EDGE('',*,*,#41376,.T.) ;
#56044 = ORIENTED_EDGE('',*,*,#41377,.T.) ;
#56045 = ORIENTED_EDGE('',*,*,#41376,.F.) ;
#56046 = ORIENTED_EDGE('',*,*,#41378,.T.) ;
#56047 = ORIENTED_EDGE('',*,*,#41379,.T.) ;
#56048 = ORIENTED_EDGE('',*,*,#41380,.T.) ;
#56049 = ORIENTED_EDGE('',*,*,#41379,.F.) ;
#56050 = ORIENTED_EDGE('',*,*,#41381,.T.) ;
#56051 = ORIENTED_EDGE('',*,*,#41382,.T.) ;
#56052 = ORIENTED_EDGE('',*,*,#41383,.T.) ;
#56053 = ORIENTED_EDGE('',*,*,#41382,.F.) ;
#56054 = ORIENTED_EDGE('',*,*,#41384,.T.) ;
#56055 = ORIENTED_EDGE('',*,*,#41385,.T.) ;
#56056 = ORIENTED_EDGE('',*,*,#41386,.T.) ;
#56057 = ORIENTED_EDGE('',*,*,#41385,.F.) ;
#56058 = ORIENTED_EDGE('',*,*,#41387,.T.) ;
#56059 = ORIENTED_EDGE('',*,*,#41388,.T.) ;
#56060 = ORIENTED_EDGE('',*,*,#41389,.T.) ;
#56061 = ORIENTED_EDGE('',*,*,#41388,.F.) ;
#56062 = ORIENTED_EDGE('',*,*,#41390,.T.) ;
#56063 = ORIENTED_EDGE('',*,*,#41391,.T.) ;
#56064 = ORIENTED_EDGE('',*,*,#41392,.T.) ;
#56065 = ORIENTED_EDGE('',*,*,#41391,.F.) ;
#56066 = ORIENTED_EDGE('',*,*,#41393,.T.) ;
#56067 = ORIENTED_EDGE('',*,*,#41394,.T.) ;
#56068 = ORIENTED_EDGE('',*,*,#41395,.T.) ;
#56069 = ORIENTED_EDGE('',*,*,#41394,.F.) ;
#56070 = ORIENTED_EDGE('',*,*,#41396,.T.) ;
#56071 = ORIENTED_EDGE('',*,*,#41397,.T.) ;
#56072 = ORIENTED_EDGE('',*,*,#41398,.T.) ;
#56073 = ORIENTED_EDGE('',*,*,#41397,.F.) ;
#56074 = ORIENTED_EDGE('',*,*,#41399,.T.) ;
#56075 = ORIENTED_EDGE('',*,*,#41400,.T.) ;
#56076 = ORIENTED_EDGE('',*,*,#41401,.T.) ;
#56077 = ORIENTED_EDGE('',*,*,#41400,.F.) ;
#56078 = ORIENTED_EDGE('',*,*,#41402,.T.) ;
#56079 = ORIENTED_EDGE('',*,*,#41403,.T.) ;
#56080 = ORIENTED_EDGE('',*,*,#41404,.T.) ;
#56081 = ORIENTED_EDGE('',*,*,#41403,.F.) ;
#56082 = ORIENTED_EDGE('',*,*,#41405,.T.) ;
#56083 = ORIENTED_EDGE('',*,*,#41406,.T.) ;
#56084 = ORIENTED_EDGE('',*,*,#41407,.T.) ;
#56085 = ORIENTED_EDGE('',*,*,#41406,.F.) ;
#56086 = ORIENTED_EDGE('',*,*,#41408,.T.) ;
#56087 = ORIENTED_EDGE('',*,*,#41409,.T.) ;
#56088 = ORIENTED_EDGE('',*,*,#41410,.T.) ;
#56089 = ORIENTED_EDGE('',*,*,#41409,.F.) ;
#56090 = ORIENTED_EDGE('',*,*,#41411,.T.) ;
#56091 = ORIENTED_EDGE('',*,*,#41412,.T.) ;
#56092 = ORIENTED_EDGE('',*,*,#41413,.T.) ;
#56093 = ORIENTED_EDGE('',*,*,#41412,.F.) ;
#56094 = ORIENTED_EDGE('',*,*,#41414,.T.) ;
#56095 = ORIENTED_EDGE('',*,*,#41415,.T.) ;
#56096 = ORIENTED_EDGE('',*,*,#41416,.T.) ;
#56097 = ORIENTED_EDGE('',*,*,#41415,.F.) ;
#56098 = ORIENTED_EDGE('',*,*,#41417,.T.) ;
#56099 = ORIENTED_EDGE('',*,*,#41340,.T.) ;
#56100 = ORIENTED_EDGE('',*,*,#41418,.T.) ;
#56101 = ORIENTED_EDGE('',*,*,#41419,.T.) ;
#56102 = ORIENTED_EDGE('',*,*,#41420,.T.) ;
#56103 = ORIENTED_EDGE('',*,*,#41421,.T.) ;
#56104 = ORIENTED_EDGE('',*,*,#41422,.T.) ;
#56105 = ORIENTED_EDGE('',*,*,#41423,.T.) ;
#56106 = ORIENTED_EDGE('',*,*,#41424,.T.) ;
#56107 = ORIENTED_EDGE('',*,*,#41425,.T.) ;
#56108 = ORIENTED_EDGE('',*,*,#41426,.T.) ;
#56109 = ORIENTED_EDGE('',*,*,#41427,.T.) ;
#56110 = ORIENTED_EDGE('',*,*,#41428,.T.) ;
#56111 = ORIENTED_EDGE('',*,*,#41429,.T.) ;
#56112 = ORIENTED_EDGE('',*,*,#41430,.T.) ;
#56113 = ORIENTED_EDGE('',*,*,#41431,.T.) ;
#56114 = ORIENTED_EDGE('',*,*,#41432,.T.) ;
#56115 = ORIENTED_EDGE('',*,*,#41433,.T.) ;
#56116 = ORIENTED_EDGE('',*,*,#41434,.T.) ;
#56117 = ORIENTED_EDGE('',*,*,#41435,.T.) ;
#56118 = ORIENTED_EDGE('',*,*,#41436,.T.) ;
#56119 = ORIENTED_EDGE('',*,*,#39211,.T.) ;
#56120 = ORIENTED_EDGE('',*,*,#41437,.F.) ;
#56121 = ORIENTED_EDGE('',*,*,#41438,.T.) ;
#56122 = ORIENTED_EDGE('',*,*,#41439,.T.) ;
#56123 = ORIENTED_EDGE('',*,*,#41440,.T.) ;
#56124 = ORIENTED_EDGE('',*,*,#41439,.F.) ;
#56125 = ORIENTED_EDGE('',*,*,#41441,.T.) ;
#56126 = ORIENTED_EDGE('',*,*,#41442,.T.) ;
#56127 = ORIENTED_EDGE('',*,*,#41443,.T.) ;
#56128 = ORIENTED_EDGE('',*,*,#41442,.F.) ;
#56129 = ORIENTED_EDGE('',*,*,#41444,.T.) ;
#56130 = ORIENTED_EDGE('',*,*,#41445,.T.) ;
#56131 = ORIENTED_EDGE('',*,*,#41446,.T.) ;
#56132 = ORIENTED_EDGE('',*,*,#41445,.F.) ;
#56133 = ORIENTED_EDGE('',*,*,#41447,.T.) ;
#56134 = ORIENTED_EDGE('',*,*,#41448,.T.) ;
#56135 = ORIENTED_EDGE('',*,*,#41449,.T.) ;
#56136 = ORIENTED_EDGE('',*,*,#41448,.F.) ;
#56137 = ORIENTED_EDGE('',*,*,#41450,.T.) ;
#56138 = ORIENTED_EDGE('',*,*,#41451,.T.) ;
#56139 = ORIENTED_EDGE('',*,*,#41452,.T.) ;
#56140 = ORIENTED_EDGE('',*,*,#41451,.F.) ;
#56141 = ORIENTED_EDGE('',*,*,#41453,.T.) ;
#56142 = ORIENTED_EDGE('',*,*,#41454,.T.) ;
#56143 = ORIENTED_EDGE('',*,*,#41455,.T.) ;
#56144 = ORIENTED_EDGE('',*,*,#41454,.F.) ;
#56145 = ORIENTED_EDGE('',*,*,#39267,.T.) ;
#56146 = ORIENTED_EDGE('',*,*,#41456,.T.) ;
#56147 = ORIENTED_EDGE('',*,*,#41457,.T.) ;
#56148 = ORIENTED_EDGE('',*,*,#41456,.F.) ;
#56149 = ORIENTED_EDGE('',*,*,#41458,.T.) ;
#56150 = ORIENTED_EDGE('',*,*,#39288,.T.) ;
#56151 = ORIENTED_EDGE('',*,*,#41459,.T.) ;
#56152 = ORIENTED_EDGE('',*,*,#39287,.F.) ;
#56153 = ORIENTED_EDGE('',*,*,#41460,.T.) ;
#56154 = ORIENTED_EDGE('',*,*,#41461,.T.) ;
#56155 = ORIENTED_EDGE('',*,*,#41462,.T.) ;
#56156 = ORIENTED_EDGE('',*,*,#41461,.F.) ;
#56157 = ORIENTED_EDGE('',*,*,#41463,.T.) ;
#56158 = ORIENTED_EDGE('',*,*,#41464,.T.) ;
#56159 = ORIENTED_EDGE('',*,*,#41465,.T.) ;
#56160 = ORIENTED_EDGE('',*,*,#41464,.F.) ;
#56161 = ORIENTED_EDGE('',*,*,#41466,.T.) ;
#56162 = ORIENTED_EDGE('',*,*,#41467,.T.) ;
#56163 = ORIENTED_EDGE('',*,*,#41468,.T.) ;
#56164 = ORIENTED_EDGE('',*,*,#41467,.F.) ;
#56165 = ORIENTED_EDGE('',*,*,#41469,.T.) ;
#56166 = ORIENTED_EDGE('',*,*,#41470,.T.) ;
#56167 = ORIENTED_EDGE('',*,*,#41471,.T.) ;
#56168 = ORIENTED_EDGE('',*,*,#41470,.F.) ;
#56169 = ORIENTED_EDGE('',*,*,#41472,.T.) ;
#56170 = ORIENTED_EDGE('',*,*,#41473,.T.) ;
#56171 = ORIENTED_EDGE('',*,*,#41474,.T.) ;
#56172 = ORIENTED_EDGE('',*,*,#41473,.F.) ;
#56173 = ORIENTED_EDGE('',*,*,#41475,.T.) ;
#56174 = ORIENTED_EDGE('',*,*,#41476,.T.) ;
#56175 = ORIENTED_EDGE('',*,*,#41477,.T.) ;
#56176 = ORIENTED_EDGE('',*,*,#41476,.F.) ;
#56177 = ORIENTED_EDGE('',*,*,#41478,.T.) ;
#56178 = ORIENTED_EDGE('',*,*,#41479,.T.) ;
#56179 = ORIENTED_EDGE('',*,*,#41480,.T.) ;
#56180 = ORIENTED_EDGE('',*,*,#41479,.F.) ;
#56181 = ORIENTED_EDGE('',*,*,#41481,.T.) ;
#56182 = ORIENTED_EDGE('',*,*,#41482,.T.) ;
#56183 = ORIENTED_EDGE('',*,*,#41483,.T.) ;
#56184 = ORIENTED_EDGE('',*,*,#41482,.F.) ;
#56185 = ORIENTED_EDGE('',*,*,#41484,.T.) ;
#56186 = ORIENTED_EDGE('',*,*,#41485,.T.) ;
#56187 = ORIENTED_EDGE('',*,*,#41486,.T.) ;
#56188 = ORIENTED_EDGE('',*,*,#41485,.F.) ;
#56189 = ORIENTED_EDGE('',*,*,#41487,.T.) ;
#56190 = ORIENTED_EDGE('',*,*,#41488,.T.) ;
#56191 = ORIENTED_EDGE('',*,*,#41489,.T.) ;
#56192 = ORIENTED_EDGE('',*,*,#41488,.F.) ;
#56193 = ORIENTED_EDGE('',*,*,#41490,.T.) ;
#56194 = ORIENTED_EDGE('',*,*,#41491,.T.) ;
#56195 = ORIENTED_EDGE('',*,*,#41492,.T.) ;
#56196 = ORIENTED_EDGE('',*,*,#41491,.F.) ;
#56197 = ORIENTED_EDGE('',*,*,#41493,.T.) ;
#56198 = ORIENTED_EDGE('',*,*,#41494,.T.) ;
#56199 = ORIENTED_EDGE('',*,*,#41495,.T.) ;
#56200 = ORIENTED_EDGE('',*,*,#41494,.F.) ;
#56201 = ORIENTED_EDGE('',*,*,#41496,.T.) ;
#56202 = ORIENTED_EDGE('',*,*,#41497,.T.) ;
#56203 = ORIENTED_EDGE('',*,*,#41498,.T.) ;
#56204 = ORIENTED_EDGE('',*,*,#41497,.F.) ;
#56205 = ORIENTED_EDGE('',*,*,#41499,.T.) ;
#56206 = ORIENTED_EDGE('',*,*,#41500,.T.) ;
#56207 = ORIENTED_EDGE('',*,*,#41501,.T.) ;
#56208 = ORIENTED_EDGE('',*,*,#41500,.F.) ;
#56209 = ORIENTED_EDGE('',*,*,#41502,.T.) ;
#56210 = ORIENTED_EDGE('',*,*,#41503,.T.) ;
#56211 = ORIENTED_EDGE('',*,*,#41504,.T.) ;
#56212 = ORIENTED_EDGE('',*,*,#41503,.F.) ;
#56213 = ORIENTED_EDGE('',*,*,#41505,.T.) ;
#56214 = ORIENTED_EDGE('',*,*,#41506,.T.) ;
#56215 = ORIENTED_EDGE('',*,*,#41507,.T.) ;
#56216 = ORIENTED_EDGE('',*,*,#41506,.F.) ;
#56217 = ORIENTED_EDGE('',*,*,#41508,.T.) ;
#56218 = ORIENTED_EDGE('',*,*,#41509,.T.) ;
#56219 = ORIENTED_EDGE('',*,*,#41510,.T.) ;
#56220 = ORIENTED_EDGE('',*,*,#41509,.F.) ;
#56221 = ORIENTED_EDGE('',*,*,#41511,.T.) ;
#56222 = ORIENTED_EDGE('',*,*,#41512,.T.) ;
#56223 = ORIENTED_EDGE('',*,*,#41513,.T.) ;
#56224 = ORIENTED_EDGE('',*,*,#41512,.F.) ;
#56225 = ORIENTED_EDGE('',*,*,#41514,.T.) ;
#56226 = ORIENTED_EDGE('',*,*,#41437,.T.) ;
#56227 = ORIENTED_EDGE('',*,*,#41515,.T.) ;
#56228 = ORIENTED_EDGE('',*,*,#41516,.T.) ;
#56229 = ORIENTED_EDGE('',*,*,#41517,.T.) ;
#56230 = ORIENTED_EDGE('',*,*,#41518,.T.) ;
#56231 = ORIENTED_EDGE('',*,*,#41519,.T.) ;
#56232 = ORIENTED_EDGE('',*,*,#41520,.T.) ;
#56233 = ORIENTED_EDGE('',*,*,#41521,.T.) ;
#56234 = ORIENTED_EDGE('',*,*,#41522,.T.) ;
#56235 = ORIENTED_EDGE('',*,*,#41523,.T.) ;
#56236 = ORIENTED_EDGE('',*,*,#41524,.T.) ;
#56237 = ORIENTED_EDGE('',*,*,#41525,.T.) ;
#56238 = ORIENTED_EDGE('',*,*,#41526,.T.) ;
#56239 = ORIENTED_EDGE('',*,*,#41527,.T.) ;
#56240 = ORIENTED_EDGE('',*,*,#41528,.T.) ;
#56241 = ORIENTED_EDGE('',*,*,#41529,.T.) ;
#56242 = ORIENTED_EDGE('',*,*,#41530,.T.) ;
#56243 = ORIENTED_EDGE('',*,*,#41531,.T.) ;
#56244 = ORIENTED_EDGE('',*,*,#41532,.T.) ;
#56245 = ORIENTED_EDGE('',*,*,#41533,.T.) ;
#56246 = ORIENTED_EDGE('',*,*,#39264,.T.) ;
#56247 = ORIENTED_EDGE('',*,*,#39224,.T.) ;
#56248 = ORIENTED_EDGE('',*,*,#41534,.F.) ;
#56249 = ORIENTED_EDGE('',*,*,#41535,.T.) ;
#56250 = ORIENTED_EDGE('',*,*,#41536,.T.) ;
#56251 = ORIENTED_EDGE('',*,*,#41537,.T.) ;
#56252 = ORIENTED_EDGE('',*,*,#41538,.T.) ;
#56253 = ORIENTED_EDGE('',*,*,#41539,.T.) ;
#56254 = ORIENTED_EDGE('',*,*,#41540,.T.) ;
#56255 = ORIENTED_EDGE('',*,*,#41541,.T.) ;
#56256 = ORIENTED_EDGE('',*,*,#39207,.T.) ;
#56257 = ORIENTED_EDGE('',*,*,#41542,.F.) ;
#56258 = ORIENTED_EDGE('',*,*,#41543,.T.) ;
#56259 = ORIENTED_EDGE('',*,*,#41544,.T.) ;
#56260 = ORIENTED_EDGE('',*,*,#41545,.T.) ;
#56261 = ORIENTED_EDGE('',*,*,#41546,.T.) ;
#56262 = ORIENTED_EDGE('',*,*,#41547,.T.) ;
#56263 = ORIENTED_EDGE('',*,*,#41548,.T.) ;
#56264 = ORIENTED_EDGE('',*,*,#41549,.T.) ;
#56265 = ORIENTED_EDGE('',*,*,#39190,.T.) ;
#56266 = ORIENTED_EDGE('',*,*,#41550,.F.) ;
#56267 = ORIENTED_EDGE('',*,*,#41551,.T.) ;
#56268 = ORIENTED_EDGE('',*,*,#41552,.T.) ;
#56269 = ORIENTED_EDGE('',*,*,#41553,.T.) ;
#56270 = ORIENTED_EDGE('',*,*,#41554,.T.) ;
#56271 = ORIENTED_EDGE('',*,*,#41555,.T.) ;
#56272 = ORIENTED_EDGE('',*,*,#41556,.T.) ;
#56273 = ORIENTED_EDGE('',*,*,#41557,.T.) ;
#56274 = ORIENTED_EDGE('',*,*,#39173,.T.) ;
#56275 = ORIENTED_EDGE('',*,*,#41558,.F.) ;
#56276 = ORIENTED_EDGE('',*,*,#41559,.T.) ;
#56277 = ORIENTED_EDGE('',*,*,#41560,.T.) ;
#56278 = ORIENTED_EDGE('',*,*,#41561,.T.) ;
#56279 = ORIENTED_EDGE('',*,*,#41562,.T.) ;
#56280 = ORIENTED_EDGE('',*,*,#41563,.T.) ;
#56281 = ORIENTED_EDGE('',*,*,#41564,.T.) ;
#56282 = ORIENTED_EDGE('',*,*,#41565,.T.) ;
#56283 = ORIENTED_EDGE('',*,*,#39156,.T.) ;
#56284 = ORIENTED_EDGE('',*,*,#41566,.F.) ;
#56285 = ORIENTED_EDGE('',*,*,#41567,.T.) ;
#56286 = ORIENTED_EDGE('',*,*,#41568,.T.) ;
#56287 = ORIENTED_EDGE('',*,*,#41569,.T.) ;
#56288 = ORIENTED_EDGE('',*,*,#41570,.T.) ;
#56289 = ORIENTED_EDGE('',*,*,#41571,.T.) ;
#56290 = ORIENTED_EDGE('',*,*,#41572,.T.) ;
#56291 = ORIENTED_EDGE('',*,*,#41573,.T.) ;
#56292 = ORIENTED_EDGE('',*,*,#39139,.T.) ;
#56293 = ORIENTED_EDGE('',*,*,#41574,.F.) ;
#56294 = ORIENTED_EDGE('',*,*,#41575,.T.) ;
#56295 = ORIENTED_EDGE('',*,*,#41576,.T.) ;
#56296 = ORIENTED_EDGE('',*,*,#41577,.T.) ;
#56297 = ORIENTED_EDGE('',*,*,#41578,.T.) ;
#56298 = ORIENTED_EDGE('',*,*,#41579,.T.) ;
#56299 = ORIENTED_EDGE('',*,*,#41580,.T.) ;
#56300 = ORIENTED_EDGE('',*,*,#41581,.T.) ;
#56301 = ORIENTED_EDGE('',*,*,#39122,.T.) ;
#56302 = ORIENTED_EDGE('',*,*,#41582,.F.) ;
#56303 = ORIENTED_EDGE('',*,*,#41583,.T.) ;
#56304 = ORIENTED_EDGE('',*,*,#41584,.T.) ;
#56305 = ORIENTED_EDGE('',*,*,#41585,.T.) ;
#56306 = ORIENTED_EDGE('',*,*,#41586,.T.) ;
#56307 = ORIENTED_EDGE('',*,*,#41587,.T.) ;
#56308 = ORIENTED_EDGE('',*,*,#41588,.T.) ;
#56309 = ORIENTED_EDGE('',*,*,#41589,.T.) ;
#56310 = ORIENTED_EDGE('',*,*,#39105,.T.) ;
#56311 = ORIENTED_EDGE('',*,*,#41590,.F.) ;
#56312 = ORIENTED_EDGE('',*,*,#41591,.T.) ;
#56313 = ORIENTED_EDGE('',*,*,#41592,.T.) ;
#56314 = ORIENTED_EDGE('',*,*,#41593,.T.) ;
#56315 = ORIENTED_EDGE('',*,*,#41594,.T.) ;
#56316 = ORIENTED_EDGE('',*,*,#41595,.T.) ;
#56317 = ORIENTED_EDGE('',*,*,#41596,.T.) ;
#56318 = ORIENTED_EDGE('',*,*,#41597,.T.) ;
#56319 = ORIENTED_EDGE('',*,*,#39088,.T.) ;
#56320 = ORIENTED_EDGE('',*,*,#41598,.F.) ;
#56321 = ORIENTED_EDGE('',*,*,#41599,.T.) ;
#56322 = ORIENTED_EDGE('',*,*,#41600,.T.) ;
#56323 = ORIENTED_EDGE('',*,*,#41601,.T.) ;
#56324 = ORIENTED_EDGE('',*,*,#41602,.T.) ;
#56325 = ORIENTED_EDGE('',*,*,#41603,.T.) ;
#56326 = ORIENTED_EDGE('',*,*,#41604,.T.) ;
#56327 = ORIENTED_EDGE('',*,*,#41605,.T.) ;
#56328 = ORIENTED_EDGE('',*,*,#41606,.F.) ;
#56329 = ORIENTED_EDGE('',*,*,#40502,.F.) ;
#56330 = ORIENTED_EDGE('',*,*,#41607,.F.) ;
#56331 = ORIENTED_EDGE('',*,*,#40489,.F.) ;
#56332 = ORIENTED_EDGE('',*,*,#41608,.F.) ;
#56333 = ORIENTED_EDGE('',*,*,#40503,.F.) ;
#56334 = ORIENTED_EDGE('',*,*,#41609,.F.) ;
#56335 = ORIENTED_EDGE('',*,*,#40497,.F.) ;
#56336 = ORIENTED_EDGE('',*,*,#41610,.F.) ;
#56337 = ORIENTED_EDGE('',*,*,#41608,.T.) ;
#56338 = ORIENTED_EDGE('',*,*,#41611,.F.) ;
#56339 = ORIENTED_EDGE('',*,*,#41612,.F.) ;
#56340 = ORIENTED_EDGE('',*,*,#41607,.T.) ;
#56341 = ORIENTED_EDGE('',*,*,#41613,.F.) ;
#56342 = ORIENTED_EDGE('',*,*,#41606,.T.) ;
#56343 = ORIENTED_EDGE('',*,*,#40488,.T.) ;
#56344 = ORIENTED_EDGE('',*,*,#41614,.F.) ;
#56345 = ORIENTED_EDGE('',*,*,#41609,.T.) ;
#56346 = ORIENTED_EDGE('',*,*,#41611,.T.) ;
#56347 = ORIENTED_EDGE('',*,*,#40500,.F.) ;
#56348 = ORIENTED_EDGE('',*,*,#41615,.F.) ;
#56349 = ORIENTED_EDGE('',*,*,#39270,.T.) ;
#56350 = ORIENTED_EDGE('',*,*,#41616,.T.) ;
#56351 = ORIENTED_EDGE('',*,*,#41617,.F.) ;
#56352 = ORIENTED_EDGE('',*,*,#41610,.T.) ;
#56353 = ORIENTED_EDGE('',*,*,#41618,.F.) ;
#56354 = ORIENTED_EDGE('',*,*,#41619,.T.) ;
#56355 = ORIENTED_EDGE('',*,*,#41620,.F.) ;
#56356 = ORIENTED_EDGE('',*,*,#39426,.F.) ;
#56357 = ORIENTED_EDGE('',*,*,#41621,.F.) ;
#56358 = ORIENTED_EDGE('',*,*,#40504,.F.) ;
#56359 = ORIENTED_EDGE('',*,*,#41613,.T.) ;
#56360 = ORIENTED_EDGE('',*,*,#40501,.F.) ;
#56361 = ORIENTED_EDGE('',*,*,#41622,.F.) ;
#56362 = ORIENTED_EDGE('',*,*,#40507,.F.) ;
#56363 = ORIENTED_EDGE('',*,*,#41612,.T.) ;
#56364 = ORIENTED_EDGE('',*,*,#40506,.F.) ;
#56365 = ORIENTED_EDGE('',*,*,#41623,.F.) ;
#56366 = ORIENTED_EDGE('',*,*,#40480,.F.) ;
#56367 = ORIENTED_EDGE('',*,*,#41614,.T.) ;
#56368 = ORIENTED_EDGE('',*,*,#40487,.F.) ;
#56369 = ORIENTED_EDGE('',*,*,#41624,.F.) ;
#56370 = ORIENTED_EDGE('',*,*,#40498,.F.) ;
#56371 = ORIENTED_EDGE('',*,*,#41625,.F.) ;
#56372 = ORIENTED_EDGE('',*,*,#40499,.F.) ;
#56373 = ORIENTED_EDGE('',*,*,#41626,.F.) ;
#56374 = ORIENTED_EDGE('',*,*,#40494,.F.) ;
#56375 = ORIENTED_EDGE('',*,*,#41615,.T.) ;
#56376 = ORIENTED_EDGE('',*,*,#41625,.T.) ;
#56377 = ORIENTED_EDGE('',*,*,#39271,.F.) ;
#56378 = ORIENTED_EDGE('',*,*,#41621,.T.) ;
#56379 = ORIENTED_EDGE('',*,*,#39436,.T.) ;
#56380 = ORIENTED_EDGE('',*,*,#41627,.F.) ;
#56381 = ORIENTED_EDGE('',*,*,#41622,.T.) ;
#56382 = ORIENTED_EDGE('',*,*,#41628,.F.) ;
#56383 = ORIENTED_EDGE('',*,*,#41623,.T.) ;
#56384 = ORIENTED_EDGE('',*,*,#41629,.F.) ;
#56385 = ORIENTED_EDGE('',*,*,#39522,.T.) ;
#56386 = ORIENTED_EDGE('',*,*,#41624,.T.) ;
#56387 = ORIENTED_EDGE('',*,*,#40486,.T.) ;
#56388 = ORIENTED_EDGE('',*,*,#41630,.F.) ;
#56389 = ORIENTED_EDGE('',*,*,#41626,.T.) ;
#56390 = ORIENTED_EDGE('',*,*,#41627,.T.) ;
#56391 = ORIENTED_EDGE('',*,*,#39435,.F.) ;
#56392 = ORIENTED_EDGE('',*,*,#41631,.F.) ;
#56393 = ORIENTED_EDGE('',*,*,#40508,.F.) ;
#56394 = ORIENTED_EDGE('',*,*,#41629,.T.) ;
#56395 = ORIENTED_EDGE('',*,*,#40505,.F.) ;
#56396 = ORIENTED_EDGE('',*,*,#41632,.F.) ;
#56397 = ORIENTED_EDGE('',*,*,#39523,.F.) ;
#56398 = ORIENTED_EDGE('',*,*,#40481,.F.) ;
#56399 = ORIENTED_EDGE('',*,*,#41628,.T.) ;
#56400 = ORIENTED_EDGE('',*,*,#41633,.F.) ;
#56401 = ORIENTED_EDGE('',*,*,#41634,.F.) ;
#56402 = ORIENTED_EDGE('',*,*,#41630,.T.) ;
#56403 = ORIENTED_EDGE('',*,*,#40485,.F.) ;
#56404 = ORIENTED_EDGE('',*,*,#41635,.F.) ;
#56405 = ORIENTED_EDGE('',*,*,#40495,.F.) ;
#56406 = ORIENTED_EDGE('',*,*,#41636,.F.) ;
#56407 = ORIENTED_EDGE('',*,*,#40496,.F.) ;
#56408 = ORIENTED_EDGE('',*,*,#41637,.F.) ;
#56409 = ORIENTED_EDGE('',*,*,#40490,.F.) ;
#56410 = ORIENTED_EDGE('',*,*,#39273,.T.) ;
#56411 = ORIENTED_EDGE('',*,*,#41636,.T.) ;
#56412 = ORIENTED_EDGE('',*,*,#41638,.F.) ;
#56413 = ORIENTED_EDGE('',*,*,#39430,.T.) ;
#56414 = ORIENTED_EDGE('',*,*,#41632,.T.) ;
#56415 = ORIENTED_EDGE('',*,*,#41631,.T.) ;
#56416 = ORIENTED_EDGE('',*,*,#41639,.F.) ;
#56417 = ORIENTED_EDGE('',*,*,#41640,.F.) ;
#56418 = ORIENTED_EDGE('',*,*,#39528,.F.) ;
#56419 = ORIENTED_EDGE('',*,*,#41641,.F.) ;
#56420 = ORIENTED_EDGE('',*,*,#41642,.F.) ;
#56421 = ORIENTED_EDGE('',*,*,#41633,.T.) ;
#56422 = ORIENTED_EDGE('',*,*,#39526,.F.) ;
#56423 = ORIENTED_EDGE('',*,*,#41641,.T.) ;
#56424 = ORIENTED_EDGE('',*,*,#39689,.F.) ;
#56425 = ORIENTED_EDGE('',*,*,#41634,.T.) ;
#56426 = ORIENTED_EDGE('',*,*,#41643,.F.) ;
#56427 = ORIENTED_EDGE('',*,*,#41644,.F.) ;
#56428 = ORIENTED_EDGE('',*,*,#41637,.T.) ;
#56429 = ORIENTED_EDGE('',*,*,#41635,.T.) ;
#56430 = ORIENTED_EDGE('',*,*,#41645,.F.) ;
#56431 = ORIENTED_EDGE('',*,*,#41638,.T.) ;
#56432 = ORIENTED_EDGE('',*,*,#40493,.F.) ;
#56433 = ORIENTED_EDGE('',*,*,#41646,.F.) ;
#56434 = ORIENTED_EDGE('',*,*,#39431,.F.) ;
#56435 = ORIENTED_EDGE('',*,*,#41639,.T.) ;
#56436 = ORIENTED_EDGE('',*,*,#39434,.F.) ;
#56437 = ORIENTED_EDGE('',*,*,#41647,.F.) ;
#56438 = ORIENTED_EDGE('',*,*,#39524,.F.) ;
#56439 = ORIENTED_EDGE('',*,*,#41640,.T.) ;
#56440 = ORIENTED_EDGE('',*,*,#39525,.F.) ;
#56441 = ORIENTED_EDGE('',*,*,#41648,.F.) ;
#56442 = ORIENTED_EDGE('',*,*,#39602,.F.) ;
#56443 = ORIENTED_EDGE('',*,*,#41642,.T.) ;
#56444 = ORIENTED_EDGE('',*,*,#39688,.T.) ;
#56445 = ORIENTED_EDGE('',*,*,#41649,.F.) ;
#56446 = ORIENTED_EDGE('',*,*,#41643,.T.) ;
#56447 = ORIENTED_EDGE('',*,*,#40482,.F.) ;
#56448 = ORIENTED_EDGE('',*,*,#41644,.T.) ;
#56449 = ORIENTED_EDGE('',*,*,#41650,.F.) ;
#56450 = ORIENTED_EDGE('',*,*,#41651,.F.) ;
#56451 = ORIENTED_EDGE('',*,*,#41645,.T.) ;
#56452 = ORIENTED_EDGE('',*,*,#40484,.F.) ;
#56453 = ORIENTED_EDGE('',*,*,#41652,.F.) ;
#56454 = ORIENTED_EDGE('',*,*,#40491,.F.) ;
#56455 = ORIENTED_EDGE('',*,*,#41653,.F.) ;
#56456 = ORIENTED_EDGE('',*,*,#40492,.F.) ;
#56457 = ORIENTED_EDGE('',*,*,#41654,.F.) ;
#56458 = ORIENTED_EDGE('',*,*,#39521,.F.) ;
#56459 = ORIENTED_EDGE('',*,*,#41646,.T.) ;
#56460 = ORIENTED_EDGE('',*,*,#41653,.T.) ;
#56461 = ORIENTED_EDGE('',*,*,#41655,.F.) ;
#56462 = ORIENTED_EDGE('',*,*,#41648,.T.) ;
#56463 = ORIENTED_EDGE('',*,*,#41647,.T.) ;
#56464 = ORIENTED_EDGE('',*,*,#41656,.F.) ;
#56465 = ORIENTED_EDGE('',*,*,#39603,.T.) ;
#56466 = ORIENTED_EDGE('',*,*,#41657,.F.) ;
#56467 = ORIENTED_EDGE('',*,*,#41650,.T.) ;
#56468 = ORIENTED_EDGE('',*,*,#41649,.T.) ;
#56469 = ORIENTED_EDGE('',*,*,#39687,.F.) ;
#56470 = ORIENTED_EDGE('',*,*,#41651,.T.) ;
#56471 = ORIENTED_EDGE('',*,*,#41658,.F.) ;
#56472 = ORIENTED_EDGE('',*,*,#41659,.F.) ;
#56473 = ORIENTED_EDGE('',*,*,#41654,.T.) ;
#56474 = ORIENTED_EDGE('',*,*,#41652,.T.) ;
#56475 = ORIENTED_EDGE('',*,*,#41660,.F.) ;
#56476 = ORIENTED_EDGE('',*,*,#39517,.T.) ;
#56477 = ORIENTED_EDGE('',*,*,#41655,.T.) ;
#56478 = ORIENTED_EDGE('',*,*,#39520,.F.) ;
#56479 = ORIENTED_EDGE('',*,*,#41661,.F.) ;
#56480 = ORIENTED_EDGE('',*,*,#39432,.F.) ;
#56481 = ORIENTED_EDGE('',*,*,#41656,.T.) ;
#56482 = ORIENTED_EDGE('',*,*,#39433,.F.) ;
#56483 = ORIENTED_EDGE('',*,*,#41662,.F.) ;
#56484 = ORIENTED_EDGE('',*,*,#39604,.F.) ;
#56485 = ORIENTED_EDGE('',*,*,#41657,.T.) ;
#56486 = ORIENTED_EDGE('',*,*,#39686,.T.) ;
#56487 = ORIENTED_EDGE('',*,*,#41663,.F.) ;
#56488 = ORIENTED_EDGE('',*,*,#41658,.T.) ;
#56489 = ORIENTED_EDGE('',*,*,#40483,.F.) ;
#56490 = ORIENTED_EDGE('',*,*,#41659,.T.) ;
#56491 = ORIENTED_EDGE('',*,*,#41664,.F.) ;
#56492 = ORIENTED_EDGE('',*,*,#41660,.T.) ;
#56493 = ORIENTED_EDGE('',*,*,#41662,.T.) ;
#56494 = ORIENTED_EDGE('',*,*,#41661,.T.) ;
#56495 = ORIENTED_EDGE('',*,*,#41665,.F.) ;
#56496 = ORIENTED_EDGE('',*,*,#39605,.T.) ;
#56497 = ORIENTED_EDGE('',*,*,#41663,.T.) ;
#56498 = ORIENTED_EDGE('',*,*,#39685,.F.) ;
#56499 = ORIENTED_EDGE('',*,*,#41666,.F.) ;
#56500 = ORIENTED_EDGE('',*,*,#39518,.F.) ;
#56501 = ORIENTED_EDGE('',*,*,#41664,.T.) ;
#56502 = ORIENTED_EDGE('',*,*,#41665,.T.) ;
#56503 = ORIENTED_EDGE('',*,*,#39519,.F.) ;
#56504 = ORIENTED_EDGE('',*,*,#41667,.F.) ;
#56505 = ORIENTED_EDGE('',*,*,#39606,.F.) ;
#56506 = ORIENTED_EDGE('',*,*,#41666,.T.) ;
#56507 = ORIENTED_EDGE('',*,*,#39534,.F.) ;
#56508 = ORIENTED_EDGE('',*,*,#41667,.T.) ;
#56509 = ORIENTED_EDGE('',*,*,#41668,.F.) ;
#56510 = ORIENTED_EDGE('',*,*,#41478,.F.) ;
#56511 = ORIENTED_EDGE('',*,*,#41669,.F.) ;
#56512 = ORIENTED_EDGE('',*,*,#41525,.F.) ;
#56513 = ORIENTED_EDGE('',*,*,#41669,.T.) ;
#56514 = ORIENTED_EDGE('',*,*,#41475,.F.) ;
#56515 = ORIENTED_EDGE('',*,*,#41670,.F.) ;
#56516 = ORIENTED_EDGE('',*,*,#41526,.F.) ;
#56517 = ORIENTED_EDGE('',*,*,#41481,.F.) ;
#56518 = ORIENTED_EDGE('',*,*,#41668,.T.) ;
#56519 = ORIENTED_EDGE('',*,*,#41671,.F.) ;
#56520 = ORIENTED_EDGE('',*,*,#41670,.T.) ;
#56521 = ORIENTED_EDGE('',*,*,#41472,.F.) ;
#56522 = ORIENTED_EDGE('',*,*,#41672,.F.) ;
#56523 = ORIENTED_EDGE('',*,*,#41527,.F.) ;
#56524 = ORIENTED_EDGE('',*,*,#41671,.T.) ;
#56525 = ORIENTED_EDGE('',*,*,#41524,.F.) ;
#56526 = ORIENTED_EDGE('',*,*,#41673,.F.) ;
#56527 = ORIENTED_EDGE('',*,*,#41484,.F.) ;
#56528 = ORIENTED_EDGE('',*,*,#41672,.T.) ;
#56529 = ORIENTED_EDGE('',*,*,#41469,.F.) ;
#56530 = ORIENTED_EDGE('',*,*,#41674,.F.) ;
#56531 = ORIENTED_EDGE('',*,*,#41528,.F.) ;
#56532 = ORIENTED_EDGE('',*,*,#41487,.F.) ;
#56533 = ORIENTED_EDGE('',*,*,#41673,.T.) ;
#56534 = ORIENTED_EDGE('',*,*,#41675,.F.) ;
#56535 = ORIENTED_EDGE('',*,*,#41674,.T.) ;
#56536 = ORIENTED_EDGE('',*,*,#41466,.F.) ;
#56537 = ORIENTED_EDGE('',*,*,#41676,.F.) ;
#56538 = ORIENTED_EDGE('',*,*,#41529,.F.) ;
#56539 = ORIENTED_EDGE('',*,*,#41675,.T.) ;
#56540 = ORIENTED_EDGE('',*,*,#41523,.F.) ;
#56541 = ORIENTED_EDGE('',*,*,#41677,.F.) ;
#56542 = ORIENTED_EDGE('',*,*,#41490,.F.) ;
#56543 = ORIENTED_EDGE('',*,*,#41676,.T.) ;
#56544 = ORIENTED_EDGE('',*,*,#41463,.F.) ;
#56545 = ORIENTED_EDGE('',*,*,#41678,.F.) ;
#56546 = ORIENTED_EDGE('',*,*,#41493,.F.) ;
#56547 = ORIENTED_EDGE('',*,*,#41677,.T.) ;
#56548 = ORIENTED_EDGE('',*,*,#41679,.F.) ;
#56549 = ORIENTED_EDGE('',*,*,#41678,.T.) ;
#56550 = ORIENTED_EDGE('',*,*,#41460,.F.) ;
#56551 = ORIENTED_EDGE('',*,*,#41680,.F.) ;
#56552 = ORIENTED_EDGE('',*,*,#41530,.F.) ;
#56553 = ORIENTED_EDGE('',*,*,#41679,.T.) ;
#56554 = ORIENTED_EDGE('',*,*,#41522,.F.) ;
#56555 = ORIENTED_EDGE('',*,*,#41681,.F.) ;
#56556 = ORIENTED_EDGE('',*,*,#41496,.F.) ;
#56557 = ORIENTED_EDGE('',*,*,#41680,.T.) ;
#56558 = ORIENTED_EDGE('',*,*,#39286,.F.) ;
#56559 = ORIENTED_EDGE('',*,*,#41682,.F.) ;
#56560 = ORIENTED_EDGE('',*,*,#41499,.F.) ;
#56561 = ORIENTED_EDGE('',*,*,#41681,.T.) ;
#56562 = ORIENTED_EDGE('',*,*,#41683,.F.) ;
#56563 = ORIENTED_EDGE('',*,*,#41682,.T.) ;
#56564 = ORIENTED_EDGE('',*,*,#41458,.F.) ;
#56565 = ORIENTED_EDGE('',*,*,#39269,.F.) ;
#56566 = ORIENTED_EDGE('',*,*,#41531,.F.) ;
#56567 = ORIENTED_EDGE('',*,*,#41683,.T.) ;
#56568 = ORIENTED_EDGE('',*,*,#41521,.F.) ;
#56569 = ORIENTED_EDGE('',*,*,#41684,.F.) ;
#56570 = ORIENTED_EDGE('',*,*,#41502,.F.) ;
#56571 = ORIENTED_EDGE('',*,*,#41505,.F.) ;
#56572 = ORIENTED_EDGE('',*,*,#41684,.T.) ;
#56573 = ORIENTED_EDGE('',*,*,#41685,.F.) ;
#56574 = ORIENTED_EDGE('',*,*,#39268,.T.) ;
#56575 = ORIENTED_EDGE('',*,*,#41453,.F.) ;
#56576 = ORIENTED_EDGE('',*,*,#41686,.F.) ;
#56577 = ORIENTED_EDGE('',*,*,#41532,.F.) ;
#56578 = ORIENTED_EDGE('',*,*,#41685,.T.) ;
#56579 = ORIENTED_EDGE('',*,*,#41520,.F.) ;
#56580 = ORIENTED_EDGE('',*,*,#41687,.F.) ;
#56581 = ORIENTED_EDGE('',*,*,#41508,.F.) ;
#56582 = ORIENTED_EDGE('',*,*,#41686,.T.) ;
#56583 = ORIENTED_EDGE('',*,*,#41450,.F.) ;
#56584 = ORIENTED_EDGE('',*,*,#41688,.F.) ;
#56585 = ORIENTED_EDGE('',*,*,#41511,.F.) ;
#56586 = ORIENTED_EDGE('',*,*,#41687,.T.) ;
#56587 = ORIENTED_EDGE('',*,*,#41689,.F.) ;
#56588 = ORIENTED_EDGE('',*,*,#41688,.T.) ;
#56589 = ORIENTED_EDGE('',*,*,#41447,.F.) ;
#56590 = ORIENTED_EDGE('',*,*,#41690,.F.) ;
#56591 = ORIENTED_EDGE('',*,*,#41533,.F.) ;
#56592 = ORIENTED_EDGE('',*,*,#41689,.T.) ;
#56593 = ORIENTED_EDGE('',*,*,#41519,.F.) ;
#56594 = ORIENTED_EDGE('',*,*,#41691,.F.) ;
#56595 = ORIENTED_EDGE('',*,*,#41514,.F.) ;
#56596 = ORIENTED_EDGE('',*,*,#41690,.T.) ;
#56597 = ORIENTED_EDGE('',*,*,#41444,.F.) ;
#56598 = ORIENTED_EDGE('',*,*,#41692,.F.) ;
#56599 = ORIENTED_EDGE('',*,*,#41516,.F.) ;
#56600 = ORIENTED_EDGE('',*,*,#41691,.T.) ;
#56601 = ORIENTED_EDGE('',*,*,#41518,.F.) ;
#56602 = ORIENTED_EDGE('',*,*,#41693,.F.) ;
#56603 = ORIENTED_EDGE('',*,*,#41438,.F.) ;
#56604 = ORIENTED_EDGE('',*,*,#41692,.T.) ;
#56605 = ORIENTED_EDGE('',*,*,#41441,.F.) ;
#56606 = ORIENTED_EDGE('',*,*,#41693,.T.) ;
#56607 = ORIENTED_EDGE('',*,*,#41517,.F.) ;
#56608 = ORIENTED_EDGE('',*,*,#41694,.F.) ;
#56609 = ORIENTED_EDGE('',*,*,#40698,.F.) ;
#56610 = ORIENTED_EDGE('',*,*,#41695,.F.) ;
#56611 = ORIENTED_EDGE('',*,*,#39747,.F.) ;
#56612 = ORIENTED_EDGE('',*,*,#40695,.F.) ;
#56613 = ORIENTED_EDGE('',*,*,#41694,.T.) ;
#56614 = ORIENTED_EDGE('',*,*,#41696,.F.) ;
#56615 = ORIENTED_EDGE('',*,*,#41695,.T.) ;
#56616 = ORIENTED_EDGE('',*,*,#40701,.F.) ;
#56617 = ORIENTED_EDGE('',*,*,#41697,.F.) ;
#56618 = ORIENTED_EDGE('',*,*,#41696,.T.) ;
#56619 = ORIENTED_EDGE('',*,*,#39746,.F.) ;
#56620 = ORIENTED_EDGE('',*,*,#41698,.F.) ;
#56621 = ORIENTED_EDGE('',*,*,#40692,.F.) ;
#56622 = ORIENTED_EDGE('',*,*,#41697,.T.) ;
#56623 = ORIENTED_EDGE('',*,*,#40704,.F.) ;
#56624 = ORIENTED_EDGE('',*,*,#41699,.F.) ;
#56625 = ORIENTED_EDGE('',*,*,#39748,.F.) ;
#56626 = ORIENTED_EDGE('',*,*,#41698,.T.) ;
#56627 = ORIENTED_EDGE('',*,*,#39745,.F.) ;
#56628 = ORIENTED_EDGE('',*,*,#41700,.F.) ;
#56629 = ORIENTED_EDGE('',*,*,#40689,.F.) ;
#56630 = ORIENTED_EDGE('',*,*,#41699,.T.) ;
#56631 = ORIENTED_EDGE('',*,*,#40707,.F.) ;
#56632 = ORIENTED_EDGE('',*,*,#41701,.F.) ;
#56633 = ORIENTED_EDGE('',*,*,#39749,.F.) ;
#56634 = ORIENTED_EDGE('',*,*,#41700,.T.) ;
#56635 = ORIENTED_EDGE('',*,*,#39744,.F.) ;
#56636 = ORIENTED_EDGE('',*,*,#39263,.F.) ;
#56637 = ORIENTED_EDGE('',*,*,#40686,.F.) ;
#56638 = ORIENTED_EDGE('',*,*,#41701,.T.) ;
#56639 = ORIENTED_EDGE('',*,*,#40710,.F.) ;
#56640 = ORIENTED_EDGE('',*,*,#41702,.F.) ;
#56641 = ORIENTED_EDGE('',*,*,#39750,.F.) ;
#56642 = ORIENTED_EDGE('',*,*,#41702,.T.) ;
#56643 = ORIENTED_EDGE('',*,*,#40713,.F.) ;
#56644 = ORIENTED_EDGE('',*,*,#41703,.F.) ;
#56645 = ORIENTED_EDGE('',*,*,#39751,.F.) ;
#56646 = ORIENTED_EDGE('',*,*,#39261,.T.) ;
#56647 = ORIENTED_EDGE('',*,*,#39743,.F.) ;
#56648 = ORIENTED_EDGE('',*,*,#41704,.F.) ;
#56649 = ORIENTED_EDGE('',*,*,#40683,.F.) ;
#56650 = ORIENTED_EDGE('',*,*,#41703,.T.) ;
#56651 = ORIENTED_EDGE('',*,*,#40716,.F.) ;
#56652 = ORIENTED_EDGE('',*,*,#41705,.F.) ;
#56653 = ORIENTED_EDGE('',*,*,#39752,.F.) ;
#56654 = ORIENTED_EDGE('',*,*,#41704,.T.) ;
#56655 = ORIENTED_EDGE('',*,*,#39742,.F.) ;
#56656 = ORIENTED_EDGE('',*,*,#41706,.F.) ;
#56657 = ORIENTED_EDGE('',*,*,#40681,.F.) ;
#56658 = ORIENTED_EDGE('',*,*,#41705,.T.) ;
#56659 = ORIENTED_EDGE('',*,*,#40719,.F.) ;
#56660 = ORIENTED_EDGE('',*,*,#41707,.F.) ;
#56661 = ORIENTED_EDGE('',*,*,#39753,.F.) ;
#56662 = ORIENTED_EDGE('',*,*,#41706,.T.) ;
#56663 = ORIENTED_EDGE('',*,*,#39741,.F.) ;
#56664 = ORIENTED_EDGE('',*,*,#41708,.F.) ;
#56665 = ORIENTED_EDGE('',*,*,#40679,.F.) ;
#56666 = ORIENTED_EDGE('',*,*,#41707,.T.) ;
#56667 = ORIENTED_EDGE('',*,*,#40722,.F.) ;
#56668 = ORIENTED_EDGE('',*,*,#41709,.F.) ;
#56669 = ORIENTED_EDGE('',*,*,#39754,.F.) ;
#56670 = ORIENTED_EDGE('',*,*,#41708,.T.) ;
#56671 = ORIENTED_EDGE('',*,*,#39740,.F.) ;
#56672 = ORIENTED_EDGE('',*,*,#41710,.F.) ;
#56673 = ORIENTED_EDGE('',*,*,#40676,.F.) ;
#56674 = ORIENTED_EDGE('',*,*,#41709,.T.) ;
#56675 = ORIENTED_EDGE('',*,*,#40725,.F.) ;
#56676 = ORIENTED_EDGE('',*,*,#41711,.F.) ;
#56677 = ORIENTED_EDGE('',*,*,#39755,.F.) ;
#56678 = ORIENTED_EDGE('',*,*,#41710,.T.) ;
#56679 = ORIENTED_EDGE('',*,*,#39739,.F.) ;
#56680 = ORIENTED_EDGE('',*,*,#41712,.F.) ;
#56681 = ORIENTED_EDGE('',*,*,#40673,.F.) ;
#56682 = ORIENTED_EDGE('',*,*,#41711,.T.) ;
#56683 = ORIENTED_EDGE('',*,*,#40728,.F.) ;
#56684 = ORIENTED_EDGE('',*,*,#41713,.F.) ;
#56685 = ORIENTED_EDGE('',*,*,#39756,.F.) ;
#56686 = ORIENTED_EDGE('',*,*,#40670,.F.) ;
#56687 = ORIENTED_EDGE('',*,*,#41712,.T.) ;
#56688 = ORIENTED_EDGE('',*,*,#41714,.F.) ;
#56689 = ORIENTED_EDGE('',*,*,#41713,.T.) ;
#56690 = ORIENTED_EDGE('',*,*,#40731,.F.) ;
#56691 = ORIENTED_EDGE('',*,*,#41715,.F.) ;
#56692 = ORIENTED_EDGE('',*,*,#39757,.F.) ;
#56693 = ORIENTED_EDGE('',*,*,#41714,.T.) ;
#56694 = ORIENTED_EDGE('',*,*,#39738,.F.) ;
#56695 = ORIENTED_EDGE('',*,*,#41716,.F.) ;
#56696 = ORIENTED_EDGE('',*,*,#40667,.F.) ;
#56697 = ORIENTED_EDGE('',*,*,#41715,.T.) ;
#56698 = ORIENTED_EDGE('',*,*,#40734,.F.) ;
#56699 = ORIENTED_EDGE('',*,*,#41717,.F.) ;
#56700 = ORIENTED_EDGE('',*,*,#39758,.F.) ;
#56701 = ORIENTED_EDGE('',*,*,#40664,.F.) ;
#56702 = ORIENTED_EDGE('',*,*,#41716,.T.) ;
#56703 = ORIENTED_EDGE('',*,*,#41718,.F.) ;
#56704 = ORIENTED_EDGE('',*,*,#41717,.T.) ;
#56705 = ORIENTED_EDGE('',*,*,#40737,.F.) ;
#56706 = ORIENTED_EDGE('',*,*,#41719,.F.) ;
#56707 = ORIENTED_EDGE('',*,*,#39736,.F.) ;
#56708 = ORIENTED_EDGE('',*,*,#41718,.T.) ;
#56709 = ORIENTED_EDGE('',*,*,#39737,.F.) ;
#56710 = ORIENTED_EDGE('',*,*,#41719,.T.) ;
#56711 = ORIENTED_EDGE('',*,*,#40739,.F.) ;
#56712 = ORIENTED_EDGE('',*,*,#41720,.F.) ;
#56713 = ORIENTED_EDGE('',*,*,#40795,.F.) ;
#56714 = ORIENTED_EDGE('',*,*,#41721,.F.) ;
#56715 = ORIENTED_EDGE('',*,*,#39770,.F.) ;
#56716 = ORIENTED_EDGE('',*,*,#40792,.F.) ;
#56717 = ORIENTED_EDGE('',*,*,#41720,.T.) ;
#56718 = ORIENTED_EDGE('',*,*,#41722,.F.) ;
#56719 = ORIENTED_EDGE('',*,*,#41721,.T.) ;
#56720 = ORIENTED_EDGE('',*,*,#40798,.F.) ;
#56721 = ORIENTED_EDGE('',*,*,#41723,.F.) ;
#56722 = ORIENTED_EDGE('',*,*,#41722,.T.) ;
#56723 = ORIENTED_EDGE('',*,*,#39769,.F.) ;
#56724 = ORIENTED_EDGE('',*,*,#41724,.F.) ;
#56725 = ORIENTED_EDGE('',*,*,#40789,.F.) ;
#56726 = ORIENTED_EDGE('',*,*,#41723,.T.) ;
#56727 = ORIENTED_EDGE('',*,*,#40801,.F.) ;
#56728 = ORIENTED_EDGE('',*,*,#41725,.F.) ;
#56729 = ORIENTED_EDGE('',*,*,#39771,.F.) ;
#56730 = ORIENTED_EDGE('',*,*,#41724,.T.) ;
#56731 = ORIENTED_EDGE('',*,*,#39768,.F.) ;
#56732 = ORIENTED_EDGE('',*,*,#41726,.F.) ;
#56733 = ORIENTED_EDGE('',*,*,#40786,.F.) ;
#56734 = ORIENTED_EDGE('',*,*,#41725,.T.) ;
#56735 = ORIENTED_EDGE('',*,*,#40804,.F.) ;
#56736 = ORIENTED_EDGE('',*,*,#41727,.F.) ;
#56737 = ORIENTED_EDGE('',*,*,#39772,.F.) ;
#56738 = ORIENTED_EDGE('',*,*,#41726,.T.) ;
#56739 = ORIENTED_EDGE('',*,*,#39767,.F.) ;
#56740 = ORIENTED_EDGE('',*,*,#39259,.F.) ;
#56741 = ORIENTED_EDGE('',*,*,#40783,.F.) ;
#56742 = ORIENTED_EDGE('',*,*,#41727,.T.) ;
#56743 = ORIENTED_EDGE('',*,*,#40807,.F.) ;
#56744 = ORIENTED_EDGE('',*,*,#41728,.F.) ;
#56745 = ORIENTED_EDGE('',*,*,#39773,.F.) ;
#56746 = ORIENTED_EDGE('',*,*,#41728,.T.) ;
#56747 = ORIENTED_EDGE('',*,*,#40810,.F.) ;
#56748 = ORIENTED_EDGE('',*,*,#41729,.F.) ;
#56749 = ORIENTED_EDGE('',*,*,#39774,.F.) ;
#56750 = ORIENTED_EDGE('',*,*,#39257,.T.) ;
#56751 = ORIENTED_EDGE('',*,*,#39766,.F.) ;
#56752 = ORIENTED_EDGE('',*,*,#41730,.F.) ;
#56753 = ORIENTED_EDGE('',*,*,#40780,.F.) ;
#56754 = ORIENTED_EDGE('',*,*,#41729,.T.) ;
#56755 = ORIENTED_EDGE('',*,*,#40813,.F.) ;
#56756 = ORIENTED_EDGE('',*,*,#41731,.F.) ;
#56757 = ORIENTED_EDGE('',*,*,#39775,.F.) ;
#56758 = ORIENTED_EDGE('',*,*,#41730,.T.) ;
#56759 = ORIENTED_EDGE('',*,*,#39765,.F.) ;
#56760 = ORIENTED_EDGE('',*,*,#41732,.F.) ;
#56761 = ORIENTED_EDGE('',*,*,#40778,.F.) ;
#56762 = ORIENTED_EDGE('',*,*,#41731,.T.) ;
#56763 = ORIENTED_EDGE('',*,*,#40816,.F.) ;
#56764 = ORIENTED_EDGE('',*,*,#41733,.F.) ;
#56765 = ORIENTED_EDGE('',*,*,#39776,.F.) ;
#56766 = ORIENTED_EDGE('',*,*,#41732,.T.) ;
#56767 = ORIENTED_EDGE('',*,*,#39764,.F.) ;
#56768 = ORIENTED_EDGE('',*,*,#41734,.F.) ;
#56769 = ORIENTED_EDGE('',*,*,#40776,.F.) ;
#56770 = ORIENTED_EDGE('',*,*,#41733,.T.) ;
#56771 = ORIENTED_EDGE('',*,*,#40819,.F.) ;
#56772 = ORIENTED_EDGE('',*,*,#41735,.F.) ;
#56773 = ORIENTED_EDGE('',*,*,#39777,.F.) ;
#56774 = ORIENTED_EDGE('',*,*,#41734,.T.) ;
#56775 = ORIENTED_EDGE('',*,*,#39763,.F.) ;
#56776 = ORIENTED_EDGE('',*,*,#41736,.F.) ;
#56777 = ORIENTED_EDGE('',*,*,#40773,.F.) ;
#56778 = ORIENTED_EDGE('',*,*,#41735,.T.) ;
#56779 = ORIENTED_EDGE('',*,*,#40822,.F.) ;
#56780 = ORIENTED_EDGE('',*,*,#41737,.F.) ;
#56781 = ORIENTED_EDGE('',*,*,#39778,.F.) ;
#56782 = ORIENTED_EDGE('',*,*,#41736,.T.) ;
#56783 = ORIENTED_EDGE('',*,*,#39762,.F.) ;
#56784 = ORIENTED_EDGE('',*,*,#41738,.F.) ;
#56785 = ORIENTED_EDGE('',*,*,#40770,.F.) ;
#56786 = ORIENTED_EDGE('',*,*,#41737,.T.) ;
#56787 = ORIENTED_EDGE('',*,*,#40825,.F.) ;
#56788 = ORIENTED_EDGE('',*,*,#41739,.F.) ;
#56789 = ORIENTED_EDGE('',*,*,#39779,.F.) ;
#56790 = ORIENTED_EDGE('',*,*,#40767,.F.) ;
#56791 = ORIENTED_EDGE('',*,*,#41738,.T.) ;
#56792 = ORIENTED_EDGE('',*,*,#41740,.F.) ;
#56793 = ORIENTED_EDGE('',*,*,#41739,.T.) ;
#56794 = ORIENTED_EDGE('',*,*,#40828,.F.) ;
#56795 = ORIENTED_EDGE('',*,*,#41741,.F.) ;
#56796 = ORIENTED_EDGE('',*,*,#39780,.F.) ;
#56797 = ORIENTED_EDGE('',*,*,#41740,.T.) ;
#56798 = ORIENTED_EDGE('',*,*,#39761,.F.) ;
#56799 = ORIENTED_EDGE('',*,*,#41742,.F.) ;
#56800 = ORIENTED_EDGE('',*,*,#40764,.F.) ;
#56801 = ORIENTED_EDGE('',*,*,#41741,.T.) ;
#56802 = ORIENTED_EDGE('',*,*,#40831,.F.) ;
#56803 = ORIENTED_EDGE('',*,*,#41743,.F.) ;
#56804 = ORIENTED_EDGE('',*,*,#39781,.F.) ;
#56805 = ORIENTED_EDGE('',*,*,#40761,.F.) ;
#56806 = ORIENTED_EDGE('',*,*,#41742,.T.) ;
#56807 = ORIENTED_EDGE('',*,*,#41744,.F.) ;
#56808 = ORIENTED_EDGE('',*,*,#41743,.T.) ;
#56809 = ORIENTED_EDGE('',*,*,#40834,.F.) ;
#56810 = ORIENTED_EDGE('',*,*,#41745,.F.) ;
#56811 = ORIENTED_EDGE('',*,*,#39759,.F.) ;
#56812 = ORIENTED_EDGE('',*,*,#41744,.T.) ;
#56813 = ORIENTED_EDGE('',*,*,#39760,.F.) ;
#56814 = ORIENTED_EDGE('',*,*,#41745,.T.) ;
#56815 = ORIENTED_EDGE('',*,*,#40836,.F.) ;
#56816 = ORIENTED_EDGE('',*,*,#41746,.F.) ;
#56817 = ORIENTED_EDGE('',*,*,#40892,.F.) ;
#56818 = ORIENTED_EDGE('',*,*,#41747,.F.) ;
#56819 = ORIENTED_EDGE('',*,*,#39793,.F.) ;
#56820 = ORIENTED_EDGE('',*,*,#40889,.F.) ;
#56821 = ORIENTED_EDGE('',*,*,#41746,.T.) ;
#56822 = ORIENTED_EDGE('',*,*,#41748,.F.) ;
#56823 = ORIENTED_EDGE('',*,*,#41747,.T.) ;
#56824 = ORIENTED_EDGE('',*,*,#40895,.F.) ;
#56825 = ORIENTED_EDGE('',*,*,#41749,.F.) ;
#56826 = ORIENTED_EDGE('',*,*,#41748,.T.) ;
#56827 = ORIENTED_EDGE('',*,*,#39792,.F.) ;
#56828 = ORIENTED_EDGE('',*,*,#41750,.F.) ;
#56829 = ORIENTED_EDGE('',*,*,#40886,.F.) ;
#56830 = ORIENTED_EDGE('',*,*,#41749,.T.) ;
#56831 = ORIENTED_EDGE('',*,*,#40898,.F.) ;
#56832 = ORIENTED_EDGE('',*,*,#41751,.F.) ;
#56833 = ORIENTED_EDGE('',*,*,#39794,.F.) ;
#56834 = ORIENTED_EDGE('',*,*,#41750,.T.) ;
#56835 = ORIENTED_EDGE('',*,*,#39791,.F.) ;
#56836 = ORIENTED_EDGE('',*,*,#41752,.F.) ;
#56837 = ORIENTED_EDGE('',*,*,#40883,.F.) ;
#56838 = ORIENTED_EDGE('',*,*,#41751,.T.) ;
#56839 = ORIENTED_EDGE('',*,*,#40901,.F.) ;
#56840 = ORIENTED_EDGE('',*,*,#41753,.F.) ;
#56841 = ORIENTED_EDGE('',*,*,#39795,.F.) ;
#56842 = ORIENTED_EDGE('',*,*,#41752,.T.) ;
#56843 = ORIENTED_EDGE('',*,*,#39790,.F.) ;
#56844 = ORIENTED_EDGE('',*,*,#39255,.F.) ;
#56845 = ORIENTED_EDGE('',*,*,#40880,.F.) ;
#56846 = ORIENTED_EDGE('',*,*,#41753,.T.) ;
#56847 = ORIENTED_EDGE('',*,*,#40904,.F.) ;
#56848 = ORIENTED_EDGE('',*,*,#41754,.F.) ;
#56849 = ORIENTED_EDGE('',*,*,#39796,.F.) ;
#56850 = ORIENTED_EDGE('',*,*,#41754,.T.) ;
#56851 = ORIENTED_EDGE('',*,*,#40907,.F.) ;
#56852 = ORIENTED_EDGE('',*,*,#41755,.F.) ;
#56853 = ORIENTED_EDGE('',*,*,#39797,.F.) ;
#56854 = ORIENTED_EDGE('',*,*,#39253,.T.) ;
#56855 = ORIENTED_EDGE('',*,*,#39789,.F.) ;
#56856 = ORIENTED_EDGE('',*,*,#41756,.F.) ;
#56857 = ORIENTED_EDGE('',*,*,#40877,.F.) ;
#56858 = ORIENTED_EDGE('',*,*,#41755,.T.) ;
#56859 = ORIENTED_EDGE('',*,*,#40910,.F.) ;
#56860 = ORIENTED_EDGE('',*,*,#41757,.F.) ;
#56861 = ORIENTED_EDGE('',*,*,#39798,.F.) ;
#56862 = ORIENTED_EDGE('',*,*,#41756,.T.) ;
#56863 = ORIENTED_EDGE('',*,*,#39788,.F.) ;
#56864 = ORIENTED_EDGE('',*,*,#41758,.F.) ;
#56865 = ORIENTED_EDGE('',*,*,#40875,.F.) ;
#56866 = ORIENTED_EDGE('',*,*,#41757,.T.) ;
#56867 = ORIENTED_EDGE('',*,*,#40913,.F.) ;
#56868 = ORIENTED_EDGE('',*,*,#41759,.F.) ;
#56869 = ORIENTED_EDGE('',*,*,#39799,.F.) ;
#56870 = ORIENTED_EDGE('',*,*,#41758,.T.) ;
#56871 = ORIENTED_EDGE('',*,*,#39787,.F.) ;
#56872 = ORIENTED_EDGE('',*,*,#41760,.F.) ;
#56873 = ORIENTED_EDGE('',*,*,#40873,.F.) ;
#56874 = ORIENTED_EDGE('',*,*,#41759,.T.) ;
#56875 = ORIENTED_EDGE('',*,*,#40916,.F.) ;
#56876 = ORIENTED_EDGE('',*,*,#41761,.F.) ;
#56877 = ORIENTED_EDGE('',*,*,#39800,.F.) ;
#56878 = ORIENTED_EDGE('',*,*,#41760,.T.) ;
#56879 = ORIENTED_EDGE('',*,*,#39786,.F.) ;
#56880 = ORIENTED_EDGE('',*,*,#41762,.F.) ;
#56881 = ORIENTED_EDGE('',*,*,#40870,.F.) ;
#56882 = ORIENTED_EDGE('',*,*,#41761,.T.) ;
#56883 = ORIENTED_EDGE('',*,*,#40919,.F.) ;
#56884 = ORIENTED_EDGE('',*,*,#41763,.F.) ;
#56885 = ORIENTED_EDGE('',*,*,#39801,.F.) ;
#56886 = ORIENTED_EDGE('',*,*,#41762,.T.) ;
#56887 = ORIENTED_EDGE('',*,*,#39785,.F.) ;
#56888 = ORIENTED_EDGE('',*,*,#41764,.F.) ;
#56889 = ORIENTED_EDGE('',*,*,#40867,.F.) ;
#56890 = ORIENTED_EDGE('',*,*,#41763,.T.) ;
#56891 = ORIENTED_EDGE('',*,*,#40922,.F.) ;
#56892 = ORIENTED_EDGE('',*,*,#41765,.F.) ;
#56893 = ORIENTED_EDGE('',*,*,#39802,.F.) ;
#56894 = ORIENTED_EDGE('',*,*,#40864,.F.) ;
#56895 = ORIENTED_EDGE('',*,*,#41764,.T.) ;
#56896 = ORIENTED_EDGE('',*,*,#41766,.F.) ;
#56897 = ORIENTED_EDGE('',*,*,#41765,.T.) ;
#56898 = ORIENTED_EDGE('',*,*,#40925,.F.) ;
#56899 = ORIENTED_EDGE('',*,*,#41767,.F.) ;
#56900 = ORIENTED_EDGE('',*,*,#39803,.F.) ;
#56901 = ORIENTED_EDGE('',*,*,#41766,.T.) ;
#56902 = ORIENTED_EDGE('',*,*,#39784,.F.) ;
#56903 = ORIENTED_EDGE('',*,*,#41768,.F.) ;
#56904 = ORIENTED_EDGE('',*,*,#40861,.F.) ;
#56905 = ORIENTED_EDGE('',*,*,#41767,.T.) ;
#56906 = ORIENTED_EDGE('',*,*,#40928,.F.) ;
#56907 = ORIENTED_EDGE('',*,*,#41769,.F.) ;
#56908 = ORIENTED_EDGE('',*,*,#39804,.F.) ;
#56909 = ORIENTED_EDGE('',*,*,#40858,.F.) ;
#56910 = ORIENTED_EDGE('',*,*,#41768,.T.) ;
#56911 = ORIENTED_EDGE('',*,*,#41770,.F.) ;
#56912 = ORIENTED_EDGE('',*,*,#41769,.T.) ;
#56913 = ORIENTED_EDGE('',*,*,#40931,.F.) ;
#56914 = ORIENTED_EDGE('',*,*,#41771,.F.) ;
#56915 = ORIENTED_EDGE('',*,*,#39782,.F.) ;
#56916 = ORIENTED_EDGE('',*,*,#41770,.T.) ;
#56917 = ORIENTED_EDGE('',*,*,#39783,.F.) ;
#56918 = ORIENTED_EDGE('',*,*,#41771,.T.) ;
#56919 = ORIENTED_EDGE('',*,*,#40933,.F.) ;
#56920 = ORIENTED_EDGE('',*,*,#41772,.F.) ;
#56921 = ORIENTED_EDGE('',*,*,#40989,.F.) ;
#56922 = ORIENTED_EDGE('',*,*,#41773,.F.) ;
#56923 = ORIENTED_EDGE('',*,*,#39816,.F.) ;
#56924 = ORIENTED_EDGE('',*,*,#40986,.F.) ;
#56925 = ORIENTED_EDGE('',*,*,#41772,.T.) ;
#56926 = ORIENTED_EDGE('',*,*,#41774,.F.) ;
#56927 = ORIENTED_EDGE('',*,*,#41773,.T.) ;
#56928 = ORIENTED_EDGE('',*,*,#40992,.F.) ;
#56929 = ORIENTED_EDGE('',*,*,#41775,.F.) ;
#56930 = ORIENTED_EDGE('',*,*,#41774,.T.) ;
#56931 = ORIENTED_EDGE('',*,*,#39815,.F.) ;
#56932 = ORIENTED_EDGE('',*,*,#41776,.F.) ;
#56933 = ORIENTED_EDGE('',*,*,#40983,.F.) ;
#56934 = ORIENTED_EDGE('',*,*,#41775,.T.) ;
#56935 = ORIENTED_EDGE('',*,*,#40995,.F.) ;
#56936 = ORIENTED_EDGE('',*,*,#41777,.F.) ;
#56937 = ORIENTED_EDGE('',*,*,#39817,.F.) ;
#56938 = ORIENTED_EDGE('',*,*,#41776,.T.) ;
#56939 = ORIENTED_EDGE('',*,*,#39814,.F.) ;
#56940 = ORIENTED_EDGE('',*,*,#41778,.F.) ;
#56941 = ORIENTED_EDGE('',*,*,#40980,.F.) ;
#56942 = ORIENTED_EDGE('',*,*,#41777,.T.) ;
#56943 = ORIENTED_EDGE('',*,*,#40998,.F.) ;
#56944 = ORIENTED_EDGE('',*,*,#41779,.F.) ;
#56945 = ORIENTED_EDGE('',*,*,#39818,.F.) ;
#56946 = ORIENTED_EDGE('',*,*,#41778,.T.) ;
#56947 = ORIENTED_EDGE('',*,*,#39813,.F.) ;
#56948 = ORIENTED_EDGE('',*,*,#39251,.F.) ;
#56949 = ORIENTED_EDGE('',*,*,#40977,.F.) ;
#56950 = ORIENTED_EDGE('',*,*,#41779,.T.) ;
#56951 = ORIENTED_EDGE('',*,*,#41001,.F.) ;
#56952 = ORIENTED_EDGE('',*,*,#41780,.F.) ;
#56953 = ORIENTED_EDGE('',*,*,#39819,.F.) ;
#56954 = ORIENTED_EDGE('',*,*,#41780,.T.) ;
#56955 = ORIENTED_EDGE('',*,*,#41004,.F.) ;
#56956 = ORIENTED_EDGE('',*,*,#41781,.F.) ;
#56957 = ORIENTED_EDGE('',*,*,#39820,.F.) ;
#56958 = ORIENTED_EDGE('',*,*,#39249,.T.) ;
#56959 = ORIENTED_EDGE('',*,*,#39812,.F.) ;
#56960 = ORIENTED_EDGE('',*,*,#41782,.F.) ;
#56961 = ORIENTED_EDGE('',*,*,#40974,.F.) ;
#56962 = ORIENTED_EDGE('',*,*,#41781,.T.) ;
#56963 = ORIENTED_EDGE('',*,*,#41007,.F.) ;
#56964 = ORIENTED_EDGE('',*,*,#41783,.F.) ;
#56965 = ORIENTED_EDGE('',*,*,#39821,.F.) ;
#56966 = ORIENTED_EDGE('',*,*,#41782,.T.) ;
#56967 = ORIENTED_EDGE('',*,*,#39811,.F.) ;
#56968 = ORIENTED_EDGE('',*,*,#41784,.F.) ;
#56969 = ORIENTED_EDGE('',*,*,#40972,.F.) ;
#56970 = ORIENTED_EDGE('',*,*,#41783,.T.) ;
#56971 = ORIENTED_EDGE('',*,*,#41010,.F.) ;
#56972 = ORIENTED_EDGE('',*,*,#41785,.F.) ;
#56973 = ORIENTED_EDGE('',*,*,#39822,.F.) ;
#56974 = ORIENTED_EDGE('',*,*,#41784,.T.) ;
#56975 = ORIENTED_EDGE('',*,*,#39810,.F.) ;
#56976 = ORIENTED_EDGE('',*,*,#41786,.F.) ;
#56977 = ORIENTED_EDGE('',*,*,#40970,.F.) ;
#56978 = ORIENTED_EDGE('',*,*,#41785,.T.) ;
#56979 = ORIENTED_EDGE('',*,*,#41013,.F.) ;
#56980 = ORIENTED_EDGE('',*,*,#41787,.F.) ;
#56981 = ORIENTED_EDGE('',*,*,#39823,.F.) ;
#56982 = ORIENTED_EDGE('',*,*,#41786,.T.) ;
#56983 = ORIENTED_EDGE('',*,*,#39809,.F.) ;
#56984 = ORIENTED_EDGE('',*,*,#41788,.F.) ;
#56985 = ORIENTED_EDGE('',*,*,#40967,.F.) ;
#56986 = ORIENTED_EDGE('',*,*,#41787,.T.) ;
#56987 = ORIENTED_EDGE('',*,*,#41016,.F.) ;
#56988 = ORIENTED_EDGE('',*,*,#41789,.F.) ;
#56989 = ORIENTED_EDGE('',*,*,#39824,.F.) ;
#56990 = ORIENTED_EDGE('',*,*,#41788,.T.) ;
#56991 = ORIENTED_EDGE('',*,*,#39808,.F.) ;
#56992 = ORIENTED_EDGE('',*,*,#41790,.F.) ;
#56993 = ORIENTED_EDGE('',*,*,#40964,.F.) ;
#56994 = ORIENTED_EDGE('',*,*,#41789,.T.) ;
#56995 = ORIENTED_EDGE('',*,*,#41019,.F.) ;
#56996 = ORIENTED_EDGE('',*,*,#41791,.F.) ;
#56997 = ORIENTED_EDGE('',*,*,#39825,.F.) ;
#56998 = ORIENTED_EDGE('',*,*,#40961,.F.) ;
#56999 = ORIENTED_EDGE('',*,*,#41790,.T.) ;
#57000 = ORIENTED_EDGE('',*,*,#41792,.F.) ;
#57001 = ORIENTED_EDGE('',*,*,#41791,.T.) ;
#57002 = ORIENTED_EDGE('',*,*,#41022,.F.) ;
#57003 = ORIENTED_EDGE('',*,*,#41793,.F.) ;
#57004 = ORIENTED_EDGE('',*,*,#39826,.F.) ;
#57005 = ORIENTED_EDGE('',*,*,#41792,.T.) ;
#57006 = ORIENTED_EDGE('',*,*,#39807,.F.) ;
#57007 = ORIENTED_EDGE('',*,*,#41794,.F.) ;
#57008 = ORIENTED_EDGE('',*,*,#40958,.F.) ;
#57009 = ORIENTED_EDGE('',*,*,#41793,.T.) ;
#57010 = ORIENTED_EDGE('',*,*,#41025,.F.) ;
#57011 = ORIENTED_EDGE('',*,*,#41795,.F.) ;
#57012 = ORIENTED_EDGE('',*,*,#39827,.F.) ;
#57013 = ORIENTED_EDGE('',*,*,#40955,.F.) ;
#57014 = ORIENTED_EDGE('',*,*,#41794,.T.) ;
#57015 = ORIENTED_EDGE('',*,*,#41796,.F.) ;
#57016 = ORIENTED_EDGE('',*,*,#41795,.T.) ;
#57017 = ORIENTED_EDGE('',*,*,#41028,.F.) ;
#57018 = ORIENTED_EDGE('',*,*,#41797,.F.) ;
#57019 = ORIENTED_EDGE('',*,*,#39805,.F.) ;
#57020 = ORIENTED_EDGE('',*,*,#41796,.T.) ;
#57021 = ORIENTED_EDGE('',*,*,#39806,.F.) ;
#57022 = ORIENTED_EDGE('',*,*,#41797,.T.) ;
#57023 = ORIENTED_EDGE('',*,*,#41030,.F.) ;
#57024 = ORIENTED_EDGE('',*,*,#41798,.F.) ;
#57025 = ORIENTED_EDGE('',*,*,#41086,.F.) ;
#57026 = ORIENTED_EDGE('',*,*,#41799,.F.) ;
#57027 = ORIENTED_EDGE('',*,*,#39839,.F.) ;
#57028 = ORIENTED_EDGE('',*,*,#41083,.F.) ;
#57029 = ORIENTED_EDGE('',*,*,#41798,.T.) ;
#57030 = ORIENTED_EDGE('',*,*,#41800,.F.) ;
#57031 = ORIENTED_EDGE('',*,*,#41799,.T.) ;
#57032 = ORIENTED_EDGE('',*,*,#41089,.F.) ;
#57033 = ORIENTED_EDGE('',*,*,#41801,.F.) ;
#57034 = ORIENTED_EDGE('',*,*,#41800,.T.) ;
#57035 = ORIENTED_EDGE('',*,*,#39838,.F.) ;
#57036 = ORIENTED_EDGE('',*,*,#41802,.F.) ;
#57037 = ORIENTED_EDGE('',*,*,#41080,.F.) ;
#57038 = ORIENTED_EDGE('',*,*,#41801,.T.) ;
#57039 = ORIENTED_EDGE('',*,*,#41092,.F.) ;
#57040 = ORIENTED_EDGE('',*,*,#41803,.F.) ;
#57041 = ORIENTED_EDGE('',*,*,#39840,.F.) ;
#57042 = ORIENTED_EDGE('',*,*,#41802,.T.) ;
#57043 = ORIENTED_EDGE('',*,*,#39837,.F.) ;
#57044 = ORIENTED_EDGE('',*,*,#41804,.F.) ;
#57045 = ORIENTED_EDGE('',*,*,#41077,.F.) ;
#57046 = ORIENTED_EDGE('',*,*,#41803,.T.) ;
#57047 = ORIENTED_EDGE('',*,*,#41095,.F.) ;
#57048 = ORIENTED_EDGE('',*,*,#41805,.F.) ;
#57049 = ORIENTED_EDGE('',*,*,#39841,.F.) ;
#57050 = ORIENTED_EDGE('',*,*,#41804,.T.) ;
#57051 = ORIENTED_EDGE('',*,*,#39836,.F.) ;
#57052 = ORIENTED_EDGE('',*,*,#39247,.F.) ;
#57053 = ORIENTED_EDGE('',*,*,#41074,.F.) ;
#57054 = ORIENTED_EDGE('',*,*,#41805,.T.) ;
#57055 = ORIENTED_EDGE('',*,*,#41098,.F.) ;
#57056 = ORIENTED_EDGE('',*,*,#41806,.F.) ;
#57057 = ORIENTED_EDGE('',*,*,#39842,.F.) ;
#57058 = ORIENTED_EDGE('',*,*,#41806,.T.) ;
#57059 = ORIENTED_EDGE('',*,*,#41101,.F.) ;
#57060 = ORIENTED_EDGE('',*,*,#41807,.F.) ;
#57061 = ORIENTED_EDGE('',*,*,#39843,.F.) ;
#57062 = ORIENTED_EDGE('',*,*,#39245,.T.) ;
#57063 = ORIENTED_EDGE('',*,*,#39835,.F.) ;
#57064 = ORIENTED_EDGE('',*,*,#41808,.F.) ;
#57065 = ORIENTED_EDGE('',*,*,#41071,.F.) ;
#57066 = ORIENTED_EDGE('',*,*,#41807,.T.) ;
#57067 = ORIENTED_EDGE('',*,*,#41104,.F.) ;
#57068 = ORIENTED_EDGE('',*,*,#41809,.F.) ;
#57069 = ORIENTED_EDGE('',*,*,#39844,.F.) ;
#57070 = ORIENTED_EDGE('',*,*,#41808,.T.) ;
#57071 = ORIENTED_EDGE('',*,*,#39834,.F.) ;
#57072 = ORIENTED_EDGE('',*,*,#41810,.F.) ;
#57073 = ORIENTED_EDGE('',*,*,#41069,.F.) ;
#57074 = ORIENTED_EDGE('',*,*,#41809,.T.) ;
#57075 = ORIENTED_EDGE('',*,*,#41107,.F.) ;
#57076 = ORIENTED_EDGE('',*,*,#41811,.F.) ;
#57077 = ORIENTED_EDGE('',*,*,#39845,.F.) ;
#57078 = ORIENTED_EDGE('',*,*,#41810,.T.) ;
#57079 = ORIENTED_EDGE('',*,*,#39833,.F.) ;
#57080 = ORIENTED_EDGE('',*,*,#41812,.F.) ;
#57081 = ORIENTED_EDGE('',*,*,#41067,.F.) ;
#57082 = ORIENTED_EDGE('',*,*,#41811,.T.) ;
#57083 = ORIENTED_EDGE('',*,*,#41110,.F.) ;
#57084 = ORIENTED_EDGE('',*,*,#41813,.F.) ;
#57085 = ORIENTED_EDGE('',*,*,#39846,.F.) ;
#57086 = ORIENTED_EDGE('',*,*,#41812,.T.) ;
#57087 = ORIENTED_EDGE('',*,*,#39832,.F.) ;
#57088 = ORIENTED_EDGE('',*,*,#41814,.F.) ;
#57089 = ORIENTED_EDGE('',*,*,#41064,.F.) ;
#57090 = ORIENTED_EDGE('',*,*,#41813,.T.) ;
#57091 = ORIENTED_EDGE('',*,*,#41113,.F.) ;
#57092 = ORIENTED_EDGE('',*,*,#41815,.F.) ;
#57093 = ORIENTED_EDGE('',*,*,#39847,.F.) ;
#57094 = ORIENTED_EDGE('',*,*,#41814,.T.) ;
#57095 = ORIENTED_EDGE('',*,*,#39831,.F.) ;
#57096 = ORIENTED_EDGE('',*,*,#41816,.F.) ;
#57097 = ORIENTED_EDGE('',*,*,#41061,.F.) ;
#57098 = ORIENTED_EDGE('',*,*,#41815,.T.) ;
#57099 = ORIENTED_EDGE('',*,*,#41116,.F.) ;
#57100 = ORIENTED_EDGE('',*,*,#41817,.F.) ;
#57101 = ORIENTED_EDGE('',*,*,#39848,.F.) ;
#57102 = ORIENTED_EDGE('',*,*,#41058,.F.) ;
#57103 = ORIENTED_EDGE('',*,*,#41816,.T.) ;
#57104 = ORIENTED_EDGE('',*,*,#41818,.F.) ;
#57105 = ORIENTED_EDGE('',*,*,#41817,.T.) ;
#57106 = ORIENTED_EDGE('',*,*,#41119,.F.) ;
#57107 = ORIENTED_EDGE('',*,*,#41819,.F.) ;
#57108 = ORIENTED_EDGE('',*,*,#39849,.F.) ;
#57109 = ORIENTED_EDGE('',*,*,#41818,.T.) ;
#57110 = ORIENTED_EDGE('',*,*,#39830,.F.) ;
#57111 = ORIENTED_EDGE('',*,*,#41820,.F.) ;
#57112 = ORIENTED_EDGE('',*,*,#41055,.F.) ;
#57113 = ORIENTED_EDGE('',*,*,#41819,.T.) ;
#57114 = ORIENTED_EDGE('',*,*,#41122,.F.) ;
#57115 = ORIENTED_EDGE('',*,*,#41821,.F.) ;
#57116 = ORIENTED_EDGE('',*,*,#39850,.F.) ;
#57117 = ORIENTED_EDGE('',*,*,#41052,.F.) ;
#57118 = ORIENTED_EDGE('',*,*,#41820,.T.) ;
#57119 = ORIENTED_EDGE('',*,*,#41822,.F.) ;
#57120 = ORIENTED_EDGE('',*,*,#41821,.T.) ;
#57121 = ORIENTED_EDGE('',*,*,#41125,.F.) ;
#57122 = ORIENTED_EDGE('',*,*,#41823,.F.) ;
#57123 = ORIENTED_EDGE('',*,*,#39828,.F.) ;
#57124 = ORIENTED_EDGE('',*,*,#41822,.T.) ;
#57125 = ORIENTED_EDGE('',*,*,#39829,.F.) ;
#57126 = ORIENTED_EDGE('',*,*,#41823,.T.) ;
#57127 = ORIENTED_EDGE('',*,*,#41127,.F.) ;
#57128 = ORIENTED_EDGE('',*,*,#41824,.F.) ;
#57129 = ORIENTED_EDGE('',*,*,#41183,.F.) ;
#57130 = ORIENTED_EDGE('',*,*,#41825,.F.) ;
#57131 = ORIENTED_EDGE('',*,*,#39862,.F.) ;
#57132 = ORIENTED_EDGE('',*,*,#41180,.F.) ;
#57133 = ORIENTED_EDGE('',*,*,#41824,.T.) ;
#57134 = ORIENTED_EDGE('',*,*,#41826,.F.) ;
#57135 = ORIENTED_EDGE('',*,*,#41825,.T.) ;
#57136 = ORIENTED_EDGE('',*,*,#41186,.F.) ;
#57137 = ORIENTED_EDGE('',*,*,#41827,.F.) ;
#57138 = ORIENTED_EDGE('',*,*,#41826,.T.) ;
#57139 = ORIENTED_EDGE('',*,*,#39861,.F.) ;
#57140 = ORIENTED_EDGE('',*,*,#41828,.F.) ;
#57141 = ORIENTED_EDGE('',*,*,#41177,.F.) ;
#57142 = ORIENTED_EDGE('',*,*,#41827,.T.) ;
#57143 = ORIENTED_EDGE('',*,*,#41189,.F.) ;
#57144 = ORIENTED_EDGE('',*,*,#41829,.F.) ;
#57145 = ORIENTED_EDGE('',*,*,#39863,.F.) ;
#57146 = ORIENTED_EDGE('',*,*,#41828,.T.) ;
#57147 = ORIENTED_EDGE('',*,*,#39860,.F.) ;
#57148 = ORIENTED_EDGE('',*,*,#41830,.F.) ;
#57149 = ORIENTED_EDGE('',*,*,#41174,.F.) ;
#57150 = ORIENTED_EDGE('',*,*,#41829,.T.) ;
#57151 = ORIENTED_EDGE('',*,*,#41192,.F.) ;
#57152 = ORIENTED_EDGE('',*,*,#41831,.F.) ;
#57153 = ORIENTED_EDGE('',*,*,#39864,.F.) ;
#57154 = ORIENTED_EDGE('',*,*,#41830,.T.) ;
#57155 = ORIENTED_EDGE('',*,*,#39859,.F.) ;
#57156 = ORIENTED_EDGE('',*,*,#39243,.F.) ;
#57157 = ORIENTED_EDGE('',*,*,#41171,.F.) ;
#57158 = ORIENTED_EDGE('',*,*,#41831,.T.) ;
#57159 = ORIENTED_EDGE('',*,*,#41195,.F.) ;
#57160 = ORIENTED_EDGE('',*,*,#41832,.F.) ;
#57161 = ORIENTED_EDGE('',*,*,#39865,.F.) ;
#57162 = ORIENTED_EDGE('',*,*,#41832,.T.) ;
#57163 = ORIENTED_EDGE('',*,*,#41198,.F.) ;
#57164 = ORIENTED_EDGE('',*,*,#41833,.F.) ;
#57165 = ORIENTED_EDGE('',*,*,#39866,.F.) ;
#57166 = ORIENTED_EDGE('',*,*,#39241,.T.) ;
#57167 = ORIENTED_EDGE('',*,*,#39858,.F.) ;
#57168 = ORIENTED_EDGE('',*,*,#41834,.F.) ;
#57169 = ORIENTED_EDGE('',*,*,#41168,.F.) ;
#57170 = ORIENTED_EDGE('',*,*,#41833,.T.) ;
#57171 = ORIENTED_EDGE('',*,*,#41201,.F.) ;
#57172 = ORIENTED_EDGE('',*,*,#41835,.F.) ;
#57173 = ORIENTED_EDGE('',*,*,#39867,.F.) ;
#57174 = ORIENTED_EDGE('',*,*,#41834,.T.) ;
#57175 = ORIENTED_EDGE('',*,*,#39857,.F.) ;
#57176 = ORIENTED_EDGE('',*,*,#41836,.F.) ;
#57177 = ORIENTED_EDGE('',*,*,#41166,.F.) ;
#57178 = ORIENTED_EDGE('',*,*,#41835,.T.) ;
#57179 = ORIENTED_EDGE('',*,*,#41204,.F.) ;
#57180 = ORIENTED_EDGE('',*,*,#41837,.F.) ;
#57181 = ORIENTED_EDGE('',*,*,#39868,.F.) ;
#57182 = ORIENTED_EDGE('',*,*,#41836,.T.) ;
#57183 = ORIENTED_EDGE('',*,*,#39856,.F.) ;
#57184 = ORIENTED_EDGE('',*,*,#41838,.F.) ;
#57185 = ORIENTED_EDGE('',*,*,#41164,.F.) ;
#57186 = ORIENTED_EDGE('',*,*,#41837,.T.) ;
#57187 = ORIENTED_EDGE('',*,*,#41207,.F.) ;
#57188 = ORIENTED_EDGE('',*,*,#41839,.F.) ;
#57189 = ORIENTED_EDGE('',*,*,#39869,.F.) ;
#57190 = ORIENTED_EDGE('',*,*,#41838,.T.) ;
#57191 = ORIENTED_EDGE('',*,*,#39855,.F.) ;
#57192 = ORIENTED_EDGE('',*,*,#41840,.F.) ;
#57193 = ORIENTED_EDGE('',*,*,#41161,.F.) ;
#57194 = ORIENTED_EDGE('',*,*,#41839,.T.) ;
#57195 = ORIENTED_EDGE('',*,*,#41210,.F.) ;
#57196 = ORIENTED_EDGE('',*,*,#41841,.F.) ;
#57197 = ORIENTED_EDGE('',*,*,#39870,.F.) ;
#57198 = ORIENTED_EDGE('',*,*,#41840,.T.) ;
#57199 = ORIENTED_EDGE('',*,*,#39854,.F.) ;
#57200 = ORIENTED_EDGE('',*,*,#41842,.F.) ;
#57201 = ORIENTED_EDGE('',*,*,#41158,.F.) ;
#57202 = ORIENTED_EDGE('',*,*,#41841,.T.) ;
#57203 = ORIENTED_EDGE('',*,*,#41213,.F.) ;
#57204 = ORIENTED_EDGE('',*,*,#41843,.F.) ;
#57205 = ORIENTED_EDGE('',*,*,#39871,.F.) ;
#57206 = ORIENTED_EDGE('',*,*,#41155,.F.) ;
#57207 = ORIENTED_EDGE('',*,*,#41842,.T.) ;
#57208 = ORIENTED_EDGE('',*,*,#41844,.F.) ;
#57209 = ORIENTED_EDGE('',*,*,#41843,.T.) ;
#57210 = ORIENTED_EDGE('',*,*,#41216,.F.) ;
#57211 = ORIENTED_EDGE('',*,*,#41845,.F.) ;
#57212 = ORIENTED_EDGE('',*,*,#39872,.F.) ;
#57213 = ORIENTED_EDGE('',*,*,#41844,.T.) ;
#57214 = ORIENTED_EDGE('',*,*,#39853,.F.) ;
#57215 = ORIENTED_EDGE('',*,*,#41846,.F.) ;
#57216 = ORIENTED_EDGE('',*,*,#41152,.F.) ;
#57217 = ORIENTED_EDGE('',*,*,#41845,.T.) ;
#57218 = ORIENTED_EDGE('',*,*,#41219,.F.) ;
#57219 = ORIENTED_EDGE('',*,*,#41847,.F.) ;
#57220 = ORIENTED_EDGE('',*,*,#39873,.F.) ;
#57221 = ORIENTED_EDGE('',*,*,#41149,.F.) ;
#57222 = ORIENTED_EDGE('',*,*,#41846,.T.) ;
#57223 = ORIENTED_EDGE('',*,*,#41848,.F.) ;
#57224 = ORIENTED_EDGE('',*,*,#41847,.T.) ;
#57225 = ORIENTED_EDGE('',*,*,#41222,.F.) ;
#57226 = ORIENTED_EDGE('',*,*,#41849,.F.) ;
#57227 = ORIENTED_EDGE('',*,*,#39851,.F.) ;
#57228 = ORIENTED_EDGE('',*,*,#41848,.T.) ;
#57229 = ORIENTED_EDGE('',*,*,#39852,.F.) ;
#57230 = ORIENTED_EDGE('',*,*,#41849,.T.) ;
#57231 = ORIENTED_EDGE('',*,*,#41224,.F.) ;
#57232 = ORIENTED_EDGE('',*,*,#41850,.F.) ;
#57233 = ORIENTED_EDGE('',*,*,#41280,.F.) ;
#57234 = ORIENTED_EDGE('',*,*,#41851,.F.) ;
#57235 = ORIENTED_EDGE('',*,*,#39885,.F.) ;
#57236 = ORIENTED_EDGE('',*,*,#41277,.F.) ;
#57237 = ORIENTED_EDGE('',*,*,#41850,.T.) ;
#57238 = ORIENTED_EDGE('',*,*,#41852,.F.) ;
#57239 = ORIENTED_EDGE('',*,*,#41851,.T.) ;
#57240 = ORIENTED_EDGE('',*,*,#41283,.F.) ;
#57241 = ORIENTED_EDGE('',*,*,#41853,.F.) ;
#57242 = ORIENTED_EDGE('',*,*,#41852,.T.) ;
#57243 = ORIENTED_EDGE('',*,*,#39884,.F.) ;
#57244 = ORIENTED_EDGE('',*,*,#41854,.F.) ;
#57245 = ORIENTED_EDGE('',*,*,#41274,.F.) ;
#57246 = ORIENTED_EDGE('',*,*,#41853,.T.) ;
#57247 = ORIENTED_EDGE('',*,*,#41286,.F.) ;
#57248 = ORIENTED_EDGE('',*,*,#41855,.F.) ;
#57249 = ORIENTED_EDGE('',*,*,#39886,.F.) ;
#57250 = ORIENTED_EDGE('',*,*,#41854,.T.) ;
#57251 = ORIENTED_EDGE('',*,*,#39883,.F.) ;
#57252 = ORIENTED_EDGE('',*,*,#41856,.F.) ;
#57253 = ORIENTED_EDGE('',*,*,#41271,.F.) ;
#57254 = ORIENTED_EDGE('',*,*,#41855,.T.) ;
#57255 = ORIENTED_EDGE('',*,*,#41289,.F.) ;
#57256 = ORIENTED_EDGE('',*,*,#41857,.F.) ;
#57257 = ORIENTED_EDGE('',*,*,#39887,.F.) ;
#57258 = ORIENTED_EDGE('',*,*,#41856,.T.) ;
#57259 = ORIENTED_EDGE('',*,*,#39882,.F.) ;
#57260 = ORIENTED_EDGE('',*,*,#39239,.F.) ;
#57261 = ORIENTED_EDGE('',*,*,#41268,.F.) ;
#57262 = ORIENTED_EDGE('',*,*,#41857,.T.) ;
#57263 = ORIENTED_EDGE('',*,*,#41292,.F.) ;
#57264 = ORIENTED_EDGE('',*,*,#41858,.F.) ;
#57265 = ORIENTED_EDGE('',*,*,#39888,.F.) ;
#57266 = ORIENTED_EDGE('',*,*,#41858,.T.) ;
#57267 = ORIENTED_EDGE('',*,*,#41295,.F.) ;
#57268 = ORIENTED_EDGE('',*,*,#41859,.F.) ;
#57269 = ORIENTED_EDGE('',*,*,#39889,.F.) ;
#57270 = ORIENTED_EDGE('',*,*,#39237,.T.) ;
#57271 = ORIENTED_EDGE('',*,*,#39881,.F.) ;
#57272 = ORIENTED_EDGE('',*,*,#41860,.F.) ;
#57273 = ORIENTED_EDGE('',*,*,#41265,.F.) ;
#57274 = ORIENTED_EDGE('',*,*,#41859,.T.) ;
#57275 = ORIENTED_EDGE('',*,*,#41298,.F.) ;
#57276 = ORIENTED_EDGE('',*,*,#41861,.F.) ;
#57277 = ORIENTED_EDGE('',*,*,#39890,.F.) ;
#57278 = ORIENTED_EDGE('',*,*,#41860,.T.) ;
#57279 = ORIENTED_EDGE('',*,*,#39880,.F.) ;
#57280 = ORIENTED_EDGE('',*,*,#41862,.F.) ;
#57281 = ORIENTED_EDGE('',*,*,#41263,.F.) ;
#57282 = ORIENTED_EDGE('',*,*,#41861,.T.) ;
#57283 = ORIENTED_EDGE('',*,*,#41301,.F.) ;
#57284 = ORIENTED_EDGE('',*,*,#41863,.F.) ;
#57285 = ORIENTED_EDGE('',*,*,#39891,.F.) ;
#57286 = ORIENTED_EDGE('',*,*,#41862,.T.) ;
#57287 = ORIENTED_EDGE('',*,*,#39879,.F.) ;
#57288 = ORIENTED_EDGE('',*,*,#41864,.F.) ;
#57289 = ORIENTED_EDGE('',*,*,#41261,.F.) ;
#57290 = ORIENTED_EDGE('',*,*,#41863,.T.) ;
#57291 = ORIENTED_EDGE('',*,*,#41304,.F.) ;
#57292 = ORIENTED_EDGE('',*,*,#41865,.F.) ;
#57293 = ORIENTED_EDGE('',*,*,#39892,.F.) ;
#57294 = ORIENTED_EDGE('',*,*,#41864,.T.) ;
#57295 = ORIENTED_EDGE('',*,*,#39878,.F.) ;
#57296 = ORIENTED_EDGE('',*,*,#41866,.F.) ;
#57297 = ORIENTED_EDGE('',*,*,#41258,.F.) ;
#57298 = ORIENTED_EDGE('',*,*,#41865,.T.) ;
#57299 = ORIENTED_EDGE('',*,*,#41307,.F.) ;
#57300 = ORIENTED_EDGE('',*,*,#41867,.F.) ;
#57301 = ORIENTED_EDGE('',*,*,#39893,.F.) ;
#57302 = ORIENTED_EDGE('',*,*,#41866,.T.) ;
#57303 = ORIENTED_EDGE('',*,*,#39877,.F.) ;
#57304 = ORIENTED_EDGE('',*,*,#41868,.F.) ;
#57305 = ORIENTED_EDGE('',*,*,#41255,.F.) ;
#57306 = ORIENTED_EDGE('',*,*,#41867,.T.) ;
#57307 = ORIENTED_EDGE('',*,*,#41310,.F.) ;
#57308 = ORIENTED_EDGE('',*,*,#41869,.F.) ;
#57309 = ORIENTED_EDGE('',*,*,#39894,.F.) ;
#57310 = ORIENTED_EDGE('',*,*,#41252,.F.) ;
#57311 = ORIENTED_EDGE('',*,*,#41868,.T.) ;
#57312 = ORIENTED_EDGE('',*,*,#41870,.F.) ;
#57313 = ORIENTED_EDGE('',*,*,#41869,.T.) ;
#57314 = ORIENTED_EDGE('',*,*,#41313,.F.) ;
#57315 = ORIENTED_EDGE('',*,*,#41871,.F.) ;
#57316 = ORIENTED_EDGE('',*,*,#39895,.F.) ;
#57317 = ORIENTED_EDGE('',*,*,#41870,.T.) ;
#57318 = ORIENTED_EDGE('',*,*,#39876,.F.) ;
#57319 = ORIENTED_EDGE('',*,*,#41872,.F.) ;
#57320 = ORIENTED_EDGE('',*,*,#41249,.F.) ;
#57321 = ORIENTED_EDGE('',*,*,#41871,.T.) ;
#57322 = ORIENTED_EDGE('',*,*,#41316,.F.) ;
#57323 = ORIENTED_EDGE('',*,*,#41873,.F.) ;
#57324 = ORIENTED_EDGE('',*,*,#39896,.F.) ;
#57325 = ORIENTED_EDGE('',*,*,#41246,.F.) ;
#57326 = ORIENTED_EDGE('',*,*,#41872,.T.) ;
#57327 = ORIENTED_EDGE('',*,*,#41874,.F.) ;
#57328 = ORIENTED_EDGE('',*,*,#41873,.T.) ;
#57329 = ORIENTED_EDGE('',*,*,#41319,.F.) ;
#57330 = ORIENTED_EDGE('',*,*,#41875,.F.) ;
#57331 = ORIENTED_EDGE('',*,*,#39874,.F.) ;
#57332 = ORIENTED_EDGE('',*,*,#41874,.T.) ;
#57333 = ORIENTED_EDGE('',*,*,#39875,.F.) ;
#57334 = ORIENTED_EDGE('',*,*,#41875,.T.) ;
#57335 = ORIENTED_EDGE('',*,*,#41321,.F.) ;
#57336 = ORIENTED_EDGE('',*,*,#41876,.F.) ;
#57337 = ORIENTED_EDGE('',*,*,#41377,.F.) ;
#57338 = ORIENTED_EDGE('',*,*,#41877,.F.) ;
#57339 = ORIENTED_EDGE('',*,*,#39908,.F.) ;
#57340 = ORIENTED_EDGE('',*,*,#41374,.F.) ;
#57341 = ORIENTED_EDGE('',*,*,#41876,.T.) ;
#57342 = ORIENTED_EDGE('',*,*,#41878,.F.) ;
#57343 = ORIENTED_EDGE('',*,*,#41877,.T.) ;
#57344 = ORIENTED_EDGE('',*,*,#41380,.F.) ;
#57345 = ORIENTED_EDGE('',*,*,#41879,.F.) ;
#57346 = ORIENTED_EDGE('',*,*,#41878,.T.) ;
#57347 = ORIENTED_EDGE('',*,*,#39907,.F.) ;
#57348 = ORIENTED_EDGE('',*,*,#41880,.F.) ;
#57349 = ORIENTED_EDGE('',*,*,#41371,.F.) ;
#57350 = ORIENTED_EDGE('',*,*,#41879,.T.) ;
#57351 = ORIENTED_EDGE('',*,*,#41383,.F.) ;
#57352 = ORIENTED_EDGE('',*,*,#41881,.F.) ;
#57353 = ORIENTED_EDGE('',*,*,#39909,.F.) ;
#57354 = ORIENTED_EDGE('',*,*,#41880,.T.) ;
#57355 = ORIENTED_EDGE('',*,*,#39906,.F.) ;
#57356 = ORIENTED_EDGE('',*,*,#41882,.F.) ;
#57357 = ORIENTED_EDGE('',*,*,#41368,.F.) ;
#57358 = ORIENTED_EDGE('',*,*,#41881,.T.) ;
#57359 = ORIENTED_EDGE('',*,*,#41386,.F.) ;
#57360 = ORIENTED_EDGE('',*,*,#41883,.F.) ;
#57361 = ORIENTED_EDGE('',*,*,#39910,.F.) ;
#57362 = ORIENTED_EDGE('',*,*,#41882,.T.) ;
#57363 = ORIENTED_EDGE('',*,*,#39905,.F.) ;
#57364 = ORIENTED_EDGE('',*,*,#39235,.F.) ;
#57365 = ORIENTED_EDGE('',*,*,#41365,.F.) ;
#57366 = ORIENTED_EDGE('',*,*,#41883,.T.) ;
#57367 = ORIENTED_EDGE('',*,*,#41389,.F.) ;
#57368 = ORIENTED_EDGE('',*,*,#41884,.F.) ;
#57369 = ORIENTED_EDGE('',*,*,#39911,.F.) ;
#57370 = ORIENTED_EDGE('',*,*,#41884,.T.) ;
#57371 = ORIENTED_EDGE('',*,*,#41392,.F.) ;
#57372 = ORIENTED_EDGE('',*,*,#41885,.F.) ;
#57373 = ORIENTED_EDGE('',*,*,#39912,.F.) ;
#57374 = ORIENTED_EDGE('',*,*,#39233,.T.) ;
#57375 = ORIENTED_EDGE('',*,*,#39904,.F.) ;
#57376 = ORIENTED_EDGE('',*,*,#41886,.F.) ;
#57377 = ORIENTED_EDGE('',*,*,#41362,.F.) ;
#57378 = ORIENTED_EDGE('',*,*,#41885,.T.) ;
#57379 = ORIENTED_EDGE('',*,*,#41395,.F.) ;
#57380 = ORIENTED_EDGE('',*,*,#41887,.F.) ;
#57381 = ORIENTED_EDGE('',*,*,#39913,.F.) ;
#57382 = ORIENTED_EDGE('',*,*,#41886,.T.) ;
#57383 = ORIENTED_EDGE('',*,*,#39903,.F.) ;
#57384 = ORIENTED_EDGE('',*,*,#41888,.F.) ;
#57385 = ORIENTED_EDGE('',*,*,#41360,.F.) ;
#57386 = ORIENTED_EDGE('',*,*,#41887,.T.) ;
#57387 = ORIENTED_EDGE('',*,*,#41398,.F.) ;
#57388 = ORIENTED_EDGE('',*,*,#41889,.F.) ;
#57389 = ORIENTED_EDGE('',*,*,#39914,.F.) ;
#57390 = ORIENTED_EDGE('',*,*,#41888,.T.) ;
#57391 = ORIENTED_EDGE('',*,*,#39902,.F.) ;
#57392 = ORIENTED_EDGE('',*,*,#41890,.F.) ;
#57393 = ORIENTED_EDGE('',*,*,#41358,.F.) ;
#57394 = ORIENTED_EDGE('',*,*,#41889,.T.) ;
#57395 = ORIENTED_EDGE('',*,*,#41401,.F.) ;
#57396 = ORIENTED_EDGE('',*,*,#41891,.F.) ;
#57397 = ORIENTED_EDGE('',*,*,#39915,.F.) ;
#57398 = ORIENTED_EDGE('',*,*,#41890,.T.) ;
#57399 = ORIENTED_EDGE('',*,*,#39901,.F.) ;
#57400 = ORIENTED_EDGE('',*,*,#41892,.F.) ;
#57401 = ORIENTED_EDGE('',*,*,#41355,.F.) ;
#57402 = ORIENTED_EDGE('',*,*,#41891,.T.) ;
#57403 = ORIENTED_EDGE('',*,*,#41404,.F.) ;
#57404 = ORIENTED_EDGE('',*,*,#41893,.F.) ;
#57405 = ORIENTED_EDGE('',*,*,#39916,.F.) ;
#57406 = ORIENTED_EDGE('',*,*,#41892,.T.) ;
#57407 = ORIENTED_EDGE('',*,*,#39900,.F.) ;
#57408 = ORIENTED_EDGE('',*,*,#41894,.F.) ;
#57409 = ORIENTED_EDGE('',*,*,#41352,.F.) ;
#57410 = ORIENTED_EDGE('',*,*,#41893,.T.) ;
#57411 = ORIENTED_EDGE('',*,*,#41407,.F.) ;
#57412 = ORIENTED_EDGE('',*,*,#41895,.F.) ;
#57413 = ORIENTED_EDGE('',*,*,#39917,.F.) ;
#57414 = ORIENTED_EDGE('',*,*,#41349,.F.) ;
#57415 = ORIENTED_EDGE('',*,*,#41894,.T.) ;
#57416 = ORIENTED_EDGE('',*,*,#41896,.F.) ;
#57417 = ORIENTED_EDGE('',*,*,#41895,.T.) ;
#57418 = ORIENTED_EDGE('',*,*,#41410,.F.) ;
#57419 = ORIENTED_EDGE('',*,*,#41897,.F.) ;
#57420 = ORIENTED_EDGE('',*,*,#39918,.F.) ;
#57421 = ORIENTED_EDGE('',*,*,#41896,.T.) ;
#57422 = ORIENTED_EDGE('',*,*,#39899,.F.) ;
#57423 = ORIENTED_EDGE('',*,*,#41898,.F.) ;
#57424 = ORIENTED_EDGE('',*,*,#41346,.F.) ;
#57425 = ORIENTED_EDGE('',*,*,#41897,.T.) ;
#57426 = ORIENTED_EDGE('',*,*,#41413,.F.) ;
#57427 = ORIENTED_EDGE('',*,*,#41899,.F.) ;
#57428 = ORIENTED_EDGE('',*,*,#39919,.F.) ;
#57429 = ORIENTED_EDGE('',*,*,#41343,.F.) ;
#57430 = ORIENTED_EDGE('',*,*,#41898,.T.) ;
#57431 = ORIENTED_EDGE('',*,*,#41900,.F.) ;
#57432 = ORIENTED_EDGE('',*,*,#41899,.T.) ;
#57433 = ORIENTED_EDGE('',*,*,#41416,.F.) ;
#57434 = ORIENTED_EDGE('',*,*,#41901,.F.) ;
#57435 = ORIENTED_EDGE('',*,*,#39897,.F.) ;
#57436 = ORIENTED_EDGE('',*,*,#41900,.T.) ;
#57437 = ORIENTED_EDGE('',*,*,#39898,.F.) ;
#57438 = ORIENTED_EDGE('',*,*,#41901,.T.) ;
#57439 = ORIENTED_EDGE('',*,*,#41418,.F.) ;
#57440 = ORIENTED_EDGE('',*,*,#41902,.F.) ;
#57441 = ORIENTED_EDGE('',*,*,#41474,.F.) ;
#57442 = ORIENTED_EDGE('',*,*,#41903,.F.) ;
#57443 = ORIENTED_EDGE('',*,*,#39931,.F.) ;
#57444 = ORIENTED_EDGE('',*,*,#41471,.F.) ;
#57445 = ORIENTED_EDGE('',*,*,#41902,.T.) ;
#57446 = ORIENTED_EDGE('',*,*,#41904,.F.) ;
#57447 = ORIENTED_EDGE('',*,*,#41903,.T.) ;
#57448 = ORIENTED_EDGE('',*,*,#41477,.F.) ;
#57449 = ORIENTED_EDGE('',*,*,#41905,.F.) ;
#57450 = ORIENTED_EDGE('',*,*,#41904,.T.) ;
#57451 = ORIENTED_EDGE('',*,*,#39930,.F.) ;
#57452 = ORIENTED_EDGE('',*,*,#41906,.F.) ;
#57453 = ORIENTED_EDGE('',*,*,#41468,.F.) ;
#57454 = ORIENTED_EDGE('',*,*,#41905,.T.) ;
#57455 = ORIENTED_EDGE('',*,*,#41480,.F.) ;
#57456 = ORIENTED_EDGE('',*,*,#41907,.F.) ;
#57457 = ORIENTED_EDGE('',*,*,#39932,.F.) ;
#57458 = ORIENTED_EDGE('',*,*,#41906,.T.) ;
#57459 = ORIENTED_EDGE('',*,*,#39929,.F.) ;
#57460 = ORIENTED_EDGE('',*,*,#41908,.F.) ;
#57461 = ORIENTED_EDGE('',*,*,#41465,.F.) ;
#57462 = ORIENTED_EDGE('',*,*,#41907,.T.) ;
#57463 = ORIENTED_EDGE('',*,*,#41483,.F.) ;
#57464 = ORIENTED_EDGE('',*,*,#41909,.F.) ;
#57465 = ORIENTED_EDGE('',*,*,#39933,.F.) ;
#57466 = ORIENTED_EDGE('',*,*,#41908,.T.) ;
#57467 = ORIENTED_EDGE('',*,*,#39928,.F.) ;
#57468 = ORIENTED_EDGE('',*,*,#39231,.F.) ;
#57469 = ORIENTED_EDGE('',*,*,#41462,.F.) ;
#57470 = ORIENTED_EDGE('',*,*,#41909,.T.) ;
#57471 = ORIENTED_EDGE('',*,*,#41486,.F.) ;
#57472 = ORIENTED_EDGE('',*,*,#41910,.F.) ;
#57473 = ORIENTED_EDGE('',*,*,#39934,.F.) ;
#57474 = ORIENTED_EDGE('',*,*,#41910,.T.) ;
#57475 = ORIENTED_EDGE('',*,*,#41489,.F.) ;
#57476 = ORIENTED_EDGE('',*,*,#41911,.F.) ;
#57477 = ORIENTED_EDGE('',*,*,#39935,.F.) ;
#57478 = ORIENTED_EDGE('',*,*,#39229,.T.) ;
#57479 = ORIENTED_EDGE('',*,*,#39927,.F.) ;
#57480 = ORIENTED_EDGE('',*,*,#41912,.F.) ;
#57481 = ORIENTED_EDGE('',*,*,#41459,.F.) ;
#57482 = ORIENTED_EDGE('',*,*,#41911,.T.) ;
#57483 = ORIENTED_EDGE('',*,*,#41492,.F.) ;
#57484 = ORIENTED_EDGE('',*,*,#41913,.F.) ;
#57485 = ORIENTED_EDGE('',*,*,#39936,.F.) ;
#57486 = ORIENTED_EDGE('',*,*,#41912,.T.) ;
#57487 = ORIENTED_EDGE('',*,*,#39926,.F.) ;
#57488 = ORIENTED_EDGE('',*,*,#41914,.F.) ;
#57489 = ORIENTED_EDGE('',*,*,#41457,.F.) ;
#57490 = ORIENTED_EDGE('',*,*,#41913,.T.) ;
#57491 = ORIENTED_EDGE('',*,*,#41495,.F.) ;
#57492 = ORIENTED_EDGE('',*,*,#41915,.F.) ;
#57493 = ORIENTED_EDGE('',*,*,#39937,.F.) ;
#57494 = ORIENTED_EDGE('',*,*,#41914,.T.) ;
#57495 = ORIENTED_EDGE('',*,*,#39925,.F.) ;
#57496 = ORIENTED_EDGE('',*,*,#41916,.F.) ;
#57497 = ORIENTED_EDGE('',*,*,#41455,.F.) ;
#57498 = ORIENTED_EDGE('',*,*,#41915,.T.) ;
#57499 = ORIENTED_EDGE('',*,*,#41498,.F.) ;
#57500 = ORIENTED_EDGE('',*,*,#41917,.F.) ;
#57501 = ORIENTED_EDGE('',*,*,#39938,.F.) ;
#57502 = ORIENTED_EDGE('',*,*,#41916,.T.) ;
#57503 = ORIENTED_EDGE('',*,*,#39924,.F.) ;
#57504 = ORIENTED_EDGE('',*,*,#41918,.F.) ;
#57505 = ORIENTED_EDGE('',*,*,#41452,.F.) ;
#57506 = ORIENTED_EDGE('',*,*,#41917,.T.) ;
#57507 = ORIENTED_EDGE('',*,*,#41501,.F.) ;
#57508 = ORIENTED_EDGE('',*,*,#41919,.F.) ;
#57509 = ORIENTED_EDGE('',*,*,#39939,.F.) ;
#57510 = ORIENTED_EDGE('',*,*,#41918,.T.) ;
#57511 = ORIENTED_EDGE('',*,*,#39923,.F.) ;
#57512 = ORIENTED_EDGE('',*,*,#41920,.F.) ;
#57513 = ORIENTED_EDGE('',*,*,#41449,.F.) ;
#57514 = ORIENTED_EDGE('',*,*,#41919,.T.) ;
#57515 = ORIENTED_EDGE('',*,*,#41504,.F.) ;
#57516 = ORIENTED_EDGE('',*,*,#41921,.F.) ;
#57517 = ORIENTED_EDGE('',*,*,#39940,.F.) ;
#57518 = ORIENTED_EDGE('',*,*,#41446,.F.) ;
#57519 = ORIENTED_EDGE('',*,*,#41920,.T.) ;
#57520 = ORIENTED_EDGE('',*,*,#41922,.F.) ;
#57521 = ORIENTED_EDGE('',*,*,#41921,.T.) ;
#57522 = ORIENTED_EDGE('',*,*,#41507,.F.) ;
#57523 = ORIENTED_EDGE('',*,*,#41923,.F.) ;
#57524 = ORIENTED_EDGE('',*,*,#39941,.F.) ;
#57525 = ORIENTED_EDGE('',*,*,#41922,.T.) ;
#57526 = ORIENTED_EDGE('',*,*,#39922,.F.) ;
#57527 = ORIENTED_EDGE('',*,*,#41924,.F.) ;
#57528 = ORIENTED_EDGE('',*,*,#41443,.F.) ;
#57529 = ORIENTED_EDGE('',*,*,#41923,.T.) ;
#57530 = ORIENTED_EDGE('',*,*,#41510,.F.) ;
#57531 = ORIENTED_EDGE('',*,*,#41925,.F.) ;
#57532 = ORIENTED_EDGE('',*,*,#39942,.F.) ;
#57533 = ORIENTED_EDGE('',*,*,#41440,.F.) ;
#57534 = ORIENTED_EDGE('',*,*,#41924,.T.) ;
#57535 = ORIENTED_EDGE('',*,*,#41926,.F.) ;
#57536 = ORIENTED_EDGE('',*,*,#41925,.T.) ;
#57537 = ORIENTED_EDGE('',*,*,#41513,.F.) ;
#57538 = ORIENTED_EDGE('',*,*,#41927,.F.) ;
#57539 = ORIENTED_EDGE('',*,*,#39920,.F.) ;
#57540 = ORIENTED_EDGE('',*,*,#41926,.T.) ;
#57541 = ORIENTED_EDGE('',*,*,#39921,.F.) ;
#57542 = ORIENTED_EDGE('',*,*,#41927,.T.) ;
#57543 = ORIENTED_EDGE('',*,*,#41515,.F.) ;
#57544 = ORIENTED_EDGE('',*,*,#41928,.F.) ;
#57545 = ORIENTED_EDGE('',*,*,#40521,.F.) ;
#57546 = ORIENTED_EDGE('',*,*,#41929,.F.) ;
#57547 = ORIENTED_EDGE('',*,*,#40479,.F.) ;
#57548 = ORIENTED_EDGE('',*,*,#41930,.F.) ;
#57549 = ORIENTED_EDGE('',*,*,#40522,.F.) ;
#57550 = ORIENTED_EDGE('',*,*,#41931,.F.) ;
#57551 = ORIENTED_EDGE('',*,*,#40516,.F.) ;
#57552 = ORIENTED_EDGE('',*,*,#41932,.F.) ;
#57553 = ORIENTED_EDGE('',*,*,#41930,.T.) ;
#57554 = ORIENTED_EDGE('',*,*,#41933,.F.) ;
#57555 = ORIENTED_EDGE('',*,*,#41934,.F.) ;
#57556 = ORIENTED_EDGE('',*,*,#41929,.T.) ;
#57557 = ORIENTED_EDGE('',*,*,#41935,.F.) ;
#57558 = ORIENTED_EDGE('',*,*,#41928,.T.) ;
#57559 = ORIENTED_EDGE('',*,*,#40478,.T.) ;
#57560 = ORIENTED_EDGE('',*,*,#41936,.F.) ;
#57561 = ORIENTED_EDGE('',*,*,#41931,.T.) ;
#57562 = ORIENTED_EDGE('',*,*,#41933,.T.) ;
#57563 = ORIENTED_EDGE('',*,*,#40519,.F.) ;
#57564 = ORIENTED_EDGE('',*,*,#41937,.F.) ;
#57565 = ORIENTED_EDGE('',*,*,#39217,.T.) ;
#57566 = ORIENTED_EDGE('',*,*,#41938,.T.) ;
#57567 = ORIENTED_EDGE('',*,*,#41939,.F.) ;
#57568 = ORIENTED_EDGE('',*,*,#41932,.T.) ;
#57569 = ORIENTED_EDGE('',*,*,#41940,.F.) ;
#57570 = ORIENTED_EDGE('',*,*,#41941,.T.) ;
#57571 = ORIENTED_EDGE('',*,*,#41942,.F.) ;
#57572 = ORIENTED_EDGE('',*,*,#39415,.F.) ;
#57573 = ORIENTED_EDGE('',*,*,#41943,.F.) ;
#57574 = ORIENTED_EDGE('',*,*,#40523,.F.) ;
#57575 = ORIENTED_EDGE('',*,*,#41935,.T.) ;
#57576 = ORIENTED_EDGE('',*,*,#40520,.F.) ;
#57577 = ORIENTED_EDGE('',*,*,#41944,.F.) ;
#57578 = ORIENTED_EDGE('',*,*,#40526,.F.) ;
#57579 = ORIENTED_EDGE('',*,*,#41934,.T.) ;
#57580 = ORIENTED_EDGE('',*,*,#40525,.F.) ;
#57581 = ORIENTED_EDGE('',*,*,#41945,.F.) ;
#57582 = ORIENTED_EDGE('',*,*,#40470,.F.) ;
#57583 = ORIENTED_EDGE('',*,*,#41936,.T.) ;
#57584 = ORIENTED_EDGE('',*,*,#40477,.F.) ;
#57585 = ORIENTED_EDGE('',*,*,#41946,.F.) ;
#57586 = ORIENTED_EDGE('',*,*,#40517,.F.) ;
#57587 = ORIENTED_EDGE('',*,*,#41947,.F.) ;
#57588 = ORIENTED_EDGE('',*,*,#40518,.F.) ;
#57589 = ORIENTED_EDGE('',*,*,#41948,.F.) ;
#57590 = ORIENTED_EDGE('',*,*,#40513,.F.) ;
#57591 = ORIENTED_EDGE('',*,*,#41937,.T.) ;
#57592 = ORIENTED_EDGE('',*,*,#41947,.T.) ;
#57593 = ORIENTED_EDGE('',*,*,#39218,.F.) ;
#57594 = ORIENTED_EDGE('',*,*,#41943,.T.) ;
#57595 = ORIENTED_EDGE('',*,*,#39425,.T.) ;
#57596 = ORIENTED_EDGE('',*,*,#41949,.F.) ;
#57597 = ORIENTED_EDGE('',*,*,#41944,.T.) ;
#57598 = ORIENTED_EDGE('',*,*,#41950,.F.) ;
#57599 = ORIENTED_EDGE('',*,*,#41945,.T.) ;
#57600 = ORIENTED_EDGE('',*,*,#41951,.F.) ;
#57601 = ORIENTED_EDGE('',*,*,#39512,.T.) ;
#57602 = ORIENTED_EDGE('',*,*,#41946,.T.) ;
#57603 = ORIENTED_EDGE('',*,*,#40476,.T.) ;
#57604 = ORIENTED_EDGE('',*,*,#41952,.F.) ;
#57605 = ORIENTED_EDGE('',*,*,#41948,.T.) ;
#57606 = ORIENTED_EDGE('',*,*,#41949,.T.) ;
#57607 = ORIENTED_EDGE('',*,*,#39424,.F.) ;
#57608 = ORIENTED_EDGE('',*,*,#41953,.F.) ;
#57609 = ORIENTED_EDGE('',*,*,#40527,.F.) ;
#57610 = ORIENTED_EDGE('',*,*,#41951,.T.) ;
#57611 = ORIENTED_EDGE('',*,*,#40524,.F.) ;
#57612 = ORIENTED_EDGE('',*,*,#41954,.F.) ;
#57613 = ORIENTED_EDGE('',*,*,#39513,.F.) ;
#57614 = ORIENTED_EDGE('',*,*,#40471,.F.) ;
#57615 = ORIENTED_EDGE('',*,*,#41950,.T.) ;
#57616 = ORIENTED_EDGE('',*,*,#41955,.F.) ;
#57617 = ORIENTED_EDGE('',*,*,#41956,.F.) ;
#57618 = ORIENTED_EDGE('',*,*,#41952,.T.) ;
#57619 = ORIENTED_EDGE('',*,*,#40475,.F.) ;
#57620 = ORIENTED_EDGE('',*,*,#41957,.F.) ;
#57621 = ORIENTED_EDGE('',*,*,#40514,.F.) ;
#57622 = ORIENTED_EDGE('',*,*,#41958,.F.) ;
#57623 = ORIENTED_EDGE('',*,*,#40515,.F.) ;
#57624 = ORIENTED_EDGE('',*,*,#41959,.F.) ;
#57625 = ORIENTED_EDGE('',*,*,#40509,.F.) ;
#57626 = ORIENTED_EDGE('',*,*,#39220,.T.) ;
#57627 = ORIENTED_EDGE('',*,*,#41958,.T.) ;
#57628 = ORIENTED_EDGE('',*,*,#41960,.F.) ;
#57629 = ORIENTED_EDGE('',*,*,#39419,.T.) ;
#57630 = ORIENTED_EDGE('',*,*,#41954,.T.) ;
#57631 = ORIENTED_EDGE('',*,*,#41953,.T.) ;
#57632 = ORIENTED_EDGE('',*,*,#41961,.F.) ;
#57633 = ORIENTED_EDGE('',*,*,#41962,.F.) ;
#57634 = ORIENTED_EDGE('',*,*,#39532,.F.) ;
#57635 = ORIENTED_EDGE('',*,*,#41963,.F.) ;
#57636 = ORIENTED_EDGE('',*,*,#41964,.F.) ;
#57637 = ORIENTED_EDGE('',*,*,#41955,.T.) ;
#57638 = ORIENTED_EDGE('',*,*,#39516,.F.) ;
#57639 = ORIENTED_EDGE('',*,*,#41963,.T.) ;
#57640 = ORIENTED_EDGE('',*,*,#39684,.F.) ;
#57641 = ORIENTED_EDGE('',*,*,#41956,.T.) ;
#57642 = ORIENTED_EDGE('',*,*,#41965,.F.) ;
#57643 = ORIENTED_EDGE('',*,*,#41966,.F.) ;
#57644 = ORIENTED_EDGE('',*,*,#41959,.T.) ;
#57645 = ORIENTED_EDGE('',*,*,#41957,.T.) ;
#57646 = ORIENTED_EDGE('',*,*,#41967,.F.) ;
#57647 = ORIENTED_EDGE('',*,*,#41960,.T.) ;
#57648 = ORIENTED_EDGE('',*,*,#40512,.F.) ;
#57649 = ORIENTED_EDGE('',*,*,#41968,.F.) ;
#57650 = ORIENTED_EDGE('',*,*,#39420,.F.) ;
#57651 = ORIENTED_EDGE('',*,*,#41961,.T.) ;
#57652 = ORIENTED_EDGE('',*,*,#39423,.F.) ;
#57653 = ORIENTED_EDGE('',*,*,#41969,.F.) ;
#57654 = ORIENTED_EDGE('',*,*,#39514,.F.) ;
#57655 = ORIENTED_EDGE('',*,*,#41962,.T.) ;
#57656 = ORIENTED_EDGE('',*,*,#39515,.F.) ;
#57657 = ORIENTED_EDGE('',*,*,#41970,.F.) ;
#57658 = ORIENTED_EDGE('',*,*,#39607,.F.) ;
#57659 = ORIENTED_EDGE('',*,*,#41964,.T.) ;
#57660 = ORIENTED_EDGE('',*,*,#39683,.T.) ;
#57661 = ORIENTED_EDGE('',*,*,#41971,.F.) ;
#57662 = ORIENTED_EDGE('',*,*,#41965,.T.) ;
#57663 = ORIENTED_EDGE('',*,*,#40472,.F.) ;
#57664 = ORIENTED_EDGE('',*,*,#41966,.T.) ;
#57665 = ORIENTED_EDGE('',*,*,#41972,.F.) ;
#57666 = ORIENTED_EDGE('',*,*,#41973,.F.) ;
#57667 = ORIENTED_EDGE('',*,*,#41967,.T.) ;
#57668 = ORIENTED_EDGE('',*,*,#40474,.F.) ;
#57669 = ORIENTED_EDGE('',*,*,#41974,.F.) ;
#57670 = ORIENTED_EDGE('',*,*,#40510,.F.) ;
#57671 = ORIENTED_EDGE('',*,*,#41975,.F.) ;
#57672 = ORIENTED_EDGE('',*,*,#40511,.F.) ;
#57673 = ORIENTED_EDGE('',*,*,#41976,.F.) ;
#57674 = ORIENTED_EDGE('',*,*,#39511,.F.) ;
#57675 = ORIENTED_EDGE('',*,*,#41968,.T.) ;
#57676 = ORIENTED_EDGE('',*,*,#41975,.T.) ;
#57677 = ORIENTED_EDGE('',*,*,#41977,.F.) ;
#57678 = ORIENTED_EDGE('',*,*,#41970,.T.) ;
#57679 = ORIENTED_EDGE('',*,*,#41969,.T.) ;
#57680 = ORIENTED_EDGE('',*,*,#41978,.F.) ;
#57681 = ORIENTED_EDGE('',*,*,#39608,.T.) ;
#57682 = ORIENTED_EDGE('',*,*,#41979,.F.) ;
#57683 = ORIENTED_EDGE('',*,*,#41972,.T.) ;
#57684 = ORIENTED_EDGE('',*,*,#41971,.T.) ;
#57685 = ORIENTED_EDGE('',*,*,#39682,.F.) ;
#57686 = ORIENTED_EDGE('',*,*,#41973,.T.) ;
#57687 = ORIENTED_EDGE('',*,*,#41980,.F.) ;
#57688 = ORIENTED_EDGE('',*,*,#41981,.F.) ;
#57689 = ORIENTED_EDGE('',*,*,#41976,.T.) ;
#57690 = ORIENTED_EDGE('',*,*,#41974,.T.) ;
#57691 = ORIENTED_EDGE('',*,*,#41982,.F.) ;
#57692 = ORIENTED_EDGE('',*,*,#39507,.T.) ;
#57693 = ORIENTED_EDGE('',*,*,#41977,.T.) ;
#57694 = ORIENTED_EDGE('',*,*,#39510,.F.) ;
#57695 = ORIENTED_EDGE('',*,*,#41983,.F.) ;
#57696 = ORIENTED_EDGE('',*,*,#39421,.F.) ;
#57697 = ORIENTED_EDGE('',*,*,#41978,.T.) ;
#57698 = ORIENTED_EDGE('',*,*,#39422,.F.) ;
#57699 = ORIENTED_EDGE('',*,*,#41984,.F.) ;
#57700 = ORIENTED_EDGE('',*,*,#39609,.F.) ;
#57701 = ORIENTED_EDGE('',*,*,#41979,.T.) ;
#57702 = ORIENTED_EDGE('',*,*,#39681,.T.) ;
#57703 = ORIENTED_EDGE('',*,*,#41985,.F.) ;
#57704 = ORIENTED_EDGE('',*,*,#41980,.T.) ;
#57705 = ORIENTED_EDGE('',*,*,#40473,.F.) ;
#57706 = ORIENTED_EDGE('',*,*,#41981,.T.) ;
#57707 = ORIENTED_EDGE('',*,*,#41986,.F.) ;
#57708 = ORIENTED_EDGE('',*,*,#41982,.T.) ;
#57709 = ORIENTED_EDGE('',*,*,#41984,.T.) ;
#57710 = ORIENTED_EDGE('',*,*,#41983,.T.) ;
#57711 = ORIENTED_EDGE('',*,*,#41987,.F.) ;
#57712 = ORIENTED_EDGE('',*,*,#39610,.T.) ;
#57713 = ORIENTED_EDGE('',*,*,#41985,.T.) ;
#57714 = ORIENTED_EDGE('',*,*,#39680,.F.) ;
#57715 = ORIENTED_EDGE('',*,*,#41988,.F.) ;
#57716 = ORIENTED_EDGE('',*,*,#39508,.F.) ;
#57717 = ORIENTED_EDGE('',*,*,#41986,.T.) ;
#57718 = ORIENTED_EDGE('',*,*,#41987,.T.) ;
#57719 = ORIENTED_EDGE('',*,*,#39509,.F.) ;
#57720 = ORIENTED_EDGE('',*,*,#41989,.F.) ;
#57721 = ORIENTED_EDGE('',*,*,#39611,.F.) ;
#57722 = ORIENTED_EDGE('',*,*,#41988,.T.) ;
#57723 = ORIENTED_EDGE('',*,*,#39538,.F.) ;
#57724 = ORIENTED_EDGE('',*,*,#41989,.T.) ;
#57725 = ORIENTED_EDGE('',*,*,#41990,.F.) ;
#57726 = ORIENTED_EDGE('',*,*,#41381,.F.) ;
#57727 = ORIENTED_EDGE('',*,*,#41991,.F.) ;
#57728 = ORIENTED_EDGE('',*,*,#41428,.F.) ;
#57729 = ORIENTED_EDGE('',*,*,#41991,.T.) ;
#57730 = ORIENTED_EDGE('',*,*,#41378,.F.) ;
#57731 = ORIENTED_EDGE('',*,*,#41992,.F.) ;
#57732 = ORIENTED_EDGE('',*,*,#41429,.F.) ;
#57733 = ORIENTED_EDGE('',*,*,#41384,.F.) ;
#57734 = ORIENTED_EDGE('',*,*,#41990,.T.) ;
#57735 = ORIENTED_EDGE('',*,*,#41993,.F.) ;
#57736 = ORIENTED_EDGE('',*,*,#41992,.T.) ;
#57737 = ORIENTED_EDGE('',*,*,#41375,.F.) ;
#57738 = ORIENTED_EDGE('',*,*,#41994,.F.) ;
#57739 = ORIENTED_EDGE('',*,*,#41430,.F.) ;
#57740 = ORIENTED_EDGE('',*,*,#41993,.T.) ;
#57741 = ORIENTED_EDGE('',*,*,#41427,.F.) ;
#57742 = ORIENTED_EDGE('',*,*,#41995,.F.) ;
#57743 = ORIENTED_EDGE('',*,*,#41387,.F.) ;
#57744 = ORIENTED_EDGE('',*,*,#41994,.T.) ;
#57745 = ORIENTED_EDGE('',*,*,#41372,.F.) ;
#57746 = ORIENTED_EDGE('',*,*,#41996,.F.) ;
#57747 = ORIENTED_EDGE('',*,*,#41431,.F.) ;
#57748 = ORIENTED_EDGE('',*,*,#41390,.F.) ;
#57749 = ORIENTED_EDGE('',*,*,#41995,.T.) ;
#57750 = ORIENTED_EDGE('',*,*,#41997,.F.) ;
#57751 = ORIENTED_EDGE('',*,*,#41996,.T.) ;
#57752 = ORIENTED_EDGE('',*,*,#41369,.F.) ;
#57753 = ORIENTED_EDGE('',*,*,#41998,.F.) ;
#57754 = ORIENTED_EDGE('',*,*,#41432,.F.) ;
#57755 = ORIENTED_EDGE('',*,*,#41997,.T.) ;
#57756 = ORIENTED_EDGE('',*,*,#41426,.F.) ;
#57757 = ORIENTED_EDGE('',*,*,#41999,.F.) ;
#57758 = ORIENTED_EDGE('',*,*,#41393,.F.) ;
#57759 = ORIENTED_EDGE('',*,*,#41998,.T.) ;
#57760 = ORIENTED_EDGE('',*,*,#41366,.F.) ;
#57761 = ORIENTED_EDGE('',*,*,#42000,.F.) ;
#57762 = ORIENTED_EDGE('',*,*,#41396,.F.) ;
#57763 = ORIENTED_EDGE('',*,*,#41999,.T.) ;
#57764 = ORIENTED_EDGE('',*,*,#42001,.F.) ;
#57765 = ORIENTED_EDGE('',*,*,#42000,.T.) ;
#57766 = ORIENTED_EDGE('',*,*,#41363,.F.) ;
#57767 = ORIENTED_EDGE('',*,*,#42002,.F.) ;
#57768 = ORIENTED_EDGE('',*,*,#41433,.F.) ;
#57769 = ORIENTED_EDGE('',*,*,#42001,.T.) ;
#57770 = ORIENTED_EDGE('',*,*,#41425,.F.) ;
#57771 = ORIENTED_EDGE('',*,*,#42003,.F.) ;
#57772 = ORIENTED_EDGE('',*,*,#41399,.F.) ;
#57773 = ORIENTED_EDGE('',*,*,#42002,.T.) ;
#57774 = ORIENTED_EDGE('',*,*,#39289,.F.) ;
#57775 = ORIENTED_EDGE('',*,*,#42004,.F.) ;
#57776 = ORIENTED_EDGE('',*,*,#41402,.F.) ;
#57777 = ORIENTED_EDGE('',*,*,#42003,.T.) ;
#57778 = ORIENTED_EDGE('',*,*,#42005,.F.) ;
#57779 = ORIENTED_EDGE('',*,*,#42004,.T.) ;
#57780 = ORIENTED_EDGE('',*,*,#41361,.F.) ;
#57781 = ORIENTED_EDGE('',*,*,#39216,.F.) ;
#57782 = ORIENTED_EDGE('',*,*,#41434,.F.) ;
#57783 = ORIENTED_EDGE('',*,*,#42005,.T.) ;
#57784 = ORIENTED_EDGE('',*,*,#41424,.F.) ;
#57785 = ORIENTED_EDGE('',*,*,#42006,.F.) ;
#57786 = ORIENTED_EDGE('',*,*,#41405,.F.) ;
#57787 = ORIENTED_EDGE('',*,*,#41408,.F.) ;
#57788 = ORIENTED_EDGE('',*,*,#42006,.T.) ;
#57789 = ORIENTED_EDGE('',*,*,#42007,.F.) ;
#57790 = ORIENTED_EDGE('',*,*,#39215,.T.) ;
#57791 = ORIENTED_EDGE('',*,*,#41356,.F.) ;
#57792 = ORIENTED_EDGE('',*,*,#42008,.F.) ;
#57793 = ORIENTED_EDGE('',*,*,#41435,.F.) ;
#57794 = ORIENTED_EDGE('',*,*,#42007,.T.) ;
#57795 = ORIENTED_EDGE('',*,*,#41423,.F.) ;
#57796 = ORIENTED_EDGE('',*,*,#42009,.F.) ;
#57797 = ORIENTED_EDGE('',*,*,#41411,.F.) ;
#57798 = ORIENTED_EDGE('',*,*,#42008,.T.) ;
#57799 = ORIENTED_EDGE('',*,*,#41353,.F.) ;
#57800 = ORIENTED_EDGE('',*,*,#42010,.F.) ;
#57801 = ORIENTED_EDGE('',*,*,#41414,.F.) ;
#57802 = ORIENTED_EDGE('',*,*,#42009,.T.) ;
#57803 = ORIENTED_EDGE('',*,*,#42011,.F.) ;
#57804 = ORIENTED_EDGE('',*,*,#42010,.T.) ;
#57805 = ORIENTED_EDGE('',*,*,#41350,.F.) ;
#57806 = ORIENTED_EDGE('',*,*,#42012,.F.) ;
#57807 = ORIENTED_EDGE('',*,*,#41436,.F.) ;
#57808 = ORIENTED_EDGE('',*,*,#42011,.T.) ;
#57809 = ORIENTED_EDGE('',*,*,#41422,.F.) ;
#57810 = ORIENTED_EDGE('',*,*,#42013,.F.) ;
#57811 = ORIENTED_EDGE('',*,*,#41417,.F.) ;
#57812 = ORIENTED_EDGE('',*,*,#42012,.T.) ;
#57813 = ORIENTED_EDGE('',*,*,#41347,.F.) ;
#57814 = ORIENTED_EDGE('',*,*,#42014,.F.) ;
#57815 = ORIENTED_EDGE('',*,*,#41419,.F.) ;
#57816 = ORIENTED_EDGE('',*,*,#42013,.T.) ;
#57817 = ORIENTED_EDGE('',*,*,#41421,.F.) ;
#57818 = ORIENTED_EDGE('',*,*,#42015,.F.) ;
#57819 = ORIENTED_EDGE('',*,*,#41341,.F.) ;
#57820 = ORIENTED_EDGE('',*,*,#42014,.T.) ;
#57821 = ORIENTED_EDGE('',*,*,#41344,.F.) ;
#57822 = ORIENTED_EDGE('',*,*,#42015,.T.) ;
#57823 = ORIENTED_EDGE('',*,*,#41420,.F.) ;
#57824 = ORIENTED_EDGE('',*,*,#42016,.F.) ;
#57825 = ORIENTED_EDGE('',*,*,#40540,.F.) ;
#57826 = ORIENTED_EDGE('',*,*,#42017,.F.) ;
#57827 = ORIENTED_EDGE('',*,*,#40469,.F.) ;
#57828 = ORIENTED_EDGE('',*,*,#42018,.F.) ;
#57829 = ORIENTED_EDGE('',*,*,#40541,.F.) ;
#57830 = ORIENTED_EDGE('',*,*,#42019,.F.) ;
#57831 = ORIENTED_EDGE('',*,*,#40535,.F.) ;
#57832 = ORIENTED_EDGE('',*,*,#42020,.F.) ;
#57833 = ORIENTED_EDGE('',*,*,#42018,.T.) ;
#57834 = ORIENTED_EDGE('',*,*,#42021,.F.) ;
#57835 = ORIENTED_EDGE('',*,*,#42022,.F.) ;
#57836 = ORIENTED_EDGE('',*,*,#42017,.T.) ;
#57837 = ORIENTED_EDGE('',*,*,#42023,.F.) ;
#57838 = ORIENTED_EDGE('',*,*,#42016,.T.) ;
#57839 = ORIENTED_EDGE('',*,*,#40468,.T.) ;
#57840 = ORIENTED_EDGE('',*,*,#42024,.F.) ;
#57841 = ORIENTED_EDGE('',*,*,#42019,.T.) ;
#57842 = ORIENTED_EDGE('',*,*,#42021,.T.) ;
#57843 = ORIENTED_EDGE('',*,*,#40538,.F.) ;
#57844 = ORIENTED_EDGE('',*,*,#42025,.F.) ;
#57845 = ORIENTED_EDGE('',*,*,#39200,.T.) ;
#57846 = ORIENTED_EDGE('',*,*,#42026,.T.) ;
#57847 = ORIENTED_EDGE('',*,*,#42027,.F.) ;
#57848 = ORIENTED_EDGE('',*,*,#42020,.T.) ;
#57849 = ORIENTED_EDGE('',*,*,#42028,.F.) ;
#57850 = ORIENTED_EDGE('',*,*,#42029,.T.) ;
#57851 = ORIENTED_EDGE('',*,*,#42030,.F.) ;
#57852 = ORIENTED_EDGE('',*,*,#39404,.F.) ;
#57853 = ORIENTED_EDGE('',*,*,#42031,.F.) ;
#57854 = ORIENTED_EDGE('',*,*,#40542,.F.) ;
#57855 = ORIENTED_EDGE('',*,*,#42023,.T.) ;
#57856 = ORIENTED_EDGE('',*,*,#40539,.F.) ;
#57857 = ORIENTED_EDGE('',*,*,#42032,.F.) ;
#57858 = ORIENTED_EDGE('',*,*,#40545,.F.) ;
#57859 = ORIENTED_EDGE('',*,*,#42022,.T.) ;
#57860 = ORIENTED_EDGE('',*,*,#40544,.F.) ;
#57861 = ORIENTED_EDGE('',*,*,#42033,.F.) ;
#57862 = ORIENTED_EDGE('',*,*,#40460,.F.) ;
#57863 = ORIENTED_EDGE('',*,*,#42024,.T.) ;
#57864 = ORIENTED_EDGE('',*,*,#40467,.F.) ;
#57865 = ORIENTED_EDGE('',*,*,#42034,.F.) ;
#57866 = ORIENTED_EDGE('',*,*,#40536,.F.) ;
#57867 = ORIENTED_EDGE('',*,*,#42035,.F.) ;
#57868 = ORIENTED_EDGE('',*,*,#40537,.F.) ;
#57869 = ORIENTED_EDGE('',*,*,#42036,.F.) ;
#57870 = ORIENTED_EDGE('',*,*,#40532,.F.) ;
#57871 = ORIENTED_EDGE('',*,*,#42025,.T.) ;
#57872 = ORIENTED_EDGE('',*,*,#42035,.T.) ;
#57873 = ORIENTED_EDGE('',*,*,#39201,.F.) ;
#57874 = ORIENTED_EDGE('',*,*,#42031,.T.) ;
#57875 = ORIENTED_EDGE('',*,*,#39414,.T.) ;
#57876 = ORIENTED_EDGE('',*,*,#42037,.F.) ;
#57877 = ORIENTED_EDGE('',*,*,#42032,.T.) ;
#57878 = ORIENTED_EDGE('',*,*,#42038,.F.) ;
#57879 = ORIENTED_EDGE('',*,*,#42033,.T.) ;
#57880 = ORIENTED_EDGE('',*,*,#42039,.F.) ;
#57881 = ORIENTED_EDGE('',*,*,#39502,.T.) ;
#57882 = ORIENTED_EDGE('',*,*,#42034,.T.) ;
#57883 = ORIENTED_EDGE('',*,*,#40466,.T.) ;
#57884 = ORIENTED_EDGE('',*,*,#42040,.F.) ;
#57885 = ORIENTED_EDGE('',*,*,#42036,.T.) ;
#57886 = ORIENTED_EDGE('',*,*,#42037,.T.) ;
#57887 = ORIENTED_EDGE('',*,*,#39413,.F.) ;
#57888 = ORIENTED_EDGE('',*,*,#42041,.F.) ;
#57889 = ORIENTED_EDGE('',*,*,#40546,.F.) ;
#57890 = ORIENTED_EDGE('',*,*,#42039,.T.) ;
#57891 = ORIENTED_EDGE('',*,*,#40543,.F.) ;
#57892 = ORIENTED_EDGE('',*,*,#42042,.F.) ;
#57893 = ORIENTED_EDGE('',*,*,#39503,.F.) ;
#57894 = ORIENTED_EDGE('',*,*,#40461,.F.) ;
#57895 = ORIENTED_EDGE('',*,*,#42038,.T.) ;
#57896 = ORIENTED_EDGE('',*,*,#42043,.F.) ;
#57897 = ORIENTED_EDGE('',*,*,#42044,.F.) ;
#57898 = ORIENTED_EDGE('',*,*,#42040,.T.) ;
#57899 = ORIENTED_EDGE('',*,*,#40465,.F.) ;
#57900 = ORIENTED_EDGE('',*,*,#42045,.F.) ;
#57901 = ORIENTED_EDGE('',*,*,#40533,.F.) ;
#57902 = ORIENTED_EDGE('',*,*,#42046,.F.) ;
#57903 = ORIENTED_EDGE('',*,*,#40534,.F.) ;
#57904 = ORIENTED_EDGE('',*,*,#42047,.F.) ;
#57905 = ORIENTED_EDGE('',*,*,#40528,.F.) ;
#57906 = ORIENTED_EDGE('',*,*,#39203,.T.) ;
#57907 = ORIENTED_EDGE('',*,*,#42046,.T.) ;
#57908 = ORIENTED_EDGE('',*,*,#42048,.F.) ;
#57909 = ORIENTED_EDGE('',*,*,#39408,.T.) ;
#57910 = ORIENTED_EDGE('',*,*,#42042,.T.) ;
#57911 = ORIENTED_EDGE('',*,*,#42041,.T.) ;
#57912 = ORIENTED_EDGE('',*,*,#42049,.F.) ;
#57913 = ORIENTED_EDGE('',*,*,#42050,.F.) ;
#57914 = ORIENTED_EDGE('',*,*,#39536,.F.) ;
#57915 = ORIENTED_EDGE('',*,*,#42051,.F.) ;
#57916 = ORIENTED_EDGE('',*,*,#42052,.F.) ;
#57917 = ORIENTED_EDGE('',*,*,#42043,.T.) ;
#57918 = ORIENTED_EDGE('',*,*,#39506,.F.) ;
#57919 = ORIENTED_EDGE('',*,*,#42051,.T.) ;
#57920 = ORIENTED_EDGE('',*,*,#39679,.F.) ;
#57921 = ORIENTED_EDGE('',*,*,#42044,.T.) ;
#57922 = ORIENTED_EDGE('',*,*,#42053,.F.) ;
#57923 = ORIENTED_EDGE('',*,*,#42054,.F.) ;
#57924 = ORIENTED_EDGE('',*,*,#42047,.T.) ;
#57925 = ORIENTED_EDGE('',*,*,#42045,.T.) ;
#57926 = ORIENTED_EDGE('',*,*,#42055,.F.) ;
#57927 = ORIENTED_EDGE('',*,*,#42048,.T.) ;
#57928 = ORIENTED_EDGE('',*,*,#40531,.F.) ;
#57929 = ORIENTED_EDGE('',*,*,#42056,.F.) ;
#57930 = ORIENTED_EDGE('',*,*,#39409,.F.) ;
#57931 = ORIENTED_EDGE('',*,*,#42049,.T.) ;
#57932 = ORIENTED_EDGE('',*,*,#39412,.F.) ;
#57933 = ORIENTED_EDGE('',*,*,#42057,.F.) ;
#57934 = ORIENTED_EDGE('',*,*,#39504,.F.) ;
#57935 = ORIENTED_EDGE('',*,*,#42050,.T.) ;
#57936 = ORIENTED_EDGE('',*,*,#39505,.F.) ;
#57937 = ORIENTED_EDGE('',*,*,#42058,.F.) ;
#57938 = ORIENTED_EDGE('',*,*,#39612,.F.) ;
#57939 = ORIENTED_EDGE('',*,*,#42052,.T.) ;
#57940 = ORIENTED_EDGE('',*,*,#39678,.T.) ;
#57941 = ORIENTED_EDGE('',*,*,#42059,.F.) ;
#57942 = ORIENTED_EDGE('',*,*,#42053,.T.) ;
#57943 = ORIENTED_EDGE('',*,*,#40462,.F.) ;
#57944 = ORIENTED_EDGE('',*,*,#42054,.T.) ;
#57945 = ORIENTED_EDGE('',*,*,#42060,.F.) ;
#57946 = ORIENTED_EDGE('',*,*,#42061,.F.) ;
#57947 = ORIENTED_EDGE('',*,*,#42055,.T.) ;
#57948 = ORIENTED_EDGE('',*,*,#40464,.F.) ;
#57949 = ORIENTED_EDGE('',*,*,#42062,.F.) ;
#57950 = ORIENTED_EDGE('',*,*,#40529,.F.) ;
#57951 = ORIENTED_EDGE('',*,*,#42063,.F.) ;
#57952 = ORIENTED_EDGE('',*,*,#40530,.F.) ;
#57953 = ORIENTED_EDGE('',*,*,#42064,.F.) ;
#57954 = ORIENTED_EDGE('',*,*,#39501,.F.) ;
#57955 = ORIENTED_EDGE('',*,*,#42056,.T.) ;
#57956 = ORIENTED_EDGE('',*,*,#42063,.T.) ;
#57957 = ORIENTED_EDGE('',*,*,#42065,.F.) ;
#57958 = ORIENTED_EDGE('',*,*,#42058,.T.) ;
#57959 = ORIENTED_EDGE('',*,*,#42057,.T.) ;
#57960 = ORIENTED_EDGE('',*,*,#42066,.F.) ;
#57961 = ORIENTED_EDGE('',*,*,#39613,.T.) ;
#57962 = ORIENTED_EDGE('',*,*,#42067,.F.) ;
#57963 = ORIENTED_EDGE('',*,*,#42060,.T.) ;
#57964 = ORIENTED_EDGE('',*,*,#42059,.T.) ;
#57965 = ORIENTED_EDGE('',*,*,#39677,.F.) ;
#57966 = ORIENTED_EDGE('',*,*,#42061,.T.) ;
#57967 = ORIENTED_EDGE('',*,*,#42068,.F.) ;
#57968 = ORIENTED_EDGE('',*,*,#42069,.F.) ;
#57969 = ORIENTED_EDGE('',*,*,#42064,.T.) ;
#57970 = ORIENTED_EDGE('',*,*,#42062,.T.) ;
#57971 = ORIENTED_EDGE('',*,*,#42070,.F.) ;
#57972 = ORIENTED_EDGE('',*,*,#39497,.T.) ;
#57973 = ORIENTED_EDGE('',*,*,#42065,.T.) ;
#57974 = ORIENTED_EDGE('',*,*,#39500,.F.) ;
#57975 = ORIENTED_EDGE('',*,*,#42071,.F.) ;
#57976 = ORIENTED_EDGE('',*,*,#39410,.F.) ;
#57977 = ORIENTED_EDGE('',*,*,#42066,.T.) ;
#57978 = ORIENTED_EDGE('',*,*,#39411,.F.) ;
#57979 = ORIENTED_EDGE('',*,*,#42072,.F.) ;
#57980 = ORIENTED_EDGE('',*,*,#39614,.F.) ;
#57981 = ORIENTED_EDGE('',*,*,#42067,.T.) ;
#57982 = ORIENTED_EDGE('',*,*,#39676,.T.) ;
#57983 = ORIENTED_EDGE('',*,*,#42073,.F.) ;
#57984 = ORIENTED_EDGE('',*,*,#42068,.T.) ;
#57985 = ORIENTED_EDGE('',*,*,#40463,.F.) ;
#57986 = ORIENTED_EDGE('',*,*,#42069,.T.) ;
#57987 = ORIENTED_EDGE('',*,*,#42074,.F.) ;
#57988 = ORIENTED_EDGE('',*,*,#42070,.T.) ;
#57989 = ORIENTED_EDGE('',*,*,#42072,.T.) ;
#57990 = ORIENTED_EDGE('',*,*,#42071,.T.) ;
#57991 = ORIENTED_EDGE('',*,*,#42075,.F.) ;
#57992 = ORIENTED_EDGE('',*,*,#39615,.T.) ;
#57993 = ORIENTED_EDGE('',*,*,#42073,.T.) ;
#57994 = ORIENTED_EDGE('',*,*,#39675,.F.) ;
#57995 = ORIENTED_EDGE('',*,*,#42076,.F.) ;
#57996 = ORIENTED_EDGE('',*,*,#39498,.F.) ;
#57997 = ORIENTED_EDGE('',*,*,#42074,.T.) ;
#57998 = ORIENTED_EDGE('',*,*,#42075,.T.) ;
#57999 = ORIENTED_EDGE('',*,*,#39499,.F.) ;
#58000 = ORIENTED_EDGE('',*,*,#42077,.F.) ;
#58001 = ORIENTED_EDGE('',*,*,#39616,.F.) ;
#58002 = ORIENTED_EDGE('',*,*,#42076,.T.) ;
#58003 = ORIENTED_EDGE('',*,*,#39542,.F.) ;
#58004 = ORIENTED_EDGE('',*,*,#42077,.T.) ;
#58005 = ORIENTED_EDGE('',*,*,#42078,.F.) ;
#58006 = ORIENTED_EDGE('',*,*,#41284,.F.) ;
#58007 = ORIENTED_EDGE('',*,*,#42079,.F.) ;
#58008 = ORIENTED_EDGE('',*,*,#41331,.F.) ;
#58009 = ORIENTED_EDGE('',*,*,#42079,.T.) ;
#58010 = ORIENTED_EDGE('',*,*,#41281,.F.) ;
#58011 = ORIENTED_EDGE('',*,*,#42080,.F.) ;
#58012 = ORIENTED_EDGE('',*,*,#41332,.F.) ;
#58013 = ORIENTED_EDGE('',*,*,#41287,.F.) ;
#58014 = ORIENTED_EDGE('',*,*,#42078,.T.) ;
#58015 = ORIENTED_EDGE('',*,*,#42081,.F.) ;
#58016 = ORIENTED_EDGE('',*,*,#42080,.T.) ;
#58017 = ORIENTED_EDGE('',*,*,#41278,.F.) ;
#58018 = ORIENTED_EDGE('',*,*,#42082,.F.) ;
#58019 = ORIENTED_EDGE('',*,*,#41333,.F.) ;
#58020 = ORIENTED_EDGE('',*,*,#42081,.T.) ;
#58021 = ORIENTED_EDGE('',*,*,#41330,.F.) ;
#58022 = ORIENTED_EDGE('',*,*,#42083,.F.) ;
#58023 = ORIENTED_EDGE('',*,*,#41290,.F.) ;
#58024 = ORIENTED_EDGE('',*,*,#42082,.T.) ;
#58025 = ORIENTED_EDGE('',*,*,#41275,.F.) ;
#58026 = ORIENTED_EDGE('',*,*,#42084,.F.) ;
#58027 = ORIENTED_EDGE('',*,*,#41334,.F.) ;
#58028 = ORIENTED_EDGE('',*,*,#41293,.F.) ;
#58029 = ORIENTED_EDGE('',*,*,#42083,.T.) ;
#58030 = ORIENTED_EDGE('',*,*,#42085,.F.) ;
#58031 = ORIENTED_EDGE('',*,*,#42084,.T.) ;
#58032 = ORIENTED_EDGE('',*,*,#41272,.F.) ;
#58033 = ORIENTED_EDGE('',*,*,#42086,.F.) ;
#58034 = ORIENTED_EDGE('',*,*,#41335,.F.) ;
#58035 = ORIENTED_EDGE('',*,*,#42085,.T.) ;
#58036 = ORIENTED_EDGE('',*,*,#41329,.F.) ;
#58037 = ORIENTED_EDGE('',*,*,#42087,.F.) ;
#58038 = ORIENTED_EDGE('',*,*,#41296,.F.) ;
#58039 = ORIENTED_EDGE('',*,*,#42086,.T.) ;
#58040 = ORIENTED_EDGE('',*,*,#41269,.F.) ;
#58041 = ORIENTED_EDGE('',*,*,#42088,.F.) ;
#58042 = ORIENTED_EDGE('',*,*,#41299,.F.) ;
#58043 = ORIENTED_EDGE('',*,*,#42087,.T.) ;
#58044 = ORIENTED_EDGE('',*,*,#42089,.F.) ;
#58045 = ORIENTED_EDGE('',*,*,#42088,.T.) ;
#58046 = ORIENTED_EDGE('',*,*,#41266,.F.) ;
#58047 = ORIENTED_EDGE('',*,*,#42090,.F.) ;
#58048 = ORIENTED_EDGE('',*,*,#41336,.F.) ;
#58049 = ORIENTED_EDGE('',*,*,#42089,.T.) ;
#58050 = ORIENTED_EDGE('',*,*,#41328,.F.) ;
#58051 = ORIENTED_EDGE('',*,*,#42091,.F.) ;
#58052 = ORIENTED_EDGE('',*,*,#41302,.F.) ;
#58053 = ORIENTED_EDGE('',*,*,#42090,.T.) ;
#58054 = ORIENTED_EDGE('',*,*,#39292,.F.) ;
#58055 = ORIENTED_EDGE('',*,*,#42092,.F.) ;
#58056 = ORIENTED_EDGE('',*,*,#41305,.F.) ;
#58057 = ORIENTED_EDGE('',*,*,#42091,.T.) ;
#58058 = ORIENTED_EDGE('',*,*,#42093,.F.) ;
#58059 = ORIENTED_EDGE('',*,*,#42092,.T.) ;
#58060 = ORIENTED_EDGE('',*,*,#41264,.F.) ;
#58061 = ORIENTED_EDGE('',*,*,#39199,.F.) ;
#58062 = ORIENTED_EDGE('',*,*,#41337,.F.) ;
#58063 = ORIENTED_EDGE('',*,*,#42093,.T.) ;
#58064 = ORIENTED_EDGE('',*,*,#41327,.F.) ;
#58065 = ORIENTED_EDGE('',*,*,#42094,.F.) ;
#58066 = ORIENTED_EDGE('',*,*,#41308,.F.) ;
#58067 = ORIENTED_EDGE('',*,*,#41311,.F.) ;
#58068 = ORIENTED_EDGE('',*,*,#42094,.T.) ;
#58069 = ORIENTED_EDGE('',*,*,#42095,.F.) ;
#58070 = ORIENTED_EDGE('',*,*,#39198,.T.) ;
#58071 = ORIENTED_EDGE('',*,*,#41259,.F.) ;
#58072 = ORIENTED_EDGE('',*,*,#42096,.F.) ;
#58073 = ORIENTED_EDGE('',*,*,#41338,.F.) ;
#58074 = ORIENTED_EDGE('',*,*,#42095,.T.) ;
#58075 = ORIENTED_EDGE('',*,*,#41326,.F.) ;
#58076 = ORIENTED_EDGE('',*,*,#42097,.F.) ;
#58077 = ORIENTED_EDGE('',*,*,#41314,.F.) ;
#58078 = ORIENTED_EDGE('',*,*,#42096,.T.) ;
#58079 = ORIENTED_EDGE('',*,*,#41256,.F.) ;
#58080 = ORIENTED_EDGE('',*,*,#42098,.F.) ;
#58081 = ORIENTED_EDGE('',*,*,#41317,.F.) ;
#58082 = ORIENTED_EDGE('',*,*,#42097,.T.) ;
#58083 = ORIENTED_EDGE('',*,*,#42099,.F.) ;
#58084 = ORIENTED_EDGE('',*,*,#42098,.T.) ;
#58085 = ORIENTED_EDGE('',*,*,#41253,.F.) ;
#58086 = ORIENTED_EDGE('',*,*,#42100,.F.) ;
#58087 = ORIENTED_EDGE('',*,*,#41339,.F.) ;
#58088 = ORIENTED_EDGE('',*,*,#42099,.T.) ;
#58089 = ORIENTED_EDGE('',*,*,#41325,.F.) ;
#58090 = ORIENTED_EDGE('',*,*,#42101,.F.) ;
#58091 = ORIENTED_EDGE('',*,*,#41320,.F.) ;
#58092 = ORIENTED_EDGE('',*,*,#42100,.T.) ;
#58093 = ORIENTED_EDGE('',*,*,#41250,.F.) ;
#58094 = ORIENTED_EDGE('',*,*,#42102,.F.) ;
#58095 = ORIENTED_EDGE('',*,*,#41322,.F.) ;
#58096 = ORIENTED_EDGE('',*,*,#42101,.T.) ;
#58097 = ORIENTED_EDGE('',*,*,#41324,.F.) ;
#58098 = ORIENTED_EDGE('',*,*,#42103,.F.) ;
#58099 = ORIENTED_EDGE('',*,*,#41244,.F.) ;
#58100 = ORIENTED_EDGE('',*,*,#42102,.T.) ;
#58101 = ORIENTED_EDGE('',*,*,#41247,.F.) ;
#58102 = ORIENTED_EDGE('',*,*,#42103,.T.) ;
#58103 = ORIENTED_EDGE('',*,*,#41323,.F.) ;
#58104 = ORIENTED_EDGE('',*,*,#42104,.F.) ;
#58105 = ORIENTED_EDGE('',*,*,#40559,.F.) ;
#58106 = ORIENTED_EDGE('',*,*,#42105,.F.) ;
#58107 = ORIENTED_EDGE('',*,*,#40459,.F.) ;
#58108 = ORIENTED_EDGE('',*,*,#42106,.F.) ;
#58109 = ORIENTED_EDGE('',*,*,#40560,.F.) ;
#58110 = ORIENTED_EDGE('',*,*,#42107,.F.) ;
#58111 = ORIENTED_EDGE('',*,*,#40554,.F.) ;
#58112 = ORIENTED_EDGE('',*,*,#42108,.F.) ;
#58113 = ORIENTED_EDGE('',*,*,#42106,.T.) ;
#58114 = ORIENTED_EDGE('',*,*,#42109,.F.) ;
#58115 = ORIENTED_EDGE('',*,*,#42110,.F.) ;
#58116 = ORIENTED_EDGE('',*,*,#42105,.T.) ;
#58117 = ORIENTED_EDGE('',*,*,#42111,.F.) ;
#58118 = ORIENTED_EDGE('',*,*,#42104,.T.) ;
#58119 = ORIENTED_EDGE('',*,*,#40458,.T.) ;
#58120 = ORIENTED_EDGE('',*,*,#42112,.F.) ;
#58121 = ORIENTED_EDGE('',*,*,#42107,.T.) ;
#58122 = ORIENTED_EDGE('',*,*,#42109,.T.) ;
#58123 = ORIENTED_EDGE('',*,*,#40557,.F.) ;
#58124 = ORIENTED_EDGE('',*,*,#42113,.F.) ;
#58125 = ORIENTED_EDGE('',*,*,#39183,.T.) ;
#58126 = ORIENTED_EDGE('',*,*,#42114,.T.) ;
#58127 = ORIENTED_EDGE('',*,*,#42115,.F.) ;
#58128 = ORIENTED_EDGE('',*,*,#42108,.T.) ;
#58129 = ORIENTED_EDGE('',*,*,#42116,.F.) ;
#58130 = ORIENTED_EDGE('',*,*,#42117,.T.) ;
#58131 = ORIENTED_EDGE('',*,*,#42118,.F.) ;
#58132 = ORIENTED_EDGE('',*,*,#39393,.F.) ;
#58133 = ORIENTED_EDGE('',*,*,#42119,.F.) ;
#58134 = ORIENTED_EDGE('',*,*,#40561,.F.) ;
#58135 = ORIENTED_EDGE('',*,*,#42111,.T.) ;
#58136 = ORIENTED_EDGE('',*,*,#40558,.F.) ;
#58137 = ORIENTED_EDGE('',*,*,#42120,.F.) ;
#58138 = ORIENTED_EDGE('',*,*,#40564,.F.) ;
#58139 = ORIENTED_EDGE('',*,*,#42110,.T.) ;
#58140 = ORIENTED_EDGE('',*,*,#40563,.F.) ;
#58141 = ORIENTED_EDGE('',*,*,#42121,.F.) ;
#58142 = ORIENTED_EDGE('',*,*,#40450,.F.) ;
#58143 = ORIENTED_EDGE('',*,*,#42112,.T.) ;
#58144 = ORIENTED_EDGE('',*,*,#40457,.F.) ;
#58145 = ORIENTED_EDGE('',*,*,#42122,.F.) ;
#58146 = ORIENTED_EDGE('',*,*,#40555,.F.) ;
#58147 = ORIENTED_EDGE('',*,*,#42123,.F.) ;
#58148 = ORIENTED_EDGE('',*,*,#40556,.F.) ;
#58149 = ORIENTED_EDGE('',*,*,#42124,.F.) ;
#58150 = ORIENTED_EDGE('',*,*,#40551,.F.) ;
#58151 = ORIENTED_EDGE('',*,*,#42113,.T.) ;
#58152 = ORIENTED_EDGE('',*,*,#42123,.T.) ;
#58153 = ORIENTED_EDGE('',*,*,#39184,.F.) ;
#58154 = ORIENTED_EDGE('',*,*,#42119,.T.) ;
#58155 = ORIENTED_EDGE('',*,*,#39403,.T.) ;
#58156 = ORIENTED_EDGE('',*,*,#42125,.F.) ;
#58157 = ORIENTED_EDGE('',*,*,#42120,.T.) ;
#58158 = ORIENTED_EDGE('',*,*,#42126,.F.) ;
#58159 = ORIENTED_EDGE('',*,*,#42121,.T.) ;
#58160 = ORIENTED_EDGE('',*,*,#42127,.F.) ;
#58161 = ORIENTED_EDGE('',*,*,#39492,.T.) ;
#58162 = ORIENTED_EDGE('',*,*,#42122,.T.) ;
#58163 = ORIENTED_EDGE('',*,*,#40456,.T.) ;
#58164 = ORIENTED_EDGE('',*,*,#42128,.F.) ;
#58165 = ORIENTED_EDGE('',*,*,#42124,.T.) ;
#58166 = ORIENTED_EDGE('',*,*,#42125,.T.) ;
#58167 = ORIENTED_EDGE('',*,*,#39402,.F.) ;
#58168 = ORIENTED_EDGE('',*,*,#42129,.F.) ;
#58169 = ORIENTED_EDGE('',*,*,#40565,.F.) ;
#58170 = ORIENTED_EDGE('',*,*,#42127,.T.) ;
#58171 = ORIENTED_EDGE('',*,*,#40562,.F.) ;
#58172 = ORIENTED_EDGE('',*,*,#42130,.F.) ;
#58173 = ORIENTED_EDGE('',*,*,#39493,.F.) ;
#58174 = ORIENTED_EDGE('',*,*,#40451,.F.) ;
#58175 = ORIENTED_EDGE('',*,*,#42126,.T.) ;
#58176 = ORIENTED_EDGE('',*,*,#42131,.F.) ;
#58177 = ORIENTED_EDGE('',*,*,#42132,.F.) ;
#58178 = ORIENTED_EDGE('',*,*,#42128,.T.) ;
#58179 = ORIENTED_EDGE('',*,*,#40455,.F.) ;
#58180 = ORIENTED_EDGE('',*,*,#42133,.F.) ;
#58181 = ORIENTED_EDGE('',*,*,#40552,.F.) ;
#58182 = ORIENTED_EDGE('',*,*,#42134,.F.) ;
#58183 = ORIENTED_EDGE('',*,*,#40553,.F.) ;
#58184 = ORIENTED_EDGE('',*,*,#42135,.F.) ;
#58185 = ORIENTED_EDGE('',*,*,#40547,.F.) ;
#58186 = ORIENTED_EDGE('',*,*,#39186,.T.) ;
#58187 = ORIENTED_EDGE('',*,*,#42134,.T.) ;
#58188 = ORIENTED_EDGE('',*,*,#42136,.F.) ;
#58189 = ORIENTED_EDGE('',*,*,#39397,.T.) ;
#58190 = ORIENTED_EDGE('',*,*,#42130,.T.) ;
#58191 = ORIENTED_EDGE('',*,*,#42129,.T.) ;
#58192 = ORIENTED_EDGE('',*,*,#42137,.F.) ;
#58193 = ORIENTED_EDGE('',*,*,#42138,.F.) ;
#58194 = ORIENTED_EDGE('',*,*,#39540,.F.) ;
#58195 = ORIENTED_EDGE('',*,*,#42139,.F.) ;
#58196 = ORIENTED_EDGE('',*,*,#42140,.F.) ;
#58197 = ORIENTED_EDGE('',*,*,#42131,.T.) ;
#58198 = ORIENTED_EDGE('',*,*,#39496,.F.) ;
#58199 = ORIENTED_EDGE('',*,*,#42139,.T.) ;
#58200 = ORIENTED_EDGE('',*,*,#39674,.F.) ;
#58201 = ORIENTED_EDGE('',*,*,#42132,.T.) ;
#58202 = ORIENTED_EDGE('',*,*,#42141,.F.) ;
#58203 = ORIENTED_EDGE('',*,*,#42142,.F.) ;
#58204 = ORIENTED_EDGE('',*,*,#42135,.T.) ;
#58205 = ORIENTED_EDGE('',*,*,#42133,.T.) ;
#58206 = ORIENTED_EDGE('',*,*,#42143,.F.) ;
#58207 = ORIENTED_EDGE('',*,*,#42136,.T.) ;
#58208 = ORIENTED_EDGE('',*,*,#40550,.F.) ;
#58209 = ORIENTED_EDGE('',*,*,#42144,.F.) ;
#58210 = ORIENTED_EDGE('',*,*,#39398,.F.) ;
#58211 = ORIENTED_EDGE('',*,*,#42137,.T.) ;
#58212 = ORIENTED_EDGE('',*,*,#39401,.F.) ;
#58213 = ORIENTED_EDGE('',*,*,#42145,.F.) ;
#58214 = ORIENTED_EDGE('',*,*,#39494,.F.) ;
#58215 = ORIENTED_EDGE('',*,*,#42138,.T.) ;
#58216 = ORIENTED_EDGE('',*,*,#39495,.F.) ;
#58217 = ORIENTED_EDGE('',*,*,#42146,.F.) ;
#58218 = ORIENTED_EDGE('',*,*,#39617,.F.) ;
#58219 = ORIENTED_EDGE('',*,*,#42140,.T.) ;
#58220 = ORIENTED_EDGE('',*,*,#39673,.T.) ;
#58221 = ORIENTED_EDGE('',*,*,#42147,.F.) ;
#58222 = ORIENTED_EDGE('',*,*,#42141,.T.) ;
#58223 = ORIENTED_EDGE('',*,*,#40452,.F.) ;
#58224 = ORIENTED_EDGE('',*,*,#42142,.T.) ;
#58225 = ORIENTED_EDGE('',*,*,#42148,.F.) ;
#58226 = ORIENTED_EDGE('',*,*,#42149,.F.) ;
#58227 = ORIENTED_EDGE('',*,*,#42143,.T.) ;
#58228 = ORIENTED_EDGE('',*,*,#40454,.F.) ;
#58229 = ORIENTED_EDGE('',*,*,#42150,.F.) ;
#58230 = ORIENTED_EDGE('',*,*,#40548,.F.) ;
#58231 = ORIENTED_EDGE('',*,*,#42151,.F.) ;
#58232 = ORIENTED_EDGE('',*,*,#40549,.F.) ;
#58233 = ORIENTED_EDGE('',*,*,#42152,.F.) ;
#58234 = ORIENTED_EDGE('',*,*,#39491,.F.) ;
#58235 = ORIENTED_EDGE('',*,*,#42144,.T.) ;
#58236 = ORIENTED_EDGE('',*,*,#42151,.T.) ;
#58237 = ORIENTED_EDGE('',*,*,#42153,.F.) ;
#58238 = ORIENTED_EDGE('',*,*,#42146,.T.) ;
#58239 = ORIENTED_EDGE('',*,*,#42145,.T.) ;
#58240 = ORIENTED_EDGE('',*,*,#42154,.F.) ;
#58241 = ORIENTED_EDGE('',*,*,#39618,.T.) ;
#58242 = ORIENTED_EDGE('',*,*,#42155,.F.) ;
#58243 = ORIENTED_EDGE('',*,*,#42148,.T.) ;
#58244 = ORIENTED_EDGE('',*,*,#42147,.T.) ;
#58245 = ORIENTED_EDGE('',*,*,#39672,.F.) ;
#58246 = ORIENTED_EDGE('',*,*,#42149,.T.) ;
#58247 = ORIENTED_EDGE('',*,*,#42156,.F.) ;
#58248 = ORIENTED_EDGE('',*,*,#42157,.F.) ;
#58249 = ORIENTED_EDGE('',*,*,#42152,.T.) ;
#58250 = ORIENTED_EDGE('',*,*,#42150,.T.) ;
#58251 = ORIENTED_EDGE('',*,*,#42158,.F.) ;
#58252 = ORIENTED_EDGE('',*,*,#39487,.T.) ;
#58253 = ORIENTED_EDGE('',*,*,#42153,.T.) ;
#58254 = ORIENTED_EDGE('',*,*,#39490,.F.) ;
#58255 = ORIENTED_EDGE('',*,*,#42159,.F.) ;
#58256 = ORIENTED_EDGE('',*,*,#39399,.F.) ;
#58257 = ORIENTED_EDGE('',*,*,#42154,.T.) ;
#58258 = ORIENTED_EDGE('',*,*,#39400,.F.) ;
#58259 = ORIENTED_EDGE('',*,*,#42160,.F.) ;
#58260 = ORIENTED_EDGE('',*,*,#39619,.F.) ;
#58261 = ORIENTED_EDGE('',*,*,#42155,.T.) ;
#58262 = ORIENTED_EDGE('',*,*,#39671,.T.) ;
#58263 = ORIENTED_EDGE('',*,*,#42161,.F.) ;
#58264 = ORIENTED_EDGE('',*,*,#42156,.T.) ;
#58265 = ORIENTED_EDGE('',*,*,#40453,.F.) ;
#58266 = ORIENTED_EDGE('',*,*,#42157,.T.) ;
#58267 = ORIENTED_EDGE('',*,*,#42162,.F.) ;
#58268 = ORIENTED_EDGE('',*,*,#42158,.T.) ;
#58269 = ORIENTED_EDGE('',*,*,#42160,.T.) ;
#58270 = ORIENTED_EDGE('',*,*,#42159,.T.) ;
#58271 = ORIENTED_EDGE('',*,*,#42163,.F.) ;
#58272 = ORIENTED_EDGE('',*,*,#39620,.T.) ;
#58273 = ORIENTED_EDGE('',*,*,#42161,.T.) ;
#58274 = ORIENTED_EDGE('',*,*,#39670,.F.) ;
#58275 = ORIENTED_EDGE('',*,*,#42164,.F.) ;
#58276 = ORIENTED_EDGE('',*,*,#39488,.F.) ;
#58277 = ORIENTED_EDGE('',*,*,#42162,.T.) ;
#58278 = ORIENTED_EDGE('',*,*,#42163,.T.) ;
#58279 = ORIENTED_EDGE('',*,*,#39489,.F.) ;
#58280 = ORIENTED_EDGE('',*,*,#42165,.F.) ;
#58281 = ORIENTED_EDGE('',*,*,#39621,.F.) ;
#58282 = ORIENTED_EDGE('',*,*,#42164,.T.) ;
#58283 = ORIENTED_EDGE('',*,*,#39546,.F.) ;
#58284 = ORIENTED_EDGE('',*,*,#42165,.T.) ;
#58285 = ORIENTED_EDGE('',*,*,#42166,.F.) ;
#58286 = ORIENTED_EDGE('',*,*,#41187,.F.) ;
#58287 = ORIENTED_EDGE('',*,*,#42167,.F.) ;
#58288 = ORIENTED_EDGE('',*,*,#41234,.F.) ;
#58289 = ORIENTED_EDGE('',*,*,#42167,.T.) ;
#58290 = ORIENTED_EDGE('',*,*,#41184,.F.) ;
#58291 = ORIENTED_EDGE('',*,*,#42168,.F.) ;
#58292 = ORIENTED_EDGE('',*,*,#41235,.F.) ;
#58293 = ORIENTED_EDGE('',*,*,#41190,.F.) ;
#58294 = ORIENTED_EDGE('',*,*,#42166,.T.) ;
#58295 = ORIENTED_EDGE('',*,*,#42169,.F.) ;
#58296 = ORIENTED_EDGE('',*,*,#42168,.T.) ;
#58297 = ORIENTED_EDGE('',*,*,#41181,.F.) ;
#58298 = ORIENTED_EDGE('',*,*,#42170,.F.) ;
#58299 = ORIENTED_EDGE('',*,*,#41236,.F.) ;
#58300 = ORIENTED_EDGE('',*,*,#42169,.T.) ;
#58301 = ORIENTED_EDGE('',*,*,#41233,.F.) ;
#58302 = ORIENTED_EDGE('',*,*,#42171,.F.) ;
#58303 = ORIENTED_EDGE('',*,*,#41193,.F.) ;
#58304 = ORIENTED_EDGE('',*,*,#42170,.T.) ;
#58305 = ORIENTED_EDGE('',*,*,#41178,.F.) ;
#58306 = ORIENTED_EDGE('',*,*,#42172,.F.) ;
#58307 = ORIENTED_EDGE('',*,*,#41237,.F.) ;
#58308 = ORIENTED_EDGE('',*,*,#41196,.F.) ;
#58309 = ORIENTED_EDGE('',*,*,#42171,.T.) ;
#58310 = ORIENTED_EDGE('',*,*,#42173,.F.) ;
#58311 = ORIENTED_EDGE('',*,*,#42172,.T.) ;
#58312 = ORIENTED_EDGE('',*,*,#41175,.F.) ;
#58313 = ORIENTED_EDGE('',*,*,#42174,.F.) ;
#58314 = ORIENTED_EDGE('',*,*,#41238,.F.) ;
#58315 = ORIENTED_EDGE('',*,*,#42173,.T.) ;
#58316 = ORIENTED_EDGE('',*,*,#41232,.F.) ;
#58317 = ORIENTED_EDGE('',*,*,#42175,.F.) ;
#58318 = ORIENTED_EDGE('',*,*,#41199,.F.) ;
#58319 = ORIENTED_EDGE('',*,*,#42174,.T.) ;
#58320 = ORIENTED_EDGE('',*,*,#41172,.F.) ;
#58321 = ORIENTED_EDGE('',*,*,#42176,.F.) ;
#58322 = ORIENTED_EDGE('',*,*,#41202,.F.) ;
#58323 = ORIENTED_EDGE('',*,*,#42175,.T.) ;
#58324 = ORIENTED_EDGE('',*,*,#42177,.F.) ;
#58325 = ORIENTED_EDGE('',*,*,#42176,.T.) ;
#58326 = ORIENTED_EDGE('',*,*,#41169,.F.) ;
#58327 = ORIENTED_EDGE('',*,*,#42178,.F.) ;
#58328 = ORIENTED_EDGE('',*,*,#41239,.F.) ;
#58329 = ORIENTED_EDGE('',*,*,#42177,.T.) ;
#58330 = ORIENTED_EDGE('',*,*,#41231,.F.) ;
#58331 = ORIENTED_EDGE('',*,*,#42179,.F.) ;
#58332 = ORIENTED_EDGE('',*,*,#41205,.F.) ;
#58333 = ORIENTED_EDGE('',*,*,#42178,.T.) ;
#58334 = ORIENTED_EDGE('',*,*,#39295,.F.) ;
#58335 = ORIENTED_EDGE('',*,*,#42180,.F.) ;
#58336 = ORIENTED_EDGE('',*,*,#41208,.F.) ;
#58337 = ORIENTED_EDGE('',*,*,#42179,.T.) ;
#58338 = ORIENTED_EDGE('',*,*,#42181,.F.) ;
#58339 = ORIENTED_EDGE('',*,*,#42180,.T.) ;
#58340 = ORIENTED_EDGE('',*,*,#41167,.F.) ;
#58341 = ORIENTED_EDGE('',*,*,#39182,.F.) ;
#58342 = ORIENTED_EDGE('',*,*,#41240,.F.) ;
#58343 = ORIENTED_EDGE('',*,*,#42181,.T.) ;
#58344 = ORIENTED_EDGE('',*,*,#41230,.F.) ;
#58345 = ORIENTED_EDGE('',*,*,#42182,.F.) ;
#58346 = ORIENTED_EDGE('',*,*,#41211,.F.) ;
#58347 = ORIENTED_EDGE('',*,*,#41214,.F.) ;
#58348 = ORIENTED_EDGE('',*,*,#42182,.T.) ;
#58349 = ORIENTED_EDGE('',*,*,#42183,.F.) ;
#58350 = ORIENTED_EDGE('',*,*,#39181,.T.) ;
#58351 = ORIENTED_EDGE('',*,*,#41162,.F.) ;
#58352 = ORIENTED_EDGE('',*,*,#42184,.F.) ;
#58353 = ORIENTED_EDGE('',*,*,#41241,.F.) ;
#58354 = ORIENTED_EDGE('',*,*,#42183,.T.) ;
#58355 = ORIENTED_EDGE('',*,*,#41229,.F.) ;
#58356 = ORIENTED_EDGE('',*,*,#42185,.F.) ;
#58357 = ORIENTED_EDGE('',*,*,#41217,.F.) ;
#58358 = ORIENTED_EDGE('',*,*,#42184,.T.) ;
#58359 = ORIENTED_EDGE('',*,*,#41159,.F.) ;
#58360 = ORIENTED_EDGE('',*,*,#42186,.F.) ;
#58361 = ORIENTED_EDGE('',*,*,#41220,.F.) ;
#58362 = ORIENTED_EDGE('',*,*,#42185,.T.) ;
#58363 = ORIENTED_EDGE('',*,*,#42187,.F.) ;
#58364 = ORIENTED_EDGE('',*,*,#42186,.T.) ;
#58365 = ORIENTED_EDGE('',*,*,#41156,.F.) ;
#58366 = ORIENTED_EDGE('',*,*,#42188,.F.) ;
#58367 = ORIENTED_EDGE('',*,*,#41242,.F.) ;
#58368 = ORIENTED_EDGE('',*,*,#42187,.T.) ;
#58369 = ORIENTED_EDGE('',*,*,#41228,.F.) ;
#58370 = ORIENTED_EDGE('',*,*,#42189,.F.) ;
#58371 = ORIENTED_EDGE('',*,*,#41223,.F.) ;
#58372 = ORIENTED_EDGE('',*,*,#42188,.T.) ;
#58373 = ORIENTED_EDGE('',*,*,#41153,.F.) ;
#58374 = ORIENTED_EDGE('',*,*,#42190,.F.) ;
#58375 = ORIENTED_EDGE('',*,*,#41225,.F.) ;
#58376 = ORIENTED_EDGE('',*,*,#42189,.T.) ;
#58377 = ORIENTED_EDGE('',*,*,#41227,.F.) ;
#58378 = ORIENTED_EDGE('',*,*,#42191,.F.) ;
#58379 = ORIENTED_EDGE('',*,*,#41147,.F.) ;
#58380 = ORIENTED_EDGE('',*,*,#42190,.T.) ;
#58381 = ORIENTED_EDGE('',*,*,#41150,.F.) ;
#58382 = ORIENTED_EDGE('',*,*,#42191,.T.) ;
#58383 = ORIENTED_EDGE('',*,*,#41226,.F.) ;
#58384 = ORIENTED_EDGE('',*,*,#42192,.F.) ;
#58385 = ORIENTED_EDGE('',*,*,#40578,.F.) ;
#58386 = ORIENTED_EDGE('',*,*,#42193,.F.) ;
#58387 = ORIENTED_EDGE('',*,*,#40449,.F.) ;
#58388 = ORIENTED_EDGE('',*,*,#42194,.F.) ;
#58389 = ORIENTED_EDGE('',*,*,#40579,.F.) ;
#58390 = ORIENTED_EDGE('',*,*,#42195,.F.) ;
#58391 = ORIENTED_EDGE('',*,*,#40573,.F.) ;
#58392 = ORIENTED_EDGE('',*,*,#42196,.F.) ;
#58393 = ORIENTED_EDGE('',*,*,#42194,.T.) ;
#58394 = ORIENTED_EDGE('',*,*,#42197,.F.) ;
#58395 = ORIENTED_EDGE('',*,*,#42198,.F.) ;
#58396 = ORIENTED_EDGE('',*,*,#42193,.T.) ;
#58397 = ORIENTED_EDGE('',*,*,#42199,.F.) ;
#58398 = ORIENTED_EDGE('',*,*,#42192,.T.) ;
#58399 = ORIENTED_EDGE('',*,*,#40448,.T.) ;
#58400 = ORIENTED_EDGE('',*,*,#42200,.F.) ;
#58401 = ORIENTED_EDGE('',*,*,#42195,.T.) ;
#58402 = ORIENTED_EDGE('',*,*,#42197,.T.) ;
#58403 = ORIENTED_EDGE('',*,*,#40576,.F.) ;
#58404 = ORIENTED_EDGE('',*,*,#42201,.F.) ;
#58405 = ORIENTED_EDGE('',*,*,#39166,.T.) ;
#58406 = ORIENTED_EDGE('',*,*,#42202,.T.) ;
#58407 = ORIENTED_EDGE('',*,*,#42203,.F.) ;
#58408 = ORIENTED_EDGE('',*,*,#42196,.T.) ;
#58409 = ORIENTED_EDGE('',*,*,#42204,.F.) ;
#58410 = ORIENTED_EDGE('',*,*,#42205,.T.) ;
#58411 = ORIENTED_EDGE('',*,*,#42206,.F.) ;
#58412 = ORIENTED_EDGE('',*,*,#39382,.F.) ;
#58413 = ORIENTED_EDGE('',*,*,#42207,.F.) ;
#58414 = ORIENTED_EDGE('',*,*,#40580,.F.) ;
#58415 = ORIENTED_EDGE('',*,*,#42199,.T.) ;
#58416 = ORIENTED_EDGE('',*,*,#40577,.F.) ;
#58417 = ORIENTED_EDGE('',*,*,#42208,.F.) ;
#58418 = ORIENTED_EDGE('',*,*,#40583,.F.) ;
#58419 = ORIENTED_EDGE('',*,*,#42198,.T.) ;
#58420 = ORIENTED_EDGE('',*,*,#40582,.F.) ;
#58421 = ORIENTED_EDGE('',*,*,#42209,.F.) ;
#58422 = ORIENTED_EDGE('',*,*,#40440,.F.) ;
#58423 = ORIENTED_EDGE('',*,*,#42200,.T.) ;
#58424 = ORIENTED_EDGE('',*,*,#40447,.F.) ;
#58425 = ORIENTED_EDGE('',*,*,#42210,.F.) ;
#58426 = ORIENTED_EDGE('',*,*,#40574,.F.) ;
#58427 = ORIENTED_EDGE('',*,*,#42211,.F.) ;
#58428 = ORIENTED_EDGE('',*,*,#40575,.F.) ;
#58429 = ORIENTED_EDGE('',*,*,#42212,.F.) ;
#58430 = ORIENTED_EDGE('',*,*,#40570,.F.) ;
#58431 = ORIENTED_EDGE('',*,*,#42201,.T.) ;
#58432 = ORIENTED_EDGE('',*,*,#42211,.T.) ;
#58433 = ORIENTED_EDGE('',*,*,#39167,.F.) ;
#58434 = ORIENTED_EDGE('',*,*,#42207,.T.) ;
#58435 = ORIENTED_EDGE('',*,*,#39392,.T.) ;
#58436 = ORIENTED_EDGE('',*,*,#42213,.F.) ;
#58437 = ORIENTED_EDGE('',*,*,#42208,.T.) ;
#58438 = ORIENTED_EDGE('',*,*,#42214,.F.) ;
#58439 = ORIENTED_EDGE('',*,*,#42209,.T.) ;
#58440 = ORIENTED_EDGE('',*,*,#42215,.F.) ;
#58441 = ORIENTED_EDGE('',*,*,#39482,.T.) ;
#58442 = ORIENTED_EDGE('',*,*,#42210,.T.) ;
#58443 = ORIENTED_EDGE('',*,*,#40446,.T.) ;
#58444 = ORIENTED_EDGE('',*,*,#42216,.F.) ;
#58445 = ORIENTED_EDGE('',*,*,#42212,.T.) ;
#58446 = ORIENTED_EDGE('',*,*,#42213,.T.) ;
#58447 = ORIENTED_EDGE('',*,*,#39391,.F.) ;
#58448 = ORIENTED_EDGE('',*,*,#42217,.F.) ;
#58449 = ORIENTED_EDGE('',*,*,#40584,.F.) ;
#58450 = ORIENTED_EDGE('',*,*,#42215,.T.) ;
#58451 = ORIENTED_EDGE('',*,*,#40581,.F.) ;
#58452 = ORIENTED_EDGE('',*,*,#42218,.F.) ;
#58453 = ORIENTED_EDGE('',*,*,#39483,.F.) ;
#58454 = ORIENTED_EDGE('',*,*,#40441,.F.) ;
#58455 = ORIENTED_EDGE('',*,*,#42214,.T.) ;
#58456 = ORIENTED_EDGE('',*,*,#42219,.F.) ;
#58457 = ORIENTED_EDGE('',*,*,#42220,.F.) ;
#58458 = ORIENTED_EDGE('',*,*,#42216,.T.) ;
#58459 = ORIENTED_EDGE('',*,*,#40445,.F.) ;
#58460 = ORIENTED_EDGE('',*,*,#42221,.F.) ;
#58461 = ORIENTED_EDGE('',*,*,#40571,.F.) ;
#58462 = ORIENTED_EDGE('',*,*,#42222,.F.) ;
#58463 = ORIENTED_EDGE('',*,*,#40572,.F.) ;
#58464 = ORIENTED_EDGE('',*,*,#42223,.F.) ;
#58465 = ORIENTED_EDGE('',*,*,#40566,.F.) ;
#58466 = ORIENTED_EDGE('',*,*,#39169,.T.) ;
#58467 = ORIENTED_EDGE('',*,*,#42222,.T.) ;
#58468 = ORIENTED_EDGE('',*,*,#42224,.F.) ;
#58469 = ORIENTED_EDGE('',*,*,#39386,.T.) ;
#58470 = ORIENTED_EDGE('',*,*,#42218,.T.) ;
#58471 = ORIENTED_EDGE('',*,*,#42217,.T.) ;
#58472 = ORIENTED_EDGE('',*,*,#42225,.F.) ;
#58473 = ORIENTED_EDGE('',*,*,#42226,.F.) ;
#58474 = ORIENTED_EDGE('',*,*,#39544,.F.) ;
#58475 = ORIENTED_EDGE('',*,*,#42227,.F.) ;
#58476 = ORIENTED_EDGE('',*,*,#42228,.F.) ;
#58477 = ORIENTED_EDGE('',*,*,#42219,.T.) ;
#58478 = ORIENTED_EDGE('',*,*,#39486,.F.) ;
#58479 = ORIENTED_EDGE('',*,*,#42227,.T.) ;
#58480 = ORIENTED_EDGE('',*,*,#39669,.F.) ;
#58481 = ORIENTED_EDGE('',*,*,#42220,.T.) ;
#58482 = ORIENTED_EDGE('',*,*,#42229,.F.) ;
#58483 = ORIENTED_EDGE('',*,*,#42230,.F.) ;
#58484 = ORIENTED_EDGE('',*,*,#42223,.T.) ;
#58485 = ORIENTED_EDGE('',*,*,#42221,.T.) ;
#58486 = ORIENTED_EDGE('',*,*,#42231,.F.) ;
#58487 = ORIENTED_EDGE('',*,*,#42224,.T.) ;
#58488 = ORIENTED_EDGE('',*,*,#40569,.F.) ;
#58489 = ORIENTED_EDGE('',*,*,#42232,.F.) ;
#58490 = ORIENTED_EDGE('',*,*,#39387,.F.) ;
#58491 = ORIENTED_EDGE('',*,*,#42225,.T.) ;
#58492 = ORIENTED_EDGE('',*,*,#39390,.F.) ;
#58493 = ORIENTED_EDGE('',*,*,#42233,.F.) ;
#58494 = ORIENTED_EDGE('',*,*,#39484,.F.) ;
#58495 = ORIENTED_EDGE('',*,*,#42226,.T.) ;
#58496 = ORIENTED_EDGE('',*,*,#39485,.F.) ;
#58497 = ORIENTED_EDGE('',*,*,#42234,.F.) ;
#58498 = ORIENTED_EDGE('',*,*,#39622,.F.) ;
#58499 = ORIENTED_EDGE('',*,*,#42228,.T.) ;
#58500 = ORIENTED_EDGE('',*,*,#39668,.T.) ;
#58501 = ORIENTED_EDGE('',*,*,#42235,.F.) ;
#58502 = ORIENTED_EDGE('',*,*,#42229,.T.) ;
#58503 = ORIENTED_EDGE('',*,*,#40442,.F.) ;
#58504 = ORIENTED_EDGE('',*,*,#42230,.T.) ;
#58505 = ORIENTED_EDGE('',*,*,#42236,.F.) ;
#58506 = ORIENTED_EDGE('',*,*,#42237,.F.) ;
#58507 = ORIENTED_EDGE('',*,*,#42231,.T.) ;
#58508 = ORIENTED_EDGE('',*,*,#40444,.F.) ;
#58509 = ORIENTED_EDGE('',*,*,#42238,.F.) ;
#58510 = ORIENTED_EDGE('',*,*,#40567,.F.) ;
#58511 = ORIENTED_EDGE('',*,*,#42239,.F.) ;
#58512 = ORIENTED_EDGE('',*,*,#40568,.F.) ;
#58513 = ORIENTED_EDGE('',*,*,#42240,.F.) ;
#58514 = ORIENTED_EDGE('',*,*,#39481,.F.) ;
#58515 = ORIENTED_EDGE('',*,*,#42232,.T.) ;
#58516 = ORIENTED_EDGE('',*,*,#42239,.T.) ;
#58517 = ORIENTED_EDGE('',*,*,#42241,.F.) ;
#58518 = ORIENTED_EDGE('',*,*,#42234,.T.) ;
#58519 = ORIENTED_EDGE('',*,*,#42233,.T.) ;
#58520 = ORIENTED_EDGE('',*,*,#42242,.F.) ;
#58521 = ORIENTED_EDGE('',*,*,#39623,.T.) ;
#58522 = ORIENTED_EDGE('',*,*,#42243,.F.) ;
#58523 = ORIENTED_EDGE('',*,*,#42236,.T.) ;
#58524 = ORIENTED_EDGE('',*,*,#42235,.T.) ;
#58525 = ORIENTED_EDGE('',*,*,#39667,.F.) ;
#58526 = ORIENTED_EDGE('',*,*,#42237,.T.) ;
#58527 = ORIENTED_EDGE('',*,*,#42244,.F.) ;
#58528 = ORIENTED_EDGE('',*,*,#42245,.F.) ;
#58529 = ORIENTED_EDGE('',*,*,#42240,.T.) ;
#58530 = ORIENTED_EDGE('',*,*,#42238,.T.) ;
#58531 = ORIENTED_EDGE('',*,*,#42246,.F.) ;
#58532 = ORIENTED_EDGE('',*,*,#39477,.T.) ;
#58533 = ORIENTED_EDGE('',*,*,#42241,.T.) ;
#58534 = ORIENTED_EDGE('',*,*,#39480,.F.) ;
#58535 = ORIENTED_EDGE('',*,*,#42247,.F.) ;
#58536 = ORIENTED_EDGE('',*,*,#39388,.F.) ;
#58537 = ORIENTED_EDGE('',*,*,#42242,.T.) ;
#58538 = ORIENTED_EDGE('',*,*,#39389,.F.) ;
#58539 = ORIENTED_EDGE('',*,*,#42248,.F.) ;
#58540 = ORIENTED_EDGE('',*,*,#39624,.F.) ;
#58541 = ORIENTED_EDGE('',*,*,#42243,.T.) ;
#58542 = ORIENTED_EDGE('',*,*,#39666,.T.) ;
#58543 = ORIENTED_EDGE('',*,*,#42249,.F.) ;
#58544 = ORIENTED_EDGE('',*,*,#42244,.T.) ;
#58545 = ORIENTED_EDGE('',*,*,#40443,.F.) ;
#58546 = ORIENTED_EDGE('',*,*,#42245,.T.) ;
#58547 = ORIENTED_EDGE('',*,*,#42250,.F.) ;
#58548 = ORIENTED_EDGE('',*,*,#42246,.T.) ;
#58549 = ORIENTED_EDGE('',*,*,#42248,.T.) ;
#58550 = ORIENTED_EDGE('',*,*,#42247,.T.) ;
#58551 = ORIENTED_EDGE('',*,*,#42251,.F.) ;
#58552 = ORIENTED_EDGE('',*,*,#39625,.T.) ;
#58553 = ORIENTED_EDGE('',*,*,#42249,.T.) ;
#58554 = ORIENTED_EDGE('',*,*,#39665,.F.) ;
#58555 = ORIENTED_EDGE('',*,*,#42252,.F.) ;
#58556 = ORIENTED_EDGE('',*,*,#39478,.F.) ;
#58557 = ORIENTED_EDGE('',*,*,#42250,.T.) ;
#58558 = ORIENTED_EDGE('',*,*,#42251,.T.) ;
#58559 = ORIENTED_EDGE('',*,*,#39479,.F.) ;
#58560 = ORIENTED_EDGE('',*,*,#42253,.F.) ;
#58561 = ORIENTED_EDGE('',*,*,#39626,.F.) ;
#58562 = ORIENTED_EDGE('',*,*,#42252,.T.) ;
#58563 = ORIENTED_EDGE('',*,*,#39550,.F.) ;
#58564 = ORIENTED_EDGE('',*,*,#42253,.T.) ;
#58565 = ORIENTED_EDGE('',*,*,#42254,.F.) ;
#58566 = ORIENTED_EDGE('',*,*,#41090,.F.) ;
#58567 = ORIENTED_EDGE('',*,*,#42255,.F.) ;
#58568 = ORIENTED_EDGE('',*,*,#41137,.F.) ;
#58569 = ORIENTED_EDGE('',*,*,#42255,.T.) ;
#58570 = ORIENTED_EDGE('',*,*,#41087,.F.) ;
#58571 = ORIENTED_EDGE('',*,*,#42256,.F.) ;
#58572 = ORIENTED_EDGE('',*,*,#41138,.F.) ;
#58573 = ORIENTED_EDGE('',*,*,#41093,.F.) ;
#58574 = ORIENTED_EDGE('',*,*,#42254,.T.) ;
#58575 = ORIENTED_EDGE('',*,*,#42257,.F.) ;
#58576 = ORIENTED_EDGE('',*,*,#42256,.T.) ;
#58577 = ORIENTED_EDGE('',*,*,#41084,.F.) ;
#58578 = ORIENTED_EDGE('',*,*,#42258,.F.) ;
#58579 = ORIENTED_EDGE('',*,*,#41139,.F.) ;
#58580 = ORIENTED_EDGE('',*,*,#42257,.T.) ;
#58581 = ORIENTED_EDGE('',*,*,#41136,.F.) ;
#58582 = ORIENTED_EDGE('',*,*,#42259,.F.) ;
#58583 = ORIENTED_EDGE('',*,*,#41096,.F.) ;
#58584 = ORIENTED_EDGE('',*,*,#42258,.T.) ;
#58585 = ORIENTED_EDGE('',*,*,#41081,.F.) ;
#58586 = ORIENTED_EDGE('',*,*,#42260,.F.) ;
#58587 = ORIENTED_EDGE('',*,*,#41140,.F.) ;
#58588 = ORIENTED_EDGE('',*,*,#41099,.F.) ;
#58589 = ORIENTED_EDGE('',*,*,#42259,.T.) ;
#58590 = ORIENTED_EDGE('',*,*,#42261,.F.) ;
#58591 = ORIENTED_EDGE('',*,*,#42260,.T.) ;
#58592 = ORIENTED_EDGE('',*,*,#41078,.F.) ;
#58593 = ORIENTED_EDGE('',*,*,#42262,.F.) ;
#58594 = ORIENTED_EDGE('',*,*,#41141,.F.) ;
#58595 = ORIENTED_EDGE('',*,*,#42261,.T.) ;
#58596 = ORIENTED_EDGE('',*,*,#41135,.F.) ;
#58597 = ORIENTED_EDGE('',*,*,#42263,.F.) ;
#58598 = ORIENTED_EDGE('',*,*,#41102,.F.) ;
#58599 = ORIENTED_EDGE('',*,*,#42262,.T.) ;
#58600 = ORIENTED_EDGE('',*,*,#41075,.F.) ;
#58601 = ORIENTED_EDGE('',*,*,#42264,.F.) ;
#58602 = ORIENTED_EDGE('',*,*,#41105,.F.) ;
#58603 = ORIENTED_EDGE('',*,*,#42263,.T.) ;
#58604 = ORIENTED_EDGE('',*,*,#42265,.F.) ;
#58605 = ORIENTED_EDGE('',*,*,#42264,.T.) ;
#58606 = ORIENTED_EDGE('',*,*,#41072,.F.) ;
#58607 = ORIENTED_EDGE('',*,*,#42266,.F.) ;
#58608 = ORIENTED_EDGE('',*,*,#41142,.F.) ;
#58609 = ORIENTED_EDGE('',*,*,#42265,.T.) ;
#58610 = ORIENTED_EDGE('',*,*,#41134,.F.) ;
#58611 = ORIENTED_EDGE('',*,*,#42267,.F.) ;
#58612 = ORIENTED_EDGE('',*,*,#41108,.F.) ;
#58613 = ORIENTED_EDGE('',*,*,#42266,.T.) ;
#58614 = ORIENTED_EDGE('',*,*,#39298,.F.) ;
#58615 = ORIENTED_EDGE('',*,*,#42268,.F.) ;
#58616 = ORIENTED_EDGE('',*,*,#41111,.F.) ;
#58617 = ORIENTED_EDGE('',*,*,#42267,.T.) ;
#58618 = ORIENTED_EDGE('',*,*,#42269,.F.) ;
#58619 = ORIENTED_EDGE('',*,*,#42268,.T.) ;
#58620 = ORIENTED_EDGE('',*,*,#41070,.F.) ;
#58621 = ORIENTED_EDGE('',*,*,#39165,.F.) ;
#58622 = ORIENTED_EDGE('',*,*,#41143,.F.) ;
#58623 = ORIENTED_EDGE('',*,*,#42269,.T.) ;
#58624 = ORIENTED_EDGE('',*,*,#41133,.F.) ;
#58625 = ORIENTED_EDGE('',*,*,#42270,.F.) ;
#58626 = ORIENTED_EDGE('',*,*,#41114,.F.) ;
#58627 = ORIENTED_EDGE('',*,*,#41117,.F.) ;
#58628 = ORIENTED_EDGE('',*,*,#42270,.T.) ;
#58629 = ORIENTED_EDGE('',*,*,#42271,.F.) ;
#58630 = ORIENTED_EDGE('',*,*,#39164,.T.) ;
#58631 = ORIENTED_EDGE('',*,*,#41065,.F.) ;
#58632 = ORIENTED_EDGE('',*,*,#42272,.F.) ;
#58633 = ORIENTED_EDGE('',*,*,#41144,.F.) ;
#58634 = ORIENTED_EDGE('',*,*,#42271,.T.) ;
#58635 = ORIENTED_EDGE('',*,*,#41132,.F.) ;
#58636 = ORIENTED_EDGE('',*,*,#42273,.F.) ;
#58637 = ORIENTED_EDGE('',*,*,#41120,.F.) ;
#58638 = ORIENTED_EDGE('',*,*,#42272,.T.) ;
#58639 = ORIENTED_EDGE('',*,*,#41062,.F.) ;
#58640 = ORIENTED_EDGE('',*,*,#42274,.F.) ;
#58641 = ORIENTED_EDGE('',*,*,#41123,.F.) ;
#58642 = ORIENTED_EDGE('',*,*,#42273,.T.) ;
#58643 = ORIENTED_EDGE('',*,*,#42275,.F.) ;
#58644 = ORIENTED_EDGE('',*,*,#42274,.T.) ;
#58645 = ORIENTED_EDGE('',*,*,#41059,.F.) ;
#58646 = ORIENTED_EDGE('',*,*,#42276,.F.) ;
#58647 = ORIENTED_EDGE('',*,*,#41145,.F.) ;
#58648 = ORIENTED_EDGE('',*,*,#42275,.T.) ;
#58649 = ORIENTED_EDGE('',*,*,#41131,.F.) ;
#58650 = ORIENTED_EDGE('',*,*,#42277,.F.) ;
#58651 = ORIENTED_EDGE('',*,*,#41126,.F.) ;
#58652 = ORIENTED_EDGE('',*,*,#42276,.T.) ;
#58653 = ORIENTED_EDGE('',*,*,#41056,.F.) ;
#58654 = ORIENTED_EDGE('',*,*,#42278,.F.) ;
#58655 = ORIENTED_EDGE('',*,*,#41128,.F.) ;
#58656 = ORIENTED_EDGE('',*,*,#42277,.T.) ;
#58657 = ORIENTED_EDGE('',*,*,#41130,.F.) ;
#58658 = ORIENTED_EDGE('',*,*,#42279,.F.) ;
#58659 = ORIENTED_EDGE('',*,*,#41050,.F.) ;
#58660 = ORIENTED_EDGE('',*,*,#42278,.T.) ;
#58661 = ORIENTED_EDGE('',*,*,#41053,.F.) ;
#58662 = ORIENTED_EDGE('',*,*,#42279,.T.) ;
#58663 = ORIENTED_EDGE('',*,*,#41129,.F.) ;
#58664 = ORIENTED_EDGE('',*,*,#42280,.F.) ;
#58665 = ORIENTED_EDGE('',*,*,#40597,.F.) ;
#58666 = ORIENTED_EDGE('',*,*,#42281,.F.) ;
#58667 = ORIENTED_EDGE('',*,*,#40439,.F.) ;
#58668 = ORIENTED_EDGE('',*,*,#42282,.F.) ;
#58669 = ORIENTED_EDGE('',*,*,#40598,.F.) ;
#58670 = ORIENTED_EDGE('',*,*,#42283,.F.) ;
#58671 = ORIENTED_EDGE('',*,*,#40592,.F.) ;
#58672 = ORIENTED_EDGE('',*,*,#42284,.F.) ;
#58673 = ORIENTED_EDGE('',*,*,#42282,.T.) ;
#58674 = ORIENTED_EDGE('',*,*,#42285,.F.) ;
#58675 = ORIENTED_EDGE('',*,*,#42286,.F.) ;
#58676 = ORIENTED_EDGE('',*,*,#42281,.T.) ;
#58677 = ORIENTED_EDGE('',*,*,#42287,.F.) ;
#58678 = ORIENTED_EDGE('',*,*,#42280,.T.) ;
#58679 = ORIENTED_EDGE('',*,*,#40438,.T.) ;
#58680 = ORIENTED_EDGE('',*,*,#42288,.F.) ;
#58681 = ORIENTED_EDGE('',*,*,#42283,.T.) ;
#58682 = ORIENTED_EDGE('',*,*,#42285,.T.) ;
#58683 = ORIENTED_EDGE('',*,*,#40595,.F.) ;
#58684 = ORIENTED_EDGE('',*,*,#42289,.F.) ;
#58685 = ORIENTED_EDGE('',*,*,#39149,.T.) ;
#58686 = ORIENTED_EDGE('',*,*,#42290,.T.) ;
#58687 = ORIENTED_EDGE('',*,*,#42291,.F.) ;
#58688 = ORIENTED_EDGE('',*,*,#42284,.T.) ;
#58689 = ORIENTED_EDGE('',*,*,#42292,.F.) ;
#58690 = ORIENTED_EDGE('',*,*,#42293,.T.) ;
#58691 = ORIENTED_EDGE('',*,*,#42294,.F.) ;
#58692 = ORIENTED_EDGE('',*,*,#39371,.F.) ;
#58693 = ORIENTED_EDGE('',*,*,#42295,.F.) ;
#58694 = ORIENTED_EDGE('',*,*,#40599,.F.) ;
#58695 = ORIENTED_EDGE('',*,*,#42287,.T.) ;
#58696 = ORIENTED_EDGE('',*,*,#40596,.F.) ;
#58697 = ORIENTED_EDGE('',*,*,#42296,.F.) ;
#58698 = ORIENTED_EDGE('',*,*,#40602,.F.) ;
#58699 = ORIENTED_EDGE('',*,*,#42286,.T.) ;
#58700 = ORIENTED_EDGE('',*,*,#40601,.F.) ;
#58701 = ORIENTED_EDGE('',*,*,#42297,.F.) ;
#58702 = ORIENTED_EDGE('',*,*,#40430,.F.) ;
#58703 = ORIENTED_EDGE('',*,*,#42288,.T.) ;
#58704 = ORIENTED_EDGE('',*,*,#40437,.F.) ;
#58705 = ORIENTED_EDGE('',*,*,#42298,.F.) ;
#58706 = ORIENTED_EDGE('',*,*,#40593,.F.) ;
#58707 = ORIENTED_EDGE('',*,*,#42299,.F.) ;
#58708 = ORIENTED_EDGE('',*,*,#40594,.F.) ;
#58709 = ORIENTED_EDGE('',*,*,#42300,.F.) ;
#58710 = ORIENTED_EDGE('',*,*,#40589,.F.) ;
#58711 = ORIENTED_EDGE('',*,*,#42289,.T.) ;
#58712 = ORIENTED_EDGE('',*,*,#42299,.T.) ;
#58713 = ORIENTED_EDGE('',*,*,#39150,.F.) ;
#58714 = ORIENTED_EDGE('',*,*,#42295,.T.) ;
#58715 = ORIENTED_EDGE('',*,*,#39381,.T.) ;
#58716 = ORIENTED_EDGE('',*,*,#42301,.F.) ;
#58717 = ORIENTED_EDGE('',*,*,#42296,.T.) ;
#58718 = ORIENTED_EDGE('',*,*,#42302,.F.) ;
#58719 = ORIENTED_EDGE('',*,*,#42297,.T.) ;
#58720 = ORIENTED_EDGE('',*,*,#42303,.F.) ;
#58721 = ORIENTED_EDGE('',*,*,#39472,.T.) ;
#58722 = ORIENTED_EDGE('',*,*,#42298,.T.) ;
#58723 = ORIENTED_EDGE('',*,*,#40436,.T.) ;
#58724 = ORIENTED_EDGE('',*,*,#42304,.F.) ;
#58725 = ORIENTED_EDGE('',*,*,#42300,.T.) ;
#58726 = ORIENTED_EDGE('',*,*,#42301,.T.) ;
#58727 = ORIENTED_EDGE('',*,*,#39380,.F.) ;
#58728 = ORIENTED_EDGE('',*,*,#42305,.F.) ;
#58729 = ORIENTED_EDGE('',*,*,#40603,.F.) ;
#58730 = ORIENTED_EDGE('',*,*,#42303,.T.) ;
#58731 = ORIENTED_EDGE('',*,*,#40600,.F.) ;
#58732 = ORIENTED_EDGE('',*,*,#42306,.F.) ;
#58733 = ORIENTED_EDGE('',*,*,#39473,.F.) ;
#58734 = ORIENTED_EDGE('',*,*,#40431,.F.) ;
#58735 = ORIENTED_EDGE('',*,*,#42302,.T.) ;
#58736 = ORIENTED_EDGE('',*,*,#42307,.F.) ;
#58737 = ORIENTED_EDGE('',*,*,#42308,.F.) ;
#58738 = ORIENTED_EDGE('',*,*,#42304,.T.) ;
#58739 = ORIENTED_EDGE('',*,*,#40435,.F.) ;
#58740 = ORIENTED_EDGE('',*,*,#42309,.F.) ;
#58741 = ORIENTED_EDGE('',*,*,#40590,.F.) ;
#58742 = ORIENTED_EDGE('',*,*,#42310,.F.) ;
#58743 = ORIENTED_EDGE('',*,*,#40591,.F.) ;
#58744 = ORIENTED_EDGE('',*,*,#42311,.F.) ;
#58745 = ORIENTED_EDGE('',*,*,#40585,.F.) ;
#58746 = ORIENTED_EDGE('',*,*,#39152,.T.) ;
#58747 = ORIENTED_EDGE('',*,*,#42310,.T.) ;
#58748 = ORIENTED_EDGE('',*,*,#42312,.F.) ;
#58749 = ORIENTED_EDGE('',*,*,#39375,.T.) ;
#58750 = ORIENTED_EDGE('',*,*,#42306,.T.) ;
#58751 = ORIENTED_EDGE('',*,*,#42305,.T.) ;
#58752 = ORIENTED_EDGE('',*,*,#42313,.F.) ;
#58753 = ORIENTED_EDGE('',*,*,#42314,.F.) ;
#58754 = ORIENTED_EDGE('',*,*,#39548,.F.) ;
#58755 = ORIENTED_EDGE('',*,*,#42315,.F.) ;
#58756 = ORIENTED_EDGE('',*,*,#42316,.F.) ;
#58757 = ORIENTED_EDGE('',*,*,#42307,.T.) ;
#58758 = ORIENTED_EDGE('',*,*,#39476,.F.) ;
#58759 = ORIENTED_EDGE('',*,*,#42315,.T.) ;
#58760 = ORIENTED_EDGE('',*,*,#39664,.F.) ;
#58761 = ORIENTED_EDGE('',*,*,#42308,.T.) ;
#58762 = ORIENTED_EDGE('',*,*,#42317,.F.) ;
#58763 = ORIENTED_EDGE('',*,*,#42318,.F.) ;
#58764 = ORIENTED_EDGE('',*,*,#42311,.T.) ;
#58765 = ORIENTED_EDGE('',*,*,#42309,.T.) ;
#58766 = ORIENTED_EDGE('',*,*,#42319,.F.) ;
#58767 = ORIENTED_EDGE('',*,*,#42312,.T.) ;
#58768 = ORIENTED_EDGE('',*,*,#40588,.F.) ;
#58769 = ORIENTED_EDGE('',*,*,#42320,.F.) ;
#58770 = ORIENTED_EDGE('',*,*,#39376,.F.) ;
#58771 = ORIENTED_EDGE('',*,*,#42313,.T.) ;
#58772 = ORIENTED_EDGE('',*,*,#39379,.F.) ;
#58773 = ORIENTED_EDGE('',*,*,#42321,.F.) ;
#58774 = ORIENTED_EDGE('',*,*,#39474,.F.) ;
#58775 = ORIENTED_EDGE('',*,*,#42314,.T.) ;
#58776 = ORIENTED_EDGE('',*,*,#39475,.F.) ;
#58777 = ORIENTED_EDGE('',*,*,#42322,.F.) ;
#58778 = ORIENTED_EDGE('',*,*,#39627,.F.) ;
#58779 = ORIENTED_EDGE('',*,*,#42316,.T.) ;
#58780 = ORIENTED_EDGE('',*,*,#39663,.T.) ;
#58781 = ORIENTED_EDGE('',*,*,#42323,.F.) ;
#58782 = ORIENTED_EDGE('',*,*,#42317,.T.) ;
#58783 = ORIENTED_EDGE('',*,*,#40432,.F.) ;
#58784 = ORIENTED_EDGE('',*,*,#42318,.T.) ;
#58785 = ORIENTED_EDGE('',*,*,#42324,.F.) ;
#58786 = ORIENTED_EDGE('',*,*,#42325,.F.) ;
#58787 = ORIENTED_EDGE('',*,*,#42319,.T.) ;
#58788 = ORIENTED_EDGE('',*,*,#40434,.F.) ;
#58789 = ORIENTED_EDGE('',*,*,#42326,.F.) ;
#58790 = ORIENTED_EDGE('',*,*,#40586,.F.) ;
#58791 = ORIENTED_EDGE('',*,*,#42327,.F.) ;
#58792 = ORIENTED_EDGE('',*,*,#40587,.F.) ;
#58793 = ORIENTED_EDGE('',*,*,#42328,.F.) ;
#58794 = ORIENTED_EDGE('',*,*,#39471,.F.) ;
#58795 = ORIENTED_EDGE('',*,*,#42320,.T.) ;
#58796 = ORIENTED_EDGE('',*,*,#42327,.T.) ;
#58797 = ORIENTED_EDGE('',*,*,#42329,.F.) ;
#58798 = ORIENTED_EDGE('',*,*,#42322,.T.) ;
#58799 = ORIENTED_EDGE('',*,*,#42321,.T.) ;
#58800 = ORIENTED_EDGE('',*,*,#42330,.F.) ;
#58801 = ORIENTED_EDGE('',*,*,#39628,.T.) ;
#58802 = ORIENTED_EDGE('',*,*,#42331,.F.) ;
#58803 = ORIENTED_EDGE('',*,*,#42324,.T.) ;
#58804 = ORIENTED_EDGE('',*,*,#42323,.T.) ;
#58805 = ORIENTED_EDGE('',*,*,#39662,.F.) ;
#58806 = ORIENTED_EDGE('',*,*,#42325,.T.) ;
#58807 = ORIENTED_EDGE('',*,*,#42332,.F.) ;
#58808 = ORIENTED_EDGE('',*,*,#42333,.F.) ;
#58809 = ORIENTED_EDGE('',*,*,#42328,.T.) ;
#58810 = ORIENTED_EDGE('',*,*,#42326,.T.) ;
#58811 = ORIENTED_EDGE('',*,*,#42334,.F.) ;
#58812 = ORIENTED_EDGE('',*,*,#39467,.T.) ;
#58813 = ORIENTED_EDGE('',*,*,#42329,.T.) ;
#58814 = ORIENTED_EDGE('',*,*,#39470,.F.) ;
#58815 = ORIENTED_EDGE('',*,*,#42335,.F.) ;
#58816 = ORIENTED_EDGE('',*,*,#39377,.F.) ;
#58817 = ORIENTED_EDGE('',*,*,#42330,.T.) ;
#58818 = ORIENTED_EDGE('',*,*,#39378,.F.) ;
#58819 = ORIENTED_EDGE('',*,*,#42336,.F.) ;
#58820 = ORIENTED_EDGE('',*,*,#39629,.F.) ;
#58821 = ORIENTED_EDGE('',*,*,#42331,.T.) ;
#58822 = ORIENTED_EDGE('',*,*,#39661,.T.) ;
#58823 = ORIENTED_EDGE('',*,*,#42337,.F.) ;
#58824 = ORIENTED_EDGE('',*,*,#42332,.T.) ;
#58825 = ORIENTED_EDGE('',*,*,#40433,.F.) ;
#58826 = ORIENTED_EDGE('',*,*,#42333,.T.) ;
#58827 = ORIENTED_EDGE('',*,*,#42338,.F.) ;
#58828 = ORIENTED_EDGE('',*,*,#42334,.T.) ;
#58829 = ORIENTED_EDGE('',*,*,#42336,.T.) ;
#58830 = ORIENTED_EDGE('',*,*,#42335,.T.) ;
#58831 = ORIENTED_EDGE('',*,*,#42339,.F.) ;
#58832 = ORIENTED_EDGE('',*,*,#39630,.T.) ;
#58833 = ORIENTED_EDGE('',*,*,#42337,.T.) ;
#58834 = ORIENTED_EDGE('',*,*,#39660,.F.) ;
#58835 = ORIENTED_EDGE('',*,*,#42340,.F.) ;
#58836 = ORIENTED_EDGE('',*,*,#39468,.F.) ;
#58837 = ORIENTED_EDGE('',*,*,#42338,.T.) ;
#58838 = ORIENTED_EDGE('',*,*,#42339,.T.) ;
#58839 = ORIENTED_EDGE('',*,*,#39469,.F.) ;
#58840 = ORIENTED_EDGE('',*,*,#42341,.F.) ;
#58841 = ORIENTED_EDGE('',*,*,#39631,.F.) ;
#58842 = ORIENTED_EDGE('',*,*,#42340,.T.) ;
#58843 = ORIENTED_EDGE('',*,*,#39554,.F.) ;
#58844 = ORIENTED_EDGE('',*,*,#42341,.T.) ;
#58845 = ORIENTED_EDGE('',*,*,#42342,.F.) ;
#58846 = ORIENTED_EDGE('',*,*,#40993,.F.) ;
#58847 = ORIENTED_EDGE('',*,*,#42343,.F.) ;
#58848 = ORIENTED_EDGE('',*,*,#41040,.F.) ;
#58849 = ORIENTED_EDGE('',*,*,#42343,.T.) ;
#58850 = ORIENTED_EDGE('',*,*,#40990,.F.) ;
#58851 = ORIENTED_EDGE('',*,*,#42344,.F.) ;
#58852 = ORIENTED_EDGE('',*,*,#41041,.F.) ;
#58853 = ORIENTED_EDGE('',*,*,#40996,.F.) ;
#58854 = ORIENTED_EDGE('',*,*,#42342,.T.) ;
#58855 = ORIENTED_EDGE('',*,*,#42345,.F.) ;
#58856 = ORIENTED_EDGE('',*,*,#42344,.T.) ;
#58857 = ORIENTED_EDGE('',*,*,#40987,.F.) ;
#58858 = ORIENTED_EDGE('',*,*,#42346,.F.) ;
#58859 = ORIENTED_EDGE('',*,*,#41042,.F.) ;
#58860 = ORIENTED_EDGE('',*,*,#42345,.T.) ;
#58861 = ORIENTED_EDGE('',*,*,#41039,.F.) ;
#58862 = ORIENTED_EDGE('',*,*,#42347,.F.) ;
#58863 = ORIENTED_EDGE('',*,*,#40999,.F.) ;
#58864 = ORIENTED_EDGE('',*,*,#42346,.T.) ;
#58865 = ORIENTED_EDGE('',*,*,#40984,.F.) ;
#58866 = ORIENTED_EDGE('',*,*,#42348,.F.) ;
#58867 = ORIENTED_EDGE('',*,*,#41043,.F.) ;
#58868 = ORIENTED_EDGE('',*,*,#41002,.F.) ;
#58869 = ORIENTED_EDGE('',*,*,#42347,.T.) ;
#58870 = ORIENTED_EDGE('',*,*,#42349,.F.) ;
#58871 = ORIENTED_EDGE('',*,*,#42348,.T.) ;
#58872 = ORIENTED_EDGE('',*,*,#40981,.F.) ;
#58873 = ORIENTED_EDGE('',*,*,#42350,.F.) ;
#58874 = ORIENTED_EDGE('',*,*,#41044,.F.) ;
#58875 = ORIENTED_EDGE('',*,*,#42349,.T.) ;
#58876 = ORIENTED_EDGE('',*,*,#41038,.F.) ;
#58877 = ORIENTED_EDGE('',*,*,#42351,.F.) ;
#58878 = ORIENTED_EDGE('',*,*,#41005,.F.) ;
#58879 = ORIENTED_EDGE('',*,*,#42350,.T.) ;
#58880 = ORIENTED_EDGE('',*,*,#40978,.F.) ;
#58881 = ORIENTED_EDGE('',*,*,#42352,.F.) ;
#58882 = ORIENTED_EDGE('',*,*,#41008,.F.) ;
#58883 = ORIENTED_EDGE('',*,*,#42351,.T.) ;
#58884 = ORIENTED_EDGE('',*,*,#42353,.F.) ;
#58885 = ORIENTED_EDGE('',*,*,#42352,.T.) ;
#58886 = ORIENTED_EDGE('',*,*,#40975,.F.) ;
#58887 = ORIENTED_EDGE('',*,*,#42354,.F.) ;
#58888 = ORIENTED_EDGE('',*,*,#41045,.F.) ;
#58889 = ORIENTED_EDGE('',*,*,#42353,.T.) ;
#58890 = ORIENTED_EDGE('',*,*,#41037,.F.) ;
#58891 = ORIENTED_EDGE('',*,*,#42355,.F.) ;
#58892 = ORIENTED_EDGE('',*,*,#41011,.F.) ;
#58893 = ORIENTED_EDGE('',*,*,#42354,.T.) ;
#58894 = ORIENTED_EDGE('',*,*,#39301,.F.) ;
#58895 = ORIENTED_EDGE('',*,*,#42356,.F.) ;
#58896 = ORIENTED_EDGE('',*,*,#41014,.F.) ;
#58897 = ORIENTED_EDGE('',*,*,#42355,.T.) ;
#58898 = ORIENTED_EDGE('',*,*,#42357,.F.) ;
#58899 = ORIENTED_EDGE('',*,*,#42356,.T.) ;
#58900 = ORIENTED_EDGE('',*,*,#40973,.F.) ;
#58901 = ORIENTED_EDGE('',*,*,#39148,.F.) ;
#58902 = ORIENTED_EDGE('',*,*,#41046,.F.) ;
#58903 = ORIENTED_EDGE('',*,*,#42357,.T.) ;
#58904 = ORIENTED_EDGE('',*,*,#41036,.F.) ;
#58905 = ORIENTED_EDGE('',*,*,#42358,.F.) ;
#58906 = ORIENTED_EDGE('',*,*,#41017,.F.) ;
#58907 = ORIENTED_EDGE('',*,*,#41020,.F.) ;
#58908 = ORIENTED_EDGE('',*,*,#42358,.T.) ;
#58909 = ORIENTED_EDGE('',*,*,#42359,.F.) ;
#58910 = ORIENTED_EDGE('',*,*,#39147,.T.) ;
#58911 = ORIENTED_EDGE('',*,*,#40968,.F.) ;
#58912 = ORIENTED_EDGE('',*,*,#42360,.F.) ;
#58913 = ORIENTED_EDGE('',*,*,#41047,.F.) ;
#58914 = ORIENTED_EDGE('',*,*,#42359,.T.) ;
#58915 = ORIENTED_EDGE('',*,*,#41035,.F.) ;
#58916 = ORIENTED_EDGE('',*,*,#42361,.F.) ;
#58917 = ORIENTED_EDGE('',*,*,#41023,.F.) ;
#58918 = ORIENTED_EDGE('',*,*,#42360,.T.) ;
#58919 = ORIENTED_EDGE('',*,*,#40965,.F.) ;
#58920 = ORIENTED_EDGE('',*,*,#42362,.F.) ;
#58921 = ORIENTED_EDGE('',*,*,#41026,.F.) ;
#58922 = ORIENTED_EDGE('',*,*,#42361,.T.) ;
#58923 = ORIENTED_EDGE('',*,*,#42363,.F.) ;
#58924 = ORIENTED_EDGE('',*,*,#42362,.T.) ;
#58925 = ORIENTED_EDGE('',*,*,#40962,.F.) ;
#58926 = ORIENTED_EDGE('',*,*,#42364,.F.) ;
#58927 = ORIENTED_EDGE('',*,*,#41048,.F.) ;
#58928 = ORIENTED_EDGE('',*,*,#42363,.T.) ;
#58929 = ORIENTED_EDGE('',*,*,#41034,.F.) ;
#58930 = ORIENTED_EDGE('',*,*,#42365,.F.) ;
#58931 = ORIENTED_EDGE('',*,*,#41029,.F.) ;
#58932 = ORIENTED_EDGE('',*,*,#42364,.T.) ;
#58933 = ORIENTED_EDGE('',*,*,#40959,.F.) ;
#58934 = ORIENTED_EDGE('',*,*,#42366,.F.) ;
#58935 = ORIENTED_EDGE('',*,*,#41031,.F.) ;
#58936 = ORIENTED_EDGE('',*,*,#42365,.T.) ;
#58937 = ORIENTED_EDGE('',*,*,#41033,.F.) ;
#58938 = ORIENTED_EDGE('',*,*,#42367,.F.) ;
#58939 = ORIENTED_EDGE('',*,*,#40953,.F.) ;
#58940 = ORIENTED_EDGE('',*,*,#42366,.T.) ;
#58941 = ORIENTED_EDGE('',*,*,#40956,.F.) ;
#58942 = ORIENTED_EDGE('',*,*,#42367,.T.) ;
#58943 = ORIENTED_EDGE('',*,*,#41032,.F.) ;
#58944 = ORIENTED_EDGE('',*,*,#42368,.F.) ;
#58945 = ORIENTED_EDGE('',*,*,#40616,.F.) ;
#58946 = ORIENTED_EDGE('',*,*,#42369,.F.) ;
#58947 = ORIENTED_EDGE('',*,*,#40429,.F.) ;
#58948 = ORIENTED_EDGE('',*,*,#42370,.F.) ;
#58949 = ORIENTED_EDGE('',*,*,#40617,.F.) ;
#58950 = ORIENTED_EDGE('',*,*,#42371,.F.) ;
#58951 = ORIENTED_EDGE('',*,*,#40611,.F.) ;
#58952 = ORIENTED_EDGE('',*,*,#42372,.F.) ;
#58953 = ORIENTED_EDGE('',*,*,#42370,.T.) ;
#58954 = ORIENTED_EDGE('',*,*,#42373,.F.) ;
#58955 = ORIENTED_EDGE('',*,*,#42374,.F.) ;
#58956 = ORIENTED_EDGE('',*,*,#42369,.T.) ;
#58957 = ORIENTED_EDGE('',*,*,#42375,.F.) ;
#58958 = ORIENTED_EDGE('',*,*,#42368,.T.) ;
#58959 = ORIENTED_EDGE('',*,*,#40428,.T.) ;
#58960 = ORIENTED_EDGE('',*,*,#42376,.F.) ;
#58961 = ORIENTED_EDGE('',*,*,#42371,.T.) ;
#58962 = ORIENTED_EDGE('',*,*,#42373,.T.) ;
#58963 = ORIENTED_EDGE('',*,*,#40614,.F.) ;
#58964 = ORIENTED_EDGE('',*,*,#42377,.F.) ;
#58965 = ORIENTED_EDGE('',*,*,#39132,.T.) ;
#58966 = ORIENTED_EDGE('',*,*,#42378,.T.) ;
#58967 = ORIENTED_EDGE('',*,*,#42379,.F.) ;
#58968 = ORIENTED_EDGE('',*,*,#42372,.T.) ;
#58969 = ORIENTED_EDGE('',*,*,#42380,.F.) ;
#58970 = ORIENTED_EDGE('',*,*,#42381,.T.) ;
#58971 = ORIENTED_EDGE('',*,*,#42382,.F.) ;
#58972 = ORIENTED_EDGE('',*,*,#39360,.F.) ;
#58973 = ORIENTED_EDGE('',*,*,#42383,.F.) ;
#58974 = ORIENTED_EDGE('',*,*,#40618,.F.) ;
#58975 = ORIENTED_EDGE('',*,*,#42375,.T.) ;
#58976 = ORIENTED_EDGE('',*,*,#40615,.F.) ;
#58977 = ORIENTED_EDGE('',*,*,#42384,.F.) ;
#58978 = ORIENTED_EDGE('',*,*,#40621,.F.) ;
#58979 = ORIENTED_EDGE('',*,*,#42374,.T.) ;
#58980 = ORIENTED_EDGE('',*,*,#40620,.F.) ;
#58981 = ORIENTED_EDGE('',*,*,#42385,.F.) ;
#58982 = ORIENTED_EDGE('',*,*,#40420,.F.) ;
#58983 = ORIENTED_EDGE('',*,*,#42376,.T.) ;
#58984 = ORIENTED_EDGE('',*,*,#40427,.F.) ;
#58985 = ORIENTED_EDGE('',*,*,#42386,.F.) ;
#58986 = ORIENTED_EDGE('',*,*,#40612,.F.) ;
#58987 = ORIENTED_EDGE('',*,*,#42387,.F.) ;
#58988 = ORIENTED_EDGE('',*,*,#40613,.F.) ;
#58989 = ORIENTED_EDGE('',*,*,#42388,.F.) ;
#58990 = ORIENTED_EDGE('',*,*,#40608,.F.) ;
#58991 = ORIENTED_EDGE('',*,*,#42377,.T.) ;
#58992 = ORIENTED_EDGE('',*,*,#42387,.T.) ;
#58993 = ORIENTED_EDGE('',*,*,#39133,.F.) ;
#58994 = ORIENTED_EDGE('',*,*,#42383,.T.) ;
#58995 = ORIENTED_EDGE('',*,*,#39370,.T.) ;
#58996 = ORIENTED_EDGE('',*,*,#42389,.F.) ;
#58997 = ORIENTED_EDGE('',*,*,#42384,.T.) ;
#58998 = ORIENTED_EDGE('',*,*,#42390,.F.) ;
#58999 = ORIENTED_EDGE('',*,*,#42385,.T.) ;
#59000 = ORIENTED_EDGE('',*,*,#42391,.F.) ;
#59001 = ORIENTED_EDGE('',*,*,#39462,.T.) ;
#59002 = ORIENTED_EDGE('',*,*,#42386,.T.) ;
#59003 = ORIENTED_EDGE('',*,*,#40426,.T.) ;
#59004 = ORIENTED_EDGE('',*,*,#42392,.F.) ;
#59005 = ORIENTED_EDGE('',*,*,#42388,.T.) ;
#59006 = ORIENTED_EDGE('',*,*,#42389,.T.) ;
#59007 = ORIENTED_EDGE('',*,*,#39369,.F.) ;
#59008 = ORIENTED_EDGE('',*,*,#42393,.F.) ;
#59009 = ORIENTED_EDGE('',*,*,#40622,.F.) ;
#59010 = ORIENTED_EDGE('',*,*,#42391,.T.) ;
#59011 = ORIENTED_EDGE('',*,*,#40619,.F.) ;
#59012 = ORIENTED_EDGE('',*,*,#42394,.F.) ;
#59013 = ORIENTED_EDGE('',*,*,#39463,.F.) ;
#59014 = ORIENTED_EDGE('',*,*,#40421,.F.) ;
#59015 = ORIENTED_EDGE('',*,*,#42390,.T.) ;
#59016 = ORIENTED_EDGE('',*,*,#42395,.F.) ;
#59017 = ORIENTED_EDGE('',*,*,#42396,.F.) ;
#59018 = ORIENTED_EDGE('',*,*,#42392,.T.) ;
#59019 = ORIENTED_EDGE('',*,*,#40425,.F.) ;
#59020 = ORIENTED_EDGE('',*,*,#42397,.F.) ;
#59021 = ORIENTED_EDGE('',*,*,#40609,.F.) ;
#59022 = ORIENTED_EDGE('',*,*,#42398,.F.) ;
#59023 = ORIENTED_EDGE('',*,*,#40610,.F.) ;
#59024 = ORIENTED_EDGE('',*,*,#42399,.F.) ;
#59025 = ORIENTED_EDGE('',*,*,#40604,.F.) ;
#59026 = ORIENTED_EDGE('',*,*,#39135,.T.) ;
#59027 = ORIENTED_EDGE('',*,*,#42398,.T.) ;
#59028 = ORIENTED_EDGE('',*,*,#42400,.F.) ;
#59029 = ORIENTED_EDGE('',*,*,#39364,.T.) ;
#59030 = ORIENTED_EDGE('',*,*,#42394,.T.) ;
#59031 = ORIENTED_EDGE('',*,*,#42393,.T.) ;
#59032 = ORIENTED_EDGE('',*,*,#42401,.F.) ;
#59033 = ORIENTED_EDGE('',*,*,#42402,.F.) ;
#59034 = ORIENTED_EDGE('',*,*,#39552,.F.) ;
#59035 = ORIENTED_EDGE('',*,*,#42403,.F.) ;
#59036 = ORIENTED_EDGE('',*,*,#42404,.F.) ;
#59037 = ORIENTED_EDGE('',*,*,#42395,.T.) ;
#59038 = ORIENTED_EDGE('',*,*,#39466,.F.) ;
#59039 = ORIENTED_EDGE('',*,*,#42403,.T.) ;
#59040 = ORIENTED_EDGE('',*,*,#39659,.F.) ;
#59041 = ORIENTED_EDGE('',*,*,#42396,.T.) ;
#59042 = ORIENTED_EDGE('',*,*,#42405,.F.) ;
#59043 = ORIENTED_EDGE('',*,*,#42406,.F.) ;
#59044 = ORIENTED_EDGE('',*,*,#42399,.T.) ;
#59045 = ORIENTED_EDGE('',*,*,#42397,.T.) ;
#59046 = ORIENTED_EDGE('',*,*,#42407,.F.) ;
#59047 = ORIENTED_EDGE('',*,*,#42400,.T.) ;
#59048 = ORIENTED_EDGE('',*,*,#40607,.F.) ;
#59049 = ORIENTED_EDGE('',*,*,#42408,.F.) ;
#59050 = ORIENTED_EDGE('',*,*,#39365,.F.) ;
#59051 = ORIENTED_EDGE('',*,*,#42401,.T.) ;
#59052 = ORIENTED_EDGE('',*,*,#39368,.F.) ;
#59053 = ORIENTED_EDGE('',*,*,#42409,.F.) ;
#59054 = ORIENTED_EDGE('',*,*,#39464,.F.) ;
#59055 = ORIENTED_EDGE('',*,*,#42402,.T.) ;
#59056 = ORIENTED_EDGE('',*,*,#39465,.F.) ;
#59057 = ORIENTED_EDGE('',*,*,#42410,.F.) ;
#59058 = ORIENTED_EDGE('',*,*,#39632,.F.) ;
#59059 = ORIENTED_EDGE('',*,*,#42404,.T.) ;
#59060 = ORIENTED_EDGE('',*,*,#39658,.T.) ;
#59061 = ORIENTED_EDGE('',*,*,#42411,.F.) ;
#59062 = ORIENTED_EDGE('',*,*,#42405,.T.) ;
#59063 = ORIENTED_EDGE('',*,*,#40422,.F.) ;
#59064 = ORIENTED_EDGE('',*,*,#42406,.T.) ;
#59065 = ORIENTED_EDGE('',*,*,#42412,.F.) ;
#59066 = ORIENTED_EDGE('',*,*,#42413,.F.) ;
#59067 = ORIENTED_EDGE('',*,*,#42407,.T.) ;
#59068 = ORIENTED_EDGE('',*,*,#40424,.F.) ;
#59069 = ORIENTED_EDGE('',*,*,#42414,.F.) ;
#59070 = ORIENTED_EDGE('',*,*,#40605,.F.) ;
#59071 = ORIENTED_EDGE('',*,*,#42415,.F.) ;
#59072 = ORIENTED_EDGE('',*,*,#40606,.F.) ;
#59073 = ORIENTED_EDGE('',*,*,#42416,.F.) ;
#59074 = ORIENTED_EDGE('',*,*,#39461,.F.) ;
#59075 = ORIENTED_EDGE('',*,*,#42408,.T.) ;
#59076 = ORIENTED_EDGE('',*,*,#42415,.T.) ;
#59077 = ORIENTED_EDGE('',*,*,#42417,.F.) ;
#59078 = ORIENTED_EDGE('',*,*,#42410,.T.) ;
#59079 = ORIENTED_EDGE('',*,*,#42409,.T.) ;
#59080 = ORIENTED_EDGE('',*,*,#42418,.F.) ;
#59081 = ORIENTED_EDGE('',*,*,#39633,.T.) ;
#59082 = ORIENTED_EDGE('',*,*,#42419,.F.) ;
#59083 = ORIENTED_EDGE('',*,*,#42412,.T.) ;
#59084 = ORIENTED_EDGE('',*,*,#42411,.T.) ;
#59085 = ORIENTED_EDGE('',*,*,#39657,.F.) ;
#59086 = ORIENTED_EDGE('',*,*,#42413,.T.) ;
#59087 = ORIENTED_EDGE('',*,*,#42420,.F.) ;
#59088 = ORIENTED_EDGE('',*,*,#42421,.F.) ;
#59089 = ORIENTED_EDGE('',*,*,#42416,.T.) ;
#59090 = ORIENTED_EDGE('',*,*,#42414,.T.) ;
#59091 = ORIENTED_EDGE('',*,*,#42422,.F.) ;
#59092 = ORIENTED_EDGE('',*,*,#39457,.T.) ;
#59093 = ORIENTED_EDGE('',*,*,#42417,.T.) ;
#59094 = ORIENTED_EDGE('',*,*,#39460,.F.) ;
#59095 = ORIENTED_EDGE('',*,*,#42423,.F.) ;
#59096 = ORIENTED_EDGE('',*,*,#39366,.F.) ;
#59097 = ORIENTED_EDGE('',*,*,#42418,.T.) ;
#59098 = ORIENTED_EDGE('',*,*,#39367,.F.) ;
#59099 = ORIENTED_EDGE('',*,*,#42424,.F.) ;
#59100 = ORIENTED_EDGE('',*,*,#39634,.F.) ;
#59101 = ORIENTED_EDGE('',*,*,#42419,.T.) ;
#59102 = ORIENTED_EDGE('',*,*,#39656,.T.) ;
#59103 = ORIENTED_EDGE('',*,*,#42425,.F.) ;
#59104 = ORIENTED_EDGE('',*,*,#42420,.T.) ;
#59105 = ORIENTED_EDGE('',*,*,#40423,.F.) ;
#59106 = ORIENTED_EDGE('',*,*,#42421,.T.) ;
#59107 = ORIENTED_EDGE('',*,*,#42426,.F.) ;
#59108 = ORIENTED_EDGE('',*,*,#42422,.T.) ;
#59109 = ORIENTED_EDGE('',*,*,#42424,.T.) ;
#59110 = ORIENTED_EDGE('',*,*,#42423,.T.) ;
#59111 = ORIENTED_EDGE('',*,*,#42427,.F.) ;
#59112 = ORIENTED_EDGE('',*,*,#39635,.T.) ;
#59113 = ORIENTED_EDGE('',*,*,#42425,.T.) ;
#59114 = ORIENTED_EDGE('',*,*,#39655,.F.) ;
#59115 = ORIENTED_EDGE('',*,*,#42428,.F.) ;
#59116 = ORIENTED_EDGE('',*,*,#39458,.F.) ;
#59117 = ORIENTED_EDGE('',*,*,#42426,.T.) ;
#59118 = ORIENTED_EDGE('',*,*,#42427,.T.) ;
#59119 = ORIENTED_EDGE('',*,*,#39459,.F.) ;
#59120 = ORIENTED_EDGE('',*,*,#42429,.F.) ;
#59121 = ORIENTED_EDGE('',*,*,#39636,.F.) ;
#59122 = ORIENTED_EDGE('',*,*,#42428,.T.) ;
#59123 = ORIENTED_EDGE('',*,*,#39558,.F.) ;
#59124 = ORIENTED_EDGE('',*,*,#42429,.T.) ;
#59125 = ORIENTED_EDGE('',*,*,#42430,.F.) ;
#59126 = ORIENTED_EDGE('',*,*,#40896,.F.) ;
#59127 = ORIENTED_EDGE('',*,*,#42431,.F.) ;
#59128 = ORIENTED_EDGE('',*,*,#40943,.F.) ;
#59129 = ORIENTED_EDGE('',*,*,#42431,.T.) ;
#59130 = ORIENTED_EDGE('',*,*,#40893,.F.) ;
#59131 = ORIENTED_EDGE('',*,*,#42432,.F.) ;
#59132 = ORIENTED_EDGE('',*,*,#40944,.F.) ;
#59133 = ORIENTED_EDGE('',*,*,#40899,.F.) ;
#59134 = ORIENTED_EDGE('',*,*,#42430,.T.) ;
#59135 = ORIENTED_EDGE('',*,*,#42433,.F.) ;
#59136 = ORIENTED_EDGE('',*,*,#42432,.T.) ;
#59137 = ORIENTED_EDGE('',*,*,#40890,.F.) ;
#59138 = ORIENTED_EDGE('',*,*,#42434,.F.) ;
#59139 = ORIENTED_EDGE('',*,*,#40945,.F.) ;
#59140 = ORIENTED_EDGE('',*,*,#42433,.T.) ;
#59141 = ORIENTED_EDGE('',*,*,#40942,.F.) ;
#59142 = ORIENTED_EDGE('',*,*,#42435,.F.) ;
#59143 = ORIENTED_EDGE('',*,*,#40902,.F.) ;
#59144 = ORIENTED_EDGE('',*,*,#42434,.T.) ;
#59145 = ORIENTED_EDGE('',*,*,#40887,.F.) ;
#59146 = ORIENTED_EDGE('',*,*,#42436,.F.) ;
#59147 = ORIENTED_EDGE('',*,*,#40946,.F.) ;
#59148 = ORIENTED_EDGE('',*,*,#40905,.F.) ;
#59149 = ORIENTED_EDGE('',*,*,#42435,.T.) ;
#59150 = ORIENTED_EDGE('',*,*,#42437,.F.) ;
#59151 = ORIENTED_EDGE('',*,*,#42436,.T.) ;
#59152 = ORIENTED_EDGE('',*,*,#40884,.F.) ;
#59153 = ORIENTED_EDGE('',*,*,#42438,.F.) ;
#59154 = ORIENTED_EDGE('',*,*,#40947,.F.) ;
#59155 = ORIENTED_EDGE('',*,*,#42437,.T.) ;
#59156 = ORIENTED_EDGE('',*,*,#40941,.F.) ;
#59157 = ORIENTED_EDGE('',*,*,#42439,.F.) ;
#59158 = ORIENTED_EDGE('',*,*,#40908,.F.) ;
#59159 = ORIENTED_EDGE('',*,*,#42438,.T.) ;
#59160 = ORIENTED_EDGE('',*,*,#40881,.F.) ;
#59161 = ORIENTED_EDGE('',*,*,#42440,.F.) ;
#59162 = ORIENTED_EDGE('',*,*,#40911,.F.) ;
#59163 = ORIENTED_EDGE('',*,*,#42439,.T.) ;
#59164 = ORIENTED_EDGE('',*,*,#42441,.F.) ;
#59165 = ORIENTED_EDGE('',*,*,#42440,.T.) ;
#59166 = ORIENTED_EDGE('',*,*,#40878,.F.) ;
#59167 = ORIENTED_EDGE('',*,*,#42442,.F.) ;
#59168 = ORIENTED_EDGE('',*,*,#40948,.F.) ;
#59169 = ORIENTED_EDGE('',*,*,#42441,.T.) ;
#59170 = ORIENTED_EDGE('',*,*,#40940,.F.) ;
#59171 = ORIENTED_EDGE('',*,*,#42443,.F.) ;
#59172 = ORIENTED_EDGE('',*,*,#40914,.F.) ;
#59173 = ORIENTED_EDGE('',*,*,#42442,.T.) ;
#59174 = ORIENTED_EDGE('',*,*,#39304,.F.) ;
#59175 = ORIENTED_EDGE('',*,*,#42444,.F.) ;
#59176 = ORIENTED_EDGE('',*,*,#40917,.F.) ;
#59177 = ORIENTED_EDGE('',*,*,#42443,.T.) ;
#59178 = ORIENTED_EDGE('',*,*,#42445,.F.) ;
#59179 = ORIENTED_EDGE('',*,*,#42444,.T.) ;
#59180 = ORIENTED_EDGE('',*,*,#40876,.F.) ;
#59181 = ORIENTED_EDGE('',*,*,#39131,.F.) ;
#59182 = ORIENTED_EDGE('',*,*,#40949,.F.) ;
#59183 = ORIENTED_EDGE('',*,*,#42445,.T.) ;
#59184 = ORIENTED_EDGE('',*,*,#40939,.F.) ;
#59185 = ORIENTED_EDGE('',*,*,#42446,.F.) ;
#59186 = ORIENTED_EDGE('',*,*,#40920,.F.) ;
#59187 = ORIENTED_EDGE('',*,*,#40923,.F.) ;
#59188 = ORIENTED_EDGE('',*,*,#42446,.T.) ;
#59189 = ORIENTED_EDGE('',*,*,#42447,.F.) ;
#59190 = ORIENTED_EDGE('',*,*,#39130,.T.) ;
#59191 = ORIENTED_EDGE('',*,*,#40871,.F.) ;
#59192 = ORIENTED_EDGE('',*,*,#42448,.F.) ;
#59193 = ORIENTED_EDGE('',*,*,#40950,.F.) ;
#59194 = ORIENTED_EDGE('',*,*,#42447,.T.) ;
#59195 = ORIENTED_EDGE('',*,*,#40938,.F.) ;
#59196 = ORIENTED_EDGE('',*,*,#42449,.F.) ;
#59197 = ORIENTED_EDGE('',*,*,#40926,.F.) ;
#59198 = ORIENTED_EDGE('',*,*,#42448,.T.) ;
#59199 = ORIENTED_EDGE('',*,*,#40868,.F.) ;
#59200 = ORIENTED_EDGE('',*,*,#42450,.F.) ;
#59201 = ORIENTED_EDGE('',*,*,#40929,.F.) ;
#59202 = ORIENTED_EDGE('',*,*,#42449,.T.) ;
#59203 = ORIENTED_EDGE('',*,*,#42451,.F.) ;
#59204 = ORIENTED_EDGE('',*,*,#42450,.T.) ;
#59205 = ORIENTED_EDGE('',*,*,#40865,.F.) ;
#59206 = ORIENTED_EDGE('',*,*,#42452,.F.) ;
#59207 = ORIENTED_EDGE('',*,*,#40951,.F.) ;
#59208 = ORIENTED_EDGE('',*,*,#42451,.T.) ;
#59209 = ORIENTED_EDGE('',*,*,#40937,.F.) ;
#59210 = ORIENTED_EDGE('',*,*,#42453,.F.) ;
#59211 = ORIENTED_EDGE('',*,*,#40932,.F.) ;
#59212 = ORIENTED_EDGE('',*,*,#42452,.T.) ;
#59213 = ORIENTED_EDGE('',*,*,#40862,.F.) ;
#59214 = ORIENTED_EDGE('',*,*,#42454,.F.) ;
#59215 = ORIENTED_EDGE('',*,*,#40934,.F.) ;
#59216 = ORIENTED_EDGE('',*,*,#42453,.T.) ;
#59217 = ORIENTED_EDGE('',*,*,#40936,.F.) ;
#59218 = ORIENTED_EDGE('',*,*,#42455,.F.) ;
#59219 = ORIENTED_EDGE('',*,*,#40856,.F.) ;
#59220 = ORIENTED_EDGE('',*,*,#42454,.T.) ;
#59221 = ORIENTED_EDGE('',*,*,#40859,.F.) ;
#59222 = ORIENTED_EDGE('',*,*,#42455,.T.) ;
#59223 = ORIENTED_EDGE('',*,*,#40935,.F.) ;
#59224 = ORIENTED_EDGE('',*,*,#42456,.F.) ;
#59225 = ORIENTED_EDGE('',*,*,#40635,.F.) ;
#59226 = ORIENTED_EDGE('',*,*,#42457,.F.) ;
#59227 = ORIENTED_EDGE('',*,*,#40419,.F.) ;
#59228 = ORIENTED_EDGE('',*,*,#42458,.F.) ;
#59229 = ORIENTED_EDGE('',*,*,#40636,.F.) ;
#59230 = ORIENTED_EDGE('',*,*,#42459,.F.) ;
#59231 = ORIENTED_EDGE('',*,*,#40630,.F.) ;
#59232 = ORIENTED_EDGE('',*,*,#42460,.F.) ;
#59233 = ORIENTED_EDGE('',*,*,#42458,.T.) ;
#59234 = ORIENTED_EDGE('',*,*,#42461,.F.) ;
#59235 = ORIENTED_EDGE('',*,*,#42462,.F.) ;
#59236 = ORIENTED_EDGE('',*,*,#42457,.T.) ;
#59237 = ORIENTED_EDGE('',*,*,#42463,.F.) ;
#59238 = ORIENTED_EDGE('',*,*,#42456,.T.) ;
#59239 = ORIENTED_EDGE('',*,*,#40418,.T.) ;
#59240 = ORIENTED_EDGE('',*,*,#42464,.F.) ;
#59241 = ORIENTED_EDGE('',*,*,#42459,.T.) ;
#59242 = ORIENTED_EDGE('',*,*,#42461,.T.) ;
#59243 = ORIENTED_EDGE('',*,*,#40633,.F.) ;
#59244 = ORIENTED_EDGE('',*,*,#42465,.F.) ;
#59245 = ORIENTED_EDGE('',*,*,#39115,.T.) ;
#59246 = ORIENTED_EDGE('',*,*,#42466,.T.) ;
#59247 = ORIENTED_EDGE('',*,*,#42467,.F.) ;
#59248 = ORIENTED_EDGE('',*,*,#42460,.T.) ;
#59249 = ORIENTED_EDGE('',*,*,#42468,.F.) ;
#59250 = ORIENTED_EDGE('',*,*,#42469,.T.) ;
#59251 = ORIENTED_EDGE('',*,*,#42470,.F.) ;
#59252 = ORIENTED_EDGE('',*,*,#39349,.F.) ;
#59253 = ORIENTED_EDGE('',*,*,#42471,.F.) ;
#59254 = ORIENTED_EDGE('',*,*,#40637,.F.) ;
#59255 = ORIENTED_EDGE('',*,*,#42463,.T.) ;
#59256 = ORIENTED_EDGE('',*,*,#40634,.F.) ;
#59257 = ORIENTED_EDGE('',*,*,#42472,.F.) ;
#59258 = ORIENTED_EDGE('',*,*,#40640,.F.) ;
#59259 = ORIENTED_EDGE('',*,*,#42462,.T.) ;
#59260 = ORIENTED_EDGE('',*,*,#40639,.F.) ;
#59261 = ORIENTED_EDGE('',*,*,#42473,.F.) ;
#59262 = ORIENTED_EDGE('',*,*,#40410,.F.) ;
#59263 = ORIENTED_EDGE('',*,*,#42464,.T.) ;
#59264 = ORIENTED_EDGE('',*,*,#40417,.F.) ;
#59265 = ORIENTED_EDGE('',*,*,#42474,.F.) ;
#59266 = ORIENTED_EDGE('',*,*,#40631,.F.) ;
#59267 = ORIENTED_EDGE('',*,*,#42475,.F.) ;
#59268 = ORIENTED_EDGE('',*,*,#40632,.F.) ;
#59269 = ORIENTED_EDGE('',*,*,#42476,.F.) ;
#59270 = ORIENTED_EDGE('',*,*,#40627,.F.) ;
#59271 = ORIENTED_EDGE('',*,*,#42465,.T.) ;
#59272 = ORIENTED_EDGE('',*,*,#42475,.T.) ;
#59273 = ORIENTED_EDGE('',*,*,#39116,.F.) ;
#59274 = ORIENTED_EDGE('',*,*,#42471,.T.) ;
#59275 = ORIENTED_EDGE('',*,*,#39359,.T.) ;
#59276 = ORIENTED_EDGE('',*,*,#42477,.F.) ;
#59277 = ORIENTED_EDGE('',*,*,#42472,.T.) ;
#59278 = ORIENTED_EDGE('',*,*,#42478,.F.) ;
#59279 = ORIENTED_EDGE('',*,*,#42473,.T.) ;
#59280 = ORIENTED_EDGE('',*,*,#42479,.F.) ;
#59281 = ORIENTED_EDGE('',*,*,#39452,.T.) ;
#59282 = ORIENTED_EDGE('',*,*,#42474,.T.) ;
#59283 = ORIENTED_EDGE('',*,*,#40416,.T.) ;
#59284 = ORIENTED_EDGE('',*,*,#42480,.F.) ;
#59285 = ORIENTED_EDGE('',*,*,#42476,.T.) ;
#59286 = ORIENTED_EDGE('',*,*,#42477,.T.) ;
#59287 = ORIENTED_EDGE('',*,*,#39358,.F.) ;
#59288 = ORIENTED_EDGE('',*,*,#42481,.F.) ;
#59289 = ORIENTED_EDGE('',*,*,#40641,.F.) ;
#59290 = ORIENTED_EDGE('',*,*,#42479,.T.) ;
#59291 = ORIENTED_EDGE('',*,*,#40638,.F.) ;
#59292 = ORIENTED_EDGE('',*,*,#42482,.F.) ;
#59293 = ORIENTED_EDGE('',*,*,#39453,.F.) ;
#59294 = ORIENTED_EDGE('',*,*,#40411,.F.) ;
#59295 = ORIENTED_EDGE('',*,*,#42478,.T.) ;
#59296 = ORIENTED_EDGE('',*,*,#42483,.F.) ;
#59297 = ORIENTED_EDGE('',*,*,#42484,.F.) ;
#59298 = ORIENTED_EDGE('',*,*,#42480,.T.) ;
#59299 = ORIENTED_EDGE('',*,*,#40415,.F.) ;
#59300 = ORIENTED_EDGE('',*,*,#42485,.F.) ;
#59301 = ORIENTED_EDGE('',*,*,#40628,.F.) ;
#59302 = ORIENTED_EDGE('',*,*,#42486,.F.) ;
#59303 = ORIENTED_EDGE('',*,*,#40629,.F.) ;
#59304 = ORIENTED_EDGE('',*,*,#42487,.F.) ;
#59305 = ORIENTED_EDGE('',*,*,#40623,.F.) ;
#59306 = ORIENTED_EDGE('',*,*,#39118,.T.) ;
#59307 = ORIENTED_EDGE('',*,*,#42486,.T.) ;
#59308 = ORIENTED_EDGE('',*,*,#42488,.F.) ;
#59309 = ORIENTED_EDGE('',*,*,#39353,.T.) ;
#59310 = ORIENTED_EDGE('',*,*,#42482,.T.) ;
#59311 = ORIENTED_EDGE('',*,*,#42481,.T.) ;
#59312 = ORIENTED_EDGE('',*,*,#42489,.F.) ;
#59313 = ORIENTED_EDGE('',*,*,#42490,.F.) ;
#59314 = ORIENTED_EDGE('',*,*,#39556,.F.) ;
#59315 = ORIENTED_EDGE('',*,*,#42491,.F.) ;
#59316 = ORIENTED_EDGE('',*,*,#42492,.F.) ;
#59317 = ORIENTED_EDGE('',*,*,#42483,.T.) ;
#59318 = ORIENTED_EDGE('',*,*,#39456,.F.) ;
#59319 = ORIENTED_EDGE('',*,*,#42491,.T.) ;
#59320 = ORIENTED_EDGE('',*,*,#39654,.F.) ;
#59321 = ORIENTED_EDGE('',*,*,#42484,.T.) ;
#59322 = ORIENTED_EDGE('',*,*,#42493,.F.) ;
#59323 = ORIENTED_EDGE('',*,*,#42494,.F.) ;
#59324 = ORIENTED_EDGE('',*,*,#42487,.T.) ;
#59325 = ORIENTED_EDGE('',*,*,#42485,.T.) ;
#59326 = ORIENTED_EDGE('',*,*,#42495,.F.) ;
#59327 = ORIENTED_EDGE('',*,*,#42488,.T.) ;
#59328 = ORIENTED_EDGE('',*,*,#40626,.F.) ;
#59329 = ORIENTED_EDGE('',*,*,#42496,.F.) ;
#59330 = ORIENTED_EDGE('',*,*,#39354,.F.) ;
#59331 = ORIENTED_EDGE('',*,*,#42489,.T.) ;
#59332 = ORIENTED_EDGE('',*,*,#39357,.F.) ;
#59333 = ORIENTED_EDGE('',*,*,#42497,.F.) ;
#59334 = ORIENTED_EDGE('',*,*,#39454,.F.) ;
#59335 = ORIENTED_EDGE('',*,*,#42490,.T.) ;
#59336 = ORIENTED_EDGE('',*,*,#39455,.F.) ;
#59337 = ORIENTED_EDGE('',*,*,#42498,.F.) ;
#59338 = ORIENTED_EDGE('',*,*,#39637,.F.) ;
#59339 = ORIENTED_EDGE('',*,*,#42492,.T.) ;
#59340 = ORIENTED_EDGE('',*,*,#39653,.T.) ;
#59341 = ORIENTED_EDGE('',*,*,#42499,.F.) ;
#59342 = ORIENTED_EDGE('',*,*,#42493,.T.) ;
#59343 = ORIENTED_EDGE('',*,*,#40412,.F.) ;
#59344 = ORIENTED_EDGE('',*,*,#42494,.T.) ;
#59345 = ORIENTED_EDGE('',*,*,#42500,.F.) ;
#59346 = ORIENTED_EDGE('',*,*,#42501,.F.) ;
#59347 = ORIENTED_EDGE('',*,*,#42495,.T.) ;
#59348 = ORIENTED_EDGE('',*,*,#40414,.F.) ;
#59349 = ORIENTED_EDGE('',*,*,#42502,.F.) ;
#59350 = ORIENTED_EDGE('',*,*,#40624,.F.) ;
#59351 = ORIENTED_EDGE('',*,*,#42503,.F.) ;
#59352 = ORIENTED_EDGE('',*,*,#40625,.F.) ;
#59353 = ORIENTED_EDGE('',*,*,#42504,.F.) ;
#59354 = ORIENTED_EDGE('',*,*,#39451,.F.) ;
#59355 = ORIENTED_EDGE('',*,*,#42496,.T.) ;
#59356 = ORIENTED_EDGE('',*,*,#42503,.T.) ;
#59357 = ORIENTED_EDGE('',*,*,#42505,.F.) ;
#59358 = ORIENTED_EDGE('',*,*,#42498,.T.) ;
#59359 = ORIENTED_EDGE('',*,*,#42497,.T.) ;
#59360 = ORIENTED_EDGE('',*,*,#42506,.F.) ;
#59361 = ORIENTED_EDGE('',*,*,#39638,.T.) ;
#59362 = ORIENTED_EDGE('',*,*,#42507,.F.) ;
#59363 = ORIENTED_EDGE('',*,*,#42500,.T.) ;
#59364 = ORIENTED_EDGE('',*,*,#42499,.T.) ;
#59365 = ORIENTED_EDGE('',*,*,#39652,.F.) ;
#59366 = ORIENTED_EDGE('',*,*,#42501,.T.) ;
#59367 = ORIENTED_EDGE('',*,*,#42508,.F.) ;
#59368 = ORIENTED_EDGE('',*,*,#42509,.F.) ;
#59369 = ORIENTED_EDGE('',*,*,#42504,.T.) ;
#59370 = ORIENTED_EDGE('',*,*,#42502,.T.) ;
#59371 = ORIENTED_EDGE('',*,*,#42510,.F.) ;
#59372 = ORIENTED_EDGE('',*,*,#39447,.T.) ;
#59373 = ORIENTED_EDGE('',*,*,#42505,.T.) ;
#59374 = ORIENTED_EDGE('',*,*,#39450,.F.) ;
#59375 = ORIENTED_EDGE('',*,*,#42511,.F.) ;
#59376 = ORIENTED_EDGE('',*,*,#39355,.F.) ;
#59377 = ORIENTED_EDGE('',*,*,#42506,.T.) ;
#59378 = ORIENTED_EDGE('',*,*,#39356,.F.) ;
#59379 = ORIENTED_EDGE('',*,*,#42512,.F.) ;
#59380 = ORIENTED_EDGE('',*,*,#39639,.F.) ;
#59381 = ORIENTED_EDGE('',*,*,#42507,.T.) ;
#59382 = ORIENTED_EDGE('',*,*,#39651,.T.) ;
#59383 = ORIENTED_EDGE('',*,*,#42513,.F.) ;
#59384 = ORIENTED_EDGE('',*,*,#42508,.T.) ;
#59385 = ORIENTED_EDGE('',*,*,#40413,.F.) ;
#59386 = ORIENTED_EDGE('',*,*,#42509,.T.) ;
#59387 = ORIENTED_EDGE('',*,*,#42514,.F.) ;
#59388 = ORIENTED_EDGE('',*,*,#42510,.T.) ;
#59389 = ORIENTED_EDGE('',*,*,#42512,.T.) ;
#59390 = ORIENTED_EDGE('',*,*,#42511,.T.) ;
#59391 = ORIENTED_EDGE('',*,*,#42515,.F.) ;
#59392 = ORIENTED_EDGE('',*,*,#39640,.T.) ;
#59393 = ORIENTED_EDGE('',*,*,#42513,.T.) ;
#59394 = ORIENTED_EDGE('',*,*,#39650,.F.) ;
#59395 = ORIENTED_EDGE('',*,*,#42516,.F.) ;
#59396 = ORIENTED_EDGE('',*,*,#39448,.F.) ;
#59397 = ORIENTED_EDGE('',*,*,#42514,.T.) ;
#59398 = ORIENTED_EDGE('',*,*,#42515,.T.) ;
#59399 = ORIENTED_EDGE('',*,*,#39449,.F.) ;
#59400 = ORIENTED_EDGE('',*,*,#42517,.F.) ;
#59401 = ORIENTED_EDGE('',*,*,#39641,.F.) ;
#59402 = ORIENTED_EDGE('',*,*,#42516,.T.) ;
#59403 = ORIENTED_EDGE('',*,*,#39562,.F.) ;
#59404 = ORIENTED_EDGE('',*,*,#42517,.T.) ;
#59405 = ORIENTED_EDGE('',*,*,#42518,.F.) ;
#59406 = ORIENTED_EDGE('',*,*,#40799,.F.) ;
#59407 = ORIENTED_EDGE('',*,*,#42519,.F.) ;
#59408 = ORIENTED_EDGE('',*,*,#40846,.F.) ;
#59409 = ORIENTED_EDGE('',*,*,#42519,.T.) ;
#59410 = ORIENTED_EDGE('',*,*,#40796,.F.) ;
#59411 = ORIENTED_EDGE('',*,*,#42520,.F.) ;
#59412 = ORIENTED_EDGE('',*,*,#40847,.F.) ;
#59413 = ORIENTED_EDGE('',*,*,#40802,.F.) ;
#59414 = ORIENTED_EDGE('',*,*,#42518,.T.) ;
#59415 = ORIENTED_EDGE('',*,*,#42521,.F.) ;
#59416 = ORIENTED_EDGE('',*,*,#42520,.T.) ;
#59417 = ORIENTED_EDGE('',*,*,#40793,.F.) ;
#59418 = ORIENTED_EDGE('',*,*,#42522,.F.) ;
#59419 = ORIENTED_EDGE('',*,*,#40848,.F.) ;
#59420 = ORIENTED_EDGE('',*,*,#42521,.T.) ;
#59421 = ORIENTED_EDGE('',*,*,#40845,.F.) ;
#59422 = ORIENTED_EDGE('',*,*,#42523,.F.) ;
#59423 = ORIENTED_EDGE('',*,*,#40805,.F.) ;
#59424 = ORIENTED_EDGE('',*,*,#42522,.T.) ;
#59425 = ORIENTED_EDGE('',*,*,#40790,.F.) ;
#59426 = ORIENTED_EDGE('',*,*,#42524,.F.) ;
#59427 = ORIENTED_EDGE('',*,*,#40849,.F.) ;
#59428 = ORIENTED_EDGE('',*,*,#40808,.F.) ;
#59429 = ORIENTED_EDGE('',*,*,#42523,.T.) ;
#59430 = ORIENTED_EDGE('',*,*,#42525,.F.) ;
#59431 = ORIENTED_EDGE('',*,*,#42524,.T.) ;
#59432 = ORIENTED_EDGE('',*,*,#40787,.F.) ;
#59433 = ORIENTED_EDGE('',*,*,#42526,.F.) ;
#59434 = ORIENTED_EDGE('',*,*,#40850,.F.) ;
#59435 = ORIENTED_EDGE('',*,*,#42525,.T.) ;
#59436 = ORIENTED_EDGE('',*,*,#40844,.F.) ;
#59437 = ORIENTED_EDGE('',*,*,#42527,.F.) ;
#59438 = ORIENTED_EDGE('',*,*,#40811,.F.) ;
#59439 = ORIENTED_EDGE('',*,*,#42526,.T.) ;
#59440 = ORIENTED_EDGE('',*,*,#40784,.F.) ;
#59441 = ORIENTED_EDGE('',*,*,#42528,.F.) ;
#59442 = ORIENTED_EDGE('',*,*,#40814,.F.) ;
#59443 = ORIENTED_EDGE('',*,*,#42527,.T.) ;
#59444 = ORIENTED_EDGE('',*,*,#42529,.F.) ;
#59445 = ORIENTED_EDGE('',*,*,#42528,.T.) ;
#59446 = ORIENTED_EDGE('',*,*,#40781,.F.) ;
#59447 = ORIENTED_EDGE('',*,*,#42530,.F.) ;
#59448 = ORIENTED_EDGE('',*,*,#40851,.F.) ;
#59449 = ORIENTED_EDGE('',*,*,#42529,.T.) ;
#59450 = ORIENTED_EDGE('',*,*,#40843,.F.) ;
#59451 = ORIENTED_EDGE('',*,*,#42531,.F.) ;
#59452 = ORIENTED_EDGE('',*,*,#40817,.F.) ;
#59453 = ORIENTED_EDGE('',*,*,#42530,.T.) ;
#59454 = ORIENTED_EDGE('',*,*,#39307,.F.) ;
#59455 = ORIENTED_EDGE('',*,*,#42532,.F.) ;
#59456 = ORIENTED_EDGE('',*,*,#40820,.F.) ;
#59457 = ORIENTED_EDGE('',*,*,#42531,.T.) ;
#59458 = ORIENTED_EDGE('',*,*,#42533,.F.) ;
#59459 = ORIENTED_EDGE('',*,*,#42532,.T.) ;
#59460 = ORIENTED_EDGE('',*,*,#40779,.F.) ;
#59461 = ORIENTED_EDGE('',*,*,#39114,.F.) ;
#59462 = ORIENTED_EDGE('',*,*,#40852,.F.) ;
#59463 = ORIENTED_EDGE('',*,*,#42533,.T.) ;
#59464 = ORIENTED_EDGE('',*,*,#40842,.F.) ;
#59465 = ORIENTED_EDGE('',*,*,#42534,.F.) ;
#59466 = ORIENTED_EDGE('',*,*,#40823,.F.) ;
#59467 = ORIENTED_EDGE('',*,*,#40826,.F.) ;
#59468 = ORIENTED_EDGE('',*,*,#42534,.T.) ;
#59469 = ORIENTED_EDGE('',*,*,#42535,.F.) ;
#59470 = ORIENTED_EDGE('',*,*,#39113,.T.) ;
#59471 = ORIENTED_EDGE('',*,*,#40774,.F.) ;
#59472 = ORIENTED_EDGE('',*,*,#42536,.F.) ;
#59473 = ORIENTED_EDGE('',*,*,#40853,.F.) ;
#59474 = ORIENTED_EDGE('',*,*,#42535,.T.) ;
#59475 = ORIENTED_EDGE('',*,*,#40841,.F.) ;
#59476 = ORIENTED_EDGE('',*,*,#42537,.F.) ;
#59477 = ORIENTED_EDGE('',*,*,#40829,.F.) ;
#59478 = ORIENTED_EDGE('',*,*,#42536,.T.) ;
#59479 = ORIENTED_EDGE('',*,*,#40771,.F.) ;
#59480 = ORIENTED_EDGE('',*,*,#42538,.F.) ;
#59481 = ORIENTED_EDGE('',*,*,#40832,.F.) ;
#59482 = ORIENTED_EDGE('',*,*,#42537,.T.) ;
#59483 = ORIENTED_EDGE('',*,*,#42539,.F.) ;
#59484 = ORIENTED_EDGE('',*,*,#42538,.T.) ;
#59485 = ORIENTED_EDGE('',*,*,#40768,.F.) ;
#59486 = ORIENTED_EDGE('',*,*,#42540,.F.) ;
#59487 = ORIENTED_EDGE('',*,*,#40854,.F.) ;
#59488 = ORIENTED_EDGE('',*,*,#42539,.T.) ;
#59489 = ORIENTED_EDGE('',*,*,#40840,.F.) ;
#59490 = ORIENTED_EDGE('',*,*,#42541,.F.) ;
#59491 = ORIENTED_EDGE('',*,*,#40835,.F.) ;
#59492 = ORIENTED_EDGE('',*,*,#42540,.T.) ;
#59493 = ORIENTED_EDGE('',*,*,#40765,.F.) ;
#59494 = ORIENTED_EDGE('',*,*,#42542,.F.) ;
#59495 = ORIENTED_EDGE('',*,*,#40837,.F.) ;
#59496 = ORIENTED_EDGE('',*,*,#42541,.T.) ;
#59497 = ORIENTED_EDGE('',*,*,#40839,.F.) ;
#59498 = ORIENTED_EDGE('',*,*,#42543,.F.) ;
#59499 = ORIENTED_EDGE('',*,*,#40759,.F.) ;
#59500 = ORIENTED_EDGE('',*,*,#42542,.T.) ;
#59501 = ORIENTED_EDGE('',*,*,#40762,.F.) ;
#59502 = ORIENTED_EDGE('',*,*,#42543,.T.) ;
#59503 = ORIENTED_EDGE('',*,*,#40838,.F.) ;
#59504 = ORIENTED_EDGE('',*,*,#42544,.F.) ;
#59505 = ORIENTED_EDGE('',*,*,#40654,.F.) ;
#59506 = ORIENTED_EDGE('',*,*,#42545,.F.) ;
#59507 = ORIENTED_EDGE('',*,*,#40409,.F.) ;
#59508 = ORIENTED_EDGE('',*,*,#42546,.F.) ;
#59509 = ORIENTED_EDGE('',*,*,#40655,.F.) ;
#59510 = ORIENTED_EDGE('',*,*,#42547,.F.) ;
#59511 = ORIENTED_EDGE('',*,*,#40649,.F.) ;
#59512 = ORIENTED_EDGE('',*,*,#42548,.F.) ;
#59513 = ORIENTED_EDGE('',*,*,#42546,.T.) ;
#59514 = ORIENTED_EDGE('',*,*,#42549,.F.) ;
#59515 = ORIENTED_EDGE('',*,*,#42550,.F.) ;
#59516 = ORIENTED_EDGE('',*,*,#42545,.T.) ;
#59517 = ORIENTED_EDGE('',*,*,#42551,.F.) ;
#59518 = ORIENTED_EDGE('',*,*,#42544,.T.) ;
#59519 = ORIENTED_EDGE('',*,*,#40408,.T.) ;
#59520 = ORIENTED_EDGE('',*,*,#42552,.F.) ;
#59521 = ORIENTED_EDGE('',*,*,#42547,.T.) ;
#59522 = ORIENTED_EDGE('',*,*,#42549,.T.) ;
#59523 = ORIENTED_EDGE('',*,*,#40652,.F.) ;
#59524 = ORIENTED_EDGE('',*,*,#42553,.F.) ;
#59525 = ORIENTED_EDGE('',*,*,#39098,.T.) ;
#59526 = ORIENTED_EDGE('',*,*,#42554,.T.) ;
#59527 = ORIENTED_EDGE('',*,*,#42555,.F.) ;
#59528 = ORIENTED_EDGE('',*,*,#42548,.T.) ;
#59529 = ORIENTED_EDGE('',*,*,#42556,.F.) ;
#59530 = ORIENTED_EDGE('',*,*,#42557,.T.) ;
#59531 = ORIENTED_EDGE('',*,*,#42558,.F.) ;
#59532 = ORIENTED_EDGE('',*,*,#39338,.F.) ;
#59533 = ORIENTED_EDGE('',*,*,#42559,.F.) ;
#59534 = ORIENTED_EDGE('',*,*,#40656,.F.) ;
#59535 = ORIENTED_EDGE('',*,*,#42551,.T.) ;
#59536 = ORIENTED_EDGE('',*,*,#40653,.F.) ;
#59537 = ORIENTED_EDGE('',*,*,#42560,.F.) ;
#59538 = ORIENTED_EDGE('',*,*,#40659,.F.) ;
#59539 = ORIENTED_EDGE('',*,*,#42550,.T.) ;
#59540 = ORIENTED_EDGE('',*,*,#40658,.F.) ;
#59541 = ORIENTED_EDGE('',*,*,#42561,.F.) ;
#59542 = ORIENTED_EDGE('',*,*,#40400,.F.) ;
#59543 = ORIENTED_EDGE('',*,*,#42552,.T.) ;
#59544 = ORIENTED_EDGE('',*,*,#40407,.F.) ;
#59545 = ORIENTED_EDGE('',*,*,#42562,.F.) ;
#59546 = ORIENTED_EDGE('',*,*,#40650,.F.) ;
#59547 = ORIENTED_EDGE('',*,*,#42563,.F.) ;
#59548 = ORIENTED_EDGE('',*,*,#40651,.F.) ;
#59549 = ORIENTED_EDGE('',*,*,#42564,.F.) ;
#59550 = ORIENTED_EDGE('',*,*,#40646,.F.) ;
#59551 = ORIENTED_EDGE('',*,*,#42553,.T.) ;
#59552 = ORIENTED_EDGE('',*,*,#42563,.T.) ;
#59553 = ORIENTED_EDGE('',*,*,#39099,.F.) ;
#59554 = ORIENTED_EDGE('',*,*,#42559,.T.) ;
#59555 = ORIENTED_EDGE('',*,*,#39348,.T.) ;
#59556 = ORIENTED_EDGE('',*,*,#42565,.F.) ;
#59557 = ORIENTED_EDGE('',*,*,#42560,.T.) ;
#59558 = ORIENTED_EDGE('',*,*,#42566,.F.) ;
#59559 = ORIENTED_EDGE('',*,*,#42561,.T.) ;
#59560 = ORIENTED_EDGE('',*,*,#42567,.F.) ;
#59561 = ORIENTED_EDGE('',*,*,#39442,.T.) ;
#59562 = ORIENTED_EDGE('',*,*,#42562,.T.) ;
#59563 = ORIENTED_EDGE('',*,*,#40406,.T.) ;
#59564 = ORIENTED_EDGE('',*,*,#42568,.F.) ;
#59565 = ORIENTED_EDGE('',*,*,#42564,.T.) ;
#59566 = ORIENTED_EDGE('',*,*,#42565,.T.) ;
#59567 = ORIENTED_EDGE('',*,*,#39347,.F.) ;
#59568 = ORIENTED_EDGE('',*,*,#42569,.F.) ;
#59569 = ORIENTED_EDGE('',*,*,#40660,.F.) ;
#59570 = ORIENTED_EDGE('',*,*,#42567,.T.) ;
#59571 = ORIENTED_EDGE('',*,*,#40657,.F.) ;
#59572 = ORIENTED_EDGE('',*,*,#42570,.F.) ;
#59573 = ORIENTED_EDGE('',*,*,#39443,.F.) ;
#59574 = ORIENTED_EDGE('',*,*,#40401,.F.) ;
#59575 = ORIENTED_EDGE('',*,*,#42566,.T.) ;
#59576 = ORIENTED_EDGE('',*,*,#42571,.F.) ;
#59577 = ORIENTED_EDGE('',*,*,#42572,.F.) ;
#59578 = ORIENTED_EDGE('',*,*,#42568,.T.) ;
#59579 = ORIENTED_EDGE('',*,*,#40405,.F.) ;
#59580 = ORIENTED_EDGE('',*,*,#42573,.F.) ;
#59581 = ORIENTED_EDGE('',*,*,#40647,.F.) ;
#59582 = ORIENTED_EDGE('',*,*,#42574,.F.) ;
#59583 = ORIENTED_EDGE('',*,*,#40648,.F.) ;
#59584 = ORIENTED_EDGE('',*,*,#42575,.F.) ;
#59585 = ORIENTED_EDGE('',*,*,#40642,.F.) ;
#59586 = ORIENTED_EDGE('',*,*,#39101,.T.) ;
#59587 = ORIENTED_EDGE('',*,*,#42574,.T.) ;
#59588 = ORIENTED_EDGE('',*,*,#42576,.F.) ;
#59589 = ORIENTED_EDGE('',*,*,#39342,.T.) ;
#59590 = ORIENTED_EDGE('',*,*,#42570,.T.) ;
#59591 = ORIENTED_EDGE('',*,*,#42569,.T.) ;
#59592 = ORIENTED_EDGE('',*,*,#42577,.F.) ;
#59593 = ORIENTED_EDGE('',*,*,#42578,.F.) ;
#59594 = ORIENTED_EDGE('',*,*,#39560,.F.) ;
#59595 = ORIENTED_EDGE('',*,*,#42579,.F.) ;
#59596 = ORIENTED_EDGE('',*,*,#42580,.F.) ;
#59597 = ORIENTED_EDGE('',*,*,#42571,.T.) ;
#59598 = ORIENTED_EDGE('',*,*,#39446,.F.) ;
#59599 = ORIENTED_EDGE('',*,*,#42579,.T.) ;
#59600 = ORIENTED_EDGE('',*,*,#39649,.F.) ;
#59601 = ORIENTED_EDGE('',*,*,#42572,.T.) ;
#59602 = ORIENTED_EDGE('',*,*,#42581,.F.) ;
#59603 = ORIENTED_EDGE('',*,*,#42582,.F.) ;
#59604 = ORIENTED_EDGE('',*,*,#42575,.T.) ;
#59605 = ORIENTED_EDGE('',*,*,#42573,.T.) ;
#59606 = ORIENTED_EDGE('',*,*,#42583,.F.) ;
#59607 = ORIENTED_EDGE('',*,*,#42576,.T.) ;
#59608 = ORIENTED_EDGE('',*,*,#40645,.F.) ;
#59609 = ORIENTED_EDGE('',*,*,#42584,.F.) ;
#59610 = ORIENTED_EDGE('',*,*,#39343,.F.) ;
#59611 = ORIENTED_EDGE('',*,*,#42577,.T.) ;
#59612 = ORIENTED_EDGE('',*,*,#39346,.F.) ;
#59613 = ORIENTED_EDGE('',*,*,#42585,.F.) ;
#59614 = ORIENTED_EDGE('',*,*,#39444,.F.) ;
#59615 = ORIENTED_EDGE('',*,*,#42578,.T.) ;
#59616 = ORIENTED_EDGE('',*,*,#39445,.F.) ;
#59617 = ORIENTED_EDGE('',*,*,#42586,.F.) ;
#59618 = ORIENTED_EDGE('',*,*,#39642,.F.) ;
#59619 = ORIENTED_EDGE('',*,*,#42580,.T.) ;
#59620 = ORIENTED_EDGE('',*,*,#39648,.T.) ;
#59621 = ORIENTED_EDGE('',*,*,#42587,.F.) ;
#59622 = ORIENTED_EDGE('',*,*,#42581,.T.) ;
#59623 = ORIENTED_EDGE('',*,*,#40402,.F.) ;
#59624 = ORIENTED_EDGE('',*,*,#42582,.T.) ;
#59625 = ORIENTED_EDGE('',*,*,#42588,.F.) ;
#59626 = ORIENTED_EDGE('',*,*,#42589,.F.) ;
#59627 = ORIENTED_EDGE('',*,*,#42583,.T.) ;
#59628 = ORIENTED_EDGE('',*,*,#40404,.F.) ;
#59629 = ORIENTED_EDGE('',*,*,#42590,.F.) ;
#59630 = ORIENTED_EDGE('',*,*,#40643,.F.) ;
#59631 = ORIENTED_EDGE('',*,*,#42591,.F.) ;
#59632 = ORIENTED_EDGE('',*,*,#40644,.F.) ;
#59633 = ORIENTED_EDGE('',*,*,#42592,.F.) ;
#59634 = ORIENTED_EDGE('',*,*,#39441,.F.) ;
#59635 = ORIENTED_EDGE('',*,*,#42584,.T.) ;
#59636 = ORIENTED_EDGE('',*,*,#42591,.T.) ;
#59637 = ORIENTED_EDGE('',*,*,#42593,.F.) ;
#59638 = ORIENTED_EDGE('',*,*,#42586,.T.) ;
#59639 = ORIENTED_EDGE('',*,*,#42585,.T.) ;
#59640 = ORIENTED_EDGE('',*,*,#42594,.F.) ;
#59641 = ORIENTED_EDGE('',*,*,#39643,.T.) ;
#59642 = ORIENTED_EDGE('',*,*,#42595,.F.) ;
#59643 = ORIENTED_EDGE('',*,*,#42588,.T.) ;
#59644 = ORIENTED_EDGE('',*,*,#42587,.T.) ;
#59645 = ORIENTED_EDGE('',*,*,#39700,.F.) ;
#59646 = ORIENTED_EDGE('',*,*,#42589,.T.) ;
#59647 = ORIENTED_EDGE('',*,*,#42596,.F.) ;
#59648 = ORIENTED_EDGE('',*,*,#42597,.F.) ;
#59649 = ORIENTED_EDGE('',*,*,#42592,.T.) ;
#59650 = ORIENTED_EDGE('',*,*,#42590,.T.) ;
#59651 = ORIENTED_EDGE('',*,*,#42598,.F.) ;
#59652 = ORIENTED_EDGE('',*,*,#39437,.T.) ;
#59653 = ORIENTED_EDGE('',*,*,#42593,.T.) ;
#59654 = ORIENTED_EDGE('',*,*,#39440,.F.) ;
#59655 = ORIENTED_EDGE('',*,*,#42599,.F.) ;
#59656 = ORIENTED_EDGE('',*,*,#39344,.F.) ;
#59657 = ORIENTED_EDGE('',*,*,#42594,.T.) ;
#59658 = ORIENTED_EDGE('',*,*,#39345,.F.) ;
#59659 = ORIENTED_EDGE('',*,*,#42600,.F.) ;
#59660 = ORIENTED_EDGE('',*,*,#39644,.F.) ;
#59661 = ORIENTED_EDGE('',*,*,#42595,.T.) ;
#59662 = ORIENTED_EDGE('',*,*,#39699,.T.) ;
#59663 = ORIENTED_EDGE('',*,*,#42601,.F.) ;
#59664 = ORIENTED_EDGE('',*,*,#42596,.T.) ;
#59665 = ORIENTED_EDGE('',*,*,#40403,.F.) ;
#59666 = ORIENTED_EDGE('',*,*,#42597,.T.) ;
#59667 = ORIENTED_EDGE('',*,*,#42602,.F.) ;
#59668 = ORIENTED_EDGE('',*,*,#42598,.T.) ;
#59669 = ORIENTED_EDGE('',*,*,#42600,.T.) ;
#59670 = ORIENTED_EDGE('',*,*,#42599,.T.) ;
#59671 = ORIENTED_EDGE('',*,*,#42603,.F.) ;
#59672 = ORIENTED_EDGE('',*,*,#39592,.T.) ;
#59673 = ORIENTED_EDGE('',*,*,#42601,.T.) ;
#59674 = ORIENTED_EDGE('',*,*,#39698,.F.) ;
#59675 = ORIENTED_EDGE('',*,*,#42604,.F.) ;
#59676 = ORIENTED_EDGE('',*,*,#39438,.F.) ;
#59677 = ORIENTED_EDGE('',*,*,#42602,.T.) ;
#59678 = ORIENTED_EDGE('',*,*,#42603,.T.) ;
#59679 = ORIENTED_EDGE('',*,*,#39439,.F.) ;
#59680 = ORIENTED_EDGE('',*,*,#42605,.F.) ;
#59681 = ORIENTED_EDGE('',*,*,#39593,.F.) ;
#59682 = ORIENTED_EDGE('',*,*,#42604,.T.) ;
#59683 = ORIENTED_EDGE('',*,*,#39645,.F.) ;
#59684 = ORIENTED_EDGE('',*,*,#42605,.T.) ;
#59685 = ORIENTED_EDGE('',*,*,#42606,.F.) ;
#59686 = ORIENTED_EDGE('',*,*,#40702,.F.) ;
#59687 = ORIENTED_EDGE('',*,*,#42607,.F.) ;
#59688 = ORIENTED_EDGE('',*,*,#40749,.F.) ;
#59689 = ORIENTED_EDGE('',*,*,#42607,.T.) ;
#59690 = ORIENTED_EDGE('',*,*,#40699,.F.) ;
#59691 = ORIENTED_EDGE('',*,*,#42608,.F.) ;
#59692 = ORIENTED_EDGE('',*,*,#40750,.F.) ;
#59693 = ORIENTED_EDGE('',*,*,#40705,.F.) ;
#59694 = ORIENTED_EDGE('',*,*,#42606,.T.) ;
#59695 = ORIENTED_EDGE('',*,*,#42609,.F.) ;
#59696 = ORIENTED_EDGE('',*,*,#42608,.T.) ;
#59697 = ORIENTED_EDGE('',*,*,#40696,.F.) ;
#59698 = ORIENTED_EDGE('',*,*,#42610,.F.) ;
#59699 = ORIENTED_EDGE('',*,*,#40751,.F.) ;
#59700 = ORIENTED_EDGE('',*,*,#42609,.T.) ;
#59701 = ORIENTED_EDGE('',*,*,#40748,.F.) ;
#59702 = ORIENTED_EDGE('',*,*,#42611,.F.) ;
#59703 = ORIENTED_EDGE('',*,*,#40708,.F.) ;
#59704 = ORIENTED_EDGE('',*,*,#42610,.T.) ;
#59705 = ORIENTED_EDGE('',*,*,#40693,.F.) ;
#59706 = ORIENTED_EDGE('',*,*,#42612,.F.) ;
#59707 = ORIENTED_EDGE('',*,*,#40752,.F.) ;
#59708 = ORIENTED_EDGE('',*,*,#40711,.F.) ;
#59709 = ORIENTED_EDGE('',*,*,#42611,.T.) ;
#59710 = ORIENTED_EDGE('',*,*,#42613,.F.) ;
#59711 = ORIENTED_EDGE('',*,*,#42612,.T.) ;
#59712 = ORIENTED_EDGE('',*,*,#40690,.F.) ;
#59713 = ORIENTED_EDGE('',*,*,#42614,.F.) ;
#59714 = ORIENTED_EDGE('',*,*,#40753,.F.) ;
#59715 = ORIENTED_EDGE('',*,*,#42613,.T.) ;
#59716 = ORIENTED_EDGE('',*,*,#40747,.F.) ;
#59717 = ORIENTED_EDGE('',*,*,#42615,.F.) ;
#59718 = ORIENTED_EDGE('',*,*,#40714,.F.) ;
#59719 = ORIENTED_EDGE('',*,*,#42614,.T.) ;
#59720 = ORIENTED_EDGE('',*,*,#40687,.F.) ;
#59721 = ORIENTED_EDGE('',*,*,#42616,.F.) ;
#59722 = ORIENTED_EDGE('',*,*,#40717,.F.) ;
#59723 = ORIENTED_EDGE('',*,*,#42615,.T.) ;
#59724 = ORIENTED_EDGE('',*,*,#42617,.F.) ;
#59725 = ORIENTED_EDGE('',*,*,#42616,.T.) ;
#59726 = ORIENTED_EDGE('',*,*,#40684,.F.) ;
#59727 = ORIENTED_EDGE('',*,*,#42618,.F.) ;
#59728 = ORIENTED_EDGE('',*,*,#40754,.F.) ;
#59729 = ORIENTED_EDGE('',*,*,#42617,.T.) ;
#59730 = ORIENTED_EDGE('',*,*,#40746,.F.) ;
#59731 = ORIENTED_EDGE('',*,*,#42619,.F.) ;
#59732 = ORIENTED_EDGE('',*,*,#40720,.F.) ;
#59733 = ORIENTED_EDGE('',*,*,#42618,.T.) ;
#59734 = ORIENTED_EDGE('',*,*,#39310,.F.) ;
#59735 = ORIENTED_EDGE('',*,*,#42620,.F.) ;
#59736 = ORIENTED_EDGE('',*,*,#40723,.F.) ;
#59737 = ORIENTED_EDGE('',*,*,#42619,.T.) ;
#59738 = ORIENTED_EDGE('',*,*,#42621,.F.) ;
#59739 = ORIENTED_EDGE('',*,*,#42620,.T.) ;
#59740 = ORIENTED_EDGE('',*,*,#40682,.F.) ;
#59741 = ORIENTED_EDGE('',*,*,#39097,.F.) ;
#59742 = ORIENTED_EDGE('',*,*,#40755,.F.) ;
#59743 = ORIENTED_EDGE('',*,*,#42621,.T.) ;
#59744 = ORIENTED_EDGE('',*,*,#40745,.F.) ;
#59745 = ORIENTED_EDGE('',*,*,#42622,.F.) ;
#59746 = ORIENTED_EDGE('',*,*,#40726,.F.) ;
#59747 = ORIENTED_EDGE('',*,*,#40729,.F.) ;
#59748 = ORIENTED_EDGE('',*,*,#42622,.T.) ;
#59749 = ORIENTED_EDGE('',*,*,#42623,.F.) ;
#59750 = ORIENTED_EDGE('',*,*,#39096,.T.) ;
#59751 = ORIENTED_EDGE('',*,*,#40677,.F.) ;
#59752 = ORIENTED_EDGE('',*,*,#42624,.F.) ;
#59753 = ORIENTED_EDGE('',*,*,#40756,.F.) ;
#59754 = ORIENTED_EDGE('',*,*,#42623,.T.) ;
#59755 = ORIENTED_EDGE('',*,*,#40744,.F.) ;
#59756 = ORIENTED_EDGE('',*,*,#42625,.F.) ;
#59757 = ORIENTED_EDGE('',*,*,#40732,.F.) ;
#59758 = ORIENTED_EDGE('',*,*,#42624,.T.) ;
#59759 = ORIENTED_EDGE('',*,*,#40674,.F.) ;
#59760 = ORIENTED_EDGE('',*,*,#42626,.F.) ;
#59761 = ORIENTED_EDGE('',*,*,#40735,.F.) ;
#59762 = ORIENTED_EDGE('',*,*,#42625,.T.) ;
#59763 = ORIENTED_EDGE('',*,*,#42627,.F.) ;
#59764 = ORIENTED_EDGE('',*,*,#42626,.T.) ;
#59765 = ORIENTED_EDGE('',*,*,#40671,.F.) ;
#59766 = ORIENTED_EDGE('',*,*,#42628,.F.) ;
#59767 = ORIENTED_EDGE('',*,*,#40757,.F.) ;
#59768 = ORIENTED_EDGE('',*,*,#42627,.T.) ;
#59769 = ORIENTED_EDGE('',*,*,#40743,.F.) ;
#59770 = ORIENTED_EDGE('',*,*,#42629,.F.) ;
#59771 = ORIENTED_EDGE('',*,*,#40738,.F.) ;
#59772 = ORIENTED_EDGE('',*,*,#42628,.T.) ;
#59773 = ORIENTED_EDGE('',*,*,#40668,.F.) ;
#59774 = ORIENTED_EDGE('',*,*,#42630,.F.) ;
#59775 = ORIENTED_EDGE('',*,*,#40740,.F.) ;
#59776 = ORIENTED_EDGE('',*,*,#42629,.T.) ;
#59777 = ORIENTED_EDGE('',*,*,#40742,.F.) ;
#59778 = ORIENTED_EDGE('',*,*,#42631,.F.) ;
#59779 = ORIENTED_EDGE('',*,*,#40662,.F.) ;
#59780 = ORIENTED_EDGE('',*,*,#42630,.T.) ;
#59781 = ORIENTED_EDGE('',*,*,#40665,.F.) ;
#59782 = ORIENTED_EDGE('',*,*,#42631,.T.) ;
#59783 = ORIENTED_EDGE('',*,*,#40741,.F.) ;
#59784 = ORIENTED_EDGE('',*,*,#42632,.T.) ;
#59785 = ORIENTED_EDGE('',*,*,#42633,.T.) ;
#59786 = ORIENTED_EDGE('',*,*,#42634,.T.) ;
#59787 = ORIENTED_EDGE('',*,*,#42635,.T.) ;
#59788 = ORIENTED_EDGE('',*,*,#42636,.T.) ;
#59789 = ORIENTED_EDGE('',*,*,#42637,.T.) ;
#59790 = ORIENTED_EDGE('',*,*,#42638,.T.) ;
#59791 = ORIENTED_EDGE('',*,*,#42639,.T.) ;
#59792 = ORIENTED_EDGE('',*,*,#42640,.T.) ;
#59793 = ORIENTED_EDGE('',*,*,#42641,.T.) ;
#59794 = ORIENTED_EDGE('',*,*,#42642,.T.) ;
#59795 = ORIENTED_EDGE('',*,*,#42643,.T.) ;
#59796 = ORIENTED_EDGE('',*,*,#42644,.T.) ;
#59797 = ORIENTED_EDGE('',*,*,#42645,.T.) ;
#59798 = ORIENTED_EDGE('',*,*,#42646,.T.) ;
#59799 = ORIENTED_EDGE('',*,*,#42647,.T.) ;
#59800 = ORIENTED_EDGE('',*,*,#42648,.T.) ;
#59801 = ORIENTED_EDGE('',*,*,#42649,.T.) ;
#59802 = ORIENTED_EDGE('',*,*,#42650,.F.) ;
#59803 = ORIENTED_EDGE('',*,*,#42651,.T.) ;
#59804 = ORIENTED_EDGE('',*,*,#42652,.T.) ;
#59805 = ORIENTED_EDGE('',*,*,#42653,.T.) ;
#59806 = ORIENTED_EDGE('',*,*,#41620,.T.) ;
#59807 = ORIENTED_EDGE('',*,*,#42654,.T.) ;
#59808 = ORIENTED_EDGE('',*,*,#42655,.T.) ;
#59809 = ORIENTED_EDGE('',*,*,#42656,.T.) ;
#59810 = ORIENTED_EDGE('',*,*,#42657,.T.) ;
#59811 = ORIENTED_EDGE('',*,*,#42658,.T.) ;
#59812 = ORIENTED_EDGE('',*,*,#39275,.T.) ;
#59813 = ORIENTED_EDGE('',*,*,#42659,.T.) ;
#59814 = ORIENTED_EDGE('',*,*,#42660,.T.) ;
#59815 = ORIENTED_EDGE('',*,*,#42661,.T.) ;
#59816 = ORIENTED_EDGE('',*,*,#41617,.T.) ;
#59817 = ORIENTED_EDGE('',*,*,#42662,.T.) ;
#59818 = ORIENTED_EDGE('',*,*,#42632,.F.) ;
#59819 = ORIENTED_EDGE('',*,*,#42663,.T.) ;
#59820 = ORIENTED_EDGE('',*,*,#41618,.T.) ;
#59821 = ORIENTED_EDGE('',*,*,#42650,.T.) ;
#59822 = ORIENTED_EDGE('',*,*,#42664,.T.) ;
#59823 = ORIENTED_EDGE('',*,*,#39428,.F.) ;
#59824 = ORIENTED_EDGE('',*,*,#42665,.T.) ;
#59825 = ORIENTED_EDGE('',*,*,#42666,.T.) ;
#59826 = ORIENTED_EDGE('',*,*,#42667,.T.) ;
#59827 = ORIENTED_EDGE('',*,*,#42668,.T.) ;
#59828 = ORIENTED_EDGE('',*,*,#42669,.T.) ;
#59829 = ORIENTED_EDGE('',*,*,#42670,.T.) ;
#59830 = ORIENTED_EDGE('',*,*,#42671,.T.) ;
#59831 = ORIENTED_EDGE('',*,*,#41536,.F.) ;
#59832 = ORIENTED_EDGE('',*,*,#42672,.T.) ;
#59833 = ORIENTED_EDGE('',*,*,#41540,.F.) ;
#59834 = ORIENTED_EDGE('',*,*,#42673,.T.) ;
#59835 = ORIENTED_EDGE('',*,*,#42674,.T.) ;
#59836 = ORIENTED_EDGE('',*,*,#42675,.T.) ;
#59837 = ORIENTED_EDGE('',*,*,#42676,.T.) ;
#59838 = ORIENTED_EDGE('',*,*,#42677,.T.) ;
#59839 = ORIENTED_EDGE('',*,*,#42678,.T.) ;
#59840 = ORIENTED_EDGE('',*,*,#42679,.T.) ;
#59841 = ORIENTED_EDGE('',*,*,#42680,.T.) ;
#59842 = ORIENTED_EDGE('',*,*,#42681,.T.) ;
#59843 = ORIENTED_EDGE('',*,*,#42682,.T.) ;
#59844 = ORIENTED_EDGE('',*,*,#42683,.T.) ;
#59845 = ORIENTED_EDGE('',*,*,#42684,.T.) ;
#59846 = ORIENTED_EDGE('',*,*,#42685,.T.) ;
#59847 = ORIENTED_EDGE('',*,*,#41534,.T.) ;
#59848 = ORIENTED_EDGE('',*,*,#42686,.T.) ;
#59849 = ORIENTED_EDGE('',*,*,#41538,.F.) ;
#59850 = ORIENTED_EDGE('',*,*,#42687,.T.) ;
#59851 = ORIENTED_EDGE('',*,*,#42688,.T.) ;
#59852 = ORIENTED_EDGE('',*,*,#42689,.T.) ;
#59853 = ORIENTED_EDGE('',*,*,#42690,.T.) ;
#59854 = ORIENTED_EDGE('',*,*,#42691,.T.) ;
#59855 = ORIENTED_EDGE('',*,*,#42692,.T.) ;
#59856 = ORIENTED_EDGE('',*,*,#42693,.T.) ;
#59857 = ORIENTED_EDGE('',*,*,#42694,.T.) ;
#59858 = ORIENTED_EDGE('',*,*,#42695,.T.) ;
#59859 = ORIENTED_EDGE('',*,*,#42696,.T.) ;
#59860 = ORIENTED_EDGE('',*,*,#42697,.T.) ;
#59861 = ORIENTED_EDGE('',*,*,#42698,.T.) ;
#59862 = ORIENTED_EDGE('',*,*,#42699,.T.) ;
#59863 = ORIENTED_EDGE('',*,*,#42700,.T.) ;
#59864 = ORIENTED_EDGE('',*,*,#42701,.T.) ;
#59865 = ORIENTED_EDGE('',*,*,#42702,.T.) ;
#59866 = ORIENTED_EDGE('',*,*,#42703,.T.) ;
#59867 = ORIENTED_EDGE('',*,*,#42704,.T.) ;
#59868 = ORIENTED_EDGE('',*,*,#42705,.T.) ;
#59869 = ORIENTED_EDGE('',*,*,#42706,.T.) ;
#59870 = ORIENTED_EDGE('',*,*,#42707,.T.) ;
#59871 = ORIENTED_EDGE('',*,*,#42708,.F.) ;
#59872 = ORIENTED_EDGE('',*,*,#42709,.T.) ;
#59873 = ORIENTED_EDGE('',*,*,#42710,.T.) ;
#59874 = ORIENTED_EDGE('',*,*,#42711,.T.) ;
#59875 = ORIENTED_EDGE('',*,*,#41942,.T.) ;
#59876 = ORIENTED_EDGE('',*,*,#42712,.T.) ;
#59877 = ORIENTED_EDGE('',*,*,#42713,.T.) ;
#59878 = ORIENTED_EDGE('',*,*,#42714,.T.) ;
#59879 = ORIENTED_EDGE('',*,*,#42715,.T.) ;
#59880 = ORIENTED_EDGE('',*,*,#42716,.T.) ;
#59881 = ORIENTED_EDGE('',*,*,#39222,.T.) ;
#59882 = ORIENTED_EDGE('',*,*,#42717,.T.) ;
#59883 = ORIENTED_EDGE('',*,*,#42718,.T.) ;
#59884 = ORIENTED_EDGE('',*,*,#42719,.T.) ;
#59885 = ORIENTED_EDGE('',*,*,#41939,.T.) ;
#59886 = ORIENTED_EDGE('',*,*,#42720,.T.) ;
#59887 = ORIENTED_EDGE('',*,*,#42690,.F.) ;
#59888 = ORIENTED_EDGE('',*,*,#42721,.T.) ;
#59889 = ORIENTED_EDGE('',*,*,#41940,.T.) ;
#59890 = ORIENTED_EDGE('',*,*,#42708,.T.) ;
#59891 = ORIENTED_EDGE('',*,*,#42722,.T.) ;
#59892 = ORIENTED_EDGE('',*,*,#39417,.F.) ;
#59893 = ORIENTED_EDGE('',*,*,#42723,.T.) ;
#59894 = ORIENTED_EDGE('',*,*,#42724,.T.) ;
#59895 = ORIENTED_EDGE('',*,*,#42725,.T.) ;
#59896 = ORIENTED_EDGE('',*,*,#42726,.T.) ;
#59897 = ORIENTED_EDGE('',*,*,#42727,.T.) ;
#59898 = ORIENTED_EDGE('',*,*,#42728,.T.) ;
#59899 = ORIENTED_EDGE('',*,*,#42729,.T.) ;
#59900 = ORIENTED_EDGE('',*,*,#41544,.F.) ;
#59901 = ORIENTED_EDGE('',*,*,#42730,.T.) ;
#59902 = ORIENTED_EDGE('',*,*,#41548,.F.) ;
#59903 = ORIENTED_EDGE('',*,*,#42731,.T.) ;
#59904 = ORIENTED_EDGE('',*,*,#42732,.T.) ;
#59905 = ORIENTED_EDGE('',*,*,#42733,.T.) ;
#59906 = ORIENTED_EDGE('',*,*,#42734,.T.) ;
#59907 = ORIENTED_EDGE('',*,*,#42735,.T.) ;
#59908 = ORIENTED_EDGE('',*,*,#42736,.T.) ;
#59909 = ORIENTED_EDGE('',*,*,#42737,.T.) ;
#59910 = ORIENTED_EDGE('',*,*,#42738,.T.) ;
#59911 = ORIENTED_EDGE('',*,*,#42739,.T.) ;
#59912 = ORIENTED_EDGE('',*,*,#42740,.T.) ;
#59913 = ORIENTED_EDGE('',*,*,#42741,.T.) ;
#59914 = ORIENTED_EDGE('',*,*,#42742,.T.) ;
#59915 = ORIENTED_EDGE('',*,*,#42743,.T.) ;
#59916 = ORIENTED_EDGE('',*,*,#41542,.T.) ;
#59917 = ORIENTED_EDGE('',*,*,#42744,.T.) ;
#59918 = ORIENTED_EDGE('',*,*,#41546,.F.) ;
#59919 = ORIENTED_EDGE('',*,*,#42745,.T.) ;
#59920 = ORIENTED_EDGE('',*,*,#42746,.T.) ;
#59921 = ORIENTED_EDGE('',*,*,#42747,.T.) ;
#59922 = ORIENTED_EDGE('',*,*,#42748,.T.) ;
#59923 = ORIENTED_EDGE('',*,*,#42749,.T.) ;
#59924 = ORIENTED_EDGE('',*,*,#42750,.T.) ;
#59925 = ORIENTED_EDGE('',*,*,#42751,.T.) ;
#59926 = ORIENTED_EDGE('',*,*,#42752,.T.) ;
#59927 = ORIENTED_EDGE('',*,*,#42753,.T.) ;
#59928 = ORIENTED_EDGE('',*,*,#42754,.T.) ;
#59929 = ORIENTED_EDGE('',*,*,#42755,.T.) ;
#59930 = ORIENTED_EDGE('',*,*,#42756,.T.) ;
#59931 = ORIENTED_EDGE('',*,*,#42757,.T.) ;
#59932 = ORIENTED_EDGE('',*,*,#42758,.T.) ;
#59933 = ORIENTED_EDGE('',*,*,#42759,.T.) ;
#59934 = ORIENTED_EDGE('',*,*,#42760,.T.) ;
#59935 = ORIENTED_EDGE('',*,*,#42761,.T.) ;
#59936 = ORIENTED_EDGE('',*,*,#42762,.T.) ;
#59937 = ORIENTED_EDGE('',*,*,#42763,.T.) ;
#59938 = ORIENTED_EDGE('',*,*,#42764,.T.) ;
#59939 = ORIENTED_EDGE('',*,*,#42765,.T.) ;
#59940 = ORIENTED_EDGE('',*,*,#42766,.F.) ;
#59941 = ORIENTED_EDGE('',*,*,#42767,.T.) ;
#59942 = ORIENTED_EDGE('',*,*,#42768,.T.) ;
#59943 = ORIENTED_EDGE('',*,*,#42769,.T.) ;
#59944 = ORIENTED_EDGE('',*,*,#42030,.T.) ;
#59945 = ORIENTED_EDGE('',*,*,#42770,.T.) ;
#59946 = ORIENTED_EDGE('',*,*,#42771,.T.) ;
#59947 = ORIENTED_EDGE('',*,*,#42772,.T.) ;
#59948 = ORIENTED_EDGE('',*,*,#42773,.T.) ;
#59949 = ORIENTED_EDGE('',*,*,#42774,.T.) ;
#59950 = ORIENTED_EDGE('',*,*,#39205,.T.) ;
#59951 = ORIENTED_EDGE('',*,*,#42775,.T.) ;
#59952 = ORIENTED_EDGE('',*,*,#42776,.T.) ;
#59953 = ORIENTED_EDGE('',*,*,#42777,.T.) ;
#59954 = ORIENTED_EDGE('',*,*,#42027,.T.) ;
#59955 = ORIENTED_EDGE('',*,*,#42778,.T.) ;
#59956 = ORIENTED_EDGE('',*,*,#42748,.F.) ;
#59957 = ORIENTED_EDGE('',*,*,#42779,.T.) ;
#59958 = ORIENTED_EDGE('',*,*,#42028,.T.) ;
#59959 = ORIENTED_EDGE('',*,*,#42766,.T.) ;
#59960 = ORIENTED_EDGE('',*,*,#42780,.T.) ;
#59961 = ORIENTED_EDGE('',*,*,#39406,.F.) ;
#59962 = ORIENTED_EDGE('',*,*,#42781,.T.) ;
#59963 = ORIENTED_EDGE('',*,*,#42782,.T.) ;
#59964 = ORIENTED_EDGE('',*,*,#42783,.T.) ;
#59965 = ORIENTED_EDGE('',*,*,#42784,.T.) ;
#59966 = ORIENTED_EDGE('',*,*,#42785,.T.) ;
#59967 = ORIENTED_EDGE('',*,*,#42786,.T.) ;
#59968 = ORIENTED_EDGE('',*,*,#42787,.T.) ;
#59969 = ORIENTED_EDGE('',*,*,#41552,.F.) ;
#59970 = ORIENTED_EDGE('',*,*,#42788,.T.) ;
#59971 = ORIENTED_EDGE('',*,*,#41556,.F.) ;
#59972 = ORIENTED_EDGE('',*,*,#42789,.T.) ;
#59973 = ORIENTED_EDGE('',*,*,#42790,.T.) ;
#59974 = ORIENTED_EDGE('',*,*,#42791,.T.) ;
#59975 = ORIENTED_EDGE('',*,*,#42792,.T.) ;
#59976 = ORIENTED_EDGE('',*,*,#42793,.T.) ;
#59977 = ORIENTED_EDGE('',*,*,#42794,.T.) ;
#59978 = ORIENTED_EDGE('',*,*,#42795,.T.) ;
#59979 = ORIENTED_EDGE('',*,*,#42796,.T.) ;
#59980 = ORIENTED_EDGE('',*,*,#42797,.T.) ;
#59981 = ORIENTED_EDGE('',*,*,#42798,.T.) ;
#59982 = ORIENTED_EDGE('',*,*,#42799,.T.) ;
#59983 = ORIENTED_EDGE('',*,*,#42800,.T.) ;
#59984 = ORIENTED_EDGE('',*,*,#42801,.T.) ;
#59985 = ORIENTED_EDGE('',*,*,#41550,.T.) ;
#59986 = ORIENTED_EDGE('',*,*,#42802,.T.) ;
#59987 = ORIENTED_EDGE('',*,*,#41554,.F.) ;
#59988 = ORIENTED_EDGE('',*,*,#42803,.T.) ;
#59989 = ORIENTED_EDGE('',*,*,#42804,.T.) ;
#59990 = ORIENTED_EDGE('',*,*,#42805,.T.) ;
#59991 = ORIENTED_EDGE('',*,*,#42806,.T.) ;
#59992 = ORIENTED_EDGE('',*,*,#42807,.T.) ;
#59993 = ORIENTED_EDGE('',*,*,#42808,.T.) ;
#59994 = ORIENTED_EDGE('',*,*,#42809,.T.) ;
#59995 = ORIENTED_EDGE('',*,*,#42810,.T.) ;
#59996 = ORIENTED_EDGE('',*,*,#42811,.T.) ;
#59997 = ORIENTED_EDGE('',*,*,#42812,.T.) ;
#59998 = ORIENTED_EDGE('',*,*,#42813,.T.) ;
#59999 = ORIENTED_EDGE('',*,*,#42814,.T.) ;
#60000 = ORIENTED_EDGE('',*,*,#42815,.T.) ;
#60001 = ORIENTED_EDGE('',*,*,#42816,.T.) ;
#60002 = ORIENTED_EDGE('',*,*,#42817,.T.) ;
#60003 = ORIENTED_EDGE('',*,*,#42818,.T.) ;
#60004 = ORIENTED_EDGE('',*,*,#42819,.T.) ;
#60005 = ORIENTED_EDGE('',*,*,#42820,.T.) ;
#60006 = ORIENTED_EDGE('',*,*,#42821,.T.) ;
#60007 = ORIENTED_EDGE('',*,*,#42822,.T.) ;
#60008 = ORIENTED_EDGE('',*,*,#42823,.T.) ;
#60009 = ORIENTED_EDGE('',*,*,#42824,.F.) ;
#60010 = ORIENTED_EDGE('',*,*,#42825,.T.) ;
#60011 = ORIENTED_EDGE('',*,*,#42826,.T.) ;
#60012 = ORIENTED_EDGE('',*,*,#42827,.T.) ;
#60013 = ORIENTED_EDGE('',*,*,#42118,.T.) ;
#60014 = ORIENTED_EDGE('',*,*,#42828,.T.) ;
#60015 = ORIENTED_EDGE('',*,*,#42829,.T.) ;
#60016 = ORIENTED_EDGE('',*,*,#42830,.T.) ;
#60017 = ORIENTED_EDGE('',*,*,#42831,.T.) ;
#60018 = ORIENTED_EDGE('',*,*,#42832,.T.) ;
#60019 = ORIENTED_EDGE('',*,*,#39188,.T.) ;
#60020 = ORIENTED_EDGE('',*,*,#42833,.T.) ;
#60021 = ORIENTED_EDGE('',*,*,#42834,.T.) ;
#60022 = ORIENTED_EDGE('',*,*,#42835,.T.) ;
#60023 = ORIENTED_EDGE('',*,*,#42115,.T.) ;
#60024 = ORIENTED_EDGE('',*,*,#42836,.T.) ;
#60025 = ORIENTED_EDGE('',*,*,#42806,.F.) ;
#60026 = ORIENTED_EDGE('',*,*,#42837,.T.) ;
#60027 = ORIENTED_EDGE('',*,*,#42116,.T.) ;
#60028 = ORIENTED_EDGE('',*,*,#42824,.T.) ;
#60029 = ORIENTED_EDGE('',*,*,#42838,.T.) ;
#60030 = ORIENTED_EDGE('',*,*,#39395,.F.) ;
#60031 = ORIENTED_EDGE('',*,*,#42839,.T.) ;
#60032 = ORIENTED_EDGE('',*,*,#42840,.T.) ;
#60033 = ORIENTED_EDGE('',*,*,#42841,.T.) ;
#60034 = ORIENTED_EDGE('',*,*,#42842,.T.) ;
#60035 = ORIENTED_EDGE('',*,*,#42843,.T.) ;
#60036 = ORIENTED_EDGE('',*,*,#42844,.T.) ;
#60037 = ORIENTED_EDGE('',*,*,#42845,.T.) ;
#60038 = ORIENTED_EDGE('',*,*,#41560,.F.) ;
#60039 = ORIENTED_EDGE('',*,*,#42846,.T.) ;
#60040 = ORIENTED_EDGE('',*,*,#41564,.F.) ;
#60041 = ORIENTED_EDGE('',*,*,#42847,.T.) ;
#60042 = ORIENTED_EDGE('',*,*,#42848,.T.) ;
#60043 = ORIENTED_EDGE('',*,*,#42849,.T.) ;
#60044 = ORIENTED_EDGE('',*,*,#42850,.T.) ;
#60045 = ORIENTED_EDGE('',*,*,#42851,.T.) ;
#60046 = ORIENTED_EDGE('',*,*,#42852,.T.) ;
#60047 = ORIENTED_EDGE('',*,*,#42853,.T.) ;
#60048 = ORIENTED_EDGE('',*,*,#42854,.T.) ;
#60049 = ORIENTED_EDGE('',*,*,#42855,.T.) ;
#60050 = ORIENTED_EDGE('',*,*,#42856,.T.) ;
#60051 = ORIENTED_EDGE('',*,*,#42857,.T.) ;
#60052 = ORIENTED_EDGE('',*,*,#42858,.T.) ;
#60053 = ORIENTED_EDGE('',*,*,#42859,.T.) ;
#60054 = ORIENTED_EDGE('',*,*,#41558,.T.) ;
#60055 = ORIENTED_EDGE('',*,*,#42860,.T.) ;
#60056 = ORIENTED_EDGE('',*,*,#41562,.F.) ;
#60057 = ORIENTED_EDGE('',*,*,#42861,.T.) ;
#60058 = ORIENTED_EDGE('',*,*,#42862,.T.) ;
#60059 = ORIENTED_EDGE('',*,*,#42863,.T.) ;
#60060 = ORIENTED_EDGE('',*,*,#42864,.T.) ;
#60061 = ORIENTED_EDGE('',*,*,#42865,.T.) ;
#60062 = ORIENTED_EDGE('',*,*,#42866,.T.) ;
#60063 = ORIENTED_EDGE('',*,*,#42867,.T.) ;
#60064 = ORIENTED_EDGE('',*,*,#42868,.T.) ;
#60065 = ORIENTED_EDGE('',*,*,#42869,.T.) ;
#60066 = ORIENTED_EDGE('',*,*,#42870,.T.) ;
#60067 = ORIENTED_EDGE('',*,*,#42871,.T.) ;
#60068 = ORIENTED_EDGE('',*,*,#42872,.T.) ;
#60069 = ORIENTED_EDGE('',*,*,#42873,.T.) ;
#60070 = ORIENTED_EDGE('',*,*,#42874,.T.) ;
#60071 = ORIENTED_EDGE('',*,*,#42875,.T.) ;
#60072 = ORIENTED_EDGE('',*,*,#42876,.T.) ;
#60073 = ORIENTED_EDGE('',*,*,#42877,.T.) ;
#60074 = ORIENTED_EDGE('',*,*,#42878,.T.) ;
#60075 = ORIENTED_EDGE('',*,*,#42879,.T.) ;
#60076 = ORIENTED_EDGE('',*,*,#42880,.T.) ;
#60077 = ORIENTED_EDGE('',*,*,#42881,.T.) ;
#60078 = ORIENTED_EDGE('',*,*,#42882,.F.) ;
#60079 = ORIENTED_EDGE('',*,*,#42883,.T.) ;
#60080 = ORIENTED_EDGE('',*,*,#42884,.T.) ;
#60081 = ORIENTED_EDGE('',*,*,#42885,.T.) ;
#60082 = ORIENTED_EDGE('',*,*,#42206,.T.) ;
#60083 = ORIENTED_EDGE('',*,*,#42886,.T.) ;
#60084 = ORIENTED_EDGE('',*,*,#42887,.T.) ;
#60085 = ORIENTED_EDGE('',*,*,#42888,.T.) ;
#60086 = ORIENTED_EDGE('',*,*,#42889,.T.) ;
#60087 = ORIENTED_EDGE('',*,*,#42890,.T.) ;
#60088 = ORIENTED_EDGE('',*,*,#39171,.T.) ;
#60089 = ORIENTED_EDGE('',*,*,#42891,.T.) ;
#60090 = ORIENTED_EDGE('',*,*,#42892,.T.) ;
#60091 = ORIENTED_EDGE('',*,*,#42893,.T.) ;
#60092 = ORIENTED_EDGE('',*,*,#42203,.T.) ;
#60093 = ORIENTED_EDGE('',*,*,#42894,.T.) ;
#60094 = ORIENTED_EDGE('',*,*,#42864,.F.) ;
#60095 = ORIENTED_EDGE('',*,*,#42895,.T.) ;
#60096 = ORIENTED_EDGE('',*,*,#42204,.T.) ;
#60097 = ORIENTED_EDGE('',*,*,#42882,.T.) ;
#60098 = ORIENTED_EDGE('',*,*,#42896,.T.) ;
#60099 = ORIENTED_EDGE('',*,*,#39384,.F.) ;
#60100 = ORIENTED_EDGE('',*,*,#42897,.T.) ;
#60101 = ORIENTED_EDGE('',*,*,#42898,.T.) ;
#60102 = ORIENTED_EDGE('',*,*,#42899,.T.) ;
#60103 = ORIENTED_EDGE('',*,*,#42900,.T.) ;
#60104 = ORIENTED_EDGE('',*,*,#42901,.T.) ;
#60105 = ORIENTED_EDGE('',*,*,#42902,.T.) ;
#60106 = ORIENTED_EDGE('',*,*,#42903,.T.) ;
#60107 = ORIENTED_EDGE('',*,*,#41568,.F.) ;
#60108 = ORIENTED_EDGE('',*,*,#42904,.T.) ;
#60109 = ORIENTED_EDGE('',*,*,#41572,.F.) ;
#60110 = ORIENTED_EDGE('',*,*,#42905,.T.) ;
#60111 = ORIENTED_EDGE('',*,*,#42906,.T.) ;
#60112 = ORIENTED_EDGE('',*,*,#42907,.T.) ;
#60113 = ORIENTED_EDGE('',*,*,#42908,.T.) ;
#60114 = ORIENTED_EDGE('',*,*,#42909,.T.) ;
#60115 = ORIENTED_EDGE('',*,*,#42910,.T.) ;
#60116 = ORIENTED_EDGE('',*,*,#42911,.T.) ;
#60117 = ORIENTED_EDGE('',*,*,#42912,.T.) ;
#60118 = ORIENTED_EDGE('',*,*,#42913,.T.) ;
#60119 = ORIENTED_EDGE('',*,*,#42914,.T.) ;
#60120 = ORIENTED_EDGE('',*,*,#42915,.T.) ;
#60121 = ORIENTED_EDGE('',*,*,#42916,.T.) ;
#60122 = ORIENTED_EDGE('',*,*,#42917,.T.) ;
#60123 = ORIENTED_EDGE('',*,*,#41566,.T.) ;
#60124 = ORIENTED_EDGE('',*,*,#42918,.T.) ;
#60125 = ORIENTED_EDGE('',*,*,#41570,.F.) ;
#60126 = ORIENTED_EDGE('',*,*,#42919,.T.) ;
#60127 = ORIENTED_EDGE('',*,*,#42920,.T.) ;
#60128 = ORIENTED_EDGE('',*,*,#42921,.T.) ;
#60129 = ORIENTED_EDGE('',*,*,#42922,.T.) ;
#60130 = ORIENTED_EDGE('',*,*,#42923,.T.) ;
#60131 = ORIENTED_EDGE('',*,*,#42924,.T.) ;
#60132 = ORIENTED_EDGE('',*,*,#42925,.T.) ;
#60133 = ORIENTED_EDGE('',*,*,#42926,.T.) ;
#60134 = ORIENTED_EDGE('',*,*,#42927,.T.) ;
#60135 = ORIENTED_EDGE('',*,*,#42928,.T.) ;
#60136 = ORIENTED_EDGE('',*,*,#42929,.T.) ;
#60137 = ORIENTED_EDGE('',*,*,#42930,.T.) ;
#60138 = ORIENTED_EDGE('',*,*,#42931,.T.) ;
#60139 = ORIENTED_EDGE('',*,*,#42932,.T.) ;
#60140 = ORIENTED_EDGE('',*,*,#42933,.T.) ;
#60141 = ORIENTED_EDGE('',*,*,#42934,.T.) ;
#60142 = ORIENTED_EDGE('',*,*,#42935,.T.) ;
#60143 = ORIENTED_EDGE('',*,*,#42936,.T.) ;
#60144 = ORIENTED_EDGE('',*,*,#42937,.T.) ;
#60145 = ORIENTED_EDGE('',*,*,#42938,.T.) ;
#60146 = ORIENTED_EDGE('',*,*,#42939,.T.) ;
#60147 = ORIENTED_EDGE('',*,*,#42940,.F.) ;
#60148 = ORIENTED_EDGE('',*,*,#42941,.T.) ;
#60149 = ORIENTED_EDGE('',*,*,#42942,.T.) ;
#60150 = ORIENTED_EDGE('',*,*,#42943,.T.) ;
#60151 = ORIENTED_EDGE('',*,*,#42294,.T.) ;
#60152 = ORIENTED_EDGE('',*,*,#42944,.T.) ;
#60153 = ORIENTED_EDGE('',*,*,#42945,.T.) ;
#60154 = ORIENTED_EDGE('',*,*,#42946,.T.) ;
#60155 = ORIENTED_EDGE('',*,*,#42947,.T.) ;
#60156 = ORIENTED_EDGE('',*,*,#42948,.T.) ;
#60157 = ORIENTED_EDGE('',*,*,#39154,.T.) ;
#60158 = ORIENTED_EDGE('',*,*,#42949,.T.) ;
#60159 = ORIENTED_EDGE('',*,*,#42950,.T.) ;
#60160 = ORIENTED_EDGE('',*,*,#42951,.T.) ;
#60161 = ORIENTED_EDGE('',*,*,#42291,.T.) ;
#60162 = ORIENTED_EDGE('',*,*,#42952,.T.) ;
#60163 = ORIENTED_EDGE('',*,*,#42922,.F.) ;
#60164 = ORIENTED_EDGE('',*,*,#42953,.T.) ;
#60165 = ORIENTED_EDGE('',*,*,#42292,.T.) ;
#60166 = ORIENTED_EDGE('',*,*,#42940,.T.) ;
#60167 = ORIENTED_EDGE('',*,*,#42954,.T.) ;
#60168 = ORIENTED_EDGE('',*,*,#39373,.F.) ;
#60169 = ORIENTED_EDGE('',*,*,#42955,.T.) ;
#60170 = ORIENTED_EDGE('',*,*,#42956,.T.) ;
#60171 = ORIENTED_EDGE('',*,*,#42957,.T.) ;
#60172 = ORIENTED_EDGE('',*,*,#42958,.T.) ;
#60173 = ORIENTED_EDGE('',*,*,#42959,.T.) ;
#60174 = ORIENTED_EDGE('',*,*,#42960,.T.) ;
#60175 = ORIENTED_EDGE('',*,*,#42961,.T.) ;
#60176 = ORIENTED_EDGE('',*,*,#41576,.F.) ;
#60177 = ORIENTED_EDGE('',*,*,#42962,.T.) ;
#60178 = ORIENTED_EDGE('',*,*,#41580,.F.) ;
#60179 = ORIENTED_EDGE('',*,*,#42963,.T.) ;
#60180 = ORIENTED_EDGE('',*,*,#42964,.T.) ;
#60181 = ORIENTED_EDGE('',*,*,#42965,.T.) ;
#60182 = ORIENTED_EDGE('',*,*,#42966,.T.) ;
#60183 = ORIENTED_EDGE('',*,*,#42967,.T.) ;
#60184 = ORIENTED_EDGE('',*,*,#42968,.T.) ;
#60185 = ORIENTED_EDGE('',*,*,#42969,.T.) ;
#60186 = ORIENTED_EDGE('',*,*,#42970,.T.) ;
#60187 = ORIENTED_EDGE('',*,*,#42971,.T.) ;
#60188 = ORIENTED_EDGE('',*,*,#42972,.T.) ;
#60189 = ORIENTED_EDGE('',*,*,#42973,.T.) ;
#60190 = ORIENTED_EDGE('',*,*,#42974,.T.) ;
#60191 = ORIENTED_EDGE('',*,*,#42975,.T.) ;
#60192 = ORIENTED_EDGE('',*,*,#41574,.T.) ;
#60193 = ORIENTED_EDGE('',*,*,#42976,.T.) ;
#60194 = ORIENTED_EDGE('',*,*,#41578,.F.) ;
#60195 = ORIENTED_EDGE('',*,*,#42977,.T.) ;
#60196 = ORIENTED_EDGE('',*,*,#42978,.T.) ;
#60197 = ORIENTED_EDGE('',*,*,#42979,.T.) ;
#60198 = ORIENTED_EDGE('',*,*,#42980,.T.) ;
#60199 = ORIENTED_EDGE('',*,*,#42981,.T.) ;
#60200 = ORIENTED_EDGE('',*,*,#42982,.T.) ;
#60201 = ORIENTED_EDGE('',*,*,#42983,.T.) ;
#60202 = ORIENTED_EDGE('',*,*,#42984,.T.) ;
#60203 = ORIENTED_EDGE('',*,*,#42985,.T.) ;
#60204 = ORIENTED_EDGE('',*,*,#42986,.T.) ;
#60205 = ORIENTED_EDGE('',*,*,#42987,.T.) ;
#60206 = ORIENTED_EDGE('',*,*,#42988,.T.) ;
#60207 = ORIENTED_EDGE('',*,*,#42989,.T.) ;
#60208 = ORIENTED_EDGE('',*,*,#42990,.T.) ;
#60209 = ORIENTED_EDGE('',*,*,#42991,.T.) ;
#60210 = ORIENTED_EDGE('',*,*,#42992,.T.) ;
#60211 = ORIENTED_EDGE('',*,*,#42993,.T.) ;
#60212 = ORIENTED_EDGE('',*,*,#42994,.T.) ;
#60213 = ORIENTED_EDGE('',*,*,#42995,.T.) ;
#60214 = ORIENTED_EDGE('',*,*,#42996,.T.) ;
#60215 = ORIENTED_EDGE('',*,*,#42997,.T.) ;
#60216 = ORIENTED_EDGE('',*,*,#42998,.F.) ;
#60217 = ORIENTED_EDGE('',*,*,#42999,.T.) ;
#60218 = ORIENTED_EDGE('',*,*,#43000,.T.) ;
#60219 = ORIENTED_EDGE('',*,*,#43001,.T.) ;
#60220 = ORIENTED_EDGE('',*,*,#42382,.T.) ;
#60221 = ORIENTED_EDGE('',*,*,#43002,.T.) ;
#60222 = ORIENTED_EDGE('',*,*,#43003,.T.) ;
#60223 = ORIENTED_EDGE('',*,*,#43004,.T.) ;
#60224 = ORIENTED_EDGE('',*,*,#43005,.T.) ;
#60225 = ORIENTED_EDGE('',*,*,#43006,.T.) ;
#60226 = ORIENTED_EDGE('',*,*,#39137,.T.) ;
#60227 = ORIENTED_EDGE('',*,*,#43007,.T.) ;
#60228 = ORIENTED_EDGE('',*,*,#43008,.T.) ;
#60229 = ORIENTED_EDGE('',*,*,#43009,.T.) ;
#60230 = ORIENTED_EDGE('',*,*,#42379,.T.) ;
#60231 = ORIENTED_EDGE('',*,*,#43010,.T.) ;
#60232 = ORIENTED_EDGE('',*,*,#42980,.F.) ;
#60233 = ORIENTED_EDGE('',*,*,#43011,.T.) ;
#60234 = ORIENTED_EDGE('',*,*,#42380,.T.) ;
#60235 = ORIENTED_EDGE('',*,*,#42998,.T.) ;
#60236 = ORIENTED_EDGE('',*,*,#43012,.T.) ;
#60237 = ORIENTED_EDGE('',*,*,#39362,.F.) ;
#60238 = ORIENTED_EDGE('',*,*,#43013,.T.) ;
#60239 = ORIENTED_EDGE('',*,*,#43014,.T.) ;
#60240 = ORIENTED_EDGE('',*,*,#43015,.T.) ;
#60241 = ORIENTED_EDGE('',*,*,#43016,.T.) ;
#60242 = ORIENTED_EDGE('',*,*,#43017,.T.) ;
#60243 = ORIENTED_EDGE('',*,*,#43018,.T.) ;
#60244 = ORIENTED_EDGE('',*,*,#43019,.T.) ;
#60245 = ORIENTED_EDGE('',*,*,#41584,.F.) ;
#60246 = ORIENTED_EDGE('',*,*,#43020,.T.) ;
#60247 = ORIENTED_EDGE('',*,*,#41588,.F.) ;
#60248 = ORIENTED_EDGE('',*,*,#43021,.T.) ;
#60249 = ORIENTED_EDGE('',*,*,#43022,.T.) ;
#60250 = ORIENTED_EDGE('',*,*,#43023,.T.) ;
#60251 = ORIENTED_EDGE('',*,*,#43024,.T.) ;
#60252 = ORIENTED_EDGE('',*,*,#43025,.T.) ;
#60253 = ORIENTED_EDGE('',*,*,#43026,.T.) ;
#60254 = ORIENTED_EDGE('',*,*,#43027,.T.) ;
#60255 = ORIENTED_EDGE('',*,*,#43028,.T.) ;
#60256 = ORIENTED_EDGE('',*,*,#43029,.T.) ;
#60257 = ORIENTED_EDGE('',*,*,#43030,.T.) ;
#60258 = ORIENTED_EDGE('',*,*,#43031,.T.) ;
#60259 = ORIENTED_EDGE('',*,*,#43032,.T.) ;
#60260 = ORIENTED_EDGE('',*,*,#43033,.T.) ;
#60261 = ORIENTED_EDGE('',*,*,#41582,.T.) ;
#60262 = ORIENTED_EDGE('',*,*,#43034,.T.) ;
#60263 = ORIENTED_EDGE('',*,*,#41586,.F.) ;
#60264 = ORIENTED_EDGE('',*,*,#43035,.T.) ;
#60265 = ORIENTED_EDGE('',*,*,#43036,.T.) ;
#60266 = ORIENTED_EDGE('',*,*,#43037,.T.) ;
#60267 = ORIENTED_EDGE('',*,*,#43038,.T.) ;
#60268 = ORIENTED_EDGE('',*,*,#43039,.T.) ;
#60269 = ORIENTED_EDGE('',*,*,#43040,.T.) ;
#60270 = ORIENTED_EDGE('',*,*,#43041,.T.) ;
#60271 = ORIENTED_EDGE('',*,*,#43042,.T.) ;
#60272 = ORIENTED_EDGE('',*,*,#43043,.T.) ;
#60273 = ORIENTED_EDGE('',*,*,#43044,.T.) ;
#60274 = ORIENTED_EDGE('',*,*,#43045,.T.) ;
#60275 = ORIENTED_EDGE('',*,*,#43046,.T.) ;
#60276 = ORIENTED_EDGE('',*,*,#43047,.T.) ;
#60277 = ORIENTED_EDGE('',*,*,#43048,.T.) ;
#60278 = ORIENTED_EDGE('',*,*,#43049,.T.) ;
#60279 = ORIENTED_EDGE('',*,*,#43050,.T.) ;
#60280 = ORIENTED_EDGE('',*,*,#43051,.T.) ;
#60281 = ORIENTED_EDGE('',*,*,#43052,.T.) ;
#60282 = ORIENTED_EDGE('',*,*,#43053,.T.) ;
#60283 = ORIENTED_EDGE('',*,*,#43054,.T.) ;
#60284 = ORIENTED_EDGE('',*,*,#43055,.T.) ;
#60285 = ORIENTED_EDGE('',*,*,#43056,.F.) ;
#60286 = ORIENTED_EDGE('',*,*,#43057,.T.) ;
#60287 = ORIENTED_EDGE('',*,*,#43058,.T.) ;
#60288 = ORIENTED_EDGE('',*,*,#43059,.T.) ;
#60289 = ORIENTED_EDGE('',*,*,#42470,.T.) ;
#60290 = ORIENTED_EDGE('',*,*,#43060,.T.) ;
#60291 = ORIENTED_EDGE('',*,*,#43061,.T.) ;
#60292 = ORIENTED_EDGE('',*,*,#43062,.T.) ;
#60293 = ORIENTED_EDGE('',*,*,#43063,.T.) ;
#60294 = ORIENTED_EDGE('',*,*,#43064,.T.) ;
#60295 = ORIENTED_EDGE('',*,*,#39120,.T.) ;
#60296 = ORIENTED_EDGE('',*,*,#43065,.T.) ;
#60297 = ORIENTED_EDGE('',*,*,#43066,.T.) ;
#60298 = ORIENTED_EDGE('',*,*,#43067,.T.) ;
#60299 = ORIENTED_EDGE('',*,*,#42467,.T.) ;
#60300 = ORIENTED_EDGE('',*,*,#43068,.T.) ;
#60301 = ORIENTED_EDGE('',*,*,#43038,.F.) ;
#60302 = ORIENTED_EDGE('',*,*,#43069,.T.) ;
#60303 = ORIENTED_EDGE('',*,*,#42468,.T.) ;
#60304 = ORIENTED_EDGE('',*,*,#43056,.T.) ;
#60305 = ORIENTED_EDGE('',*,*,#43070,.T.) ;
#60306 = ORIENTED_EDGE('',*,*,#39351,.F.) ;
#60307 = ORIENTED_EDGE('',*,*,#43071,.T.) ;
#60308 = ORIENTED_EDGE('',*,*,#43072,.T.) ;
#60309 = ORIENTED_EDGE('',*,*,#43073,.T.) ;
#60310 = ORIENTED_EDGE('',*,*,#43074,.T.) ;
#60311 = ORIENTED_EDGE('',*,*,#43075,.T.) ;
#60312 = ORIENTED_EDGE('',*,*,#43076,.T.) ;
#60313 = ORIENTED_EDGE('',*,*,#43077,.T.) ;
#60314 = ORIENTED_EDGE('',*,*,#41592,.F.) ;
#60315 = ORIENTED_EDGE('',*,*,#43078,.T.) ;
#60316 = ORIENTED_EDGE('',*,*,#41596,.F.) ;
#60317 = ORIENTED_EDGE('',*,*,#43079,.T.) ;
#60318 = ORIENTED_EDGE('',*,*,#43080,.T.) ;
#60319 = ORIENTED_EDGE('',*,*,#43081,.T.) ;
#60320 = ORIENTED_EDGE('',*,*,#43082,.T.) ;
#60321 = ORIENTED_EDGE('',*,*,#43083,.T.) ;
#60322 = ORIENTED_EDGE('',*,*,#43084,.T.) ;
#60323 = ORIENTED_EDGE('',*,*,#43085,.T.) ;
#60324 = ORIENTED_EDGE('',*,*,#43086,.T.) ;
#60325 = ORIENTED_EDGE('',*,*,#43087,.T.) ;
#60326 = ORIENTED_EDGE('',*,*,#43088,.T.) ;
#60327 = ORIENTED_EDGE('',*,*,#43089,.T.) ;
#60328 = ORIENTED_EDGE('',*,*,#43090,.T.) ;
#60329 = ORIENTED_EDGE('',*,*,#43091,.T.) ;
#60330 = ORIENTED_EDGE('',*,*,#41590,.T.) ;
#60331 = ORIENTED_EDGE('',*,*,#43092,.T.) ;
#60332 = ORIENTED_EDGE('',*,*,#41594,.F.) ;
#60333 = ORIENTED_EDGE('',*,*,#43093,.T.) ;
#60334 = ORIENTED_EDGE('',*,*,#43094,.T.) ;
#60335 = ORIENTED_EDGE('',*,*,#43095,.T.) ;
#60336 = ORIENTED_EDGE('',*,*,#43096,.T.) ;
#60337 = ORIENTED_EDGE('',*,*,#43097,.T.) ;
#60338 = ORIENTED_EDGE('',*,*,#43098,.T.) ;
#60339 = ORIENTED_EDGE('',*,*,#43099,.T.) ;
#60340 = ORIENTED_EDGE('',*,*,#43100,.T.) ;
#60341 = ORIENTED_EDGE('',*,*,#43101,.T.) ;
#60342 = ORIENTED_EDGE('',*,*,#43102,.T.) ;
#60343 = ORIENTED_EDGE('',*,*,#43103,.T.) ;
#60344 = ORIENTED_EDGE('',*,*,#43104,.T.) ;
#60345 = ORIENTED_EDGE('',*,*,#43105,.T.) ;
#60346 = ORIENTED_EDGE('',*,*,#43106,.T.) ;
#60347 = ORIENTED_EDGE('',*,*,#43107,.T.) ;
#60348 = ORIENTED_EDGE('',*,*,#43108,.T.) ;
#60349 = ORIENTED_EDGE('',*,*,#43109,.T.) ;
#60350 = ORIENTED_EDGE('',*,*,#43110,.T.) ;
#60351 = ORIENTED_EDGE('',*,*,#43111,.T.) ;
#60352 = ORIENTED_EDGE('',*,*,#43112,.T.) ;
#60353 = ORIENTED_EDGE('',*,*,#43113,.T.) ;
#60354 = ORIENTED_EDGE('',*,*,#43114,.F.) ;
#60355 = ORIENTED_EDGE('',*,*,#43115,.T.) ;
#60356 = ORIENTED_EDGE('',*,*,#43116,.T.) ;
#60357 = ORIENTED_EDGE('',*,*,#43117,.T.) ;
#60358 = ORIENTED_EDGE('',*,*,#42558,.T.) ;
#60359 = ORIENTED_EDGE('',*,*,#43118,.T.) ;
#60360 = ORIENTED_EDGE('',*,*,#43119,.T.) ;
#60361 = ORIENTED_EDGE('',*,*,#43120,.T.) ;
#60362 = ORIENTED_EDGE('',*,*,#43121,.T.) ;
#60363 = ORIENTED_EDGE('',*,*,#43122,.T.) ;
#60364 = ORIENTED_EDGE('',*,*,#39103,.T.) ;
#60365 = ORIENTED_EDGE('',*,*,#43123,.T.) ;
#60366 = ORIENTED_EDGE('',*,*,#43124,.T.) ;
#60367 = ORIENTED_EDGE('',*,*,#43125,.T.) ;
#60368 = ORIENTED_EDGE('',*,*,#42555,.T.) ;
#60369 = ORIENTED_EDGE('',*,*,#43126,.T.) ;
#60370 = ORIENTED_EDGE('',*,*,#43096,.F.) ;
#60371 = ORIENTED_EDGE('',*,*,#43127,.T.) ;
#60372 = ORIENTED_EDGE('',*,*,#42556,.T.) ;
#60373 = ORIENTED_EDGE('',*,*,#43114,.T.) ;
#60374 = ORIENTED_EDGE('',*,*,#43128,.T.) ;
#60375 = ORIENTED_EDGE('',*,*,#39340,.F.) ;
#60376 = ORIENTED_EDGE('',*,*,#43129,.T.) ;
#60377 = ORIENTED_EDGE('',*,*,#43130,.T.) ;
#60378 = ORIENTED_EDGE('',*,*,#43131,.T.) ;
#60379 = ORIENTED_EDGE('',*,*,#43132,.T.) ;
#60380 = ORIENTED_EDGE('',*,*,#43133,.T.) ;
#60381 = ORIENTED_EDGE('',*,*,#43134,.T.) ;
#60382 = ORIENTED_EDGE('',*,*,#43135,.T.) ;
#60383 = ORIENTED_EDGE('',*,*,#41600,.F.) ;
#60384 = ORIENTED_EDGE('',*,*,#43136,.T.) ;
#60385 = ORIENTED_EDGE('',*,*,#41604,.F.) ;
#60386 = ORIENTED_EDGE('',*,*,#43137,.T.) ;
#60387 = ORIENTED_EDGE('',*,*,#43138,.T.) ;
#60388 = ORIENTED_EDGE('',*,*,#43139,.T.) ;
#60389 = ORIENTED_EDGE('',*,*,#43140,.T.) ;
#60390 = ORIENTED_EDGE('',*,*,#43141,.T.) ;
#60391 = ORIENTED_EDGE('',*,*,#43142,.T.) ;
#60392 = ORIENTED_EDGE('',*,*,#43143,.T.) ;
#60393 = ORIENTED_EDGE('',*,*,#43144,.T.) ;
#60394 = ORIENTED_EDGE('',*,*,#43145,.T.) ;
#60395 = ORIENTED_EDGE('',*,*,#43146,.T.) ;
#60396 = ORIENTED_EDGE('',*,*,#43147,.T.) ;
#60397 = ORIENTED_EDGE('',*,*,#43148,.T.) ;
#60398 = ORIENTED_EDGE('',*,*,#43149,.T.) ;
#60399 = ORIENTED_EDGE('',*,*,#41598,.T.) ;
#60400 = ORIENTED_EDGE('',*,*,#43150,.T.) ;
#60401 = ORIENTED_EDGE('',*,*,#41602,.F.) ;
#60402 = ORIENTED_EDGE('',*,*,#43151,.T.) ;
#60403 = ORIENTED_EDGE('',*,*,#43152,.T.) ;
#60404 = ORIENTED_EDGE('',*,*,#43153,.T.) ;
#60405 = ORIENTED_EDGE('',*,*,#43154,.T.) ;
#60406 = ORIENTED_EDGE('',*,*,#43155,.T.) ;
#60407 = ORIENTED_EDGE('',*,*,#43156,.T.) ;
#60408 = ORIENTED_EDGE('',*,*,#43157,.T.) ;
#60409 = ORIENTED_EDGE('',*,*,#43158,.T.) ;
#60410 = ORIENTED_EDGE('',*,*,#43159,.T.) ;
#60411 = ORIENTED_EDGE('',*,*,#43160,.T.) ;
#60412 = ORIENTED_EDGE('',*,*,#43161,.T.) ;
#60413 = ORIENTED_EDGE('',*,*,#43162,.T.) ;
#60414 = ORIENTED_EDGE('',*,*,#43163,.T.) ;
#60415 = ORIENTED_EDGE('',*,*,#43164,.T.) ;
#60416 = ORIENTED_EDGE('',*,*,#43165,.T.) ;
#60417 = ORIENTED_EDGE('',*,*,#43166,.T.) ;
#60418 = ORIENTED_EDGE('',*,*,#43167,.T.) ;
#60419 = ORIENTED_EDGE('',*,*,#43168,.T.) ;
#60420 = ORIENTED_EDGE('',*,*,#43169,.T.) ;
#60421 = ORIENTED_EDGE('',*,*,#43170,.T.) ;
#60422 = ORIENTED_EDGE('',*,*,#43171,.T.) ;
#60423 = ORIENTED_EDGE('',*,*,#43172,.T.) ;
#60424 = ORIENTED_EDGE('',*,*,#43173,.T.) ;
#60425 = ORIENTED_EDGE('',*,*,#43174,.T.) ;
#60426 = ORIENTED_EDGE('',*,*,#43175,.T.) ;
#60427 = ORIENTED_EDGE('',*,*,#43176,.T.) ;
#60428 = ORIENTED_EDGE('',*,*,#43177,.T.) ;
#60429 = ORIENTED_EDGE('',*,*,#43178,.T.) ;
#60430 = ORIENTED_EDGE('',*,*,#43179,.T.) ;
#60431 = ORIENTED_EDGE('',*,*,#43180,.T.) ;
#60432 = ORIENTED_EDGE('',*,*,#43181,.T.) ;
#60433 = ORIENTED_EDGE('',*,*,#43182,.T.) ;
#60434 = ORIENTED_EDGE('',*,*,#43183,.T.) ;
#60435 = ORIENTED_EDGE('',*,*,#43184,.T.) ;
#60436 = ORIENTED_EDGE('',*,*,#43185,.T.) ;
#60437 = ORIENTED_EDGE('',*,*,#43186,.T.) ;
#60438 = ORIENTED_EDGE('',*,*,#43187,.T.) ;
#60439 = ORIENTED_EDGE('',*,*,#43188,.T.) ;
#60440 = ORIENTED_EDGE('',*,*,#43189,.T.) ;
#60441 = ORIENTED_EDGE('',*,*,#43190,.T.) ;
#60442 = ORIENTED_EDGE('',*,*,#43191,.T.) ;
#60443 = ORIENTED_EDGE('',*,*,#43192,.T.) ;
#60444 = ORIENTED_EDGE('',*,*,#43193,.T.) ;
#60445 = ORIENTED_EDGE('',*,*,#43194,.T.) ;
#60446 = ORIENTED_EDGE('',*,*,#43195,.T.) ;
#60447 = ORIENTED_EDGE('',*,*,#43196,.T.) ;
#60448 = ORIENTED_EDGE('',*,*,#43197,.T.) ;
#60449 = ORIENTED_EDGE('',*,*,#43198,.T.) ;
#60450 = ORIENTED_EDGE('',*,*,#43199,.T.) ;
#60451 = ORIENTED_EDGE('',*,*,#43200,.T.) ;
#60452 = ORIENTED_EDGE('',*,*,#43201,.T.) ;
#60453 = ORIENTED_EDGE('',*,*,#43202,.T.) ;
#60454 = ORIENTED_EDGE('',*,*,#43203,.T.) ;
#60455 = ORIENTED_EDGE('',*,*,#43204,.T.) ;
#60456 = ORIENTED_EDGE('',*,*,#43205,.T.) ;
#60457 = ORIENTED_EDGE('',*,*,#43206,.T.) ;
#60458 = ORIENTED_EDGE('',*,*,#43207,.T.) ;
#60459 = ORIENTED_EDGE('',*,*,#43208,.T.) ;
#60460 = ORIENTED_EDGE('',*,*,#43209,.T.) ;
#60461 = ORIENTED_EDGE('',*,*,#43210,.T.) ;
#60462 = ORIENTED_EDGE('',*,*,#43211,.T.) ;
#60463 = ORIENTED_EDGE('',*,*,#43212,.T.) ;
#60464 = ORIENTED_EDGE('',*,*,#43213,.T.) ;
#60465 = ORIENTED_EDGE('',*,*,#43214,.T.) ;
#60466 = ORIENTED_EDGE('',*,*,#43215,.T.) ;
#60467 = ORIENTED_EDGE('',*,*,#43216,.T.) ;
#60468 = ORIENTED_EDGE('',*,*,#43217,.T.) ;
#60469 = ORIENTED_EDGE('',*,*,#43218,.T.) ;
#60470 = ORIENTED_EDGE('',*,*,#43219,.T.) ;
#60471 = ORIENTED_EDGE('',*,*,#43220,.T.) ;
#60472 = ORIENTED_EDGE('',*,*,#43221,.T.) ;
#60473 = ORIENTED_EDGE('',*,*,#43222,.T.) ;
#60474 = ORIENTED_EDGE('',*,*,#43223,.T.) ;
#60475 = ORIENTED_EDGE('',*,*,#43224,.T.) ;
#60476 = ORIENTED_EDGE('',*,*,#43225,.T.) ;
#60477 = ORIENTED_EDGE('',*,*,#43226,.T.) ;
#60478 = ORIENTED_EDGE('',*,*,#43227,.T.) ;
#60479 = ORIENTED_EDGE('',*,*,#43228,.T.) ;
#60480 = ORIENTED_EDGE('',*,*,#43229,.T.) ;
#60481 = ORIENTED_EDGE('',*,*,#43230,.T.) ;
#60482 = ORIENTED_EDGE('',*,*,#43231,.T.) ;
#60483 = ORIENTED_EDGE('',*,*,#43232,.T.) ;
#60484 = ORIENTED_EDGE('',*,*,#43233,.T.) ;
#60485 = ORIENTED_EDGE('',*,*,#43234,.T.) ;
#60486 = ORIENTED_EDGE('',*,*,#43235,.T.) ;
#60487 = ORIENTED_EDGE('',*,*,#43236,.T.) ;
#60488 = ORIENTED_EDGE('',*,*,#43237,.T.) ;
#60489 = ORIENTED_EDGE('',*,*,#43238,.T.) ;
#60490 = ORIENTED_EDGE('',*,*,#43239,.T.) ;
#60491 = ORIENTED_EDGE('',*,*,#43240,.T.) ;
#60492 = ORIENTED_EDGE('',*,*,#43241,.T.) ;
#60493 = ORIENTED_EDGE('',*,*,#43242,.T.) ;
#60494 = ORIENTED_EDGE('',*,*,#43243,.T.) ;
#60495 = ORIENTED_EDGE('',*,*,#43244,.T.) ;
#60496 = ORIENTED_EDGE('',*,*,#43245,.T.) ;
#60497 = ORIENTED_EDGE('',*,*,#43246,.T.) ;
#60498 = ORIENTED_EDGE('',*,*,#43247,.T.) ;
#60499 = ORIENTED_EDGE('',*,*,#43248,.T.) ;
#60500 = ORIENTED_EDGE('',*,*,#43249,.T.) ;
#60501 = ORIENTED_EDGE('',*,*,#43250,.T.) ;
#60502 = ORIENTED_EDGE('',*,*,#43251,.T.) ;
#60503 = ORIENTED_EDGE('',*,*,#43252,.T.) ;
#60504 = ORIENTED_EDGE('',*,*,#43253,.T.) ;
#60505 = ORIENTED_EDGE('',*,*,#43254,.T.) ;
#60506 = ORIENTED_EDGE('',*,*,#43255,.T.) ;
#60507 = ORIENTED_EDGE('',*,*,#43256,.T.) ;
#60508 = ORIENTED_EDGE('',*,*,#43257,.T.) ;
#60509 = ORIENTED_EDGE('',*,*,#43258,.T.) ;
#60510 = ORIENTED_EDGE('',*,*,#43259,.T.) ;
#60511 = ORIENTED_EDGE('',*,*,#43260,.T.) ;
#60512 = ORIENTED_EDGE('',*,*,#43261,.T.) ;
#60513 = ORIENTED_EDGE('',*,*,#43262,.T.) ;
#60514 = ORIENTED_EDGE('',*,*,#43263,.T.) ;
#60515 = ORIENTED_EDGE('',*,*,#43264,.T.) ;
#60516 = ORIENTED_EDGE('',*,*,#43265,.T.) ;
#60517 = ORIENTED_EDGE('',*,*,#43266,.T.) ;
#60518 = ORIENTED_EDGE('',*,*,#43267,.T.) ;
#60519 = ORIENTED_EDGE('',*,*,#43268,.T.) ;
#60520 = ORIENTED_EDGE('',*,*,#43269,.T.) ;
#60521 = ORIENTED_EDGE('',*,*,#43270,.T.) ;
#60522 = ORIENTED_EDGE('',*,*,#43271,.T.) ;
#60523 = ORIENTED_EDGE('',*,*,#43272,.T.) ;
#60524 = ORIENTED_EDGE('',*,*,#43273,.T.) ;
#60525 = ORIENTED_EDGE('',*,*,#43274,.T.) ;
#60526 = ORIENTED_EDGE('',*,*,#43275,.T.) ;
#60527 = ORIENTED_EDGE('',*,*,#43276,.T.) ;
#60528 = ORIENTED_EDGE('',*,*,#43277,.T.) ;
#60529 = ORIENTED_EDGE('',*,*,#43278,.T.) ;
#60530 = ORIENTED_EDGE('',*,*,#43279,.T.) ;
#60531 = ORIENTED_EDGE('',*,*,#43280,.T.) ;
#60532 = ORIENTED_EDGE('',*,*,#43281,.T.) ;
#60533 = ORIENTED_EDGE('',*,*,#43282,.T.) ;
#60534 = ORIENTED_EDGE('',*,*,#43283,.T.) ;
#60535 = ORIENTED_EDGE('',*,*,#43284,.T.) ;
#60536 = ORIENTED_EDGE('',*,*,#43285,.T.) ;
#60537 = ORIENTED_EDGE('',*,*,#43286,.T.) ;
#60538 = ORIENTED_EDGE('',*,*,#43287,.T.) ;
#60539 = ORIENTED_EDGE('',*,*,#43288,.T.) ;
#60540 = ORIENTED_EDGE('',*,*,#43289,.T.) ;
#60541 = ORIENTED_EDGE('',*,*,#43290,.T.) ;
#60542 = ORIENTED_EDGE('',*,*,#43291,.T.) ;
#60543 = ORIENTED_EDGE('',*,*,#43292,.T.) ;
#60544 = ORIENTED_EDGE('',*,*,#43293,.T.) ;
#60545 = ORIENTED_EDGE('',*,*,#43294,.T.) ;
#60546 = ORIENTED_EDGE('',*,*,#43295,.T.) ;
#60547 = ORIENTED_EDGE('',*,*,#43296,.T.) ;
#60548 = ORIENTED_EDGE('',*,*,#43297,.T.) ;
#60549 = ORIENTED_EDGE('',*,*,#43220,.F.) ;
#60550 = ORIENTED_EDGE('',*,*,#43298,.T.) ;
#60551 = ORIENTED_EDGE('',*,*,#42647,.F.) ;
#60552 = ORIENTED_EDGE('',*,*,#43299,.F.) ;
#60553 = ORIENTED_EDGE('',*,*,#42644,.F.) ;
#60554 = ORIENTED_EDGE('',*,*,#43300,.T.) ;
#60555 = ORIENTED_EDGE('',*,*,#42648,.F.) ;
#60556 = ORIENTED_EDGE('',*,*,#43301,.T.) ;
#60557 = ORIENTED_EDGE('',*,*,#43302,.F.) ;
#60558 = ORIENTED_EDGE('',*,*,#43299,.T.) ;
#60559 = ORIENTED_EDGE('',*,*,#43303,.F.) ;
#60560 = ORIENTED_EDGE('',*,*,#42645,.F.) ;
#60561 = ORIENTED_EDGE('',*,*,#43304,.T.) ;
#60562 = ORIENTED_EDGE('',*,*,#43222,.F.) ;
#60563 = ORIENTED_EDGE('',*,*,#43305,.F.) ;
#60564 = ORIENTED_EDGE('',*,*,#43303,.T.) ;
#60565 = ORIENTED_EDGE('',*,*,#42646,.F.) ;
#60566 = ORIENTED_EDGE('',*,*,#43306,.F.) ;
#60567 = ORIENTED_EDGE('',*,*,#42640,.F.) ;
#60568 = ORIENTED_EDGE('',*,*,#43302,.T.) ;
#60569 = ORIENTED_EDGE('',*,*,#42643,.F.) ;
#60570 = ORIENTED_EDGE('',*,*,#43307,.F.) ;
#60571 = ORIENTED_EDGE('',*,*,#43221,.F.) ;
#60572 = ORIENTED_EDGE('',*,*,#43306,.T.) ;
#60573 = ORIENTED_EDGE('',*,*,#43305,.T.) ;
#60574 = ORIENTED_EDGE('',*,*,#43308,.F.) ;
#60575 = ORIENTED_EDGE('',*,*,#43309,.F.) ;
#60576 = ORIENTED_EDGE('',*,*,#43307,.T.) ;
#60577 = ORIENTED_EDGE('',*,*,#43310,.F.) ;
#60578 = ORIENTED_EDGE('',*,*,#43308,.T.) ;
#60579 = ORIENTED_EDGE('',*,*,#43225,.F.) ;
#60580 = ORIENTED_EDGE('',*,*,#43311,.F.) ;
#60581 = ORIENTED_EDGE('',*,*,#42641,.F.) ;
#60582 = ORIENTED_EDGE('',*,*,#43310,.T.) ;
#60583 = ORIENTED_EDGE('',*,*,#42642,.F.) ;
#60584 = ORIENTED_EDGE('',*,*,#43312,.F.) ;
#60585 = ORIENTED_EDGE('',*,*,#42636,.F.) ;
#60586 = ORIENTED_EDGE('',*,*,#42639,.F.) ;
#60587 = ORIENTED_EDGE('',*,*,#43313,.T.) ;
#60588 = ORIENTED_EDGE('',*,*,#43218,.F.) ;
#60589 = ORIENTED_EDGE('',*,*,#43309,.T.) ;
#60590 = ORIENTED_EDGE('',*,*,#43312,.T.) ;
#60591 = ORIENTED_EDGE('',*,*,#43311,.T.) ;
#60592 = ORIENTED_EDGE('',*,*,#43314,.F.) ;
#60593 = ORIENTED_EDGE('',*,*,#42634,.F.) ;
#60594 = ORIENTED_EDGE('',*,*,#43315,.T.) ;
#60595 = ORIENTED_EDGE('',*,*,#42638,.F.) ;
#60596 = ORIENTED_EDGE('',*,*,#43316,.T.) ;
#60597 = ORIENTED_EDGE('',*,*,#43224,.F.) ;
#60598 = ORIENTED_EDGE('',*,*,#43317,.T.) ;
#60599 = ORIENTED_EDGE('',*,*,#42637,.F.) ;
#60600 = ORIENTED_EDGE('',*,*,#43314,.T.) ;
#60601 = ORIENTED_EDGE('',*,*,#43292,.F.) ;
#60602 = ORIENTED_EDGE('',*,*,#43318,.T.) ;
#60603 = ORIENTED_EDGE('',*,*,#42669,.F.) ;
#60604 = ORIENTED_EDGE('',*,*,#43319,.F.) ;
#60605 = ORIENTED_EDGE('',*,*,#42666,.F.) ;
#60606 = ORIENTED_EDGE('',*,*,#43320,.T.) ;
#60607 = ORIENTED_EDGE('',*,*,#42670,.F.) ;
#60608 = ORIENTED_EDGE('',*,*,#43321,.T.) ;
#60609 = ORIENTED_EDGE('',*,*,#43322,.F.) ;
#60610 = ORIENTED_EDGE('',*,*,#43319,.T.) ;
#60611 = ORIENTED_EDGE('',*,*,#43323,.F.) ;
#60612 = ORIENTED_EDGE('',*,*,#42667,.F.) ;
#60613 = ORIENTED_EDGE('',*,*,#43324,.T.) ;
#60614 = ORIENTED_EDGE('',*,*,#43294,.F.) ;
#60615 = ORIENTED_EDGE('',*,*,#43325,.F.) ;
#60616 = ORIENTED_EDGE('',*,*,#43323,.T.) ;
#60617 = ORIENTED_EDGE('',*,*,#42668,.F.) ;
#60618 = ORIENTED_EDGE('',*,*,#43326,.F.) ;
#60619 = ORIENTED_EDGE('',*,*,#42682,.F.) ;
#60620 = ORIENTED_EDGE('',*,*,#43322,.T.) ;
#60621 = ORIENTED_EDGE('',*,*,#42681,.F.) ;
#60622 = ORIENTED_EDGE('',*,*,#43327,.F.) ;
#60623 = ORIENTED_EDGE('',*,*,#43293,.F.) ;
#60624 = ORIENTED_EDGE('',*,*,#43326,.T.) ;
#60625 = ORIENTED_EDGE('',*,*,#43325,.T.) ;
#60626 = ORIENTED_EDGE('',*,*,#43328,.F.) ;
#60627 = ORIENTED_EDGE('',*,*,#43329,.F.) ;
#60628 = ORIENTED_EDGE('',*,*,#43327,.T.) ;
#60629 = ORIENTED_EDGE('',*,*,#43330,.F.) ;
#60630 = ORIENTED_EDGE('',*,*,#43328,.T.) ;
#60631 = ORIENTED_EDGE('',*,*,#43297,.F.) ;
#60632 = ORIENTED_EDGE('',*,*,#43331,.F.) ;
#60633 = ORIENTED_EDGE('',*,*,#42683,.F.) ;
#60634 = ORIENTED_EDGE('',*,*,#43330,.T.) ;
#60635 = ORIENTED_EDGE('',*,*,#42680,.F.) ;
#60636 = ORIENTED_EDGE('',*,*,#43332,.F.) ;
#60637 = ORIENTED_EDGE('',*,*,#42676,.F.) ;
#60638 = ORIENTED_EDGE('',*,*,#42679,.F.) ;
#60639 = ORIENTED_EDGE('',*,*,#43333,.T.) ;
#60640 = ORIENTED_EDGE('',*,*,#43290,.F.) ;
#60641 = ORIENTED_EDGE('',*,*,#43329,.T.) ;
#60642 = ORIENTED_EDGE('',*,*,#43332,.T.) ;
#60643 = ORIENTED_EDGE('',*,*,#43331,.T.) ;
#60644 = ORIENTED_EDGE('',*,*,#43334,.F.) ;
#60645 = ORIENTED_EDGE('',*,*,#42674,.F.) ;
#60646 = ORIENTED_EDGE('',*,*,#43335,.T.) ;
#60647 = ORIENTED_EDGE('',*,*,#42678,.F.) ;
#60648 = ORIENTED_EDGE('',*,*,#43336,.T.) ;
#60649 = ORIENTED_EDGE('',*,*,#43296,.F.) ;
#60650 = ORIENTED_EDGE('',*,*,#43337,.T.) ;
#60651 = ORIENTED_EDGE('',*,*,#42677,.F.) ;
#60652 = ORIENTED_EDGE('',*,*,#43334,.T.) ;
#60653 = ORIENTED_EDGE('',*,*,#43212,.F.) ;
#60654 = ORIENTED_EDGE('',*,*,#43338,.T.) ;
#60655 = ORIENTED_EDGE('',*,*,#42705,.F.) ;
#60656 = ORIENTED_EDGE('',*,*,#43339,.F.) ;
#60657 = ORIENTED_EDGE('',*,*,#42702,.F.) ;
#60658 = ORIENTED_EDGE('',*,*,#43340,.T.) ;
#60659 = ORIENTED_EDGE('',*,*,#42706,.F.) ;
#60660 = ORIENTED_EDGE('',*,*,#43341,.T.) ;
#60661 = ORIENTED_EDGE('',*,*,#43342,.F.) ;
#60662 = ORIENTED_EDGE('',*,*,#43339,.T.) ;
#60663 = ORIENTED_EDGE('',*,*,#43343,.F.) ;
#60664 = ORIENTED_EDGE('',*,*,#42703,.F.) ;
#60665 = ORIENTED_EDGE('',*,*,#43344,.T.) ;
#60666 = ORIENTED_EDGE('',*,*,#43214,.F.) ;
#60667 = ORIENTED_EDGE('',*,*,#43345,.F.) ;
#60668 = ORIENTED_EDGE('',*,*,#43343,.T.) ;
#60669 = ORIENTED_EDGE('',*,*,#42704,.F.) ;
#60670 = ORIENTED_EDGE('',*,*,#43346,.F.) ;
#60671 = ORIENTED_EDGE('',*,*,#42698,.F.) ;
#60672 = ORIENTED_EDGE('',*,*,#43342,.T.) ;
#60673 = ORIENTED_EDGE('',*,*,#42701,.F.) ;
#60674 = ORIENTED_EDGE('',*,*,#43347,.F.) ;
#60675 = ORIENTED_EDGE('',*,*,#43213,.F.) ;
#60676 = ORIENTED_EDGE('',*,*,#43346,.T.) ;
#60677 = ORIENTED_EDGE('',*,*,#43345,.T.) ;
#60678 = ORIENTED_EDGE('',*,*,#43348,.F.) ;
#60679 = ORIENTED_EDGE('',*,*,#43349,.F.) ;
#60680 = ORIENTED_EDGE('',*,*,#43347,.T.) ;
#60681 = ORIENTED_EDGE('',*,*,#43350,.F.) ;
#60682 = ORIENTED_EDGE('',*,*,#43348,.T.) ;
#60683 = ORIENTED_EDGE('',*,*,#43217,.F.) ;
#60684 = ORIENTED_EDGE('',*,*,#43351,.F.) ;
#60685 = ORIENTED_EDGE('',*,*,#42699,.F.) ;
#60686 = ORIENTED_EDGE('',*,*,#43350,.T.) ;
#60687 = ORIENTED_EDGE('',*,*,#42700,.F.) ;
#60688 = ORIENTED_EDGE('',*,*,#43352,.F.) ;
#60689 = ORIENTED_EDGE('',*,*,#42694,.F.) ;
#60690 = ORIENTED_EDGE('',*,*,#42697,.F.) ;
#60691 = ORIENTED_EDGE('',*,*,#43353,.T.) ;
#60692 = ORIENTED_EDGE('',*,*,#43210,.F.) ;
#60693 = ORIENTED_EDGE('',*,*,#43349,.T.) ;
#60694 = ORIENTED_EDGE('',*,*,#43352,.T.) ;
#60695 = ORIENTED_EDGE('',*,*,#43351,.T.) ;
#60696 = ORIENTED_EDGE('',*,*,#43354,.F.) ;
#60697 = ORIENTED_EDGE('',*,*,#42692,.F.) ;
#60698 = ORIENTED_EDGE('',*,*,#43355,.T.) ;
#60699 = ORIENTED_EDGE('',*,*,#42696,.F.) ;
#60700 = ORIENTED_EDGE('',*,*,#43356,.T.) ;
#60701 = ORIENTED_EDGE('',*,*,#43216,.F.) ;
#60702 = ORIENTED_EDGE('',*,*,#43357,.T.) ;
#60703 = ORIENTED_EDGE('',*,*,#42695,.F.) ;
#60704 = ORIENTED_EDGE('',*,*,#43354,.T.) ;
#60705 = ORIENTED_EDGE('',*,*,#43284,.F.) ;
#60706 = ORIENTED_EDGE('',*,*,#43358,.T.) ;
#60707 = ORIENTED_EDGE('',*,*,#42727,.F.) ;
#60708 = ORIENTED_EDGE('',*,*,#43359,.F.) ;
#60709 = ORIENTED_EDGE('',*,*,#42724,.F.) ;
#60710 = ORIENTED_EDGE('',*,*,#43360,.T.) ;
#60711 = ORIENTED_EDGE('',*,*,#42728,.F.) ;
#60712 = ORIENTED_EDGE('',*,*,#43361,.T.) ;
#60713 = ORIENTED_EDGE('',*,*,#43362,.F.) ;
#60714 = ORIENTED_EDGE('',*,*,#43359,.T.) ;
#60715 = ORIENTED_EDGE('',*,*,#43363,.F.) ;
#60716 = ORIENTED_EDGE('',*,*,#42725,.F.) ;
#60717 = ORIENTED_EDGE('',*,*,#43364,.T.) ;
#60718 = ORIENTED_EDGE('',*,*,#43286,.F.) ;
#60719 = ORIENTED_EDGE('',*,*,#43365,.F.) ;
#60720 = ORIENTED_EDGE('',*,*,#43363,.T.) ;
#60721 = ORIENTED_EDGE('',*,*,#42726,.F.) ;
#60722 = ORIENTED_EDGE('',*,*,#43366,.F.) ;
#60723 = ORIENTED_EDGE('',*,*,#42740,.F.) ;
#60724 = ORIENTED_EDGE('',*,*,#43362,.T.) ;
#60725 = ORIENTED_EDGE('',*,*,#42739,.F.) ;
#60726 = ORIENTED_EDGE('',*,*,#43367,.F.) ;
#60727 = ORIENTED_EDGE('',*,*,#43285,.F.) ;
#60728 = ORIENTED_EDGE('',*,*,#43366,.T.) ;
#60729 = ORIENTED_EDGE('',*,*,#43365,.T.) ;
#60730 = ORIENTED_EDGE('',*,*,#43368,.F.) ;
#60731 = ORIENTED_EDGE('',*,*,#43369,.F.) ;
#60732 = ORIENTED_EDGE('',*,*,#43367,.T.) ;
#60733 = ORIENTED_EDGE('',*,*,#43370,.F.) ;
#60734 = ORIENTED_EDGE('',*,*,#43368,.T.) ;
#60735 = ORIENTED_EDGE('',*,*,#43289,.F.) ;
#60736 = ORIENTED_EDGE('',*,*,#43371,.F.) ;
#60737 = ORIENTED_EDGE('',*,*,#42741,.F.) ;
#60738 = ORIENTED_EDGE('',*,*,#43370,.T.) ;
#60739 = ORIENTED_EDGE('',*,*,#42738,.F.) ;
#60740 = ORIENTED_EDGE('',*,*,#43372,.F.) ;
#60741 = ORIENTED_EDGE('',*,*,#42734,.F.) ;
#60742 = ORIENTED_EDGE('',*,*,#42737,.F.) ;
#60743 = ORIENTED_EDGE('',*,*,#43373,.T.) ;
#60744 = ORIENTED_EDGE('',*,*,#43282,.F.) ;
#60745 = ORIENTED_EDGE('',*,*,#43369,.T.) ;
#60746 = ORIENTED_EDGE('',*,*,#43372,.T.) ;
#60747 = ORIENTED_EDGE('',*,*,#43371,.T.) ;
#60748 = ORIENTED_EDGE('',*,*,#43374,.F.) ;
#60749 = ORIENTED_EDGE('',*,*,#42732,.F.) ;
#60750 = ORIENTED_EDGE('',*,*,#43375,.T.) ;
#60751 = ORIENTED_EDGE('',*,*,#42736,.F.) ;
#60752 = ORIENTED_EDGE('',*,*,#43376,.T.) ;
#60753 = ORIENTED_EDGE('',*,*,#43288,.F.) ;
#60754 = ORIENTED_EDGE('',*,*,#43377,.T.) ;
#60755 = ORIENTED_EDGE('',*,*,#42735,.F.) ;
#60756 = ORIENTED_EDGE('',*,*,#43374,.T.) ;
#60757 = ORIENTED_EDGE('',*,*,#43204,.F.) ;
#60758 = ORIENTED_EDGE('',*,*,#43378,.T.) ;
#60759 = ORIENTED_EDGE('',*,*,#42763,.F.) ;
#60760 = ORIENTED_EDGE('',*,*,#43379,.F.) ;
#60761 = ORIENTED_EDGE('',*,*,#42760,.F.) ;
#60762 = ORIENTED_EDGE('',*,*,#43380,.T.) ;
#60763 = ORIENTED_EDGE('',*,*,#42764,.F.) ;
#60764 = ORIENTED_EDGE('',*,*,#43381,.T.) ;
#60765 = ORIENTED_EDGE('',*,*,#43382,.F.) ;
#60766 = ORIENTED_EDGE('',*,*,#43379,.T.) ;
#60767 = ORIENTED_EDGE('',*,*,#43383,.F.) ;
#60768 = ORIENTED_EDGE('',*,*,#42761,.F.) ;
#60769 = ORIENTED_EDGE('',*,*,#43384,.T.) ;
#60770 = ORIENTED_EDGE('',*,*,#43206,.F.) ;
#60771 = ORIENTED_EDGE('',*,*,#43385,.F.) ;
#60772 = ORIENTED_EDGE('',*,*,#43383,.T.) ;
#60773 = ORIENTED_EDGE('',*,*,#42762,.F.) ;
#60774 = ORIENTED_EDGE('',*,*,#43386,.F.) ;
#60775 = ORIENTED_EDGE('',*,*,#42756,.F.) ;
#60776 = ORIENTED_EDGE('',*,*,#43382,.T.) ;
#60777 = ORIENTED_EDGE('',*,*,#42759,.F.) ;
#60778 = ORIENTED_EDGE('',*,*,#43387,.F.) ;
#60779 = ORIENTED_EDGE('',*,*,#43205,.F.) ;
#60780 = ORIENTED_EDGE('',*,*,#43386,.T.) ;
#60781 = ORIENTED_EDGE('',*,*,#43385,.T.) ;
#60782 = ORIENTED_EDGE('',*,*,#43388,.F.) ;
#60783 = ORIENTED_EDGE('',*,*,#43389,.F.) ;
#60784 = ORIENTED_EDGE('',*,*,#43387,.T.) ;
#60785 = ORIENTED_EDGE('',*,*,#43390,.F.) ;
#60786 = ORIENTED_EDGE('',*,*,#43388,.T.) ;
#60787 = ORIENTED_EDGE('',*,*,#43209,.F.) ;
#60788 = ORIENTED_EDGE('',*,*,#43391,.F.) ;
#60789 = ORIENTED_EDGE('',*,*,#42757,.F.) ;
#60790 = ORIENTED_EDGE('',*,*,#43390,.T.) ;
#60791 = ORIENTED_EDGE('',*,*,#42758,.F.) ;
#60792 = ORIENTED_EDGE('',*,*,#43392,.F.) ;
#60793 = ORIENTED_EDGE('',*,*,#42752,.F.) ;
#60794 = ORIENTED_EDGE('',*,*,#42755,.F.) ;
#60795 = ORIENTED_EDGE('',*,*,#43393,.T.) ;
#60796 = ORIENTED_EDGE('',*,*,#43202,.F.) ;
#60797 = ORIENTED_EDGE('',*,*,#43389,.T.) ;
#60798 = ORIENTED_EDGE('',*,*,#43392,.T.) ;
#60799 = ORIENTED_EDGE('',*,*,#43391,.T.) ;
#60800 = ORIENTED_EDGE('',*,*,#43394,.F.) ;
#60801 = ORIENTED_EDGE('',*,*,#42750,.F.) ;
#60802 = ORIENTED_EDGE('',*,*,#43395,.T.) ;
#60803 = ORIENTED_EDGE('',*,*,#42754,.F.) ;
#60804 = ORIENTED_EDGE('',*,*,#43396,.T.) ;
#60805 = ORIENTED_EDGE('',*,*,#43208,.F.) ;
#60806 = ORIENTED_EDGE('',*,*,#43397,.T.) ;
#60807 = ORIENTED_EDGE('',*,*,#42753,.F.) ;
#60808 = ORIENTED_EDGE('',*,*,#43394,.T.) ;
#60809 = ORIENTED_EDGE('',*,*,#43276,.F.) ;
#60810 = ORIENTED_EDGE('',*,*,#43398,.T.) ;
#60811 = ORIENTED_EDGE('',*,*,#42785,.F.) ;
#60812 = ORIENTED_EDGE('',*,*,#43399,.F.) ;
#60813 = ORIENTED_EDGE('',*,*,#42782,.F.) ;
#60814 = ORIENTED_EDGE('',*,*,#43400,.T.) ;
#60815 = ORIENTED_EDGE('',*,*,#42786,.F.) ;
#60816 = ORIENTED_EDGE('',*,*,#43401,.T.) ;
#60817 = ORIENTED_EDGE('',*,*,#43402,.F.) ;
#60818 = ORIENTED_EDGE('',*,*,#43399,.T.) ;
#60819 = ORIENTED_EDGE('',*,*,#43403,.F.) ;
#60820 = ORIENTED_EDGE('',*,*,#42783,.F.) ;
#60821 = ORIENTED_EDGE('',*,*,#43404,.T.) ;
#60822 = ORIENTED_EDGE('',*,*,#43278,.F.) ;
#60823 = ORIENTED_EDGE('',*,*,#43405,.F.) ;
#60824 = ORIENTED_EDGE('',*,*,#43403,.T.) ;
#60825 = ORIENTED_EDGE('',*,*,#42784,.F.) ;
#60826 = ORIENTED_EDGE('',*,*,#43406,.F.) ;
#60827 = ORIENTED_EDGE('',*,*,#42798,.F.) ;
#60828 = ORIENTED_EDGE('',*,*,#43402,.T.) ;
#60829 = ORIENTED_EDGE('',*,*,#42797,.F.) ;
#60830 = ORIENTED_EDGE('',*,*,#43407,.F.) ;
#60831 = ORIENTED_EDGE('',*,*,#43277,.F.) ;
#60832 = ORIENTED_EDGE('',*,*,#43406,.T.) ;
#60833 = ORIENTED_EDGE('',*,*,#43405,.T.) ;
#60834 = ORIENTED_EDGE('',*,*,#43408,.F.) ;
#60835 = ORIENTED_EDGE('',*,*,#43409,.F.) ;
#60836 = ORIENTED_EDGE('',*,*,#43407,.T.) ;
#60837 = ORIENTED_EDGE('',*,*,#43410,.F.) ;
#60838 = ORIENTED_EDGE('',*,*,#43408,.T.) ;
#60839 = ORIENTED_EDGE('',*,*,#43281,.F.) ;
#60840 = ORIENTED_EDGE('',*,*,#43411,.F.) ;
#60841 = ORIENTED_EDGE('',*,*,#42799,.F.) ;
#60842 = ORIENTED_EDGE('',*,*,#43410,.T.) ;
#60843 = ORIENTED_EDGE('',*,*,#42796,.F.) ;
#60844 = ORIENTED_EDGE('',*,*,#43412,.F.) ;
#60845 = ORIENTED_EDGE('',*,*,#42792,.F.) ;
#60846 = ORIENTED_EDGE('',*,*,#42795,.F.) ;
#60847 = ORIENTED_EDGE('',*,*,#43413,.T.) ;
#60848 = ORIENTED_EDGE('',*,*,#43274,.F.) ;
#60849 = ORIENTED_EDGE('',*,*,#43409,.T.) ;
#60850 = ORIENTED_EDGE('',*,*,#43412,.T.) ;
#60851 = ORIENTED_EDGE('',*,*,#43411,.T.) ;
#60852 = ORIENTED_EDGE('',*,*,#43414,.F.) ;
#60853 = ORIENTED_EDGE('',*,*,#42790,.F.) ;
#60854 = ORIENTED_EDGE('',*,*,#43415,.T.) ;
#60855 = ORIENTED_EDGE('',*,*,#42794,.F.) ;
#60856 = ORIENTED_EDGE('',*,*,#43416,.T.) ;
#60857 = ORIENTED_EDGE('',*,*,#43280,.F.) ;
#60858 = ORIENTED_EDGE('',*,*,#43417,.T.) ;
#60859 = ORIENTED_EDGE('',*,*,#42793,.F.) ;
#60860 = ORIENTED_EDGE('',*,*,#43414,.T.) ;
#60861 = ORIENTED_EDGE('',*,*,#43196,.F.) ;
#60862 = ORIENTED_EDGE('',*,*,#43418,.T.) ;
#60863 = ORIENTED_EDGE('',*,*,#42821,.F.) ;
#60864 = ORIENTED_EDGE('',*,*,#43419,.F.) ;
#60865 = ORIENTED_EDGE('',*,*,#42818,.F.) ;
#60866 = ORIENTED_EDGE('',*,*,#43420,.T.) ;
#60867 = ORIENTED_EDGE('',*,*,#42822,.F.) ;
#60868 = ORIENTED_EDGE('',*,*,#43421,.T.) ;
#60869 = ORIENTED_EDGE('',*,*,#43422,.F.) ;
#60870 = ORIENTED_EDGE('',*,*,#43419,.T.) ;
#60871 = ORIENTED_EDGE('',*,*,#43423,.F.) ;
#60872 = ORIENTED_EDGE('',*,*,#42819,.F.) ;
#60873 = ORIENTED_EDGE('',*,*,#43424,.T.) ;
#60874 = ORIENTED_EDGE('',*,*,#43198,.F.) ;
#60875 = ORIENTED_EDGE('',*,*,#43425,.F.) ;
#60876 = ORIENTED_EDGE('',*,*,#43423,.T.) ;
#60877 = ORIENTED_EDGE('',*,*,#42820,.F.) ;
#60878 = ORIENTED_EDGE('',*,*,#43426,.F.) ;
#60879 = ORIENTED_EDGE('',*,*,#42814,.F.) ;
#60880 = ORIENTED_EDGE('',*,*,#43422,.T.) ;
#60881 = ORIENTED_EDGE('',*,*,#42817,.F.) ;
#60882 = ORIENTED_EDGE('',*,*,#43427,.F.) ;
#60883 = ORIENTED_EDGE('',*,*,#43197,.F.) ;
#60884 = ORIENTED_EDGE('',*,*,#43426,.T.) ;
#60885 = ORIENTED_EDGE('',*,*,#43425,.T.) ;
#60886 = ORIENTED_EDGE('',*,*,#43428,.F.) ;
#60887 = ORIENTED_EDGE('',*,*,#43429,.F.) ;
#60888 = ORIENTED_EDGE('',*,*,#43427,.T.) ;
#60889 = ORIENTED_EDGE('',*,*,#43430,.F.) ;
#60890 = ORIENTED_EDGE('',*,*,#43428,.T.) ;
#60891 = ORIENTED_EDGE('',*,*,#43201,.F.) ;
#60892 = ORIENTED_EDGE('',*,*,#43431,.F.) ;
#60893 = ORIENTED_EDGE('',*,*,#42815,.F.) ;
#60894 = ORIENTED_EDGE('',*,*,#43430,.T.) ;
#60895 = ORIENTED_EDGE('',*,*,#42816,.F.) ;
#60896 = ORIENTED_EDGE('',*,*,#43432,.F.) ;
#60897 = ORIENTED_EDGE('',*,*,#42810,.F.) ;
#60898 = ORIENTED_EDGE('',*,*,#42813,.F.) ;
#60899 = ORIENTED_EDGE('',*,*,#43433,.T.) ;
#60900 = ORIENTED_EDGE('',*,*,#43194,.F.) ;
#60901 = ORIENTED_EDGE('',*,*,#43429,.T.) ;
#60902 = ORIENTED_EDGE('',*,*,#43432,.T.) ;
#60903 = ORIENTED_EDGE('',*,*,#43431,.T.) ;
#60904 = ORIENTED_EDGE('',*,*,#43434,.F.) ;
#60905 = ORIENTED_EDGE('',*,*,#42808,.F.) ;
#60906 = ORIENTED_EDGE('',*,*,#43435,.T.) ;
#60907 = ORIENTED_EDGE('',*,*,#42812,.F.) ;
#60908 = ORIENTED_EDGE('',*,*,#43436,.T.) ;
#60909 = ORIENTED_EDGE('',*,*,#43200,.F.) ;
#60910 = ORIENTED_EDGE('',*,*,#43437,.T.) ;
#60911 = ORIENTED_EDGE('',*,*,#42811,.F.) ;
#60912 = ORIENTED_EDGE('',*,*,#43434,.T.) ;
#60913 = ORIENTED_EDGE('',*,*,#43268,.F.) ;
#60914 = ORIENTED_EDGE('',*,*,#43438,.T.) ;
#60915 = ORIENTED_EDGE('',*,*,#42843,.F.) ;
#60916 = ORIENTED_EDGE('',*,*,#43439,.F.) ;
#60917 = ORIENTED_EDGE('',*,*,#42840,.F.) ;
#60918 = ORIENTED_EDGE('',*,*,#43440,.T.) ;
#60919 = ORIENTED_EDGE('',*,*,#42844,.F.) ;
#60920 = ORIENTED_EDGE('',*,*,#43441,.T.) ;
#60921 = ORIENTED_EDGE('',*,*,#43442,.F.) ;
#60922 = ORIENTED_EDGE('',*,*,#43439,.T.) ;
#60923 = ORIENTED_EDGE('',*,*,#43443,.F.) ;
#60924 = ORIENTED_EDGE('',*,*,#42841,.F.) ;
#60925 = ORIENTED_EDGE('',*,*,#43444,.T.) ;
#60926 = ORIENTED_EDGE('',*,*,#43270,.F.) ;
#60927 = ORIENTED_EDGE('',*,*,#43445,.F.) ;
#60928 = ORIENTED_EDGE('',*,*,#43443,.T.) ;
#60929 = ORIENTED_EDGE('',*,*,#42842,.F.) ;
#60930 = ORIENTED_EDGE('',*,*,#43446,.F.) ;
#60931 = ORIENTED_EDGE('',*,*,#42856,.F.) ;
#60932 = ORIENTED_EDGE('',*,*,#43442,.T.) ;
#60933 = ORIENTED_EDGE('',*,*,#42855,.F.) ;
#60934 = ORIENTED_EDGE('',*,*,#43447,.F.) ;
#60935 = ORIENTED_EDGE('',*,*,#43269,.F.) ;
#60936 = ORIENTED_EDGE('',*,*,#43446,.T.) ;
#60937 = ORIENTED_EDGE('',*,*,#43445,.T.) ;
#60938 = ORIENTED_EDGE('',*,*,#43448,.F.) ;
#60939 = ORIENTED_EDGE('',*,*,#43449,.F.) ;
#60940 = ORIENTED_EDGE('',*,*,#43447,.T.) ;
#60941 = ORIENTED_EDGE('',*,*,#43450,.F.) ;
#60942 = ORIENTED_EDGE('',*,*,#43448,.T.) ;
#60943 = ORIENTED_EDGE('',*,*,#43273,.F.) ;
#60944 = ORIENTED_EDGE('',*,*,#43451,.F.) ;
#60945 = ORIENTED_EDGE('',*,*,#42857,.F.) ;
#60946 = ORIENTED_EDGE('',*,*,#43450,.T.) ;
#60947 = ORIENTED_EDGE('',*,*,#42854,.F.) ;
#60948 = ORIENTED_EDGE('',*,*,#43452,.F.) ;
#60949 = ORIENTED_EDGE('',*,*,#42850,.F.) ;
#60950 = ORIENTED_EDGE('',*,*,#42853,.F.) ;
#60951 = ORIENTED_EDGE('',*,*,#43453,.T.) ;
#60952 = ORIENTED_EDGE('',*,*,#43266,.F.) ;
#60953 = ORIENTED_EDGE('',*,*,#43449,.T.) ;
#60954 = ORIENTED_EDGE('',*,*,#43452,.T.) ;
#60955 = ORIENTED_EDGE('',*,*,#43451,.T.) ;
#60956 = ORIENTED_EDGE('',*,*,#43454,.F.) ;
#60957 = ORIENTED_EDGE('',*,*,#42848,.F.) ;
#60958 = ORIENTED_EDGE('',*,*,#43455,.T.) ;
#60959 = ORIENTED_EDGE('',*,*,#42852,.F.) ;
#60960 = ORIENTED_EDGE('',*,*,#43456,.T.) ;
#60961 = ORIENTED_EDGE('',*,*,#43272,.F.) ;
#60962 = ORIENTED_EDGE('',*,*,#43457,.T.) ;
#60963 = ORIENTED_EDGE('',*,*,#42851,.F.) ;
#60964 = ORIENTED_EDGE('',*,*,#43454,.T.) ;
#60965 = ORIENTED_EDGE('',*,*,#43188,.F.) ;
#60966 = ORIENTED_EDGE('',*,*,#43458,.T.) ;
#60967 = ORIENTED_EDGE('',*,*,#42879,.F.) ;
#60968 = ORIENTED_EDGE('',*,*,#43459,.F.) ;
#60969 = ORIENTED_EDGE('',*,*,#42876,.F.) ;
#60970 = ORIENTED_EDGE('',*,*,#43460,.T.) ;
#60971 = ORIENTED_EDGE('',*,*,#42880,.F.) ;
#60972 = ORIENTED_EDGE('',*,*,#43461,.T.) ;
#60973 = ORIENTED_EDGE('',*,*,#43462,.F.) ;
#60974 = ORIENTED_EDGE('',*,*,#43459,.T.) ;
#60975 = ORIENTED_EDGE('',*,*,#43463,.F.) ;
#60976 = ORIENTED_EDGE('',*,*,#42877,.F.) ;
#60977 = ORIENTED_EDGE('',*,*,#43464,.T.) ;
#60978 = ORIENTED_EDGE('',*,*,#43190,.F.) ;
#60979 = ORIENTED_EDGE('',*,*,#43465,.F.) ;
#60980 = ORIENTED_EDGE('',*,*,#43463,.T.) ;
#60981 = ORIENTED_EDGE('',*,*,#42878,.F.) ;
#60982 = ORIENTED_EDGE('',*,*,#43466,.F.) ;
#60983 = ORIENTED_EDGE('',*,*,#42872,.F.) ;
#60984 = ORIENTED_EDGE('',*,*,#43462,.T.) ;
#60985 = ORIENTED_EDGE('',*,*,#42875,.F.) ;
#60986 = ORIENTED_EDGE('',*,*,#43467,.F.) ;
#60987 = ORIENTED_EDGE('',*,*,#43189,.F.) ;
#60988 = ORIENTED_EDGE('',*,*,#43466,.T.) ;
#60989 = ORIENTED_EDGE('',*,*,#43465,.T.) ;
#60990 = ORIENTED_EDGE('',*,*,#43468,.F.) ;
#60991 = ORIENTED_EDGE('',*,*,#43469,.F.) ;
#60992 = ORIENTED_EDGE('',*,*,#43467,.T.) ;
#60993 = ORIENTED_EDGE('',*,*,#43470,.F.) ;
#60994 = ORIENTED_EDGE('',*,*,#43468,.T.) ;
#60995 = ORIENTED_EDGE('',*,*,#43193,.F.) ;
#60996 = ORIENTED_EDGE('',*,*,#43471,.F.) ;
#60997 = ORIENTED_EDGE('',*,*,#42873,.F.) ;
#60998 = ORIENTED_EDGE('',*,*,#43470,.T.) ;
#60999 = ORIENTED_EDGE('',*,*,#42874,.F.) ;
#61000 = ORIENTED_EDGE('',*,*,#43472,.F.) ;
#61001 = ORIENTED_EDGE('',*,*,#42868,.F.) ;
#61002 = ORIENTED_EDGE('',*,*,#42871,.F.) ;
#61003 = ORIENTED_EDGE('',*,*,#43473,.T.) ;
#61004 = ORIENTED_EDGE('',*,*,#43186,.F.) ;
#61005 = ORIENTED_EDGE('',*,*,#43469,.T.) ;
#61006 = ORIENTED_EDGE('',*,*,#43472,.T.) ;
#61007 = ORIENTED_EDGE('',*,*,#43471,.T.) ;
#61008 = ORIENTED_EDGE('',*,*,#43474,.F.) ;
#61009 = ORIENTED_EDGE('',*,*,#42866,.F.) ;
#61010 = ORIENTED_EDGE('',*,*,#43475,.T.) ;
#61011 = ORIENTED_EDGE('',*,*,#42870,.F.) ;
#61012 = ORIENTED_EDGE('',*,*,#43476,.T.) ;
#61013 = ORIENTED_EDGE('',*,*,#43192,.F.) ;
#61014 = ORIENTED_EDGE('',*,*,#43477,.T.) ;
#61015 = ORIENTED_EDGE('',*,*,#42869,.F.) ;
#61016 = ORIENTED_EDGE('',*,*,#43474,.T.) ;
#61017 = ORIENTED_EDGE('',*,*,#43260,.F.) ;
#61018 = ORIENTED_EDGE('',*,*,#43478,.T.) ;
#61019 = ORIENTED_EDGE('',*,*,#42901,.F.) ;
#61020 = ORIENTED_EDGE('',*,*,#43479,.F.) ;
#61021 = ORIENTED_EDGE('',*,*,#42898,.F.) ;
#61022 = ORIENTED_EDGE('',*,*,#43480,.T.) ;
#61023 = ORIENTED_EDGE('',*,*,#42902,.F.) ;
#61024 = ORIENTED_EDGE('',*,*,#43481,.T.) ;
#61025 = ORIENTED_EDGE('',*,*,#43482,.F.) ;
#61026 = ORIENTED_EDGE('',*,*,#43479,.T.) ;
#61027 = ORIENTED_EDGE('',*,*,#43483,.F.) ;
#61028 = ORIENTED_EDGE('',*,*,#42899,.F.) ;
#61029 = ORIENTED_EDGE('',*,*,#43484,.T.) ;
#61030 = ORIENTED_EDGE('',*,*,#43262,.F.) ;
#61031 = ORIENTED_EDGE('',*,*,#43485,.F.) ;
#61032 = ORIENTED_EDGE('',*,*,#43483,.T.) ;
#61033 = ORIENTED_EDGE('',*,*,#42900,.F.) ;
#61034 = ORIENTED_EDGE('',*,*,#43486,.F.) ;
#61035 = ORIENTED_EDGE('',*,*,#42914,.F.) ;
#61036 = ORIENTED_EDGE('',*,*,#43482,.T.) ;
#61037 = ORIENTED_EDGE('',*,*,#42913,.F.) ;
#61038 = ORIENTED_EDGE('',*,*,#43487,.F.) ;
#61039 = ORIENTED_EDGE('',*,*,#43261,.F.) ;
#61040 = ORIENTED_EDGE('',*,*,#43486,.T.) ;
#61041 = ORIENTED_EDGE('',*,*,#43485,.T.) ;
#61042 = ORIENTED_EDGE('',*,*,#43488,.F.) ;
#61043 = ORIENTED_EDGE('',*,*,#43489,.F.) ;
#61044 = ORIENTED_EDGE('',*,*,#43487,.T.) ;
#61045 = ORIENTED_EDGE('',*,*,#43490,.F.) ;
#61046 = ORIENTED_EDGE('',*,*,#43488,.T.) ;
#61047 = ORIENTED_EDGE('',*,*,#43265,.F.) ;
#61048 = ORIENTED_EDGE('',*,*,#43491,.F.) ;
#61049 = ORIENTED_EDGE('',*,*,#42915,.F.) ;
#61050 = ORIENTED_EDGE('',*,*,#43490,.T.) ;
#61051 = ORIENTED_EDGE('',*,*,#42912,.F.) ;
#61052 = ORIENTED_EDGE('',*,*,#43492,.F.) ;
#61053 = ORIENTED_EDGE('',*,*,#42908,.F.) ;
#61054 = ORIENTED_EDGE('',*,*,#42911,.F.) ;
#61055 = ORIENTED_EDGE('',*,*,#43493,.T.) ;
#61056 = ORIENTED_EDGE('',*,*,#43258,.F.) ;
#61057 = ORIENTED_EDGE('',*,*,#43489,.T.) ;
#61058 = ORIENTED_EDGE('',*,*,#43492,.T.) ;
#61059 = ORIENTED_EDGE('',*,*,#43491,.T.) ;
#61060 = ORIENTED_EDGE('',*,*,#43494,.F.) ;
#61061 = ORIENTED_EDGE('',*,*,#42906,.F.) ;
#61062 = ORIENTED_EDGE('',*,*,#43495,.T.) ;
#61063 = ORIENTED_EDGE('',*,*,#42910,.F.) ;
#61064 = ORIENTED_EDGE('',*,*,#43496,.T.) ;
#61065 = ORIENTED_EDGE('',*,*,#43264,.F.) ;
#61066 = ORIENTED_EDGE('',*,*,#43497,.T.) ;
#61067 = ORIENTED_EDGE('',*,*,#42909,.F.) ;
#61068 = ORIENTED_EDGE('',*,*,#43494,.T.) ;
#61069 = ORIENTED_EDGE('',*,*,#43180,.F.) ;
#61070 = ORIENTED_EDGE('',*,*,#43498,.T.) ;
#61071 = ORIENTED_EDGE('',*,*,#42937,.F.) ;
#61072 = ORIENTED_EDGE('',*,*,#43499,.F.) ;
#61073 = ORIENTED_EDGE('',*,*,#42934,.F.) ;
#61074 = ORIENTED_EDGE('',*,*,#43500,.T.) ;
#61075 = ORIENTED_EDGE('',*,*,#42938,.F.) ;
#61076 = ORIENTED_EDGE('',*,*,#43501,.T.) ;
#61077 = ORIENTED_EDGE('',*,*,#43502,.F.) ;
#61078 = ORIENTED_EDGE('',*,*,#43499,.T.) ;
#61079 = ORIENTED_EDGE('',*,*,#43503,.F.) ;
#61080 = ORIENTED_EDGE('',*,*,#42935,.F.) ;
#61081 = ORIENTED_EDGE('',*,*,#43504,.T.) ;
#61082 = ORIENTED_EDGE('',*,*,#43182,.F.) ;
#61083 = ORIENTED_EDGE('',*,*,#43505,.F.) ;
#61084 = ORIENTED_EDGE('',*,*,#43503,.T.) ;
#61085 = ORIENTED_EDGE('',*,*,#42936,.F.) ;
#61086 = ORIENTED_EDGE('',*,*,#43506,.F.) ;
#61087 = ORIENTED_EDGE('',*,*,#42930,.F.) ;
#61088 = ORIENTED_EDGE('',*,*,#43502,.T.) ;
#61089 = ORIENTED_EDGE('',*,*,#42933,.F.) ;
#61090 = ORIENTED_EDGE('',*,*,#43507,.F.) ;
#61091 = ORIENTED_EDGE('',*,*,#43181,.F.) ;
#61092 = ORIENTED_EDGE('',*,*,#43506,.T.) ;
#61093 = ORIENTED_EDGE('',*,*,#43505,.T.) ;
#61094 = ORIENTED_EDGE('',*,*,#43508,.F.) ;
#61095 = ORIENTED_EDGE('',*,*,#43509,.F.) ;
#61096 = ORIENTED_EDGE('',*,*,#43507,.T.) ;
#61097 = ORIENTED_EDGE('',*,*,#43510,.F.) ;
#61098 = ORIENTED_EDGE('',*,*,#43508,.T.) ;
#61099 = ORIENTED_EDGE('',*,*,#43185,.F.) ;
#61100 = ORIENTED_EDGE('',*,*,#43511,.F.) ;
#61101 = ORIENTED_EDGE('',*,*,#42931,.F.) ;
#61102 = ORIENTED_EDGE('',*,*,#43510,.T.) ;
#61103 = ORIENTED_EDGE('',*,*,#42932,.F.) ;
#61104 = ORIENTED_EDGE('',*,*,#43512,.F.) ;
#61105 = ORIENTED_EDGE('',*,*,#42926,.F.) ;
#61106 = ORIENTED_EDGE('',*,*,#42929,.F.) ;
#61107 = ORIENTED_EDGE('',*,*,#43513,.T.) ;
#61108 = ORIENTED_EDGE('',*,*,#43178,.F.) ;
#61109 = ORIENTED_EDGE('',*,*,#43509,.T.) ;
#61110 = ORIENTED_EDGE('',*,*,#43512,.T.) ;
#61111 = ORIENTED_EDGE('',*,*,#43511,.T.) ;
#61112 = ORIENTED_EDGE('',*,*,#43514,.F.) ;
#61113 = ORIENTED_EDGE('',*,*,#42924,.F.) ;
#61114 = ORIENTED_EDGE('',*,*,#43515,.T.) ;
#61115 = ORIENTED_EDGE('',*,*,#42928,.F.) ;
#61116 = ORIENTED_EDGE('',*,*,#43516,.T.) ;
#61117 = ORIENTED_EDGE('',*,*,#43184,.F.) ;
#61118 = ORIENTED_EDGE('',*,*,#43517,.T.) ;
#61119 = ORIENTED_EDGE('',*,*,#42927,.F.) ;
#61120 = ORIENTED_EDGE('',*,*,#43514,.T.) ;
#61121 = ORIENTED_EDGE('',*,*,#43252,.F.) ;
#61122 = ORIENTED_EDGE('',*,*,#43518,.T.) ;
#61123 = ORIENTED_EDGE('',*,*,#42959,.F.) ;
#61124 = ORIENTED_EDGE('',*,*,#43519,.F.) ;
#61125 = ORIENTED_EDGE('',*,*,#42956,.F.) ;
#61126 = ORIENTED_EDGE('',*,*,#43520,.T.) ;
#61127 = ORIENTED_EDGE('',*,*,#42960,.F.) ;
#61128 = ORIENTED_EDGE('',*,*,#43521,.T.) ;
#61129 = ORIENTED_EDGE('',*,*,#43522,.F.) ;
#61130 = ORIENTED_EDGE('',*,*,#43519,.T.) ;
#61131 = ORIENTED_EDGE('',*,*,#43523,.F.) ;
#61132 = ORIENTED_EDGE('',*,*,#42957,.F.) ;
#61133 = ORIENTED_EDGE('',*,*,#43524,.T.) ;
#61134 = ORIENTED_EDGE('',*,*,#43254,.F.) ;
#61135 = ORIENTED_EDGE('',*,*,#43525,.F.) ;
#61136 = ORIENTED_EDGE('',*,*,#43523,.T.) ;
#61137 = ORIENTED_EDGE('',*,*,#42958,.F.) ;
#61138 = ORIENTED_EDGE('',*,*,#43526,.F.) ;
#61139 = ORIENTED_EDGE('',*,*,#42972,.F.) ;
#61140 = ORIENTED_EDGE('',*,*,#43522,.T.) ;
#61141 = ORIENTED_EDGE('',*,*,#42971,.F.) ;
#61142 = ORIENTED_EDGE('',*,*,#43527,.F.) ;
#61143 = ORIENTED_EDGE('',*,*,#43253,.F.) ;
#61144 = ORIENTED_EDGE('',*,*,#43526,.T.) ;
#61145 = ORIENTED_EDGE('',*,*,#43525,.T.) ;
#61146 = ORIENTED_EDGE('',*,*,#43528,.F.) ;
#61147 = ORIENTED_EDGE('',*,*,#43529,.F.) ;
#61148 = ORIENTED_EDGE('',*,*,#43527,.T.) ;
#61149 = ORIENTED_EDGE('',*,*,#43530,.F.) ;
#61150 = ORIENTED_EDGE('',*,*,#43528,.T.) ;
#61151 = ORIENTED_EDGE('',*,*,#43257,.F.) ;
#61152 = ORIENTED_EDGE('',*,*,#43531,.F.) ;
#61153 = ORIENTED_EDGE('',*,*,#42973,.F.) ;
#61154 = ORIENTED_EDGE('',*,*,#43530,.T.) ;
#61155 = ORIENTED_EDGE('',*,*,#42970,.F.) ;
#61156 = ORIENTED_EDGE('',*,*,#43532,.F.) ;
#61157 = ORIENTED_EDGE('',*,*,#42966,.F.) ;
#61158 = ORIENTED_EDGE('',*,*,#42969,.F.) ;
#61159 = ORIENTED_EDGE('',*,*,#43533,.T.) ;
#61160 = ORIENTED_EDGE('',*,*,#43250,.F.) ;
#61161 = ORIENTED_EDGE('',*,*,#43529,.T.) ;
#61162 = ORIENTED_EDGE('',*,*,#43532,.T.) ;
#61163 = ORIENTED_EDGE('',*,*,#43531,.T.) ;
#61164 = ORIENTED_EDGE('',*,*,#43534,.F.) ;
#61165 = ORIENTED_EDGE('',*,*,#42964,.F.) ;
#61166 = ORIENTED_EDGE('',*,*,#43535,.T.) ;
#61167 = ORIENTED_EDGE('',*,*,#42968,.F.) ;
#61168 = ORIENTED_EDGE('',*,*,#43536,.T.) ;
#61169 = ORIENTED_EDGE('',*,*,#43256,.F.) ;
#61170 = ORIENTED_EDGE('',*,*,#43537,.T.) ;
#61171 = ORIENTED_EDGE('',*,*,#42967,.F.) ;
#61172 = ORIENTED_EDGE('',*,*,#43534,.T.) ;
#61173 = ORIENTED_EDGE('',*,*,#43172,.F.) ;
#61174 = ORIENTED_EDGE('',*,*,#43538,.T.) ;
#61175 = ORIENTED_EDGE('',*,*,#42995,.F.) ;
#61176 = ORIENTED_EDGE('',*,*,#43539,.F.) ;
#61177 = ORIENTED_EDGE('',*,*,#42992,.F.) ;
#61178 = ORIENTED_EDGE('',*,*,#43540,.T.) ;
#61179 = ORIENTED_EDGE('',*,*,#42996,.F.) ;
#61180 = ORIENTED_EDGE('',*,*,#43541,.T.) ;
#61181 = ORIENTED_EDGE('',*,*,#43542,.F.) ;
#61182 = ORIENTED_EDGE('',*,*,#43539,.T.) ;
#61183 = ORIENTED_EDGE('',*,*,#43543,.F.) ;
#61184 = ORIENTED_EDGE('',*,*,#42993,.F.) ;
#61185 = ORIENTED_EDGE('',*,*,#43544,.T.) ;
#61186 = ORIENTED_EDGE('',*,*,#43174,.F.) ;
#61187 = ORIENTED_EDGE('',*,*,#43545,.F.) ;
#61188 = ORIENTED_EDGE('',*,*,#43543,.T.) ;
#61189 = ORIENTED_EDGE('',*,*,#42994,.F.) ;
#61190 = ORIENTED_EDGE('',*,*,#43546,.F.) ;
#61191 = ORIENTED_EDGE('',*,*,#42988,.F.) ;
#61192 = ORIENTED_EDGE('',*,*,#43542,.T.) ;
#61193 = ORIENTED_EDGE('',*,*,#42991,.F.) ;
#61194 = ORIENTED_EDGE('',*,*,#43547,.F.) ;
#61195 = ORIENTED_EDGE('',*,*,#43173,.F.) ;
#61196 = ORIENTED_EDGE('',*,*,#43546,.T.) ;
#61197 = ORIENTED_EDGE('',*,*,#43545,.T.) ;
#61198 = ORIENTED_EDGE('',*,*,#43548,.F.) ;
#61199 = ORIENTED_EDGE('',*,*,#43549,.F.) ;
#61200 = ORIENTED_EDGE('',*,*,#43547,.T.) ;
#61201 = ORIENTED_EDGE('',*,*,#43550,.F.) ;
#61202 = ORIENTED_EDGE('',*,*,#43548,.T.) ;
#61203 = ORIENTED_EDGE('',*,*,#43177,.F.) ;
#61204 = ORIENTED_EDGE('',*,*,#43551,.F.) ;
#61205 = ORIENTED_EDGE('',*,*,#42989,.F.) ;
#61206 = ORIENTED_EDGE('',*,*,#43550,.T.) ;
#61207 = ORIENTED_EDGE('',*,*,#42990,.F.) ;
#61208 = ORIENTED_EDGE('',*,*,#43552,.F.) ;
#61209 = ORIENTED_EDGE('',*,*,#42984,.F.) ;
#61210 = ORIENTED_EDGE('',*,*,#42987,.F.) ;
#61211 = ORIENTED_EDGE('',*,*,#43553,.T.) ;
#61212 = ORIENTED_EDGE('',*,*,#43170,.F.) ;
#61213 = ORIENTED_EDGE('',*,*,#43549,.T.) ;
#61214 = ORIENTED_EDGE('',*,*,#43552,.T.) ;
#61215 = ORIENTED_EDGE('',*,*,#43551,.T.) ;
#61216 = ORIENTED_EDGE('',*,*,#43554,.F.) ;
#61217 = ORIENTED_EDGE('',*,*,#42982,.F.) ;
#61218 = ORIENTED_EDGE('',*,*,#43555,.T.) ;
#61219 = ORIENTED_EDGE('',*,*,#42986,.F.) ;
#61220 = ORIENTED_EDGE('',*,*,#43556,.T.) ;
#61221 = ORIENTED_EDGE('',*,*,#43176,.F.) ;
#61222 = ORIENTED_EDGE('',*,*,#43557,.T.) ;
#61223 = ORIENTED_EDGE('',*,*,#42985,.F.) ;
#61224 = ORIENTED_EDGE('',*,*,#43554,.T.) ;
#61225 = ORIENTED_EDGE('',*,*,#43244,.F.) ;
#61226 = ORIENTED_EDGE('',*,*,#43558,.T.) ;
#61227 = ORIENTED_EDGE('',*,*,#43017,.F.) ;
#61228 = ORIENTED_EDGE('',*,*,#43559,.F.) ;
#61229 = ORIENTED_EDGE('',*,*,#43014,.F.) ;
#61230 = ORIENTED_EDGE('',*,*,#43560,.T.) ;
#61231 = ORIENTED_EDGE('',*,*,#43018,.F.) ;
#61232 = ORIENTED_EDGE('',*,*,#43561,.T.) ;
#61233 = ORIENTED_EDGE('',*,*,#43562,.F.) ;
#61234 = ORIENTED_EDGE('',*,*,#43559,.T.) ;
#61235 = ORIENTED_EDGE('',*,*,#43563,.F.) ;
#61236 = ORIENTED_EDGE('',*,*,#43015,.F.) ;
#61237 = ORIENTED_EDGE('',*,*,#43564,.T.) ;
#61238 = ORIENTED_EDGE('',*,*,#43246,.F.) ;
#61239 = ORIENTED_EDGE('',*,*,#43565,.F.) ;
#61240 = ORIENTED_EDGE('',*,*,#43563,.T.) ;
#61241 = ORIENTED_EDGE('',*,*,#43016,.F.) ;
#61242 = ORIENTED_EDGE('',*,*,#43566,.F.) ;
#61243 = ORIENTED_EDGE('',*,*,#43030,.F.) ;
#61244 = ORIENTED_EDGE('',*,*,#43562,.T.) ;
#61245 = ORIENTED_EDGE('',*,*,#43029,.F.) ;
#61246 = ORIENTED_EDGE('',*,*,#43567,.F.) ;
#61247 = ORIENTED_EDGE('',*,*,#43245,.F.) ;
#61248 = ORIENTED_EDGE('',*,*,#43566,.T.) ;
#61249 = ORIENTED_EDGE('',*,*,#43565,.T.) ;
#61250 = ORIENTED_EDGE('',*,*,#43568,.F.) ;
#61251 = ORIENTED_EDGE('',*,*,#43569,.F.) ;
#61252 = ORIENTED_EDGE('',*,*,#43567,.T.) ;
#61253 = ORIENTED_EDGE('',*,*,#43570,.F.) ;
#61254 = ORIENTED_EDGE('',*,*,#43568,.T.) ;
#61255 = ORIENTED_EDGE('',*,*,#43249,.F.) ;
#61256 = ORIENTED_EDGE('',*,*,#43571,.F.) ;
#61257 = ORIENTED_EDGE('',*,*,#43031,.F.) ;
#61258 = ORIENTED_EDGE('',*,*,#43570,.T.) ;
#61259 = ORIENTED_EDGE('',*,*,#43028,.F.) ;
#61260 = ORIENTED_EDGE('',*,*,#43572,.F.) ;
#61261 = ORIENTED_EDGE('',*,*,#43024,.F.) ;
#61262 = ORIENTED_EDGE('',*,*,#43027,.F.) ;
#61263 = ORIENTED_EDGE('',*,*,#43573,.T.) ;
#61264 = ORIENTED_EDGE('',*,*,#43242,.F.) ;
#61265 = ORIENTED_EDGE('',*,*,#43569,.T.) ;
#61266 = ORIENTED_EDGE('',*,*,#43572,.T.) ;
#61267 = ORIENTED_EDGE('',*,*,#43571,.T.) ;
#61268 = ORIENTED_EDGE('',*,*,#43574,.F.) ;
#61269 = ORIENTED_EDGE('',*,*,#43022,.F.) ;
#61270 = ORIENTED_EDGE('',*,*,#43575,.T.) ;
#61271 = ORIENTED_EDGE('',*,*,#43026,.F.) ;
#61272 = ORIENTED_EDGE('',*,*,#43576,.T.) ;
#61273 = ORIENTED_EDGE('',*,*,#43248,.F.) ;
#61274 = ORIENTED_EDGE('',*,*,#43577,.T.) ;
#61275 = ORIENTED_EDGE('',*,*,#43025,.F.) ;
#61276 = ORIENTED_EDGE('',*,*,#43574,.T.) ;
#61277 = ORIENTED_EDGE('',*,*,#43164,.F.) ;
#61278 = ORIENTED_EDGE('',*,*,#43578,.T.) ;
#61279 = ORIENTED_EDGE('',*,*,#43053,.F.) ;
#61280 = ORIENTED_EDGE('',*,*,#43579,.F.) ;
#61281 = ORIENTED_EDGE('',*,*,#43050,.F.) ;
#61282 = ORIENTED_EDGE('',*,*,#43580,.T.) ;
#61283 = ORIENTED_EDGE('',*,*,#43054,.F.) ;
#61284 = ORIENTED_EDGE('',*,*,#43581,.T.) ;
#61285 = ORIENTED_EDGE('',*,*,#43582,.F.) ;
#61286 = ORIENTED_EDGE('',*,*,#43579,.T.) ;
#61287 = ORIENTED_EDGE('',*,*,#43583,.F.) ;
#61288 = ORIENTED_EDGE('',*,*,#43051,.F.) ;
#61289 = ORIENTED_EDGE('',*,*,#43584,.T.) ;
#61290 = ORIENTED_EDGE('',*,*,#43166,.F.) ;
#61291 = ORIENTED_EDGE('',*,*,#43585,.F.) ;
#61292 = ORIENTED_EDGE('',*,*,#43583,.T.) ;
#61293 = ORIENTED_EDGE('',*,*,#43052,.F.) ;
#61294 = ORIENTED_EDGE('',*,*,#43586,.F.) ;
#61295 = ORIENTED_EDGE('',*,*,#43046,.F.) ;
#61296 = ORIENTED_EDGE('',*,*,#43582,.T.) ;
#61297 = ORIENTED_EDGE('',*,*,#43049,.F.) ;
#61298 = ORIENTED_EDGE('',*,*,#43587,.F.) ;
#61299 = ORIENTED_EDGE('',*,*,#43165,.F.) ;
#61300 = ORIENTED_EDGE('',*,*,#43586,.T.) ;
#61301 = ORIENTED_EDGE('',*,*,#43585,.T.) ;
#61302 = ORIENTED_EDGE('',*,*,#43588,.F.) ;
#61303 = ORIENTED_EDGE('',*,*,#43589,.F.) ;
#61304 = ORIENTED_EDGE('',*,*,#43587,.T.) ;
#61305 = ORIENTED_EDGE('',*,*,#43590,.F.) ;
#61306 = ORIENTED_EDGE('',*,*,#43588,.T.) ;
#61307 = ORIENTED_EDGE('',*,*,#43169,.F.) ;
#61308 = ORIENTED_EDGE('',*,*,#43591,.F.) ;
#61309 = ORIENTED_EDGE('',*,*,#43047,.F.) ;
#61310 = ORIENTED_EDGE('',*,*,#43590,.T.) ;
#61311 = ORIENTED_EDGE('',*,*,#43048,.F.) ;
#61312 = ORIENTED_EDGE('',*,*,#43592,.F.) ;
#61313 = ORIENTED_EDGE('',*,*,#43042,.F.) ;
#61314 = ORIENTED_EDGE('',*,*,#43045,.F.) ;
#61315 = ORIENTED_EDGE('',*,*,#43593,.T.) ;
#61316 = ORIENTED_EDGE('',*,*,#43162,.F.) ;
#61317 = ORIENTED_EDGE('',*,*,#43589,.T.) ;
#61318 = ORIENTED_EDGE('',*,*,#43592,.T.) ;
#61319 = ORIENTED_EDGE('',*,*,#43591,.T.) ;
#61320 = ORIENTED_EDGE('',*,*,#43594,.F.) ;
#61321 = ORIENTED_EDGE('',*,*,#43040,.F.) ;
#61322 = ORIENTED_EDGE('',*,*,#43595,.T.) ;
#61323 = ORIENTED_EDGE('',*,*,#43044,.F.) ;
#61324 = ORIENTED_EDGE('',*,*,#43596,.T.) ;
#61325 = ORIENTED_EDGE('',*,*,#43168,.F.) ;
#61326 = ORIENTED_EDGE('',*,*,#43597,.T.) ;
#61327 = ORIENTED_EDGE('',*,*,#43043,.F.) ;
#61328 = ORIENTED_EDGE('',*,*,#43594,.T.) ;
#61329 = ORIENTED_EDGE('',*,*,#43236,.F.) ;
#61330 = ORIENTED_EDGE('',*,*,#43598,.T.) ;
#61331 = ORIENTED_EDGE('',*,*,#43075,.F.) ;
#61332 = ORIENTED_EDGE('',*,*,#43599,.F.) ;
#61333 = ORIENTED_EDGE('',*,*,#43072,.F.) ;
#61334 = ORIENTED_EDGE('',*,*,#43600,.T.) ;
#61335 = ORIENTED_EDGE('',*,*,#43076,.F.) ;
#61336 = ORIENTED_EDGE('',*,*,#43601,.T.) ;
#61337 = ORIENTED_EDGE('',*,*,#43602,.F.) ;
#61338 = ORIENTED_EDGE('',*,*,#43599,.T.) ;
#61339 = ORIENTED_EDGE('',*,*,#43603,.F.) ;
#61340 = ORIENTED_EDGE('',*,*,#43073,.F.) ;
#61341 = ORIENTED_EDGE('',*,*,#43604,.T.) ;
#61342 = ORIENTED_EDGE('',*,*,#43238,.F.) ;
#61343 = ORIENTED_EDGE('',*,*,#43605,.F.) ;
#61344 = ORIENTED_EDGE('',*,*,#43603,.T.) ;
#61345 = ORIENTED_EDGE('',*,*,#43074,.F.) ;
#61346 = ORIENTED_EDGE('',*,*,#43606,.F.) ;
#61347 = ORIENTED_EDGE('',*,*,#43088,.F.) ;
#61348 = ORIENTED_EDGE('',*,*,#43602,.T.) ;
#61349 = ORIENTED_EDGE('',*,*,#43087,.F.) ;
#61350 = ORIENTED_EDGE('',*,*,#43607,.F.) ;
#61351 = ORIENTED_EDGE('',*,*,#43237,.F.) ;
#61352 = ORIENTED_EDGE('',*,*,#43606,.T.) ;
#61353 = ORIENTED_EDGE('',*,*,#43605,.T.) ;
#61354 = ORIENTED_EDGE('',*,*,#43608,.F.) ;
#61355 = ORIENTED_EDGE('',*,*,#43609,.F.) ;
#61356 = ORIENTED_EDGE('',*,*,#43607,.T.) ;
#61357 = ORIENTED_EDGE('',*,*,#43610,.F.) ;
#61358 = ORIENTED_EDGE('',*,*,#43608,.T.) ;
#61359 = ORIENTED_EDGE('',*,*,#43241,.F.) ;
#61360 = ORIENTED_EDGE('',*,*,#43611,.F.) ;
#61361 = ORIENTED_EDGE('',*,*,#43089,.F.) ;
#61362 = ORIENTED_EDGE('',*,*,#43610,.T.) ;
#61363 = ORIENTED_EDGE('',*,*,#43086,.F.) ;
#61364 = ORIENTED_EDGE('',*,*,#43612,.F.) ;
#61365 = ORIENTED_EDGE('',*,*,#43082,.F.) ;
#61366 = ORIENTED_EDGE('',*,*,#43085,.F.) ;
#61367 = ORIENTED_EDGE('',*,*,#43613,.T.) ;
#61368 = ORIENTED_EDGE('',*,*,#43234,.F.) ;
#61369 = ORIENTED_EDGE('',*,*,#43609,.T.) ;
#61370 = ORIENTED_EDGE('',*,*,#43612,.T.) ;
#61371 = ORIENTED_EDGE('',*,*,#43611,.T.) ;
#61372 = ORIENTED_EDGE('',*,*,#43614,.F.) ;
#61373 = ORIENTED_EDGE('',*,*,#43080,.F.) ;
#61374 = ORIENTED_EDGE('',*,*,#43615,.T.) ;
#61375 = ORIENTED_EDGE('',*,*,#43084,.F.) ;
#61376 = ORIENTED_EDGE('',*,*,#43616,.T.) ;
#61377 = ORIENTED_EDGE('',*,*,#43240,.F.) ;
#61378 = ORIENTED_EDGE('',*,*,#43617,.T.) ;
#61379 = ORIENTED_EDGE('',*,*,#43083,.F.) ;
#61380 = ORIENTED_EDGE('',*,*,#43614,.T.) ;
#61381 = ORIENTED_EDGE('',*,*,#43156,.F.) ;
#61382 = ORIENTED_EDGE('',*,*,#43618,.T.) ;
#61383 = ORIENTED_EDGE('',*,*,#43111,.F.) ;
#61384 = ORIENTED_EDGE('',*,*,#43619,.F.) ;
#61385 = ORIENTED_EDGE('',*,*,#43108,.F.) ;
#61386 = ORIENTED_EDGE('',*,*,#43620,.T.) ;
#61387 = ORIENTED_EDGE('',*,*,#43112,.F.) ;
#61388 = ORIENTED_EDGE('',*,*,#43621,.T.) ;
#61389 = ORIENTED_EDGE('',*,*,#43622,.F.) ;
#61390 = ORIENTED_EDGE('',*,*,#43619,.T.) ;
#61391 = ORIENTED_EDGE('',*,*,#43623,.F.) ;
#61392 = ORIENTED_EDGE('',*,*,#43109,.F.) ;
#61393 = ORIENTED_EDGE('',*,*,#43624,.T.) ;
#61394 = ORIENTED_EDGE('',*,*,#43158,.F.) ;
#61395 = ORIENTED_EDGE('',*,*,#43625,.F.) ;
#61396 = ORIENTED_EDGE('',*,*,#43623,.T.) ;
#61397 = ORIENTED_EDGE('',*,*,#43110,.F.) ;
#61398 = ORIENTED_EDGE('',*,*,#43626,.F.) ;
#61399 = ORIENTED_EDGE('',*,*,#43104,.F.) ;
#61400 = ORIENTED_EDGE('',*,*,#43622,.T.) ;
#61401 = ORIENTED_EDGE('',*,*,#43107,.F.) ;
#61402 = ORIENTED_EDGE('',*,*,#43627,.F.) ;
#61403 = ORIENTED_EDGE('',*,*,#43157,.F.) ;
#61404 = ORIENTED_EDGE('',*,*,#43626,.T.) ;
#61405 = ORIENTED_EDGE('',*,*,#43625,.T.) ;
#61406 = ORIENTED_EDGE('',*,*,#43628,.F.) ;
#61407 = ORIENTED_EDGE('',*,*,#43629,.F.) ;
#61408 = ORIENTED_EDGE('',*,*,#43627,.T.) ;
#61409 = ORIENTED_EDGE('',*,*,#43630,.F.) ;
#61410 = ORIENTED_EDGE('',*,*,#43628,.T.) ;
#61411 = ORIENTED_EDGE('',*,*,#43161,.F.) ;
#61412 = ORIENTED_EDGE('',*,*,#43631,.F.) ;
#61413 = ORIENTED_EDGE('',*,*,#43105,.F.) ;
#61414 = ORIENTED_EDGE('',*,*,#43630,.T.) ;
#61415 = ORIENTED_EDGE('',*,*,#43106,.F.) ;
#61416 = ORIENTED_EDGE('',*,*,#43632,.F.) ;
#61417 = ORIENTED_EDGE('',*,*,#43100,.F.) ;
#61418 = ORIENTED_EDGE('',*,*,#43103,.F.) ;
#61419 = ORIENTED_EDGE('',*,*,#43633,.T.) ;
#61420 = ORIENTED_EDGE('',*,*,#43154,.F.) ;
#61421 = ORIENTED_EDGE('',*,*,#43629,.T.) ;
#61422 = ORIENTED_EDGE('',*,*,#43632,.T.) ;
#61423 = ORIENTED_EDGE('',*,*,#43631,.T.) ;
#61424 = ORIENTED_EDGE('',*,*,#43634,.F.) ;
#61425 = ORIENTED_EDGE('',*,*,#43098,.F.) ;
#61426 = ORIENTED_EDGE('',*,*,#43635,.T.) ;
#61427 = ORIENTED_EDGE('',*,*,#43102,.F.) ;
#61428 = ORIENTED_EDGE('',*,*,#43636,.T.) ;
#61429 = ORIENTED_EDGE('',*,*,#43160,.F.) ;
#61430 = ORIENTED_EDGE('',*,*,#43637,.T.) ;
#61431 = ORIENTED_EDGE('',*,*,#43101,.F.) ;
#61432 = ORIENTED_EDGE('',*,*,#43634,.T.) ;
#61433 = ORIENTED_EDGE('',*,*,#43228,.F.) ;
#61434 = ORIENTED_EDGE('',*,*,#43638,.T.) ;
#61435 = ORIENTED_EDGE('',*,*,#43133,.F.) ;
#61436 = ORIENTED_EDGE('',*,*,#43639,.F.) ;
#61437 = ORIENTED_EDGE('',*,*,#43130,.F.) ;
#61438 = ORIENTED_EDGE('',*,*,#43640,.T.) ;
#61439 = ORIENTED_EDGE('',*,*,#43134,.F.) ;
#61440 = ORIENTED_EDGE('',*,*,#43641,.T.) ;
#61441 = ORIENTED_EDGE('',*,*,#43642,.F.) ;
#61442 = ORIENTED_EDGE('',*,*,#43639,.T.) ;
#61443 = ORIENTED_EDGE('',*,*,#43643,.F.) ;
#61444 = ORIENTED_EDGE('',*,*,#43131,.F.) ;
#61445 = ORIENTED_EDGE('',*,*,#43644,.T.) ;
#61446 = ORIENTED_EDGE('',*,*,#43230,.F.) ;
#61447 = ORIENTED_EDGE('',*,*,#43645,.F.) ;
#61448 = ORIENTED_EDGE('',*,*,#43643,.T.) ;
#61449 = ORIENTED_EDGE('',*,*,#43132,.F.) ;
#61450 = ORIENTED_EDGE('',*,*,#43646,.F.) ;
#61451 = ORIENTED_EDGE('',*,*,#43146,.F.) ;
#61452 = ORIENTED_EDGE('',*,*,#43642,.T.) ;
#61453 = ORIENTED_EDGE('',*,*,#43145,.F.) ;
#61454 = ORIENTED_EDGE('',*,*,#43647,.F.) ;
#61455 = ORIENTED_EDGE('',*,*,#43229,.F.) ;
#61456 = ORIENTED_EDGE('',*,*,#43646,.T.) ;
#61457 = ORIENTED_EDGE('',*,*,#43645,.T.) ;
#61458 = ORIENTED_EDGE('',*,*,#43648,.F.) ;
#61459 = ORIENTED_EDGE('',*,*,#43649,.F.) ;
#61460 = ORIENTED_EDGE('',*,*,#43647,.T.) ;
#61461 = ORIENTED_EDGE('',*,*,#43650,.F.) ;
#61462 = ORIENTED_EDGE('',*,*,#43648,.T.) ;
#61463 = ORIENTED_EDGE('',*,*,#43233,.F.) ;
#61464 = ORIENTED_EDGE('',*,*,#43651,.F.) ;
#61465 = ORIENTED_EDGE('',*,*,#43147,.F.) ;
#61466 = ORIENTED_EDGE('',*,*,#43650,.T.) ;
#61467 = ORIENTED_EDGE('',*,*,#43144,.F.) ;
#61468 = ORIENTED_EDGE('',*,*,#43652,.F.) ;
#61469 = ORIENTED_EDGE('',*,*,#43140,.F.) ;
#61470 = ORIENTED_EDGE('',*,*,#43143,.F.) ;
#61471 = ORIENTED_EDGE('',*,*,#43653,.T.) ;
#61472 = ORIENTED_EDGE('',*,*,#43226,.F.) ;
#61473 = ORIENTED_EDGE('',*,*,#43649,.T.) ;
#61474 = ORIENTED_EDGE('',*,*,#43652,.T.) ;
#61475 = ORIENTED_EDGE('',*,*,#43651,.T.) ;
#61476 = ORIENTED_EDGE('',*,*,#43654,.F.) ;
#61477 = ORIENTED_EDGE('',*,*,#43138,.F.) ;
#61478 = ORIENTED_EDGE('',*,*,#43655,.T.) ;
#61479 = ORIENTED_EDGE('',*,*,#43142,.F.) ;
#61480 = ORIENTED_EDGE('',*,*,#43656,.T.) ;
#61481 = ORIENTED_EDGE('',*,*,#43232,.F.) ;
#61482 = ORIENTED_EDGE('',*,*,#43657,.T.) ;
#61483 = ORIENTED_EDGE('',*,*,#43141,.F.) ;
#61484 = ORIENTED_EDGE('',*,*,#43654,.T.) ;
#61485 = ORIENTED_EDGE('',*,*,#39429,.F.) ;
#61486 = ORIENTED_EDGE('',*,*,#42664,.F.) ;
#61487 = ORIENTED_EDGE('',*,*,#43658,.F.) ;
#61488 = ORIENTED_EDGE('',*,*,#42659,.F.) ;
#61489 = ORIENTED_EDGE('',*,*,#43658,.T.) ;
#61490 = ORIENTED_EDGE('',*,*,#42649,.F.) ;
#61491 = ORIENTED_EDGE('',*,*,#43659,.F.) ;
#61492 = ORIENTED_EDGE('',*,*,#42660,.F.) ;
#61493 = ORIENTED_EDGE('',*,*,#43659,.T.) ;
#61494 = ORIENTED_EDGE('',*,*,#43300,.F.) ;
#61495 = ORIENTED_EDGE('',*,*,#43298,.F.) ;
#61496 = ORIENTED_EDGE('',*,*,#43660,.F.) ;
#61497 = ORIENTED_EDGE('',*,*,#43660,.T.) ;
#61498 = ORIENTED_EDGE('',*,*,#43219,.F.) ;
#61499 = ORIENTED_EDGE('',*,*,#43661,.F.) ;
#61500 = ORIENTED_EDGE('',*,*,#42661,.F.) ;
#61501 = ORIENTED_EDGE('',*,*,#43661,.T.) ;
#61502 = ORIENTED_EDGE('',*,*,#43313,.F.) ;
#61503 = ORIENTED_EDGE('',*,*,#43315,.F.) ;
#61504 = ORIENTED_EDGE('',*,*,#43662,.F.) ;
#61505 = ORIENTED_EDGE('',*,*,#43662,.T.) ;
#61506 = ORIENTED_EDGE('',*,*,#42633,.F.) ;
#61507 = ORIENTED_EDGE('',*,*,#43663,.F.) ;
#61508 = ORIENTED_EDGE('',*,*,#42657,.F.) ;
#61509 = ORIENTED_EDGE('',*,*,#39276,.F.) ;
#61510 = ORIENTED_EDGE('',*,*,#42658,.F.) ;
#61511 = ORIENTED_EDGE('',*,*,#43663,.T.) ;
#61512 = ORIENTED_EDGE('',*,*,#42662,.F.) ;
#61513 = ORIENTED_EDGE('',*,*,#41616,.F.) ;
#61514 = ORIENTED_EDGE('',*,*,#41619,.F.) ;
#61515 = ORIENTED_EDGE('',*,*,#42663,.F.) ;
#61516 = ORIENTED_EDGE('',*,*,#43664,.F.) ;
#61517 = ORIENTED_EDGE('',*,*,#42654,.F.) ;
#61518 = ORIENTED_EDGE('',*,*,#43664,.T.) ;
#61519 = ORIENTED_EDGE('',*,*,#42635,.F.) ;
#61520 = ORIENTED_EDGE('',*,*,#43665,.F.) ;
#61521 = ORIENTED_EDGE('',*,*,#42655,.F.) ;
#61522 = ORIENTED_EDGE('',*,*,#43665,.T.) ;
#61523 = ORIENTED_EDGE('',*,*,#43316,.F.) ;
#61524 = ORIENTED_EDGE('',*,*,#43317,.F.) ;
#61525 = ORIENTED_EDGE('',*,*,#43666,.F.) ;
#61526 = ORIENTED_EDGE('',*,*,#43666,.T.) ;
#61527 = ORIENTED_EDGE('',*,*,#43223,.F.) ;
#61528 = ORIENTED_EDGE('',*,*,#43667,.F.) ;
#61529 = ORIENTED_EDGE('',*,*,#42656,.F.) ;
#61530 = ORIENTED_EDGE('',*,*,#43667,.T.) ;
#61531 = ORIENTED_EDGE('',*,*,#43304,.F.) ;
#61532 = ORIENTED_EDGE('',*,*,#43301,.F.) ;
#61533 = ORIENTED_EDGE('',*,*,#43668,.F.) ;
#61534 = ORIENTED_EDGE('',*,*,#43668,.T.) ;
#61535 = ORIENTED_EDGE('',*,*,#42651,.F.) ;
#61536 = ORIENTED_EDGE('',*,*,#43669,.F.) ;
#61537 = ORIENTED_EDGE('',*,*,#42652,.F.) ;
#61538 = ORIENTED_EDGE('',*,*,#43669,.T.) ;
#61539 = ORIENTED_EDGE('',*,*,#42665,.F.) ;
#61540 = ORIENTED_EDGE('',*,*,#39427,.F.) ;
#61541 = ORIENTED_EDGE('',*,*,#42653,.F.) ;
#61542 = ORIENTED_EDGE('',*,*,#41537,.F.) ;
#61543 = ORIENTED_EDGE('',*,*,#42671,.F.) ;
#61544 = ORIENTED_EDGE('',*,*,#43670,.F.) ;
#61545 = ORIENTED_EDGE('',*,*,#42687,.F.) ;
#61546 = ORIENTED_EDGE('',*,*,#43670,.T.) ;
#61547 = ORIENTED_EDGE('',*,*,#43320,.F.) ;
#61548 = ORIENTED_EDGE('',*,*,#43318,.F.) ;
#61549 = ORIENTED_EDGE('',*,*,#43671,.F.) ;
#61550 = ORIENTED_EDGE('',*,*,#43671,.T.) ;
#61551 = ORIENTED_EDGE('',*,*,#43291,.F.) ;
#61552 = ORIENTED_EDGE('',*,*,#43672,.F.) ;
#61553 = ORIENTED_EDGE('',*,*,#42688,.F.) ;
#61554 = ORIENTED_EDGE('',*,*,#43672,.T.) ;
#61555 = ORIENTED_EDGE('',*,*,#43333,.F.) ;
#61556 = ORIENTED_EDGE('',*,*,#43335,.F.) ;
#61557 = ORIENTED_EDGE('',*,*,#43673,.F.) ;
#61558 = ORIENTED_EDGE('',*,*,#41539,.F.) ;
#61559 = ORIENTED_EDGE('',*,*,#42689,.F.) ;
#61560 = ORIENTED_EDGE('',*,*,#43673,.T.) ;
#61561 = ORIENTED_EDGE('',*,*,#42673,.F.) ;
#61562 = ORIENTED_EDGE('',*,*,#43674,.F.) ;
#61563 = ORIENTED_EDGE('',*,*,#42672,.F.) ;
#61564 = ORIENTED_EDGE('',*,*,#41535,.F.) ;
#61565 = ORIENTED_EDGE('',*,*,#42685,.F.) ;
#61566 = ORIENTED_EDGE('',*,*,#43321,.F.) ;
#61567 = ORIENTED_EDGE('',*,*,#43674,.T.) ;
#61568 = ORIENTED_EDGE('',*,*,#43675,.F.) ;
#61569 = ORIENTED_EDGE('',*,*,#43324,.F.) ;
#61570 = ORIENTED_EDGE('',*,*,#43675,.T.) ;
#61571 = ORIENTED_EDGE('',*,*,#42684,.F.) ;
#61572 = ORIENTED_EDGE('',*,*,#43676,.F.) ;
#61573 = ORIENTED_EDGE('',*,*,#43295,.F.) ;
#61574 = ORIENTED_EDGE('',*,*,#41541,.F.) ;
#61575 = ORIENTED_EDGE('',*,*,#42675,.F.) ;
#61576 = ORIENTED_EDGE('',*,*,#43677,.F.) ;
#61577 = ORIENTED_EDGE('',*,*,#42686,.F.) ;
#61578 = ORIENTED_EDGE('',*,*,#43337,.F.) ;
#61579 = ORIENTED_EDGE('',*,*,#43676,.T.) ;
#61580 = ORIENTED_EDGE('',*,*,#43677,.T.) ;
#61581 = ORIENTED_EDGE('',*,*,#43336,.F.) ;
#61582 = ORIENTED_EDGE('',*,*,#39418,.F.) ;
#61583 = ORIENTED_EDGE('',*,*,#42722,.F.) ;
#61584 = ORIENTED_EDGE('',*,*,#43678,.F.) ;
#61585 = ORIENTED_EDGE('',*,*,#42717,.F.) ;
#61586 = ORIENTED_EDGE('',*,*,#43678,.T.) ;
#61587 = ORIENTED_EDGE('',*,*,#42707,.F.) ;
#61588 = ORIENTED_EDGE('',*,*,#43679,.F.) ;
#61589 = ORIENTED_EDGE('',*,*,#42718,.F.) ;
#61590 = ORIENTED_EDGE('',*,*,#43679,.T.) ;
#61591 = ORIENTED_EDGE('',*,*,#43340,.F.) ;
#61592 = ORIENTED_EDGE('',*,*,#43338,.F.) ;
#61593 = ORIENTED_EDGE('',*,*,#43680,.F.) ;
#61594 = ORIENTED_EDGE('',*,*,#43680,.T.) ;
#61595 = ORIENTED_EDGE('',*,*,#43211,.F.) ;
#61596 = ORIENTED_EDGE('',*,*,#43681,.F.) ;
#61597 = ORIENTED_EDGE('',*,*,#42719,.F.) ;
#61598 = ORIENTED_EDGE('',*,*,#43681,.T.) ;
#61599 = ORIENTED_EDGE('',*,*,#43353,.F.) ;
#61600 = ORIENTED_EDGE('',*,*,#43355,.F.) ;
#61601 = ORIENTED_EDGE('',*,*,#43682,.F.) ;
#61602 = ORIENTED_EDGE('',*,*,#43682,.T.) ;
#61603 = ORIENTED_EDGE('',*,*,#42691,.F.) ;
#61604 = ORIENTED_EDGE('',*,*,#43683,.F.) ;
#61605 = ORIENTED_EDGE('',*,*,#42715,.F.) ;
#61606 = ORIENTED_EDGE('',*,*,#39223,.F.) ;
#61607 = ORIENTED_EDGE('',*,*,#42716,.F.) ;
#61608 = ORIENTED_EDGE('',*,*,#43683,.T.) ;
#61609 = ORIENTED_EDGE('',*,*,#42720,.F.) ;
#61610 = ORIENTED_EDGE('',*,*,#41938,.F.) ;
#61611 = ORIENTED_EDGE('',*,*,#41941,.F.) ;
#61612 = ORIENTED_EDGE('',*,*,#42721,.F.) ;
#61613 = ORIENTED_EDGE('',*,*,#43684,.F.) ;
#61614 = ORIENTED_EDGE('',*,*,#42712,.F.) ;
#61615 = ORIENTED_EDGE('',*,*,#43684,.T.) ;
#61616 = ORIENTED_EDGE('',*,*,#42693,.F.) ;
#61617 = ORIENTED_EDGE('',*,*,#43685,.F.) ;
#61618 = ORIENTED_EDGE('',*,*,#42713,.F.) ;
#61619 = ORIENTED_EDGE('',*,*,#43685,.T.) ;
#61620 = ORIENTED_EDGE('',*,*,#43356,.F.) ;
#61621 = ORIENTED_EDGE('',*,*,#43357,.F.) ;
#61622 = ORIENTED_EDGE('',*,*,#43686,.F.) ;
#61623 = ORIENTED_EDGE('',*,*,#43686,.T.) ;
#61624 = ORIENTED_EDGE('',*,*,#43215,.F.) ;
#61625 = ORIENTED_EDGE('',*,*,#43687,.F.) ;
#61626 = ORIENTED_EDGE('',*,*,#42714,.F.) ;
#61627 = ORIENTED_EDGE('',*,*,#43687,.T.) ;
#61628 = ORIENTED_EDGE('',*,*,#43344,.F.) ;
#61629 = ORIENTED_EDGE('',*,*,#43341,.F.) ;
#61630 = ORIENTED_EDGE('',*,*,#43688,.F.) ;
#61631 = ORIENTED_EDGE('',*,*,#43688,.T.) ;
#61632 = ORIENTED_EDGE('',*,*,#42709,.F.) ;
#61633 = ORIENTED_EDGE('',*,*,#43689,.F.) ;
#61634 = ORIENTED_EDGE('',*,*,#42710,.F.) ;
#61635 = ORIENTED_EDGE('',*,*,#43689,.T.) ;
#61636 = ORIENTED_EDGE('',*,*,#42723,.F.) ;
#61637 = ORIENTED_EDGE('',*,*,#39416,.F.) ;
#61638 = ORIENTED_EDGE('',*,*,#42711,.F.) ;
#61639 = ORIENTED_EDGE('',*,*,#41545,.F.) ;
#61640 = ORIENTED_EDGE('',*,*,#42729,.F.) ;
#61641 = ORIENTED_EDGE('',*,*,#43690,.F.) ;
#61642 = ORIENTED_EDGE('',*,*,#42745,.F.) ;
#61643 = ORIENTED_EDGE('',*,*,#43690,.T.) ;
#61644 = ORIENTED_EDGE('',*,*,#43360,.F.) ;
#61645 = ORIENTED_EDGE('',*,*,#43358,.F.) ;
#61646 = ORIENTED_EDGE('',*,*,#43691,.F.) ;
#61647 = ORIENTED_EDGE('',*,*,#43691,.T.) ;
#61648 = ORIENTED_EDGE('',*,*,#43283,.F.) ;
#61649 = ORIENTED_EDGE('',*,*,#43692,.F.) ;
#61650 = ORIENTED_EDGE('',*,*,#42746,.F.) ;
#61651 = ORIENTED_EDGE('',*,*,#43692,.T.) ;
#61652 = ORIENTED_EDGE('',*,*,#43373,.F.) ;
#61653 = ORIENTED_EDGE('',*,*,#43375,.F.) ;
#61654 = ORIENTED_EDGE('',*,*,#43693,.F.) ;
#61655 = ORIENTED_EDGE('',*,*,#41547,.F.) ;
#61656 = ORIENTED_EDGE('',*,*,#42747,.F.) ;
#61657 = ORIENTED_EDGE('',*,*,#43693,.T.) ;
#61658 = ORIENTED_EDGE('',*,*,#42731,.F.) ;
#61659 = ORIENTED_EDGE('',*,*,#43694,.F.) ;
#61660 = ORIENTED_EDGE('',*,*,#42730,.F.) ;
#61661 = ORIENTED_EDGE('',*,*,#41543,.F.) ;
#61662 = ORIENTED_EDGE('',*,*,#42743,.F.) ;
#61663 = ORIENTED_EDGE('',*,*,#43361,.F.) ;
#61664 = ORIENTED_EDGE('',*,*,#43694,.T.) ;
#61665 = ORIENTED_EDGE('',*,*,#43695,.F.) ;
#61666 = ORIENTED_EDGE('',*,*,#43364,.F.) ;
#61667 = ORIENTED_EDGE('',*,*,#43695,.T.) ;
#61668 = ORIENTED_EDGE('',*,*,#42742,.F.) ;
#61669 = ORIENTED_EDGE('',*,*,#43696,.F.) ;
#61670 = ORIENTED_EDGE('',*,*,#43287,.F.) ;
#61671 = ORIENTED_EDGE('',*,*,#41549,.F.) ;
#61672 = ORIENTED_EDGE('',*,*,#42733,.F.) ;
#61673 = ORIENTED_EDGE('',*,*,#43697,.F.) ;
#61674 = ORIENTED_EDGE('',*,*,#42744,.F.) ;
#61675 = ORIENTED_EDGE('',*,*,#43377,.F.) ;
#61676 = ORIENTED_EDGE('',*,*,#43696,.T.) ;
#61677 = ORIENTED_EDGE('',*,*,#43697,.T.) ;
#61678 = ORIENTED_EDGE('',*,*,#43376,.F.) ;
#61679 = ORIENTED_EDGE('',*,*,#39407,.F.) ;
#61680 = ORIENTED_EDGE('',*,*,#42780,.F.) ;
#61681 = ORIENTED_EDGE('',*,*,#43698,.F.) ;
#61682 = ORIENTED_EDGE('',*,*,#42775,.F.) ;
#61683 = ORIENTED_EDGE('',*,*,#43698,.T.) ;
#61684 = ORIENTED_EDGE('',*,*,#42765,.F.) ;
#61685 = ORIENTED_EDGE('',*,*,#43699,.F.) ;
#61686 = ORIENTED_EDGE('',*,*,#42776,.F.) ;
#61687 = ORIENTED_EDGE('',*,*,#43699,.T.) ;
#61688 = ORIENTED_EDGE('',*,*,#43380,.F.) ;
#61689 = ORIENTED_EDGE('',*,*,#43378,.F.) ;
#61690 = ORIENTED_EDGE('',*,*,#43700,.F.) ;
#61691 = ORIENTED_EDGE('',*,*,#43700,.T.) ;
#61692 = ORIENTED_EDGE('',*,*,#43203,.F.) ;
#61693 = ORIENTED_EDGE('',*,*,#43701,.F.) ;
#61694 = ORIENTED_EDGE('',*,*,#42777,.F.) ;
#61695 = ORIENTED_EDGE('',*,*,#43701,.T.) ;
#61696 = ORIENTED_EDGE('',*,*,#43393,.F.) ;
#61697 = ORIENTED_EDGE('',*,*,#43395,.F.) ;
#61698 = ORIENTED_EDGE('',*,*,#43702,.F.) ;
#61699 = ORIENTED_EDGE('',*,*,#43702,.T.) ;
#61700 = ORIENTED_EDGE('',*,*,#42749,.F.) ;
#61701 = ORIENTED_EDGE('',*,*,#43703,.F.) ;
#61702 = ORIENTED_EDGE('',*,*,#42773,.F.) ;
#61703 = ORIENTED_EDGE('',*,*,#39206,.F.) ;
#61704 = ORIENTED_EDGE('',*,*,#42774,.F.) ;
#61705 = ORIENTED_EDGE('',*,*,#43703,.T.) ;
#61706 = ORIENTED_EDGE('',*,*,#42778,.F.) ;
#61707 = ORIENTED_EDGE('',*,*,#42026,.F.) ;
#61708 = ORIENTED_EDGE('',*,*,#42029,.F.) ;
#61709 = ORIENTED_EDGE('',*,*,#42779,.F.) ;
#61710 = ORIENTED_EDGE('',*,*,#43704,.F.) ;
#61711 = ORIENTED_EDGE('',*,*,#42770,.F.) ;
#61712 = ORIENTED_EDGE('',*,*,#43704,.T.) ;
#61713 = ORIENTED_EDGE('',*,*,#42751,.F.) ;
#61714 = ORIENTED_EDGE('',*,*,#43705,.F.) ;
#61715 = ORIENTED_EDGE('',*,*,#42771,.F.) ;
#61716 = ORIENTED_EDGE('',*,*,#43705,.T.) ;
#61717 = ORIENTED_EDGE('',*,*,#43396,.F.) ;
#61718 = ORIENTED_EDGE('',*,*,#43397,.F.) ;
#61719 = ORIENTED_EDGE('',*,*,#43706,.F.) ;
#61720 = ORIENTED_EDGE('',*,*,#43706,.T.) ;
#61721 = ORIENTED_EDGE('',*,*,#43207,.F.) ;
#61722 = ORIENTED_EDGE('',*,*,#43707,.F.) ;
#61723 = ORIENTED_EDGE('',*,*,#42772,.F.) ;
#61724 = ORIENTED_EDGE('',*,*,#43707,.T.) ;
#61725 = ORIENTED_EDGE('',*,*,#43384,.F.) ;
#61726 = ORIENTED_EDGE('',*,*,#43381,.F.) ;
#61727 = ORIENTED_EDGE('',*,*,#43708,.F.) ;
#61728 = ORIENTED_EDGE('',*,*,#43708,.T.) ;
#61729 = ORIENTED_EDGE('',*,*,#42767,.F.) ;
#61730 = ORIENTED_EDGE('',*,*,#43709,.F.) ;
#61731 = ORIENTED_EDGE('',*,*,#42768,.F.) ;
#61732 = ORIENTED_EDGE('',*,*,#43709,.T.) ;
#61733 = ORIENTED_EDGE('',*,*,#42781,.F.) ;
#61734 = ORIENTED_EDGE('',*,*,#39405,.F.) ;
#61735 = ORIENTED_EDGE('',*,*,#42769,.F.) ;
#61736 = ORIENTED_EDGE('',*,*,#41553,.F.) ;
#61737 = ORIENTED_EDGE('',*,*,#42787,.F.) ;
#61738 = ORIENTED_EDGE('',*,*,#43710,.F.) ;
#61739 = ORIENTED_EDGE('',*,*,#42803,.F.) ;
#61740 = ORIENTED_EDGE('',*,*,#43710,.T.) ;
#61741 = ORIENTED_EDGE('',*,*,#43400,.F.) ;
#61742 = ORIENTED_EDGE('',*,*,#43398,.F.) ;
#61743 = ORIENTED_EDGE('',*,*,#43711,.F.) ;
#61744 = ORIENTED_EDGE('',*,*,#43711,.T.) ;
#61745 = ORIENTED_EDGE('',*,*,#43275,.F.) ;
#61746 = ORIENTED_EDGE('',*,*,#43712,.F.) ;
#61747 = ORIENTED_EDGE('',*,*,#42804,.F.) ;
#61748 = ORIENTED_EDGE('',*,*,#43712,.T.) ;
#61749 = ORIENTED_EDGE('',*,*,#43413,.F.) ;
#61750 = ORIENTED_EDGE('',*,*,#43415,.F.) ;
#61751 = ORIENTED_EDGE('',*,*,#43713,.F.) ;
#61752 = ORIENTED_EDGE('',*,*,#41555,.F.) ;
#61753 = ORIENTED_EDGE('',*,*,#42805,.F.) ;
#61754 = ORIENTED_EDGE('',*,*,#43713,.T.) ;
#61755 = ORIENTED_EDGE('',*,*,#42789,.F.) ;
#61756 = ORIENTED_EDGE('',*,*,#43714,.F.) ;
#61757 = ORIENTED_EDGE('',*,*,#42788,.F.) ;
#61758 = ORIENTED_EDGE('',*,*,#41551,.F.) ;
#61759 = ORIENTED_EDGE('',*,*,#42801,.F.) ;
#61760 = ORIENTED_EDGE('',*,*,#43401,.F.) ;
#61761 = ORIENTED_EDGE('',*,*,#43714,.T.) ;
#61762 = ORIENTED_EDGE('',*,*,#43715,.F.) ;
#61763 = ORIENTED_EDGE('',*,*,#43404,.F.) ;
#61764 = ORIENTED_EDGE('',*,*,#43715,.T.) ;
#61765 = ORIENTED_EDGE('',*,*,#42800,.F.) ;
#61766 = ORIENTED_EDGE('',*,*,#43716,.F.) ;
#61767 = ORIENTED_EDGE('',*,*,#43279,.F.) ;
#61768 = ORIENTED_EDGE('',*,*,#41557,.F.) ;
#61769 = ORIENTED_EDGE('',*,*,#42791,.F.) ;
#61770 = ORIENTED_EDGE('',*,*,#43717,.F.) ;
#61771 = ORIENTED_EDGE('',*,*,#42802,.F.) ;
#61772 = ORIENTED_EDGE('',*,*,#43417,.F.) ;
#61773 = ORIENTED_EDGE('',*,*,#43716,.T.) ;
#61774 = ORIENTED_EDGE('',*,*,#43717,.T.) ;
#61775 = ORIENTED_EDGE('',*,*,#43416,.F.) ;
#61776 = ORIENTED_EDGE('',*,*,#39396,.F.) ;
#61777 = ORIENTED_EDGE('',*,*,#42838,.F.) ;
#61778 = ORIENTED_EDGE('',*,*,#43718,.F.) ;
#61779 = ORIENTED_EDGE('',*,*,#42833,.F.) ;
#61780 = ORIENTED_EDGE('',*,*,#43718,.T.) ;
#61781 = ORIENTED_EDGE('',*,*,#42823,.F.) ;
#61782 = ORIENTED_EDGE('',*,*,#43719,.F.) ;
#61783 = ORIENTED_EDGE('',*,*,#42834,.F.) ;
#61784 = ORIENTED_EDGE('',*,*,#43719,.T.) ;
#61785 = ORIENTED_EDGE('',*,*,#43420,.F.) ;
#61786 = ORIENTED_EDGE('',*,*,#43418,.F.) ;
#61787 = ORIENTED_EDGE('',*,*,#43720,.F.) ;
#61788 = ORIENTED_EDGE('',*,*,#43720,.T.) ;
#61789 = ORIENTED_EDGE('',*,*,#43195,.F.) ;
#61790 = ORIENTED_EDGE('',*,*,#43721,.F.) ;
#61791 = ORIENTED_EDGE('',*,*,#42835,.F.) ;
#61792 = ORIENTED_EDGE('',*,*,#43721,.T.) ;
#61793 = ORIENTED_EDGE('',*,*,#43433,.F.) ;
#61794 = ORIENTED_EDGE('',*,*,#43435,.F.) ;
#61795 = ORIENTED_EDGE('',*,*,#43722,.F.) ;
#61796 = ORIENTED_EDGE('',*,*,#43722,.T.) ;
#61797 = ORIENTED_EDGE('',*,*,#42807,.F.) ;
#61798 = ORIENTED_EDGE('',*,*,#43723,.F.) ;
#61799 = ORIENTED_EDGE('',*,*,#42831,.F.) ;
#61800 = ORIENTED_EDGE('',*,*,#39189,.F.) ;
#61801 = ORIENTED_EDGE('',*,*,#42832,.F.) ;
#61802 = ORIENTED_EDGE('',*,*,#43723,.T.) ;
#61803 = ORIENTED_EDGE('',*,*,#42836,.F.) ;
#61804 = ORIENTED_EDGE('',*,*,#42114,.F.) ;
#61805 = ORIENTED_EDGE('',*,*,#42117,.F.) ;
#61806 = ORIENTED_EDGE('',*,*,#42837,.F.) ;
#61807 = ORIENTED_EDGE('',*,*,#43724,.F.) ;
#61808 = ORIENTED_EDGE('',*,*,#42828,.F.) ;
#61809 = ORIENTED_EDGE('',*,*,#43724,.T.) ;
#61810 = ORIENTED_EDGE('',*,*,#42809,.F.) ;
#61811 = ORIENTED_EDGE('',*,*,#43725,.F.) ;
#61812 = ORIENTED_EDGE('',*,*,#42829,.F.) ;
#61813 = ORIENTED_EDGE('',*,*,#43725,.T.) ;
#61814 = ORIENTED_EDGE('',*,*,#43436,.F.) ;
#61815 = ORIENTED_EDGE('',*,*,#43437,.F.) ;
#61816 = ORIENTED_EDGE('',*,*,#43726,.F.) ;
#61817 = ORIENTED_EDGE('',*,*,#43726,.T.) ;
#61818 = ORIENTED_EDGE('',*,*,#43199,.F.) ;
#61819 = ORIENTED_EDGE('',*,*,#43727,.F.) ;
#61820 = ORIENTED_EDGE('',*,*,#42830,.F.) ;
#61821 = ORIENTED_EDGE('',*,*,#43727,.T.) ;
#61822 = ORIENTED_EDGE('',*,*,#43424,.F.) ;
#61823 = ORIENTED_EDGE('',*,*,#43421,.F.) ;
#61824 = ORIENTED_EDGE('',*,*,#43728,.F.) ;
#61825 = ORIENTED_EDGE('',*,*,#43728,.T.) ;
#61826 = ORIENTED_EDGE('',*,*,#42825,.F.) ;
#61827 = ORIENTED_EDGE('',*,*,#43729,.F.) ;
#61828 = ORIENTED_EDGE('',*,*,#42826,.F.) ;
#61829 = ORIENTED_EDGE('',*,*,#43729,.T.) ;
#61830 = ORIENTED_EDGE('',*,*,#42839,.F.) ;
#61831 = ORIENTED_EDGE('',*,*,#39394,.F.) ;
#61832 = ORIENTED_EDGE('',*,*,#42827,.F.) ;
#61833 = ORIENTED_EDGE('',*,*,#41561,.F.) ;
#61834 = ORIENTED_EDGE('',*,*,#42845,.F.) ;
#61835 = ORIENTED_EDGE('',*,*,#43730,.F.) ;
#61836 = ORIENTED_EDGE('',*,*,#42861,.F.) ;
#61837 = ORIENTED_EDGE('',*,*,#43730,.T.) ;
#61838 = ORIENTED_EDGE('',*,*,#43440,.F.) ;
#61839 = ORIENTED_EDGE('',*,*,#43438,.F.) ;
#61840 = ORIENTED_EDGE('',*,*,#43731,.F.) ;
#61841 = ORIENTED_EDGE('',*,*,#43731,.T.) ;
#61842 = ORIENTED_EDGE('',*,*,#43267,.F.) ;
#61843 = ORIENTED_EDGE('',*,*,#43732,.F.) ;
#61844 = ORIENTED_EDGE('',*,*,#42862,.F.) ;
#61845 = ORIENTED_EDGE('',*,*,#43732,.T.) ;
#61846 = ORIENTED_EDGE('',*,*,#43453,.F.) ;
#61847 = ORIENTED_EDGE('',*,*,#43455,.F.) ;
#61848 = ORIENTED_EDGE('',*,*,#43733,.F.) ;
#61849 = ORIENTED_EDGE('',*,*,#41563,.F.) ;
#61850 = ORIENTED_EDGE('',*,*,#42863,.F.) ;
#61851 = ORIENTED_EDGE('',*,*,#43733,.T.) ;
#61852 = ORIENTED_EDGE('',*,*,#42847,.F.) ;
#61853 = ORIENTED_EDGE('',*,*,#43734,.F.) ;
#61854 = ORIENTED_EDGE('',*,*,#42846,.F.) ;
#61855 = ORIENTED_EDGE('',*,*,#41559,.F.) ;
#61856 = ORIENTED_EDGE('',*,*,#42859,.F.) ;
#61857 = ORIENTED_EDGE('',*,*,#43441,.F.) ;
#61858 = ORIENTED_EDGE('',*,*,#43734,.T.) ;
#61859 = ORIENTED_EDGE('',*,*,#43735,.F.) ;
#61860 = ORIENTED_EDGE('',*,*,#43444,.F.) ;
#61861 = ORIENTED_EDGE('',*,*,#43735,.T.) ;
#61862 = ORIENTED_EDGE('',*,*,#42858,.F.) ;
#61863 = ORIENTED_EDGE('',*,*,#43736,.F.) ;
#61864 = ORIENTED_EDGE('',*,*,#43271,.F.) ;
#61865 = ORIENTED_EDGE('',*,*,#41565,.F.) ;
#61866 = ORIENTED_EDGE('',*,*,#42849,.F.) ;
#61867 = ORIENTED_EDGE('',*,*,#43737,.F.) ;
#61868 = ORIENTED_EDGE('',*,*,#42860,.F.) ;
#61869 = ORIENTED_EDGE('',*,*,#43457,.F.) ;
#61870 = ORIENTED_EDGE('',*,*,#43736,.T.) ;
#61871 = ORIENTED_EDGE('',*,*,#43737,.T.) ;
#61872 = ORIENTED_EDGE('',*,*,#43456,.F.) ;
#61873 = ORIENTED_EDGE('',*,*,#39385,.F.) ;
#61874 = ORIENTED_EDGE('',*,*,#42896,.F.) ;
#61875 = ORIENTED_EDGE('',*,*,#43738,.F.) ;
#61876 = ORIENTED_EDGE('',*,*,#42891,.F.) ;
#61877 = ORIENTED_EDGE('',*,*,#43738,.T.) ;
#61878 = ORIENTED_EDGE('',*,*,#42881,.F.) ;
#61879 = ORIENTED_EDGE('',*,*,#43739,.F.) ;
#61880 = ORIENTED_EDGE('',*,*,#42892,.F.) ;
#61881 = ORIENTED_EDGE('',*,*,#43739,.T.) ;
#61882 = ORIENTED_EDGE('',*,*,#43460,.F.) ;
#61883 = ORIENTED_EDGE('',*,*,#43458,.F.) ;
#61884 = ORIENTED_EDGE('',*,*,#43740,.F.) ;
#61885 = ORIENTED_EDGE('',*,*,#43740,.T.) ;
#61886 = ORIENTED_EDGE('',*,*,#43187,.F.) ;
#61887 = ORIENTED_EDGE('',*,*,#43741,.F.) ;
#61888 = ORIENTED_EDGE('',*,*,#42893,.F.) ;
#61889 = ORIENTED_EDGE('',*,*,#43741,.T.) ;
#61890 = ORIENTED_EDGE('',*,*,#43473,.F.) ;
#61891 = ORIENTED_EDGE('',*,*,#43475,.F.) ;
#61892 = ORIENTED_EDGE('',*,*,#43742,.F.) ;
#61893 = ORIENTED_EDGE('',*,*,#43742,.T.) ;
#61894 = ORIENTED_EDGE('',*,*,#42865,.F.) ;
#61895 = ORIENTED_EDGE('',*,*,#43743,.F.) ;
#61896 = ORIENTED_EDGE('',*,*,#42889,.F.) ;
#61897 = ORIENTED_EDGE('',*,*,#39172,.F.) ;
#61898 = ORIENTED_EDGE('',*,*,#42890,.F.) ;
#61899 = ORIENTED_EDGE('',*,*,#43743,.T.) ;
#61900 = ORIENTED_EDGE('',*,*,#42894,.F.) ;
#61901 = ORIENTED_EDGE('',*,*,#42202,.F.) ;
#61902 = ORIENTED_EDGE('',*,*,#42205,.F.) ;
#61903 = ORIENTED_EDGE('',*,*,#42895,.F.) ;
#61904 = ORIENTED_EDGE('',*,*,#43744,.F.) ;
#61905 = ORIENTED_EDGE('',*,*,#42886,.F.) ;
#61906 = ORIENTED_EDGE('',*,*,#43744,.T.) ;
#61907 = ORIENTED_EDGE('',*,*,#42867,.F.) ;
#61908 = ORIENTED_EDGE('',*,*,#43745,.F.) ;
#61909 = ORIENTED_EDGE('',*,*,#42887,.F.) ;
#61910 = ORIENTED_EDGE('',*,*,#43745,.T.) ;
#61911 = ORIENTED_EDGE('',*,*,#43476,.F.) ;
#61912 = ORIENTED_EDGE('',*,*,#43477,.F.) ;
#61913 = ORIENTED_EDGE('',*,*,#43746,.F.) ;
#61914 = ORIENTED_EDGE('',*,*,#43746,.T.) ;
#61915 = ORIENTED_EDGE('',*,*,#43191,.F.) ;
#61916 = ORIENTED_EDGE('',*,*,#43747,.F.) ;
#61917 = ORIENTED_EDGE('',*,*,#42888,.F.) ;
#61918 = ORIENTED_EDGE('',*,*,#43747,.T.) ;
#61919 = ORIENTED_EDGE('',*,*,#43464,.F.) ;
#61920 = ORIENTED_EDGE('',*,*,#43461,.F.) ;
#61921 = ORIENTED_EDGE('',*,*,#43748,.F.) ;
#61922 = ORIENTED_EDGE('',*,*,#43748,.T.) ;
#61923 = ORIENTED_EDGE('',*,*,#42883,.F.) ;
#61924 = ORIENTED_EDGE('',*,*,#43749,.F.) ;
#61925 = ORIENTED_EDGE('',*,*,#42884,.F.) ;
#61926 = ORIENTED_EDGE('',*,*,#43749,.T.) ;
#61927 = ORIENTED_EDGE('',*,*,#42897,.F.) ;
#61928 = ORIENTED_EDGE('',*,*,#39383,.F.) ;
#61929 = ORIENTED_EDGE('',*,*,#42885,.F.) ;
#61930 = ORIENTED_EDGE('',*,*,#41569,.F.) ;
#61931 = ORIENTED_EDGE('',*,*,#42903,.F.) ;
#61932 = ORIENTED_EDGE('',*,*,#43750,.F.) ;
#61933 = ORIENTED_EDGE('',*,*,#42919,.F.) ;
#61934 = ORIENTED_EDGE('',*,*,#43750,.T.) ;
#61935 = ORIENTED_EDGE('',*,*,#43480,.F.) ;
#61936 = ORIENTED_EDGE('',*,*,#43478,.F.) ;
#61937 = ORIENTED_EDGE('',*,*,#43751,.F.) ;
#61938 = ORIENTED_EDGE('',*,*,#43751,.T.) ;
#61939 = ORIENTED_EDGE('',*,*,#43259,.F.) ;
#61940 = ORIENTED_EDGE('',*,*,#43752,.F.) ;
#61941 = ORIENTED_EDGE('',*,*,#42920,.F.) ;
#61942 = ORIENTED_EDGE('',*,*,#43752,.T.) ;
#61943 = ORIENTED_EDGE('',*,*,#43493,.F.) ;
#61944 = ORIENTED_EDGE('',*,*,#43495,.F.) ;
#61945 = ORIENTED_EDGE('',*,*,#43753,.F.) ;
#61946 = ORIENTED_EDGE('',*,*,#41571,.F.) ;
#61947 = ORIENTED_EDGE('',*,*,#42921,.F.) ;
#61948 = ORIENTED_EDGE('',*,*,#43753,.T.) ;
#61949 = ORIENTED_EDGE('',*,*,#42905,.F.) ;
#61950 = ORIENTED_EDGE('',*,*,#43754,.F.) ;
#61951 = ORIENTED_EDGE('',*,*,#42904,.F.) ;
#61952 = ORIENTED_EDGE('',*,*,#41567,.F.) ;
#61953 = ORIENTED_EDGE('',*,*,#42917,.F.) ;
#61954 = ORIENTED_EDGE('',*,*,#43481,.F.) ;
#61955 = ORIENTED_EDGE('',*,*,#43754,.T.) ;
#61956 = ORIENTED_EDGE('',*,*,#43755,.F.) ;
#61957 = ORIENTED_EDGE('',*,*,#43484,.F.) ;
#61958 = ORIENTED_EDGE('',*,*,#43755,.T.) ;
#61959 = ORIENTED_EDGE('',*,*,#42916,.F.) ;
#61960 = ORIENTED_EDGE('',*,*,#43756,.F.) ;
#61961 = ORIENTED_EDGE('',*,*,#43263,.F.) ;
#61962 = ORIENTED_EDGE('',*,*,#41573,.F.) ;
#61963 = ORIENTED_EDGE('',*,*,#42907,.F.) ;
#61964 = ORIENTED_EDGE('',*,*,#43757,.F.) ;
#61965 = ORIENTED_EDGE('',*,*,#42918,.F.) ;
#61966 = ORIENTED_EDGE('',*,*,#43497,.F.) ;
#61967 = ORIENTED_EDGE('',*,*,#43756,.T.) ;
#61968 = ORIENTED_EDGE('',*,*,#43757,.T.) ;
#61969 = ORIENTED_EDGE('',*,*,#43496,.F.) ;
#61970 = ORIENTED_EDGE('',*,*,#39374,.F.) ;
#61971 = ORIENTED_EDGE('',*,*,#42954,.F.) ;
#61972 = ORIENTED_EDGE('',*,*,#43758,.F.) ;
#61973 = ORIENTED_EDGE('',*,*,#42949,.F.) ;
#61974 = ORIENTED_EDGE('',*,*,#43758,.T.) ;
#61975 = ORIENTED_EDGE('',*,*,#42939,.F.) ;
#61976 = ORIENTED_EDGE('',*,*,#43759,.F.) ;
#61977 = ORIENTED_EDGE('',*,*,#42950,.F.) ;
#61978 = ORIENTED_EDGE('',*,*,#43759,.T.) ;
#61979 = ORIENTED_EDGE('',*,*,#43500,.F.) ;
#61980 = ORIENTED_EDGE('',*,*,#43498,.F.) ;
#61981 = ORIENTED_EDGE('',*,*,#43760,.F.) ;
#61982 = ORIENTED_EDGE('',*,*,#43760,.T.) ;
#61983 = ORIENTED_EDGE('',*,*,#43179,.F.) ;
#61984 = ORIENTED_EDGE('',*,*,#43761,.F.) ;
#61985 = ORIENTED_EDGE('',*,*,#42951,.F.) ;
#61986 = ORIENTED_EDGE('',*,*,#43761,.T.) ;
#61987 = ORIENTED_EDGE('',*,*,#43513,.F.) ;
#61988 = ORIENTED_EDGE('',*,*,#43515,.F.) ;
#61989 = ORIENTED_EDGE('',*,*,#43762,.F.) ;
#61990 = ORIENTED_EDGE('',*,*,#43762,.T.) ;
#61991 = ORIENTED_EDGE('',*,*,#42923,.F.) ;
#61992 = ORIENTED_EDGE('',*,*,#43763,.F.) ;
#61993 = ORIENTED_EDGE('',*,*,#42947,.F.) ;
#61994 = ORIENTED_EDGE('',*,*,#39155,.F.) ;
#61995 = ORIENTED_EDGE('',*,*,#42948,.F.) ;
#61996 = ORIENTED_EDGE('',*,*,#43763,.T.) ;
#61997 = ORIENTED_EDGE('',*,*,#42952,.F.) ;
#61998 = ORIENTED_EDGE('',*,*,#42290,.F.) ;
#61999 = ORIENTED_EDGE('',*,*,#42293,.F.) ;
#62000 = ORIENTED_EDGE('',*,*,#42953,.F.) ;
#62001 = ORIENTED_EDGE('',*,*,#43764,.F.) ;
#62002 = ORIENTED_EDGE('',*,*,#42944,.F.) ;
#62003 = ORIENTED_EDGE('',*,*,#43764,.T.) ;
#62004 = ORIENTED_EDGE('',*,*,#42925,.F.) ;
#62005 = ORIENTED_EDGE('',*,*,#43765,.F.) ;
#62006 = ORIENTED_EDGE('',*,*,#42945,.F.) ;
#62007 = ORIENTED_EDGE('',*,*,#43765,.T.) ;
#62008 = ORIENTED_EDGE('',*,*,#43516,.F.) ;
#62009 = ORIENTED_EDGE('',*,*,#43517,.F.) ;
#62010 = ORIENTED_EDGE('',*,*,#43766,.F.) ;
#62011 = ORIENTED_EDGE('',*,*,#43766,.T.) ;
#62012 = ORIENTED_EDGE('',*,*,#43183,.F.) ;
#62013 = ORIENTED_EDGE('',*,*,#43767,.F.) ;
#62014 = ORIENTED_EDGE('',*,*,#42946,.F.) ;
#62015 = ORIENTED_EDGE('',*,*,#43767,.T.) ;
#62016 = ORIENTED_EDGE('',*,*,#43504,.F.) ;
#62017 = ORIENTED_EDGE('',*,*,#43501,.F.) ;
#62018 = ORIENTED_EDGE('',*,*,#43768,.F.) ;
#62019 = ORIENTED_EDGE('',*,*,#43768,.T.) ;
#62020 = ORIENTED_EDGE('',*,*,#42941,.F.) ;
#62021 = ORIENTED_EDGE('',*,*,#43769,.F.) ;
#62022 = ORIENTED_EDGE('',*,*,#42942,.F.) ;
#62023 = ORIENTED_EDGE('',*,*,#43769,.T.) ;
#62024 = ORIENTED_EDGE('',*,*,#42955,.F.) ;
#62025 = ORIENTED_EDGE('',*,*,#39372,.F.) ;
#62026 = ORIENTED_EDGE('',*,*,#42943,.F.) ;
#62027 = ORIENTED_EDGE('',*,*,#41577,.F.) ;
#62028 = ORIENTED_EDGE('',*,*,#42961,.F.) ;
#62029 = ORIENTED_EDGE('',*,*,#43770,.F.) ;
#62030 = ORIENTED_EDGE('',*,*,#42977,.F.) ;
#62031 = ORIENTED_EDGE('',*,*,#43770,.T.) ;
#62032 = ORIENTED_EDGE('',*,*,#43520,.F.) ;
#62033 = ORIENTED_EDGE('',*,*,#43518,.F.) ;
#62034 = ORIENTED_EDGE('',*,*,#43771,.F.) ;
#62035 = ORIENTED_EDGE('',*,*,#43771,.T.) ;
#62036 = ORIENTED_EDGE('',*,*,#43251,.F.) ;
#62037 = ORIENTED_EDGE('',*,*,#43772,.F.) ;
#62038 = ORIENTED_EDGE('',*,*,#42978,.F.) ;
#62039 = ORIENTED_EDGE('',*,*,#43772,.T.) ;
#62040 = ORIENTED_EDGE('',*,*,#43533,.F.) ;
#62041 = ORIENTED_EDGE('',*,*,#43535,.F.) ;
#62042 = ORIENTED_EDGE('',*,*,#43773,.F.) ;
#62043 = ORIENTED_EDGE('',*,*,#41579,.F.) ;
#62044 = ORIENTED_EDGE('',*,*,#42979,.F.) ;
#62045 = ORIENTED_EDGE('',*,*,#43773,.T.) ;
#62046 = ORIENTED_EDGE('',*,*,#42963,.F.) ;
#62047 = ORIENTED_EDGE('',*,*,#43774,.F.) ;
#62048 = ORIENTED_EDGE('',*,*,#42962,.F.) ;
#62049 = ORIENTED_EDGE('',*,*,#41575,.F.) ;
#62050 = ORIENTED_EDGE('',*,*,#42975,.F.) ;
#62051 = ORIENTED_EDGE('',*,*,#43521,.F.) ;
#62052 = ORIENTED_EDGE('',*,*,#43774,.T.) ;
#62053 = ORIENTED_EDGE('',*,*,#43775,.F.) ;
#62054 = ORIENTED_EDGE('',*,*,#43524,.F.) ;
#62055 = ORIENTED_EDGE('',*,*,#43775,.T.) ;
#62056 = ORIENTED_EDGE('',*,*,#42974,.F.) ;
#62057 = ORIENTED_EDGE('',*,*,#43776,.F.) ;
#62058 = ORIENTED_EDGE('',*,*,#43255,.F.) ;
#62059 = ORIENTED_EDGE('',*,*,#41581,.F.) ;
#62060 = ORIENTED_EDGE('',*,*,#42965,.F.) ;
#62061 = ORIENTED_EDGE('',*,*,#43777,.F.) ;
#62062 = ORIENTED_EDGE('',*,*,#42976,.F.) ;
#62063 = ORIENTED_EDGE('',*,*,#43537,.F.) ;
#62064 = ORIENTED_EDGE('',*,*,#43776,.T.) ;
#62065 = ORIENTED_EDGE('',*,*,#43777,.T.) ;
#62066 = ORIENTED_EDGE('',*,*,#43536,.F.) ;
#62067 = ORIENTED_EDGE('',*,*,#39363,.F.) ;
#62068 = ORIENTED_EDGE('',*,*,#43012,.F.) ;
#62069 = ORIENTED_EDGE('',*,*,#43778,.F.) ;
#62070 = ORIENTED_EDGE('',*,*,#43007,.F.) ;
#62071 = ORIENTED_EDGE('',*,*,#43778,.T.) ;
#62072 = ORIENTED_EDGE('',*,*,#42997,.F.) ;
#62073 = ORIENTED_EDGE('',*,*,#43779,.F.) ;
#62074 = ORIENTED_EDGE('',*,*,#43008,.F.) ;
#62075 = ORIENTED_EDGE('',*,*,#43779,.T.) ;
#62076 = ORIENTED_EDGE('',*,*,#43540,.F.) ;
#62077 = ORIENTED_EDGE('',*,*,#43538,.F.) ;
#62078 = ORIENTED_EDGE('',*,*,#43780,.F.) ;
#62079 = ORIENTED_EDGE('',*,*,#43780,.T.) ;
#62080 = ORIENTED_EDGE('',*,*,#43171,.F.) ;
#62081 = ORIENTED_EDGE('',*,*,#43781,.F.) ;
#62082 = ORIENTED_EDGE('',*,*,#43009,.F.) ;
#62083 = ORIENTED_EDGE('',*,*,#43781,.T.) ;
#62084 = ORIENTED_EDGE('',*,*,#43553,.F.) ;
#62085 = ORIENTED_EDGE('',*,*,#43555,.F.) ;
#62086 = ORIENTED_EDGE('',*,*,#43782,.F.) ;
#62087 = ORIENTED_EDGE('',*,*,#43782,.T.) ;
#62088 = ORIENTED_EDGE('',*,*,#42981,.F.) ;
#62089 = ORIENTED_EDGE('',*,*,#43783,.F.) ;
#62090 = ORIENTED_EDGE('',*,*,#43005,.F.) ;
#62091 = ORIENTED_EDGE('',*,*,#39138,.F.) ;
#62092 = ORIENTED_EDGE('',*,*,#43006,.F.) ;
#62093 = ORIENTED_EDGE('',*,*,#43783,.T.) ;
#62094 = ORIENTED_EDGE('',*,*,#43010,.F.) ;
#62095 = ORIENTED_EDGE('',*,*,#42378,.F.) ;
#62096 = ORIENTED_EDGE('',*,*,#42381,.F.) ;
#62097 = ORIENTED_EDGE('',*,*,#43011,.F.) ;
#62098 = ORIENTED_EDGE('',*,*,#43784,.F.) ;
#62099 = ORIENTED_EDGE('',*,*,#43002,.F.) ;
#62100 = ORIENTED_EDGE('',*,*,#43784,.T.) ;
#62101 = ORIENTED_EDGE('',*,*,#42983,.F.) ;
#62102 = ORIENTED_EDGE('',*,*,#43785,.F.) ;
#62103 = ORIENTED_EDGE('',*,*,#43003,.F.) ;
#62104 = ORIENTED_EDGE('',*,*,#43785,.T.) ;
#62105 = ORIENTED_EDGE('',*,*,#43556,.F.) ;
#62106 = ORIENTED_EDGE('',*,*,#43557,.F.) ;
#62107 = ORIENTED_EDGE('',*,*,#43786,.F.) ;
#62108 = ORIENTED_EDGE('',*,*,#43786,.T.) ;
#62109 = ORIENTED_EDGE('',*,*,#43175,.F.) ;
#62110 = ORIENTED_EDGE('',*,*,#43787,.F.) ;
#62111 = ORIENTED_EDGE('',*,*,#43004,.F.) ;
#62112 = ORIENTED_EDGE('',*,*,#43787,.T.) ;
#62113 = ORIENTED_EDGE('',*,*,#43544,.F.) ;
#62114 = ORIENTED_EDGE('',*,*,#43541,.F.) ;
#62115 = ORIENTED_EDGE('',*,*,#43788,.F.) ;
#62116 = ORIENTED_EDGE('',*,*,#43788,.T.) ;
#62117 = ORIENTED_EDGE('',*,*,#42999,.F.) ;
#62118 = ORIENTED_EDGE('',*,*,#43789,.F.) ;
#62119 = ORIENTED_EDGE('',*,*,#43000,.F.) ;
#62120 = ORIENTED_EDGE('',*,*,#43789,.T.) ;
#62121 = ORIENTED_EDGE('',*,*,#43013,.F.) ;
#62122 = ORIENTED_EDGE('',*,*,#39361,.F.) ;
#62123 = ORIENTED_EDGE('',*,*,#43001,.F.) ;
#62124 = ORIENTED_EDGE('',*,*,#41585,.F.) ;
#62125 = ORIENTED_EDGE('',*,*,#43019,.F.) ;
#62126 = ORIENTED_EDGE('',*,*,#43790,.F.) ;
#62127 = ORIENTED_EDGE('',*,*,#43035,.F.) ;
#62128 = ORIENTED_EDGE('',*,*,#43790,.T.) ;
#62129 = ORIENTED_EDGE('',*,*,#43560,.F.) ;
#62130 = ORIENTED_EDGE('',*,*,#43558,.F.) ;
#62131 = ORIENTED_EDGE('',*,*,#43791,.F.) ;
#62132 = ORIENTED_EDGE('',*,*,#43791,.T.) ;
#62133 = ORIENTED_EDGE('',*,*,#43243,.F.) ;
#62134 = ORIENTED_EDGE('',*,*,#43792,.F.) ;
#62135 = ORIENTED_EDGE('',*,*,#43036,.F.) ;
#62136 = ORIENTED_EDGE('',*,*,#43792,.T.) ;
#62137 = ORIENTED_EDGE('',*,*,#43573,.F.) ;
#62138 = ORIENTED_EDGE('',*,*,#43575,.F.) ;
#62139 = ORIENTED_EDGE('',*,*,#43793,.F.) ;
#62140 = ORIENTED_EDGE('',*,*,#41587,.F.) ;
#62141 = ORIENTED_EDGE('',*,*,#43037,.F.) ;
#62142 = ORIENTED_EDGE('',*,*,#43793,.T.) ;
#62143 = ORIENTED_EDGE('',*,*,#43021,.F.) ;
#62144 = ORIENTED_EDGE('',*,*,#43794,.F.) ;
#62145 = ORIENTED_EDGE('',*,*,#43020,.F.) ;
#62146 = ORIENTED_EDGE('',*,*,#41583,.F.) ;
#62147 = ORIENTED_EDGE('',*,*,#43033,.F.) ;
#62148 = ORIENTED_EDGE('',*,*,#43561,.F.) ;
#62149 = ORIENTED_EDGE('',*,*,#43794,.T.) ;
#62150 = ORIENTED_EDGE('',*,*,#43795,.F.) ;
#62151 = ORIENTED_EDGE('',*,*,#43564,.F.) ;
#62152 = ORIENTED_EDGE('',*,*,#43795,.T.) ;
#62153 = ORIENTED_EDGE('',*,*,#43032,.F.) ;
#62154 = ORIENTED_EDGE('',*,*,#43796,.F.) ;
#62155 = ORIENTED_EDGE('',*,*,#43247,.F.) ;
#62156 = ORIENTED_EDGE('',*,*,#41589,.F.) ;
#62157 = ORIENTED_EDGE('',*,*,#43023,.F.) ;
#62158 = ORIENTED_EDGE('',*,*,#43797,.F.) ;
#62159 = ORIENTED_EDGE('',*,*,#43034,.F.) ;
#62160 = ORIENTED_EDGE('',*,*,#43577,.F.) ;
#62161 = ORIENTED_EDGE('',*,*,#43796,.T.) ;
#62162 = ORIENTED_EDGE('',*,*,#43797,.T.) ;
#62163 = ORIENTED_EDGE('',*,*,#43576,.F.) ;
#62164 = ORIENTED_EDGE('',*,*,#39352,.F.) ;
#62165 = ORIENTED_EDGE('',*,*,#43070,.F.) ;
#62166 = ORIENTED_EDGE('',*,*,#43798,.F.) ;
#62167 = ORIENTED_EDGE('',*,*,#43065,.F.) ;
#62168 = ORIENTED_EDGE('',*,*,#43798,.T.) ;
#62169 = ORIENTED_EDGE('',*,*,#43055,.F.) ;
#62170 = ORIENTED_EDGE('',*,*,#43799,.F.) ;
#62171 = ORIENTED_EDGE('',*,*,#43066,.F.) ;
#62172 = ORIENTED_EDGE('',*,*,#43799,.T.) ;
#62173 = ORIENTED_EDGE('',*,*,#43580,.F.) ;
#62174 = ORIENTED_EDGE('',*,*,#43578,.F.) ;
#62175 = ORIENTED_EDGE('',*,*,#43800,.F.) ;
#62176 = ORIENTED_EDGE('',*,*,#43800,.T.) ;
#62177 = ORIENTED_EDGE('',*,*,#43163,.F.) ;
#62178 = ORIENTED_EDGE('',*,*,#43801,.F.) ;
#62179 = ORIENTED_EDGE('',*,*,#43067,.F.) ;
#62180 = ORIENTED_EDGE('',*,*,#43801,.T.) ;
#62181 = ORIENTED_EDGE('',*,*,#43593,.F.) ;
#62182 = ORIENTED_EDGE('',*,*,#43595,.F.) ;
#62183 = ORIENTED_EDGE('',*,*,#43802,.F.) ;
#62184 = ORIENTED_EDGE('',*,*,#43802,.T.) ;
#62185 = ORIENTED_EDGE('',*,*,#43039,.F.) ;
#62186 = ORIENTED_EDGE('',*,*,#43803,.F.) ;
#62187 = ORIENTED_EDGE('',*,*,#43063,.F.) ;
#62188 = ORIENTED_EDGE('',*,*,#39121,.F.) ;
#62189 = ORIENTED_EDGE('',*,*,#43064,.F.) ;
#62190 = ORIENTED_EDGE('',*,*,#43803,.T.) ;
#62191 = ORIENTED_EDGE('',*,*,#43068,.F.) ;
#62192 = ORIENTED_EDGE('',*,*,#42466,.F.) ;
#62193 = ORIENTED_EDGE('',*,*,#42469,.F.) ;
#62194 = ORIENTED_EDGE('',*,*,#43069,.F.) ;
#62195 = ORIENTED_EDGE('',*,*,#43804,.F.) ;
#62196 = ORIENTED_EDGE('',*,*,#43060,.F.) ;
#62197 = ORIENTED_EDGE('',*,*,#43804,.T.) ;
#62198 = ORIENTED_EDGE('',*,*,#43041,.F.) ;
#62199 = ORIENTED_EDGE('',*,*,#43805,.F.) ;
#62200 = ORIENTED_EDGE('',*,*,#43061,.F.) ;
#62201 = ORIENTED_EDGE('',*,*,#43805,.T.) ;
#62202 = ORIENTED_EDGE('',*,*,#43596,.F.) ;
#62203 = ORIENTED_EDGE('',*,*,#43597,.F.) ;
#62204 = ORIENTED_EDGE('',*,*,#43806,.F.) ;
#62205 = ORIENTED_EDGE('',*,*,#43806,.T.) ;
#62206 = ORIENTED_EDGE('',*,*,#43167,.F.) ;
#62207 = ORIENTED_EDGE('',*,*,#43807,.F.) ;
#62208 = ORIENTED_EDGE('',*,*,#43062,.F.) ;
#62209 = ORIENTED_EDGE('',*,*,#43807,.T.) ;
#62210 = ORIENTED_EDGE('',*,*,#43584,.F.) ;
#62211 = ORIENTED_EDGE('',*,*,#43581,.F.) ;
#62212 = ORIENTED_EDGE('',*,*,#43808,.F.) ;
#62213 = ORIENTED_EDGE('',*,*,#43808,.T.) ;
#62214 = ORIENTED_EDGE('',*,*,#43057,.F.) ;
#62215 = ORIENTED_EDGE('',*,*,#43809,.F.) ;
#62216 = ORIENTED_EDGE('',*,*,#43058,.F.) ;
#62217 = ORIENTED_EDGE('',*,*,#43809,.T.) ;
#62218 = ORIENTED_EDGE('',*,*,#43071,.F.) ;
#62219 = ORIENTED_EDGE('',*,*,#39350,.F.) ;
#62220 = ORIENTED_EDGE('',*,*,#43059,.F.) ;
#62221 = ORIENTED_EDGE('',*,*,#41593,.F.) ;
#62222 = ORIENTED_EDGE('',*,*,#43077,.F.) ;
#62223 = ORIENTED_EDGE('',*,*,#43810,.F.) ;
#62224 = ORIENTED_EDGE('',*,*,#43093,.F.) ;
#62225 = ORIENTED_EDGE('',*,*,#43810,.T.) ;
#62226 = ORIENTED_EDGE('',*,*,#43600,.F.) ;
#62227 = ORIENTED_EDGE('',*,*,#43598,.F.) ;
#62228 = ORIENTED_EDGE('',*,*,#43811,.F.) ;
#62229 = ORIENTED_EDGE('',*,*,#43811,.T.) ;
#62230 = ORIENTED_EDGE('',*,*,#43235,.F.) ;
#62231 = ORIENTED_EDGE('',*,*,#43812,.F.) ;
#62232 = ORIENTED_EDGE('',*,*,#43094,.F.) ;
#62233 = ORIENTED_EDGE('',*,*,#43812,.T.) ;
#62234 = ORIENTED_EDGE('',*,*,#43613,.F.) ;
#62235 = ORIENTED_EDGE('',*,*,#43615,.F.) ;
#62236 = ORIENTED_EDGE('',*,*,#43813,.F.) ;
#62237 = ORIENTED_EDGE('',*,*,#41595,.F.) ;
#62238 = ORIENTED_EDGE('',*,*,#43095,.F.) ;
#62239 = ORIENTED_EDGE('',*,*,#43813,.T.) ;
#62240 = ORIENTED_EDGE('',*,*,#43079,.F.) ;
#62241 = ORIENTED_EDGE('',*,*,#43814,.F.) ;
#62242 = ORIENTED_EDGE('',*,*,#43078,.F.) ;
#62243 = ORIENTED_EDGE('',*,*,#41591,.F.) ;
#62244 = ORIENTED_EDGE('',*,*,#43091,.F.) ;
#62245 = ORIENTED_EDGE('',*,*,#43601,.F.) ;
#62246 = ORIENTED_EDGE('',*,*,#43814,.T.) ;
#62247 = ORIENTED_EDGE('',*,*,#43815,.F.) ;
#62248 = ORIENTED_EDGE('',*,*,#43604,.F.) ;
#62249 = ORIENTED_EDGE('',*,*,#43815,.T.) ;
#62250 = ORIENTED_EDGE('',*,*,#43090,.F.) ;
#62251 = ORIENTED_EDGE('',*,*,#43816,.F.) ;
#62252 = ORIENTED_EDGE('',*,*,#43239,.F.) ;
#62253 = ORIENTED_EDGE('',*,*,#41597,.F.) ;
#62254 = ORIENTED_EDGE('',*,*,#43081,.F.) ;
#62255 = ORIENTED_EDGE('',*,*,#43817,.F.) ;
#62256 = ORIENTED_EDGE('',*,*,#43092,.F.) ;
#62257 = ORIENTED_EDGE('',*,*,#43617,.F.) ;
#62258 = ORIENTED_EDGE('',*,*,#43816,.T.) ;
#62259 = ORIENTED_EDGE('',*,*,#43817,.T.) ;
#62260 = ORIENTED_EDGE('',*,*,#43616,.F.) ;
#62261 = ORIENTED_EDGE('',*,*,#39341,.F.) ;
#62262 = ORIENTED_EDGE('',*,*,#43128,.F.) ;
#62263 = ORIENTED_EDGE('',*,*,#43818,.F.) ;
#62264 = ORIENTED_EDGE('',*,*,#43123,.F.) ;
#62265 = ORIENTED_EDGE('',*,*,#43818,.T.) ;
#62266 = ORIENTED_EDGE('',*,*,#43113,.F.) ;
#62267 = ORIENTED_EDGE('',*,*,#43819,.F.) ;
#62268 = ORIENTED_EDGE('',*,*,#43124,.F.) ;
#62269 = ORIENTED_EDGE('',*,*,#43819,.T.) ;
#62270 = ORIENTED_EDGE('',*,*,#43620,.F.) ;
#62271 = ORIENTED_EDGE('',*,*,#43618,.F.) ;
#62272 = ORIENTED_EDGE('',*,*,#43820,.F.) ;
#62273 = ORIENTED_EDGE('',*,*,#43820,.T.) ;
#62274 = ORIENTED_EDGE('',*,*,#43155,.F.) ;
#62275 = ORIENTED_EDGE('',*,*,#43821,.F.) ;
#62276 = ORIENTED_EDGE('',*,*,#43125,.F.) ;
#62277 = ORIENTED_EDGE('',*,*,#43821,.T.) ;
#62278 = ORIENTED_EDGE('',*,*,#43633,.F.) ;
#62279 = ORIENTED_EDGE('',*,*,#43635,.F.) ;
#62280 = ORIENTED_EDGE('',*,*,#43822,.F.) ;
#62281 = ORIENTED_EDGE('',*,*,#43822,.T.) ;
#62282 = ORIENTED_EDGE('',*,*,#43097,.F.) ;
#62283 = ORIENTED_EDGE('',*,*,#43823,.F.) ;
#62284 = ORIENTED_EDGE('',*,*,#43121,.F.) ;
#62285 = ORIENTED_EDGE('',*,*,#39104,.F.) ;
#62286 = ORIENTED_EDGE('',*,*,#43122,.F.) ;
#62287 = ORIENTED_EDGE('',*,*,#43823,.T.) ;
#62288 = ORIENTED_EDGE('',*,*,#43126,.F.) ;
#62289 = ORIENTED_EDGE('',*,*,#42554,.F.) ;
#62290 = ORIENTED_EDGE('',*,*,#42557,.F.) ;
#62291 = ORIENTED_EDGE('',*,*,#43127,.F.) ;
#62292 = ORIENTED_EDGE('',*,*,#43824,.F.) ;
#62293 = ORIENTED_EDGE('',*,*,#43118,.F.) ;
#62294 = ORIENTED_EDGE('',*,*,#43824,.T.) ;
#62295 = ORIENTED_EDGE('',*,*,#43099,.F.) ;
#62296 = ORIENTED_EDGE('',*,*,#43825,.F.) ;
#62297 = ORIENTED_EDGE('',*,*,#43119,.F.) ;
#62298 = ORIENTED_EDGE('',*,*,#43825,.T.) ;
#62299 = ORIENTED_EDGE('',*,*,#43636,.F.) ;
#62300 = ORIENTED_EDGE('',*,*,#43637,.F.) ;
#62301 = ORIENTED_EDGE('',*,*,#43826,.F.) ;
#62302 = ORIENTED_EDGE('',*,*,#43826,.T.) ;
#62303 = ORIENTED_EDGE('',*,*,#43159,.F.) ;
#62304 = ORIENTED_EDGE('',*,*,#43827,.F.) ;
#62305 = ORIENTED_EDGE('',*,*,#43120,.F.) ;
#62306 = ORIENTED_EDGE('',*,*,#43827,.T.) ;
#62307 = ORIENTED_EDGE('',*,*,#43624,.F.) ;
#62308 = ORIENTED_EDGE('',*,*,#43621,.F.) ;
#62309 = ORIENTED_EDGE('',*,*,#43828,.F.) ;
#62310 = ORIENTED_EDGE('',*,*,#43828,.T.) ;
#62311 = ORIENTED_EDGE('',*,*,#43115,.F.) ;
#62312 = ORIENTED_EDGE('',*,*,#43829,.F.) ;
#62313 = ORIENTED_EDGE('',*,*,#43116,.F.) ;
#62314 = ORIENTED_EDGE('',*,*,#43829,.T.) ;
#62315 = ORIENTED_EDGE('',*,*,#43129,.F.) ;
#62316 = ORIENTED_EDGE('',*,*,#39339,.F.) ;
#62317 = ORIENTED_EDGE('',*,*,#43117,.F.) ;
#62318 = ORIENTED_EDGE('',*,*,#41601,.F.) ;
#62319 = ORIENTED_EDGE('',*,*,#43135,.F.) ;
#62320 = ORIENTED_EDGE('',*,*,#43830,.F.) ;
#62321 = ORIENTED_EDGE('',*,*,#43151,.F.) ;
#62322 = ORIENTED_EDGE('',*,*,#43830,.T.) ;
#62323 = ORIENTED_EDGE('',*,*,#43640,.F.) ;
#62324 = ORIENTED_EDGE('',*,*,#43638,.F.) ;
#62325 = ORIENTED_EDGE('',*,*,#43831,.F.) ;
#62326 = ORIENTED_EDGE('',*,*,#43831,.T.) ;
#62327 = ORIENTED_EDGE('',*,*,#43227,.F.) ;
#62328 = ORIENTED_EDGE('',*,*,#43832,.F.) ;
#62329 = ORIENTED_EDGE('',*,*,#43152,.F.) ;
#62330 = ORIENTED_EDGE('',*,*,#43832,.T.) ;
#62331 = ORIENTED_EDGE('',*,*,#43653,.F.) ;
#62332 = ORIENTED_EDGE('',*,*,#43655,.F.) ;
#62333 = ORIENTED_EDGE('',*,*,#43833,.F.) ;
#62334 = ORIENTED_EDGE('',*,*,#41603,.F.) ;
#62335 = ORIENTED_EDGE('',*,*,#43153,.F.) ;
#62336 = ORIENTED_EDGE('',*,*,#43833,.T.) ;
#62337 = ORIENTED_EDGE('',*,*,#43137,.F.) ;
#62338 = ORIENTED_EDGE('',*,*,#43834,.F.) ;
#62339 = ORIENTED_EDGE('',*,*,#43136,.F.) ;
#62340 = ORIENTED_EDGE('',*,*,#41599,.F.) ;
#62341 = ORIENTED_EDGE('',*,*,#43149,.F.) ;
#62342 = ORIENTED_EDGE('',*,*,#43641,.F.) ;
#62343 = ORIENTED_EDGE('',*,*,#43834,.T.) ;
#62344 = ORIENTED_EDGE('',*,*,#43835,.F.) ;
#62345 = ORIENTED_EDGE('',*,*,#43644,.F.) ;
#62346 = ORIENTED_EDGE('',*,*,#43835,.T.) ;
#62347 = ORIENTED_EDGE('',*,*,#43148,.F.) ;
#62348 = ORIENTED_EDGE('',*,*,#43836,.F.) ;
#62349 = ORIENTED_EDGE('',*,*,#43231,.F.) ;
#62350 = ORIENTED_EDGE('',*,*,#41605,.F.) ;
#62351 = ORIENTED_EDGE('',*,*,#43139,.F.) ;
#62352 = ORIENTED_EDGE('',*,*,#43837,.F.) ;
#62353 = ORIENTED_EDGE('',*,*,#43150,.F.) ;
#62354 = ORIENTED_EDGE('',*,*,#43657,.F.) ;
#62355 = ORIENTED_EDGE('',*,*,#43836,.T.) ;
#62356 = ORIENTED_EDGE('',*,*,#43837,.T.) ;
#62357 = ORIENTED_EDGE('',*,*,#43656,.F.) ;
#62358 = ORIENTED_EDGE('',*,*,#43838,.F.) ;
#62359 = ORIENTED_EDGE('',*,*,#43839,.T.) ;
#62360 = ORIENTED_EDGE('',*,*,#43840,.T.) ;
#62361 = ORIENTED_EDGE('',*,*,#43841,.F.) ;
#62362 = ORIENTED_EDGE('',*,*,#43842,.F.) ;
#62363 = ORIENTED_EDGE('',*,*,#43843,.T.) ;
#62364 = ORIENTED_EDGE('',*,*,#43838,.T.) ;
#62365 = ORIENTED_EDGE('',*,*,#43844,.F.) ;
#62366 = ORIENTED_EDGE('',*,*,#43845,.F.) ;
#62367 = ORIENTED_EDGE('',*,*,#43846,.T.) ;
#62368 = ORIENTED_EDGE('',*,*,#43842,.T.) ;
#62369 = ORIENTED_EDGE('',*,*,#43847,.F.) ;
#62370 = ORIENTED_EDGE('',*,*,#43848,.F.) ;
#62371 = ORIENTED_EDGE('',*,*,#43849,.T.) ;
#62372 = ORIENTED_EDGE('',*,*,#43845,.T.) ;
#62373 = ORIENTED_EDGE('',*,*,#43850,.F.) ;
#62374 = ORIENTED_EDGE('',*,*,#43851,.F.) ;
#62375 = ORIENTED_EDGE('',*,*,#43852,.T.) ;
#62376 = ORIENTED_EDGE('',*,*,#43848,.T.) ;
#62377 = ORIENTED_EDGE('',*,*,#43853,.F.) ;
#62378 = ORIENTED_EDGE('',*,*,#43854,.F.) ;
#62379 = ORIENTED_EDGE('',*,*,#43855,.T.) ;
#62380 = ORIENTED_EDGE('',*,*,#43851,.T.) ;
#62381 = ORIENTED_EDGE('',*,*,#43856,.F.) ;
#62382 = ORIENTED_EDGE('',*,*,#43857,.F.) ;
#62383 = ORIENTED_EDGE('',*,*,#43858,.T.) ;
#62384 = ORIENTED_EDGE('',*,*,#43854,.T.) ;
#62385 = ORIENTED_EDGE('',*,*,#43859,.F.) ;
#62386 = ORIENTED_EDGE('',*,*,#43860,.F.) ;
#62387 = ORIENTED_EDGE('',*,*,#43861,.T.) ;
#62388 = ORIENTED_EDGE('',*,*,#43857,.T.) ;
#62389 = ORIENTED_EDGE('',*,*,#43862,.F.) ;
#62390 = ORIENTED_EDGE('',*,*,#43863,.F.) ;
#62391 = ORIENTED_EDGE('',*,*,#43864,.T.) ;
#62392 = ORIENTED_EDGE('',*,*,#43860,.T.) ;
#62393 = ORIENTED_EDGE('',*,*,#43865,.F.) ;
#62394 = ORIENTED_EDGE('',*,*,#43866,.F.) ;
#62395 = ORIENTED_EDGE('',*,*,#43867,.T.) ;
#62396 = ORIENTED_EDGE('',*,*,#43863,.T.) ;
#62397 = ORIENTED_EDGE('',*,*,#43868,.F.) ;
#62398 = ORIENTED_EDGE('',*,*,#43869,.F.) ;
#62399 = ORIENTED_EDGE('',*,*,#43870,.F.) ;
#62400 = ORIENTED_EDGE('',*,*,#43871,.T.) ;
#62401 = ORIENTED_EDGE('',*,*,#43872,.T.) ;
#62402 = ORIENTED_EDGE('',*,*,#43873,.F.) ;
#62403 = ORIENTED_EDGE('',*,*,#43874,.F.) ;
#62404 = ORIENTED_EDGE('',*,*,#43869,.T.) ;
#62405 = ORIENTED_EDGE('',*,*,#43875,.T.) ;
#62406 = ORIENTED_EDGE('',*,*,#43876,.F.) ;
#62407 = ORIENTED_EDGE('',*,*,#43877,.F.) ;
#62408 = ORIENTED_EDGE('',*,*,#43873,.T.) ;
#62409 = ORIENTED_EDGE('',*,*,#43878,.T.) ;
#62410 = ORIENTED_EDGE('',*,*,#43879,.F.) ;
#62411 = ORIENTED_EDGE('',*,*,#43880,.F.) ;
#62412 = ORIENTED_EDGE('',*,*,#43876,.T.) ;
#62413 = ORIENTED_EDGE('',*,*,#43881,.T.) ;
#62414 = ORIENTED_EDGE('',*,*,#43882,.F.) ;
#62415 = ORIENTED_EDGE('',*,*,#43883,.F.) ;
#62416 = ORIENTED_EDGE('',*,*,#43879,.T.) ;
#62417 = ORIENTED_EDGE('',*,*,#43884,.T.) ;
#62418 = ORIENTED_EDGE('',*,*,#43885,.F.) ;
#62419 = ORIENTED_EDGE('',*,*,#43886,.F.) ;
#62420 = ORIENTED_EDGE('',*,*,#43882,.T.) ;
#62421 = ORIENTED_EDGE('',*,*,#43887,.T.) ;
#62422 = ORIENTED_EDGE('',*,*,#43888,.F.) ;
#62423 = ORIENTED_EDGE('',*,*,#43889,.F.) ;
#62424 = ORIENTED_EDGE('',*,*,#43885,.T.) ;
#62425 = ORIENTED_EDGE('',*,*,#43890,.T.) ;
#62426 = ORIENTED_EDGE('',*,*,#43891,.F.) ;
#62427 = ORIENTED_EDGE('',*,*,#43892,.F.) ;
#62428 = ORIENTED_EDGE('',*,*,#43888,.T.) ;
#62429 = ORIENTED_EDGE('',*,*,#43893,.T.) ;
#62430 = ORIENTED_EDGE('',*,*,#43894,.T.) ;
#62431 = ORIENTED_EDGE('',*,*,#43895,.T.) ;
#62432 = ORIENTED_EDGE('',*,*,#43896,.T.) ;
#62433 = ORIENTED_EDGE('',*,*,#43897,.T.) ;
#62434 = ORIENTED_EDGE('',*,*,#43898,.T.) ;
#62435 = ORIENTED_EDGE('',*,*,#43899,.T.) ;
#62436 = ORIENTED_EDGE('',*,*,#43900,.F.) ;
#62437 = ORIENTED_EDGE('',*,*,#43901,.T.) ;
#62438 = ORIENTED_EDGE('',*,*,#43902,.T.) ;
#62439 = ORIENTED_EDGE('',*,*,#43895,.F.) ;
#62440 = ORIENTED_EDGE('',*,*,#43901,.F.) ;
#62441 = ORIENTED_EDGE('',*,*,#43903,.F.) ;
#62442 = ORIENTED_EDGE('',*,*,#43891,.T.) ;
#62443 = ORIENTED_EDGE('',*,*,#43904,.T.) ;
#62444 = ORIENTED_EDGE('',*,*,#43866,.T.) ;
#62445 = ORIENTED_EDGE('',*,*,#43905,.F.) ;
#62446 = ORIENTED_EDGE('',*,*,#43906,.F.) ;
#62447 = ORIENTED_EDGE('',*,*,#43907,.T.) ;
#62448 = ORIENTED_EDGE('',*,*,#43908,.F.) ;
#62449 = ORIENTED_EDGE('',*,*,#43909,.T.) ;
#62450 = ORIENTED_EDGE('',*,*,#43910,.T.) ;
#62451 = ORIENTED_EDGE('',*,*,#43909,.F.) ;
#62452 = ORIENTED_EDGE('',*,*,#43911,.F.) ;
#62453 = ORIENTED_EDGE('',*,*,#43912,.T.) ;
#62454 = ORIENTED_EDGE('',*,*,#43908,.T.) ;
#62455 = ORIENTED_EDGE('',*,*,#43912,.F.) ;
#62456 = ORIENTED_EDGE('',*,*,#43913,.T.) ;
#62457 = ORIENTED_EDGE('',*,*,#43911,.T.) ;
#62458 = ORIENTED_EDGE('',*,*,#43913,.F.) ;
#62459 = ORIENTED_EDGE('',*,*,#43914,.F.) ;
#62460 = ORIENTED_EDGE('',*,*,#43915,.T.) ;
#62461 = ORIENTED_EDGE('',*,*,#43894,.F.) ;
#62462 = ORIENTED_EDGE('',*,*,#43915,.F.) ;
#62463 = ORIENTED_EDGE('',*,*,#43916,.T.) ;
#62464 = ORIENTED_EDGE('',*,*,#43917,.T.) ;
#62465 = ORIENTED_EDGE('',*,*,#43918,.F.) ;
#62466 = ORIENTED_EDGE('',*,*,#43917,.F.) ;
#62467 = ORIENTED_EDGE('',*,*,#43919,.T.) ;
#62468 = ORIENTED_EDGE('',*,*,#43906,.T.) ;
#62469 = ORIENTED_EDGE('',*,*,#43920,.T.) ;
#62470 = ORIENTED_EDGE('',*,*,#43871,.F.) ;
#62471 = ORIENTED_EDGE('',*,*,#43921,.F.) ;
#62472 = ORIENTED_EDGE('',*,*,#43922,.T.) ;
#62473 = ORIENTED_EDGE('',*,*,#43923,.F.) ;
#62474 = ORIENTED_EDGE('',*,*,#43924,.T.) ;
#62475 = ORIENTED_EDGE('',*,*,#43925,.F.) ;
#62476 = ORIENTED_EDGE('',*,*,#43926,.T.) ;
#62477 = ORIENTED_EDGE('',*,*,#43927,.F.) ;
#62478 = ORIENTED_EDGE('',*,*,#43928,.T.) ;
#62479 = ORIENTED_EDGE('',*,*,#43929,.F.) ;
#62480 = ORIENTED_EDGE('',*,*,#43930,.T.) ;
#62481 = ORIENTED_EDGE('',*,*,#43931,.F.) ;
#62482 = ORIENTED_EDGE('',*,*,#43932,.T.) ;
#62483 = ORIENTED_EDGE('',*,*,#43933,.F.) ;
#62484 = ORIENTED_EDGE('',*,*,#43934,.T.) ;
#62485 = ORIENTED_EDGE('',*,*,#43935,.F.) ;
#62486 = ORIENTED_EDGE('',*,*,#43936,.T.) ;
#62487 = ORIENTED_EDGE('',*,*,#43937,.F.) ;
#62488 = ORIENTED_EDGE('',*,*,#43938,.T.) ;
#62489 = ORIENTED_EDGE('',*,*,#43939,.F.) ;
#62490 = ORIENTED_EDGE('',*,*,#43940,.T.) ;
#62491 = ORIENTED_EDGE('',*,*,#43941,.F.) ;
#62492 = ORIENTED_EDGE('',*,*,#43942,.T.) ;
#62493 = ORIENTED_EDGE('',*,*,#43943,.F.) ;
#62494 = ORIENTED_EDGE('',*,*,#43944,.T.) ;
#62495 = ORIENTED_EDGE('',*,*,#43926,.F.) ;
#62496 = ORIENTED_EDGE('',*,*,#43945,.T.) ;
#62497 = ORIENTED_EDGE('',*,*,#43946,.F.) ;
#62498 = ORIENTED_EDGE('',*,*,#43947,.T.) ;
#62499 = ORIENTED_EDGE('',*,*,#43948,.F.) ;
#62500 = ORIENTED_EDGE('',*,*,#43949,.T.) ;
#62501 = ORIENTED_EDGE('',*,*,#43924,.F.) ;
#62502 = ORIENTED_EDGE('',*,*,#43950,.T.) ;
#62503 = ORIENTED_EDGE('',*,*,#43951,.F.) ;
#62504 = ORIENTED_EDGE('',*,*,#43952,.T.) ;
#62505 = ORIENTED_EDGE('',*,*,#43932,.F.) ;
#62506 = ORIENTED_EDGE('',*,*,#43953,.T.) ;
#62507 = ORIENTED_EDGE('',*,*,#43954,.F.) ;
#62508 = ORIENTED_EDGE('',*,*,#43955,.T.) ;
#62509 = ORIENTED_EDGE('',*,*,#43936,.F.) ;
#62510 = ORIENTED_EDGE('',*,*,#43956,.T.) ;
#62511 = ORIENTED_EDGE('',*,*,#43957,.F.) ;
#62512 = ORIENTED_EDGE('',*,*,#43958,.T.) ;
#62513 = ORIENTED_EDGE('',*,*,#43940,.F.) ;
#62514 = ORIENTED_EDGE('',*,*,#43959,.T.) ;
#62515 = ORIENTED_EDGE('',*,*,#43960,.F.) ;
#62516 = ORIENTED_EDGE('',*,*,#43961,.T.) ;
#62517 = ORIENTED_EDGE('',*,*,#43944,.F.) ;
#62518 = ORIENTED_EDGE('',*,*,#43962,.T.) ;
#62519 = ORIENTED_EDGE('',*,*,#43922,.F.) ;
#62520 = ORIENTED_EDGE('',*,*,#43963,.T.) ;
#62521 = ORIENTED_EDGE('',*,*,#43964,.F.) ;
#62522 = ORIENTED_EDGE('',*,*,#43965,.T.) ;
#62523 = ORIENTED_EDGE('',*,*,#43966,.F.) ;
#62524 = ORIENTED_EDGE('',*,*,#43967,.T.) ;
#62525 = ORIENTED_EDGE('',*,*,#43928,.F.) ;
#62526 = ORIENTED_EDGE('',*,*,#43968,.T.) ;
#62527 = ORIENTED_EDGE('',*,*,#43930,.F.) ;
#62528 = ORIENTED_EDGE('',*,*,#43969,.T.) ;
#62529 = ORIENTED_EDGE('',*,*,#43970,.F.) ;
#62530 = ORIENTED_EDGE('',*,*,#43971,.T.) ;
#62531 = ORIENTED_EDGE('',*,*,#43934,.F.) ;
#62532 = ORIENTED_EDGE('',*,*,#43972,.T.) ;
#62533 = ORIENTED_EDGE('',*,*,#43973,.F.) ;
#62534 = ORIENTED_EDGE('',*,*,#43974,.T.) ;
#62535 = ORIENTED_EDGE('',*,*,#43938,.F.) ;
#62536 = ORIENTED_EDGE('',*,*,#43975,.T.) ;
#62537 = ORIENTED_EDGE('',*,*,#43976,.F.) ;
#62538 = ORIENTED_EDGE('',*,*,#43977,.T.) ;
#62539 = ORIENTED_EDGE('',*,*,#43942,.F.) ;
#62540 = ORIENTED_EDGE('',*,*,#43978,.T.) ;
#62541 = ORIENTED_EDGE('',*,*,#43979,.F.) ;
#62542 = ORIENTED_EDGE('',*,*,#43980,.T.) ;
#62543 = ORIENTED_EDGE('',*,*,#43964,.T.) ;
#62544 = ORIENTED_EDGE('',*,*,#43966,.T.) ;
#62545 = ORIENTED_EDGE('',*,*,#43979,.T.) ;
#62546 = ORIENTED_EDGE('',*,*,#43976,.T.) ;
#62547 = ORIENTED_EDGE('',*,*,#43973,.T.) ;
#62548 = ORIENTED_EDGE('',*,*,#43970,.T.) ;
#62549 = ORIENTED_EDGE('',*,*,#43910,.F.) ;
#62550 = ORIENTED_EDGE('',*,*,#43951,.T.) ;
#62551 = ORIENTED_EDGE('',*,*,#43954,.T.) ;
#62552 = ORIENTED_EDGE('',*,*,#43957,.T.) ;
#62553 = ORIENTED_EDGE('',*,*,#43960,.T.) ;
#62554 = ORIENTED_EDGE('',*,*,#43946,.T.) ;
#62555 = ORIENTED_EDGE('',*,*,#43948,.T.) ;
#62556 = ORIENTED_EDGE('',*,*,#43914,.T.) ;
#62557 = ORIENTED_EDGE('',*,*,#43918,.T.) ;
#62558 = ORIENTED_EDGE('',*,*,#43943,.T.) ;
#62559 = ORIENTED_EDGE('',*,*,#43980,.F.) ;
#62560 = ORIENTED_EDGE('',*,*,#43968,.F.) ;
#62561 = ORIENTED_EDGE('',*,*,#43927,.T.) ;
#62562 = ORIENTED_EDGE('',*,*,#43947,.F.) ;
#62563 = ORIENTED_EDGE('',*,*,#43962,.F.) ;
#62564 = ORIENTED_EDGE('',*,*,#43939,.T.) ;
#62565 = ORIENTED_EDGE('',*,*,#43977,.F.) ;
#62566 = ORIENTED_EDGE('',*,*,#43978,.F.) ;
#62567 = ORIENTED_EDGE('',*,*,#43941,.T.) ;
#62568 = ORIENTED_EDGE('',*,*,#43961,.F.) ;
#62569 = ORIENTED_EDGE('',*,*,#43959,.F.) ;
#62570 = ORIENTED_EDGE('',*,*,#43935,.T.) ;
#62571 = ORIENTED_EDGE('',*,*,#43974,.F.) ;
#62572 = ORIENTED_EDGE('',*,*,#43975,.F.) ;
#62573 = ORIENTED_EDGE('',*,*,#43937,.T.) ;
#62574 = ORIENTED_EDGE('',*,*,#43958,.F.) ;
#62575 = ORIENTED_EDGE('',*,*,#43956,.F.) ;
#62576 = ORIENTED_EDGE('',*,*,#43931,.T.) ;
#62577 = ORIENTED_EDGE('',*,*,#43971,.F.) ;
#62578 = ORIENTED_EDGE('',*,*,#43972,.F.) ;
#62579 = ORIENTED_EDGE('',*,*,#43933,.T.) ;
#62580 = ORIENTED_EDGE('',*,*,#43955,.F.) ;
#62581 = ORIENTED_EDGE('',*,*,#43953,.F.) ;
#62582 = ORIENTED_EDGE('',*,*,#43923,.T.) ;
#62583 = ORIENTED_EDGE('',*,*,#43965,.F.) ;
#62584 = ORIENTED_EDGE('',*,*,#43969,.F.) ;
#62585 = ORIENTED_EDGE('',*,*,#43929,.T.) ;
#62586 = ORIENTED_EDGE('',*,*,#43952,.F.) ;
#62587 = ORIENTED_EDGE('',*,*,#43950,.F.) ;
#62588 = ORIENTED_EDGE('',*,*,#43925,.T.) ;
#62589 = ORIENTED_EDGE('',*,*,#43967,.F.) ;
#62590 = ORIENTED_EDGE('',*,*,#43963,.F.) ;
#62591 = ORIENTED_EDGE('',*,*,#43921,.T.) ;
#62592 = ORIENTED_EDGE('',*,*,#43949,.F.) ;
#62593 = ORIENTED_EDGE('',*,*,#43945,.F.) ;
#62594 = ORIENTED_EDGE('',*,*,#43870,.T.) ;
#62595 = ORIENTED_EDGE('',*,*,#43874,.T.) ;
#62596 = ORIENTED_EDGE('',*,*,#43877,.T.) ;
#62597 = ORIENTED_EDGE('',*,*,#43880,.T.) ;
#62598 = ORIENTED_EDGE('',*,*,#43883,.T.) ;
#62599 = ORIENTED_EDGE('',*,*,#43886,.T.) ;
#62600 = ORIENTED_EDGE('',*,*,#43889,.T.) ;
#62601 = ORIENTED_EDGE('',*,*,#43892,.T.) ;
#62602 = ORIENTED_EDGE('',*,*,#43903,.T.) ;
#62603 = ORIENTED_EDGE('',*,*,#43900,.T.) ;
#62604 = ORIENTED_EDGE('',*,*,#43981,.T.) ;
#62605 = ORIENTED_EDGE('',*,*,#43839,.F.) ;
#62606 = ORIENTED_EDGE('',*,*,#43843,.F.) ;
#62607 = ORIENTED_EDGE('',*,*,#43846,.F.) ;
#62608 = ORIENTED_EDGE('',*,*,#43849,.F.) ;
#62609 = ORIENTED_EDGE('',*,*,#43852,.F.) ;
#62610 = ORIENTED_EDGE('',*,*,#43855,.F.) ;
#62611 = ORIENTED_EDGE('',*,*,#43858,.F.) ;
#62612 = ORIENTED_EDGE('',*,*,#43861,.F.) ;
#62613 = ORIENTED_EDGE('',*,*,#43864,.F.) ;
#62614 = ORIENTED_EDGE('',*,*,#43867,.F.) ;
#62615 = ORIENTED_EDGE('',*,*,#43907,.F.) ;
#62616 = ORIENTED_EDGE('',*,*,#43919,.F.) ;
#62617 = ORIENTED_EDGE('',*,*,#43916,.F.) ;
#62618 = ORIENTED_EDGE('',*,*,#43982,.F.) ;
#62619 = ORIENTED_EDGE('',*,*,#43983,.F.) ;
#62620 = ORIENTED_EDGE('',*,*,#43896,.F.) ;
#62621 = ORIENTED_EDGE('',*,*,#43902,.F.) ;
#62622 = ORIENTED_EDGE('',*,*,#43904,.F.) ;
#62623 = ORIENTED_EDGE('',*,*,#43893,.F.) ;
#62624 = ORIENTED_EDGE('',*,*,#43890,.F.) ;
#62625 = ORIENTED_EDGE('',*,*,#43887,.F.) ;
#62626 = ORIENTED_EDGE('',*,*,#43884,.F.) ;
#62627 = ORIENTED_EDGE('',*,*,#43881,.F.) ;
#62628 = ORIENTED_EDGE('',*,*,#43878,.F.) ;
#62629 = ORIENTED_EDGE('',*,*,#43875,.F.) ;
#62630 = ORIENTED_EDGE('',*,*,#43872,.F.) ;
#62631 = ORIENTED_EDGE('',*,*,#43920,.F.) ;
#62632 = ORIENTED_EDGE('',*,*,#43905,.T.) ;
#62633 = ORIENTED_EDGE('',*,*,#43868,.T.) ;
#62634 = ORIENTED_EDGE('',*,*,#43865,.T.) ;
#62635 = ORIENTED_EDGE('',*,*,#43862,.T.) ;
#62636 = ORIENTED_EDGE('',*,*,#43859,.T.) ;
#62637 = ORIENTED_EDGE('',*,*,#43856,.T.) ;
#62638 = ORIENTED_EDGE('',*,*,#43853,.T.) ;
#62639 = ORIENTED_EDGE('',*,*,#43850,.T.) ;
#62640 = ORIENTED_EDGE('',*,*,#43847,.T.) ;
#62641 = ORIENTED_EDGE('',*,*,#43844,.T.) ;
#62642 = ORIENTED_EDGE('',*,*,#43841,.T.) ;
#62643 = ORIENTED_EDGE('',*,*,#43984,.T.) ;
#62644 = ORIENTED_EDGE('',*,*,#43981,.F.) ;
#62645 = ORIENTED_EDGE('',*,*,#43899,.F.) ;
#62646 = ORIENTED_EDGE('',*,*,#43985,.T.) ;
#62647 = ORIENTED_EDGE('',*,*,#43840,.F.) ;
#62648 = ORIENTED_EDGE('',*,*,#43984,.F.) ;
#62649 = ORIENTED_EDGE('',*,*,#43898,.F.) ;
#62650 = ORIENTED_EDGE('',*,*,#43983,.T.) ;
#62651 = ORIENTED_EDGE('',*,*,#43982,.T.) ;
#62652 = ORIENTED_EDGE('',*,*,#43985,.F.) ;
#62653 = ORIENTED_EDGE('',*,*,#43897,.F.) ;
#62654 = ORIENTED_EDGE('',*,*,#43986,.T.) ;
#62655 = ORIENTED_EDGE('',*,*,#43987,.T.) ;
#62656 = ORIENTED_EDGE('',*,*,#43988,.T.) ;
#62657 = ORIENTED_EDGE('',*,*,#43989,.T.) ;
#62658 = ORIENTED_EDGE('',*,*,#43990,.T.) ;
#62659 = ORIENTED_EDGE('',*,*,#43991,.T.) ;
#62660 = ORIENTED_EDGE('',*,*,#43992,.T.) ;
#62661 = ORIENTED_EDGE('',*,*,#43993,.T.) ;
#62662 = ORIENTED_EDGE('',*,*,#43994,.T.) ;
#62663 = ORIENTED_EDGE('',*,*,#43995,.T.) ;
#62664 = ORIENTED_EDGE('',*,*,#43996,.T.) ;
#62665 = ORIENTED_EDGE('',*,*,#43997,.T.) ;
#62666 = ORIENTED_EDGE('',*,*,#43998,.T.) ;
#62667 = ORIENTED_EDGE('',*,*,#43999,.T.) ;
#62668 = ORIENTED_EDGE('',*,*,#44000,.T.) ;
#62669 = ORIENTED_EDGE('',*,*,#44001,.T.) ;
#62670 = ORIENTED_EDGE('',*,*,#44002,.T.) ;
#62671 = ORIENTED_EDGE('',*,*,#44003,.T.) ;
#62672 = ORIENTED_EDGE('',*,*,#43986,.F.) ;
#62673 = ORIENTED_EDGE('',*,*,#43995,.F.) ;
#62674 = ORIENTED_EDGE('',*,*,#44004,.T.) ;
#62675 = ORIENTED_EDGE('',*,*,#44005,.F.) ;
#62676 = ORIENTED_EDGE('',*,*,#44006,.T.) ;
#62677 = ORIENTED_EDGE('',*,*,#44007,.F.) ;
#62678 = ORIENTED_EDGE('',*,*,#44006,.F.) ;
#62679 = ORIENTED_EDGE('',*,*,#44008,.F.) ;
#62680 = ORIENTED_EDGE('',*,*,#44009,.T.) ;
#62681 = ORIENTED_EDGE('',*,*,#44010,.T.) ;
#62682 = ORIENTED_EDGE('',*,*,#44009,.F.) ;
#62683 = ORIENTED_EDGE('',*,*,#44010,.F.) ;
#62684 = ORIENTED_EDGE('',*,*,#44011,.T.) ;
#62685 = ORIENTED_EDGE('',*,*,#44012,.T.) ;
#62686 = ORIENTED_EDGE('',*,*,#44011,.F.) ;
#62687 = ORIENTED_EDGE('',*,*,#44007,.T.) ;
#62688 = ORIENTED_EDGE('',*,*,#44013,.T.) ;
#62689 = ORIENTED_EDGE('',*,*,#44014,.T.) ;
#62690 = ORIENTED_EDGE('',*,*,#44013,.F.) ;
#62691 = ORIENTED_EDGE('',*,*,#44008,.T.) ;
#62692 = ORIENTED_EDGE('',*,*,#44015,.T.) ;
#62693 = ORIENTED_EDGE('',*,*,#44016,.F.) ;
#62694 = ORIENTED_EDGE('',*,*,#44017,.F.) ;
#62695 = ORIENTED_EDGE('',*,*,#44018,.F.) ;
#62696 = ORIENTED_EDGE('',*,*,#44019,.T.) ;
#62697 = ORIENTED_EDGE('',*,*,#44020,.F.) ;
#62698 = ORIENTED_EDGE('',*,*,#44021,.F.) ;
#62699 = ORIENTED_EDGE('',*,*,#44022,.F.) ;
#62700 = ORIENTED_EDGE('',*,*,#44023,.T.) ;
#62701 = ORIENTED_EDGE('',*,*,#44024,.F.) ;
#62702 = ORIENTED_EDGE('',*,*,#44025,.F.) ;
#62703 = ORIENTED_EDGE('',*,*,#44026,.F.) ;
#62704 = ORIENTED_EDGE('',*,*,#44027,.T.) ;
#62705 = ORIENTED_EDGE('',*,*,#44028,.F.) ;
#62706 = ORIENTED_EDGE('',*,*,#44029,.F.) ;
#62707 = ORIENTED_EDGE('',*,*,#44030,.F.) ;
#62708 = ORIENTED_EDGE('',*,*,#44030,.T.) ;
#62709 = ORIENTED_EDGE('',*,*,#44031,.T.) ;
#62710 = ORIENTED_EDGE('',*,*,#44032,.T.) ;
#62711 = ORIENTED_EDGE('',*,*,#44033,.F.) ;
#62712 = ORIENTED_EDGE('',*,*,#44034,.T.) ;
#62713 = ORIENTED_EDGE('',*,*,#44035,.T.) ;
#62714 = ORIENTED_EDGE('',*,*,#44024,.T.) ;
#62715 = ORIENTED_EDGE('',*,*,#44036,.T.) ;
#62716 = ORIENTED_EDGE('',*,*,#44037,.T.) ;
#62717 = ORIENTED_EDGE('',*,*,#44038,.T.) ;
#62718 = ORIENTED_EDGE('',*,*,#44016,.T.) ;
#62719 = ORIENTED_EDGE('',*,*,#44039,.T.) ;
#62720 = ORIENTED_EDGE('',*,*,#44022,.T.) ;
#62721 = ORIENTED_EDGE('',*,*,#44040,.T.) ;
#62722 = ORIENTED_EDGE('',*,*,#44041,.T.) ;
#62723 = ORIENTED_EDGE('',*,*,#44042,.F.) ;
#62724 = ORIENTED_EDGE('',*,*,#44043,.F.) ;
#62725 = ORIENTED_EDGE('',*,*,#44044,.F.) ;
#62726 = ORIENTED_EDGE('',*,*,#44039,.F.) ;
#62727 = ORIENTED_EDGE('',*,*,#44015,.F.) ;
#62728 = ORIENTED_EDGE('',*,*,#44033,.T.) ;
#62729 = ORIENTED_EDGE('',*,*,#44045,.F.) ;
#62730 = ORIENTED_EDGE('',*,*,#44046,.F.) ;
#62731 = ORIENTED_EDGE('',*,*,#44047,.F.) ;
#62732 = ORIENTED_EDGE('',*,*,#44036,.F.) ;
#62733 = ORIENTED_EDGE('',*,*,#44023,.F.) ;
#62734 = ORIENTED_EDGE('',*,*,#44042,.T.) ;
#62735 = ORIENTED_EDGE('',*,*,#44048,.F.) ;
#62736 = ORIENTED_EDGE('',*,*,#44049,.T.) ;
#62737 = ORIENTED_EDGE('',*,*,#43994,.F.) ;
#62738 = ORIENTED_EDGE('',*,*,#44050,.F.) ;
#62739 = ORIENTED_EDGE('',*,*,#44041,.F.) ;
#62740 = ORIENTED_EDGE('',*,*,#43992,.F.) ;
#62741 = ORIENTED_EDGE('',*,*,#44048,.T.) ;
#62742 = ORIENTED_EDGE('',*,*,#44047,.T.) ;
#62743 = ORIENTED_EDGE('',*,*,#43990,.F.) ;
#62744 = ORIENTED_EDGE('',*,*,#44034,.F.) ;
#62745 = ORIENTED_EDGE('',*,*,#44051,.F.) ;
#62746 = ORIENTED_EDGE('',*,*,#43988,.F.) ;
#62747 = ORIENTED_EDGE('',*,*,#44052,.T.) ;
#62748 = ORIENTED_EDGE('',*,*,#44053,.T.) ;
#62749 = ORIENTED_EDGE('',*,*,#44002,.F.) ;
#62750 = ORIENTED_EDGE('',*,*,#44054,.F.) ;
#62751 = ORIENTED_EDGE('',*,*,#44032,.F.) ;
#62752 = ORIENTED_EDGE('',*,*,#44000,.F.) ;
#62753 = ORIENTED_EDGE('',*,*,#44045,.T.) ;
#62754 = ORIENTED_EDGE('',*,*,#44044,.T.) ;
#62755 = ORIENTED_EDGE('',*,*,#43998,.F.) ;
#62756 = ORIENTED_EDGE('',*,*,#44037,.F.) ;
#62757 = ORIENTED_EDGE('',*,*,#44018,.T.) ;
#62758 = ORIENTED_EDGE('',*,*,#44055,.T.) ;
#62759 = ORIENTED_EDGE('',*,*,#44056,.T.) ;
#62760 = ORIENTED_EDGE('',*,*,#44057,.F.) ;
#62761 = ORIENTED_EDGE('',*,*,#44050,.T.) ;
#62762 = ORIENTED_EDGE('',*,*,#44058,.T.) ;
#62763 = ORIENTED_EDGE('',*,*,#44020,.T.) ;
#62764 = ORIENTED_EDGE('',*,*,#44059,.T.) ;
#62765 = ORIENTED_EDGE('',*,*,#44004,.F.) ;
#62766 = ORIENTED_EDGE('',*,*,#44049,.F.) ;
#62767 = ORIENTED_EDGE('',*,*,#44059,.F.) ;
#62768 = ORIENTED_EDGE('',*,*,#44019,.F.) ;
#62769 = ORIENTED_EDGE('',*,*,#44057,.T.) ;
#62770 = ORIENTED_EDGE('',*,*,#44060,.F.) ;
#62771 = ORIENTED_EDGE('',*,*,#44061,.F.) ;
#62772 = ORIENTED_EDGE('',*,*,#44053,.F.) ;
#62773 = ORIENTED_EDGE('',*,*,#44062,.F.) ;
#62774 = ORIENTED_EDGE('',*,*,#44027,.F.) ;
#62775 = ORIENTED_EDGE('',*,*,#44063,.T.) ;
#62776 = ORIENTED_EDGE('',*,*,#44052,.F.) ;
#62777 = ORIENTED_EDGE('',*,*,#44054,.T.) ;
#62778 = ORIENTED_EDGE('',*,*,#44064,.T.) ;
#62779 = ORIENTED_EDGE('',*,*,#44028,.T.) ;
#62780 = ORIENTED_EDGE('',*,*,#44062,.T.) ;
#62781 = ORIENTED_EDGE('',*,*,#44026,.T.) ;
#62782 = ORIENTED_EDGE('',*,*,#44065,.T.) ;
#62783 = ORIENTED_EDGE('',*,*,#44051,.T.) ;
#62784 = ORIENTED_EDGE('',*,*,#44063,.F.) ;
#62785 = ORIENTED_EDGE('',*,*,#44012,.F.) ;
#62786 = ORIENTED_EDGE('',*,*,#44005,.T.) ;
#62787 = ORIENTED_EDGE('',*,*,#44014,.F.) ;
#62788 = ORIENTED_EDGE('',*,*,#44056,.F.) ;
#62789 = ORIENTED_EDGE('',*,*,#43996,.F.) ;
#62790 = ORIENTED_EDGE('',*,*,#44060,.T.) ;
#62791 = ORIENTED_EDGE('',*,*,#44043,.T.) ;
#62792 = ORIENTED_EDGE('',*,*,#43999,.F.) ;
#62793 = ORIENTED_EDGE('',*,*,#44046,.T.) ;
#62794 = ORIENTED_EDGE('',*,*,#43991,.F.) ;
#62795 = ORIENTED_EDGE('',*,*,#43997,.F.) ;
#62796 = ORIENTED_EDGE('',*,*,#44055,.F.) ;
#62797 = ORIENTED_EDGE('',*,*,#44017,.T.) ;
#62798 = ORIENTED_EDGE('',*,*,#44038,.F.) ;
#62799 = ORIENTED_EDGE('',*,*,#44061,.T.) ;
#62800 = ORIENTED_EDGE('',*,*,#43987,.F.) ;
#62801 = ORIENTED_EDGE('',*,*,#44003,.F.) ;
#62802 = ORIENTED_EDGE('',*,*,#44021,.T.) ;
#62803 = ORIENTED_EDGE('',*,*,#44058,.F.) ;
#62804 = ORIENTED_EDGE('',*,*,#43993,.F.) ;
#62805 = ORIENTED_EDGE('',*,*,#44040,.F.) ;
#62806 = ORIENTED_EDGE('',*,*,#44029,.T.) ;
#62807 = ORIENTED_EDGE('',*,*,#44064,.F.) ;
#62808 = ORIENTED_EDGE('',*,*,#44001,.F.) ;
#62809 = ORIENTED_EDGE('',*,*,#44031,.F.) ;
#62810 = ORIENTED_EDGE('',*,*,#43989,.F.) ;
#62811 = ORIENTED_EDGE('',*,*,#44065,.F.) ;
#62812 = ORIENTED_EDGE('',*,*,#44025,.T.) ;
#62813 = ORIENTED_EDGE('',*,*,#44035,.F.) ;
#62814 = TOROIDAL_SURFACE('',#67765,1.75,0.15) ;
#62815 = TOROIDAL_SURFACE('',#67770,1.75,0.15) ;
#62816 = TOROIDAL_SURFACE('',#67775,1.64999999999999,0.15) ;
#62817 = TOROIDAL_SURFACE('',#67781,1.64999999999999,0.15) ;
#62818 = TOROIDAL_SURFACE('',#67785,1.64999999999999,0.15) ;
#62819 = TOROIDAL_SURFACE('',#67791,1.64999999999999,0.15) ;
#62820 = TOROIDAL_SURFACE('',#68047,0.3,0.15) ;
#62821 = TOROIDAL_SURFACE('',#68056,0.3,0.15) ;
#62822 = TOROIDAL_SURFACE('',#68083,0.3,0.15) ;
#62823 = TOROIDAL_SURFACE('',#68103,0.3,0.15) ;
#62824 = TOROIDAL_SURFACE('',#68105,1.6,0.15) ;
#62825 = TOROIDAL_SURFACE('',#68122,1.15,0.15) ;
#62826 = TOROIDAL_SURFACE('',#68124,0.3,0.15) ;
#62827 = TOROIDAL_SURFACE('',#68127,0.3,0.15) ;
#62828 = TOROIDAL_SURFACE('',#68144,0.3,0.15) ;
#62829 = TOROIDAL_SURFACE('',#68152,0.3,0.15) ;
#62830 = TOROIDAL_SURFACE('',#68171,1.6,0.15) ;
#62831 = TOROIDAL_SURFACE('',#68197,0.3,0.15) ;
#62832 = TOROIDAL_SURFACE('',#68199,0.3,0.15) ;
#62833 = TOROIDAL_SURFACE('',#68211,0.3,0.15) ;
#62834 = TOROIDAL_SURFACE('',#68213,0.3,0.15) ;
#62835 = TOROIDAL_SURFACE('',#68219,1.15,0.15) ;
#62836 = TOROIDAL_SURFACE('',#68223,0.3,0.15) ;
#62837 = TOROIDAL_SURFACE('',#68226,0.3,0.15) ;
#62838 = TOROIDAL_SURFACE('',#68243,0.3,0.15) ;
#62839 = TOROIDAL_SURFACE('',#68245,0.3,0.15) ;
#62840 = TOROIDAL_SURFACE('',#68247,0.3,0.15) ;
#62841 = TOROIDAL_SURFACE('',#68249,0.3,0.15) ;
#62842 = TOROIDAL_SURFACE('',#68259,0.3,0.15) ;
#62843 = TOROIDAL_SURFACE('',#68261,0.3,0.15) ;
#62844 = TOROIDAL_SURFACE('',#68267,0.3,0.15) ;
#62845 = TOROIDAL_SURFACE('',#68270,0.3,0.15) ;
#62846 = TOROIDAL_SURFACE('',#68287,0.3,0.15) ;
#62847 = TOROIDAL_SURFACE('',#68289,0.3,0.15) ;
#62848 = TOROIDAL_SURFACE('',#68291,0.3,0.15) ;
#62849 = TOROIDAL_SURFACE('',#68293,0.3,0.15) ;
#62850 = TOROIDAL_SURFACE('',#68303,0.3,0.15) ;
#62851 = TOROIDAL_SURFACE('',#68305,0.3,0.15) ;
#62852 = TOROIDAL_SURFACE('',#68311,0.3,0.15) ;
#62853 = TOROIDAL_SURFACE('',#68314,0.3,0.15) ;
#62854 = TOROIDAL_SURFACE('',#68331,0.3,0.15) ;
#62855 = TOROIDAL_SURFACE('',#68333,0.3,0.15) ;
#62856 = TOROIDAL_SURFACE('',#68335,0.3,0.15) ;
#62857 = TOROIDAL_SURFACE('',#68337,0.3,0.15) ;
#62858 = TOROIDAL_SURFACE('',#68347,0.3,0.15) ;
#62859 = TOROIDAL_SURFACE('',#68349,0.3,0.15) ;
#62860 = TOROIDAL_SURFACE('',#68355,0.3,0.15) ;
#62861 = TOROIDAL_SURFACE('',#68358,0.3,0.15) ;
#62862 = TOROIDAL_SURFACE('',#68375,0.3,0.15) ;
#62863 = TOROIDAL_SURFACE('',#68377,0.3,0.15) ;
#62864 = TOROIDAL_SURFACE('',#68379,0.3,0.15) ;
#62865 = TOROIDAL_SURFACE('',#68381,0.3,0.15) ;
#62866 = TOROIDAL_SURFACE('',#68391,0.3,0.15) ;
#62867 = TOROIDAL_SURFACE('',#68393,0.3,0.15) ;
#62868 = TOROIDAL_SURFACE('',#68399,0.3,0.15) ;
#62869 = TOROIDAL_SURFACE('',#68402,0.3,0.15) ;
#62870 = TOROIDAL_SURFACE('',#68419,0.3,0.15) ;
#62871 = TOROIDAL_SURFACE('',#68421,0.3,0.15) ;
#62872 = TOROIDAL_SURFACE('',#68423,0.3,0.15) ;
#62873 = TOROIDAL_SURFACE('',#68425,0.3,0.15) ;
#62874 = TOROIDAL_SURFACE('',#68435,0.3,0.15) ;
#62875 = TOROIDAL_SURFACE('',#68437,0.3,0.15) ;
#62876 = TOROIDAL_SURFACE('',#68443,0.3,0.15) ;
#62877 = TOROIDAL_SURFACE('',#68446,0.3,0.15) ;
#62878 = TOROIDAL_SURFACE('',#68463,0.3,0.15) ;
#62879 = TOROIDAL_SURFACE('',#68465,0.3,0.15) ;
#62880 = TOROIDAL_SURFACE('',#68467,0.3,0.15) ;
#62881 = TOROIDAL_SURFACE('',#68469,0.3,0.15) ;
#62882 = TOROIDAL_SURFACE('',#68479,0.3,0.15) ;
#62883 = TOROIDAL_SURFACE('',#68481,0.3,0.15) ;
#62884 = TOROIDAL_SURFACE('',#68487,0.3,0.15) ;
#62885 = TOROIDAL_SURFACE('',#68490,0.3,0.15) ;
#62886 = TOROIDAL_SURFACE('',#68507,0.3,0.15) ;
#62887 = TOROIDAL_SURFACE('',#68509,0.3,0.15) ;
#62888 = TOROIDAL_SURFACE('',#68511,0.3,0.15) ;
#62889 = TOROIDAL_SURFACE('',#68513,0.3,0.15) ;
#62890 = TOROIDAL_SURFACE('',#68523,0.3,0.15) ;
#62891 = TOROIDAL_SURFACE('',#68525,0.3,0.15) ;
#62892 = TOROIDAL_SURFACE('',#68531,0.3,0.15) ;
#62893 = TOROIDAL_SURFACE('',#68534,0.3,0.15) ;
#62894 = TOROIDAL_SURFACE('',#68551,0.3,0.15) ;
#62895 = TOROIDAL_SURFACE('',#68553,0.3,0.15) ;
#62896 = TOROIDAL_SURFACE('',#68555,0.3,0.15) ;
#62897 = TOROIDAL_SURFACE('',#68557,0.3,0.15) ;
#62898 = TOROIDAL_SURFACE('',#68567,0.3,0.15) ;
#62899 = TOROIDAL_SURFACE('',#68569,0.3,0.15) ;
#62900 = TOROIDAL_SURFACE('',#68575,0.3,0.15) ;
#62901 = TOROIDAL_SURFACE('',#68578,0.3,0.15) ;
#62902 = TOROIDAL_SURFACE('',#68595,0.3,0.15) ;
#62903 = TOROIDAL_SURFACE('',#68597,0.3,0.15) ;
#62904 = TOROIDAL_SURFACE('',#68599,0.3,0.15) ;
#62905 = TOROIDAL_SURFACE('',#68601,0.3,0.15) ;
#62906 = TOROIDAL_SURFACE('',#68611,0.3,0.15) ;
#62907 = TOROIDAL_SURFACE('',#68613,0.3,0.15) ;
#62908 = TOROIDAL_SURFACE('',#68619,0.3,0.15) ;
#62909 = TOROIDAL_SURFACE('',#68622,0.3,0.15) ;
#62910 = TOROIDAL_SURFACE('',#68639,0.3,0.15) ;
#62911 = TOROIDAL_SURFACE('',#68641,0.3,0.15) ;
#62912 = TOROIDAL_SURFACE('',#68643,0.3,0.15) ;
#62913 = TOROIDAL_SURFACE('',#68645,0.3,0.15) ;
#62914 = TOROIDAL_SURFACE('',#68655,0.3,0.15) ;
#62915 = TOROIDAL_SURFACE('',#68657,0.3,0.15) ;
#62916 = TOROIDAL_SURFACE('',#68663,0.3,0.15) ;
#62917 = TOROIDAL_SURFACE('',#68666,0.3,0.15) ;
#62918 = TOROIDAL_SURFACE('',#68683,0.3,0.15) ;
#62919 = TOROIDAL_SURFACE('',#68685,0.3,0.15) ;
#62920 = TOROIDAL_SURFACE('',#68687,0.3,0.15) ;
#62921 = TOROIDAL_SURFACE('',#68689,0.3,0.15) ;
#62922 = TOROIDAL_SURFACE('',#68699,0.3,0.15) ;
#62923 = TOROIDAL_SURFACE('',#68701,0.3,0.15) ;
#62924 = TOROIDAL_SURFACE('',#68707,0.3,0.15) ;
#62925 = TOROIDAL_SURFACE('',#68710,0.3,0.15) ;
#62926 = TOROIDAL_SURFACE('',#68727,0.3,0.15) ;
#62927 = TOROIDAL_SURFACE('',#68729,0.3,0.15) ;
#62928 = TOROIDAL_SURFACE('',#68731,0.3,0.15) ;
#62929 = TOROIDAL_SURFACE('',#68733,0.3,0.15) ;
#62930 = TOROIDAL_SURFACE('',#68743,0.3,0.15) ;
#62931 = TOROIDAL_SURFACE('',#68745,0.3,0.15) ;
#62932 = TOROIDAL_SURFACE('',#68786,1.4,0.1) ;
#62933 = TOROIDAL_SURFACE('',#68790,1.6,0.1) ;
#62934 = TOROIDAL_SURFACE('',#68801,3.1,0.1) ;
#62935 = TOROIDAL_SURFACE('',#68982,1.85,0.1) ;
#62936 = TOROIDAL_SURFACE('',#68984,0.2,0.1) ;
#62937 = TOROIDAL_SURFACE('',#68996,1.65,0.1) ;
#62938 = TOROIDAL_SURFACE('',#69006,0.2,0.1) ;
#62939 = TOROIDAL_SURFACE('',#69008,0.2,0.1) ;
#62940 = TOROIDAL_SURFACE('',#69012,1.85,0.1) ;
#62941 = TOROIDAL_SURFACE('',#69017,1.65,0.1) ;
#62942 = TOROIDAL_SURFACE('',#69025,0.2,0.1) ;
#62943 = TOROIDAL_SURFACE('',#69027,0.2,0.1) ;
#62944 = TOROIDAL_SURFACE('',#69039,0.2,0.1) ;
#62945 = TOROIDAL_SURFACE('',#69058,0.2,0.1) ;
#62946 = TOROIDAL_SURFACE('',#69077,0.2,0.1) ;
#62947 = TOROIDAL_SURFACE('',#69097,0.2,0.1) ;
#62948 = TOROIDAL_SURFACE('',#69099,0.2,0.1) ;
#62949 = TOROIDAL_SURFACE('',#69103,0.2,0.1) ;
#62950 = TOROIDAL_SURFACE('',#69113,0.2,0.1) ;
#62951 = TOROIDAL_SURFACE('',#69125,1.85,0.1) ;
#62952 = TOROIDAL_SURFACE('',#69132,0.2,0.1) ;
#62953 = TOROIDAL_SURFACE('',#69137,0.2,0.1) ;
#62954 = TOROIDAL_SURFACE('',#69139,1.65,0.1) ;
#62955 = TOROIDAL_SURFACE('',#69145,2.9,0.1) ;
#62956 = TOROIDAL_SURFACE('',#69154,0.2,0.1) ;
#62957 = TOROIDAL_SURFACE('',#69157,0.2,0.1) ;
#62958 = TOROIDAL_SURFACE('',#69163,2.9,0.1) ;
#62959 = TOROIDAL_SURFACE('',#69168,1.85,0.1) ;
#62960 = TOROIDAL_SURFACE('',#69179,0.2,0.1) ;
#62961 = TOROIDAL_SURFACE('',#69181,2.9,0.1) ;
#62962 = TOROIDAL_SURFACE('',#69185,1.65,0.1) ;
#62963 = TOROIDAL_SURFACE('',#69187,0.2,0.1) ;
#62964 = TOROIDAL_SURFACE('',#69190,1.9,0.1) ;
#62965 = TOROIDAL_SURFACE('',#69194,1.1,0.1) ;
#62966 = TOROIDAL_SURFACE('',#69199,1.9,0.1) ;
#62967 = TOROIDAL_SURFACE('',#69233,1.1,0.1) ;
#62968 = TOROIDAL_SURFACE('',#69307,3.33471270883832,0.1) ;
#62969 = TOROIDAL_SURFACE('',#69396,1.4,0.1) ;
#62970 = TOROIDAL_SURFACE('',#69400,1.6,0.1) ;
#62971 = TOROIDAL_SURFACE('',#69411,3.1,0.1) ;
#62972 = TOROIDAL_SURFACE('',#69592,1.85,0.1) ;
#62973 = TOROIDAL_SURFACE('',#69594,0.2,0.1) ;
#62974 = TOROIDAL_SURFACE('',#69606,1.65,0.1) ;
#62975 = TOROIDAL_SURFACE('',#69616,0.2,0.1) ;
#62976 = TOROIDAL_SURFACE('',#69618,0.2,0.1) ;
#62977 = TOROIDAL_SURFACE('',#69622,1.85,0.1) ;
#62978 = TOROIDAL_SURFACE('',#69627,1.65,0.1) ;
#62979 = TOROIDAL_SURFACE('',#69635,0.2,0.1) ;
#62980 = TOROIDAL_SURFACE('',#69637,0.2,0.1) ;
#62981 = TOROIDAL_SURFACE('',#69649,0.2,0.1) ;
#62982 = TOROIDAL_SURFACE('',#69668,0.2,0.1) ;
#62983 = TOROIDAL_SURFACE('',#69687,0.2,0.1) ;
#62984 = TOROIDAL_SURFACE('',#69707,0.2,0.1) ;
#62985 = TOROIDAL_SURFACE('',#69709,0.2,0.1) ;
#62986 = TOROIDAL_SURFACE('',#69713,0.2,0.1) ;
#62987 = TOROIDAL_SURFACE('',#69723,0.2,0.1) ;
#62988 = TOROIDAL_SURFACE('',#69735,1.85,0.1) ;
#62989 = TOROIDAL_SURFACE('',#69742,0.2,0.1) ;
#62990 = TOROIDAL_SURFACE('',#69747,0.2,0.1) ;
#62991 = TOROIDAL_SURFACE('',#69749,1.65,0.1) ;
#62992 = TOROIDAL_SURFACE('',#69755,2.9,0.1) ;
#62993 = TOROIDAL_SURFACE('',#69764,0.2,0.1) ;
#62994 = TOROIDAL_SURFACE('',#69767,0.2,0.1) ;
#62995 = TOROIDAL_SURFACE('',#69773,2.9,0.1) ;
#62996 = TOROIDAL_SURFACE('',#69778,1.85,0.1) ;
#62997 = TOROIDAL_SURFACE('',#69789,0.2,0.1) ;
#62998 = TOROIDAL_SURFACE('',#69791,2.9,0.1) ;
#62999 = TOROIDAL_SURFACE('',#69795,1.65,0.1) ;
#63000 = TOROIDAL_SURFACE('',#69797,0.2,0.1) ;
#63001 = TOROIDAL_SURFACE('',#69800,1.9,0.1) ;
#63002 = TOROIDAL_SURFACE('',#69804,1.1,0.1) ;
#63003 = TOROIDAL_SURFACE('',#69809,1.9,0.1) ;
#63004 = TOROIDAL_SURFACE('',#69843,1.1,0.1) ;
#63005 = TOROIDAL_SURFACE('',#69917,3.33471270883832,0.1) ;
#63006 = TOROIDAL_SURFACE('',#70006,1.4,0.1) ;
#63007 = TOROIDAL_SURFACE('',#70010,1.6,0.1) ;
#63008 = TOROIDAL_SURFACE('',#70021,3.1,0.1) ;
#63009 = TOROIDAL_SURFACE('',#70202,1.85,0.1) ;
#63010 = TOROIDAL_SURFACE('',#70204,0.2,0.1) ;
#63011 = TOROIDAL_SURFACE('',#70216,1.65,0.1) ;
#63012 = TOROIDAL_SURFACE('',#70226,0.2,0.1) ;
#63013 = TOROIDAL_SURFACE('',#70228,0.2,0.1) ;
#63014 = TOROIDAL_SURFACE('',#70232,1.85,0.1) ;
#63015 = TOROIDAL_SURFACE('',#70237,1.65,0.1) ;
#63016 = TOROIDAL_SURFACE('',#70245,0.2,0.1) ;
#63017 = TOROIDAL_SURFACE('',#70247,0.2,0.1) ;
#63018 = TOROIDAL_SURFACE('',#70259,0.2,0.1) ;
#63019 = TOROIDAL_SURFACE('',#70278,0.2,0.1) ;
#63020 = TOROIDAL_SURFACE('',#70297,0.2,0.1) ;
#63021 = TOROIDAL_SURFACE('',#70317,0.2,0.1) ;
#63022 = TOROIDAL_SURFACE('',#70319,0.2,0.1) ;
#63023 = TOROIDAL_SURFACE('',#70323,0.2,0.1) ;
#63024 = TOROIDAL_SURFACE('',#70333,0.2,0.1) ;
#63025 = TOROIDAL_SURFACE('',#70345,1.85,0.1) ;
#63026 = TOROIDAL_SURFACE('',#70352,0.2,0.1) ;
#63027 = TOROIDAL_SURFACE('',#70357,0.2,0.1) ;
#63028 = TOROIDAL_SURFACE('',#70359,1.65,0.1) ;
#63029 = TOROIDAL_SURFACE('',#70365,2.9,0.1) ;
#63030 = TOROIDAL_SURFACE('',#70374,0.2,0.1) ;
#63031 = TOROIDAL_SURFACE('',#70377,0.2,0.1) ;
#63032 = TOROIDAL_SURFACE('',#70383,2.9,0.1) ;
#63033 = TOROIDAL_SURFACE('',#70388,1.85,0.1) ;
#63034 = TOROIDAL_SURFACE('',#70399,0.2,0.1) ;
#63035 = TOROIDAL_SURFACE('',#70401,2.9,0.1) ;
#63036 = TOROIDAL_SURFACE('',#70405,1.65,0.1) ;
#63037 = TOROIDAL_SURFACE('',#70407,0.2,0.1) ;
#63038 = TOROIDAL_SURFACE('',#70410,1.9,0.1) ;
#63039 = TOROIDAL_SURFACE('',#70414,1.1,0.1) ;
#63040 = TOROIDAL_SURFACE('',#70419,1.9,0.1) ;
#63041 = TOROIDAL_SURFACE('',#70453,1.1,0.1) ;
#63042 = TOROIDAL_SURFACE('',#70527,3.33471270883832,0.1) ;
#63043 = TOROIDAL_SURFACE('',#70616,1.4,0.1) ;
#63044 = TOROIDAL_SURFACE('',#70620,1.6,0.1) ;
#63045 = TOROIDAL_SURFACE('',#70631,3.1,0.1) ;
#63046 = TOROIDAL_SURFACE('',#70812,1.85,0.1) ;
#63047 = TOROIDAL_SURFACE('',#70814,0.2,0.1) ;
#63048 = TOROIDAL_SURFACE('',#70826,1.65,0.1) ;
#63049 = TOROIDAL_SURFACE('',#70836,0.2,0.1) ;
#63050 = TOROIDAL_SURFACE('',#70838,0.2,0.1) ;
#63051 = TOROIDAL_SURFACE('',#70842,1.85,0.1) ;
#63052 = TOROIDAL_SURFACE('',#70847,1.65,0.1) ;
#63053 = TOROIDAL_SURFACE('',#70855,0.2,0.1) ;
#63054 = TOROIDAL_SURFACE('',#70857,0.2,0.1) ;
#63055 = TOROIDAL_SURFACE('',#70869,0.2,0.1) ;
#63056 = TOROIDAL_SURFACE('',#70888,0.2,0.1) ;
#63057 = TOROIDAL_SURFACE('',#70907,0.2,0.1) ;
#63058 = TOROIDAL_SURFACE('',#70927,0.2,0.1) ;
#63059 = TOROIDAL_SURFACE('',#70929,0.2,0.1) ;
#63060 = TOROIDAL_SURFACE('',#70933,0.2,0.1) ;
#63061 = TOROIDAL_SURFACE('',#70943,0.2,0.1) ;
#63062 = TOROIDAL_SURFACE('',#70955,1.85,0.1) ;
#63063 = TOROIDAL_SURFACE('',#70962,0.2,0.1) ;
#63064 = TOROIDAL_SURFACE('',#70967,0.2,0.1) ;
#63065 = TOROIDAL_SURFACE('',#70969,1.65,0.1) ;
#63066 = TOROIDAL_SURFACE('',#70975,2.9,0.1) ;
#63067 = TOROIDAL_SURFACE('',#70984,0.2,0.1) ;
#63068 = TOROIDAL_SURFACE('',#70987,0.2,0.1) ;
#63069 = TOROIDAL_SURFACE('',#70993,2.9,0.1) ;
#63070 = TOROIDAL_SURFACE('',#70998,1.85,0.1) ;
#63071 = TOROIDAL_SURFACE('',#71009,0.2,0.1) ;
#63072 = TOROIDAL_SURFACE('',#71011,2.9,0.1) ;
#63073 = TOROIDAL_SURFACE('',#71015,1.65,0.1) ;
#63074 = TOROIDAL_SURFACE('',#71017,0.2,0.1) ;
#63075 = TOROIDAL_SURFACE('',#71020,1.9,0.1) ;
#63076 = TOROIDAL_SURFACE('',#71024,1.1,0.1) ;
#63077 = TOROIDAL_SURFACE('',#71029,1.9,0.1) ;
#63078 = TOROIDAL_SURFACE('',#71063,1.1,0.1) ;
#63079 = TOROIDAL_SURFACE('',#71137,3.33471270883832,0.1) ;
#63080 = TOROIDAL_SURFACE('',#71226,1.4,0.1) ;
#63081 = TOROIDAL_SURFACE('',#71230,1.6,0.1) ;
#63082 = TOROIDAL_SURFACE('',#71241,3.1,0.1) ;
#63083 = TOROIDAL_SURFACE('',#71422,1.85,0.1) ;
#63084 = TOROIDAL_SURFACE('',#71424,0.2,0.1) ;
#63085 = TOROIDAL_SURFACE('',#71436,1.65,0.1) ;
#63086 = TOROIDAL_SURFACE('',#71446,0.2,0.1) ;
#63087 = TOROIDAL_SURFACE('',#71448,0.2,0.1) ;
#63088 = TOROIDAL_SURFACE('',#71452,1.85,0.1) ;
#63089 = TOROIDAL_SURFACE('',#71457,1.65,0.1) ;
#63090 = TOROIDAL_SURFACE('',#71465,0.2,0.1) ;
#63091 = TOROIDAL_SURFACE('',#71467,0.2,0.1) ;
#63092 = TOROIDAL_SURFACE('',#71479,0.2,0.1) ;
#63093 = TOROIDAL_SURFACE('',#71498,0.2,0.1) ;
#63094 = TOROIDAL_SURFACE('',#71517,0.2,0.1) ;
#63095 = TOROIDAL_SURFACE('',#71537,0.2,0.1) ;
#63096 = TOROIDAL_SURFACE('',#71539,0.2,0.1) ;
#63097 = TOROIDAL_SURFACE('',#71543,0.2,0.1) ;
#63098 = TOROIDAL_SURFACE('',#71553,0.2,0.1) ;
#63099 = TOROIDAL_SURFACE('',#71565,1.85,0.1) ;
#63100 = TOROIDAL_SURFACE('',#71572,0.2,0.1) ;
#63101 = TOROIDAL_SURFACE('',#71577,0.2,0.1) ;
#63102 = TOROIDAL_SURFACE('',#71579,1.65,0.1) ;
#63103 = TOROIDAL_SURFACE('',#71585,2.9,0.1) ;
#63104 = TOROIDAL_SURFACE('',#71594,0.2,0.1) ;
#63105 = TOROIDAL_SURFACE('',#71597,0.2,0.1) ;
#63106 = TOROIDAL_SURFACE('',#71603,2.9,0.1) ;
#63107 = TOROIDAL_SURFACE('',#71608,1.85,0.1) ;
#63108 = TOROIDAL_SURFACE('',#71619,0.2,0.1) ;
#63109 = TOROIDAL_SURFACE('',#71621,2.9,0.1) ;
#63110 = TOROIDAL_SURFACE('',#71625,1.65,0.1) ;
#63111 = TOROIDAL_SURFACE('',#71627,0.2,0.1) ;
#63112 = TOROIDAL_SURFACE('',#71630,1.9,0.1) ;
#63113 = TOROIDAL_SURFACE('',#71634,1.1,0.1) ;
#63114 = TOROIDAL_SURFACE('',#71639,1.9,0.1) ;
#63115 = TOROIDAL_SURFACE('',#71673,1.1,0.1) ;
#63116 = TOROIDAL_SURFACE('',#71747,3.33471270883832,0.1) ;
#63117 = TOROIDAL_SURFACE('',#71867,0.9,0.1) ;
#63118 = TOROIDAL_SURFACE('',#71872,1.1,0.1) ;
#63119 = TOROIDAL_SURFACE('',#71884,0.9,0.1) ;
#63120 = TOROIDAL_SURFACE('',#71889,1.1,0.1) ;
#63121 = TOROIDAL_SURFACE('',#71901,0.9,0.1) ;
#63122 = TOROIDAL_SURFACE('',#71906,1.1,0.1) ;
#63123 = TOROIDAL_SURFACE('',#71918,0.9,0.1) ;
#63124 = TOROIDAL_SURFACE('',#71923,1.1,0.1) ;
#63125 = TOROIDAL_SURFACE('',#71935,0.9,0.1) ;
#63126 = TOROIDAL_SURFACE('',#71940,1.1,0.1) ;
#63127 = TOROIDAL_SURFACE('',#71952,0.9,0.1) ;
#63128 = TOROIDAL_SURFACE('',#71957,1.1,0.1) ;
#63129 = TOROIDAL_SURFACE('',#71969,0.9,0.1) ;
#63130 = TOROIDAL_SURFACE('',#71974,1.1,0.1) ;
#63131 = TOROIDAL_SURFACE('',#71986,0.9,0.1) ;
#63132 = TOROIDAL_SURFACE('',#71991,1.1,0.1) ;
#63133 = TOROIDAL_SURFACE('',#72003,0.9,0.1) ;
#63134 = TOROIDAL_SURFACE('',#72008,0.2,0.1) ;
#63135 = TOROIDAL_SURFACE('',#72013,0.2,0.1) ;
#63136 = TOROIDAL_SURFACE('',#72018,0.2,0.1) ;
#63137 = TOROIDAL_SURFACE('',#72023,0.2,0.1) ;
#63138 = TOROIDAL_SURFACE('',#72028,0.2,0.1) ;
#63139 = TOROIDAL_SURFACE('',#72033,0.2,0.1) ;
#63140 = TOROIDAL_SURFACE('',#72038,0.2,0.1) ;
#63141 = TOROIDAL_SURFACE('',#72043,0.2,0.1) ;
#63142 = TOROIDAL_SURFACE('',#72048,0.2,0.1) ;
#63143 = TOROIDAL_SURFACE('',#72053,1.1,0.1) ;
#63144 = TOROIDAL_SURFACE('',#72092,0.9,0.1) ;
#63145 = TOROIDAL_SURFACE('',#72097,0.2,0.1) ;
#63146 = TOROIDAL_SURFACE('',#72102,1.1,0.1) ;
#63147 = TOROIDAL_SURFACE('',#72500,0.2,0.1) ;
#63148 = TOROIDAL_SURFACE('',#72516,0.2,0.1) ;
#63149 = TOROIDAL_SURFACE('',#72518,0.2,0.1) ;
#63150 = TOROIDAL_SURFACE('',#72521,0.2,0.1) ;
#63151 = TOROIDAL_SURFACE('',#72534,0.2,0.1) ;
#63152 = TOROIDAL_SURFACE('',#72554,0.2,0.1) ;
#63153 = TOROIDAL_SURFACE('',#72565,0.2,0.1) ;
#63154 = TOROIDAL_SURFACE('',#72572,0.2,0.1) ;
#63155 = TOROIDAL_SURFACE('',#72578,0.2,0.1) ;
#63156 = TOROIDAL_SURFACE('',#72581,0.2,0.1) ;
#63157 = TOROIDAL_SURFACE('',#72595,0.2,0.1) ;
#63158 = TOROIDAL_SURFACE('',#72605,0.2,0.1) ;
#63159 = TOROIDAL_SURFACE('',#72627,0.2,0.1) ;
#63160 = TOROIDAL_SURFACE('',#72637,0.2,0.1) ;
#63161 = TOROIDAL_SURFACE('',#72655,0.2,0.1) ;
#63162 = TOROIDAL_SURFACE('',#72663,0.2,0.1) ;
#63163 = TOROIDAL_SURFACE('',#72677,1.75625,0.1) ;
#63164 = TOROIDAL_SURFACE('',#72700,0.2,0.1) ;
#63165 = TOROIDAL_SURFACE('',#72702,0.2,0.1) ;
#63166 = TOROIDAL_SURFACE('',#72716,0.2,0.1) ;
#63167 = TOROIDAL_SURFACE('',#72718,0.2,0.1) ;
#63168 = TOROIDAL_SURFACE('',#72723,0.2,0.1) ;
#63169 = TOROIDAL_SURFACE('',#72729,0.2,0.1) ;
#63170 = TOROIDAL_SURFACE('',#72731,0.2,0.1) ;
#63171 = TOROIDAL_SURFACE('',#72735,1.55625,0.1) ;
#63172 = TOROIDAL_SURFACE('',#72737,0.199999999999999,0.1) ;
#63173 = TOROIDAL_SURFACE('',#72739,0.2,0.1) ;
#63174 = TOROIDAL_SURFACE('',#72747,0.2,0.1) ;
#63175 = TOROIDAL_SURFACE('',#72755,0.2,0.1) ;
#63176 = TOROIDAL_SURFACE('',#72854,0.3,0.1) ;
#63177 = TOROIDAL_SURFACE('',#72866,0.9,0.1) ;
#63178 = TOROIDAL_SURFACE('',#72867,0.9,0.1) ;
#63179 = TOROIDAL_SURFACE('',#72879,0.3,0.1) ;
#63180 = TOROIDAL_SURFACE('',#73567,0.2,0.1) ;
#63181 = TOROIDAL_SURFACE('',#73583,0.2,0.1) ;
#63182 = TOROIDAL_SURFACE('',#73585,0.2,0.1) ;
#63183 = TOROIDAL_SURFACE('',#73588,0.2,0.1) ;
#63184 = TOROIDAL_SURFACE('',#73601,0.2,0.1) ;
#63185 = TOROIDAL_SURFACE('',#73621,0.2,0.1) ;
#63186 = TOROIDAL_SURFACE('',#73632,0.2,0.1) ;
#63187 = TOROIDAL_SURFACE('',#73639,0.2,0.1) ;
#63188 = TOROIDAL_SURFACE('',#73645,0.2,0.1) ;
#63189 = TOROIDAL_SURFACE('',#73648,0.2,0.1) ;
#63190 = TOROIDAL_SURFACE('',#73658,0.2,0.1) ;
#63191 = TOROIDAL_SURFACE('',#73666,0.2,0.1) ;
#63192 = TOROIDAL_SURFACE('',#73680,1.75625,0.1) ;
#63193 = TOROIDAL_SURFACE('',#73703,0.2,0.1) ;
#63194 = TOROIDAL_SURFACE('',#73705,0.2,0.1) ;
#63195 = TOROIDAL_SURFACE('',#73719,0.2,0.1) ;
#63196 = TOROIDAL_SURFACE('',#73721,0.2,0.1) ;
#63197 = TOROIDAL_SURFACE('',#73726,0.2,0.1) ;
#63198 = TOROIDAL_SURFACE('',#73732,0.2,0.1) ;
#63199 = TOROIDAL_SURFACE('',#73734,0.2,0.1) ;
#63200 = TOROIDAL_SURFACE('',#73738,1.55625,0.1) ;
#63201 = TOROIDAL_SURFACE('',#73740,0.199999999999999,0.1) ;
#63202 = TOROIDAL_SURFACE('',#73742,0.2,0.1) ;
#63203 = TOROIDAL_SURFACE('',#73750,0.2,0.1) ;
#63204 = TOROIDAL_SURFACE('',#73758,0.2,0.1) ;
#63205 = TOROIDAL_SURFACE('',#73772,0.2,0.1) ;
#63206 = TOROIDAL_SURFACE('',#73774,0.2,0.1) ;
#63207 = TOROIDAL_SURFACE('',#73779,0.2,0.1) ;
#63208 = TOROIDAL_SURFACE('',#73785,0.2,0.1) ;
#63209 = TOROIDAL_SURFACE('',#73787,0.2,0.1) ;
#63210 = TOROIDAL_SURFACE('',#73791,1.55625,0.1) ;
#63211 = TOROIDAL_SURFACE('',#73793,0.199999999999999,0.1) ;
#63212 = TOROIDAL_SURFACE('',#73795,0.2,0.1) ;
#63213 = TOROIDAL_SURFACE('',#73803,0.2,0.1) ;
#63214 = TOROIDAL_SURFACE('',#73811,0.2,0.1) ;
#63215 = TOROIDAL_SURFACE('',#73825,0.2,0.1) ;
#63216 = TOROIDAL_SURFACE('',#73827,0.2,0.1) ;
#63217 = TOROIDAL_SURFACE('',#73832,0.2,0.1) ;
#63218 = TOROIDAL_SURFACE('',#73838,0.2,0.1) ;
#63219 = TOROIDAL_SURFACE('',#73840,0.2,0.1) ;
#63220 = TOROIDAL_SURFACE('',#73844,1.55625,0.1) ;
#63221 = TOROIDAL_SURFACE('',#73846,0.199999999999999,0.1) ;
#63222 = TOROIDAL_SURFACE('',#73848,0.2,0.1) ;
#63223 = TOROIDAL_SURFACE('',#73856,0.2,0.1) ;
#63224 = TOROIDAL_SURFACE('',#73864,0.2,0.1) ;
#63225 = TOROIDAL_SURFACE('',#73878,0.2,0.1) ;
#63226 = TOROIDAL_SURFACE('',#73880,0.2,0.1) ;
#63227 = TOROIDAL_SURFACE('',#73885,0.2,0.1) ;
#63228 = TOROIDAL_SURFACE('',#73891,0.2,0.1) ;
#63229 = TOROIDAL_SURFACE('',#73893,0.2,0.1) ;
#63230 = TOROIDAL_SURFACE('',#73897,1.55625,0.1) ;
#63231 = TOROIDAL_SURFACE('',#73899,0.199999999999999,0.1) ;
#63232 = TOROIDAL_SURFACE('',#73901,0.2,0.1) ;
#63233 = TOROIDAL_SURFACE('',#73909,0.2,0.1) ;
#63234 = TOROIDAL_SURFACE('',#73917,0.2,0.1) ;
#63235 = TOROIDAL_SURFACE('',#73931,0.2,0.1) ;
#63236 = TOROIDAL_SURFACE('',#73933,0.2,0.1) ;
#63237 = TOROIDAL_SURFACE('',#73938,0.2,0.1) ;
#63238 = TOROIDAL_SURFACE('',#73944,0.2,0.1) ;
#63239 = TOROIDAL_SURFACE('',#73946,0.2,0.1) ;
#63240 = TOROIDAL_SURFACE('',#73950,1.55625,0.1) ;
#63241 = TOROIDAL_SURFACE('',#73952,0.199999999999999,0.1) ;
#63242 = TOROIDAL_SURFACE('',#73954,0.2,0.1) ;
#63243 = TOROIDAL_SURFACE('',#73962,0.2,0.1) ;
#63244 = TOROIDAL_SURFACE('',#73970,0.2,0.1) ;
#63245 = TOROIDAL_SURFACE('',#73984,0.2,0.1) ;
#63246 = TOROIDAL_SURFACE('',#73986,0.2,0.1) ;
#63247 = TOROIDAL_SURFACE('',#73991,0.2,0.1) ;
#63248 = TOROIDAL_SURFACE('',#73997,0.2,0.1) ;
#63249 = TOROIDAL_SURFACE('',#73999,0.2,0.1) ;
#63250 = TOROIDAL_SURFACE('',#74003,1.55625,0.1) ;
#63251 = TOROIDAL_SURFACE('',#74005,0.199999999999999,0.1) ;
#63252 = TOROIDAL_SURFACE('',#74007,0.2,0.1) ;
#63253 = TOROIDAL_SURFACE('',#74015,0.2,0.1) ;
#63254 = TOROIDAL_SURFACE('',#74023,0.2,0.1) ;
#63255 = TOROIDAL_SURFACE('',#74037,0.2,0.1) ;
#63256 = TOROIDAL_SURFACE('',#74039,0.2,0.1) ;
#63257 = TOROIDAL_SURFACE('',#74044,0.2,0.1) ;
#63258 = TOROIDAL_SURFACE('',#74050,0.2,0.1) ;
#63259 = TOROIDAL_SURFACE('',#74052,0.2,0.1) ;
#63260 = TOROIDAL_SURFACE('',#74056,1.55625,0.1) ;
#63261 = TOROIDAL_SURFACE('',#74058,0.199999999999999,0.1) ;
#63262 = TOROIDAL_SURFACE('',#74060,0.2,0.1) ;
#63263 = TOROIDAL_SURFACE('',#74068,0.2,0.1) ;
#63264 = TOROIDAL_SURFACE('',#74076,0.2,0.1) ;
#63265 = TOROIDAL_SURFACE('',#74090,0.2,0.1) ;
#63266 = TOROIDAL_SURFACE('',#74092,0.2,0.1) ;
#63267 = TOROIDAL_SURFACE('',#74097,0.2,0.1) ;
#63268 = TOROIDAL_SURFACE('',#74103,0.2,0.1) ;
#63269 = TOROIDAL_SURFACE('',#74105,0.2,0.1) ;
#63270 = TOROIDAL_SURFACE('',#74109,1.55625,0.1) ;
#63271 = TOROIDAL_SURFACE('',#74111,0.199999999999999,0.1) ;
#63272 = TOROIDAL_SURFACE('',#74113,0.2,0.1) ;
#63273 = TOROIDAL_SURFACE('',#74121,0.2,0.1) ;
#63274 = TOROIDAL_SURFACE('',#74129,0.2,0.1) ;
#63275 = TOROIDAL_SURFACE('',#74143,0.2,0.1) ;
#63276 = TOROIDAL_SURFACE('',#74145,0.2,0.1) ;
#63277 = TOROIDAL_SURFACE('',#74150,0.2,0.1) ;
#63278 = TOROIDAL_SURFACE('',#74156,0.2,0.1) ;
#63279 = TOROIDAL_SURFACE('',#74158,0.2,0.1) ;
#63280 = TOROIDAL_SURFACE('',#74162,1.55625,0.1) ;
#63281 = TOROIDAL_SURFACE('',#74164,0.199999999999999,0.1) ;
#63282 = TOROIDAL_SURFACE('',#74166,0.2,0.1) ;
#63283 = TOROIDAL_SURFACE('',#74174,0.2,0.1) ;
#63284 = TOROIDAL_SURFACE('',#74182,0.2,0.1) ;
#63285 = TOROIDAL_SURFACE('',#74197,0.2,0.1) ;
#63286 = TOROIDAL_SURFACE('',#74213,0.2,0.1) ;
#63287 = TOROIDAL_SURFACE('',#74215,0.2,0.1) ;
#63288 = TOROIDAL_SURFACE('',#74218,0.2,0.1) ;
#63289 = TOROIDAL_SURFACE('',#74231,0.2,0.1) ;
#63290 = TOROIDAL_SURFACE('',#74251,0.2,0.1) ;
#63291 = TOROIDAL_SURFACE('',#74262,0.2,0.1) ;
#63292 = TOROIDAL_SURFACE('',#74269,0.2,0.1) ;
#63293 = TOROIDAL_SURFACE('',#74275,0.2,0.1) ;
#63294 = TOROIDAL_SURFACE('',#74278,0.2,0.1) ;
#63295 = TOROIDAL_SURFACE('',#74288,0.2,0.1) ;
#63296 = TOROIDAL_SURFACE('',#74296,0.2,0.1) ;
#63297 = TOROIDAL_SURFACE('',#74310,1.75625,0.1) ;
#63298 = TOROIDAL_SURFACE('',#74333,0.2,0.1) ;
#63299 = TOROIDAL_SURFACE('',#74335,0.2,0.1) ;
#63300 = TOROIDAL_SURFACE('',#74350,0.2,0.1) ;
#63301 = TOROIDAL_SURFACE('',#74366,0.2,0.1) ;
#63302 = TOROIDAL_SURFACE('',#74368,0.2,0.1) ;
#63303 = TOROIDAL_SURFACE('',#74371,0.2,0.1) ;
#63304 = TOROIDAL_SURFACE('',#74384,0.2,0.1) ;
#63305 = TOROIDAL_SURFACE('',#74404,0.2,0.1) ;
#63306 = TOROIDAL_SURFACE('',#74415,0.2,0.1) ;
#63307 = TOROIDAL_SURFACE('',#74422,0.2,0.1) ;
#63308 = TOROIDAL_SURFACE('',#74428,0.2,0.1) ;
#63309 = TOROIDAL_SURFACE('',#74431,0.2,0.1) ;
#63310 = TOROIDAL_SURFACE('',#74441,0.2,0.1) ;
#63311 = TOROIDAL_SURFACE('',#74449,0.2,0.1) ;
#63312 = TOROIDAL_SURFACE('',#74463,1.75625,0.1) ;
#63313 = TOROIDAL_SURFACE('',#74486,0.2,0.1) ;
#63314 = TOROIDAL_SURFACE('',#74488,0.2,0.1) ;
#63315 = TOROIDAL_SURFACE('',#74503,0.2,0.1) ;
#63316 = TOROIDAL_SURFACE('',#74519,0.2,0.1) ;
#63317 = TOROIDAL_SURFACE('',#74521,0.2,0.1) ;
#63318 = TOROIDAL_SURFACE('',#74524,0.2,0.1) ;
#63319 = TOROIDAL_SURFACE('',#74537,0.2,0.1) ;
#63320 = TOROIDAL_SURFACE('',#74557,0.2,0.1) ;
#63321 = TOROIDAL_SURFACE('',#74568,0.2,0.1) ;
#63322 = TOROIDAL_SURFACE('',#74575,0.2,0.1) ;
#63323 = TOROIDAL_SURFACE('',#74581,0.2,0.1) ;
#63324 = TOROIDAL_SURFACE('',#74584,0.2,0.1) ;
#63325 = TOROIDAL_SURFACE('',#74594,0.2,0.1) ;
#63326 = TOROIDAL_SURFACE('',#74602,0.2,0.1) ;
#63327 = TOROIDAL_SURFACE('',#74616,1.75625,0.1) ;
#63328 = TOROIDAL_SURFACE('',#74639,0.2,0.1) ;
#63329 = TOROIDAL_SURFACE('',#74641,0.2,0.1) ;
#63330 = TOROIDAL_SURFACE('',#74656,0.2,0.1) ;
#63331 = TOROIDAL_SURFACE('',#74672,0.2,0.1) ;
#63332 = TOROIDAL_SURFACE('',#74674,0.2,0.1) ;
#63333 = TOROIDAL_SURFACE('',#74677,0.2,0.1) ;
#63334 = TOROIDAL_SURFACE('',#74690,0.2,0.1) ;
#63335 = TOROIDAL_SURFACE('',#74710,0.2,0.1) ;
#63336 = TOROIDAL_SURFACE('',#74721,0.2,0.1) ;
#63337 = TOROIDAL_SURFACE('',#74728,0.2,0.1) ;
#63338 = TOROIDAL_SURFACE('',#74734,0.2,0.1) ;
#63339 = TOROIDAL_SURFACE('',#74737,0.2,0.1) ;
#63340 = TOROIDAL_SURFACE('',#74747,0.2,0.1) ;
#63341 = TOROIDAL_SURFACE('',#74755,0.2,0.1) ;
#63342 = TOROIDAL_SURFACE('',#74769,1.75625,0.1) ;
#63343 = TOROIDAL_SURFACE('',#74792,0.2,0.1) ;
#63344 = TOROIDAL_SURFACE('',#74794,0.2,0.1) ;
#63345 = TOROIDAL_SURFACE('',#74809,0.2,0.1) ;
#63346 = TOROIDAL_SURFACE('',#74825,0.2,0.1) ;
#63347 = TOROIDAL_SURFACE('',#74827,0.2,0.1) ;
#63348 = TOROIDAL_SURFACE('',#74830,0.2,0.1) ;
#63349 = TOROIDAL_SURFACE('',#74843,0.2,0.1) ;
#63350 = TOROIDAL_SURFACE('',#74863,0.2,0.1) ;
#63351 = TOROIDAL_SURFACE('',#74874,0.2,0.1) ;
#63352 = TOROIDAL_SURFACE('',#74881,0.2,0.1) ;
#63353 = TOROIDAL_SURFACE('',#74887,0.2,0.1) ;
#63354 = TOROIDAL_SURFACE('',#74890,0.2,0.1) ;
#63355 = TOROIDAL_SURFACE('',#74900,0.2,0.1) ;
#63356 = TOROIDAL_SURFACE('',#74908,0.2,0.1) ;
#63357 = TOROIDAL_SURFACE('',#74922,1.75625,0.1) ;
#63358 = TOROIDAL_SURFACE('',#74945,0.2,0.1) ;
#63359 = TOROIDAL_SURFACE('',#74947,0.2,0.1) ;
#63360 = TOROIDAL_SURFACE('',#74962,0.2,0.1) ;
#63361 = TOROIDAL_SURFACE('',#74978,0.2,0.1) ;
#63362 = TOROIDAL_SURFACE('',#74980,0.2,0.1) ;
#63363 = TOROIDAL_SURFACE('',#74983,0.2,0.1) ;
#63364 = TOROIDAL_SURFACE('',#74996,0.2,0.1) ;
#63365 = TOROIDAL_SURFACE('',#75016,0.2,0.1) ;
#63366 = TOROIDAL_SURFACE('',#75027,0.2,0.1) ;
#63367 = TOROIDAL_SURFACE('',#75034,0.2,0.1) ;
#63368 = TOROIDAL_SURFACE('',#75040,0.2,0.1) ;
#63369 = TOROIDAL_SURFACE('',#75043,0.2,0.1) ;
#63370 = TOROIDAL_SURFACE('',#75053,0.2,0.1) ;
#63371 = TOROIDAL_SURFACE('',#75061,0.2,0.1) ;
#63372 = TOROIDAL_SURFACE('',#75075,1.75625,0.1) ;
#63373 = TOROIDAL_SURFACE('',#75098,0.2,0.1) ;
#63374 = TOROIDAL_SURFACE('',#75100,0.2,0.1) ;
#63375 = TOROIDAL_SURFACE('',#75115,0.2,0.1) ;
#63376 = TOROIDAL_SURFACE('',#75131,0.2,0.1) ;
#63377 = TOROIDAL_SURFACE('',#75133,0.2,0.1) ;
#63378 = TOROIDAL_SURFACE('',#75136,0.2,0.1) ;
#63379 = TOROIDAL_SURFACE('',#75149,0.2,0.1) ;
#63380 = TOROIDAL_SURFACE('',#75169,0.2,0.1) ;
#63381 = TOROIDAL_SURFACE('',#75180,0.2,0.1) ;
#63382 = TOROIDAL_SURFACE('',#75187,0.2,0.1) ;
#63383 = TOROIDAL_SURFACE('',#75193,0.2,0.1) ;
#63384 = TOROIDAL_SURFACE('',#75196,0.2,0.1) ;
#63385 = TOROIDAL_SURFACE('',#75206,0.2,0.1) ;
#63386 = TOROIDAL_SURFACE('',#75214,0.2,0.1) ;
#63387 = TOROIDAL_SURFACE('',#75228,1.75625,0.1) ;
#63388 = TOROIDAL_SURFACE('',#75251,0.2,0.1) ;
#63389 = TOROIDAL_SURFACE('',#75253,0.2,0.1) ;
#63390 = TOROIDAL_SURFACE('',#75268,0.2,0.1) ;
#63391 = TOROIDAL_SURFACE('',#75284,0.2,0.1) ;
#63392 = TOROIDAL_SURFACE('',#75286,0.2,0.1) ;
#63393 = TOROIDAL_SURFACE('',#75289,0.2,0.1) ;
#63394 = TOROIDAL_SURFACE('',#75302,0.2,0.1) ;
#63395 = TOROIDAL_SURFACE('',#75322,0.2,0.1) ;
#63396 = TOROIDAL_SURFACE('',#75333,0.2,0.1) ;
#63397 = TOROIDAL_SURFACE('',#75340,0.2,0.1) ;
#63398 = TOROIDAL_SURFACE('',#75346,0.2,0.1) ;
#63399 = TOROIDAL_SURFACE('',#75349,0.2,0.1) ;
#63400 = TOROIDAL_SURFACE('',#75359,0.2,0.1) ;
#63401 = TOROIDAL_SURFACE('',#75367,0.2,0.1) ;
#63402 = TOROIDAL_SURFACE('',#75381,1.75625,0.1) ;
#63403 = TOROIDAL_SURFACE('',#75404,0.2,0.1) ;
#63404 = TOROIDAL_SURFACE('',#75406,0.2,0.1) ;
#63405 = TOROIDAL_SURFACE('',#76273,0.3,0.1) ;
#63406 = TOROIDAL_SURFACE('',#76285,0.9,0.1) ;
#63407 = TOROIDAL_SURFACE('',#76286,0.9,0.1) ;
#63408 = TOROIDAL_SURFACE('',#76298,0.3,0.1) ;
#63409 = TOROIDAL_SURFACE('',#76317,0.3,0.1) ;
#63410 = TOROIDAL_SURFACE('',#76329,0.9,0.1) ;
#63411 = TOROIDAL_SURFACE('',#76330,0.9,0.1) ;
#63412 = TOROIDAL_SURFACE('',#76342,0.3,0.1) ;
#63413 = TOROIDAL_SURFACE('',#76361,0.3,0.1) ;
#63414 = TOROIDAL_SURFACE('',#76373,0.9,0.1) ;
#63415 = TOROIDAL_SURFACE('',#76374,0.9,0.1) ;
#63416 = TOROIDAL_SURFACE('',#76386,0.3,0.1) ;
#63417 = TOROIDAL_SURFACE('',#76405,0.3,0.1) ;
#63418 = TOROIDAL_SURFACE('',#76417,0.9,0.1) ;
#63419 = TOROIDAL_SURFACE('',#76418,0.9,0.1) ;
#63420 = TOROIDAL_SURFACE('',#76430,0.3,0.1) ;
#63421 = TOROIDAL_SURFACE('',#76449,0.3,0.1) ;
#63422 = TOROIDAL_SURFACE('',#76461,0.9,0.1) ;
#63423 = TOROIDAL_SURFACE('',#76462,0.9,0.1) ;
#63424 = TOROIDAL_SURFACE('',#76474,0.3,0.1) ;
#63425 = TOROIDAL_SURFACE('',#76493,0.3,0.1) ;
#63426 = TOROIDAL_SURFACE('',#76505,0.9,0.1) ;
#63427 = TOROIDAL_SURFACE('',#76506,0.9,0.1) ;
#63428 = TOROIDAL_SURFACE('',#76518,0.3,0.1) ;
#63429 = TOROIDAL_SURFACE('',#76537,0.3,0.1) ;
#63430 = TOROIDAL_SURFACE('',#76549,0.9,0.1) ;
#63431 = TOROIDAL_SURFACE('',#76550,0.9,0.1) ;
#63432 = TOROIDAL_SURFACE('',#76562,0.3,0.1) ;
#63433 = TOROIDAL_SURFACE('',#76581,0.3,0.1) ;
#63434 = TOROIDAL_SURFACE('',#76593,0.9,0.1) ;
#63435 = TOROIDAL_SURFACE('',#76594,0.9,0.1) ;
#63436 = TOROIDAL_SURFACE('',#76606,0.3,0.1) ;
#63437 = TOROIDAL_SURFACE('',#76625,0.3,0.1) ;
#63438 = TOROIDAL_SURFACE('',#76637,0.9,0.1) ;
#63439 = TOROIDAL_SURFACE('',#76638,0.9,0.1) ;
#63440 = TOROIDAL_SURFACE('',#76650,0.3,0.1) ;
#63441 = TOROIDAL_SURFACE('',#76702,1.6,0.1) ;
#63442 = TOROIDAL_SURFACE('',#76783,1.6,0.1) ;
#63443 = TOROIDAL_SURFACE('',#76787,2.53,0.27) ;
#63444 = ADVANCED_FACE('',(#16159),#62814,.T.) ;
#63445 = ADVANCED_FACE('',(#16160),#62815,.T.) ;
#63446 = ADVANCED_FACE('',(#16161),#62816,.T.) ;
#63447 = ADVANCED_FACE('',(#16162),#62817,.T.) ;
#63448 = ADVANCED_FACE('',(#16163),#62818,.T.) ;
#63449 = ADVANCED_FACE('',(#16164),#62819,.T.) ;
#63450 = ADVANCED_FACE('',(#16165),#16128,.F.) ;
#63451 = ADVANCED_FACE('',(#16166),#5947,.F.) ;
#63452 = ADVANCED_FACE('',(#16167),#16129,.F.) ;
#63453 = ADVANCED_FACE('',(#16168),#5948,.F.) ;
#63454 = ADVANCED_FACE('',(#16169),#5949,.F.) ;
#63455 = ADVANCED_FACE('',(#16170,#4989,#4990),#5065,.F.) ;
#63456 = ADVANCED_FACE('',(#16171,#4991,#4992),#5066,.T.) ;
#63457 = ADVANCED_FACE('',(#16172,#4993,#4994,#4995,#4996),#5067,.T.) ;
#63458 = ADVANCED_FACE('',(#16173,#4997,#4998,#4999,#5000),#5068,.F.) ;
#63459 = ADVANCED_FACE('',(#16174,#5001,#5002,#5003,#5004,#5005,#5006,#5007),
#5069,.T.) ;
#63460 = ADVANCED_FACE('',(#16175,#5008,#5009,#5010,#5011,#5012,#5013,#5014),
#5070,.F.) ;
#63461 = ADVANCED_FACE('',(#16176,#5015,#5016),#5071,.T.) ;
#63462 = ADVANCED_FACE('',(#16177,#5017,#5018),#5072,.F.) ;
#63463 = ADVANCED_FACE('',(#16178),#5073,.T.) ;
#63464 = ADVANCED_FACE('',(#16179),#5074,.T.) ;
#63465 = ADVANCED_FACE('',(#16180),#5075,.T.) ;
#63466 = ADVANCED_FACE('',(#16181),#5076,.T.) ;
#63467 = ADVANCED_FACE('',(#16182),#5077,.T.) ;
#63468 = ADVANCED_FACE('',(#16183),#5078,.T.) ;
#63469 = ADVANCED_FACE('',(#16184),#5079,.T.) ;
#63470 = ADVANCED_FACE('',(#16185),#5950,.T.) ;
#63471 = ADVANCED_FACE('',(#16186),#5951,.F.) ;
#63472 = ADVANCED_FACE('',(#16187),#5080,.T.) ;
#63473 = ADVANCED_FACE('',(#16188),#5081,.T.) ;
#63474 = ADVANCED_FACE('',(#16189),#5082,.T.) ;
#63475 = ADVANCED_FACE('',(#16190),#5083,.T.) ;
#63476 = ADVANCED_FACE('',(#16191),#5084,.T.) ;
#63477 = ADVANCED_FACE('',(#16192),#5085,.F.) ;
#63478 = ADVANCED_FACE('',(#16193),#5086,.T.) ;
#63479 = ADVANCED_FACE('',(#16194),#5087,.T.) ;
#63480 = ADVANCED_FACE('',(#16195),#5088,.T.) ;
#63481 = ADVANCED_FACE('',(#16196),#5089,.F.) ;
#63482 = ADVANCED_FACE('',(#16197),#5090,.F.) ;
#63483 = ADVANCED_FACE('',(#16198),#5091,.F.) ;
#63484 = ADVANCED_FACE('',(#16199),#5092,.T.) ;
#63485 = ADVANCED_FACE('',(#16200),#5093,.T.) ;
#63486 = ADVANCED_FACE('',(#16201),#5094,.T.) ;
#63487 = ADVANCED_FACE('',(#16202),#5952,.T.) ;
#63488 = ADVANCED_FACE('',(#16203),#5953,.F.) ;
#63489 = ADVANCED_FACE('',(#16204),#5095,.T.) ;
#63490 = ADVANCED_FACE('',(#16205),#5096,.T.) ;
#63491 = ADVANCED_FACE('',(#16206),#5954,.T.) ;
#63492 = ADVANCED_FACE('',(#16207),#5955,.F.) ;
#63493 = ADVANCED_FACE('',(#16208),#5097,.F.) ;
#63494 = ADVANCED_FACE('',(#16209),#5098,.F.) ;
#63495 = ADVANCED_FACE('',(#16210),#5099,.F.) ;
#63496 = ADVANCED_FACE('',(#16211),#5100,.F.) ;
#63497 = ADVANCED_FACE('',(#16212),#5101,.T.) ;
#63498 = ADVANCED_FACE('',(#16213),#5102,.T.) ;
#63499 = ADVANCED_FACE('',(#16214),#5103,.T.) ;
#63500 = ADVANCED_FACE('',(#16215),#5104,.F.) ;
#63501 = ADVANCED_FACE('',(#16216),#5105,.F.) ;
#63502 = ADVANCED_FACE('',(#16217),#5106,.F.) ;
#63503 = ADVANCED_FACE('',(#16218),#5107,.F.) ;
#63504 = ADVANCED_FACE('',(#16219),#5108,.F.) ;
#63505 = ADVANCED_FACE('',(#16220),#5109,.F.) ;
#63506 = ADVANCED_FACE('',(#16221),#5110,.F.) ;
#63507 = ADVANCED_FACE('',(#16222),#5111,.F.) ;
#63508 = ADVANCED_FACE('',(#16223),#5112,.F.) ;
#63509 = ADVANCED_FACE('',(#16224),#5113,.F.) ;
#63510 = ADVANCED_FACE('',(#16225),#5114,.F.) ;
#63511 = ADVANCED_FACE('',(#16226),#5115,.F.) ;
#63512 = ADVANCED_FACE('',(#16227),#5116,.F.) ;
#63513 = ADVANCED_FACE('',(#16228),#5117,.F.) ;
#63514 = ADVANCED_FACE('',(#16229),#5118,.F.) ;
#63515 = ADVANCED_FACE('',(#16230),#5119,.F.) ;
#63516 = ADVANCED_FACE('',(#16231),#5120,.F.) ;
#63517 = ADVANCED_FACE('',(#16232),#5121,.F.) ;
#63518 = ADVANCED_FACE('',(#16233),#5122,.F.) ;
#63519 = ADVANCED_FACE('',(#16234),#5123,.F.) ;
#63520 = ADVANCED_FACE('',(#16235),#5124,.F.) ;
#63521 = ADVANCED_FACE('',(#16236),#5125,.F.) ;
#63522 = ADVANCED_FACE('',(#16237),#5126,.F.) ;
#63523 = ADVANCED_FACE('',(#16238),#5127,.F.) ;
#63524 = ADVANCED_FACE('',(#16239),#5128,.F.) ;
#63525 = ADVANCED_FACE('',(#16240),#5129,.F.) ;
#63526 = ADVANCED_FACE('',(#16241),#5130,.F.) ;
#63527 = ADVANCED_FACE('',(#16242),#5131,.F.) ;
#63528 = ADVANCED_FACE('',(#16243),#5132,.F.) ;
#63529 = ADVANCED_FACE('',(#16244),#5133,.F.) ;
#63530 = ADVANCED_FACE('',(#16245),#5134,.F.) ;
#63531 = ADVANCED_FACE('',(#16246),#5135,.F.) ;
#63532 = ADVANCED_FACE('',(#16247),#5136,.F.) ;
#63533 = ADVANCED_FACE('',(#16248),#5137,.F.) ;
#63534 = ADVANCED_FACE('',(#16249),#5138,.F.) ;
#63535 = ADVANCED_FACE('',(#16250),#5139,.F.) ;
#63536 = ADVANCED_FACE('',(#16251),#5140,.F.) ;
#63537 = ADVANCED_FACE('',(#16252),#5141,.F.) ;
#63538 = ADVANCED_FACE('',(#16253),#5142,.F.) ;
#63539 = ADVANCED_FACE('',(#16254),#5143,.F.) ;
#63540 = ADVANCED_FACE('',(#16255),#5144,.F.) ;
#63541 = ADVANCED_FACE('',(#16256),#5145,.F.) ;
#63542 = ADVANCED_FACE('',(#16257),#5146,.F.) ;
#63543 = ADVANCED_FACE('',(#16258),#5147,.F.) ;
#63544 = ADVANCED_FACE('',(#16259),#5148,.F.) ;
#63545 = ADVANCED_FACE('',(#16260),#5149,.F.) ;
#63546 = ADVANCED_FACE('',(#16261),#5150,.F.) ;
#63547 = ADVANCED_FACE('',(#16262),#5151,.F.) ;
#63548 = ADVANCED_FACE('',(#16263),#5152,.F.) ;
#63549 = ADVANCED_FACE('',(#16264),#5956,.T.) ;
#63550 = ADVANCED_FACE('',(#16265),#5957,.T.) ;
#63551 = ADVANCED_FACE('',(#16266),#4182,.T.) ;
#63552 = ADVANCED_FACE('',(#16267),#5958,.T.) ;
#63553 = ADVANCED_FACE('',(#16268),#5959,.T.) ;
#63554 = ADVANCED_FACE('',(#16269),#5960,.T.) ;
#63555 = ADVANCED_FACE('',(#16270),#4183,.T.) ;
#63556 = ADVANCED_FACE('',(#16271),#4184,.T.) ;
#63557 = ADVANCED_FACE('',(#16272),#5961,.T.) ;
#63558 = ADVANCED_FACE('',(#16273),#5962,.T.) ;
#63559 = ADVANCED_FACE('',(#16274),#5963,.T.) ;
#63560 = ADVANCED_FACE('',(#16275),#4185,.T.) ;
#63561 = ADVANCED_FACE('',(#16276),#62820,.T.) ;
#63562 = ADVANCED_FACE('',(#16277),#5964,.T.) ;
#63563 = ADVANCED_FACE('',(#16278),#5965,.F.) ;
#63564 = ADVANCED_FACE('',(#16279),#5966,.T.) ;
#63565 = ADVANCED_FACE('',(#16280),#62821,.T.) ;
#63566 = ADVANCED_FACE('',(#16281),#4186,.T.) ;
#63567 = ADVANCED_FACE('',(#16282),#5967,.T.) ;
#63568 = ADVANCED_FACE('',(#16283),#5968,.T.) ;
#63569 = ADVANCED_FACE('',(#16284),#5969,.T.) ;
#63570 = ADVANCED_FACE('',(#16285),#4187,.T.) ;
#63571 = ADVANCED_FACE('',(#16286),#4188,.T.) ;
#63572 = ADVANCED_FACE('',(#16287),#5970,.T.) ;
#63573 = ADVANCED_FACE('',(#16288),#5971,.T.) ;
#63574 = ADVANCED_FACE('',(#16289),#5972,.T.) ;
#63575 = ADVANCED_FACE('',(#16290),#5973,.T.) ;
#63576 = ADVANCED_FACE('',(#16291),#4189,.T.) ;
#63577 = ADVANCED_FACE('',(#16292),#62822,.T.) ;
#63578 = ADVANCED_FACE('',(#16293),#4190,.T.) ;
#63579 = ADVANCED_FACE('',(#16294),#5974,.T.) ;
#63580 = ADVANCED_FACE('',(#16295),#5975,.T.) ;
#63581 = ADVANCED_FACE('',(#16296),#5976,.F.) ;
#63582 = ADVANCED_FACE('',(#16297),#5977,.T.) ;
#63583 = ADVANCED_FACE('',(#16298),#5978,.T.) ;
#63584 = ADVANCED_FACE('',(#16299),#5979,.T.) ;
#63585 = ADVANCED_FACE('',(#16300),#5980,.T.) ;
#63586 = ADVANCED_FACE('',(#16301),#62823,.T.) ;
#63587 = ADVANCED_FACE('',(#16302),#62824,.T.) ;
#63588 = ADVANCED_FACE('',(#16303),#4191,.T.) ;
#63589 = ADVANCED_FACE('',(#16304),#4192,.T.) ;
#63590 = ADVANCED_FACE('',(#16305),#5981,.T.) ;
#63591 = ADVANCED_FACE('',(#16306),#5982,.T.) ;
#63592 = ADVANCED_FACE('',(#16307),#5983,.T.) ;
#63593 = ADVANCED_FACE('',(#16308),#5984,.T.) ;
#63594 = ADVANCED_FACE('',(#16309),#5985,.T.) ;
#63595 = ADVANCED_FACE('',(#16310),#62825,.T.) ;
#63596 = ADVANCED_FACE('',(#16311),#62826,.T.) ;
#63597 = ADVANCED_FACE('',(#16312),#62827,.T.) ;
#63598 = ADVANCED_FACE('',(#16313),#4193,.T.) ;
#63599 = ADVANCED_FACE('',(#16314),#5986,.T.) ;
#63600 = ADVANCED_FACE('',(#16315),#5987,.F.) ;
#63601 = ADVANCED_FACE('',(#16316),#5988,.T.) ;
#63602 = ADVANCED_FACE('',(#16317),#5989,.T.) ;
#63603 = ADVANCED_FACE('',(#16318),#5990,.F.) ;
#63604 = ADVANCED_FACE('',(#16319),#5991,.T.) ;
#63605 = ADVANCED_FACE('',(#16320),#62828,.T.) ;
#63606 = ADVANCED_FACE('',(#16321),#4194,.T.) ;
#63607 = ADVANCED_FACE('',(#16322),#4195,.T.) ;
#63608 = ADVANCED_FACE('',(#16323),#62829,.T.) ;
#63609 = ADVANCED_FACE('',(#16324),#5992,.T.) ;
#63610 = ADVANCED_FACE('',(#16325),#5993,.T.) ;
#63611 = ADVANCED_FACE('',(#16326),#5994,.T.) ;
#63612 = ADVANCED_FACE('',(#16327),#5995,.T.) ;
#63613 = ADVANCED_FACE('',(#16328),#5996,.T.) ;
#63614 = ADVANCED_FACE('',(#16329),#5997,.T.) ;
#63615 = ADVANCED_FACE('',(#16330),#4196,.T.) ;
#63616 = ADVANCED_FACE('',(#16331),#4197,.T.) ;
#63617 = ADVANCED_FACE('',(#16332),#62830,.T.) ;
#63618 = ADVANCED_FACE('',(#16333),#4198,.T.) ;
#63619 = ADVANCED_FACE('',(#16334),#4199,.T.) ;
#63620 = ADVANCED_FACE('',(#16335),#5998,.T.) ;
#63621 = ADVANCED_FACE('',(#16336),#5999,.T.) ;
#63622 = ADVANCED_FACE('',(#16337),#6000,.T.) ;
#63623 = ADVANCED_FACE('',(#16338),#6001,.T.) ;
#63624 = ADVANCED_FACE('',(#16339),#6002,.T.) ;
#63625 = ADVANCED_FACE('',(#16340),#6003,.T.) ;
#63626 = ADVANCED_FACE('',(#16341),#6004,.T.) ;
#63627 = ADVANCED_FACE('',(#16342),#6005,.T.) ;
#63628 = ADVANCED_FACE('',(#16343),#4200,.T.) ;
#63629 = ADVANCED_FACE('',(#16344),#62831,.T.) ;
#63630 = ADVANCED_FACE('',(#16345),#62832,.T.) ;
#63631 = ADVANCED_FACE('',(#16346),#4201,.T.) ;
#63632 = ADVANCED_FACE('',(#16347),#6006,.T.) ;
#63633 = ADVANCED_FACE('',(#16348),#6007,.F.) ;
#63634 = ADVANCED_FACE('',(#16349),#6008,.F.) ;
#63635 = ADVANCED_FACE('',(#16350),#6009,.T.) ;
#63636 = ADVANCED_FACE('',(#16351),#62833,.T.) ;
#63637 = ADVANCED_FACE('',(#16352),#62834,.T.) ;
#63638 = ADVANCED_FACE('',(#16353),#6010,.T.) ;
#63639 = ADVANCED_FACE('',(#16354),#6011,.T.) ;
#63640 = ADVANCED_FACE('',(#16355),#62835,.T.) ;
#63641 = ADVANCED_FACE('',(#16356),#6012,.T.) ;
#63642 = ADVANCED_FACE('',(#16357),#62836,.T.) ;
#63643 = ADVANCED_FACE('',(#16358),#62837,.T.) ;
#63644 = ADVANCED_FACE('',(#16359),#6013,.F.) ;
#63645 = ADVANCED_FACE('',(#16360),#6014,.T.) ;
#63646 = ADVANCED_FACE('',(#16361),#6015,.T.) ;
#63647 = ADVANCED_FACE('',(#16362),#6016,.T.) ;
#63648 = ADVANCED_FACE('',(#16363),#6017,.F.) ;
#63649 = ADVANCED_FACE('',(#16364),#6018,.T.) ;
#63650 = ADVANCED_FACE('',(#16365),#62838,.T.) ;
#63651 = ADVANCED_FACE('',(#16366),#62839,.T.) ;
#63652 = ADVANCED_FACE('',(#16367),#62840,.T.) ;
#63653 = ADVANCED_FACE('',(#16368),#62841,.T.) ;
#63654 = ADVANCED_FACE('',(#16369),#6019,.T.) ;
#63655 = ADVANCED_FACE('',(#16370),#6020,.F.) ;
#63656 = ADVANCED_FACE('',(#16371),#6021,.F.) ;
#63657 = ADVANCED_FACE('',(#16372),#6022,.T.) ;
#63658 = ADVANCED_FACE('',(#16373),#62842,.T.) ;
#63659 = ADVANCED_FACE('',(#16374),#62843,.T.) ;
#63660 = ADVANCED_FACE('',(#16375),#6023,.T.) ;
#63661 = ADVANCED_FACE('',(#16376),#6024,.T.) ;
#63662 = ADVANCED_FACE('',(#16377),#62844,.T.) ;
#63663 = ADVANCED_FACE('',(#16378),#62845,.T.) ;
#63664 = ADVANCED_FACE('',(#16379),#6025,.F.) ;
#63665 = ADVANCED_FACE('',(#16380),#6026,.T.) ;
#63666 = ADVANCED_FACE('',(#16381),#6027,.T.) ;
#63667 = ADVANCED_FACE('',(#16382),#6028,.T.) ;
#63668 = ADVANCED_FACE('',(#16383),#6029,.F.) ;
#63669 = ADVANCED_FACE('',(#16384),#6030,.T.) ;
#63670 = ADVANCED_FACE('',(#16385),#62846,.T.) ;
#63671 = ADVANCED_FACE('',(#16386),#62847,.T.) ;
#63672 = ADVANCED_FACE('',(#16387),#62848,.T.) ;
#63673 = ADVANCED_FACE('',(#16388),#62849,.T.) ;
#63674 = ADVANCED_FACE('',(#16389),#6031,.T.) ;
#63675 = ADVANCED_FACE('',(#16390),#6032,.F.) ;
#63676 = ADVANCED_FACE('',(#16391),#6033,.F.) ;
#63677 = ADVANCED_FACE('',(#16392),#6034,.T.) ;
#63678 = ADVANCED_FACE('',(#16393),#62850,.T.) ;
#63679 = ADVANCED_FACE('',(#16394),#62851,.T.) ;
#63680 = ADVANCED_FACE('',(#16395),#6035,.T.) ;
#63681 = ADVANCED_FACE('',(#16396),#6036,.T.) ;
#63682 = ADVANCED_FACE('',(#16397),#62852,.T.) ;
#63683 = ADVANCED_FACE('',(#16398),#62853,.T.) ;
#63684 = ADVANCED_FACE('',(#16399),#6037,.F.) ;
#63685 = ADVANCED_FACE('',(#16400),#6038,.T.) ;
#63686 = ADVANCED_FACE('',(#16401),#6039,.T.) ;
#63687 = ADVANCED_FACE('',(#16402),#6040,.T.) ;
#63688 = ADVANCED_FACE('',(#16403),#6041,.F.) ;
#63689 = ADVANCED_FACE('',(#16404),#6042,.T.) ;
#63690 = ADVANCED_FACE('',(#16405),#62854,.T.) ;
#63691 = ADVANCED_FACE('',(#16406),#62855,.T.) ;
#63692 = ADVANCED_FACE('',(#16407),#62856,.T.) ;
#63693 = ADVANCED_FACE('',(#16408),#62857,.T.) ;
#63694 = ADVANCED_FACE('',(#16409),#6043,.T.) ;
#63695 = ADVANCED_FACE('',(#16410),#6044,.F.) ;
#63696 = ADVANCED_FACE('',(#16411),#6045,.F.) ;
#63697 = ADVANCED_FACE('',(#16412),#6046,.T.) ;
#63698 = ADVANCED_FACE('',(#16413),#62858,.T.) ;
#63699 = ADVANCED_FACE('',(#16414),#62859,.T.) ;
#63700 = ADVANCED_FACE('',(#16415),#6047,.T.) ;
#63701 = ADVANCED_FACE('',(#16416),#6048,.T.) ;
#63702 = ADVANCED_FACE('',(#16417),#62860,.T.) ;
#63703 = ADVANCED_FACE('',(#16418),#62861,.T.) ;
#63704 = ADVANCED_FACE('',(#16419),#6049,.F.) ;
#63705 = ADVANCED_FACE('',(#16420),#6050,.T.) ;
#63706 = ADVANCED_FACE('',(#16421),#6051,.T.) ;
#63707 = ADVANCED_FACE('',(#16422),#6052,.T.) ;
#63708 = ADVANCED_FACE('',(#16423),#6053,.F.) ;
#63709 = ADVANCED_FACE('',(#16424),#6054,.T.) ;
#63710 = ADVANCED_FACE('',(#16425),#62862,.T.) ;
#63711 = ADVANCED_FACE('',(#16426),#62863,.T.) ;
#63712 = ADVANCED_FACE('',(#16427),#62864,.T.) ;
#63713 = ADVANCED_FACE('',(#16428),#62865,.T.) ;
#63714 = ADVANCED_FACE('',(#16429),#6055,.T.) ;
#63715 = ADVANCED_FACE('',(#16430),#6056,.F.) ;
#63716 = ADVANCED_FACE('',(#16431),#6057,.F.) ;
#63717 = ADVANCED_FACE('',(#16432),#6058,.T.) ;
#63718 = ADVANCED_FACE('',(#16433),#62866,.T.) ;
#63719 = ADVANCED_FACE('',(#16434),#62867,.T.) ;
#63720 = ADVANCED_FACE('',(#16435),#6059,.T.) ;
#63721 = ADVANCED_FACE('',(#16436),#6060,.T.) ;
#63722 = ADVANCED_FACE('',(#16437),#62868,.T.) ;
#63723 = ADVANCED_FACE('',(#16438),#62869,.T.) ;
#63724 = ADVANCED_FACE('',(#16439),#6061,.T.) ;
#63725 = ADVANCED_FACE('',(#16440),#6062,.F.) ;
#63726 = ADVANCED_FACE('',(#16441),#6063,.T.) ;
#63727 = ADVANCED_FACE('',(#16442),#6064,.F.) ;
#63728 = ADVANCED_FACE('',(#16443),#6065,.T.) ;
#63729 = ADVANCED_FACE('',(#16444),#6066,.T.) ;
#63730 = ADVANCED_FACE('',(#16445),#62870,.T.) ;
#63731 = ADVANCED_FACE('',(#16446),#62871,.T.) ;
#63732 = ADVANCED_FACE('',(#16447),#62872,.T.) ;
#63733 = ADVANCED_FACE('',(#16448),#62873,.T.) ;
#63734 = ADVANCED_FACE('',(#16449),#6067,.F.) ;
#63735 = ADVANCED_FACE('',(#16450),#6068,.T.) ;
#63736 = ADVANCED_FACE('',(#16451),#6069,.T.) ;
#63737 = ADVANCED_FACE('',(#16452),#6070,.F.) ;
#63738 = ADVANCED_FACE('',(#16453),#62874,.T.) ;
#63739 = ADVANCED_FACE('',(#16454),#62875,.T.) ;
#63740 = ADVANCED_FACE('',(#16455),#6071,.T.) ;
#63741 = ADVANCED_FACE('',(#16456),#6072,.T.) ;
#63742 = ADVANCED_FACE('',(#16457),#62876,.T.) ;
#63743 = ADVANCED_FACE('',(#16458),#62877,.T.) ;
#63744 = ADVANCED_FACE('',(#16459),#6073,.F.) ;
#63745 = ADVANCED_FACE('',(#16460),#6074,.T.) ;
#63746 = ADVANCED_FACE('',(#16461),#6075,.T.) ;
#63747 = ADVANCED_FACE('',(#16462),#6076,.T.) ;
#63748 = ADVANCED_FACE('',(#16463),#6077,.F.) ;
#63749 = ADVANCED_FACE('',(#16464),#6078,.T.) ;
#63750 = ADVANCED_FACE('',(#16465),#62878,.T.) ;
#63751 = ADVANCED_FACE('',(#16466),#62879,.T.) ;
#63752 = ADVANCED_FACE('',(#16467),#62880,.T.) ;
#63753 = ADVANCED_FACE('',(#16468),#62881,.T.) ;
#63754 = ADVANCED_FACE('',(#16469),#6079,.T.) ;
#63755 = ADVANCED_FACE('',(#16470),#6080,.F.) ;
#63756 = ADVANCED_FACE('',(#16471),#6081,.F.) ;
#63757 = ADVANCED_FACE('',(#16472),#6082,.T.) ;
#63758 = ADVANCED_FACE('',(#16473),#62882,.T.) ;
#63759 = ADVANCED_FACE('',(#16474),#62883,.T.) ;
#63760 = ADVANCED_FACE('',(#16475),#6083,.T.) ;
#63761 = ADVANCED_FACE('',(#16476),#6084,.T.) ;
#63762 = ADVANCED_FACE('',(#16477),#62884,.T.) ;
#63763 = ADVANCED_FACE('',(#16478),#62885,.T.) ;
#63764 = ADVANCED_FACE('',(#16479),#6085,.F.) ;
#63765 = ADVANCED_FACE('',(#16480),#6086,.T.) ;
#63766 = ADVANCED_FACE('',(#16481),#6087,.T.) ;
#63767 = ADVANCED_FACE('',(#16482),#6088,.T.) ;
#63768 = ADVANCED_FACE('',(#16483),#6089,.F.) ;
#63769 = ADVANCED_FACE('',(#16484),#6090,.T.) ;
#63770 = ADVANCED_FACE('',(#16485),#62886,.T.) ;
#63771 = ADVANCED_FACE('',(#16486),#62887,.T.) ;
#63772 = ADVANCED_FACE('',(#16487),#62888,.T.) ;
#63773 = ADVANCED_FACE('',(#16488),#62889,.T.) ;
#63774 = ADVANCED_FACE('',(#16489),#6091,.T.) ;
#63775 = ADVANCED_FACE('',(#16490),#6092,.F.) ;
#63776 = ADVANCED_FACE('',(#16491),#6093,.F.) ;
#63777 = ADVANCED_FACE('',(#16492),#6094,.T.) ;
#63778 = ADVANCED_FACE('',(#16493),#62890,.T.) ;
#63779 = ADVANCED_FACE('',(#16494),#62891,.T.) ;
#63780 = ADVANCED_FACE('',(#16495),#6095,.T.) ;
#63781 = ADVANCED_FACE('',(#16496),#6096,.T.) ;
#63782 = ADVANCED_FACE('',(#16497),#62892,.T.) ;
#63783 = ADVANCED_FACE('',(#16498),#62893,.T.) ;
#63784 = ADVANCED_FACE('',(#16499),#6097,.F.) ;
#63785 = ADVANCED_FACE('',(#16500),#6098,.T.) ;
#63786 = ADVANCED_FACE('',(#16501),#6099,.T.) ;
#63787 = ADVANCED_FACE('',(#16502),#6100,.T.) ;
#63788 = ADVANCED_FACE('',(#16503),#6101,.F.) ;
#63789 = ADVANCED_FACE('',(#16504),#6102,.T.) ;
#63790 = ADVANCED_FACE('',(#16505),#62894,.T.) ;
#63791 = ADVANCED_FACE('',(#16506),#62895,.T.) ;
#63792 = ADVANCED_FACE('',(#16507),#62896,.T.) ;
#63793 = ADVANCED_FACE('',(#16508),#62897,.T.) ;
#63794 = ADVANCED_FACE('',(#16509),#6103,.T.) ;
#63795 = ADVANCED_FACE('',(#16510),#6104,.F.) ;
#63796 = ADVANCED_FACE('',(#16511),#6105,.F.) ;
#63797 = ADVANCED_FACE('',(#16512),#6106,.T.) ;
#63798 = ADVANCED_FACE('',(#16513),#62898,.T.) ;
#63799 = ADVANCED_FACE('',(#16514),#62899,.T.) ;
#63800 = ADVANCED_FACE('',(#16515),#6107,.T.) ;
#63801 = ADVANCED_FACE('',(#16516),#6108,.T.) ;
#63802 = ADVANCED_FACE('',(#16517),#62900,.T.) ;
#63803 = ADVANCED_FACE('',(#16518),#62901,.T.) ;
#63804 = ADVANCED_FACE('',(#16519),#6109,.F.) ;
#63805 = ADVANCED_FACE('',(#16520),#6110,.T.) ;
#63806 = ADVANCED_FACE('',(#16521),#6111,.T.) ;
#63807 = ADVANCED_FACE('',(#16522),#6112,.T.) ;
#63808 = ADVANCED_FACE('',(#16523),#6113,.F.) ;
#63809 = ADVANCED_FACE('',(#16524),#6114,.T.) ;
#63810 = ADVANCED_FACE('',(#16525),#62902,.T.) ;
#63811 = ADVANCED_FACE('',(#16526),#62903,.T.) ;
#63812 = ADVANCED_FACE('',(#16527),#62904,.T.) ;
#63813 = ADVANCED_FACE('',(#16528),#62905,.T.) ;
#63814 = ADVANCED_FACE('',(#16529),#6115,.T.) ;
#63815 = ADVANCED_FACE('',(#16530),#6116,.F.) ;
#63816 = ADVANCED_FACE('',(#16531),#6117,.F.) ;
#63817 = ADVANCED_FACE('',(#16532),#6118,.T.) ;
#63818 = ADVANCED_FACE('',(#16533),#62906,.T.) ;
#63819 = ADVANCED_FACE('',(#16534),#62907,.T.) ;
#63820 = ADVANCED_FACE('',(#16535),#6119,.T.) ;
#63821 = ADVANCED_FACE('',(#16536),#6120,.T.) ;
#63822 = ADVANCED_FACE('',(#16537),#62908,.T.) ;
#63823 = ADVANCED_FACE('',(#16538),#62909,.T.) ;
#63824 = ADVANCED_FACE('',(#16539),#6121,.F.) ;
#63825 = ADVANCED_FACE('',(#16540),#6122,.T.) ;
#63826 = ADVANCED_FACE('',(#16541),#6123,.T.) ;
#63827 = ADVANCED_FACE('',(#16542),#6124,.T.) ;
#63828 = ADVANCED_FACE('',(#16543),#6125,.F.) ;
#63829 = ADVANCED_FACE('',(#16544),#6126,.T.) ;
#63830 = ADVANCED_FACE('',(#16545),#62910,.T.) ;
#63831 = ADVANCED_FACE('',(#16546),#62911,.T.) ;
#63832 = ADVANCED_FACE('',(#16547),#62912,.T.) ;
#63833 = ADVANCED_FACE('',(#16548),#62913,.T.) ;
#63834 = ADVANCED_FACE('',(#16549),#6127,.T.) ;
#63835 = ADVANCED_FACE('',(#16550),#6128,.F.) ;
#63836 = ADVANCED_FACE('',(#16551),#6129,.F.) ;
#63837 = ADVANCED_FACE('',(#16552),#6130,.T.) ;
#63838 = ADVANCED_FACE('',(#16553),#62914,.T.) ;
#63839 = ADVANCED_FACE('',(#16554),#62915,.T.) ;
#63840 = ADVANCED_FACE('',(#16555),#6131,.T.) ;
#63841 = ADVANCED_FACE('',(#16556),#6132,.T.) ;
#63842 = ADVANCED_FACE('',(#16557),#62916,.T.) ;
#63843 = ADVANCED_FACE('',(#16558),#62917,.T.) ;
#63844 = ADVANCED_FACE('',(#16559),#6133,.F.) ;
#63845 = ADVANCED_FACE('',(#16560),#6134,.T.) ;
#63846 = ADVANCED_FACE('',(#16561),#6135,.T.) ;
#63847 = ADVANCED_FACE('',(#16562),#6136,.T.) ;
#63848 = ADVANCED_FACE('',(#16563),#6137,.F.) ;
#63849 = ADVANCED_FACE('',(#16564),#6138,.T.) ;
#63850 = ADVANCED_FACE('',(#16565),#62918,.T.) ;
#63851 = ADVANCED_FACE('',(#16566),#62919,.T.) ;
#63852 = ADVANCED_FACE('',(#16567),#62920,.T.) ;
#63853 = ADVANCED_FACE('',(#16568),#62921,.T.) ;
#63854 = ADVANCED_FACE('',(#16569),#6139,.T.) ;
#63855 = ADVANCED_FACE('',(#16570),#6140,.F.) ;
#63856 = ADVANCED_FACE('',(#16571),#6141,.F.) ;
#63857 = ADVANCED_FACE('',(#16572),#6142,.T.) ;
#63858 = ADVANCED_FACE('',(#16573),#62922,.T.) ;
#63859 = ADVANCED_FACE('',(#16574),#62923,.T.) ;
#63860 = ADVANCED_FACE('',(#16575),#6143,.T.) ;
#63861 = ADVANCED_FACE('',(#16576),#6144,.T.) ;
#63862 = ADVANCED_FACE('',(#16577),#62924,.T.) ;
#63863 = ADVANCED_FACE('',(#16578),#62925,.T.) ;
#63864 = ADVANCED_FACE('',(#16579),#6145,.F.) ;
#63865 = ADVANCED_FACE('',(#16580),#6146,.T.) ;
#63866 = ADVANCED_FACE('',(#16581),#6147,.T.) ;
#63867 = ADVANCED_FACE('',(#16582),#6148,.T.) ;
#63868 = ADVANCED_FACE('',(#16583),#6149,.F.) ;
#63869 = ADVANCED_FACE('',(#16584),#6150,.T.) ;
#63870 = ADVANCED_FACE('',(#16585),#62926,.T.) ;
#63871 = ADVANCED_FACE('',(#16586),#62927,.T.) ;
#63872 = ADVANCED_FACE('',(#16587),#62928,.T.) ;
#63873 = ADVANCED_FACE('',(#16588),#62929,.T.) ;
#63874 = ADVANCED_FACE('',(#16589),#6151,.T.) ;
#63875 = ADVANCED_FACE('',(#16590),#6152,.F.) ;
#63876 = ADVANCED_FACE('',(#16591),#6153,.F.) ;
#63877 = ADVANCED_FACE('',(#16592),#6154,.T.) ;
#63878 = ADVANCED_FACE('',(#16593),#62930,.T.) ;
#63879 = ADVANCED_FACE('',(#16594),#62931,.T.) ;
#63880 = ADVANCED_FACE('',(#16595),#6155,.T.) ;
#63881 = ADVANCED_FACE('',(#16596),#6156,.T.) ;
#63882 = ADVANCED_FACE('',(#16597),#6157,.T.) ;
#63883 = ADVANCED_FACE('',(#16598),#6158,.T.) ;
#63884 = ADVANCED_FACE('',(#16599),#4202,.T.) ;
#63885 = ADVANCED_FACE('',(#16600),#6159,.T.) ;
#63886 = ADVANCED_FACE('',(#16601),#6160,.T.) ;
#63887 = ADVANCED_FACE('',(#16602),#4203,.T.) ;
#63888 = ADVANCED_FACE('',(#16603),#6161,.T.) ;
#63889 = ADVANCED_FACE('',(#16604),#6162,.T.) ;
#63890 = ADVANCED_FACE('',(#16605),#6163,.T.) ;
#63891 = ADVANCED_FACE('',(#16606),#6164,.T.) ;
#63892 = ADVANCED_FACE('',(#16607),#4204,.T.) ;
#63893 = ADVANCED_FACE('',(#16608),#4205,.T.) ;
#63894 = ADVANCED_FACE('',(#16609),#6165,.T.) ;
#63895 = ADVANCED_FACE('',(#16610),#377,.F.) ;
#63896 = ADVANCED_FACE('',(#16611),#378,.F.) ;
#63897 = ADVANCED_FACE('',(#16612),#62932,.T.) ;
#63898 = ADVANCED_FACE('',(#16613),#62933,.F.) ;
#63899 = ADVANCED_FACE('',(#16614),#6166,.F.) ;
#63900 = ADVANCED_FACE('',(#16615),#6167,.F.) ;
#63901 = ADVANCED_FACE('',(#16616),#62934,.T.) ;
#63902 = ADVANCED_FACE('',(#16617),#6168,.T.) ;
#63903 = ADVANCED_FACE('',(#16618),#6169,.F.) ;
#63904 = ADVANCED_FACE('',(#16619),#5153,.T.) ;
#63905 = ADVANCED_FACE('',(#16620),#5154,.T.) ;
#63906 = ADVANCED_FACE('',(#16621),#5155,.T.) ;
#63907 = ADVANCED_FACE('',(#16622),#5156,.T.) ;
#63908 = ADVANCED_FACE('',(#16623),#5157,.T.) ;
#63909 = ADVANCED_FACE('',(#16624),#5158,.T.) ;
#63910 = ADVANCED_FACE('',(#16625),#5159,.T.) ;
#63911 = ADVANCED_FACE('',(#16626),#5160,.F.) ;
#63912 = ADVANCED_FACE('',(#16627),#5161,.T.) ;
#63913 = ADVANCED_FACE('',(#16628),#5162,.T.) ;
#63914 = ADVANCED_FACE('',(#16629),#5163,.T.) ;
#63915 = ADVANCED_FACE('',(#16630),#5164,.T.) ;
#63916 = ADVANCED_FACE('',(#16631),#5165,.T.) ;
#63917 = ADVANCED_FACE('',(#16632),#5166,.T.) ;
#63918 = ADVANCED_FACE('',(#16633),#5167,.T.) ;
#63919 = ADVANCED_FACE('',(#16634),#5168,.T.) ;
#63920 = ADVANCED_FACE('',(#16635,#5019),#5169,.T.) ;
#63921 = ADVANCED_FACE('',(#16636),#5170,.T.) ;
#63922 = ADVANCED_FACE('',(#16637),#5171,.T.) ;
#63923 = ADVANCED_FACE('',(#16638),#5172,.F.) ;
#63924 = ADVANCED_FACE('',(#16639),#5173,.F.) ;
#63925 = ADVANCED_FACE('',(#16640),#5174,.T.) ;
#63926 = ADVANCED_FACE('',(#16641),#5175,.F.) ;
#63927 = ADVANCED_FACE('',(#16642),#5176,.F.) ;
#63928 = ADVANCED_FACE('',(#16643),#5177,.F.) ;
#63929 = ADVANCED_FACE('',(#16644),#5178,.T.) ;
#63930 = ADVANCED_FACE('',(#16645),#5179,.F.) ;
#63931 = ADVANCED_FACE('',(#16646,#5020),#5180,.T.) ;
#63932 = ADVANCED_FACE('',(#16647),#5181,.T.) ;
#63933 = ADVANCED_FACE('',(#16648),#5182,.F.) ;
#63934 = ADVANCED_FACE('',(#16649),#5183,.F.) ;
#63935 = ADVANCED_FACE('',(#16650),#6170,.T.) ;
#63936 = ADVANCED_FACE('',(#16651),#6171,.T.) ;
#63937 = ADVANCED_FACE('',(#16652),#5184,.F.) ;
#63938 = ADVANCED_FACE('',(#16653),#5185,.F.) ;
#63939 = ADVANCED_FACE('',(#16654),#5186,.F.) ;
#63940 = ADVANCED_FACE('',(#16655),#5187,.T.) ;
#63941 = ADVANCED_FACE('',(#16656),#5188,.F.) ;
#63942 = ADVANCED_FACE('',(#16657),#6172,.T.) ;
#63943 = ADVANCED_FACE('',(#16658),#5189,.F.) ;
#63944 = ADVANCED_FACE('',(#16659),#6173,.T.) ;
#63945 = ADVANCED_FACE('',(#16660),#5190,.F.) ;
#63946 = ADVANCED_FACE('',(#16661),#5191,.F.) ;
#63947 = ADVANCED_FACE('',(#16662),#5192,.F.) ;
#63948 = ADVANCED_FACE('',(#16663),#5193,.F.) ;
#63949 = ADVANCED_FACE('',(#16664),#5194,.F.) ;
#63950 = ADVANCED_FACE('',(#16665),#5195,.F.) ;
#63951 = ADVANCED_FACE('',(#16666),#5196,.F.) ;
#63952 = ADVANCED_FACE('',(#16667),#5197,.F.) ;
#63953 = ADVANCED_FACE('',(#16668),#5198,.F.) ;
#63954 = ADVANCED_FACE('',(#16669),#5199,.T.) ;
#63955 = ADVANCED_FACE('',(#16670),#5200,.F.) ;
#63956 = ADVANCED_FACE('',(#16671),#5201,.F.) ;
#63957 = ADVANCED_FACE('',(#16672),#5202,.F.) ;
#63958 = ADVANCED_FACE('',(#16673),#5203,.T.) ;
#63959 = ADVANCED_FACE('',(#16674),#5204,.F.) ;
#63960 = ADVANCED_FACE('',(#16675),#6174,.T.) ;
#63961 = ADVANCED_FACE('',(#16676),#5205,.F.) ;
#63962 = ADVANCED_FACE('',(#16677),#5206,.F.) ;
#63963 = ADVANCED_FACE('',(#16678),#5207,.F.) ;
#63964 = ADVANCED_FACE('',(#16679),#5208,.F.) ;
#63965 = ADVANCED_FACE('',(#16680),#5209,.F.) ;
#63966 = ADVANCED_FACE('',(#16681),#6175,.F.) ;
#63967 = ADVANCED_FACE('',(#16682),#5210,.F.) ;
#63968 = ADVANCED_FACE('',(#16683),#5211,.F.) ;
#63969 = ADVANCED_FACE('',(#16684),#5212,.F.) ;
#63970 = ADVANCED_FACE('',(#16685),#5213,.F.) ;
#63971 = ADVANCED_FACE('',(#16686),#5214,.F.) ;
#63972 = ADVANCED_FACE('',(#16687),#16130,.F.) ;
#63973 = ADVANCED_FACE('',(#16688),#5215,.F.) ;
#63974 = ADVANCED_FACE('',(#16689),#6176,.F.) ;
#63975 = ADVANCED_FACE('',(#16690),#4206,.F.) ;
#63976 = ADVANCED_FACE('',(#16691),#6177,.T.) ;
#63977 = ADVANCED_FACE('',(#16692),#6178,.F.) ;
#63978 = ADVANCED_FACE('',(#16693),#62935,.F.) ;
#63979 = ADVANCED_FACE('',(#16694),#62936,.T.) ;
#63980 = ADVANCED_FACE('',(#16695),#4207,.F.) ;
#63981 = ADVANCED_FACE('',(#16696),#6179,.F.) ;
#63982 = ADVANCED_FACE('',(#16697),#6180,.F.) ;
#63983 = ADVANCED_FACE('',(#16698),#6181,.T.) ;
#63984 = ADVANCED_FACE('',(#16699),#62937,.T.) ;
#63985 = ADVANCED_FACE('',(#16700),#6182,.F.) ;
#63986 = ADVANCED_FACE('',(#16701),#6183,.F.) ;
#63987 = ADVANCED_FACE('',(#16702),#6184,.F.) ;
#63988 = ADVANCED_FACE('',(#16703),#4208,.F.) ;
#63989 = ADVANCED_FACE('',(#16704),#62938,.T.) ;
#63990 = ADVANCED_FACE('',(#16705),#62939,.T.) ;
#63991 = ADVANCED_FACE('',(#16706),#4209,.F.) ;
#63992 = ADVANCED_FACE('',(#16707),#62940,.F.) ;
#63993 = ADVANCED_FACE('',(#16708),#6185,.F.) ;
#63994 = ADVANCED_FACE('',(#16709),#62941,.T.) ;
#63995 = ADVANCED_FACE('',(#16710),#6186,.T.) ;
#63996 = ADVANCED_FACE('',(#16711),#6187,.F.) ;
#63997 = ADVANCED_FACE('',(#16712),#4210,.F.) ;
#63998 = ADVANCED_FACE('',(#16713),#62942,.T.) ;
#63999 = ADVANCED_FACE('',(#16714),#62943,.F.) ;
#64000 = ADVANCED_FACE('',(#16715),#6188,.F.) ;
#64001 = ADVANCED_FACE('',(#16716),#6189,.F.) ;
#64002 = ADVANCED_FACE('',(#16717),#6190,.T.) ;
#64003 = ADVANCED_FACE('',(#16718),#6191,.F.) ;
#64004 = ADVANCED_FACE('',(#16719),#4211,.F.) ;
#64005 = ADVANCED_FACE('',(#16720),#62944,.F.) ;
#64006 = ADVANCED_FACE('',(#16721),#6192,.F.) ;
#64007 = ADVANCED_FACE('',(#16722),#4212,.T.) ;
#64008 = ADVANCED_FACE('',(#16723),#6193,.T.) ;
#64009 = ADVANCED_FACE('',(#16724),#6194,.T.) ;
#64010 = ADVANCED_FACE('',(#16725),#6195,.T.) ;
#64011 = ADVANCED_FACE('',(#16726),#6196,.T.) ;
#64012 = ADVANCED_FACE('',(#16727),#6197,.T.) ;
#64013 = ADVANCED_FACE('',(#16728),#62945,.F.) ;
#64014 = ADVANCED_FACE('',(#16729),#6198,.F.) ;
#64015 = ADVANCED_FACE('',(#16730),#4213,.F.) ;
#64016 = ADVANCED_FACE('',(#16731),#6199,.T.) ;
#64017 = ADVANCED_FACE('',(#16732),#6200,.T.) ;
#64018 = ADVANCED_FACE('',(#16733),#6201,.F.) ;
#64019 = ADVANCED_FACE('',(#16734),#6202,.T.) ;
#64020 = ADVANCED_FACE('',(#16735),#62946,.T.) ;
#64021 = ADVANCED_FACE('',(#16736),#6203,.F.) ;
#64022 = ADVANCED_FACE('',(#16737),#4214,.T.) ;
#64023 = ADVANCED_FACE('',(#16738),#4215,.F.) ;
#64024 = ADVANCED_FACE('',(#16739),#6204,.T.) ;
#64025 = ADVANCED_FACE('',(#16740),#6205,.T.) ;
#64026 = ADVANCED_FACE('',(#16741),#4216,.F.) ;
#64027 = ADVANCED_FACE('',(#16742),#6206,.T.) ;
#64028 = ADVANCED_FACE('',(#16743),#6207,.F.) ;
#64029 = ADVANCED_FACE('',(#16744),#62947,.T.) ;
#64030 = ADVANCED_FACE('',(#16745),#62948,.T.) ;
#64031 = ADVANCED_FACE('',(#16746),#6208,.F.) ;
#64032 = ADVANCED_FACE('',(#16747),#62949,.F.) ;
#64033 = ADVANCED_FACE('',(#16748),#4217,.F.) ;
#64034 = ADVANCED_FACE('',(#16749),#6209,.T.) ;
#64035 = ADVANCED_FACE('',(#16750),#6210,.T.) ;
#64036 = ADVANCED_FACE('',(#16751),#6211,.F.) ;
#64037 = ADVANCED_FACE('',(#16752),#62950,.T.) ;
#64038 = ADVANCED_FACE('',(#16753),#6212,.T.) ;
#64039 = ADVANCED_FACE('',(#16754),#6213,.F.) ;
#64040 = ADVANCED_FACE('',(#16755),#4218,.F.) ;
#64041 = ADVANCED_FACE('',(#16756),#6214,.T.) ;
#64042 = ADVANCED_FACE('',(#16757),#6215,.F.) ;
#64043 = ADVANCED_FACE('',(#16758),#62951,.F.) ;
#64044 = ADVANCED_FACE('',(#16759),#6216,.F.) ;
#64045 = ADVANCED_FACE('',(#16760),#6217,.T.) ;
#64046 = ADVANCED_FACE('',(#16761),#62952,.T.) ;
#64047 = ADVANCED_FACE('',(#16762),#4219,.F.) ;
#64048 = ADVANCED_FACE('',(#16763),#62953,.F.) ;
#64049 = ADVANCED_FACE('',(#16764),#62954,.T.) ;
#64050 = ADVANCED_FACE('',(#16765),#6218,.F.) ;
#64051 = ADVANCED_FACE('',(#16766),#6219,.F.) ;
#64052 = ADVANCED_FACE('',(#16767),#62955,.F.) ;
#64053 = ADVANCED_FACE('',(#16768),#6220,.T.) ;
#64054 = ADVANCED_FACE('',(#16769),#6221,.F.) ;
#64055 = ADVANCED_FACE('',(#16770),#6222,.F.) ;
#64056 = ADVANCED_FACE('',(#16771),#62956,.T.) ;
#64057 = ADVANCED_FACE('',(#16772),#4220,.F.) ;
#64058 = ADVANCED_FACE('',(#16773),#62957,.F.) ;
#64059 = ADVANCED_FACE('',(#16774),#4221,.F.) ;
#64060 = ADVANCED_FACE('',(#16775),#6223,.T.) ;
#64061 = ADVANCED_FACE('',(#16776),#62958,.F.) ;
#64062 = ADVANCED_FACE('',(#16777),#6224,.F.) ;
#64063 = ADVANCED_FACE('',(#16778),#62959,.F.) ;
#64064 = ADVANCED_FACE('',(#16779),#6225,.F.) ;
#64065 = ADVANCED_FACE('',(#16780),#6226,.T.) ;
#64066 = ADVANCED_FACE('',(#16781),#379,.F.) ;
#64067 = ADVANCED_FACE('',(#16782),#4222,.F.) ;
#64068 = ADVANCED_FACE('',(#16783),#4223,.F.) ;
#64069 = ADVANCED_FACE('',(#16784),#62960,.T.) ;
#64070 = ADVANCED_FACE('',(#16785),#62961,.F.) ;
#64071 = ADVANCED_FACE('',(#16786),#6227,.F.) ;
#64072 = ADVANCED_FACE('',(#16787),#62962,.T.) ;
#64073 = ADVANCED_FACE('',(#16788),#380,.F.) ;
#64074 = ADVANCED_FACE('',(#16789),#62963,.T.) ;
#64075 = ADVANCED_FACE('',(#16790),#6228,.T.) ;
#64076 = ADVANCED_FACE('',(#16791),#62964,.T.) ;
#64077 = ADVANCED_FACE('',(#16792),#6229,.T.) ;
#64078 = ADVANCED_FACE('',(#16793),#62965,.T.) ;
#64079 = ADVANCED_FACE('',(#16794),#6230,.T.) ;
#64080 = ADVANCED_FACE('',(#16795),#62966,.T.) ;
#64081 = ADVANCED_FACE('',(#16796),#6231,.T.) ;
#64082 = ADVANCED_FACE('',(#16797),#4224,.T.) ;
#64083 = ADVANCED_FACE('',(#16798),#6232,.T.) ;
#64084 = ADVANCED_FACE('',(#16799),#6233,.T.) ;
#64085 = ADVANCED_FACE('',(#16800),#6234,.T.) ;
#64086 = ADVANCED_FACE('',(#16801),#6235,.T.) ;
#64087 = ADVANCED_FACE('',(#16802),#6236,.T.) ;
#64088 = ADVANCED_FACE('',(#16803),#4225,.T.) ;
#64089 = ADVANCED_FACE('',(#16804),#4226,.T.) ;
#64090 = ADVANCED_FACE('',(#16805),#6237,.T.) ;
#64091 = ADVANCED_FACE('',(#16806),#6238,.T.) ;
#64092 = ADVANCED_FACE('',(#16807),#4227,.T.) ;
#64093 = ADVANCED_FACE('',(#16808),#6239,.T.) ;
#64094 = ADVANCED_FACE('',(#16809),#6240,.T.) ;
#64095 = ADVANCED_FACE('',(#16810),#62967,.T.) ;
#64096 = ADVANCED_FACE('',(#16811),#6241,.T.) ;
#64097 = ADVANCED_FACE('',(#16812),#6242,.T.) ;
#64098 = ADVANCED_FACE('',(#16813),#6243,.T.) ;
#64099 = ADVANCED_FACE('',(#16814),#6244,.T.) ;
#64100 = ADVANCED_FACE('',(#16815),#6245,.T.) ;
#64101 = ADVANCED_FACE('',(#16816),#4228,.T.) ;
#64102 = ADVANCED_FACE('',(#16817),#6246,.T.) ;
#64103 = ADVANCED_FACE('',(#16818),#6247,.T.) ;
#64104 = ADVANCED_FACE('',(#16819),#4229,.T.) ;
#64105 = ADVANCED_FACE('',(#16820),#6248,.T.) ;
#64106 = ADVANCED_FACE('',(#16821),#6249,.T.) ;
#64107 = ADVANCED_FACE('',(#16822),#6250,.T.) ;
#64108 = ADVANCED_FACE('',(#16823),#6251,.T.) ;
#64109 = ADVANCED_FACE('',(#16824),#4230,.T.) ;
#64110 = ADVANCED_FACE('',(#16825),#4231,.T.) ;
#64111 = ADVANCED_FACE('',(#16826),#6252,.T.) ;
#64112 = ADVANCED_FACE('',(#16827),#6253,.T.) ;
#64113 = ADVANCED_FACE('',(#16828),#6254,.T.) ;
#64114 = ADVANCED_FACE('',(#16829),#4232,.T.) ;
#64115 = ADVANCED_FACE('',(#16830),#6255,.T.) ;
#64116 = ADVANCED_FACE('',(#16831),#6256,.T.) ;
#64117 = ADVANCED_FACE('',(#16832),#4233,.T.) ;
#64118 = ADVANCED_FACE('',(#16833),#6257,.T.) ;
#64119 = ADVANCED_FACE('',(#16834),#6258,.T.) ;
#64120 = ADVANCED_FACE('',(#16835),#6259,.T.) ;
#64121 = ADVANCED_FACE('',(#16836),#4234,.T.) ;
#64122 = ADVANCED_FACE('',(#16837),#6260,.T.) ;
#64123 = ADVANCED_FACE('',(#16838),#6261,.T.) ;
#64124 = ADVANCED_FACE('',(#16839),#4235,.T.) ;
#64125 = ADVANCED_FACE('',(#16840),#6262,.T.) ;
#64126 = ADVANCED_FACE('',(#16841),#6263,.F.) ;
#64127 = ADVANCED_FACE('',(#16842),#6264,.T.) ;
#64128 = ADVANCED_FACE('',(#16843),#6265,.F.) ;
#64129 = ADVANCED_FACE('',(#16844),#6266,.T.) ;
#64130 = ADVANCED_FACE('',(#16845),#6267,.T.) ;
#64131 = ADVANCED_FACE('',(#16846),#6268,.T.) ;
#64132 = ADVANCED_FACE('',(#16847),#62968,.T.) ;
#64133 = ADVANCED_FACE('',(#16848),#6269,.T.) ;
#64134 = ADVANCED_FACE('',(#16849),#381,.F.) ;
#64135 = ADVANCED_FACE('',(#16850),#6270,.F.) ;
#64136 = ADVANCED_FACE('',(#16851),#4236,.F.) ;
#64137 = ADVANCED_FACE('',(#16852),#6271,.F.) ;
#64138 = ADVANCED_FACE('',(#16853),#382,.F.) ;
#64139 = ADVANCED_FACE('',(#16854),#383,.F.) ;
#64140 = ADVANCED_FACE('',(#16855),#6272,.F.) ;
#64141 = ADVANCED_FACE('',(#16856),#4237,.F.) ;
#64142 = ADVANCED_FACE('',(#16857),#6273,.F.) ;
#64143 = ADVANCED_FACE('',(#16858),#384,.F.) ;
#64144 = ADVANCED_FACE('',(#16859),#385,.F.) ;
#64145 = ADVANCED_FACE('',(#16860),#6274,.F.) ;
#64146 = ADVANCED_FACE('',(#16861),#386,.F.) ;
#64147 = ADVANCED_FACE('',(#16862),#6275,.T.) ;
#64148 = ADVANCED_FACE('',(#16863),#387,.T.) ;
#64149 = ADVANCED_FACE('',(#16864),#388,.F.) ;
#64150 = ADVANCED_FACE('',(#16865),#6276,.T.) ;
#64151 = ADVANCED_FACE('',(#16866),#6277,.T.) ;
#64152 = ADVANCED_FACE('',(#16867),#6278,.F.) ;
#64153 = ADVANCED_FACE('',(#16868),#389,.T.) ;
#64154 = ADVANCED_FACE('',(#16869),#390,.F.) ;
#64155 = ADVANCED_FACE('',(#16870),#6279,.T.) ;
#64156 = ADVANCED_FACE('',(#16871),#4238,.T.) ;
#64157 = ADVANCED_FACE('',(#16872),#391,.T.) ;
#64158 = ADVANCED_FACE('',(#16873),#4239,.T.) ;
#64159 = ADVANCED_FACE('',(#16874),#4240,.T.) ;
#64160 = ADVANCED_FACE('',(#16875),#6280,.T.) ;
#64161 = ADVANCED_FACE('',(#16876),#6281,.T.) ;
#64162 = ADVANCED_FACE('',(#16877),#4241,.T.) ;
#64163 = ADVANCED_FACE('',(#16878),#4242,.T.) ;
#64164 = ADVANCED_FACE('',(#16879),#6282,.T.) ;
#64165 = ADVANCED_FACE('',(#16880),#6283,.T.) ;
#64166 = ADVANCED_FACE('',(#16881),#4243,.T.) ;
#64167 = ADVANCED_FACE('',(#16882),#4244,.T.) ;
#64168 = ADVANCED_FACE('',(#16883),#6284,.T.) ;
#64169 = ADVANCED_FACE('',(#16884),#6285,.T.) ;
#64170 = ADVANCED_FACE('',(#16885),#4245,.T.) ;
#64171 = ADVANCED_FACE('',(#16886),#4246,.T.) ;
#64172 = ADVANCED_FACE('',(#16887),#6286,.T.) ;
#64173 = ADVANCED_FACE('',(#16888),#6287,.T.) ;
#64174 = ADVANCED_FACE('',(#16889),#4247,.T.) ;
#64175 = ADVANCED_FACE('',(#16890),#6288,.T.) ;
#64176 = ADVANCED_FACE('',(#16891),#4248,.T.) ;
#64177 = ADVANCED_FACE('',(#16892),#392,.T.) ;
#64178 = ADVANCED_FACE('',(#16893),#4249,.T.) ;
#64179 = ADVANCED_FACE('',(#16894),#6289,.T.) ;
#64180 = ADVANCED_FACE('',(#16895),#393,.T.) ;
#64181 = ADVANCED_FACE('',(#16896),#6290,.T.) ;
#64182 = ADVANCED_FACE('',(#16897),#394,.T.) ;
#64183 = ADVANCED_FACE('',(#16898),#6291,.T.) ;
#64184 = ADVANCED_FACE('',(#16899),#395,.F.) ;
#64185 = ADVANCED_FACE('',(#16900),#396,.F.) ;
#64186 = ADVANCED_FACE('',(#16901),#62969,.T.) ;
#64187 = ADVANCED_FACE('',(#16902),#62970,.F.) ;
#64188 = ADVANCED_FACE('',(#16903),#6292,.F.) ;
#64189 = ADVANCED_FACE('',(#16904),#6293,.F.) ;
#64190 = ADVANCED_FACE('',(#16905),#62971,.T.) ;
#64191 = ADVANCED_FACE('',(#16906),#6294,.T.) ;
#64192 = ADVANCED_FACE('',(#16907),#6295,.F.) ;
#64193 = ADVANCED_FACE('',(#16908),#5216,.T.) ;
#64194 = ADVANCED_FACE('',(#16909),#5217,.T.) ;
#64195 = ADVANCED_FACE('',(#16910),#5218,.T.) ;
#64196 = ADVANCED_FACE('',(#16911),#5219,.T.) ;
#64197 = ADVANCED_FACE('',(#16912),#5220,.T.) ;
#64198 = ADVANCED_FACE('',(#16913),#5221,.T.) ;
#64199 = ADVANCED_FACE('',(#16914),#5222,.T.) ;
#64200 = ADVANCED_FACE('',(#16915),#5223,.F.) ;
#64201 = ADVANCED_FACE('',(#16916),#5224,.T.) ;
#64202 = ADVANCED_FACE('',(#16917),#5225,.T.) ;
#64203 = ADVANCED_FACE('',(#16918),#5226,.T.) ;
#64204 = ADVANCED_FACE('',(#16919),#5227,.T.) ;
#64205 = ADVANCED_FACE('',(#16920),#5228,.T.) ;
#64206 = ADVANCED_FACE('',(#16921),#5229,.T.) ;
#64207 = ADVANCED_FACE('',(#16922),#5230,.T.) ;
#64208 = ADVANCED_FACE('',(#16923),#5231,.T.) ;
#64209 = ADVANCED_FACE('',(#16924,#5021),#5232,.T.) ;
#64210 = ADVANCED_FACE('',(#16925),#5233,.T.) ;
#64211 = ADVANCED_FACE('',(#16926),#5234,.T.) ;
#64212 = ADVANCED_FACE('',(#16927),#5235,.F.) ;
#64213 = ADVANCED_FACE('',(#16928),#5236,.F.) ;
#64214 = ADVANCED_FACE('',(#16929),#5237,.T.) ;
#64215 = ADVANCED_FACE('',(#16930),#5238,.F.) ;
#64216 = ADVANCED_FACE('',(#16931),#5239,.F.) ;
#64217 = ADVANCED_FACE('',(#16932),#5240,.F.) ;
#64218 = ADVANCED_FACE('',(#16933),#5241,.T.) ;
#64219 = ADVANCED_FACE('',(#16934),#5242,.F.) ;
#64220 = ADVANCED_FACE('',(#16935,#5022),#5243,.T.) ;
#64221 = ADVANCED_FACE('',(#16936),#5244,.T.) ;
#64222 = ADVANCED_FACE('',(#16937),#5245,.F.) ;
#64223 = ADVANCED_FACE('',(#16938),#5246,.F.) ;
#64224 = ADVANCED_FACE('',(#16939),#6296,.T.) ;
#64225 = ADVANCED_FACE('',(#16940),#6297,.T.) ;
#64226 = ADVANCED_FACE('',(#16941),#5247,.F.) ;
#64227 = ADVANCED_FACE('',(#16942),#5248,.F.) ;
#64228 = ADVANCED_FACE('',(#16943),#5249,.F.) ;
#64229 = ADVANCED_FACE('',(#16944),#5250,.T.) ;
#64230 = ADVANCED_FACE('',(#16945),#5251,.F.) ;
#64231 = ADVANCED_FACE('',(#16946),#6298,.T.) ;
#64232 = ADVANCED_FACE('',(#16947),#5252,.F.) ;
#64233 = ADVANCED_FACE('',(#16948),#6299,.T.) ;
#64234 = ADVANCED_FACE('',(#16949),#5253,.F.) ;
#64235 = ADVANCED_FACE('',(#16950),#5254,.F.) ;
#64236 = ADVANCED_FACE('',(#16951),#5255,.F.) ;
#64237 = ADVANCED_FACE('',(#16952),#5256,.F.) ;
#64238 = ADVANCED_FACE('',(#16953),#5257,.F.) ;
#64239 = ADVANCED_FACE('',(#16954),#5258,.F.) ;
#64240 = ADVANCED_FACE('',(#16955),#5259,.F.) ;
#64241 = ADVANCED_FACE('',(#16956),#5260,.F.) ;
#64242 = ADVANCED_FACE('',(#16957),#5261,.F.) ;
#64243 = ADVANCED_FACE('',(#16958),#5262,.T.) ;
#64244 = ADVANCED_FACE('',(#16959),#5263,.F.) ;
#64245 = ADVANCED_FACE('',(#16960),#5264,.F.) ;
#64246 = ADVANCED_FACE('',(#16961),#5265,.F.) ;
#64247 = ADVANCED_FACE('',(#16962),#5266,.T.) ;
#64248 = ADVANCED_FACE('',(#16963),#5267,.F.) ;
#64249 = ADVANCED_FACE('',(#16964),#6300,.T.) ;
#64250 = ADVANCED_FACE('',(#16965),#5268,.F.) ;
#64251 = ADVANCED_FACE('',(#16966),#5269,.F.) ;
#64252 = ADVANCED_FACE('',(#16967),#5270,.F.) ;
#64253 = ADVANCED_FACE('',(#16968),#5271,.F.) ;
#64254 = ADVANCED_FACE('',(#16969),#5272,.F.) ;
#64255 = ADVANCED_FACE('',(#16970),#6301,.F.) ;
#64256 = ADVANCED_FACE('',(#16971),#5273,.F.) ;
#64257 = ADVANCED_FACE('',(#16972),#5274,.F.) ;
#64258 = ADVANCED_FACE('',(#16973),#5275,.F.) ;
#64259 = ADVANCED_FACE('',(#16974),#5276,.F.) ;
#64260 = ADVANCED_FACE('',(#16975),#5277,.F.) ;
#64261 = ADVANCED_FACE('',(#16976),#16131,.F.) ;
#64262 = ADVANCED_FACE('',(#16977),#5278,.F.) ;
#64263 = ADVANCED_FACE('',(#16978),#6302,.F.) ;
#64264 = ADVANCED_FACE('',(#16979),#4250,.F.) ;
#64265 = ADVANCED_FACE('',(#16980),#6303,.T.) ;
#64266 = ADVANCED_FACE('',(#16981),#6304,.F.) ;
#64267 = ADVANCED_FACE('',(#16982),#62972,.F.) ;
#64268 = ADVANCED_FACE('',(#16983),#62973,.T.) ;
#64269 = ADVANCED_FACE('',(#16984),#4251,.F.) ;
#64270 = ADVANCED_FACE('',(#16985),#6305,.F.) ;
#64271 = ADVANCED_FACE('',(#16986),#6306,.F.) ;
#64272 = ADVANCED_FACE('',(#16987),#6307,.T.) ;
#64273 = ADVANCED_FACE('',(#16988),#62974,.T.) ;
#64274 = ADVANCED_FACE('',(#16989),#6308,.F.) ;
#64275 = ADVANCED_FACE('',(#16990),#6309,.F.) ;
#64276 = ADVANCED_FACE('',(#16991),#6310,.F.) ;
#64277 = ADVANCED_FACE('',(#16992),#4252,.F.) ;
#64278 = ADVANCED_FACE('',(#16993),#62975,.T.) ;
#64279 = ADVANCED_FACE('',(#16994),#62976,.T.) ;
#64280 = ADVANCED_FACE('',(#16995),#4253,.F.) ;
#64281 = ADVANCED_FACE('',(#16996),#62977,.F.) ;
#64282 = ADVANCED_FACE('',(#16997),#6311,.F.) ;
#64283 = ADVANCED_FACE('',(#16998),#62978,.T.) ;
#64284 = ADVANCED_FACE('',(#16999),#6312,.T.) ;
#64285 = ADVANCED_FACE('',(#17000),#6313,.F.) ;
#64286 = ADVANCED_FACE('',(#17001),#4254,.F.) ;
#64287 = ADVANCED_FACE('',(#17002),#62979,.T.) ;
#64288 = ADVANCED_FACE('',(#17003),#62980,.F.) ;
#64289 = ADVANCED_FACE('',(#17004),#6314,.F.) ;
#64290 = ADVANCED_FACE('',(#17005),#6315,.F.) ;
#64291 = ADVANCED_FACE('',(#17006),#6316,.T.) ;
#64292 = ADVANCED_FACE('',(#17007),#6317,.F.) ;
#64293 = ADVANCED_FACE('',(#17008),#4255,.F.) ;
#64294 = ADVANCED_FACE('',(#17009),#62981,.F.) ;
#64295 = ADVANCED_FACE('',(#17010),#6318,.F.) ;
#64296 = ADVANCED_FACE('',(#17011),#4256,.T.) ;
#64297 = ADVANCED_FACE('',(#17012),#6319,.T.) ;
#64298 = ADVANCED_FACE('',(#17013),#6320,.T.) ;
#64299 = ADVANCED_FACE('',(#17014),#6321,.T.) ;
#64300 = ADVANCED_FACE('',(#17015),#6322,.T.) ;
#64301 = ADVANCED_FACE('',(#17016),#6323,.T.) ;
#64302 = ADVANCED_FACE('',(#17017),#62982,.F.) ;
#64303 = ADVANCED_FACE('',(#17018),#6324,.F.) ;
#64304 = ADVANCED_FACE('',(#17019),#4257,.F.) ;
#64305 = ADVANCED_FACE('',(#17020),#6325,.T.) ;
#64306 = ADVANCED_FACE('',(#17021),#6326,.T.) ;
#64307 = ADVANCED_FACE('',(#17022),#6327,.F.) ;
#64308 = ADVANCED_FACE('',(#17023),#6328,.T.) ;
#64309 = ADVANCED_FACE('',(#17024),#62983,.T.) ;
#64310 = ADVANCED_FACE('',(#17025),#6329,.F.) ;
#64311 = ADVANCED_FACE('',(#17026),#4258,.T.) ;
#64312 = ADVANCED_FACE('',(#17027),#4259,.F.) ;
#64313 = ADVANCED_FACE('',(#17028),#6330,.T.) ;
#64314 = ADVANCED_FACE('',(#17029),#6331,.T.) ;
#64315 = ADVANCED_FACE('',(#17030),#4260,.F.) ;
#64316 = ADVANCED_FACE('',(#17031),#6332,.T.) ;
#64317 = ADVANCED_FACE('',(#17032),#6333,.F.) ;
#64318 = ADVANCED_FACE('',(#17033),#62984,.T.) ;
#64319 = ADVANCED_FACE('',(#17034),#62985,.T.) ;
#64320 = ADVANCED_FACE('',(#17035),#6334,.F.) ;
#64321 = ADVANCED_FACE('',(#17036),#62986,.F.) ;
#64322 = ADVANCED_FACE('',(#17037),#4261,.F.) ;
#64323 = ADVANCED_FACE('',(#17038),#6335,.T.) ;
#64324 = ADVANCED_FACE('',(#17039),#6336,.T.) ;
#64325 = ADVANCED_FACE('',(#17040),#6337,.F.) ;
#64326 = ADVANCED_FACE('',(#17041),#62987,.T.) ;
#64327 = ADVANCED_FACE('',(#17042),#6338,.T.) ;
#64328 = ADVANCED_FACE('',(#17043),#6339,.F.) ;
#64329 = ADVANCED_FACE('',(#17044),#4262,.F.) ;
#64330 = ADVANCED_FACE('',(#17045),#6340,.T.) ;
#64331 = ADVANCED_FACE('',(#17046),#6341,.F.) ;
#64332 = ADVANCED_FACE('',(#17047),#62988,.F.) ;
#64333 = ADVANCED_FACE('',(#17048),#6342,.F.) ;
#64334 = ADVANCED_FACE('',(#17049),#6343,.T.) ;
#64335 = ADVANCED_FACE('',(#17050),#62989,.T.) ;
#64336 = ADVANCED_FACE('',(#17051),#4263,.F.) ;
#64337 = ADVANCED_FACE('',(#17052),#62990,.F.) ;
#64338 = ADVANCED_FACE('',(#17053),#62991,.T.) ;
#64339 = ADVANCED_FACE('',(#17054),#6344,.F.) ;
#64340 = ADVANCED_FACE('',(#17055),#6345,.F.) ;
#64341 = ADVANCED_FACE('',(#17056),#62992,.F.) ;
#64342 = ADVANCED_FACE('',(#17057),#6346,.T.) ;
#64343 = ADVANCED_FACE('',(#17058),#6347,.F.) ;
#64344 = ADVANCED_FACE('',(#17059),#6348,.F.) ;
#64345 = ADVANCED_FACE('',(#17060),#62993,.T.) ;
#64346 = ADVANCED_FACE('',(#17061),#4264,.F.) ;
#64347 = ADVANCED_FACE('',(#17062),#62994,.F.) ;
#64348 = ADVANCED_FACE('',(#17063),#4265,.F.) ;
#64349 = ADVANCED_FACE('',(#17064),#6349,.T.) ;
#64350 = ADVANCED_FACE('',(#17065),#62995,.F.) ;
#64351 = ADVANCED_FACE('',(#17066),#6350,.F.) ;
#64352 = ADVANCED_FACE('',(#17067),#62996,.F.) ;
#64353 = ADVANCED_FACE('',(#17068),#6351,.F.) ;
#64354 = ADVANCED_FACE('',(#17069),#6352,.T.) ;
#64355 = ADVANCED_FACE('',(#17070),#397,.F.) ;
#64356 = ADVANCED_FACE('',(#17071),#4266,.F.) ;
#64357 = ADVANCED_FACE('',(#17072),#4267,.F.) ;
#64358 = ADVANCED_FACE('',(#17073),#62997,.T.) ;
#64359 = ADVANCED_FACE('',(#17074),#62998,.F.) ;
#64360 = ADVANCED_FACE('',(#17075),#6353,.F.) ;
#64361 = ADVANCED_FACE('',(#17076),#62999,.T.) ;
#64362 = ADVANCED_FACE('',(#17077),#398,.F.) ;
#64363 = ADVANCED_FACE('',(#17078),#63000,.T.) ;
#64364 = ADVANCED_FACE('',(#17079),#6354,.T.) ;
#64365 = ADVANCED_FACE('',(#17080),#63001,.T.) ;
#64366 = ADVANCED_FACE('',(#17081),#6355,.T.) ;
#64367 = ADVANCED_FACE('',(#17082),#63002,.T.) ;
#64368 = ADVANCED_FACE('',(#17083),#6356,.T.) ;
#64369 = ADVANCED_FACE('',(#17084),#63003,.T.) ;
#64370 = ADVANCED_FACE('',(#17085),#6357,.T.) ;
#64371 = ADVANCED_FACE('',(#17086),#4268,.T.) ;
#64372 = ADVANCED_FACE('',(#17087),#6358,.T.) ;
#64373 = ADVANCED_FACE('',(#17088),#6359,.T.) ;
#64374 = ADVANCED_FACE('',(#17089),#6360,.T.) ;
#64375 = ADVANCED_FACE('',(#17090),#6361,.T.) ;
#64376 = ADVANCED_FACE('',(#17091),#6362,.T.) ;
#64377 = ADVANCED_FACE('',(#17092),#4269,.T.) ;
#64378 = ADVANCED_FACE('',(#17093),#4270,.T.) ;
#64379 = ADVANCED_FACE('',(#17094),#6363,.T.) ;
#64380 = ADVANCED_FACE('',(#17095),#6364,.T.) ;
#64381 = ADVANCED_FACE('',(#17096),#4271,.T.) ;
#64382 = ADVANCED_FACE('',(#17097),#6365,.T.) ;
#64383 = ADVANCED_FACE('',(#17098),#6366,.T.) ;
#64384 = ADVANCED_FACE('',(#17099),#63004,.T.) ;
#64385 = ADVANCED_FACE('',(#17100),#6367,.T.) ;
#64386 = ADVANCED_FACE('',(#17101),#6368,.T.) ;
#64387 = ADVANCED_FACE('',(#17102),#6369,.T.) ;
#64388 = ADVANCED_FACE('',(#17103),#6370,.T.) ;
#64389 = ADVANCED_FACE('',(#17104),#6371,.T.) ;
#64390 = ADVANCED_FACE('',(#17105),#4272,.T.) ;
#64391 = ADVANCED_FACE('',(#17106),#6372,.T.) ;
#64392 = ADVANCED_FACE('',(#17107),#6373,.T.) ;
#64393 = ADVANCED_FACE('',(#17108),#4273,.T.) ;
#64394 = ADVANCED_FACE('',(#17109),#6374,.T.) ;
#64395 = ADVANCED_FACE('',(#17110),#6375,.T.) ;
#64396 = ADVANCED_FACE('',(#17111),#6376,.T.) ;
#64397 = ADVANCED_FACE('',(#17112),#6377,.T.) ;
#64398 = ADVANCED_FACE('',(#17113),#4274,.T.) ;
#64399 = ADVANCED_FACE('',(#17114),#4275,.T.) ;
#64400 = ADVANCED_FACE('',(#17115),#6378,.T.) ;
#64401 = ADVANCED_FACE('',(#17116),#6379,.T.) ;
#64402 = ADVANCED_FACE('',(#17117),#6380,.T.) ;
#64403 = ADVANCED_FACE('',(#17118),#4276,.T.) ;
#64404 = ADVANCED_FACE('',(#17119),#6381,.T.) ;
#64405 = ADVANCED_FACE('',(#17120),#6382,.T.) ;
#64406 = ADVANCED_FACE('',(#17121),#4277,.T.) ;
#64407 = ADVANCED_FACE('',(#17122),#6383,.T.) ;
#64408 = ADVANCED_FACE('',(#17123),#6384,.T.) ;
#64409 = ADVANCED_FACE('',(#17124),#6385,.T.) ;
#64410 = ADVANCED_FACE('',(#17125),#4278,.T.) ;
#64411 = ADVANCED_FACE('',(#17126),#6386,.T.) ;
#64412 = ADVANCED_FACE('',(#17127),#6387,.T.) ;
#64413 = ADVANCED_FACE('',(#17128),#4279,.T.) ;
#64414 = ADVANCED_FACE('',(#17129),#6388,.T.) ;
#64415 = ADVANCED_FACE('',(#17130),#6389,.F.) ;
#64416 = ADVANCED_FACE('',(#17131),#6390,.T.) ;
#64417 = ADVANCED_FACE('',(#17132),#6391,.F.) ;
#64418 = ADVANCED_FACE('',(#17133),#6392,.T.) ;
#64419 = ADVANCED_FACE('',(#17134),#6393,.T.) ;
#64420 = ADVANCED_FACE('',(#17135),#6394,.T.) ;
#64421 = ADVANCED_FACE('',(#17136),#63005,.T.) ;
#64422 = ADVANCED_FACE('',(#17137),#6395,.T.) ;
#64423 = ADVANCED_FACE('',(#17138),#399,.F.) ;
#64424 = ADVANCED_FACE('',(#17139),#6396,.F.) ;
#64425 = ADVANCED_FACE('',(#17140),#4280,.F.) ;
#64426 = ADVANCED_FACE('',(#17141),#6397,.F.) ;
#64427 = ADVANCED_FACE('',(#17142),#400,.F.) ;
#64428 = ADVANCED_FACE('',(#17143),#401,.F.) ;
#64429 = ADVANCED_FACE('',(#17144),#6398,.F.) ;
#64430 = ADVANCED_FACE('',(#17145),#4281,.F.) ;
#64431 = ADVANCED_FACE('',(#17146),#6399,.F.) ;
#64432 = ADVANCED_FACE('',(#17147),#402,.F.) ;
#64433 = ADVANCED_FACE('',(#17148),#403,.F.) ;
#64434 = ADVANCED_FACE('',(#17149),#6400,.F.) ;
#64435 = ADVANCED_FACE('',(#17150),#404,.F.) ;
#64436 = ADVANCED_FACE('',(#17151),#6401,.T.) ;
#64437 = ADVANCED_FACE('',(#17152),#405,.T.) ;
#64438 = ADVANCED_FACE('',(#17153),#406,.F.) ;
#64439 = ADVANCED_FACE('',(#17154),#6402,.T.) ;
#64440 = ADVANCED_FACE('',(#17155),#6403,.T.) ;
#64441 = ADVANCED_FACE('',(#17156),#6404,.F.) ;
#64442 = ADVANCED_FACE('',(#17157),#407,.T.) ;
#64443 = ADVANCED_FACE('',(#17158),#408,.F.) ;
#64444 = ADVANCED_FACE('',(#17159),#6405,.T.) ;
#64445 = ADVANCED_FACE('',(#17160),#4282,.T.) ;
#64446 = ADVANCED_FACE('',(#17161),#409,.T.) ;
#64447 = ADVANCED_FACE('',(#17162),#4283,.T.) ;
#64448 = ADVANCED_FACE('',(#17163),#4284,.T.) ;
#64449 = ADVANCED_FACE('',(#17164),#6406,.T.) ;
#64450 = ADVANCED_FACE('',(#17165),#6407,.T.) ;
#64451 = ADVANCED_FACE('',(#17166),#4285,.T.) ;
#64452 = ADVANCED_FACE('',(#17167),#4286,.T.) ;
#64453 = ADVANCED_FACE('',(#17168),#6408,.T.) ;
#64454 = ADVANCED_FACE('',(#17169),#6409,.T.) ;
#64455 = ADVANCED_FACE('',(#17170),#4287,.T.) ;
#64456 = ADVANCED_FACE('',(#17171),#4288,.T.) ;
#64457 = ADVANCED_FACE('',(#17172),#6410,.T.) ;
#64458 = ADVANCED_FACE('',(#17173),#6411,.T.) ;
#64459 = ADVANCED_FACE('',(#17174),#4289,.T.) ;
#64460 = ADVANCED_FACE('',(#17175),#4290,.T.) ;
#64461 = ADVANCED_FACE('',(#17176),#6412,.T.) ;
#64462 = ADVANCED_FACE('',(#17177),#6413,.T.) ;
#64463 = ADVANCED_FACE('',(#17178),#4291,.T.) ;
#64464 = ADVANCED_FACE('',(#17179),#6414,.T.) ;
#64465 = ADVANCED_FACE('',(#17180),#4292,.T.) ;
#64466 = ADVANCED_FACE('',(#17181),#410,.T.) ;
#64467 = ADVANCED_FACE('',(#17182),#4293,.T.) ;
#64468 = ADVANCED_FACE('',(#17183),#6415,.T.) ;
#64469 = ADVANCED_FACE('',(#17184),#411,.T.) ;
#64470 = ADVANCED_FACE('',(#17185),#6416,.T.) ;
#64471 = ADVANCED_FACE('',(#17186),#412,.T.) ;
#64472 = ADVANCED_FACE('',(#17187),#6417,.T.) ;
#64473 = ADVANCED_FACE('',(#17188),#413,.F.) ;
#64474 = ADVANCED_FACE('',(#17189),#414,.F.) ;
#64475 = ADVANCED_FACE('',(#17190),#63006,.T.) ;
#64476 = ADVANCED_FACE('',(#17191),#63007,.F.) ;
#64477 = ADVANCED_FACE('',(#17192),#6418,.F.) ;
#64478 = ADVANCED_FACE('',(#17193),#6419,.F.) ;
#64479 = ADVANCED_FACE('',(#17194),#63008,.T.) ;
#64480 = ADVANCED_FACE('',(#17195),#6420,.T.) ;
#64481 = ADVANCED_FACE('',(#17196),#6421,.F.) ;
#64482 = ADVANCED_FACE('',(#17197),#5279,.T.) ;
#64483 = ADVANCED_FACE('',(#17198),#5280,.T.) ;
#64484 = ADVANCED_FACE('',(#17199),#5281,.T.) ;
#64485 = ADVANCED_FACE('',(#17200),#5282,.T.) ;
#64486 = ADVANCED_FACE('',(#17201),#5283,.T.) ;
#64487 = ADVANCED_FACE('',(#17202),#5284,.T.) ;
#64488 = ADVANCED_FACE('',(#17203),#5285,.T.) ;
#64489 = ADVANCED_FACE('',(#17204),#5286,.F.) ;
#64490 = ADVANCED_FACE('',(#17205),#5287,.T.) ;
#64491 = ADVANCED_FACE('',(#17206),#5288,.T.) ;
#64492 = ADVANCED_FACE('',(#17207),#5289,.T.) ;
#64493 = ADVANCED_FACE('',(#17208),#5290,.T.) ;
#64494 = ADVANCED_FACE('',(#17209),#5291,.T.) ;
#64495 = ADVANCED_FACE('',(#17210),#5292,.T.) ;
#64496 = ADVANCED_FACE('',(#17211),#5293,.T.) ;
#64497 = ADVANCED_FACE('',(#17212),#5294,.T.) ;
#64498 = ADVANCED_FACE('',(#17213,#5023),#5295,.T.) ;
#64499 = ADVANCED_FACE('',(#17214),#5296,.T.) ;
#64500 = ADVANCED_FACE('',(#17215),#5297,.T.) ;
#64501 = ADVANCED_FACE('',(#17216),#5298,.F.) ;
#64502 = ADVANCED_FACE('',(#17217),#5299,.F.) ;
#64503 = ADVANCED_FACE('',(#17218),#5300,.T.) ;
#64504 = ADVANCED_FACE('',(#17219),#5301,.F.) ;
#64505 = ADVANCED_FACE('',(#17220),#5302,.F.) ;
#64506 = ADVANCED_FACE('',(#17221),#5303,.F.) ;
#64507 = ADVANCED_FACE('',(#17222),#5304,.T.) ;
#64508 = ADVANCED_FACE('',(#17223),#5305,.F.) ;
#64509 = ADVANCED_FACE('',(#17224,#5024),#5306,.T.) ;
#64510 = ADVANCED_FACE('',(#17225),#5307,.T.) ;
#64511 = ADVANCED_FACE('',(#17226),#5308,.F.) ;
#64512 = ADVANCED_FACE('',(#17227),#5309,.F.) ;
#64513 = ADVANCED_FACE('',(#17228),#6422,.T.) ;
#64514 = ADVANCED_FACE('',(#17229),#6423,.T.) ;
#64515 = ADVANCED_FACE('',(#17230),#5310,.F.) ;
#64516 = ADVANCED_FACE('',(#17231),#5311,.F.) ;
#64517 = ADVANCED_FACE('',(#17232),#5312,.F.) ;
#64518 = ADVANCED_FACE('',(#17233),#5313,.T.) ;
#64519 = ADVANCED_FACE('',(#17234),#5314,.F.) ;
#64520 = ADVANCED_FACE('',(#17235),#6424,.T.) ;
#64521 = ADVANCED_FACE('',(#17236),#5315,.F.) ;
#64522 = ADVANCED_FACE('',(#17237),#6425,.T.) ;
#64523 = ADVANCED_FACE('',(#17238),#5316,.F.) ;
#64524 = ADVANCED_FACE('',(#17239),#5317,.F.) ;
#64525 = ADVANCED_FACE('',(#17240),#5318,.F.) ;
#64526 = ADVANCED_FACE('',(#17241),#5319,.F.) ;
#64527 = ADVANCED_FACE('',(#17242),#5320,.F.) ;
#64528 = ADVANCED_FACE('',(#17243),#5321,.F.) ;
#64529 = ADVANCED_FACE('',(#17244),#5322,.F.) ;
#64530 = ADVANCED_FACE('',(#17245),#5323,.F.) ;
#64531 = ADVANCED_FACE('',(#17246),#5324,.F.) ;
#64532 = ADVANCED_FACE('',(#17247),#5325,.T.) ;
#64533 = ADVANCED_FACE('',(#17248),#5326,.F.) ;
#64534 = ADVANCED_FACE('',(#17249),#5327,.F.) ;
#64535 = ADVANCED_FACE('',(#17250),#5328,.F.) ;
#64536 = ADVANCED_FACE('',(#17251),#5329,.T.) ;
#64537 = ADVANCED_FACE('',(#17252),#5330,.F.) ;
#64538 = ADVANCED_FACE('',(#17253),#6426,.T.) ;
#64539 = ADVANCED_FACE('',(#17254),#5331,.F.) ;
#64540 = ADVANCED_FACE('',(#17255),#5332,.F.) ;
#64541 = ADVANCED_FACE('',(#17256),#5333,.F.) ;
#64542 = ADVANCED_FACE('',(#17257),#5334,.F.) ;
#64543 = ADVANCED_FACE('',(#17258),#5335,.F.) ;
#64544 = ADVANCED_FACE('',(#17259),#6427,.F.) ;
#64545 = ADVANCED_FACE('',(#17260),#5336,.F.) ;
#64546 = ADVANCED_FACE('',(#17261),#5337,.F.) ;
#64547 = ADVANCED_FACE('',(#17262),#5338,.F.) ;
#64548 = ADVANCED_FACE('',(#17263),#5339,.F.) ;
#64549 = ADVANCED_FACE('',(#17264),#5340,.F.) ;
#64550 = ADVANCED_FACE('',(#17265),#16132,.F.) ;
#64551 = ADVANCED_FACE('',(#17266),#5341,.F.) ;
#64552 = ADVANCED_FACE('',(#17267),#6428,.F.) ;
#64553 = ADVANCED_FACE('',(#17268),#4294,.F.) ;
#64554 = ADVANCED_FACE('',(#17269),#6429,.T.) ;
#64555 = ADVANCED_FACE('',(#17270),#6430,.F.) ;
#64556 = ADVANCED_FACE('',(#17271),#63009,.F.) ;
#64557 = ADVANCED_FACE('',(#17272),#63010,.T.) ;
#64558 = ADVANCED_FACE('',(#17273),#4295,.F.) ;
#64559 = ADVANCED_FACE('',(#17274),#6431,.F.) ;
#64560 = ADVANCED_FACE('',(#17275),#6432,.F.) ;
#64561 = ADVANCED_FACE('',(#17276),#6433,.T.) ;
#64562 = ADVANCED_FACE('',(#17277),#63011,.T.) ;
#64563 = ADVANCED_FACE('',(#17278),#6434,.F.) ;
#64564 = ADVANCED_FACE('',(#17279),#6435,.F.) ;
#64565 = ADVANCED_FACE('',(#17280),#6436,.F.) ;
#64566 = ADVANCED_FACE('',(#17281),#4296,.F.) ;
#64567 = ADVANCED_FACE('',(#17282),#63012,.T.) ;
#64568 = ADVANCED_FACE('',(#17283),#63013,.T.) ;
#64569 = ADVANCED_FACE('',(#17284),#4297,.F.) ;
#64570 = ADVANCED_FACE('',(#17285),#63014,.F.) ;
#64571 = ADVANCED_FACE('',(#17286),#6437,.F.) ;
#64572 = ADVANCED_FACE('',(#17287),#63015,.T.) ;
#64573 = ADVANCED_FACE('',(#17288),#6438,.T.) ;
#64574 = ADVANCED_FACE('',(#17289),#6439,.F.) ;
#64575 = ADVANCED_FACE('',(#17290),#4298,.F.) ;
#64576 = ADVANCED_FACE('',(#17291),#63016,.T.) ;
#64577 = ADVANCED_FACE('',(#17292),#63017,.F.) ;
#64578 = ADVANCED_FACE('',(#17293),#6440,.F.) ;
#64579 = ADVANCED_FACE('',(#17294),#6441,.F.) ;
#64580 = ADVANCED_FACE('',(#17295),#6442,.T.) ;
#64581 = ADVANCED_FACE('',(#17296),#6443,.F.) ;
#64582 = ADVANCED_FACE('',(#17297),#4299,.F.) ;
#64583 = ADVANCED_FACE('',(#17298),#63018,.F.) ;
#64584 = ADVANCED_FACE('',(#17299),#6444,.F.) ;
#64585 = ADVANCED_FACE('',(#17300),#4300,.T.) ;
#64586 = ADVANCED_FACE('',(#17301),#6445,.T.) ;
#64587 = ADVANCED_FACE('',(#17302),#6446,.T.) ;
#64588 = ADVANCED_FACE('',(#17303),#6447,.T.) ;
#64589 = ADVANCED_FACE('',(#17304),#6448,.T.) ;
#64590 = ADVANCED_FACE('',(#17305),#6449,.T.) ;
#64591 = ADVANCED_FACE('',(#17306),#63019,.F.) ;
#64592 = ADVANCED_FACE('',(#17307),#6450,.F.) ;
#64593 = ADVANCED_FACE('',(#17308),#4301,.F.) ;
#64594 = ADVANCED_FACE('',(#17309),#6451,.T.) ;
#64595 = ADVANCED_FACE('',(#17310),#6452,.T.) ;
#64596 = ADVANCED_FACE('',(#17311),#6453,.F.) ;
#64597 = ADVANCED_FACE('',(#17312),#6454,.T.) ;
#64598 = ADVANCED_FACE('',(#17313),#63020,.T.) ;
#64599 = ADVANCED_FACE('',(#17314),#6455,.F.) ;
#64600 = ADVANCED_FACE('',(#17315),#4302,.T.) ;
#64601 = ADVANCED_FACE('',(#17316),#4303,.F.) ;
#64602 = ADVANCED_FACE('',(#17317),#6456,.T.) ;
#64603 = ADVANCED_FACE('',(#17318),#6457,.T.) ;
#64604 = ADVANCED_FACE('',(#17319),#4304,.F.) ;
#64605 = ADVANCED_FACE('',(#17320),#6458,.T.) ;
#64606 = ADVANCED_FACE('',(#17321),#6459,.F.) ;
#64607 = ADVANCED_FACE('',(#17322),#63021,.T.) ;
#64608 = ADVANCED_FACE('',(#17323),#63022,.T.) ;
#64609 = ADVANCED_FACE('',(#17324),#6460,.F.) ;
#64610 = ADVANCED_FACE('',(#17325),#63023,.F.) ;
#64611 = ADVANCED_FACE('',(#17326),#4305,.F.) ;
#64612 = ADVANCED_FACE('',(#17327),#6461,.T.) ;
#64613 = ADVANCED_FACE('',(#17328),#6462,.T.) ;
#64614 = ADVANCED_FACE('',(#17329),#6463,.F.) ;
#64615 = ADVANCED_FACE('',(#17330),#63024,.T.) ;
#64616 = ADVANCED_FACE('',(#17331),#6464,.T.) ;
#64617 = ADVANCED_FACE('',(#17332),#6465,.F.) ;
#64618 = ADVANCED_FACE('',(#17333),#4306,.F.) ;
#64619 = ADVANCED_FACE('',(#17334),#6466,.T.) ;
#64620 = ADVANCED_FACE('',(#17335),#6467,.F.) ;
#64621 = ADVANCED_FACE('',(#17336),#63025,.F.) ;
#64622 = ADVANCED_FACE('',(#17337),#6468,.F.) ;
#64623 = ADVANCED_FACE('',(#17338),#6469,.T.) ;
#64624 = ADVANCED_FACE('',(#17339),#63026,.T.) ;
#64625 = ADVANCED_FACE('',(#17340),#4307,.F.) ;
#64626 = ADVANCED_FACE('',(#17341),#63027,.F.) ;
#64627 = ADVANCED_FACE('',(#17342),#63028,.T.) ;
#64628 = ADVANCED_FACE('',(#17343),#6470,.F.) ;
#64629 = ADVANCED_FACE('',(#17344),#6471,.F.) ;
#64630 = ADVANCED_FACE('',(#17345),#63029,.F.) ;
#64631 = ADVANCED_FACE('',(#17346),#6472,.T.) ;
#64632 = ADVANCED_FACE('',(#17347),#6473,.F.) ;
#64633 = ADVANCED_FACE('',(#17348),#6474,.F.) ;
#64634 = ADVANCED_FACE('',(#17349),#63030,.T.) ;
#64635 = ADVANCED_FACE('',(#17350),#4308,.F.) ;
#64636 = ADVANCED_FACE('',(#17351),#63031,.F.) ;
#64637 = ADVANCED_FACE('',(#17352),#4309,.F.) ;
#64638 = ADVANCED_FACE('',(#17353),#6475,.T.) ;
#64639 = ADVANCED_FACE('',(#17354),#63032,.F.) ;
#64640 = ADVANCED_FACE('',(#17355),#6476,.F.) ;
#64641 = ADVANCED_FACE('',(#17356),#63033,.F.) ;
#64642 = ADVANCED_FACE('',(#17357),#6477,.F.) ;
#64643 = ADVANCED_FACE('',(#17358),#6478,.T.) ;
#64644 = ADVANCED_FACE('',(#17359),#415,.F.) ;
#64645 = ADVANCED_FACE('',(#17360),#4310,.F.) ;
#64646 = ADVANCED_FACE('',(#17361),#4311,.F.) ;
#64647 = ADVANCED_FACE('',(#17362),#63034,.T.) ;
#64648 = ADVANCED_FACE('',(#17363),#63035,.F.) ;
#64649 = ADVANCED_FACE('',(#17364),#6479,.F.) ;
#64650 = ADVANCED_FACE('',(#17365),#63036,.T.) ;
#64651 = ADVANCED_FACE('',(#17366),#416,.F.) ;
#64652 = ADVANCED_FACE('',(#17367),#63037,.T.) ;
#64653 = ADVANCED_FACE('',(#17368),#6480,.T.) ;
#64654 = ADVANCED_FACE('',(#17369),#63038,.T.) ;
#64655 = ADVANCED_FACE('',(#17370),#6481,.T.) ;
#64656 = ADVANCED_FACE('',(#17371),#63039,.T.) ;
#64657 = ADVANCED_FACE('',(#17372),#6482,.T.) ;
#64658 = ADVANCED_FACE('',(#17373),#63040,.T.) ;
#64659 = ADVANCED_FACE('',(#17374),#6483,.T.) ;
#64660 = ADVANCED_FACE('',(#17375),#4312,.T.) ;
#64661 = ADVANCED_FACE('',(#17376),#6484,.T.) ;
#64662 = ADVANCED_FACE('',(#17377),#6485,.T.) ;
#64663 = ADVANCED_FACE('',(#17378),#6486,.T.) ;
#64664 = ADVANCED_FACE('',(#17379),#6487,.T.) ;
#64665 = ADVANCED_FACE('',(#17380),#6488,.T.) ;
#64666 = ADVANCED_FACE('',(#17381),#4313,.T.) ;
#64667 = ADVANCED_FACE('',(#17382),#4314,.T.) ;
#64668 = ADVANCED_FACE('',(#17383),#6489,.T.) ;
#64669 = ADVANCED_FACE('',(#17384),#6490,.T.) ;
#64670 = ADVANCED_FACE('',(#17385),#4315,.T.) ;
#64671 = ADVANCED_FACE('',(#17386),#6491,.T.) ;
#64672 = ADVANCED_FACE('',(#17387),#6492,.T.) ;
#64673 = ADVANCED_FACE('',(#17388),#63041,.T.) ;
#64674 = ADVANCED_FACE('',(#17389),#6493,.T.) ;
#64675 = ADVANCED_FACE('',(#17390),#6494,.T.) ;
#64676 = ADVANCED_FACE('',(#17391),#6495,.T.) ;
#64677 = ADVANCED_FACE('',(#17392),#6496,.T.) ;
#64678 = ADVANCED_FACE('',(#17393),#6497,.T.) ;
#64679 = ADVANCED_FACE('',(#17394),#4316,.T.) ;
#64680 = ADVANCED_FACE('',(#17395),#6498,.T.) ;
#64681 = ADVANCED_FACE('',(#17396),#6499,.T.) ;
#64682 = ADVANCED_FACE('',(#17397),#4317,.T.) ;
#64683 = ADVANCED_FACE('',(#17398),#6500,.T.) ;
#64684 = ADVANCED_FACE('',(#17399),#6501,.T.) ;
#64685 = ADVANCED_FACE('',(#17400),#6502,.T.) ;
#64686 = ADVANCED_FACE('',(#17401),#6503,.T.) ;
#64687 = ADVANCED_FACE('',(#17402),#4318,.T.) ;
#64688 = ADVANCED_FACE('',(#17403),#4319,.T.) ;
#64689 = ADVANCED_FACE('',(#17404),#6504,.T.) ;
#64690 = ADVANCED_FACE('',(#17405),#6505,.T.) ;
#64691 = ADVANCED_FACE('',(#17406),#6506,.T.) ;
#64692 = ADVANCED_FACE('',(#17407),#4320,.T.) ;
#64693 = ADVANCED_FACE('',(#17408),#6507,.T.) ;
#64694 = ADVANCED_FACE('',(#17409),#6508,.T.) ;
#64695 = ADVANCED_FACE('',(#17410),#4321,.T.) ;
#64696 = ADVANCED_FACE('',(#17411),#6509,.T.) ;
#64697 = ADVANCED_FACE('',(#17412),#6510,.T.) ;
#64698 = ADVANCED_FACE('',(#17413),#6511,.T.) ;
#64699 = ADVANCED_FACE('',(#17414),#4322,.T.) ;
#64700 = ADVANCED_FACE('',(#17415),#6512,.T.) ;
#64701 = ADVANCED_FACE('',(#17416),#6513,.T.) ;
#64702 = ADVANCED_FACE('',(#17417),#4323,.T.) ;
#64703 = ADVANCED_FACE('',(#17418),#6514,.T.) ;
#64704 = ADVANCED_FACE('',(#17419),#6515,.F.) ;
#64705 = ADVANCED_FACE('',(#17420),#6516,.T.) ;
#64706 = ADVANCED_FACE('',(#17421),#6517,.F.) ;
#64707 = ADVANCED_FACE('',(#17422),#6518,.T.) ;
#64708 = ADVANCED_FACE('',(#17423),#6519,.T.) ;
#64709 = ADVANCED_FACE('',(#17424),#6520,.T.) ;
#64710 = ADVANCED_FACE('',(#17425),#63042,.T.) ;
#64711 = ADVANCED_FACE('',(#17426),#6521,.T.) ;
#64712 = ADVANCED_FACE('',(#17427),#417,.F.) ;
#64713 = ADVANCED_FACE('',(#17428),#6522,.F.) ;
#64714 = ADVANCED_FACE('',(#17429),#4324,.F.) ;
#64715 = ADVANCED_FACE('',(#17430),#6523,.F.) ;
#64716 = ADVANCED_FACE('',(#17431),#418,.F.) ;
#64717 = ADVANCED_FACE('',(#17432),#419,.F.) ;
#64718 = ADVANCED_FACE('',(#17433),#6524,.F.) ;
#64719 = ADVANCED_FACE('',(#17434),#4325,.F.) ;
#64720 = ADVANCED_FACE('',(#17435),#6525,.F.) ;
#64721 = ADVANCED_FACE('',(#17436),#420,.F.) ;
#64722 = ADVANCED_FACE('',(#17437),#421,.F.) ;
#64723 = ADVANCED_FACE('',(#17438),#6526,.F.) ;
#64724 = ADVANCED_FACE('',(#17439),#422,.F.) ;
#64725 = ADVANCED_FACE('',(#17440),#6527,.T.) ;
#64726 = ADVANCED_FACE('',(#17441),#423,.T.) ;
#64727 = ADVANCED_FACE('',(#17442),#424,.F.) ;
#64728 = ADVANCED_FACE('',(#17443),#6528,.T.) ;
#64729 = ADVANCED_FACE('',(#17444),#6529,.T.) ;
#64730 = ADVANCED_FACE('',(#17445),#6530,.F.) ;
#64731 = ADVANCED_FACE('',(#17446),#425,.T.) ;
#64732 = ADVANCED_FACE('',(#17447),#426,.F.) ;
#64733 = ADVANCED_FACE('',(#17448),#6531,.T.) ;
#64734 = ADVANCED_FACE('',(#17449),#4326,.T.) ;
#64735 = ADVANCED_FACE('',(#17450),#427,.T.) ;
#64736 = ADVANCED_FACE('',(#17451),#4327,.T.) ;
#64737 = ADVANCED_FACE('',(#17452),#4328,.T.) ;
#64738 = ADVANCED_FACE('',(#17453),#6532,.T.) ;
#64739 = ADVANCED_FACE('',(#17454),#6533,.T.) ;
#64740 = ADVANCED_FACE('',(#17455),#4329,.T.) ;
#64741 = ADVANCED_FACE('',(#17456),#4330,.T.) ;
#64742 = ADVANCED_FACE('',(#17457),#6534,.T.) ;
#64743 = ADVANCED_FACE('',(#17458),#6535,.T.) ;
#64744 = ADVANCED_FACE('',(#17459),#4331,.T.) ;
#64745 = ADVANCED_FACE('',(#17460),#4332,.T.) ;
#64746 = ADVANCED_FACE('',(#17461),#6536,.T.) ;
#64747 = ADVANCED_FACE('',(#17462),#6537,.T.) ;
#64748 = ADVANCED_FACE('',(#17463),#4333,.T.) ;
#64749 = ADVANCED_FACE('',(#17464),#4334,.T.) ;
#64750 = ADVANCED_FACE('',(#17465),#6538,.T.) ;
#64751 = ADVANCED_FACE('',(#17466),#6539,.T.) ;
#64752 = ADVANCED_FACE('',(#17467),#4335,.T.) ;
#64753 = ADVANCED_FACE('',(#17468),#6540,.T.) ;
#64754 = ADVANCED_FACE('',(#17469),#4336,.T.) ;
#64755 = ADVANCED_FACE('',(#17470),#428,.T.) ;
#64756 = ADVANCED_FACE('',(#17471),#4337,.T.) ;
#64757 = ADVANCED_FACE('',(#17472),#6541,.T.) ;
#64758 = ADVANCED_FACE('',(#17473),#429,.T.) ;
#64759 = ADVANCED_FACE('',(#17474),#6542,.T.) ;
#64760 = ADVANCED_FACE('',(#17475),#430,.T.) ;
#64761 = ADVANCED_FACE('',(#17476),#6543,.T.) ;
#64762 = ADVANCED_FACE('',(#17477),#431,.F.) ;
#64763 = ADVANCED_FACE('',(#17478),#432,.F.) ;
#64764 = ADVANCED_FACE('',(#17479),#63043,.T.) ;
#64765 = ADVANCED_FACE('',(#17480),#63044,.F.) ;
#64766 = ADVANCED_FACE('',(#17481),#6544,.F.) ;
#64767 = ADVANCED_FACE('',(#17482),#6545,.F.) ;
#64768 = ADVANCED_FACE('',(#17483),#63045,.T.) ;
#64769 = ADVANCED_FACE('',(#17484),#6546,.T.) ;
#64770 = ADVANCED_FACE('',(#17485),#6547,.F.) ;
#64771 = ADVANCED_FACE('',(#17486),#5342,.T.) ;
#64772 = ADVANCED_FACE('',(#17487),#5343,.T.) ;
#64773 = ADVANCED_FACE('',(#17488),#5344,.T.) ;
#64774 = ADVANCED_FACE('',(#17489),#5345,.T.) ;
#64775 = ADVANCED_FACE('',(#17490),#5346,.T.) ;
#64776 = ADVANCED_FACE('',(#17491),#5347,.T.) ;
#64777 = ADVANCED_FACE('',(#17492),#5348,.T.) ;
#64778 = ADVANCED_FACE('',(#17493),#5349,.F.) ;
#64779 = ADVANCED_FACE('',(#17494),#5350,.T.) ;
#64780 = ADVANCED_FACE('',(#17495),#5351,.T.) ;
#64781 = ADVANCED_FACE('',(#17496),#5352,.T.) ;
#64782 = ADVANCED_FACE('',(#17497),#5353,.T.) ;
#64783 = ADVANCED_FACE('',(#17498),#5354,.T.) ;
#64784 = ADVANCED_FACE('',(#17499),#5355,.T.) ;
#64785 = ADVANCED_FACE('',(#17500),#5356,.T.) ;
#64786 = ADVANCED_FACE('',(#17501),#5357,.T.) ;
#64787 = ADVANCED_FACE('',(#17502,#5025),#5358,.T.) ;
#64788 = ADVANCED_FACE('',(#17503),#5359,.T.) ;
#64789 = ADVANCED_FACE('',(#17504),#5360,.T.) ;
#64790 = ADVANCED_FACE('',(#17505),#5361,.F.) ;
#64791 = ADVANCED_FACE('',(#17506),#5362,.F.) ;
#64792 = ADVANCED_FACE('',(#17507),#5363,.T.) ;
#64793 = ADVANCED_FACE('',(#17508),#5364,.F.) ;
#64794 = ADVANCED_FACE('',(#17509),#5365,.F.) ;
#64795 = ADVANCED_FACE('',(#17510),#5366,.F.) ;
#64796 = ADVANCED_FACE('',(#17511),#5367,.T.) ;
#64797 = ADVANCED_FACE('',(#17512),#5368,.F.) ;
#64798 = ADVANCED_FACE('',(#17513,#5026),#5369,.T.) ;
#64799 = ADVANCED_FACE('',(#17514),#5370,.T.) ;
#64800 = ADVANCED_FACE('',(#17515),#5371,.F.) ;
#64801 = ADVANCED_FACE('',(#17516),#5372,.F.) ;
#64802 = ADVANCED_FACE('',(#17517),#6548,.T.) ;
#64803 = ADVANCED_FACE('',(#17518),#6549,.T.) ;
#64804 = ADVANCED_FACE('',(#17519),#5373,.F.) ;
#64805 = ADVANCED_FACE('',(#17520),#5374,.F.) ;
#64806 = ADVANCED_FACE('',(#17521),#5375,.F.) ;
#64807 = ADVANCED_FACE('',(#17522),#5376,.T.) ;
#64808 = ADVANCED_FACE('',(#17523),#5377,.F.) ;
#64809 = ADVANCED_FACE('',(#17524),#6550,.T.) ;
#64810 = ADVANCED_FACE('',(#17525),#5378,.F.) ;
#64811 = ADVANCED_FACE('',(#17526),#6551,.T.) ;
#64812 = ADVANCED_FACE('',(#17527),#5379,.F.) ;
#64813 = ADVANCED_FACE('',(#17528),#5380,.F.) ;
#64814 = ADVANCED_FACE('',(#17529),#5381,.F.) ;
#64815 = ADVANCED_FACE('',(#17530),#5382,.F.) ;
#64816 = ADVANCED_FACE('',(#17531),#5383,.F.) ;
#64817 = ADVANCED_FACE('',(#17532),#5384,.F.) ;
#64818 = ADVANCED_FACE('',(#17533),#5385,.F.) ;
#64819 = ADVANCED_FACE('',(#17534),#5386,.F.) ;
#64820 = ADVANCED_FACE('',(#17535),#5387,.F.) ;
#64821 = ADVANCED_FACE('',(#17536),#5388,.T.) ;
#64822 = ADVANCED_FACE('',(#17537),#5389,.F.) ;
#64823 = ADVANCED_FACE('',(#17538),#5390,.F.) ;
#64824 = ADVANCED_FACE('',(#17539),#5391,.F.) ;
#64825 = ADVANCED_FACE('',(#17540),#5392,.T.) ;
#64826 = ADVANCED_FACE('',(#17541),#5393,.F.) ;
#64827 = ADVANCED_FACE('',(#17542),#6552,.T.) ;
#64828 = ADVANCED_FACE('',(#17543),#5394,.F.) ;
#64829 = ADVANCED_FACE('',(#17544),#5395,.F.) ;
#64830 = ADVANCED_FACE('',(#17545),#5396,.F.) ;
#64831 = ADVANCED_FACE('',(#17546),#5397,.F.) ;
#64832 = ADVANCED_FACE('',(#17547),#5398,.F.) ;
#64833 = ADVANCED_FACE('',(#17548),#6553,.F.) ;
#64834 = ADVANCED_FACE('',(#17549),#5399,.F.) ;
#64835 = ADVANCED_FACE('',(#17550),#5400,.F.) ;
#64836 = ADVANCED_FACE('',(#17551),#5401,.F.) ;
#64837 = ADVANCED_FACE('',(#17552),#5402,.F.) ;
#64838 = ADVANCED_FACE('',(#17553),#5403,.F.) ;
#64839 = ADVANCED_FACE('',(#17554),#16133,.F.) ;
#64840 = ADVANCED_FACE('',(#17555),#5404,.F.) ;
#64841 = ADVANCED_FACE('',(#17556),#6554,.F.) ;
#64842 = ADVANCED_FACE('',(#17557),#4338,.F.) ;
#64843 = ADVANCED_FACE('',(#17558),#6555,.T.) ;
#64844 = ADVANCED_FACE('',(#17559),#6556,.F.) ;
#64845 = ADVANCED_FACE('',(#17560),#63046,.F.) ;
#64846 = ADVANCED_FACE('',(#17561),#63047,.T.) ;
#64847 = ADVANCED_FACE('',(#17562),#4339,.F.) ;
#64848 = ADVANCED_FACE('',(#17563),#6557,.F.) ;
#64849 = ADVANCED_FACE('',(#17564),#6558,.F.) ;
#64850 = ADVANCED_FACE('',(#17565),#6559,.T.) ;
#64851 = ADVANCED_FACE('',(#17566),#63048,.T.) ;
#64852 = ADVANCED_FACE('',(#17567),#6560,.F.) ;
#64853 = ADVANCED_FACE('',(#17568),#6561,.F.) ;
#64854 = ADVANCED_FACE('',(#17569),#6562,.F.) ;
#64855 = ADVANCED_FACE('',(#17570),#4340,.F.) ;
#64856 = ADVANCED_FACE('',(#17571),#63049,.T.) ;
#64857 = ADVANCED_FACE('',(#17572),#63050,.T.) ;
#64858 = ADVANCED_FACE('',(#17573),#4341,.F.) ;
#64859 = ADVANCED_FACE('',(#17574),#63051,.F.) ;
#64860 = ADVANCED_FACE('',(#17575),#6563,.F.) ;
#64861 = ADVANCED_FACE('',(#17576),#63052,.T.) ;
#64862 = ADVANCED_FACE('',(#17577),#6564,.T.) ;
#64863 = ADVANCED_FACE('',(#17578),#6565,.F.) ;
#64864 = ADVANCED_FACE('',(#17579),#4342,.F.) ;
#64865 = ADVANCED_FACE('',(#17580),#63053,.T.) ;
#64866 = ADVANCED_FACE('',(#17581),#63054,.F.) ;
#64867 = ADVANCED_FACE('',(#17582),#6566,.F.) ;
#64868 = ADVANCED_FACE('',(#17583),#6567,.F.) ;
#64869 = ADVANCED_FACE('',(#17584),#6568,.T.) ;
#64870 = ADVANCED_FACE('',(#17585),#6569,.F.) ;
#64871 = ADVANCED_FACE('',(#17586),#4343,.F.) ;
#64872 = ADVANCED_FACE('',(#17587),#63055,.F.) ;
#64873 = ADVANCED_FACE('',(#17588),#6570,.F.) ;
#64874 = ADVANCED_FACE('',(#17589),#4344,.T.) ;
#64875 = ADVANCED_FACE('',(#17590),#6571,.T.) ;
#64876 = ADVANCED_FACE('',(#17591),#6572,.T.) ;
#64877 = ADVANCED_FACE('',(#17592),#6573,.T.) ;
#64878 = ADVANCED_FACE('',(#17593),#6574,.T.) ;
#64879 = ADVANCED_FACE('',(#17594),#6575,.T.) ;
#64880 = ADVANCED_FACE('',(#17595),#63056,.F.) ;
#64881 = ADVANCED_FACE('',(#17596),#6576,.F.) ;
#64882 = ADVANCED_FACE('',(#17597),#4345,.F.) ;
#64883 = ADVANCED_FACE('',(#17598),#6577,.T.) ;
#64884 = ADVANCED_FACE('',(#17599),#6578,.T.) ;
#64885 = ADVANCED_FACE('',(#17600),#6579,.F.) ;
#64886 = ADVANCED_FACE('',(#17601),#6580,.T.) ;
#64887 = ADVANCED_FACE('',(#17602),#63057,.T.) ;
#64888 = ADVANCED_FACE('',(#17603),#6581,.F.) ;
#64889 = ADVANCED_FACE('',(#17604),#4346,.T.) ;
#64890 = ADVANCED_FACE('',(#17605),#4347,.F.) ;
#64891 = ADVANCED_FACE('',(#17606),#6582,.T.) ;
#64892 = ADVANCED_FACE('',(#17607),#6583,.T.) ;
#64893 = ADVANCED_FACE('',(#17608),#4348,.F.) ;
#64894 = ADVANCED_FACE('',(#17609),#6584,.T.) ;
#64895 = ADVANCED_FACE('',(#17610),#6585,.F.) ;
#64896 = ADVANCED_FACE('',(#17611),#63058,.T.) ;
#64897 = ADVANCED_FACE('',(#17612),#63059,.T.) ;
#64898 = ADVANCED_FACE('',(#17613),#6586,.F.) ;
#64899 = ADVANCED_FACE('',(#17614),#63060,.F.) ;
#64900 = ADVANCED_FACE('',(#17615),#4349,.F.) ;
#64901 = ADVANCED_FACE('',(#17616),#6587,.T.) ;
#64902 = ADVANCED_FACE('',(#17617),#6588,.T.) ;
#64903 = ADVANCED_FACE('',(#17618),#6589,.F.) ;
#64904 = ADVANCED_FACE('',(#17619),#63061,.T.) ;
#64905 = ADVANCED_FACE('',(#17620),#6590,.T.) ;
#64906 = ADVANCED_FACE('',(#17621),#6591,.F.) ;
#64907 = ADVANCED_FACE('',(#17622),#4350,.F.) ;
#64908 = ADVANCED_FACE('',(#17623),#6592,.T.) ;
#64909 = ADVANCED_FACE('',(#17624),#6593,.F.) ;
#64910 = ADVANCED_FACE('',(#17625),#63062,.F.) ;
#64911 = ADVANCED_FACE('',(#17626),#6594,.F.) ;
#64912 = ADVANCED_FACE('',(#17627),#6595,.T.) ;
#64913 = ADVANCED_FACE('',(#17628),#63063,.T.) ;
#64914 = ADVANCED_FACE('',(#17629),#4351,.F.) ;
#64915 = ADVANCED_FACE('',(#17630),#63064,.F.) ;
#64916 = ADVANCED_FACE('',(#17631),#63065,.T.) ;
#64917 = ADVANCED_FACE('',(#17632),#6596,.F.) ;
#64918 = ADVANCED_FACE('',(#17633),#6597,.F.) ;
#64919 = ADVANCED_FACE('',(#17634),#63066,.F.) ;
#64920 = ADVANCED_FACE('',(#17635),#6598,.T.) ;
#64921 = ADVANCED_FACE('',(#17636),#6599,.F.) ;
#64922 = ADVANCED_FACE('',(#17637),#6600,.F.) ;
#64923 = ADVANCED_FACE('',(#17638),#63067,.T.) ;
#64924 = ADVANCED_FACE('',(#17639),#4352,.F.) ;
#64925 = ADVANCED_FACE('',(#17640),#63068,.F.) ;
#64926 = ADVANCED_FACE('',(#17641),#4353,.F.) ;
#64927 = ADVANCED_FACE('',(#17642),#6601,.T.) ;
#64928 = ADVANCED_FACE('',(#17643),#63069,.F.) ;
#64929 = ADVANCED_FACE('',(#17644),#6602,.F.) ;
#64930 = ADVANCED_FACE('',(#17645),#63070,.F.) ;
#64931 = ADVANCED_FACE('',(#17646),#6603,.F.) ;
#64932 = ADVANCED_FACE('',(#17647),#6604,.T.) ;
#64933 = ADVANCED_FACE('',(#17648),#433,.F.) ;
#64934 = ADVANCED_FACE('',(#17649),#4354,.F.) ;
#64935 = ADVANCED_FACE('',(#17650),#4355,.F.) ;
#64936 = ADVANCED_FACE('',(#17651),#63071,.T.) ;
#64937 = ADVANCED_FACE('',(#17652),#63072,.F.) ;
#64938 = ADVANCED_FACE('',(#17653),#6605,.F.) ;
#64939 = ADVANCED_FACE('',(#17654),#63073,.T.) ;
#64940 = ADVANCED_FACE('',(#17655),#434,.F.) ;
#64941 = ADVANCED_FACE('',(#17656),#63074,.T.) ;
#64942 = ADVANCED_FACE('',(#17657),#6606,.T.) ;
#64943 = ADVANCED_FACE('',(#17658),#63075,.T.) ;
#64944 = ADVANCED_FACE('',(#17659),#6607,.T.) ;
#64945 = ADVANCED_FACE('',(#17660),#63076,.T.) ;
#64946 = ADVANCED_FACE('',(#17661),#6608,.T.) ;
#64947 = ADVANCED_FACE('',(#17662),#63077,.T.) ;
#64948 = ADVANCED_FACE('',(#17663),#6609,.T.) ;
#64949 = ADVANCED_FACE('',(#17664),#4356,.T.) ;
#64950 = ADVANCED_FACE('',(#17665),#6610,.T.) ;
#64951 = ADVANCED_FACE('',(#17666),#6611,.T.) ;
#64952 = ADVANCED_FACE('',(#17667),#6612,.T.) ;
#64953 = ADVANCED_FACE('',(#17668),#6613,.T.) ;
#64954 = ADVANCED_FACE('',(#17669),#6614,.T.) ;
#64955 = ADVANCED_FACE('',(#17670),#4357,.T.) ;
#64956 = ADVANCED_FACE('',(#17671),#4358,.T.) ;
#64957 = ADVANCED_FACE('',(#17672),#6615,.T.) ;
#64958 = ADVANCED_FACE('',(#17673),#6616,.T.) ;
#64959 = ADVANCED_FACE('',(#17674),#4359,.T.) ;
#64960 = ADVANCED_FACE('',(#17675),#6617,.T.) ;
#64961 = ADVANCED_FACE('',(#17676),#6618,.T.) ;
#64962 = ADVANCED_FACE('',(#17677),#63078,.T.) ;
#64963 = ADVANCED_FACE('',(#17678),#6619,.T.) ;
#64964 = ADVANCED_FACE('',(#17679),#6620,.T.) ;
#64965 = ADVANCED_FACE('',(#17680),#6621,.T.) ;
#64966 = ADVANCED_FACE('',(#17681),#6622,.T.) ;
#64967 = ADVANCED_FACE('',(#17682),#6623,.T.) ;
#64968 = ADVANCED_FACE('',(#17683),#4360,.T.) ;
#64969 = ADVANCED_FACE('',(#17684),#6624,.T.) ;
#64970 = ADVANCED_FACE('',(#17685),#6625,.T.) ;
#64971 = ADVANCED_FACE('',(#17686),#4361,.T.) ;
#64972 = ADVANCED_FACE('',(#17687),#6626,.T.) ;
#64973 = ADVANCED_FACE('',(#17688),#6627,.T.) ;
#64974 = ADVANCED_FACE('',(#17689),#6628,.T.) ;
#64975 = ADVANCED_FACE('',(#17690),#6629,.T.) ;
#64976 = ADVANCED_FACE('',(#17691),#4362,.T.) ;
#64977 = ADVANCED_FACE('',(#17692),#4363,.T.) ;
#64978 = ADVANCED_FACE('',(#17693),#6630,.T.) ;
#64979 = ADVANCED_FACE('',(#17694),#6631,.T.) ;
#64980 = ADVANCED_FACE('',(#17695),#6632,.T.) ;
#64981 = ADVANCED_FACE('',(#17696),#4364,.T.) ;
#64982 = ADVANCED_FACE('',(#17697),#6633,.T.) ;
#64983 = ADVANCED_FACE('',(#17698),#6634,.T.) ;
#64984 = ADVANCED_FACE('',(#17699),#4365,.T.) ;
#64985 = ADVANCED_FACE('',(#17700),#6635,.T.) ;
#64986 = ADVANCED_FACE('',(#17701),#6636,.T.) ;
#64987 = ADVANCED_FACE('',(#17702),#6637,.T.) ;
#64988 = ADVANCED_FACE('',(#17703),#4366,.T.) ;
#64989 = ADVANCED_FACE('',(#17704),#6638,.T.) ;
#64990 = ADVANCED_FACE('',(#17705),#6639,.T.) ;
#64991 = ADVANCED_FACE('',(#17706),#4367,.T.) ;
#64992 = ADVANCED_FACE('',(#17707),#6640,.T.) ;
#64993 = ADVANCED_FACE('',(#17708),#6641,.F.) ;
#64994 = ADVANCED_FACE('',(#17709),#6642,.T.) ;
#64995 = ADVANCED_FACE('',(#17710),#6643,.F.) ;
#64996 = ADVANCED_FACE('',(#17711),#6644,.T.) ;
#64997 = ADVANCED_FACE('',(#17712),#6645,.T.) ;
#64998 = ADVANCED_FACE('',(#17713),#6646,.T.) ;
#64999 = ADVANCED_FACE('',(#17714),#63079,.T.) ;
#65000 = ADVANCED_FACE('',(#17715),#6647,.T.) ;
#65001 = ADVANCED_FACE('',(#17716),#435,.F.) ;
#65002 = ADVANCED_FACE('',(#17717),#6648,.F.) ;
#65003 = ADVANCED_FACE('',(#17718),#4368,.F.) ;
#65004 = ADVANCED_FACE('',(#17719),#6649,.F.) ;
#65005 = ADVANCED_FACE('',(#17720),#436,.F.) ;
#65006 = ADVANCED_FACE('',(#17721),#437,.F.) ;
#65007 = ADVANCED_FACE('',(#17722),#6650,.F.) ;
#65008 = ADVANCED_FACE('',(#17723),#4369,.F.) ;
#65009 = ADVANCED_FACE('',(#17724),#6651,.F.) ;
#65010 = ADVANCED_FACE('',(#17725),#438,.F.) ;
#65011 = ADVANCED_FACE('',(#17726),#439,.F.) ;
#65012 = ADVANCED_FACE('',(#17727),#6652,.F.) ;
#65013 = ADVANCED_FACE('',(#17728),#440,.F.) ;
#65014 = ADVANCED_FACE('',(#17729),#6653,.T.) ;
#65015 = ADVANCED_FACE('',(#17730),#441,.T.) ;
#65016 = ADVANCED_FACE('',(#17731),#442,.F.) ;
#65017 = ADVANCED_FACE('',(#17732),#6654,.T.) ;
#65018 = ADVANCED_FACE('',(#17733),#6655,.T.) ;
#65019 = ADVANCED_FACE('',(#17734),#6656,.F.) ;
#65020 = ADVANCED_FACE('',(#17735),#443,.T.) ;
#65021 = ADVANCED_FACE('',(#17736),#444,.F.) ;
#65022 = ADVANCED_FACE('',(#17737),#6657,.T.) ;
#65023 = ADVANCED_FACE('',(#17738),#4370,.T.) ;
#65024 = ADVANCED_FACE('',(#17739),#445,.T.) ;
#65025 = ADVANCED_FACE('',(#17740),#4371,.T.) ;
#65026 = ADVANCED_FACE('',(#17741),#4372,.T.) ;
#65027 = ADVANCED_FACE('',(#17742),#6658,.T.) ;
#65028 = ADVANCED_FACE('',(#17743),#6659,.T.) ;
#65029 = ADVANCED_FACE('',(#17744),#4373,.T.) ;
#65030 = ADVANCED_FACE('',(#17745),#4374,.T.) ;
#65031 = ADVANCED_FACE('',(#17746),#6660,.T.) ;
#65032 = ADVANCED_FACE('',(#17747),#6661,.T.) ;
#65033 = ADVANCED_FACE('',(#17748),#4375,.T.) ;
#65034 = ADVANCED_FACE('',(#17749),#4376,.T.) ;
#65035 = ADVANCED_FACE('',(#17750),#6662,.T.) ;
#65036 = ADVANCED_FACE('',(#17751),#6663,.T.) ;
#65037 = ADVANCED_FACE('',(#17752),#4377,.T.) ;
#65038 = ADVANCED_FACE('',(#17753),#4378,.T.) ;
#65039 = ADVANCED_FACE('',(#17754),#6664,.T.) ;
#65040 = ADVANCED_FACE('',(#17755),#6665,.T.) ;
#65041 = ADVANCED_FACE('',(#17756),#4379,.T.) ;
#65042 = ADVANCED_FACE('',(#17757),#6666,.T.) ;
#65043 = ADVANCED_FACE('',(#17758),#4380,.T.) ;
#65044 = ADVANCED_FACE('',(#17759),#446,.T.) ;
#65045 = ADVANCED_FACE('',(#17760),#4381,.T.) ;
#65046 = ADVANCED_FACE('',(#17761),#6667,.T.) ;
#65047 = ADVANCED_FACE('',(#17762),#447,.T.) ;
#65048 = ADVANCED_FACE('',(#17763),#6668,.T.) ;
#65049 = ADVANCED_FACE('',(#17764),#448,.T.) ;
#65050 = ADVANCED_FACE('',(#17765),#6669,.T.) ;
#65051 = ADVANCED_FACE('',(#17766),#449,.F.) ;
#65052 = ADVANCED_FACE('',(#17767),#450,.F.) ;
#65053 = ADVANCED_FACE('',(#17768),#63080,.T.) ;
#65054 = ADVANCED_FACE('',(#17769),#63081,.F.) ;
#65055 = ADVANCED_FACE('',(#17770),#6670,.F.) ;
#65056 = ADVANCED_FACE('',(#17771),#6671,.F.) ;
#65057 = ADVANCED_FACE('',(#17772),#63082,.T.) ;
#65058 = ADVANCED_FACE('',(#17773),#6672,.T.) ;
#65059 = ADVANCED_FACE('',(#17774),#6673,.F.) ;
#65060 = ADVANCED_FACE('',(#17775),#5405,.T.) ;
#65061 = ADVANCED_FACE('',(#17776),#5406,.T.) ;
#65062 = ADVANCED_FACE('',(#17777),#5407,.T.) ;
#65063 = ADVANCED_FACE('',(#17778),#5408,.T.) ;
#65064 = ADVANCED_FACE('',(#17779),#5409,.T.) ;
#65065 = ADVANCED_FACE('',(#17780),#5410,.T.) ;
#65066 = ADVANCED_FACE('',(#17781),#5411,.T.) ;
#65067 = ADVANCED_FACE('',(#17782),#5412,.F.) ;
#65068 = ADVANCED_FACE('',(#17783),#5413,.T.) ;
#65069 = ADVANCED_FACE('',(#17784),#5414,.T.) ;
#65070 = ADVANCED_FACE('',(#17785),#5415,.T.) ;
#65071 = ADVANCED_FACE('',(#17786),#5416,.T.) ;
#65072 = ADVANCED_FACE('',(#17787),#5417,.T.) ;
#65073 = ADVANCED_FACE('',(#17788),#5418,.T.) ;
#65074 = ADVANCED_FACE('',(#17789),#5419,.T.) ;
#65075 = ADVANCED_FACE('',(#17790),#5420,.T.) ;
#65076 = ADVANCED_FACE('',(#17791,#5027),#5421,.T.) ;
#65077 = ADVANCED_FACE('',(#17792),#5422,.T.) ;
#65078 = ADVANCED_FACE('',(#17793),#5423,.T.) ;
#65079 = ADVANCED_FACE('',(#17794),#5424,.F.) ;
#65080 = ADVANCED_FACE('',(#17795),#5425,.F.) ;
#65081 = ADVANCED_FACE('',(#17796),#5426,.T.) ;
#65082 = ADVANCED_FACE('',(#17797),#5427,.F.) ;
#65083 = ADVANCED_FACE('',(#17798),#5428,.F.) ;
#65084 = ADVANCED_FACE('',(#17799),#5429,.F.) ;
#65085 = ADVANCED_FACE('',(#17800),#5430,.T.) ;
#65086 = ADVANCED_FACE('',(#17801),#5431,.F.) ;
#65087 = ADVANCED_FACE('',(#17802,#5028),#5432,.T.) ;
#65088 = ADVANCED_FACE('',(#17803),#5433,.T.) ;
#65089 = ADVANCED_FACE('',(#17804),#5434,.F.) ;
#65090 = ADVANCED_FACE('',(#17805),#5435,.F.) ;
#65091 = ADVANCED_FACE('',(#17806),#6674,.T.) ;
#65092 = ADVANCED_FACE('',(#17807),#6675,.T.) ;
#65093 = ADVANCED_FACE('',(#17808),#5436,.F.) ;
#65094 = ADVANCED_FACE('',(#17809),#5437,.F.) ;
#65095 = ADVANCED_FACE('',(#17810),#5438,.F.) ;
#65096 = ADVANCED_FACE('',(#17811),#5439,.T.) ;
#65097 = ADVANCED_FACE('',(#17812),#5440,.F.) ;
#65098 = ADVANCED_FACE('',(#17813),#6676,.T.) ;
#65099 = ADVANCED_FACE('',(#17814),#5441,.F.) ;
#65100 = ADVANCED_FACE('',(#17815),#6677,.T.) ;
#65101 = ADVANCED_FACE('',(#17816),#5442,.F.) ;
#65102 = ADVANCED_FACE('',(#17817),#5443,.F.) ;
#65103 = ADVANCED_FACE('',(#17818),#5444,.F.) ;
#65104 = ADVANCED_FACE('',(#17819),#5445,.F.) ;
#65105 = ADVANCED_FACE('',(#17820),#5446,.F.) ;
#65106 = ADVANCED_FACE('',(#17821),#5447,.F.) ;
#65107 = ADVANCED_FACE('',(#17822),#5448,.F.) ;
#65108 = ADVANCED_FACE('',(#17823),#5449,.F.) ;
#65109 = ADVANCED_FACE('',(#17824),#5450,.F.) ;
#65110 = ADVANCED_FACE('',(#17825),#5451,.T.) ;
#65111 = ADVANCED_FACE('',(#17826),#5452,.F.) ;
#65112 = ADVANCED_FACE('',(#17827),#5453,.F.) ;
#65113 = ADVANCED_FACE('',(#17828),#5454,.F.) ;
#65114 = ADVANCED_FACE('',(#17829),#5455,.T.) ;
#65115 = ADVANCED_FACE('',(#17830),#5456,.F.) ;
#65116 = ADVANCED_FACE('',(#17831),#6678,.T.) ;
#65117 = ADVANCED_FACE('',(#17832),#5457,.F.) ;
#65118 = ADVANCED_FACE('',(#17833),#5458,.F.) ;
#65119 = ADVANCED_FACE('',(#17834),#5459,.F.) ;
#65120 = ADVANCED_FACE('',(#17835),#5460,.F.) ;
#65121 = ADVANCED_FACE('',(#17836),#5461,.F.) ;
#65122 = ADVANCED_FACE('',(#17837),#6679,.F.) ;
#65123 = ADVANCED_FACE('',(#17838),#5462,.F.) ;
#65124 = ADVANCED_FACE('',(#17839),#5463,.F.) ;
#65125 = ADVANCED_FACE('',(#17840),#5464,.F.) ;
#65126 = ADVANCED_FACE('',(#17841),#5465,.F.) ;
#65127 = ADVANCED_FACE('',(#17842),#5466,.F.) ;
#65128 = ADVANCED_FACE('',(#17843),#16134,.F.) ;
#65129 = ADVANCED_FACE('',(#17844),#5467,.F.) ;
#65130 = ADVANCED_FACE('',(#17845),#6680,.F.) ;
#65131 = ADVANCED_FACE('',(#17846),#4382,.F.) ;
#65132 = ADVANCED_FACE('',(#17847),#6681,.T.) ;
#65133 = ADVANCED_FACE('',(#17848),#6682,.F.) ;
#65134 = ADVANCED_FACE('',(#17849),#63083,.F.) ;
#65135 = ADVANCED_FACE('',(#17850),#63084,.T.) ;
#65136 = ADVANCED_FACE('',(#17851),#4383,.F.) ;
#65137 = ADVANCED_FACE('',(#17852),#6683,.F.) ;
#65138 = ADVANCED_FACE('',(#17853),#6684,.F.) ;
#65139 = ADVANCED_FACE('',(#17854),#6685,.T.) ;
#65140 = ADVANCED_FACE('',(#17855),#63085,.T.) ;
#65141 = ADVANCED_FACE('',(#17856),#6686,.F.) ;
#65142 = ADVANCED_FACE('',(#17857),#6687,.F.) ;
#65143 = ADVANCED_FACE('',(#17858),#6688,.F.) ;
#65144 = ADVANCED_FACE('',(#17859),#4384,.F.) ;
#65145 = ADVANCED_FACE('',(#17860),#63086,.T.) ;
#65146 = ADVANCED_FACE('',(#17861),#63087,.T.) ;
#65147 = ADVANCED_FACE('',(#17862),#4385,.F.) ;
#65148 = ADVANCED_FACE('',(#17863),#63088,.F.) ;
#65149 = ADVANCED_FACE('',(#17864),#6689,.F.) ;
#65150 = ADVANCED_FACE('',(#17865),#63089,.T.) ;
#65151 = ADVANCED_FACE('',(#17866),#6690,.T.) ;
#65152 = ADVANCED_FACE('',(#17867),#6691,.F.) ;
#65153 = ADVANCED_FACE('',(#17868),#4386,.F.) ;
#65154 = ADVANCED_FACE('',(#17869),#63090,.T.) ;
#65155 = ADVANCED_FACE('',(#17870),#63091,.F.) ;
#65156 = ADVANCED_FACE('',(#17871),#6692,.F.) ;
#65157 = ADVANCED_FACE('',(#17872),#6693,.F.) ;
#65158 = ADVANCED_FACE('',(#17873),#6694,.T.) ;
#65159 = ADVANCED_FACE('',(#17874),#6695,.F.) ;
#65160 = ADVANCED_FACE('',(#17875),#4387,.F.) ;
#65161 = ADVANCED_FACE('',(#17876),#63092,.F.) ;
#65162 = ADVANCED_FACE('',(#17877),#6696,.F.) ;
#65163 = ADVANCED_FACE('',(#17878),#4388,.T.) ;
#65164 = ADVANCED_FACE('',(#17879),#6697,.T.) ;
#65165 = ADVANCED_FACE('',(#17880),#6698,.T.) ;
#65166 = ADVANCED_FACE('',(#17881),#6699,.T.) ;
#65167 = ADVANCED_FACE('',(#17882),#6700,.T.) ;
#65168 = ADVANCED_FACE('',(#17883),#6701,.T.) ;
#65169 = ADVANCED_FACE('',(#17884),#63093,.F.) ;
#65170 = ADVANCED_FACE('',(#17885),#6702,.F.) ;
#65171 = ADVANCED_FACE('',(#17886),#4389,.F.) ;
#65172 = ADVANCED_FACE('',(#17887),#6703,.T.) ;
#65173 = ADVANCED_FACE('',(#17888),#6704,.T.) ;
#65174 = ADVANCED_FACE('',(#17889),#6705,.F.) ;
#65175 = ADVANCED_FACE('',(#17890),#6706,.T.) ;
#65176 = ADVANCED_FACE('',(#17891),#63094,.T.) ;
#65177 = ADVANCED_FACE('',(#17892),#6707,.F.) ;
#65178 = ADVANCED_FACE('',(#17893),#4390,.T.) ;
#65179 = ADVANCED_FACE('',(#17894),#4391,.F.) ;
#65180 = ADVANCED_FACE('',(#17895),#6708,.T.) ;
#65181 = ADVANCED_FACE('',(#17896),#6709,.T.) ;
#65182 = ADVANCED_FACE('',(#17897),#4392,.F.) ;
#65183 = ADVANCED_FACE('',(#17898),#6710,.T.) ;
#65184 = ADVANCED_FACE('',(#17899),#6711,.F.) ;
#65185 = ADVANCED_FACE('',(#17900),#63095,.T.) ;
#65186 = ADVANCED_FACE('',(#17901),#63096,.T.) ;
#65187 = ADVANCED_FACE('',(#17902),#6712,.F.) ;
#65188 = ADVANCED_FACE('',(#17903),#63097,.F.) ;
#65189 = ADVANCED_FACE('',(#17904),#4393,.F.) ;
#65190 = ADVANCED_FACE('',(#17905),#6713,.T.) ;
#65191 = ADVANCED_FACE('',(#17906),#6714,.T.) ;
#65192 = ADVANCED_FACE('',(#17907),#6715,.F.) ;
#65193 = ADVANCED_FACE('',(#17908),#63098,.T.) ;
#65194 = ADVANCED_FACE('',(#17909),#6716,.T.) ;
#65195 = ADVANCED_FACE('',(#17910),#6717,.F.) ;
#65196 = ADVANCED_FACE('',(#17911),#4394,.F.) ;
#65197 = ADVANCED_FACE('',(#17912),#6718,.T.) ;
#65198 = ADVANCED_FACE('',(#17913),#6719,.F.) ;
#65199 = ADVANCED_FACE('',(#17914),#63099,.F.) ;
#65200 = ADVANCED_FACE('',(#17915),#6720,.F.) ;
#65201 = ADVANCED_FACE('',(#17916),#6721,.T.) ;
#65202 = ADVANCED_FACE('',(#17917),#63100,.T.) ;
#65203 = ADVANCED_FACE('',(#17918),#4395,.F.) ;
#65204 = ADVANCED_FACE('',(#17919),#63101,.F.) ;
#65205 = ADVANCED_FACE('',(#17920),#63102,.T.) ;
#65206 = ADVANCED_FACE('',(#17921),#6722,.F.) ;
#65207 = ADVANCED_FACE('',(#17922),#6723,.F.) ;
#65208 = ADVANCED_FACE('',(#17923),#63103,.F.) ;
#65209 = ADVANCED_FACE('',(#17924),#6724,.T.) ;
#65210 = ADVANCED_FACE('',(#17925),#6725,.F.) ;
#65211 = ADVANCED_FACE('',(#17926),#6726,.F.) ;
#65212 = ADVANCED_FACE('',(#17927),#63104,.T.) ;
#65213 = ADVANCED_FACE('',(#17928),#4396,.F.) ;
#65214 = ADVANCED_FACE('',(#17929),#63105,.F.) ;
#65215 = ADVANCED_FACE('',(#17930),#4397,.F.) ;
#65216 = ADVANCED_FACE('',(#17931),#6727,.T.) ;
#65217 = ADVANCED_FACE('',(#17932),#63106,.F.) ;
#65218 = ADVANCED_FACE('',(#17933),#6728,.F.) ;
#65219 = ADVANCED_FACE('',(#17934),#63107,.F.) ;
#65220 = ADVANCED_FACE('',(#17935),#6729,.F.) ;
#65221 = ADVANCED_FACE('',(#17936),#6730,.T.) ;
#65222 = ADVANCED_FACE('',(#17937),#451,.F.) ;
#65223 = ADVANCED_FACE('',(#17938),#4398,.F.) ;
#65224 = ADVANCED_FACE('',(#17939),#4399,.F.) ;
#65225 = ADVANCED_FACE('',(#17940),#63108,.T.) ;
#65226 = ADVANCED_FACE('',(#17941),#63109,.F.) ;
#65227 = ADVANCED_FACE('',(#17942),#6731,.F.) ;
#65228 = ADVANCED_FACE('',(#17943),#63110,.T.) ;
#65229 = ADVANCED_FACE('',(#17944),#452,.F.) ;
#65230 = ADVANCED_FACE('',(#17945),#63111,.T.) ;
#65231 = ADVANCED_FACE('',(#17946),#6732,.T.) ;
#65232 = ADVANCED_FACE('',(#17947),#63112,.T.) ;
#65233 = ADVANCED_FACE('',(#17948),#6733,.T.) ;
#65234 = ADVANCED_FACE('',(#17949),#63113,.T.) ;
#65235 = ADVANCED_FACE('',(#17950),#6734,.T.) ;
#65236 = ADVANCED_FACE('',(#17951),#63114,.T.) ;
#65237 = ADVANCED_FACE('',(#17952),#6735,.T.) ;
#65238 = ADVANCED_FACE('',(#17953),#4400,.T.) ;
#65239 = ADVANCED_FACE('',(#17954),#6736,.T.) ;
#65240 = ADVANCED_FACE('',(#17955),#6737,.T.) ;
#65241 = ADVANCED_FACE('',(#17956),#6738,.T.) ;
#65242 = ADVANCED_FACE('',(#17957),#6739,.T.) ;
#65243 = ADVANCED_FACE('',(#17958),#6740,.T.) ;
#65244 = ADVANCED_FACE('',(#17959),#4401,.T.) ;
#65245 = ADVANCED_FACE('',(#17960),#4402,.T.) ;
#65246 = ADVANCED_FACE('',(#17961),#6741,.T.) ;
#65247 = ADVANCED_FACE('',(#17962),#6742,.T.) ;
#65248 = ADVANCED_FACE('',(#17963),#4403,.T.) ;
#65249 = ADVANCED_FACE('',(#17964),#6743,.T.) ;
#65250 = ADVANCED_FACE('',(#17965),#6744,.T.) ;
#65251 = ADVANCED_FACE('',(#17966),#63115,.T.) ;
#65252 = ADVANCED_FACE('',(#17967),#6745,.T.) ;
#65253 = ADVANCED_FACE('',(#17968),#6746,.T.) ;
#65254 = ADVANCED_FACE('',(#17969),#6747,.T.) ;
#65255 = ADVANCED_FACE('',(#17970),#6748,.T.) ;
#65256 = ADVANCED_FACE('',(#17971),#6749,.T.) ;
#65257 = ADVANCED_FACE('',(#17972),#4404,.T.) ;
#65258 = ADVANCED_FACE('',(#17973),#6750,.T.) ;
#65259 = ADVANCED_FACE('',(#17974),#6751,.T.) ;
#65260 = ADVANCED_FACE('',(#17975),#4405,.T.) ;
#65261 = ADVANCED_FACE('',(#17976),#6752,.T.) ;
#65262 = ADVANCED_FACE('',(#17977),#6753,.T.) ;
#65263 = ADVANCED_FACE('',(#17978),#6754,.T.) ;
#65264 = ADVANCED_FACE('',(#17979),#6755,.T.) ;
#65265 = ADVANCED_FACE('',(#17980),#4406,.T.) ;
#65266 = ADVANCED_FACE('',(#17981),#4407,.T.) ;
#65267 = ADVANCED_FACE('',(#17982),#6756,.T.) ;
#65268 = ADVANCED_FACE('',(#17983),#6757,.T.) ;
#65269 = ADVANCED_FACE('',(#17984),#6758,.T.) ;
#65270 = ADVANCED_FACE('',(#17985),#4408,.T.) ;
#65271 = ADVANCED_FACE('',(#17986),#6759,.T.) ;
#65272 = ADVANCED_FACE('',(#17987),#6760,.T.) ;
#65273 = ADVANCED_FACE('',(#17988),#4409,.T.) ;
#65274 = ADVANCED_FACE('',(#17989),#6761,.T.) ;
#65275 = ADVANCED_FACE('',(#17990),#6762,.T.) ;
#65276 = ADVANCED_FACE('',(#17991),#6763,.T.) ;
#65277 = ADVANCED_FACE('',(#17992),#4410,.T.) ;
#65278 = ADVANCED_FACE('',(#17993),#6764,.T.) ;
#65279 = ADVANCED_FACE('',(#17994),#6765,.T.) ;
#65280 = ADVANCED_FACE('',(#17995),#4411,.T.) ;
#65281 = ADVANCED_FACE('',(#17996),#6766,.T.) ;
#65282 = ADVANCED_FACE('',(#17997),#6767,.F.) ;
#65283 = ADVANCED_FACE('',(#17998),#6768,.T.) ;
#65284 = ADVANCED_FACE('',(#17999),#6769,.F.) ;
#65285 = ADVANCED_FACE('',(#18000),#6770,.T.) ;
#65286 = ADVANCED_FACE('',(#18001),#6771,.T.) ;
#65287 = ADVANCED_FACE('',(#18002),#6772,.T.) ;
#65288 = ADVANCED_FACE('',(#18003),#63116,.T.) ;
#65289 = ADVANCED_FACE('',(#18004),#6773,.T.) ;
#65290 = ADVANCED_FACE('',(#18005),#453,.F.) ;
#65291 = ADVANCED_FACE('',(#18006),#6774,.F.) ;
#65292 = ADVANCED_FACE('',(#18007),#4412,.F.) ;
#65293 = ADVANCED_FACE('',(#18008),#6775,.F.) ;
#65294 = ADVANCED_FACE('',(#18009),#454,.F.) ;
#65295 = ADVANCED_FACE('',(#18010),#455,.F.) ;
#65296 = ADVANCED_FACE('',(#18011),#6776,.F.) ;
#65297 = ADVANCED_FACE('',(#18012),#4413,.F.) ;
#65298 = ADVANCED_FACE('',(#18013),#6777,.F.) ;
#65299 = ADVANCED_FACE('',(#18014),#456,.F.) ;
#65300 = ADVANCED_FACE('',(#18015),#457,.F.) ;
#65301 = ADVANCED_FACE('',(#18016),#6778,.F.) ;
#65302 = ADVANCED_FACE('',(#18017),#458,.F.) ;
#65303 = ADVANCED_FACE('',(#18018),#6779,.T.) ;
#65304 = ADVANCED_FACE('',(#18019),#459,.T.) ;
#65305 = ADVANCED_FACE('',(#18020),#460,.F.) ;
#65306 = ADVANCED_FACE('',(#18021),#6780,.T.) ;
#65307 = ADVANCED_FACE('',(#18022),#6781,.T.) ;
#65308 = ADVANCED_FACE('',(#18023),#6782,.F.) ;
#65309 = ADVANCED_FACE('',(#18024),#461,.T.) ;
#65310 = ADVANCED_FACE('',(#18025),#462,.F.) ;
#65311 = ADVANCED_FACE('',(#18026),#6783,.T.) ;
#65312 = ADVANCED_FACE('',(#18027),#4414,.T.) ;
#65313 = ADVANCED_FACE('',(#18028),#463,.T.) ;
#65314 = ADVANCED_FACE('',(#18029),#4415,.T.) ;
#65315 = ADVANCED_FACE('',(#18030),#4416,.T.) ;
#65316 = ADVANCED_FACE('',(#18031),#6784,.T.) ;
#65317 = ADVANCED_FACE('',(#18032),#6785,.T.) ;
#65318 = ADVANCED_FACE('',(#18033),#4417,.T.) ;
#65319 = ADVANCED_FACE('',(#18034),#4418,.T.) ;
#65320 = ADVANCED_FACE('',(#18035),#6786,.T.) ;
#65321 = ADVANCED_FACE('',(#18036),#6787,.T.) ;
#65322 = ADVANCED_FACE('',(#18037),#4419,.T.) ;
#65323 = ADVANCED_FACE('',(#18038),#4420,.T.) ;
#65324 = ADVANCED_FACE('',(#18039),#6788,.T.) ;
#65325 = ADVANCED_FACE('',(#18040),#6789,.T.) ;
#65326 = ADVANCED_FACE('',(#18041),#4421,.T.) ;
#65327 = ADVANCED_FACE('',(#18042),#4422,.T.) ;
#65328 = ADVANCED_FACE('',(#18043),#6790,.T.) ;
#65329 = ADVANCED_FACE('',(#18044),#6791,.T.) ;
#65330 = ADVANCED_FACE('',(#18045),#4423,.T.) ;
#65331 = ADVANCED_FACE('',(#18046),#6792,.T.) ;
#65332 = ADVANCED_FACE('',(#18047),#4424,.T.) ;
#65333 = ADVANCED_FACE('',(#18048),#464,.T.) ;
#65334 = ADVANCED_FACE('',(#18049),#4425,.T.) ;
#65335 = ADVANCED_FACE('',(#18050),#6793,.T.) ;
#65336 = ADVANCED_FACE('',(#18051),#465,.T.) ;
#65337 = ADVANCED_FACE('',(#18052),#6794,.T.) ;
#65338 = ADVANCED_FACE('',(#18053),#466,.T.) ;
#65339 = ADVANCED_FACE('',(#18054),#6795,.T.) ;
#65340 = ADVANCED_FACE('',(#18055),#6796,.T.) ;
#65341 = ADVANCED_FACE('',(#18056),#6797,.T.) ;
#65342 = ADVANCED_FACE('',(#18057),#5468,.F.) ;
#65343 = ADVANCED_FACE('',(#18058),#5469,.F.) ;
#65344 = ADVANCED_FACE('',(#18059),#5470,.F.) ;
#65345 = ADVANCED_FACE('',(#18060),#5471,.F.) ;
#65346 = ADVANCED_FACE('',(#18061),#5472,.F.) ;
#65347 = ADVANCED_FACE('',(#18062),#5473,.F.) ;
#65348 = ADVANCED_FACE('',(#18063),#5474,.F.) ;
#65349 = ADVANCED_FACE('',(#18064),#5475,.T.) ;
#65350 = ADVANCED_FACE('',(#18065),#5476,.F.) ;
#65351 = ADVANCED_FACE('',(#18066),#5477,.F.) ;
#65352 = ADVANCED_FACE('',(#18067),#6798,.T.) ;
#65353 = ADVANCED_FACE('',(#18068),#6799,.T.) ;
#65354 = ADVANCED_FACE('',(#18069),#6800,.F.) ;
#65355 = ADVANCED_FACE('',(#18070),#6801,.F.) ;
#65356 = ADVANCED_FACE('',(#18071,#5029,#5030),#5478,.F.) ;
#65357 = ADVANCED_FACE('',(#18072),#5479,.F.) ;
#65358 = ADVANCED_FACE('',(#18073),#5480,.T.) ;
#65359 = ADVANCED_FACE('',(#18074),#4426,.T.) ;
#65360 = ADVANCED_FACE('',(#18075),#5481,.F.) ;
#65361 = ADVANCED_FACE('',(#18076),#5482,.F.) ;
#65362 = ADVANCED_FACE('',(#18077),#63117,.T.) ;
#65363 = ADVANCED_FACE('',(#18078),#63118,.F.) ;
#65364 = ADVANCED_FACE('',(#18079),#4427,.F.) ;
#65365 = ADVANCED_FACE('',(#18080),#6802,.F.) ;
#65366 = ADVANCED_FACE('',(#18081),#63119,.T.) ;
#65367 = ADVANCED_FACE('',(#18082),#63120,.F.) ;
#65368 = ADVANCED_FACE('',(#18083),#4428,.F.) ;
#65369 = ADVANCED_FACE('',(#18084),#6803,.F.) ;
#65370 = ADVANCED_FACE('',(#18085),#63121,.T.) ;
#65371 = ADVANCED_FACE('',(#18086),#63122,.F.) ;
#65372 = ADVANCED_FACE('',(#18087),#4429,.F.) ;
#65373 = ADVANCED_FACE('',(#18088),#6804,.F.) ;
#65374 = ADVANCED_FACE('',(#18089),#63123,.T.) ;
#65375 = ADVANCED_FACE('',(#18090),#63124,.F.) ;
#65376 = ADVANCED_FACE('',(#18091),#4430,.F.) ;
#65377 = ADVANCED_FACE('',(#18092),#6805,.F.) ;
#65378 = ADVANCED_FACE('',(#18093),#63125,.T.) ;
#65379 = ADVANCED_FACE('',(#18094),#63126,.F.) ;
#65380 = ADVANCED_FACE('',(#18095),#4431,.F.) ;
#65381 = ADVANCED_FACE('',(#18096),#6806,.F.) ;
#65382 = ADVANCED_FACE('',(#18097),#63127,.T.) ;
#65383 = ADVANCED_FACE('',(#18098),#63128,.F.) ;
#65384 = ADVANCED_FACE('',(#18099),#4432,.F.) ;
#65385 = ADVANCED_FACE('',(#18100),#6807,.F.) ;
#65386 = ADVANCED_FACE('',(#18101),#63129,.T.) ;
#65387 = ADVANCED_FACE('',(#18102),#63130,.F.) ;
#65388 = ADVANCED_FACE('',(#18103),#4433,.F.) ;
#65389 = ADVANCED_FACE('',(#18104),#6808,.F.) ;
#65390 = ADVANCED_FACE('',(#18105),#63131,.T.) ;
#65391 = ADVANCED_FACE('',(#18106),#63132,.F.) ;
#65392 = ADVANCED_FACE('',(#18107),#4434,.F.) ;
#65393 = ADVANCED_FACE('',(#18108),#6809,.F.) ;
#65394 = ADVANCED_FACE('',(#18109),#63133,.T.) ;
#65395 = ADVANCED_FACE('',(#18110),#63134,.T.) ;
#65396 = ADVANCED_FACE('',(#18111),#63135,.T.) ;
#65397 = ADVANCED_FACE('',(#18112),#63136,.T.) ;
#65398 = ADVANCED_FACE('',(#18113),#63137,.T.) ;
#65399 = ADVANCED_FACE('',(#18114),#63138,.T.) ;
#65400 = ADVANCED_FACE('',(#18115),#63139,.T.) ;
#65401 = ADVANCED_FACE('',(#18116),#63140,.T.) ;
#65402 = ADVANCED_FACE('',(#18117),#63141,.T.) ;
#65403 = ADVANCED_FACE('',(#18118),#63142,.T.) ;
#65404 = ADVANCED_FACE('',(#18119),#63143,.F.) ;
#65405 = ADVANCED_FACE('',(#18120),#4435,.F.) ;
#65406 = ADVANCED_FACE('',(#18121),#6810,.F.) ;
#65407 = ADVANCED_FACE('',(#18122),#6811,.T.) ;
#65408 = ADVANCED_FACE('',(#18123),#6812,.T.) ;
#65409 = ADVANCED_FACE('',(#18124),#6813,.T.) ;
#65410 = ADVANCED_FACE('',(#18125),#6814,.T.) ;
#65411 = ADVANCED_FACE('',(#18126),#6815,.T.) ;
#65412 = ADVANCED_FACE('',(#18127),#6816,.T.) ;
#65413 = ADVANCED_FACE('',(#18128),#6817,.T.) ;
#65414 = ADVANCED_FACE('',(#18129),#6818,.T.) ;
#65415 = ADVANCED_FACE('',(#18130),#6819,.T.) ;
#65416 = ADVANCED_FACE('',(#18131),#6820,.F.) ;
#65417 = ADVANCED_FACE('',(#18132),#6821,.F.) ;
#65418 = ADVANCED_FACE('',(#18133),#6822,.F.) ;
#65419 = ADVANCED_FACE('',(#18134),#6823,.F.) ;
#65420 = ADVANCED_FACE('',(#18135),#6824,.F.) ;
#65421 = ADVANCED_FACE('',(#18136),#6825,.F.) ;
#65422 = ADVANCED_FACE('',(#18137),#6826,.F.) ;
#65423 = ADVANCED_FACE('',(#18138),#6827,.F.) ;
#65424 = ADVANCED_FACE('',(#18139),#6828,.F.) ;
#65425 = ADVANCED_FACE('',(#18140),#63144,.T.) ;
#65426 = ADVANCED_FACE('',(#18141),#63145,.T.) ;
#65427 = ADVANCED_FACE('',(#18142),#63146,.F.) ;
#65428 = ADVANCED_FACE('',(#18143),#4436,.F.) ;
#65429 = ADVANCED_FACE('',(#18144),#6829,.F.) ;
#65430 = ADVANCED_FACE('',(#18145),#6830,.T.) ;
#65431 = ADVANCED_FACE('',(#18146),#6831,.F.) ;
#65432 = ADVANCED_FACE('',(#18147),#5483,.T.) ;
#65433 = ADVANCED_FACE('',(#18148),#5484,.T.) ;
#65434 = ADVANCED_FACE('',(#18149),#5485,.T.) ;
#65435 = ADVANCED_FACE('',(#18150),#5486,.T.) ;
#65436 = ADVANCED_FACE('',(#18151),#5487,.T.) ;
#65437 = ADVANCED_FACE('',(#18152),#5488,.T.) ;
#65438 = ADVANCED_FACE('',(#18153),#5489,.T.) ;
#65439 = ADVANCED_FACE('',(#18154),#5490,.T.) ;
#65440 = ADVANCED_FACE('',(#18155),#5491,.T.) ;
#65441 = ADVANCED_FACE('',(#18156),#5492,.F.) ;
#65442 = ADVANCED_FACE('',(#18157),#5493,.F.) ;
#65443 = ADVANCED_FACE('',(#18158),#5494,.F.) ;
#65444 = ADVANCED_FACE('',(#18159),#5495,.F.) ;
#65445 = ADVANCED_FACE('',(#18160),#5496,.F.) ;
#65446 = ADVANCED_FACE('',(#18161),#5497,.F.) ;
#65447 = ADVANCED_FACE('',(#18162),#5498,.F.) ;
#65448 = ADVANCED_FACE('',(#18163),#5499,.F.) ;
#65449 = ADVANCED_FACE('',(#18164),#5500,.F.) ;
#65450 = ADVANCED_FACE('',(#18165),#5501,.F.) ;
#65451 = ADVANCED_FACE('',(#18166),#5502,.F.) ;
#65452 = ADVANCED_FACE('',(#18167),#5503,.F.) ;
#65453 = ADVANCED_FACE('',(#18168),#5504,.F.) ;
#65454 = ADVANCED_FACE('',(#18169),#5505,.F.) ;
#65455 = ADVANCED_FACE('',(#18170),#5506,.F.) ;
#65456 = ADVANCED_FACE('',(#18171),#5507,.F.) ;
#65457 = ADVANCED_FACE('',(#18172),#5508,.F.) ;
#65458 = ADVANCED_FACE('',(#18173),#5509,.F.) ;
#65459 = ADVANCED_FACE('',(#18174),#6832,.T.) ;
#65460 = ADVANCED_FACE('',(#18175),#6833,.T.) ;
#65461 = ADVANCED_FACE('',(#18176),#6834,.T.) ;
#65462 = ADVANCED_FACE('',(#18177),#6835,.T.) ;
#65463 = ADVANCED_FACE('',(#18178),#6836,.T.) ;
#65464 = ADVANCED_FACE('',(#18179),#6837,.T.) ;
#65465 = ADVANCED_FACE('',(#18180),#6838,.T.) ;
#65466 = ADVANCED_FACE('',(#18181),#6839,.T.) ;
#65467 = ADVANCED_FACE('',(#18182),#6840,.T.) ;
#65468 = ADVANCED_FACE('',(#18183),#5510,.T.) ;
#65469 = ADVANCED_FACE('',(#18184),#5511,.F.) ;
#65470 = ADVANCED_FACE('',(#18185),#5512,.F.) ;
#65471 = ADVANCED_FACE('',(#18186),#6841,.T.) ;
#65472 = ADVANCED_FACE('',(#18187),#6842,.T.) ;
#65473 = ADVANCED_FACE('',(#18188),#5513,.T.) ;
#65474 = ADVANCED_FACE('',(#18189),#6843,.T.) ;
#65475 = ADVANCED_FACE('',(#18190),#5514,.T.) ;
#65476 = ADVANCED_FACE('',(#18191),#6844,.T.) ;
#65477 = ADVANCED_FACE('',(#18192),#5515,.T.) ;
#65478 = ADVANCED_FACE('',(#18193),#6845,.F.) ;
#65479 = ADVANCED_FACE('',(#18194),#5516,.T.) ;
#65480 = ADVANCED_FACE('',(#18195),#6846,.T.) ;
#65481 = ADVANCED_FACE('',(#18196),#5517,.T.) ;
#65482 = ADVANCED_FACE('',(#18197),#6847,.T.) ;
#65483 = ADVANCED_FACE('',(#18198),#5518,.T.) ;
#65484 = ADVANCED_FACE('',(#18199),#6848,.F.) ;
#65485 = ADVANCED_FACE('',(#18200),#5519,.T.) ;
#65486 = ADVANCED_FACE('',(#18201),#6849,.T.) ;
#65487 = ADVANCED_FACE('',(#18202,#5031,#5032,#5033,#5034,#5035,#5036,#5037,
#5038,#5039,#5040),#5520,.T.) ;
#65488 = ADVANCED_FACE('',(#18203),#5521,.F.) ;
#65489 = ADVANCED_FACE('',(#18204),#5522,.T.) ;
#65490 = ADVANCED_FACE('',(#18205),#5523,.T.) ;
#65491 = ADVANCED_FACE('',(#18206),#5524,.F.) ;
#65492 = ADVANCED_FACE('',(#18207),#5525,.F.) ;
#65493 = ADVANCED_FACE('',(#18208),#5526,.F.) ;
#65494 = ADVANCED_FACE('',(#18209),#5527,.F.) ;
#65495 = ADVANCED_FACE('',(#18210),#5528,.F.) ;
#65496 = ADVANCED_FACE('',(#18211),#6850,.T.) ;
#65497 = ADVANCED_FACE('',(#18212),#5529,.F.) ;
#65498 = ADVANCED_FACE('',(#18213),#6851,.T.) ;
#65499 = ADVANCED_FACE('',(#18214),#5530,.F.) ;
#65500 = ADVANCED_FACE('',(#18215),#6852,.F.) ;
#65501 = ADVANCED_FACE('',(#18216),#5531,.F.) ;
#65502 = ADVANCED_FACE('',(#18217),#6853,.F.) ;
#65503 = ADVANCED_FACE('',(#18218),#5532,.F.) ;
#65504 = ADVANCED_FACE('',(#18219),#5533,.F.) ;
#65505 = ADVANCED_FACE('',(#18220),#6854,.F.) ;
#65506 = ADVANCED_FACE('',(#18221),#5534,.F.) ;
#65507 = ADVANCED_FACE('',(#18222),#6855,.T.) ;
#65508 = ADVANCED_FACE('',(#18223),#5535,.F.) ;
#65509 = ADVANCED_FACE('',(#18224),#6856,.T.) ;
#65510 = ADVANCED_FACE('',(#18225),#5536,.F.) ;
#65511 = ADVANCED_FACE('',(#18226),#6857,.F.) ;
#65512 = ADVANCED_FACE('',(#18227),#5537,.F.) ;
#65513 = ADVANCED_FACE('',(#18228),#6858,.F.) ;
#65514 = ADVANCED_FACE('',(#18229),#5538,.F.) ;
#65515 = ADVANCED_FACE('',(#18230),#6859,.F.) ;
#65516 = ADVANCED_FACE('',(#18231),#6860,.T.) ;
#65517 = ADVANCED_FACE('',(#18232),#6861,.F.) ;
#65518 = ADVANCED_FACE('',(#18233),#5539,.F.) ;
#65519 = ADVANCED_FACE('',(#18234),#6862,.F.) ;
#65520 = ADVANCED_FACE('',(#18235),#5540,.F.) ;
#65521 = ADVANCED_FACE('',(#18236),#6863,.F.) ;
#65522 = ADVANCED_FACE('',(#18237),#5541,.F.) ;
#65523 = ADVANCED_FACE('',(#18238,#5041),#5542,.F.) ;
#65524 = ADVANCED_FACE('',(#18239,#5042),#5543,.T.) ;
#65525 = ADVANCED_FACE('',(#18240),#6864,.T.) ;
#65526 = ADVANCED_FACE('',(#18241),#6865,.F.) ;
#65527 = ADVANCED_FACE('',(#18242),#4437,.F.) ;
#65528 = ADVANCED_FACE('',(#18243),#4438,.T.) ;
#65529 = ADVANCED_FACE('',(#18244),#63147,.T.) ;
#65530 = ADVANCED_FACE('',(#18245),#6866,.F.) ;
#65531 = ADVANCED_FACE('',(#18246),#6867,.F.) ;
#65532 = ADVANCED_FACE('',(#18247),#6868,.T.) ;
#65533 = ADVANCED_FACE('',(#18248),#6869,.T.) ;
#65534 = ADVANCED_FACE('',(#18249),#6870,.T.) ;
#65535 = ADVANCED_FACE('',(#18250),#6871,.F.) ;
#65536 = ADVANCED_FACE('',(#18251),#4439,.F.) ;
#65537 = ADVANCED_FACE('',(#18252),#63148,.F.) ;
#65538 = ADVANCED_FACE('',(#18253),#63149,.F.) ;
#65539 = ADVANCED_FACE('',(#18254),#63150,.T.) ;
#65540 = ADVANCED_FACE('',(#18255),#6872,.F.) ;
#65541 = ADVANCED_FACE('',(#18256),#6873,.F.) ;
#65542 = ADVANCED_FACE('',(#18257),#6874,.F.) ;
#65543 = ADVANCED_FACE('',(#18258),#6875,.T.) ;
#65544 = ADVANCED_FACE('',(#18259),#6876,.T.) ;
#65545 = ADVANCED_FACE('',(#18260),#63151,.F.) ;
#65546 = ADVANCED_FACE('',(#18261),#4440,.F.) ;
#65547 = ADVANCED_FACE('',(#18262),#4441,.T.) ;
#65548 = ADVANCED_FACE('',(#18263),#6877,.T.) ;
#65549 = ADVANCED_FACE('',(#18264),#4442,.F.) ;
#65550 = ADVANCED_FACE('',(#18265),#4443,.T.) ;
#65551 = ADVANCED_FACE('',(#18266),#6878,.F.) ;
#65552 = ADVANCED_FACE('',(#18267),#6879,.F.) ;
#65553 = ADVANCED_FACE('',(#18268),#6880,.T.) ;
#65554 = ADVANCED_FACE('',(#18269),#63152,.T.) ;
#65555 = ADVANCED_FACE('',(#18270),#6881,.F.) ;
#65556 = ADVANCED_FACE('',(#18271),#6882,.T.) ;
#65557 = ADVANCED_FACE('',(#18272),#6883,.F.) ;
#65558 = ADVANCED_FACE('',(#18273),#4444,.F.) ;
#65559 = ADVANCED_FACE('',(#18274),#63153,.T.) ;
#65560 = ADVANCED_FACE('',(#18275),#6884,.T.) ;
#65561 = ADVANCED_FACE('',(#18276),#4445,.F.) ;
#65562 = ADVANCED_FACE('',(#18277),#63154,.F.) ;
#65563 = ADVANCED_FACE('',(#18278),#6885,.F.) ;
#65564 = ADVANCED_FACE('',(#18279),#6886,.T.) ;
#65565 = ADVANCED_FACE('',(#18280),#63155,.T.) ;
#65566 = ADVANCED_FACE('',(#18281),#6887,.F.) ;
#65567 = ADVANCED_FACE('',(#18282),#63156,.T.) ;
#65568 = ADVANCED_FACE('',(#18283),#6888,.T.) ;
#65569 = ADVANCED_FACE('',(#18284),#6889,.T.) ;
#65570 = ADVANCED_FACE('',(#18285),#4446,.T.) ;
#65571 = ADVANCED_FACE('',(#18286),#4447,.T.) ;
#65572 = ADVANCED_FACE('',(#18287),#6890,.T.) ;
#65573 = ADVANCED_FACE('',(#18288),#6891,.T.) ;
#65574 = ADVANCED_FACE('',(#18289),#63157,.T.) ;
#65575 = ADVANCED_FACE('',(#18290),#4448,.T.) ;
#65576 = ADVANCED_FACE('',(#18291),#6892,.T.) ;
#65577 = ADVANCED_FACE('',(#18292),#6893,.T.) ;
#65578 = ADVANCED_FACE('',(#18293),#4449,.T.) ;
#65579 = ADVANCED_FACE('',(#18294),#63158,.T.) ;
#65580 = ADVANCED_FACE('',(#18295),#6894,.T.) ;
#65581 = ADVANCED_FACE('',(#18296),#6895,.T.) ;
#65582 = ADVANCED_FACE('',(#18297),#4450,.T.) ;
#65583 = ADVANCED_FACE('',(#18298),#4451,.T.) ;
#65584 = ADVANCED_FACE('',(#18299),#6896,.T.) ;
#65585 = ADVANCED_FACE('',(#18300),#6897,.T.) ;
#65586 = ADVANCED_FACE('',(#18301),#4452,.T.) ;
#65587 = ADVANCED_FACE('',(#18302),#4453,.T.) ;
#65588 = ADVANCED_FACE('',(#18303),#6898,.T.) ;
#65589 = ADVANCED_FACE('',(#18304),#6899,.T.) ;
#65590 = ADVANCED_FACE('',(#18305),#63159,.T.) ;
#65591 = ADVANCED_FACE('',(#18306),#4454,.T.) ;
#65592 = ADVANCED_FACE('',(#18307),#6900,.T.) ;
#65593 = ADVANCED_FACE('',(#18308),#6901,.T.) ;
#65594 = ADVANCED_FACE('',(#18309),#4455,.T.) ;
#65595 = ADVANCED_FACE('',(#18310),#63160,.T.) ;
#65596 = ADVANCED_FACE('',(#18311),#6902,.T.) ;
#65597 = ADVANCED_FACE('',(#18312),#6903,.T.) ;
#65598 = ADVANCED_FACE('',(#18313),#4456,.T.) ;
#65599 = ADVANCED_FACE('',(#18314),#4457,.T.) ;
#65600 = ADVANCED_FACE('',(#18315),#6904,.T.) ;
#65601 = ADVANCED_FACE('',(#18316),#6905,.T.) ;
#65602 = ADVANCED_FACE('',(#18317),#4458,.T.) ;
#65603 = ADVANCED_FACE('',(#18318),#6906,.F.) ;
#65604 = ADVANCED_FACE('',(#18319),#63161,.F.) ;
#65605 = ADVANCED_FACE('',(#18320),#4459,.F.) ;
#65606 = ADVANCED_FACE('',(#18321),#6907,.F.) ;
#65607 = ADVANCED_FACE('',(#18322),#6908,.F.) ;
#65608 = ADVANCED_FACE('',(#18323),#63162,.F.) ;
#65609 = ADVANCED_FACE('',(#18324),#4460,.F.) ;
#65610 = ADVANCED_FACE('',(#18325),#6909,.F.) ;
#65611 = ADVANCED_FACE('',(#18326),#6910,.F.) ;
#65612 = ADVANCED_FACE('',(#18327),#4461,.F.) ;
#65613 = ADVANCED_FACE('',(#18328),#4462,.F.) ;
#65614 = ADVANCED_FACE('',(#18329),#6911,.F.) ;
#65615 = ADVANCED_FACE('',(#18330),#63163,.F.) ;
#65616 = ADVANCED_FACE('',(#18331),#4463,.F.) ;
#65617 = ADVANCED_FACE('',(#18332),#4464,.F.) ;
#65618 = ADVANCED_FACE('',(#18333),#6912,.F.) ;
#65619 = ADVANCED_FACE('',(#18334),#6913,.F.) ;
#65620 = ADVANCED_FACE('',(#18335),#4465,.F.) ;
#65621 = ADVANCED_FACE('',(#18336),#6914,.F.) ;
#65622 = ADVANCED_FACE('',(#18337),#6915,.F.) ;
#65623 = ADVANCED_FACE('',(#18338),#4466,.F.) ;
#65624 = ADVANCED_FACE('',(#18339),#4467,.F.) ;
#65625 = ADVANCED_FACE('',(#18340),#6916,.F.) ;
#65626 = ADVANCED_FACE('',(#18341),#6917,.F.) ;
#65627 = ADVANCED_FACE('',(#18342),#63164,.F.) ;
#65628 = ADVANCED_FACE('',(#18343),#63165,.F.) ;
#65629 = ADVANCED_FACE('',(#18344),#6918,.F.) ;
#65630 = ADVANCED_FACE('',(#18345),#6919,.T.) ;
#65631 = ADVANCED_FACE('',(#18346),#4468,.T.) ;
#65632 = ADVANCED_FACE('',(#18347),#4469,.T.) ;
#65633 = ADVANCED_FACE('',(#18348),#6920,.T.) ;
#65634 = ADVANCED_FACE('',(#18349),#6921,.T.) ;
#65635 = ADVANCED_FACE('',(#18350),#63166,.T.) ;
#65636 = ADVANCED_FACE('',(#18351),#63167,.T.) ;
#65637 = ADVANCED_FACE('',(#18352),#6922,.T.) ;
#65638 = ADVANCED_FACE('',(#18353),#6923,.T.) ;
#65639 = ADVANCED_FACE('',(#18354),#63168,.T.) ;
#65640 = ADVANCED_FACE('',(#18355),#6924,.T.) ;
#65641 = ADVANCED_FACE('',(#18356),#6925,.T.) ;
#65642 = ADVANCED_FACE('',(#18357),#63169,.T.) ;
#65643 = ADVANCED_FACE('',(#18358),#63170,.T.) ;
#65644 = ADVANCED_FACE('',(#18359),#6926,.T.) ;
#65645 = ADVANCED_FACE('',(#18360),#63171,.T.) ;
#65646 = ADVANCED_FACE('',(#18361),#63172,.T.) ;
#65647 = ADVANCED_FACE('',(#18362),#63173,.T.) ;
#65648 = ADVANCED_FACE('',(#18363),#6927,.T.) ;
#65649 = ADVANCED_FACE('',(#18364),#6928,.T.) ;
#65650 = ADVANCED_FACE('',(#18365),#4470,.T.) ;
#65651 = ADVANCED_FACE('',(#18366),#63174,.T.) ;
#65652 = ADVANCED_FACE('',(#18367),#6929,.T.) ;
#65653 = ADVANCED_FACE('',(#18368),#6930,.T.) ;
#65654 = ADVANCED_FACE('',(#18369),#4471,.T.) ;
#65655 = ADVANCED_FACE('',(#18370),#63175,.T.) ;
#65656 = ADVANCED_FACE('',(#18371),#6931,.T.) ;
#65657 = ADVANCED_FACE('',(#18372),#5544,.F.) ;
#65658 = ADVANCED_FACE('',(#18373),#5545,.F.) ;
#65659 = ADVANCED_FACE('',(#18374),#5546,.F.) ;
#65660 = ADVANCED_FACE('',(#18375),#5547,.F.) ;
#65661 = ADVANCED_FACE('',(#18376),#5548,.F.) ;
#65662 = ADVANCED_FACE('',(#18377),#5549,.T.) ;
#65663 = ADVANCED_FACE('',(#18378),#5550,.F.) ;
#65664 = ADVANCED_FACE('',(#18379),#6932,.T.) ;
#65665 = ADVANCED_FACE('',(#18380),#6933,.F.) ;
#65666 = ADVANCED_FACE('',(#18381),#5551,.F.) ;
#65667 = ADVANCED_FACE('',(#18382),#5552,.F.) ;
#65668 = ADVANCED_FACE('',(#18383),#5553,.F.) ;
#65669 = ADVANCED_FACE('',(#18384),#5554,.F.) ;
#65670 = ADVANCED_FACE('',(#18385),#5555,.F.) ;
#65671 = ADVANCED_FACE('',(#18386),#5556,.T.) ;
#65672 = ADVANCED_FACE('',(#18387),#5557,.F.) ;
#65673 = ADVANCED_FACE('',(#18388),#5558,.F.) ;
#65674 = ADVANCED_FACE('',(#18389),#5559,.F.) ;
#65675 = ADVANCED_FACE('',(#18390),#5560,.F.) ;
#65676 = ADVANCED_FACE('',(#18391),#5561,.F.) ;
#65677 = ADVANCED_FACE('',(#18392),#6934,.T.) ;
#65678 = ADVANCED_FACE('',(#18393),#6935,.T.) ;
#65679 = ADVANCED_FACE('',(#18394),#4472,.T.) ;
#65680 = ADVANCED_FACE('',(#18395),#6936,.T.) ;
#65681 = ADVANCED_FACE('',(#18396),#6937,.T.) ;
#65682 = ADVANCED_FACE('',(#18397),#6938,.T.) ;
#65683 = ADVANCED_FACE('',(#18398),#4473,.T.) ;
#65684 = ADVANCED_FACE('',(#18399),#4474,.T.) ;
#65685 = ADVANCED_FACE('',(#18400),#6939,.T.) ;
#65686 = ADVANCED_FACE('',(#18401),#6940,.T.) ;
#65687 = ADVANCED_FACE('',(#18402),#6941,.T.) ;
#65688 = ADVANCED_FACE('',(#18403),#4475,.T.) ;
#65689 = ADVANCED_FACE('',(#18404),#6942,.T.) ;
#65690 = ADVANCED_FACE('',(#18405),#6943,.T.) ;
#65691 = ADVANCED_FACE('',(#18406),#6944,.T.) ;
#65692 = ADVANCED_FACE('',(#18407),#6945,.T.) ;
#65693 = ADVANCED_FACE('',(#18408),#4476,.T.) ;
#65694 = ADVANCED_FACE('',(#18409),#6946,.T.) ;
#65695 = ADVANCED_FACE('',(#18410),#6947,.T.) ;
#65696 = ADVANCED_FACE('',(#18411),#6948,.T.) ;
#65697 = ADVANCED_FACE('',(#18412),#4477,.T.) ;
#65698 = ADVANCED_FACE('',(#18413),#4478,.T.) ;
#65699 = ADVANCED_FACE('',(#18414),#6949,.T.) ;
#65700 = ADVANCED_FACE('',(#18415),#6950,.T.) ;
#65701 = ADVANCED_FACE('',(#18416),#6951,.T.) ;
#65702 = ADVANCED_FACE('',(#18417),#4479,.T.) ;
#65703 = ADVANCED_FACE('',(#18418),#6952,.T.) ;
#65704 = ADVANCED_FACE('',(#18419),#6953,.T.) ;
#65705 = ADVANCED_FACE('',(#18420),#63176,.T.) ;
#65706 = ADVANCED_FACE('',(#18421),#6954,.T.) ;
#65707 = ADVANCED_FACE('',(#18422),#4480,.T.) ;
#65708 = ADVANCED_FACE('',(#18423),#6955,.T.) ;
#65709 = ADVANCED_FACE('',(#18424),#4481,.T.) ;
#65710 = ADVANCED_FACE('',(#18425),#6956,.T.) ;
#65711 = ADVANCED_FACE('',(#18426),#63177,.T.) ;
#65712 = ADVANCED_FACE('',(#18427),#63178,.T.) ;
#65713 = ADVANCED_FACE('',(#18428),#6957,.T.) ;
#65714 = ADVANCED_FACE('',(#18429),#4482,.T.) ;
#65715 = ADVANCED_FACE('',(#18430),#6958,.T.) ;
#65716 = ADVANCED_FACE('',(#18431),#4483,.T.) ;
#65717 = ADVANCED_FACE('',(#18432),#6959,.T.) ;
#65718 = ADVANCED_FACE('',(#18433),#63179,.T.) ;
#65719 = ADVANCED_FACE('',(#18434),#6960,.T.) ;
#65720 = ADVANCED_FACE('',(#18435),#4484,.T.) ;
#65721 = ADVANCED_FACE('',(#18436),#6961,.T.) ;
#65722 = ADVANCED_FACE('',(#18437),#4485,.T.) ;
#65723 = ADVANCED_FACE('',(#18438),#6962,.T.) ;
#65724 = ADVANCED_FACE('',(#18439),#6963,.T.) ;
#65725 = ADVANCED_FACE('',(#18440),#4486,.T.) ;
#65726 = ADVANCED_FACE('',(#18441),#6964,.T.) ;
#65727 = ADVANCED_FACE('',(#18442),#6965,.T.) ;
#65728 = ADVANCED_FACE('',(#18443),#4487,.T.) ;
#65729 = ADVANCED_FACE('',(#18444),#5562,.T.) ;
#65730 = ADVANCED_FACE('',(#18445),#5563,.T.) ;
#65731 = ADVANCED_FACE('',(#18446),#5564,.T.) ;
#65732 = ADVANCED_FACE('',(#18447),#5565,.T.) ;
#65733 = ADVANCED_FACE('',(#18448),#5566,.T.) ;
#65734 = ADVANCED_FACE('',(#18449),#5567,.T.) ;
#65735 = ADVANCED_FACE('',(#18450),#5568,.T.) ;
#65736 = ADVANCED_FACE('',(#18451),#5569,.T.) ;
#65737 = ADVANCED_FACE('',(#18452),#5570,.T.) ;
#65738 = ADVANCED_FACE('',(#18453),#5571,.F.) ;
#65739 = ADVANCED_FACE('',(#18454),#5572,.F.) ;
#65740 = ADVANCED_FACE('',(#18455),#5573,.F.) ;
#65741 = ADVANCED_FACE('',(#18456),#5574,.F.) ;
#65742 = ADVANCED_FACE('',(#18457),#5575,.F.) ;
#65743 = ADVANCED_FACE('',(#18458),#5576,.F.) ;
#65744 = ADVANCED_FACE('',(#18459),#5577,.F.) ;
#65745 = ADVANCED_FACE('',(#18460),#5578,.F.) ;
#65746 = ADVANCED_FACE('',(#18461),#5579,.F.) ;
#65747 = ADVANCED_FACE('',(#18462),#5580,.F.) ;
#65748 = ADVANCED_FACE('',(#18463),#5581,.F.) ;
#65749 = ADVANCED_FACE('',(#18464),#5582,.F.) ;
#65750 = ADVANCED_FACE('',(#18465),#5583,.F.) ;
#65751 = ADVANCED_FACE('',(#18466),#5584,.F.) ;
#65752 = ADVANCED_FACE('',(#18467),#5585,.F.) ;
#65753 = ADVANCED_FACE('',(#18468),#5586,.F.) ;
#65754 = ADVANCED_FACE('',(#18469),#5587,.F.) ;
#65755 = ADVANCED_FACE('',(#18470),#5588,.F.) ;
#65756 = ADVANCED_FACE('',(#18471),#5589,.F.) ;
#65757 = ADVANCED_FACE('',(#18472),#5590,.F.) ;
#65758 = ADVANCED_FACE('',(#18473),#5591,.F.) ;
#65759 = ADVANCED_FACE('',(#18474),#5592,.F.) ;
#65760 = ADVANCED_FACE('',(#18475),#5593,.F.) ;
#65761 = ADVANCED_FACE('',(#18476),#5594,.F.) ;
#65762 = ADVANCED_FACE('',(#18477),#5595,.F.) ;
#65763 = ADVANCED_FACE('',(#18478),#5596,.F.) ;
#65764 = ADVANCED_FACE('',(#18479),#5597,.F.) ;
#65765 = ADVANCED_FACE('',(#18480),#5598,.F.) ;
#65766 = ADVANCED_FACE('',(#18481),#5599,.F.) ;
#65767 = ADVANCED_FACE('',(#18482),#5600,.F.) ;
#65768 = ADVANCED_FACE('',(#18483),#5601,.F.) ;
#65769 = ADVANCED_FACE('',(#18484),#5602,.F.) ;
#65770 = ADVANCED_FACE('',(#18485),#5603,.F.) ;
#65771 = ADVANCED_FACE('',(#18486),#5604,.F.) ;
#65772 = ADVANCED_FACE('',(#18487),#5605,.F.) ;
#65773 = ADVANCED_FACE('',(#18488),#5606,.F.) ;
#65774 = ADVANCED_FACE('',(#18489),#5607,.F.) ;
#65775 = ADVANCED_FACE('',(#18490),#5608,.F.) ;
#65776 = ADVANCED_FACE('',(#18491),#5609,.F.) ;
#65777 = ADVANCED_FACE('',(#18492),#5610,.F.) ;
#65778 = ADVANCED_FACE('',(#18493),#5611,.F.) ;
#65779 = ADVANCED_FACE('',(#18494),#5612,.F.) ;
#65780 = ADVANCED_FACE('',(#18495),#5613,.F.) ;
#65781 = ADVANCED_FACE('',(#18496),#5614,.F.) ;
#65782 = ADVANCED_FACE('',(#18497),#5615,.F.) ;
#65783 = ADVANCED_FACE('',(#18498),#6966,.T.) ;
#65784 = ADVANCED_FACE('',(#18499),#5616,.F.) ;
#65785 = ADVANCED_FACE('',(#18500),#6967,.T.) ;
#65786 = ADVANCED_FACE('',(#18501),#5617,.F.) ;
#65787 = ADVANCED_FACE('',(#18502),#6968,.F.) ;
#65788 = ADVANCED_FACE('',(#18503),#5618,.F.) ;
#65789 = ADVANCED_FACE('',(#18504),#6969,.F.) ;
#65790 = ADVANCED_FACE('',(#18505),#5619,.F.) ;
#65791 = ADVANCED_FACE('',(#18506),#5620,.F.) ;
#65792 = ADVANCED_FACE('',(#18507),#6970,.F.) ;
#65793 = ADVANCED_FACE('',(#18508),#5621,.F.) ;
#65794 = ADVANCED_FACE('',(#18509),#6971,.T.) ;
#65795 = ADVANCED_FACE('',(#18510),#5622,.F.) ;
#65796 = ADVANCED_FACE('',(#18511),#6972,.T.) ;
#65797 = ADVANCED_FACE('',(#18512),#5623,.F.) ;
#65798 = ADVANCED_FACE('',(#18513),#6973,.F.) ;
#65799 = ADVANCED_FACE('',(#18514),#5624,.F.) ;
#65800 = ADVANCED_FACE('',(#18515),#6974,.F.) ;
#65801 = ADVANCED_FACE('',(#18516),#5625,.F.) ;
#65802 = ADVANCED_FACE('',(#18517),#6975,.F.) ;
#65803 = ADVANCED_FACE('',(#18518),#6976,.T.) ;
#65804 = ADVANCED_FACE('',(#18519),#6977,.F.) ;
#65805 = ADVANCED_FACE('',(#18520),#5626,.F.) ;
#65806 = ADVANCED_FACE('',(#18521),#6978,.F.) ;
#65807 = ADVANCED_FACE('',(#18522),#5627,.F.) ;
#65808 = ADVANCED_FACE('',(#18523),#6979,.F.) ;
#65809 = ADVANCED_FACE('',(#18524),#5628,.F.) ;
#65810 = ADVANCED_FACE('',(#18525,#5043),#5629,.F.) ;
#65811 = ADVANCED_FACE('',(#18526),#6980,.T.) ;
#65812 = ADVANCED_FACE('',(#18527),#5630,.F.) ;
#65813 = ADVANCED_FACE('',(#18528),#6981,.T.) ;
#65814 = ADVANCED_FACE('',(#18529),#5631,.F.) ;
#65815 = ADVANCED_FACE('',(#18530),#6982,.F.) ;
#65816 = ADVANCED_FACE('',(#18531),#5632,.F.) ;
#65817 = ADVANCED_FACE('',(#18532),#6983,.F.) ;
#65818 = ADVANCED_FACE('',(#18533),#5633,.F.) ;
#65819 = ADVANCED_FACE('',(#18534),#5634,.F.) ;
#65820 = ADVANCED_FACE('',(#18535),#6984,.F.) ;
#65821 = ADVANCED_FACE('',(#18536),#5635,.F.) ;
#65822 = ADVANCED_FACE('',(#18537),#6985,.T.) ;
#65823 = ADVANCED_FACE('',(#18538),#5636,.F.) ;
#65824 = ADVANCED_FACE('',(#18539),#6986,.T.) ;
#65825 = ADVANCED_FACE('',(#18540),#5637,.F.) ;
#65826 = ADVANCED_FACE('',(#18541),#6987,.F.) ;
#65827 = ADVANCED_FACE('',(#18542),#5638,.F.) ;
#65828 = ADVANCED_FACE('',(#18543),#6988,.F.) ;
#65829 = ADVANCED_FACE('',(#18544),#5639,.F.) ;
#65830 = ADVANCED_FACE('',(#18545),#6989,.F.) ;
#65831 = ADVANCED_FACE('',(#18546),#6990,.T.) ;
#65832 = ADVANCED_FACE('',(#18547),#6991,.F.) ;
#65833 = ADVANCED_FACE('',(#18548),#5640,.F.) ;
#65834 = ADVANCED_FACE('',(#18549),#6992,.F.) ;
#65835 = ADVANCED_FACE('',(#18550),#5641,.F.) ;
#65836 = ADVANCED_FACE('',(#18551),#6993,.F.) ;
#65837 = ADVANCED_FACE('',(#18552),#5642,.F.) ;
#65838 = ADVANCED_FACE('',(#18553,#5044),#5643,.F.) ;
#65839 = ADVANCED_FACE('',(#18554),#6994,.T.) ;
#65840 = ADVANCED_FACE('',(#18555),#5644,.F.) ;
#65841 = ADVANCED_FACE('',(#18556),#6995,.T.) ;
#65842 = ADVANCED_FACE('',(#18557),#5645,.F.) ;
#65843 = ADVANCED_FACE('',(#18558),#6996,.F.) ;
#65844 = ADVANCED_FACE('',(#18559),#5646,.F.) ;
#65845 = ADVANCED_FACE('',(#18560),#6997,.F.) ;
#65846 = ADVANCED_FACE('',(#18561),#5647,.F.) ;
#65847 = ADVANCED_FACE('',(#18562),#5648,.F.) ;
#65848 = ADVANCED_FACE('',(#18563),#6998,.F.) ;
#65849 = ADVANCED_FACE('',(#18564),#5649,.F.) ;
#65850 = ADVANCED_FACE('',(#18565),#6999,.T.) ;
#65851 = ADVANCED_FACE('',(#18566),#5650,.F.) ;
#65852 = ADVANCED_FACE('',(#18567),#7000,.T.) ;
#65853 = ADVANCED_FACE('',(#18568),#5651,.F.) ;
#65854 = ADVANCED_FACE('',(#18569),#7001,.F.) ;
#65855 = ADVANCED_FACE('',(#18570),#5652,.F.) ;
#65856 = ADVANCED_FACE('',(#18571),#7002,.F.) ;
#65857 = ADVANCED_FACE('',(#18572),#5653,.F.) ;
#65858 = ADVANCED_FACE('',(#18573),#7003,.F.) ;
#65859 = ADVANCED_FACE('',(#18574),#7004,.T.) ;
#65860 = ADVANCED_FACE('',(#18575),#7005,.F.) ;
#65861 = ADVANCED_FACE('',(#18576),#5654,.F.) ;
#65862 = ADVANCED_FACE('',(#18577),#7006,.F.) ;
#65863 = ADVANCED_FACE('',(#18578),#5655,.F.) ;
#65864 = ADVANCED_FACE('',(#18579),#7007,.F.) ;
#65865 = ADVANCED_FACE('',(#18580),#5656,.F.) ;
#65866 = ADVANCED_FACE('',(#18581,#5045),#5657,.F.) ;
#65867 = ADVANCED_FACE('',(#18582),#7008,.T.) ;
#65868 = ADVANCED_FACE('',(#18583),#5658,.F.) ;
#65869 = ADVANCED_FACE('',(#18584),#7009,.T.) ;
#65870 = ADVANCED_FACE('',(#18585),#5659,.F.) ;
#65871 = ADVANCED_FACE('',(#18586),#7010,.F.) ;
#65872 = ADVANCED_FACE('',(#18587),#5660,.F.) ;
#65873 = ADVANCED_FACE('',(#18588),#7011,.F.) ;
#65874 = ADVANCED_FACE('',(#18589),#5661,.F.) ;
#65875 = ADVANCED_FACE('',(#18590),#5662,.F.) ;
#65876 = ADVANCED_FACE('',(#18591),#7012,.F.) ;
#65877 = ADVANCED_FACE('',(#18592),#5663,.F.) ;
#65878 = ADVANCED_FACE('',(#18593),#7013,.T.) ;
#65879 = ADVANCED_FACE('',(#18594),#5664,.F.) ;
#65880 = ADVANCED_FACE('',(#18595),#7014,.T.) ;
#65881 = ADVANCED_FACE('',(#18596),#5665,.F.) ;
#65882 = ADVANCED_FACE('',(#18597),#7015,.F.) ;
#65883 = ADVANCED_FACE('',(#18598),#5666,.F.) ;
#65884 = ADVANCED_FACE('',(#18599),#7016,.F.) ;
#65885 = ADVANCED_FACE('',(#18600),#5667,.F.) ;
#65886 = ADVANCED_FACE('',(#18601),#7017,.F.) ;
#65887 = ADVANCED_FACE('',(#18602),#7018,.T.) ;
#65888 = ADVANCED_FACE('',(#18603),#7019,.F.) ;
#65889 = ADVANCED_FACE('',(#18604),#5668,.F.) ;
#65890 = ADVANCED_FACE('',(#18605),#7020,.F.) ;
#65891 = ADVANCED_FACE('',(#18606),#5669,.F.) ;
#65892 = ADVANCED_FACE('',(#18607),#7021,.F.) ;
#65893 = ADVANCED_FACE('',(#18608),#5670,.F.) ;
#65894 = ADVANCED_FACE('',(#18609,#5046),#5671,.F.) ;
#65895 = ADVANCED_FACE('',(#18610),#7022,.T.) ;
#65896 = ADVANCED_FACE('',(#18611),#5672,.F.) ;
#65897 = ADVANCED_FACE('',(#18612),#7023,.T.) ;
#65898 = ADVANCED_FACE('',(#18613),#5673,.F.) ;
#65899 = ADVANCED_FACE('',(#18614),#7024,.F.) ;
#65900 = ADVANCED_FACE('',(#18615),#5674,.F.) ;
#65901 = ADVANCED_FACE('',(#18616),#7025,.F.) ;
#65902 = ADVANCED_FACE('',(#18617),#5675,.F.) ;
#65903 = ADVANCED_FACE('',(#18618),#5676,.F.) ;
#65904 = ADVANCED_FACE('',(#18619),#7026,.F.) ;
#65905 = ADVANCED_FACE('',(#18620),#5677,.F.) ;
#65906 = ADVANCED_FACE('',(#18621),#7027,.T.) ;
#65907 = ADVANCED_FACE('',(#18622),#5678,.F.) ;
#65908 = ADVANCED_FACE('',(#18623),#7028,.T.) ;
#65909 = ADVANCED_FACE('',(#18624),#5679,.F.) ;
#65910 = ADVANCED_FACE('',(#18625),#7029,.F.) ;
#65911 = ADVANCED_FACE('',(#18626),#5680,.F.) ;
#65912 = ADVANCED_FACE('',(#18627),#7030,.F.) ;
#65913 = ADVANCED_FACE('',(#18628),#5681,.F.) ;
#65914 = ADVANCED_FACE('',(#18629),#7031,.F.) ;
#65915 = ADVANCED_FACE('',(#18630),#7032,.T.) ;
#65916 = ADVANCED_FACE('',(#18631),#7033,.F.) ;
#65917 = ADVANCED_FACE('',(#18632),#5682,.F.) ;
#65918 = ADVANCED_FACE('',(#18633),#7034,.F.) ;
#65919 = ADVANCED_FACE('',(#18634),#5683,.F.) ;
#65920 = ADVANCED_FACE('',(#18635),#7035,.F.) ;
#65921 = ADVANCED_FACE('',(#18636),#5684,.F.) ;
#65922 = ADVANCED_FACE('',(#18637,#5047),#5685,.F.) ;
#65923 = ADVANCED_FACE('',(#18638),#7036,.T.) ;
#65924 = ADVANCED_FACE('',(#18639),#5686,.F.) ;
#65925 = ADVANCED_FACE('',(#18640),#7037,.T.) ;
#65926 = ADVANCED_FACE('',(#18641),#5687,.F.) ;
#65927 = ADVANCED_FACE('',(#18642),#7038,.F.) ;
#65928 = ADVANCED_FACE('',(#18643),#5688,.F.) ;
#65929 = ADVANCED_FACE('',(#18644),#7039,.F.) ;
#65930 = ADVANCED_FACE('',(#18645),#5689,.F.) ;
#65931 = ADVANCED_FACE('',(#18646),#5690,.F.) ;
#65932 = ADVANCED_FACE('',(#18647),#7040,.F.) ;
#65933 = ADVANCED_FACE('',(#18648),#5691,.F.) ;
#65934 = ADVANCED_FACE('',(#18649),#7041,.T.) ;
#65935 = ADVANCED_FACE('',(#18650),#5692,.F.) ;
#65936 = ADVANCED_FACE('',(#18651),#7042,.T.) ;
#65937 = ADVANCED_FACE('',(#18652),#5693,.F.) ;
#65938 = ADVANCED_FACE('',(#18653),#7043,.F.) ;
#65939 = ADVANCED_FACE('',(#18654),#5694,.F.) ;
#65940 = ADVANCED_FACE('',(#18655),#7044,.F.) ;
#65941 = ADVANCED_FACE('',(#18656),#5695,.F.) ;
#65942 = ADVANCED_FACE('',(#18657),#7045,.F.) ;
#65943 = ADVANCED_FACE('',(#18658),#7046,.T.) ;
#65944 = ADVANCED_FACE('',(#18659),#7047,.F.) ;
#65945 = ADVANCED_FACE('',(#18660),#5696,.F.) ;
#65946 = ADVANCED_FACE('',(#18661),#7048,.F.) ;
#65947 = ADVANCED_FACE('',(#18662),#5697,.F.) ;
#65948 = ADVANCED_FACE('',(#18663),#7049,.F.) ;
#65949 = ADVANCED_FACE('',(#18664),#5698,.F.) ;
#65950 = ADVANCED_FACE('',(#18665,#5048),#5699,.F.) ;
#65951 = ADVANCED_FACE('',(#18666),#7050,.T.) ;
#65952 = ADVANCED_FACE('',(#18667),#5700,.F.) ;
#65953 = ADVANCED_FACE('',(#18668),#7051,.T.) ;
#65954 = ADVANCED_FACE('',(#18669),#5701,.F.) ;
#65955 = ADVANCED_FACE('',(#18670),#7052,.F.) ;
#65956 = ADVANCED_FACE('',(#18671),#5702,.F.) ;
#65957 = ADVANCED_FACE('',(#18672),#7053,.F.) ;
#65958 = ADVANCED_FACE('',(#18673),#5703,.F.) ;
#65959 = ADVANCED_FACE('',(#18674),#5704,.F.) ;
#65960 = ADVANCED_FACE('',(#18675),#7054,.F.) ;
#65961 = ADVANCED_FACE('',(#18676),#5705,.F.) ;
#65962 = ADVANCED_FACE('',(#18677),#7055,.T.) ;
#65963 = ADVANCED_FACE('',(#18678),#5706,.F.) ;
#65964 = ADVANCED_FACE('',(#18679),#7056,.T.) ;
#65965 = ADVANCED_FACE('',(#18680),#5707,.F.) ;
#65966 = ADVANCED_FACE('',(#18681),#7057,.F.) ;
#65967 = ADVANCED_FACE('',(#18682),#5708,.F.) ;
#65968 = ADVANCED_FACE('',(#18683),#7058,.F.) ;
#65969 = ADVANCED_FACE('',(#18684),#5709,.F.) ;
#65970 = ADVANCED_FACE('',(#18685),#7059,.F.) ;
#65971 = ADVANCED_FACE('',(#18686),#7060,.T.) ;
#65972 = ADVANCED_FACE('',(#18687),#7061,.F.) ;
#65973 = ADVANCED_FACE('',(#18688),#5710,.F.) ;
#65974 = ADVANCED_FACE('',(#18689),#7062,.F.) ;
#65975 = ADVANCED_FACE('',(#18690),#5711,.F.) ;
#65976 = ADVANCED_FACE('',(#18691),#7063,.F.) ;
#65977 = ADVANCED_FACE('',(#18692),#5712,.F.) ;
#65978 = ADVANCED_FACE('',(#18693,#5049),#5713,.F.) ;
#65979 = ADVANCED_FACE('',(#18694),#7064,.T.) ;
#65980 = ADVANCED_FACE('',(#18695),#5714,.F.) ;
#65981 = ADVANCED_FACE('',(#18696),#7065,.T.) ;
#65982 = ADVANCED_FACE('',(#18697),#5715,.F.) ;
#65983 = ADVANCED_FACE('',(#18698),#7066,.F.) ;
#65984 = ADVANCED_FACE('',(#18699),#5716,.F.) ;
#65985 = ADVANCED_FACE('',(#18700),#7067,.F.) ;
#65986 = ADVANCED_FACE('',(#18701),#5717,.F.) ;
#65987 = ADVANCED_FACE('',(#18702),#5718,.F.) ;
#65988 = ADVANCED_FACE('',(#18703),#7068,.F.) ;
#65989 = ADVANCED_FACE('',(#18704),#5719,.F.) ;
#65990 = ADVANCED_FACE('',(#18705),#7069,.T.) ;
#65991 = ADVANCED_FACE('',(#18706),#5720,.F.) ;
#65992 = ADVANCED_FACE('',(#18707),#7070,.T.) ;
#65993 = ADVANCED_FACE('',(#18708),#5721,.F.) ;
#65994 = ADVANCED_FACE('',(#18709),#7071,.F.) ;
#65995 = ADVANCED_FACE('',(#18710),#5722,.F.) ;
#65996 = ADVANCED_FACE('',(#18711),#7072,.F.) ;
#65997 = ADVANCED_FACE('',(#18712),#5723,.F.) ;
#65998 = ADVANCED_FACE('',(#18713),#7073,.F.) ;
#65999 = ADVANCED_FACE('',(#18714),#7074,.T.) ;
#66000 = ADVANCED_FACE('',(#18715),#7075,.F.) ;
#66001 = ADVANCED_FACE('',(#18716),#5724,.F.) ;
#66002 = ADVANCED_FACE('',(#18717),#7076,.F.) ;
#66003 = ADVANCED_FACE('',(#18718),#5725,.F.) ;
#66004 = ADVANCED_FACE('',(#18719),#7077,.F.) ;
#66005 = ADVANCED_FACE('',(#18720),#5726,.F.) ;
#66006 = ADVANCED_FACE('',(#18721,#5050),#5727,.F.) ;
#66007 = ADVANCED_FACE('',(#18722),#7078,.T.) ;
#66008 = ADVANCED_FACE('',(#18723),#5728,.F.) ;
#66009 = ADVANCED_FACE('',(#18724),#7079,.T.) ;
#66010 = ADVANCED_FACE('',(#18725),#5729,.F.) ;
#66011 = ADVANCED_FACE('',(#18726),#7080,.F.) ;
#66012 = ADVANCED_FACE('',(#18727),#5730,.F.) ;
#66013 = ADVANCED_FACE('',(#18728),#7081,.F.) ;
#66014 = ADVANCED_FACE('',(#18729),#5731,.F.) ;
#66015 = ADVANCED_FACE('',(#18730),#5732,.F.) ;
#66016 = ADVANCED_FACE('',(#18731),#7082,.F.) ;
#66017 = ADVANCED_FACE('',(#18732),#5733,.F.) ;
#66018 = ADVANCED_FACE('',(#18733),#7083,.T.) ;
#66019 = ADVANCED_FACE('',(#18734),#5734,.F.) ;
#66020 = ADVANCED_FACE('',(#18735),#7084,.T.) ;
#66021 = ADVANCED_FACE('',(#18736),#5735,.F.) ;
#66022 = ADVANCED_FACE('',(#18737),#7085,.F.) ;
#66023 = ADVANCED_FACE('',(#18738),#5736,.F.) ;
#66024 = ADVANCED_FACE('',(#18739),#7086,.F.) ;
#66025 = ADVANCED_FACE('',(#18740),#5737,.F.) ;
#66026 = ADVANCED_FACE('',(#18741),#7087,.F.) ;
#66027 = ADVANCED_FACE('',(#18742),#7088,.T.) ;
#66028 = ADVANCED_FACE('',(#18743),#7089,.F.) ;
#66029 = ADVANCED_FACE('',(#18744),#5738,.F.) ;
#66030 = ADVANCED_FACE('',(#18745),#7090,.F.) ;
#66031 = ADVANCED_FACE('',(#18746),#5739,.F.) ;
#66032 = ADVANCED_FACE('',(#18747),#7091,.F.) ;
#66033 = ADVANCED_FACE('',(#18748),#5740,.F.) ;
#66034 = ADVANCED_FACE('',(#18749,#5051),#5741,.F.) ;
#66035 = ADVANCED_FACE('',(#18750,#5052),#5742,.T.) ;
#66036 = ADVANCED_FACE('',(#18751,#5053),#5743,.T.) ;
#66037 = ADVANCED_FACE('',(#18752,#5054),#5744,.T.) ;
#66038 = ADVANCED_FACE('',(#18753,#5055),#5745,.T.) ;
#66039 = ADVANCED_FACE('',(#18754,#5056),#5746,.T.) ;
#66040 = ADVANCED_FACE('',(#18755,#5057),#5747,.T.) ;
#66041 = ADVANCED_FACE('',(#18756,#5058),#5748,.T.) ;
#66042 = ADVANCED_FACE('',(#18757,#5059),#5749,.T.) ;
#66043 = ADVANCED_FACE('',(#18758,#5060),#5750,.T.) ;
#66044 = ADVANCED_FACE('',(#18759),#7092,.T.) ;
#66045 = ADVANCED_FACE('',(#18760),#7093,.F.) ;
#66046 = ADVANCED_FACE('',(#18761),#4488,.F.) ;
#66047 = ADVANCED_FACE('',(#18762),#4489,.T.) ;
#66048 = ADVANCED_FACE('',(#18763),#63180,.T.) ;
#66049 = ADVANCED_FACE('',(#18764),#7094,.F.) ;
#66050 = ADVANCED_FACE('',(#18765),#7095,.F.) ;
#66051 = ADVANCED_FACE('',(#18766),#7096,.T.) ;
#66052 = ADVANCED_FACE('',(#18767),#7097,.T.) ;
#66053 = ADVANCED_FACE('',(#18768),#7098,.T.) ;
#66054 = ADVANCED_FACE('',(#18769),#7099,.F.) ;
#66055 = ADVANCED_FACE('',(#18770),#4490,.F.) ;
#66056 = ADVANCED_FACE('',(#18771),#63181,.F.) ;
#66057 = ADVANCED_FACE('',(#18772),#63182,.F.) ;
#66058 = ADVANCED_FACE('',(#18773),#63183,.T.) ;
#66059 = ADVANCED_FACE('',(#18774),#7100,.F.) ;
#66060 = ADVANCED_FACE('',(#18775),#7101,.F.) ;
#66061 = ADVANCED_FACE('',(#18776),#7102,.F.) ;
#66062 = ADVANCED_FACE('',(#18777),#7103,.T.) ;
#66063 = ADVANCED_FACE('',(#18778),#7104,.T.) ;
#66064 = ADVANCED_FACE('',(#18779),#63184,.F.) ;
#66065 = ADVANCED_FACE('',(#18780),#4491,.F.) ;
#66066 = ADVANCED_FACE('',(#18781),#4492,.T.) ;
#66067 = ADVANCED_FACE('',(#18782),#7105,.T.) ;
#66068 = ADVANCED_FACE('',(#18783),#4493,.F.) ;
#66069 = ADVANCED_FACE('',(#18784),#4494,.T.) ;
#66070 = ADVANCED_FACE('',(#18785),#7106,.F.) ;
#66071 = ADVANCED_FACE('',(#18786),#7107,.F.) ;
#66072 = ADVANCED_FACE('',(#18787),#7108,.T.) ;
#66073 = ADVANCED_FACE('',(#18788),#63185,.T.) ;
#66074 = ADVANCED_FACE('',(#18789),#7109,.F.) ;
#66075 = ADVANCED_FACE('',(#18790),#7110,.T.) ;
#66076 = ADVANCED_FACE('',(#18791),#7111,.F.) ;
#66077 = ADVANCED_FACE('',(#18792),#4495,.F.) ;
#66078 = ADVANCED_FACE('',(#18793),#63186,.T.) ;
#66079 = ADVANCED_FACE('',(#18794),#7112,.T.) ;
#66080 = ADVANCED_FACE('',(#18795),#4496,.F.) ;
#66081 = ADVANCED_FACE('',(#18796),#63187,.F.) ;
#66082 = ADVANCED_FACE('',(#18797),#7113,.F.) ;
#66083 = ADVANCED_FACE('',(#18798),#7114,.T.) ;
#66084 = ADVANCED_FACE('',(#18799),#63188,.T.) ;
#66085 = ADVANCED_FACE('',(#18800),#7115,.F.) ;
#66086 = ADVANCED_FACE('',(#18801),#63189,.T.) ;
#66087 = ADVANCED_FACE('',(#18802),#7116,.T.) ;
#66088 = ADVANCED_FACE('',(#18803),#7117,.T.) ;
#66089 = ADVANCED_FACE('',(#18804),#4497,.T.) ;
#66090 = ADVANCED_FACE('',(#18805),#7118,.F.) ;
#66091 = ADVANCED_FACE('',(#18806),#63190,.F.) ;
#66092 = ADVANCED_FACE('',(#18807),#4498,.F.) ;
#66093 = ADVANCED_FACE('',(#18808),#7119,.F.) ;
#66094 = ADVANCED_FACE('',(#18809),#7120,.F.) ;
#66095 = ADVANCED_FACE('',(#18810),#63191,.F.) ;
#66096 = ADVANCED_FACE('',(#18811),#4499,.F.) ;
#66097 = ADVANCED_FACE('',(#18812),#7121,.F.) ;
#66098 = ADVANCED_FACE('',(#18813),#7122,.F.) ;
#66099 = ADVANCED_FACE('',(#18814),#4500,.F.) ;
#66100 = ADVANCED_FACE('',(#18815),#4501,.F.) ;
#66101 = ADVANCED_FACE('',(#18816),#7123,.F.) ;
#66102 = ADVANCED_FACE('',(#18817),#63192,.F.) ;
#66103 = ADVANCED_FACE('',(#18818),#4502,.F.) ;
#66104 = ADVANCED_FACE('',(#18819),#4503,.F.) ;
#66105 = ADVANCED_FACE('',(#18820),#7124,.F.) ;
#66106 = ADVANCED_FACE('',(#18821),#7125,.F.) ;
#66107 = ADVANCED_FACE('',(#18822),#4504,.F.) ;
#66108 = ADVANCED_FACE('',(#18823),#7126,.F.) ;
#66109 = ADVANCED_FACE('',(#18824),#7127,.F.) ;
#66110 = ADVANCED_FACE('',(#18825),#4505,.F.) ;
#66111 = ADVANCED_FACE('',(#18826),#4506,.F.) ;
#66112 = ADVANCED_FACE('',(#18827),#7128,.F.) ;
#66113 = ADVANCED_FACE('',(#18828),#7129,.F.) ;
#66114 = ADVANCED_FACE('',(#18829),#63193,.F.) ;
#66115 = ADVANCED_FACE('',(#18830),#63194,.F.) ;
#66116 = ADVANCED_FACE('',(#18831),#7130,.F.) ;
#66117 = ADVANCED_FACE('',(#18832),#7131,.T.) ;
#66118 = ADVANCED_FACE('',(#18833),#4507,.T.) ;
#66119 = ADVANCED_FACE('',(#18834),#4508,.T.) ;
#66120 = ADVANCED_FACE('',(#18835),#7132,.T.) ;
#66121 = ADVANCED_FACE('',(#18836),#7133,.T.) ;
#66122 = ADVANCED_FACE('',(#18837),#63195,.T.) ;
#66123 = ADVANCED_FACE('',(#18838),#63196,.T.) ;
#66124 = ADVANCED_FACE('',(#18839),#7134,.T.) ;
#66125 = ADVANCED_FACE('',(#18840),#7135,.T.) ;
#66126 = ADVANCED_FACE('',(#18841),#63197,.T.) ;
#66127 = ADVANCED_FACE('',(#18842),#7136,.T.) ;
#66128 = ADVANCED_FACE('',(#18843),#7137,.T.) ;
#66129 = ADVANCED_FACE('',(#18844),#63198,.T.) ;
#66130 = ADVANCED_FACE('',(#18845),#63199,.T.) ;
#66131 = ADVANCED_FACE('',(#18846),#7138,.T.) ;
#66132 = ADVANCED_FACE('',(#18847),#63200,.T.) ;
#66133 = ADVANCED_FACE('',(#18848),#63201,.T.) ;
#66134 = ADVANCED_FACE('',(#18849),#63202,.T.) ;
#66135 = ADVANCED_FACE('',(#18850),#7139,.T.) ;
#66136 = ADVANCED_FACE('',(#18851),#7140,.T.) ;
#66137 = ADVANCED_FACE('',(#18852),#4509,.T.) ;
#66138 = ADVANCED_FACE('',(#18853),#63203,.T.) ;
#66139 = ADVANCED_FACE('',(#18854),#7141,.T.) ;
#66140 = ADVANCED_FACE('',(#18855),#7142,.T.) ;
#66141 = ADVANCED_FACE('',(#18856),#4510,.T.) ;
#66142 = ADVANCED_FACE('',(#18857),#63204,.T.) ;
#66143 = ADVANCED_FACE('',(#18858),#7143,.T.) ;
#66144 = ADVANCED_FACE('',(#18859),#7144,.T.) ;
#66145 = ADVANCED_FACE('',(#18860),#4511,.T.) ;
#66146 = ADVANCED_FACE('',(#18861),#4512,.T.) ;
#66147 = ADVANCED_FACE('',(#18862),#7145,.T.) ;
#66148 = ADVANCED_FACE('',(#18863),#7146,.T.) ;
#66149 = ADVANCED_FACE('',(#18864),#63205,.T.) ;
#66150 = ADVANCED_FACE('',(#18865),#63206,.T.) ;
#66151 = ADVANCED_FACE('',(#18866),#7147,.T.) ;
#66152 = ADVANCED_FACE('',(#18867),#7148,.T.) ;
#66153 = ADVANCED_FACE('',(#18868),#63207,.T.) ;
#66154 = ADVANCED_FACE('',(#18869),#7149,.T.) ;
#66155 = ADVANCED_FACE('',(#18870),#7150,.T.) ;
#66156 = ADVANCED_FACE('',(#18871),#63208,.T.) ;
#66157 = ADVANCED_FACE('',(#18872),#63209,.T.) ;
#66158 = ADVANCED_FACE('',(#18873),#7151,.T.) ;
#66159 = ADVANCED_FACE('',(#18874),#63210,.T.) ;
#66160 = ADVANCED_FACE('',(#18875),#63211,.T.) ;
#66161 = ADVANCED_FACE('',(#18876),#63212,.T.) ;
#66162 = ADVANCED_FACE('',(#18877),#7152,.T.) ;
#66163 = ADVANCED_FACE('',(#18878),#7153,.T.) ;
#66164 = ADVANCED_FACE('',(#18879),#4513,.T.) ;
#66165 = ADVANCED_FACE('',(#18880),#63213,.T.) ;
#66166 = ADVANCED_FACE('',(#18881),#7154,.T.) ;
#66167 = ADVANCED_FACE('',(#18882),#7155,.T.) ;
#66168 = ADVANCED_FACE('',(#18883),#4514,.T.) ;
#66169 = ADVANCED_FACE('',(#18884),#63214,.T.) ;
#66170 = ADVANCED_FACE('',(#18885),#7156,.T.) ;
#66171 = ADVANCED_FACE('',(#18886),#7157,.T.) ;
#66172 = ADVANCED_FACE('',(#18887),#4515,.T.) ;
#66173 = ADVANCED_FACE('',(#18888),#4516,.T.) ;
#66174 = ADVANCED_FACE('',(#18889),#7158,.T.) ;
#66175 = ADVANCED_FACE('',(#18890),#7159,.T.) ;
#66176 = ADVANCED_FACE('',(#18891),#63215,.T.) ;
#66177 = ADVANCED_FACE('',(#18892),#63216,.T.) ;
#66178 = ADVANCED_FACE('',(#18893),#7160,.T.) ;
#66179 = ADVANCED_FACE('',(#18894),#7161,.T.) ;
#66180 = ADVANCED_FACE('',(#18895),#63217,.T.) ;
#66181 = ADVANCED_FACE('',(#18896),#7162,.T.) ;
#66182 = ADVANCED_FACE('',(#18897),#7163,.T.) ;
#66183 = ADVANCED_FACE('',(#18898),#63218,.T.) ;
#66184 = ADVANCED_FACE('',(#18899),#63219,.T.) ;
#66185 = ADVANCED_FACE('',(#18900),#7164,.T.) ;
#66186 = ADVANCED_FACE('',(#18901),#63220,.T.) ;
#66187 = ADVANCED_FACE('',(#18902),#63221,.T.) ;
#66188 = ADVANCED_FACE('',(#18903),#63222,.T.) ;
#66189 = ADVANCED_FACE('',(#18904),#7165,.T.) ;
#66190 = ADVANCED_FACE('',(#18905),#7166,.T.) ;
#66191 = ADVANCED_FACE('',(#18906),#4517,.T.) ;
#66192 = ADVANCED_FACE('',(#18907),#63223,.T.) ;
#66193 = ADVANCED_FACE('',(#18908),#7167,.T.) ;
#66194 = ADVANCED_FACE('',(#18909),#7168,.T.) ;
#66195 = ADVANCED_FACE('',(#18910),#4518,.T.) ;
#66196 = ADVANCED_FACE('',(#18911),#63224,.T.) ;
#66197 = ADVANCED_FACE('',(#18912),#7169,.T.) ;
#66198 = ADVANCED_FACE('',(#18913),#7170,.T.) ;
#66199 = ADVANCED_FACE('',(#18914),#4519,.T.) ;
#66200 = ADVANCED_FACE('',(#18915),#4520,.T.) ;
#66201 = ADVANCED_FACE('',(#18916),#7171,.T.) ;
#66202 = ADVANCED_FACE('',(#18917),#7172,.T.) ;
#66203 = ADVANCED_FACE('',(#18918),#63225,.T.) ;
#66204 = ADVANCED_FACE('',(#18919),#63226,.T.) ;
#66205 = ADVANCED_FACE('',(#18920),#7173,.T.) ;
#66206 = ADVANCED_FACE('',(#18921),#7174,.T.) ;
#66207 = ADVANCED_FACE('',(#18922),#63227,.T.) ;
#66208 = ADVANCED_FACE('',(#18923),#7175,.T.) ;
#66209 = ADVANCED_FACE('',(#18924),#7176,.T.) ;
#66210 = ADVANCED_FACE('',(#18925),#63228,.T.) ;
#66211 = ADVANCED_FACE('',(#18926),#63229,.T.) ;
#66212 = ADVANCED_FACE('',(#18927),#7177,.T.) ;
#66213 = ADVANCED_FACE('',(#18928),#63230,.T.) ;
#66214 = ADVANCED_FACE('',(#18929),#63231,.T.) ;
#66215 = ADVANCED_FACE('',(#18930),#63232,.T.) ;
#66216 = ADVANCED_FACE('',(#18931),#7178,.T.) ;
#66217 = ADVANCED_FACE('',(#18932),#7179,.T.) ;
#66218 = ADVANCED_FACE('',(#18933),#4521,.T.) ;
#66219 = ADVANCED_FACE('',(#18934),#63233,.T.) ;
#66220 = ADVANCED_FACE('',(#18935),#7180,.T.) ;
#66221 = ADVANCED_FACE('',(#18936),#7181,.T.) ;
#66222 = ADVANCED_FACE('',(#18937),#4522,.T.) ;
#66223 = ADVANCED_FACE('',(#18938),#63234,.T.) ;
#66224 = ADVANCED_FACE('',(#18939),#7182,.T.) ;
#66225 = ADVANCED_FACE('',(#18940),#7183,.T.) ;
#66226 = ADVANCED_FACE('',(#18941),#4523,.T.) ;
#66227 = ADVANCED_FACE('',(#18942),#4524,.T.) ;
#66228 = ADVANCED_FACE('',(#18943),#7184,.T.) ;
#66229 = ADVANCED_FACE('',(#18944),#7185,.T.) ;
#66230 = ADVANCED_FACE('',(#18945),#63235,.T.) ;
#66231 = ADVANCED_FACE('',(#18946),#63236,.T.) ;
#66232 = ADVANCED_FACE('',(#18947),#7186,.T.) ;
#66233 = ADVANCED_FACE('',(#18948),#7187,.T.) ;
#66234 = ADVANCED_FACE('',(#18949),#63237,.T.) ;
#66235 = ADVANCED_FACE('',(#18950),#7188,.T.) ;
#66236 = ADVANCED_FACE('',(#18951),#7189,.T.) ;
#66237 = ADVANCED_FACE('',(#18952),#63238,.T.) ;
#66238 = ADVANCED_FACE('',(#18953),#63239,.T.) ;
#66239 = ADVANCED_FACE('',(#18954),#7190,.T.) ;
#66240 = ADVANCED_FACE('',(#18955),#63240,.T.) ;
#66241 = ADVANCED_FACE('',(#18956),#63241,.T.) ;
#66242 = ADVANCED_FACE('',(#18957),#63242,.T.) ;
#66243 = ADVANCED_FACE('',(#18958),#7191,.T.) ;
#66244 = ADVANCED_FACE('',(#18959),#7192,.T.) ;
#66245 = ADVANCED_FACE('',(#18960),#4525,.T.) ;
#66246 = ADVANCED_FACE('',(#18961),#63243,.T.) ;
#66247 = ADVANCED_FACE('',(#18962),#7193,.T.) ;
#66248 = ADVANCED_FACE('',(#18963),#7194,.T.) ;
#66249 = ADVANCED_FACE('',(#18964),#4526,.T.) ;
#66250 = ADVANCED_FACE('',(#18965),#63244,.T.) ;
#66251 = ADVANCED_FACE('',(#18966),#7195,.T.) ;
#66252 = ADVANCED_FACE('',(#18967),#7196,.T.) ;
#66253 = ADVANCED_FACE('',(#18968),#4527,.T.) ;
#66254 = ADVANCED_FACE('',(#18969),#4528,.T.) ;
#66255 = ADVANCED_FACE('',(#18970),#7197,.T.) ;
#66256 = ADVANCED_FACE('',(#18971),#7198,.T.) ;
#66257 = ADVANCED_FACE('',(#18972),#63245,.T.) ;
#66258 = ADVANCED_FACE('',(#18973),#63246,.T.) ;
#66259 = ADVANCED_FACE('',(#18974),#7199,.T.) ;
#66260 = ADVANCED_FACE('',(#18975),#7200,.T.) ;
#66261 = ADVANCED_FACE('',(#18976),#63247,.T.) ;
#66262 = ADVANCED_FACE('',(#18977),#7201,.T.) ;
#66263 = ADVANCED_FACE('',(#18978),#7202,.T.) ;
#66264 = ADVANCED_FACE('',(#18979),#63248,.T.) ;
#66265 = ADVANCED_FACE('',(#18980),#63249,.T.) ;
#66266 = ADVANCED_FACE('',(#18981),#7203,.T.) ;
#66267 = ADVANCED_FACE('',(#18982),#63250,.T.) ;
#66268 = ADVANCED_FACE('',(#18983),#63251,.T.) ;
#66269 = ADVANCED_FACE('',(#18984),#63252,.T.) ;
#66270 = ADVANCED_FACE('',(#18985),#7204,.T.) ;
#66271 = ADVANCED_FACE('',(#18986),#7205,.T.) ;
#66272 = ADVANCED_FACE('',(#18987),#4529,.T.) ;
#66273 = ADVANCED_FACE('',(#18988),#63253,.T.) ;
#66274 = ADVANCED_FACE('',(#18989),#7206,.T.) ;
#66275 = ADVANCED_FACE('',(#18990),#7207,.T.) ;
#66276 = ADVANCED_FACE('',(#18991),#4530,.T.) ;
#66277 = ADVANCED_FACE('',(#18992),#63254,.T.) ;
#66278 = ADVANCED_FACE('',(#18993),#7208,.T.) ;
#66279 = ADVANCED_FACE('',(#18994),#7209,.T.) ;
#66280 = ADVANCED_FACE('',(#18995),#4531,.T.) ;
#66281 = ADVANCED_FACE('',(#18996),#4532,.T.) ;
#66282 = ADVANCED_FACE('',(#18997),#7210,.T.) ;
#66283 = ADVANCED_FACE('',(#18998),#7211,.T.) ;
#66284 = ADVANCED_FACE('',(#18999),#63255,.T.) ;
#66285 = ADVANCED_FACE('',(#19000),#63256,.T.) ;
#66286 = ADVANCED_FACE('',(#19001),#7212,.T.) ;
#66287 = ADVANCED_FACE('',(#19002),#7213,.T.) ;
#66288 = ADVANCED_FACE('',(#19003),#63257,.T.) ;
#66289 = ADVANCED_FACE('',(#19004),#7214,.T.) ;
#66290 = ADVANCED_FACE('',(#19005),#7215,.T.) ;
#66291 = ADVANCED_FACE('',(#19006),#63258,.T.) ;
#66292 = ADVANCED_FACE('',(#19007),#63259,.T.) ;
#66293 = ADVANCED_FACE('',(#19008),#7216,.T.) ;
#66294 = ADVANCED_FACE('',(#19009),#63260,.T.) ;
#66295 = ADVANCED_FACE('',(#19010),#63261,.T.) ;
#66296 = ADVANCED_FACE('',(#19011),#63262,.T.) ;
#66297 = ADVANCED_FACE('',(#19012),#7217,.T.) ;
#66298 = ADVANCED_FACE('',(#19013),#7218,.T.) ;
#66299 = ADVANCED_FACE('',(#19014),#4533,.T.) ;
#66300 = ADVANCED_FACE('',(#19015),#63263,.T.) ;
#66301 = ADVANCED_FACE('',(#19016),#7219,.T.) ;
#66302 = ADVANCED_FACE('',(#19017),#7220,.T.) ;
#66303 = ADVANCED_FACE('',(#19018),#4534,.T.) ;
#66304 = ADVANCED_FACE('',(#19019),#63264,.T.) ;
#66305 = ADVANCED_FACE('',(#19020),#7221,.T.) ;
#66306 = ADVANCED_FACE('',(#19021),#7222,.T.) ;
#66307 = ADVANCED_FACE('',(#19022),#4535,.T.) ;
#66308 = ADVANCED_FACE('',(#19023),#4536,.T.) ;
#66309 = ADVANCED_FACE('',(#19024),#7223,.T.) ;
#66310 = ADVANCED_FACE('',(#19025),#7224,.T.) ;
#66311 = ADVANCED_FACE('',(#19026),#63265,.T.) ;
#66312 = ADVANCED_FACE('',(#19027),#63266,.T.) ;
#66313 = ADVANCED_FACE('',(#19028),#7225,.T.) ;
#66314 = ADVANCED_FACE('',(#19029),#7226,.T.) ;
#66315 = ADVANCED_FACE('',(#19030),#63267,.T.) ;
#66316 = ADVANCED_FACE('',(#19031),#7227,.T.) ;
#66317 = ADVANCED_FACE('',(#19032),#7228,.T.) ;
#66318 = ADVANCED_FACE('',(#19033),#63268,.T.) ;
#66319 = ADVANCED_FACE('',(#19034),#63269,.T.) ;
#66320 = ADVANCED_FACE('',(#19035),#7229,.T.) ;
#66321 = ADVANCED_FACE('',(#19036),#63270,.T.) ;
#66322 = ADVANCED_FACE('',(#19037),#63271,.T.) ;
#66323 = ADVANCED_FACE('',(#19038),#63272,.T.) ;
#66324 = ADVANCED_FACE('',(#19039),#7230,.T.) ;
#66325 = ADVANCED_FACE('',(#19040),#7231,.T.) ;
#66326 = ADVANCED_FACE('',(#19041),#4537,.T.) ;
#66327 = ADVANCED_FACE('',(#19042),#63273,.T.) ;
#66328 = ADVANCED_FACE('',(#19043),#7232,.T.) ;
#66329 = ADVANCED_FACE('',(#19044),#7233,.T.) ;
#66330 = ADVANCED_FACE('',(#19045),#4538,.T.) ;
#66331 = ADVANCED_FACE('',(#19046),#63274,.T.) ;
#66332 = ADVANCED_FACE('',(#19047),#7234,.T.) ;
#66333 = ADVANCED_FACE('',(#19048),#7235,.T.) ;
#66334 = ADVANCED_FACE('',(#19049),#4539,.T.) ;
#66335 = ADVANCED_FACE('',(#19050),#4540,.T.) ;
#66336 = ADVANCED_FACE('',(#19051),#7236,.T.) ;
#66337 = ADVANCED_FACE('',(#19052),#7237,.T.) ;
#66338 = ADVANCED_FACE('',(#19053),#63275,.T.) ;
#66339 = ADVANCED_FACE('',(#19054),#63276,.T.) ;
#66340 = ADVANCED_FACE('',(#19055),#7238,.T.) ;
#66341 = ADVANCED_FACE('',(#19056),#7239,.T.) ;
#66342 = ADVANCED_FACE('',(#19057),#63277,.T.) ;
#66343 = ADVANCED_FACE('',(#19058),#7240,.T.) ;
#66344 = ADVANCED_FACE('',(#19059),#7241,.T.) ;
#66345 = ADVANCED_FACE('',(#19060),#63278,.T.) ;
#66346 = ADVANCED_FACE('',(#19061),#63279,.T.) ;
#66347 = ADVANCED_FACE('',(#19062),#7242,.T.) ;
#66348 = ADVANCED_FACE('',(#19063),#63280,.T.) ;
#66349 = ADVANCED_FACE('',(#19064),#63281,.T.) ;
#66350 = ADVANCED_FACE('',(#19065),#63282,.T.) ;
#66351 = ADVANCED_FACE('',(#19066),#7243,.T.) ;
#66352 = ADVANCED_FACE('',(#19067),#7244,.T.) ;
#66353 = ADVANCED_FACE('',(#19068),#4541,.T.) ;
#66354 = ADVANCED_FACE('',(#19069),#63283,.T.) ;
#66355 = ADVANCED_FACE('',(#19070),#7245,.T.) ;
#66356 = ADVANCED_FACE('',(#19071),#7246,.T.) ;
#66357 = ADVANCED_FACE('',(#19072),#4542,.T.) ;
#66358 = ADVANCED_FACE('',(#19073),#63284,.T.) ;
#66359 = ADVANCED_FACE('',(#19074),#7247,.T.) ;
#66360 = ADVANCED_FACE('',(#19075),#7248,.T.) ;
#66361 = ADVANCED_FACE('',(#19076),#7249,.F.) ;
#66362 = ADVANCED_FACE('',(#19077),#4543,.F.) ;
#66363 = ADVANCED_FACE('',(#19078),#4544,.T.) ;
#66364 = ADVANCED_FACE('',(#19079),#63285,.T.) ;
#66365 = ADVANCED_FACE('',(#19080),#7250,.F.) ;
#66366 = ADVANCED_FACE('',(#19081),#7251,.F.) ;
#66367 = ADVANCED_FACE('',(#19082),#7252,.T.) ;
#66368 = ADVANCED_FACE('',(#19083),#7253,.T.) ;
#66369 = ADVANCED_FACE('',(#19084),#7254,.T.) ;
#66370 = ADVANCED_FACE('',(#19085),#7255,.F.) ;
#66371 = ADVANCED_FACE('',(#19086),#4545,.F.) ;
#66372 = ADVANCED_FACE('',(#19087),#63286,.F.) ;
#66373 = ADVANCED_FACE('',(#19088),#63287,.F.) ;
#66374 = ADVANCED_FACE('',(#19089),#63288,.T.) ;
#66375 = ADVANCED_FACE('',(#19090),#7256,.F.) ;
#66376 = ADVANCED_FACE('',(#19091),#7257,.F.) ;
#66377 = ADVANCED_FACE('',(#19092),#7258,.F.) ;
#66378 = ADVANCED_FACE('',(#19093),#7259,.T.) ;
#66379 = ADVANCED_FACE('',(#19094),#7260,.T.) ;
#66380 = ADVANCED_FACE('',(#19095),#63289,.F.) ;
#66381 = ADVANCED_FACE('',(#19096),#4546,.F.) ;
#66382 = ADVANCED_FACE('',(#19097),#4547,.T.) ;
#66383 = ADVANCED_FACE('',(#19098),#7261,.T.) ;
#66384 = ADVANCED_FACE('',(#19099),#4548,.F.) ;
#66385 = ADVANCED_FACE('',(#19100),#4549,.T.) ;
#66386 = ADVANCED_FACE('',(#19101),#7262,.F.) ;
#66387 = ADVANCED_FACE('',(#19102),#7263,.F.) ;
#66388 = ADVANCED_FACE('',(#19103),#7264,.T.) ;
#66389 = ADVANCED_FACE('',(#19104),#63290,.T.) ;
#66390 = ADVANCED_FACE('',(#19105),#7265,.F.) ;
#66391 = ADVANCED_FACE('',(#19106),#7266,.T.) ;
#66392 = ADVANCED_FACE('',(#19107),#7267,.F.) ;
#66393 = ADVANCED_FACE('',(#19108),#4550,.F.) ;
#66394 = ADVANCED_FACE('',(#19109),#63291,.T.) ;
#66395 = ADVANCED_FACE('',(#19110),#7268,.T.) ;
#66396 = ADVANCED_FACE('',(#19111),#4551,.F.) ;
#66397 = ADVANCED_FACE('',(#19112),#63292,.F.) ;
#66398 = ADVANCED_FACE('',(#19113),#7269,.F.) ;
#66399 = ADVANCED_FACE('',(#19114),#7270,.T.) ;
#66400 = ADVANCED_FACE('',(#19115),#63293,.T.) ;
#66401 = ADVANCED_FACE('',(#19116),#7271,.F.) ;
#66402 = ADVANCED_FACE('',(#19117),#63294,.T.) ;
#66403 = ADVANCED_FACE('',(#19118),#7272,.T.) ;
#66404 = ADVANCED_FACE('',(#19119),#7273,.T.) ;
#66405 = ADVANCED_FACE('',(#19120),#4552,.T.) ;
#66406 = ADVANCED_FACE('',(#19121),#7274,.F.) ;
#66407 = ADVANCED_FACE('',(#19122),#63295,.F.) ;
#66408 = ADVANCED_FACE('',(#19123),#4553,.F.) ;
#66409 = ADVANCED_FACE('',(#19124),#7275,.F.) ;
#66410 = ADVANCED_FACE('',(#19125),#7276,.F.) ;
#66411 = ADVANCED_FACE('',(#19126),#63296,.F.) ;
#66412 = ADVANCED_FACE('',(#19127),#4554,.F.) ;
#66413 = ADVANCED_FACE('',(#19128),#7277,.F.) ;
#66414 = ADVANCED_FACE('',(#19129),#7278,.F.) ;
#66415 = ADVANCED_FACE('',(#19130),#4555,.F.) ;
#66416 = ADVANCED_FACE('',(#19131),#4556,.F.) ;
#66417 = ADVANCED_FACE('',(#19132),#7279,.F.) ;
#66418 = ADVANCED_FACE('',(#19133),#63297,.F.) ;
#66419 = ADVANCED_FACE('',(#19134),#4557,.F.) ;
#66420 = ADVANCED_FACE('',(#19135),#4558,.F.) ;
#66421 = ADVANCED_FACE('',(#19136),#7280,.F.) ;
#66422 = ADVANCED_FACE('',(#19137),#7281,.F.) ;
#66423 = ADVANCED_FACE('',(#19138),#4559,.F.) ;
#66424 = ADVANCED_FACE('',(#19139),#7282,.F.) ;
#66425 = ADVANCED_FACE('',(#19140),#7283,.F.) ;
#66426 = ADVANCED_FACE('',(#19141),#4560,.F.) ;
#66427 = ADVANCED_FACE('',(#19142),#4561,.F.) ;
#66428 = ADVANCED_FACE('',(#19143),#7284,.F.) ;
#66429 = ADVANCED_FACE('',(#19144),#7285,.F.) ;
#66430 = ADVANCED_FACE('',(#19145),#63298,.F.) ;
#66431 = ADVANCED_FACE('',(#19146),#63299,.F.) ;
#66432 = ADVANCED_FACE('',(#19147),#7286,.F.) ;
#66433 = ADVANCED_FACE('',(#19148),#7287,.T.) ;
#66434 = ADVANCED_FACE('',(#19149),#7288,.F.) ;
#66435 = ADVANCED_FACE('',(#19150),#4562,.F.) ;
#66436 = ADVANCED_FACE('',(#19151),#4563,.T.) ;
#66437 = ADVANCED_FACE('',(#19152),#63300,.T.) ;
#66438 = ADVANCED_FACE('',(#19153),#7289,.F.) ;
#66439 = ADVANCED_FACE('',(#19154),#7290,.F.) ;
#66440 = ADVANCED_FACE('',(#19155),#7291,.T.) ;
#66441 = ADVANCED_FACE('',(#19156),#7292,.T.) ;
#66442 = ADVANCED_FACE('',(#19157),#7293,.T.) ;
#66443 = ADVANCED_FACE('',(#19158),#7294,.F.) ;
#66444 = ADVANCED_FACE('',(#19159),#4564,.F.) ;
#66445 = ADVANCED_FACE('',(#19160),#63301,.F.) ;
#66446 = ADVANCED_FACE('',(#19161),#63302,.F.) ;
#66447 = ADVANCED_FACE('',(#19162),#63303,.T.) ;
#66448 = ADVANCED_FACE('',(#19163),#7295,.F.) ;
#66449 = ADVANCED_FACE('',(#19164),#7296,.F.) ;
#66450 = ADVANCED_FACE('',(#19165),#7297,.F.) ;
#66451 = ADVANCED_FACE('',(#19166),#7298,.T.) ;
#66452 = ADVANCED_FACE('',(#19167),#7299,.T.) ;
#66453 = ADVANCED_FACE('',(#19168),#63304,.F.) ;
#66454 = ADVANCED_FACE('',(#19169),#4565,.F.) ;
#66455 = ADVANCED_FACE('',(#19170),#4566,.T.) ;
#66456 = ADVANCED_FACE('',(#19171),#7300,.T.) ;
#66457 = ADVANCED_FACE('',(#19172),#4567,.F.) ;
#66458 = ADVANCED_FACE('',(#19173),#4568,.T.) ;
#66459 = ADVANCED_FACE('',(#19174),#7301,.F.) ;
#66460 = ADVANCED_FACE('',(#19175),#7302,.F.) ;
#66461 = ADVANCED_FACE('',(#19176),#7303,.T.) ;
#66462 = ADVANCED_FACE('',(#19177),#63305,.T.) ;
#66463 = ADVANCED_FACE('',(#19178),#7304,.F.) ;
#66464 = ADVANCED_FACE('',(#19179),#7305,.T.) ;
#66465 = ADVANCED_FACE('',(#19180),#7306,.F.) ;
#66466 = ADVANCED_FACE('',(#19181),#4569,.F.) ;
#66467 = ADVANCED_FACE('',(#19182),#63306,.T.) ;
#66468 = ADVANCED_FACE('',(#19183),#7307,.T.) ;
#66469 = ADVANCED_FACE('',(#19184),#4570,.F.) ;
#66470 = ADVANCED_FACE('',(#19185),#63307,.F.) ;
#66471 = ADVANCED_FACE('',(#19186),#7308,.F.) ;
#66472 = ADVANCED_FACE('',(#19187),#7309,.T.) ;
#66473 = ADVANCED_FACE('',(#19188),#63308,.T.) ;
#66474 = ADVANCED_FACE('',(#19189),#7310,.F.) ;
#66475 = ADVANCED_FACE('',(#19190),#63309,.T.) ;
#66476 = ADVANCED_FACE('',(#19191),#7311,.T.) ;
#66477 = ADVANCED_FACE('',(#19192),#7312,.T.) ;
#66478 = ADVANCED_FACE('',(#19193),#4571,.T.) ;
#66479 = ADVANCED_FACE('',(#19194),#7313,.F.) ;
#66480 = ADVANCED_FACE('',(#19195),#63310,.F.) ;
#66481 = ADVANCED_FACE('',(#19196),#4572,.F.) ;
#66482 = ADVANCED_FACE('',(#19197),#7314,.F.) ;
#66483 = ADVANCED_FACE('',(#19198),#7315,.F.) ;
#66484 = ADVANCED_FACE('',(#19199),#63311,.F.) ;
#66485 = ADVANCED_FACE('',(#19200),#4573,.F.) ;
#66486 = ADVANCED_FACE('',(#19201),#7316,.F.) ;
#66487 = ADVANCED_FACE('',(#19202),#7317,.F.) ;
#66488 = ADVANCED_FACE('',(#19203),#4574,.F.) ;
#66489 = ADVANCED_FACE('',(#19204),#4575,.F.) ;
#66490 = ADVANCED_FACE('',(#19205),#7318,.F.) ;
#66491 = ADVANCED_FACE('',(#19206),#63312,.F.) ;
#66492 = ADVANCED_FACE('',(#19207),#4576,.F.) ;
#66493 = ADVANCED_FACE('',(#19208),#4577,.F.) ;
#66494 = ADVANCED_FACE('',(#19209),#7319,.F.) ;
#66495 = ADVANCED_FACE('',(#19210),#7320,.F.) ;
#66496 = ADVANCED_FACE('',(#19211),#4578,.F.) ;
#66497 = ADVANCED_FACE('',(#19212),#7321,.F.) ;
#66498 = ADVANCED_FACE('',(#19213),#7322,.F.) ;
#66499 = ADVANCED_FACE('',(#19214),#4579,.F.) ;
#66500 = ADVANCED_FACE('',(#19215),#4580,.F.) ;
#66501 = ADVANCED_FACE('',(#19216),#7323,.F.) ;
#66502 = ADVANCED_FACE('',(#19217),#7324,.F.) ;
#66503 = ADVANCED_FACE('',(#19218),#63313,.F.) ;
#66504 = ADVANCED_FACE('',(#19219),#63314,.F.) ;
#66505 = ADVANCED_FACE('',(#19220),#7325,.F.) ;
#66506 = ADVANCED_FACE('',(#19221),#7326,.T.) ;
#66507 = ADVANCED_FACE('',(#19222),#7327,.F.) ;
#66508 = ADVANCED_FACE('',(#19223),#4581,.F.) ;
#66509 = ADVANCED_FACE('',(#19224),#4582,.T.) ;
#66510 = ADVANCED_FACE('',(#19225),#63315,.T.) ;
#66511 = ADVANCED_FACE('',(#19226),#7328,.F.) ;
#66512 = ADVANCED_FACE('',(#19227),#7329,.F.) ;
#66513 = ADVANCED_FACE('',(#19228),#7330,.T.) ;
#66514 = ADVANCED_FACE('',(#19229),#7331,.T.) ;
#66515 = ADVANCED_FACE('',(#19230),#7332,.T.) ;
#66516 = ADVANCED_FACE('',(#19231),#7333,.F.) ;
#66517 = ADVANCED_FACE('',(#19232),#4583,.F.) ;
#66518 = ADVANCED_FACE('',(#19233),#63316,.F.) ;
#66519 = ADVANCED_FACE('',(#19234),#63317,.F.) ;
#66520 = ADVANCED_FACE('',(#19235),#63318,.T.) ;
#66521 = ADVANCED_FACE('',(#19236),#7334,.F.) ;
#66522 = ADVANCED_FACE('',(#19237),#7335,.F.) ;
#66523 = ADVANCED_FACE('',(#19238),#7336,.F.) ;
#66524 = ADVANCED_FACE('',(#19239),#7337,.T.) ;
#66525 = ADVANCED_FACE('',(#19240),#7338,.T.) ;
#66526 = ADVANCED_FACE('',(#19241),#63319,.F.) ;
#66527 = ADVANCED_FACE('',(#19242),#4584,.F.) ;
#66528 = ADVANCED_FACE('',(#19243),#4585,.T.) ;
#66529 = ADVANCED_FACE('',(#19244),#7339,.T.) ;
#66530 = ADVANCED_FACE('',(#19245),#4586,.F.) ;
#66531 = ADVANCED_FACE('',(#19246),#4587,.T.) ;
#66532 = ADVANCED_FACE('',(#19247),#7340,.F.) ;
#66533 = ADVANCED_FACE('',(#19248),#7341,.F.) ;
#66534 = ADVANCED_FACE('',(#19249),#7342,.T.) ;
#66535 = ADVANCED_FACE('',(#19250),#63320,.T.) ;
#66536 = ADVANCED_FACE('',(#19251),#7343,.F.) ;
#66537 = ADVANCED_FACE('',(#19252),#7344,.T.) ;
#66538 = ADVANCED_FACE('',(#19253),#7345,.F.) ;
#66539 = ADVANCED_FACE('',(#19254),#4588,.F.) ;
#66540 = ADVANCED_FACE('',(#19255),#63321,.T.) ;
#66541 = ADVANCED_FACE('',(#19256),#7346,.T.) ;
#66542 = ADVANCED_FACE('',(#19257),#4589,.F.) ;
#66543 = ADVANCED_FACE('',(#19258),#63322,.F.) ;
#66544 = ADVANCED_FACE('',(#19259),#7347,.F.) ;
#66545 = ADVANCED_FACE('',(#19260),#7348,.T.) ;
#66546 = ADVANCED_FACE('',(#19261),#63323,.T.) ;
#66547 = ADVANCED_FACE('',(#19262),#7349,.F.) ;
#66548 = ADVANCED_FACE('',(#19263),#63324,.T.) ;
#66549 = ADVANCED_FACE('',(#19264),#7350,.T.) ;
#66550 = ADVANCED_FACE('',(#19265),#7351,.T.) ;
#66551 = ADVANCED_FACE('',(#19266),#4590,.T.) ;
#66552 = ADVANCED_FACE('',(#19267),#7352,.F.) ;
#66553 = ADVANCED_FACE('',(#19268),#63325,.F.) ;
#66554 = ADVANCED_FACE('',(#19269),#4591,.F.) ;
#66555 = ADVANCED_FACE('',(#19270),#7353,.F.) ;
#66556 = ADVANCED_FACE('',(#19271),#7354,.F.) ;
#66557 = ADVANCED_FACE('',(#19272),#63326,.F.) ;
#66558 = ADVANCED_FACE('',(#19273),#4592,.F.) ;
#66559 = ADVANCED_FACE('',(#19274),#7355,.F.) ;
#66560 = ADVANCED_FACE('',(#19275),#7356,.F.) ;
#66561 = ADVANCED_FACE('',(#19276),#4593,.F.) ;
#66562 = ADVANCED_FACE('',(#19277),#4594,.F.) ;
#66563 = ADVANCED_FACE('',(#19278),#7357,.F.) ;
#66564 = ADVANCED_FACE('',(#19279),#63327,.F.) ;
#66565 = ADVANCED_FACE('',(#19280),#4595,.F.) ;
#66566 = ADVANCED_FACE('',(#19281),#4596,.F.) ;
#66567 = ADVANCED_FACE('',(#19282),#7358,.F.) ;
#66568 = ADVANCED_FACE('',(#19283),#7359,.F.) ;
#66569 = ADVANCED_FACE('',(#19284),#4597,.F.) ;
#66570 = ADVANCED_FACE('',(#19285),#7360,.F.) ;
#66571 = ADVANCED_FACE('',(#19286),#7361,.F.) ;
#66572 = ADVANCED_FACE('',(#19287),#4598,.F.) ;
#66573 = ADVANCED_FACE('',(#19288),#4599,.F.) ;
#66574 = ADVANCED_FACE('',(#19289),#7362,.F.) ;
#66575 = ADVANCED_FACE('',(#19290),#7363,.F.) ;
#66576 = ADVANCED_FACE('',(#19291),#63328,.F.) ;
#66577 = ADVANCED_FACE('',(#19292),#63329,.F.) ;
#66578 = ADVANCED_FACE('',(#19293),#7364,.F.) ;
#66579 = ADVANCED_FACE('',(#19294),#7365,.T.) ;
#66580 = ADVANCED_FACE('',(#19295),#7366,.F.) ;
#66581 = ADVANCED_FACE('',(#19296),#4600,.F.) ;
#66582 = ADVANCED_FACE('',(#19297),#4601,.T.) ;
#66583 = ADVANCED_FACE('',(#19298),#63330,.T.) ;
#66584 = ADVANCED_FACE('',(#19299),#7367,.F.) ;
#66585 = ADVANCED_FACE('',(#19300),#7368,.F.) ;
#66586 = ADVANCED_FACE('',(#19301),#7369,.T.) ;
#66587 = ADVANCED_FACE('',(#19302),#7370,.T.) ;
#66588 = ADVANCED_FACE('',(#19303),#7371,.T.) ;
#66589 = ADVANCED_FACE('',(#19304),#7372,.F.) ;
#66590 = ADVANCED_FACE('',(#19305),#4602,.F.) ;
#66591 = ADVANCED_FACE('',(#19306),#63331,.F.) ;
#66592 = ADVANCED_FACE('',(#19307),#63332,.F.) ;
#66593 = ADVANCED_FACE('',(#19308),#63333,.T.) ;
#66594 = ADVANCED_FACE('',(#19309),#7373,.F.) ;
#66595 = ADVANCED_FACE('',(#19310),#7374,.F.) ;
#66596 = ADVANCED_FACE('',(#19311),#7375,.F.) ;
#66597 = ADVANCED_FACE('',(#19312),#7376,.T.) ;
#66598 = ADVANCED_FACE('',(#19313),#7377,.T.) ;
#66599 = ADVANCED_FACE('',(#19314),#63334,.F.) ;
#66600 = ADVANCED_FACE('',(#19315),#4603,.F.) ;
#66601 = ADVANCED_FACE('',(#19316),#4604,.T.) ;
#66602 = ADVANCED_FACE('',(#19317),#7378,.T.) ;
#66603 = ADVANCED_FACE('',(#19318),#4605,.F.) ;
#66604 = ADVANCED_FACE('',(#19319),#4606,.T.) ;
#66605 = ADVANCED_FACE('',(#19320),#7379,.F.) ;
#66606 = ADVANCED_FACE('',(#19321),#7380,.F.) ;
#66607 = ADVANCED_FACE('',(#19322),#7381,.T.) ;
#66608 = ADVANCED_FACE('',(#19323),#63335,.T.) ;
#66609 = ADVANCED_FACE('',(#19324),#7382,.F.) ;
#66610 = ADVANCED_FACE('',(#19325),#7383,.T.) ;
#66611 = ADVANCED_FACE('',(#19326),#7384,.F.) ;
#66612 = ADVANCED_FACE('',(#19327),#4607,.F.) ;
#66613 = ADVANCED_FACE('',(#19328),#63336,.T.) ;
#66614 = ADVANCED_FACE('',(#19329),#7385,.T.) ;
#66615 = ADVANCED_FACE('',(#19330),#4608,.F.) ;
#66616 = ADVANCED_FACE('',(#19331),#63337,.F.) ;
#66617 = ADVANCED_FACE('',(#19332),#7386,.F.) ;
#66618 = ADVANCED_FACE('',(#19333),#7387,.T.) ;
#66619 = ADVANCED_FACE('',(#19334),#63338,.T.) ;
#66620 = ADVANCED_FACE('',(#19335),#7388,.F.) ;
#66621 = ADVANCED_FACE('',(#19336),#63339,.T.) ;
#66622 = ADVANCED_FACE('',(#19337),#7389,.T.) ;
#66623 = ADVANCED_FACE('',(#19338),#7390,.T.) ;
#66624 = ADVANCED_FACE('',(#19339),#4609,.T.) ;
#66625 = ADVANCED_FACE('',(#19340),#7391,.F.) ;
#66626 = ADVANCED_FACE('',(#19341),#63340,.F.) ;
#66627 = ADVANCED_FACE('',(#19342),#4610,.F.) ;
#66628 = ADVANCED_FACE('',(#19343),#7392,.F.) ;
#66629 = ADVANCED_FACE('',(#19344),#7393,.F.) ;
#66630 = ADVANCED_FACE('',(#19345),#63341,.F.) ;
#66631 = ADVANCED_FACE('',(#19346),#4611,.F.) ;
#66632 = ADVANCED_FACE('',(#19347),#7394,.F.) ;
#66633 = ADVANCED_FACE('',(#19348),#7395,.F.) ;
#66634 = ADVANCED_FACE('',(#19349),#4612,.F.) ;
#66635 = ADVANCED_FACE('',(#19350),#4613,.F.) ;
#66636 = ADVANCED_FACE('',(#19351),#7396,.F.) ;
#66637 = ADVANCED_FACE('',(#19352),#63342,.F.) ;
#66638 = ADVANCED_FACE('',(#19353),#4614,.F.) ;
#66639 = ADVANCED_FACE('',(#19354),#4615,.F.) ;
#66640 = ADVANCED_FACE('',(#19355),#7397,.F.) ;
#66641 = ADVANCED_FACE('',(#19356),#7398,.F.) ;
#66642 = ADVANCED_FACE('',(#19357),#4616,.F.) ;
#66643 = ADVANCED_FACE('',(#19358),#7399,.F.) ;
#66644 = ADVANCED_FACE('',(#19359),#7400,.F.) ;
#66645 = ADVANCED_FACE('',(#19360),#4617,.F.) ;
#66646 = ADVANCED_FACE('',(#19361),#4618,.F.) ;
#66647 = ADVANCED_FACE('',(#19362),#7401,.F.) ;
#66648 = ADVANCED_FACE('',(#19363),#7402,.F.) ;
#66649 = ADVANCED_FACE('',(#19364),#63343,.F.) ;
#66650 = ADVANCED_FACE('',(#19365),#63344,.F.) ;
#66651 = ADVANCED_FACE('',(#19366),#7403,.F.) ;
#66652 = ADVANCED_FACE('',(#19367),#7404,.T.) ;
#66653 = ADVANCED_FACE('',(#19368),#7405,.F.) ;
#66654 = ADVANCED_FACE('',(#19369),#4619,.F.) ;
#66655 = ADVANCED_FACE('',(#19370),#4620,.T.) ;
#66656 = ADVANCED_FACE('',(#19371),#63345,.T.) ;
#66657 = ADVANCED_FACE('',(#19372),#7406,.F.) ;
#66658 = ADVANCED_FACE('',(#19373),#7407,.F.) ;
#66659 = ADVANCED_FACE('',(#19374),#7408,.T.) ;
#66660 = ADVANCED_FACE('',(#19375),#7409,.T.) ;
#66661 = ADVANCED_FACE('',(#19376),#7410,.T.) ;
#66662 = ADVANCED_FACE('',(#19377),#7411,.F.) ;
#66663 = ADVANCED_FACE('',(#19378),#4621,.F.) ;
#66664 = ADVANCED_FACE('',(#19379),#63346,.F.) ;
#66665 = ADVANCED_FACE('',(#19380),#63347,.F.) ;
#66666 = ADVANCED_FACE('',(#19381),#63348,.T.) ;
#66667 = ADVANCED_FACE('',(#19382),#7412,.F.) ;
#66668 = ADVANCED_FACE('',(#19383),#7413,.F.) ;
#66669 = ADVANCED_FACE('',(#19384),#7414,.F.) ;
#66670 = ADVANCED_FACE('',(#19385),#7415,.T.) ;
#66671 = ADVANCED_FACE('',(#19386),#7416,.T.) ;
#66672 = ADVANCED_FACE('',(#19387),#63349,.F.) ;
#66673 = ADVANCED_FACE('',(#19388),#4622,.F.) ;
#66674 = ADVANCED_FACE('',(#19389),#4623,.T.) ;
#66675 = ADVANCED_FACE('',(#19390),#7417,.T.) ;
#66676 = ADVANCED_FACE('',(#19391),#4624,.F.) ;
#66677 = ADVANCED_FACE('',(#19392),#4625,.T.) ;
#66678 = ADVANCED_FACE('',(#19393),#7418,.F.) ;
#66679 = ADVANCED_FACE('',(#19394),#7419,.F.) ;
#66680 = ADVANCED_FACE('',(#19395),#7420,.T.) ;
#66681 = ADVANCED_FACE('',(#19396),#63350,.T.) ;
#66682 = ADVANCED_FACE('',(#19397),#7421,.F.) ;
#66683 = ADVANCED_FACE('',(#19398),#7422,.T.) ;
#66684 = ADVANCED_FACE('',(#19399),#7423,.F.) ;
#66685 = ADVANCED_FACE('',(#19400),#4626,.F.) ;
#66686 = ADVANCED_FACE('',(#19401),#63351,.T.) ;
#66687 = ADVANCED_FACE('',(#19402),#7424,.T.) ;
#66688 = ADVANCED_FACE('',(#19403),#4627,.F.) ;
#66689 = ADVANCED_FACE('',(#19404),#63352,.F.) ;
#66690 = ADVANCED_FACE('',(#19405),#7425,.F.) ;
#66691 = ADVANCED_FACE('',(#19406),#7426,.T.) ;
#66692 = ADVANCED_FACE('',(#19407),#63353,.T.) ;
#66693 = ADVANCED_FACE('',(#19408),#7427,.F.) ;
#66694 = ADVANCED_FACE('',(#19409),#63354,.T.) ;
#66695 = ADVANCED_FACE('',(#19410),#7428,.T.) ;
#66696 = ADVANCED_FACE('',(#19411),#7429,.T.) ;
#66697 = ADVANCED_FACE('',(#19412),#4628,.T.) ;
#66698 = ADVANCED_FACE('',(#19413),#7430,.F.) ;
#66699 = ADVANCED_FACE('',(#19414),#63355,.F.) ;
#66700 = ADVANCED_FACE('',(#19415),#4629,.F.) ;
#66701 = ADVANCED_FACE('',(#19416),#7431,.F.) ;
#66702 = ADVANCED_FACE('',(#19417),#7432,.F.) ;
#66703 = ADVANCED_FACE('',(#19418),#63356,.F.) ;
#66704 = ADVANCED_FACE('',(#19419),#4630,.F.) ;
#66705 = ADVANCED_FACE('',(#19420),#7433,.F.) ;
#66706 = ADVANCED_FACE('',(#19421),#7434,.F.) ;
#66707 = ADVANCED_FACE('',(#19422),#4631,.F.) ;
#66708 = ADVANCED_FACE('',(#19423),#4632,.F.) ;
#66709 = ADVANCED_FACE('',(#19424),#7435,.F.) ;
#66710 = ADVANCED_FACE('',(#19425),#63357,.F.) ;
#66711 = ADVANCED_FACE('',(#19426),#4633,.F.) ;
#66712 = ADVANCED_FACE('',(#19427),#4634,.F.) ;
#66713 = ADVANCED_FACE('',(#19428),#7436,.F.) ;
#66714 = ADVANCED_FACE('',(#19429),#7437,.F.) ;
#66715 = ADVANCED_FACE('',(#19430),#4635,.F.) ;
#66716 = ADVANCED_FACE('',(#19431),#7438,.F.) ;
#66717 = ADVANCED_FACE('',(#19432),#7439,.F.) ;
#66718 = ADVANCED_FACE('',(#19433),#4636,.F.) ;
#66719 = ADVANCED_FACE('',(#19434),#4637,.F.) ;
#66720 = ADVANCED_FACE('',(#19435),#7440,.F.) ;
#66721 = ADVANCED_FACE('',(#19436),#7441,.F.) ;
#66722 = ADVANCED_FACE('',(#19437),#63358,.F.) ;
#66723 = ADVANCED_FACE('',(#19438),#63359,.F.) ;
#66724 = ADVANCED_FACE('',(#19439),#7442,.F.) ;
#66725 = ADVANCED_FACE('',(#19440),#7443,.T.) ;
#66726 = ADVANCED_FACE('',(#19441),#7444,.F.) ;
#66727 = ADVANCED_FACE('',(#19442),#4638,.F.) ;
#66728 = ADVANCED_FACE('',(#19443),#4639,.T.) ;
#66729 = ADVANCED_FACE('',(#19444),#63360,.T.) ;
#66730 = ADVANCED_FACE('',(#19445),#7445,.F.) ;
#66731 = ADVANCED_FACE('',(#19446),#7446,.F.) ;
#66732 = ADVANCED_FACE('',(#19447),#7447,.T.) ;
#66733 = ADVANCED_FACE('',(#19448),#7448,.T.) ;
#66734 = ADVANCED_FACE('',(#19449),#7449,.T.) ;
#66735 = ADVANCED_FACE('',(#19450),#7450,.F.) ;
#66736 = ADVANCED_FACE('',(#19451),#4640,.F.) ;
#66737 = ADVANCED_FACE('',(#19452),#63361,.F.) ;
#66738 = ADVANCED_FACE('',(#19453),#63362,.F.) ;
#66739 = ADVANCED_FACE('',(#19454),#63363,.T.) ;
#66740 = ADVANCED_FACE('',(#19455),#7451,.F.) ;
#66741 = ADVANCED_FACE('',(#19456),#7452,.F.) ;
#66742 = ADVANCED_FACE('',(#19457),#7453,.F.) ;
#66743 = ADVANCED_FACE('',(#19458),#7454,.T.) ;
#66744 = ADVANCED_FACE('',(#19459),#7455,.T.) ;
#66745 = ADVANCED_FACE('',(#19460),#63364,.F.) ;
#66746 = ADVANCED_FACE('',(#19461),#4641,.F.) ;
#66747 = ADVANCED_FACE('',(#19462),#4642,.T.) ;
#66748 = ADVANCED_FACE('',(#19463),#7456,.T.) ;
#66749 = ADVANCED_FACE('',(#19464),#4643,.F.) ;
#66750 = ADVANCED_FACE('',(#19465),#4644,.T.) ;
#66751 = ADVANCED_FACE('',(#19466),#7457,.F.) ;
#66752 = ADVANCED_FACE('',(#19467),#7458,.F.) ;
#66753 = ADVANCED_FACE('',(#19468),#7459,.T.) ;
#66754 = ADVANCED_FACE('',(#19469),#63365,.T.) ;
#66755 = ADVANCED_FACE('',(#19470),#7460,.F.) ;
#66756 = ADVANCED_FACE('',(#19471),#7461,.T.) ;
#66757 = ADVANCED_FACE('',(#19472),#7462,.F.) ;
#66758 = ADVANCED_FACE('',(#19473),#4645,.F.) ;
#66759 = ADVANCED_FACE('',(#19474),#63366,.T.) ;
#66760 = ADVANCED_FACE('',(#19475),#7463,.T.) ;
#66761 = ADVANCED_FACE('',(#19476),#4646,.F.) ;
#66762 = ADVANCED_FACE('',(#19477),#63367,.F.) ;
#66763 = ADVANCED_FACE('',(#19478),#7464,.F.) ;
#66764 = ADVANCED_FACE('',(#19479),#7465,.T.) ;
#66765 = ADVANCED_FACE('',(#19480),#63368,.T.) ;
#66766 = ADVANCED_FACE('',(#19481),#7466,.F.) ;
#66767 = ADVANCED_FACE('',(#19482),#63369,.T.) ;
#66768 = ADVANCED_FACE('',(#19483),#7467,.T.) ;
#66769 = ADVANCED_FACE('',(#19484),#7468,.T.) ;
#66770 = ADVANCED_FACE('',(#19485),#4647,.T.) ;
#66771 = ADVANCED_FACE('',(#19486),#7469,.F.) ;
#66772 = ADVANCED_FACE('',(#19487),#63370,.F.) ;
#66773 = ADVANCED_FACE('',(#19488),#4648,.F.) ;
#66774 = ADVANCED_FACE('',(#19489),#7470,.F.) ;
#66775 = ADVANCED_FACE('',(#19490),#7471,.F.) ;
#66776 = ADVANCED_FACE('',(#19491),#63371,.F.) ;
#66777 = ADVANCED_FACE('',(#19492),#4649,.F.) ;
#66778 = ADVANCED_FACE('',(#19493),#7472,.F.) ;
#66779 = ADVANCED_FACE('',(#19494),#7473,.F.) ;
#66780 = ADVANCED_FACE('',(#19495),#4650,.F.) ;
#66781 = ADVANCED_FACE('',(#19496),#4651,.F.) ;
#66782 = ADVANCED_FACE('',(#19497),#7474,.F.) ;
#66783 = ADVANCED_FACE('',(#19498),#63372,.F.) ;
#66784 = ADVANCED_FACE('',(#19499),#4652,.F.) ;
#66785 = ADVANCED_FACE('',(#19500),#4653,.F.) ;
#66786 = ADVANCED_FACE('',(#19501),#7475,.F.) ;
#66787 = ADVANCED_FACE('',(#19502),#7476,.F.) ;
#66788 = ADVANCED_FACE('',(#19503),#4654,.F.) ;
#66789 = ADVANCED_FACE('',(#19504),#7477,.F.) ;
#66790 = ADVANCED_FACE('',(#19505),#7478,.F.) ;
#66791 = ADVANCED_FACE('',(#19506),#4655,.F.) ;
#66792 = ADVANCED_FACE('',(#19507),#4656,.F.) ;
#66793 = ADVANCED_FACE('',(#19508),#7479,.F.) ;
#66794 = ADVANCED_FACE('',(#19509),#7480,.F.) ;
#66795 = ADVANCED_FACE('',(#19510),#63373,.F.) ;
#66796 = ADVANCED_FACE('',(#19511),#63374,.F.) ;
#66797 = ADVANCED_FACE('',(#19512),#7481,.F.) ;
#66798 = ADVANCED_FACE('',(#19513),#7482,.T.) ;
#66799 = ADVANCED_FACE('',(#19514),#7483,.F.) ;
#66800 = ADVANCED_FACE('',(#19515),#4657,.F.) ;
#66801 = ADVANCED_FACE('',(#19516),#4658,.T.) ;
#66802 = ADVANCED_FACE('',(#19517),#63375,.T.) ;
#66803 = ADVANCED_FACE('',(#19518),#7484,.F.) ;
#66804 = ADVANCED_FACE('',(#19519),#7485,.F.) ;
#66805 = ADVANCED_FACE('',(#19520),#7486,.T.) ;
#66806 = ADVANCED_FACE('',(#19521),#7487,.T.) ;
#66807 = ADVANCED_FACE('',(#19522),#7488,.T.) ;
#66808 = ADVANCED_FACE('',(#19523),#7489,.F.) ;
#66809 = ADVANCED_FACE('',(#19524),#4659,.F.) ;
#66810 = ADVANCED_FACE('',(#19525),#63376,.F.) ;
#66811 = ADVANCED_FACE('',(#19526),#63377,.F.) ;
#66812 = ADVANCED_FACE('',(#19527),#63378,.T.) ;
#66813 = ADVANCED_FACE('',(#19528),#7490,.F.) ;
#66814 = ADVANCED_FACE('',(#19529),#7491,.F.) ;
#66815 = ADVANCED_FACE('',(#19530),#7492,.F.) ;
#66816 = ADVANCED_FACE('',(#19531),#7493,.T.) ;
#66817 = ADVANCED_FACE('',(#19532),#7494,.T.) ;
#66818 = ADVANCED_FACE('',(#19533),#63379,.F.) ;
#66819 = ADVANCED_FACE('',(#19534),#4660,.F.) ;
#66820 = ADVANCED_FACE('',(#19535),#4661,.T.) ;
#66821 = ADVANCED_FACE('',(#19536),#7495,.T.) ;
#66822 = ADVANCED_FACE('',(#19537),#4662,.F.) ;
#66823 = ADVANCED_FACE('',(#19538),#4663,.T.) ;
#66824 = ADVANCED_FACE('',(#19539),#7496,.F.) ;
#66825 = ADVANCED_FACE('',(#19540),#7497,.F.) ;
#66826 = ADVANCED_FACE('',(#19541),#7498,.T.) ;
#66827 = ADVANCED_FACE('',(#19542),#63380,.T.) ;
#66828 = ADVANCED_FACE('',(#19543),#7499,.F.) ;
#66829 = ADVANCED_FACE('',(#19544),#7500,.T.) ;
#66830 = ADVANCED_FACE('',(#19545),#7501,.F.) ;
#66831 = ADVANCED_FACE('',(#19546),#4664,.F.) ;
#66832 = ADVANCED_FACE('',(#19547),#63381,.T.) ;
#66833 = ADVANCED_FACE('',(#19548),#7502,.T.) ;
#66834 = ADVANCED_FACE('',(#19549),#4665,.F.) ;
#66835 = ADVANCED_FACE('',(#19550),#63382,.F.) ;
#66836 = ADVANCED_FACE('',(#19551),#7503,.F.) ;
#66837 = ADVANCED_FACE('',(#19552),#7504,.T.) ;
#66838 = ADVANCED_FACE('',(#19553),#63383,.T.) ;
#66839 = ADVANCED_FACE('',(#19554),#7505,.F.) ;
#66840 = ADVANCED_FACE('',(#19555),#63384,.T.) ;
#66841 = ADVANCED_FACE('',(#19556),#7506,.T.) ;
#66842 = ADVANCED_FACE('',(#19557),#7507,.T.) ;
#66843 = ADVANCED_FACE('',(#19558),#4666,.T.) ;
#66844 = ADVANCED_FACE('',(#19559),#7508,.F.) ;
#66845 = ADVANCED_FACE('',(#19560),#63385,.F.) ;
#66846 = ADVANCED_FACE('',(#19561),#4667,.F.) ;
#66847 = ADVANCED_FACE('',(#19562),#7509,.F.) ;
#66848 = ADVANCED_FACE('',(#19563),#7510,.F.) ;
#66849 = ADVANCED_FACE('',(#19564),#63386,.F.) ;
#66850 = ADVANCED_FACE('',(#19565),#4668,.F.) ;
#66851 = ADVANCED_FACE('',(#19566),#7511,.F.) ;
#66852 = ADVANCED_FACE('',(#19567),#7512,.F.) ;
#66853 = ADVANCED_FACE('',(#19568),#4669,.F.) ;
#66854 = ADVANCED_FACE('',(#19569),#4670,.F.) ;
#66855 = ADVANCED_FACE('',(#19570),#7513,.F.) ;
#66856 = ADVANCED_FACE('',(#19571),#63387,.F.) ;
#66857 = ADVANCED_FACE('',(#19572),#4671,.F.) ;
#66858 = ADVANCED_FACE('',(#19573),#4672,.F.) ;
#66859 = ADVANCED_FACE('',(#19574),#7514,.F.) ;
#66860 = ADVANCED_FACE('',(#19575),#7515,.F.) ;
#66861 = ADVANCED_FACE('',(#19576),#4673,.F.) ;
#66862 = ADVANCED_FACE('',(#19577),#7516,.F.) ;
#66863 = ADVANCED_FACE('',(#19578),#7517,.F.) ;
#66864 = ADVANCED_FACE('',(#19579),#4674,.F.) ;
#66865 = ADVANCED_FACE('',(#19580),#4675,.F.) ;
#66866 = ADVANCED_FACE('',(#19581),#7518,.F.) ;
#66867 = ADVANCED_FACE('',(#19582),#7519,.F.) ;
#66868 = ADVANCED_FACE('',(#19583),#63388,.F.) ;
#66869 = ADVANCED_FACE('',(#19584),#63389,.F.) ;
#66870 = ADVANCED_FACE('',(#19585),#7520,.F.) ;
#66871 = ADVANCED_FACE('',(#19586),#7521,.T.) ;
#66872 = ADVANCED_FACE('',(#19587),#7522,.F.) ;
#66873 = ADVANCED_FACE('',(#19588),#4676,.F.) ;
#66874 = ADVANCED_FACE('',(#19589),#4677,.T.) ;
#66875 = ADVANCED_FACE('',(#19590),#63390,.T.) ;
#66876 = ADVANCED_FACE('',(#19591),#7523,.F.) ;
#66877 = ADVANCED_FACE('',(#19592),#7524,.F.) ;
#66878 = ADVANCED_FACE('',(#19593),#7525,.T.) ;
#66879 = ADVANCED_FACE('',(#19594),#7526,.T.) ;
#66880 = ADVANCED_FACE('',(#19595),#7527,.T.) ;
#66881 = ADVANCED_FACE('',(#19596),#7528,.F.) ;
#66882 = ADVANCED_FACE('',(#19597),#4678,.F.) ;
#66883 = ADVANCED_FACE('',(#19598),#63391,.F.) ;
#66884 = ADVANCED_FACE('',(#19599),#63392,.F.) ;
#66885 = ADVANCED_FACE('',(#19600),#63393,.T.) ;
#66886 = ADVANCED_FACE('',(#19601),#7529,.F.) ;
#66887 = ADVANCED_FACE('',(#19602),#7530,.F.) ;
#66888 = ADVANCED_FACE('',(#19603),#7531,.F.) ;
#66889 = ADVANCED_FACE('',(#19604),#7532,.T.) ;
#66890 = ADVANCED_FACE('',(#19605),#7533,.T.) ;
#66891 = ADVANCED_FACE('',(#19606),#63394,.F.) ;
#66892 = ADVANCED_FACE('',(#19607),#4679,.F.) ;
#66893 = ADVANCED_FACE('',(#19608),#4680,.T.) ;
#66894 = ADVANCED_FACE('',(#19609),#7534,.T.) ;
#66895 = ADVANCED_FACE('',(#19610),#4681,.F.) ;
#66896 = ADVANCED_FACE('',(#19611),#4682,.T.) ;
#66897 = ADVANCED_FACE('',(#19612),#7535,.F.) ;
#66898 = ADVANCED_FACE('',(#19613),#7536,.F.) ;
#66899 = ADVANCED_FACE('',(#19614),#7537,.T.) ;
#66900 = ADVANCED_FACE('',(#19615),#63395,.T.) ;
#66901 = ADVANCED_FACE('',(#19616),#7538,.F.) ;
#66902 = ADVANCED_FACE('',(#19617),#7539,.T.) ;
#66903 = ADVANCED_FACE('',(#19618),#7540,.F.) ;
#66904 = ADVANCED_FACE('',(#19619),#4683,.F.) ;
#66905 = ADVANCED_FACE('',(#19620),#63396,.T.) ;
#66906 = ADVANCED_FACE('',(#19621),#7541,.T.) ;
#66907 = ADVANCED_FACE('',(#19622),#4684,.F.) ;
#66908 = ADVANCED_FACE('',(#19623),#63397,.F.) ;
#66909 = ADVANCED_FACE('',(#19624),#7542,.F.) ;
#66910 = ADVANCED_FACE('',(#19625),#7543,.T.) ;
#66911 = ADVANCED_FACE('',(#19626),#63398,.T.) ;
#66912 = ADVANCED_FACE('',(#19627),#7544,.F.) ;
#66913 = ADVANCED_FACE('',(#19628),#63399,.T.) ;
#66914 = ADVANCED_FACE('',(#19629),#7545,.T.) ;
#66915 = ADVANCED_FACE('',(#19630),#7546,.T.) ;
#66916 = ADVANCED_FACE('',(#19631),#4685,.T.) ;
#66917 = ADVANCED_FACE('',(#19632),#7547,.F.) ;
#66918 = ADVANCED_FACE('',(#19633),#63400,.F.) ;
#66919 = ADVANCED_FACE('',(#19634),#4686,.F.) ;
#66920 = ADVANCED_FACE('',(#19635),#7548,.F.) ;
#66921 = ADVANCED_FACE('',(#19636),#7549,.F.) ;
#66922 = ADVANCED_FACE('',(#19637),#63401,.F.) ;
#66923 = ADVANCED_FACE('',(#19638),#4687,.F.) ;
#66924 = ADVANCED_FACE('',(#19639),#7550,.F.) ;
#66925 = ADVANCED_FACE('',(#19640),#7551,.F.) ;
#66926 = ADVANCED_FACE('',(#19641),#4688,.F.) ;
#66927 = ADVANCED_FACE('',(#19642),#4689,.F.) ;
#66928 = ADVANCED_FACE('',(#19643),#7552,.F.) ;
#66929 = ADVANCED_FACE('',(#19644),#63402,.F.) ;
#66930 = ADVANCED_FACE('',(#19645),#4690,.F.) ;
#66931 = ADVANCED_FACE('',(#19646),#4691,.F.) ;
#66932 = ADVANCED_FACE('',(#19647),#7553,.F.) ;
#66933 = ADVANCED_FACE('',(#19648),#7554,.F.) ;
#66934 = ADVANCED_FACE('',(#19649),#4692,.F.) ;
#66935 = ADVANCED_FACE('',(#19650),#7555,.F.) ;
#66936 = ADVANCED_FACE('',(#19651),#7556,.F.) ;
#66937 = ADVANCED_FACE('',(#19652),#4693,.F.) ;
#66938 = ADVANCED_FACE('',(#19653),#4694,.F.) ;
#66939 = ADVANCED_FACE('',(#19654),#7557,.F.) ;
#66940 = ADVANCED_FACE('',(#19655),#7558,.F.) ;
#66941 = ADVANCED_FACE('',(#19656),#63403,.F.) ;
#66942 = ADVANCED_FACE('',(#19657),#63404,.F.) ;
#66943 = ADVANCED_FACE('',(#19658),#7559,.F.) ;
#66944 = ADVANCED_FACE('',(#19659),#5751,.F.) ;
#66945 = ADVANCED_FACE('',(#19660),#5752,.F.) ;
#66946 = ADVANCED_FACE('',(#19661),#5753,.F.) ;
#66947 = ADVANCED_FACE('',(#19662),#5754,.F.) ;
#66948 = ADVANCED_FACE('',(#19663),#5755,.F.) ;
#66949 = ADVANCED_FACE('',(#19664),#5756,.T.) ;
#66950 = ADVANCED_FACE('',(#19665),#5757,.F.) ;
#66951 = ADVANCED_FACE('',(#19666),#7560,.T.) ;
#66952 = ADVANCED_FACE('',(#19667),#7561,.F.) ;
#66953 = ADVANCED_FACE('',(#19668),#5758,.F.) ;
#66954 = ADVANCED_FACE('',(#19669),#5759,.F.) ;
#66955 = ADVANCED_FACE('',(#19670),#5760,.F.) ;
#66956 = ADVANCED_FACE('',(#19671),#5761,.F.) ;
#66957 = ADVANCED_FACE('',(#19672),#5762,.F.) ;
#66958 = ADVANCED_FACE('',(#19673),#5763,.T.) ;
#66959 = ADVANCED_FACE('',(#19674),#5764,.F.) ;
#66960 = ADVANCED_FACE('',(#19675),#5765,.F.) ;
#66961 = ADVANCED_FACE('',(#19676),#5766,.F.) ;
#66962 = ADVANCED_FACE('',(#19677),#5767,.F.) ;
#66963 = ADVANCED_FACE('',(#19678),#5768,.F.) ;
#66964 = ADVANCED_FACE('',(#19679),#5769,.F.) ;
#66965 = ADVANCED_FACE('',(#19680),#5770,.T.) ;
#66966 = ADVANCED_FACE('',(#19681),#5771,.F.) ;
#66967 = ADVANCED_FACE('',(#19682),#7562,.T.) ;
#66968 = ADVANCED_FACE('',(#19683),#7563,.F.) ;
#66969 = ADVANCED_FACE('',(#19684),#5772,.F.) ;
#66970 = ADVANCED_FACE('',(#19685),#5773,.F.) ;
#66971 = ADVANCED_FACE('',(#19686),#5774,.F.) ;
#66972 = ADVANCED_FACE('',(#19687),#5775,.F.) ;
#66973 = ADVANCED_FACE('',(#19688),#5776,.F.) ;
#66974 = ADVANCED_FACE('',(#19689),#5777,.T.) ;
#66975 = ADVANCED_FACE('',(#19690),#5778,.F.) ;
#66976 = ADVANCED_FACE('',(#19691),#5779,.F.) ;
#66977 = ADVANCED_FACE('',(#19692),#5780,.F.) ;
#66978 = ADVANCED_FACE('',(#19693),#5781,.F.) ;
#66979 = ADVANCED_FACE('',(#19694),#5782,.F.) ;
#66980 = ADVANCED_FACE('',(#19695),#5783,.F.) ;
#66981 = ADVANCED_FACE('',(#19696),#5784,.T.) ;
#66982 = ADVANCED_FACE('',(#19697),#5785,.F.) ;
#66983 = ADVANCED_FACE('',(#19698),#7564,.T.) ;
#66984 = ADVANCED_FACE('',(#19699),#7565,.F.) ;
#66985 = ADVANCED_FACE('',(#19700),#5786,.F.) ;
#66986 = ADVANCED_FACE('',(#19701),#5787,.F.) ;
#66987 = ADVANCED_FACE('',(#19702),#5788,.F.) ;
#66988 = ADVANCED_FACE('',(#19703),#5789,.F.) ;
#66989 = ADVANCED_FACE('',(#19704),#5790,.F.) ;
#66990 = ADVANCED_FACE('',(#19705),#5791,.T.) ;
#66991 = ADVANCED_FACE('',(#19706),#5792,.F.) ;
#66992 = ADVANCED_FACE('',(#19707),#5793,.F.) ;
#66993 = ADVANCED_FACE('',(#19708),#5794,.F.) ;
#66994 = ADVANCED_FACE('',(#19709),#5795,.F.) ;
#66995 = ADVANCED_FACE('',(#19710),#5796,.F.) ;
#66996 = ADVANCED_FACE('',(#19711),#5797,.F.) ;
#66997 = ADVANCED_FACE('',(#19712),#5798,.T.) ;
#66998 = ADVANCED_FACE('',(#19713),#5799,.F.) ;
#66999 = ADVANCED_FACE('',(#19714),#7566,.T.) ;
#67000 = ADVANCED_FACE('',(#19715),#7567,.F.) ;
#67001 = ADVANCED_FACE('',(#19716),#5800,.F.) ;
#67002 = ADVANCED_FACE('',(#19717),#5801,.F.) ;
#67003 = ADVANCED_FACE('',(#19718),#5802,.F.) ;
#67004 = ADVANCED_FACE('',(#19719),#5803,.F.) ;
#67005 = ADVANCED_FACE('',(#19720),#5804,.F.) ;
#67006 = ADVANCED_FACE('',(#19721),#5805,.T.) ;
#67007 = ADVANCED_FACE('',(#19722),#5806,.F.) ;
#67008 = ADVANCED_FACE('',(#19723),#5807,.F.) ;
#67009 = ADVANCED_FACE('',(#19724),#5808,.F.) ;
#67010 = ADVANCED_FACE('',(#19725),#5809,.F.) ;
#67011 = ADVANCED_FACE('',(#19726),#5810,.F.) ;
#67012 = ADVANCED_FACE('',(#19727),#5811,.F.) ;
#67013 = ADVANCED_FACE('',(#19728),#5812,.T.) ;
#67014 = ADVANCED_FACE('',(#19729),#5813,.F.) ;
#67015 = ADVANCED_FACE('',(#19730),#7568,.T.) ;
#67016 = ADVANCED_FACE('',(#19731),#7569,.F.) ;
#67017 = ADVANCED_FACE('',(#19732),#5814,.F.) ;
#67018 = ADVANCED_FACE('',(#19733),#5815,.F.) ;
#67019 = ADVANCED_FACE('',(#19734),#5816,.F.) ;
#67020 = ADVANCED_FACE('',(#19735),#5817,.F.) ;
#67021 = ADVANCED_FACE('',(#19736),#5818,.F.) ;
#67022 = ADVANCED_FACE('',(#19737),#5819,.T.) ;
#67023 = ADVANCED_FACE('',(#19738),#5820,.F.) ;
#67024 = ADVANCED_FACE('',(#19739),#5821,.F.) ;
#67025 = ADVANCED_FACE('',(#19740),#5822,.F.) ;
#67026 = ADVANCED_FACE('',(#19741),#5823,.F.) ;
#67027 = ADVANCED_FACE('',(#19742),#5824,.F.) ;
#67028 = ADVANCED_FACE('',(#19743),#5825,.F.) ;
#67029 = ADVANCED_FACE('',(#19744),#5826,.T.) ;
#67030 = ADVANCED_FACE('',(#19745),#5827,.F.) ;
#67031 = ADVANCED_FACE('',(#19746),#7570,.T.) ;
#67032 = ADVANCED_FACE('',(#19747),#7571,.F.) ;
#67033 = ADVANCED_FACE('',(#19748),#5828,.F.) ;
#67034 = ADVANCED_FACE('',(#19749),#5829,.F.) ;
#67035 = ADVANCED_FACE('',(#19750),#5830,.F.) ;
#67036 = ADVANCED_FACE('',(#19751),#5831,.F.) ;
#67037 = ADVANCED_FACE('',(#19752),#5832,.F.) ;
#67038 = ADVANCED_FACE('',(#19753),#5833,.T.) ;
#67039 = ADVANCED_FACE('',(#19754),#5834,.F.) ;
#67040 = ADVANCED_FACE('',(#19755),#5835,.F.) ;
#67041 = ADVANCED_FACE('',(#19756),#5836,.F.) ;
#67042 = ADVANCED_FACE('',(#19757),#5837,.F.) ;
#67043 = ADVANCED_FACE('',(#19758),#5838,.F.) ;
#67044 = ADVANCED_FACE('',(#19759),#5839,.F.) ;
#67045 = ADVANCED_FACE('',(#19760),#5840,.T.) ;
#67046 = ADVANCED_FACE('',(#19761),#5841,.F.) ;
#67047 = ADVANCED_FACE('',(#19762),#7572,.T.) ;
#67048 = ADVANCED_FACE('',(#19763),#7573,.F.) ;
#67049 = ADVANCED_FACE('',(#19764),#5842,.F.) ;
#67050 = ADVANCED_FACE('',(#19765),#5843,.F.) ;
#67051 = ADVANCED_FACE('',(#19766),#5844,.F.) ;
#67052 = ADVANCED_FACE('',(#19767),#5845,.F.) ;
#67053 = ADVANCED_FACE('',(#19768),#5846,.F.) ;
#67054 = ADVANCED_FACE('',(#19769),#5847,.T.) ;
#67055 = ADVANCED_FACE('',(#19770),#5848,.F.) ;
#67056 = ADVANCED_FACE('',(#19771),#5849,.F.) ;
#67057 = ADVANCED_FACE('',(#19772),#5850,.F.) ;
#67058 = ADVANCED_FACE('',(#19773),#5851,.F.) ;
#67059 = ADVANCED_FACE('',(#19774),#5852,.F.) ;
#67060 = ADVANCED_FACE('',(#19775),#5853,.F.) ;
#67061 = ADVANCED_FACE('',(#19776),#5854,.T.) ;
#67062 = ADVANCED_FACE('',(#19777),#5855,.F.) ;
#67063 = ADVANCED_FACE('',(#19778),#7574,.T.) ;
#67064 = ADVANCED_FACE('',(#19779),#7575,.F.) ;
#67065 = ADVANCED_FACE('',(#19780),#5856,.F.) ;
#67066 = ADVANCED_FACE('',(#19781),#5857,.F.) ;
#67067 = ADVANCED_FACE('',(#19782),#5858,.F.) ;
#67068 = ADVANCED_FACE('',(#19783),#5859,.F.) ;
#67069 = ADVANCED_FACE('',(#19784),#5860,.F.) ;
#67070 = ADVANCED_FACE('',(#19785),#5861,.T.) ;
#67071 = ADVANCED_FACE('',(#19786),#5862,.F.) ;
#67072 = ADVANCED_FACE('',(#19787),#5863,.F.) ;
#67073 = ADVANCED_FACE('',(#19788),#5864,.F.) ;
#67074 = ADVANCED_FACE('',(#19789),#5865,.F.) ;
#67075 = ADVANCED_FACE('',(#19790),#5866,.F.) ;
#67076 = ADVANCED_FACE('',(#19791),#5867,.F.) ;
#67077 = ADVANCED_FACE('',(#19792),#5868,.T.) ;
#67078 = ADVANCED_FACE('',(#19793),#5869,.F.) ;
#67079 = ADVANCED_FACE('',(#19794),#7576,.T.) ;
#67080 = ADVANCED_FACE('',(#19795),#7577,.F.) ;
#67081 = ADVANCED_FACE('',(#19796),#5870,.F.) ;
#67082 = ADVANCED_FACE('',(#19797),#5871,.F.) ;
#67083 = ADVANCED_FACE('',(#19798),#5872,.F.) ;
#67084 = ADVANCED_FACE('',(#19799),#5873,.F.) ;
#67085 = ADVANCED_FACE('',(#19800),#5874,.F.) ;
#67086 = ADVANCED_FACE('',(#19801),#5875,.T.) ;
#67087 = ADVANCED_FACE('',(#19802),#5876,.F.) ;
#67088 = ADVANCED_FACE('',(#19803),#5877,.F.) ;
#67089 = ADVANCED_FACE('',(#19804),#5878,.F.) ;
#67090 = ADVANCED_FACE('',(#19805),#5879,.F.) ;
#67091 = ADVANCED_FACE('',(#19806),#5880,.F.) ;
#67092 = ADVANCED_FACE('',(#19807),#5881,.F.) ;
#67093 = ADVANCED_FACE('',(#19808),#5882,.F.) ;
#67094 = ADVANCED_FACE('',(#19809),#5883,.F.) ;
#67095 = ADVANCED_FACE('',(#19810),#5884,.F.) ;
#67096 = ADVANCED_FACE('',(#19811),#5885,.F.) ;
#67097 = ADVANCED_FACE('',(#19812),#5886,.F.) ;
#67098 = ADVANCED_FACE('',(#19813),#5887,.F.) ;
#67099 = ADVANCED_FACE('',(#19814),#5888,.F.) ;
#67100 = ADVANCED_FACE('',(#19815),#5889,.F.) ;
#67101 = ADVANCED_FACE('',(#19816),#5890,.F.) ;
#67102 = ADVANCED_FACE('',(#19817),#5891,.F.) ;
#67103 = ADVANCED_FACE('',(#19818),#5892,.F.) ;
#67104 = ADVANCED_FACE('',(#19819),#5893,.F.) ;
#67105 = ADVANCED_FACE('',(#19820),#5894,.F.) ;
#67106 = ADVANCED_FACE('',(#19821),#5895,.F.) ;
#67107 = ADVANCED_FACE('',(#19822),#5896,.F.) ;
#67108 = ADVANCED_FACE('',(#19823),#5897,.F.) ;
#67109 = ADVANCED_FACE('',(#19824),#5898,.F.) ;
#67110 = ADVANCED_FACE('',(#19825),#5899,.F.) ;
#67111 = ADVANCED_FACE('',(#19826),#5900,.F.) ;
#67112 = ADVANCED_FACE('',(#19827),#5901,.F.) ;
#67113 = ADVANCED_FACE('',(#19828),#5902,.F.) ;
#67114 = ADVANCED_FACE('',(#19829),#5903,.F.) ;
#67115 = ADVANCED_FACE('',(#19830),#5904,.F.) ;
#67116 = ADVANCED_FACE('',(#19831),#5905,.F.) ;
#67117 = ADVANCED_FACE('',(#19832),#5906,.F.) ;
#67118 = ADVANCED_FACE('',(#19833),#5907,.F.) ;
#67119 = ADVANCED_FACE('',(#19834),#5908,.F.) ;
#67120 = ADVANCED_FACE('',(#19835),#5909,.F.) ;
#67121 = ADVANCED_FACE('',(#19836),#5910,.F.) ;
#67122 = ADVANCED_FACE('',(#19837),#5911,.F.) ;
#67123 = ADVANCED_FACE('',(#19838),#5912,.F.) ;
#67124 = ADVANCED_FACE('',(#19839),#7578,.T.) ;
#67125 = ADVANCED_FACE('',(#19840),#7579,.T.) ;
#67126 = ADVANCED_FACE('',(#19841),#4695,.T.) ;
#67127 = ADVANCED_FACE('',(#19842),#7580,.T.) ;
#67128 = ADVANCED_FACE('',(#19843),#7581,.T.) ;
#67129 = ADVANCED_FACE('',(#19844),#7582,.T.) ;
#67130 = ADVANCED_FACE('',(#19845),#4696,.T.) ;
#67131 = ADVANCED_FACE('',(#19846),#4697,.T.) ;
#67132 = ADVANCED_FACE('',(#19847),#7583,.T.) ;
#67133 = ADVANCED_FACE('',(#19848),#7584,.T.) ;
#67134 = ADVANCED_FACE('',(#19849),#7585,.T.) ;
#67135 = ADVANCED_FACE('',(#19850),#4698,.T.) ;
#67136 = ADVANCED_FACE('',(#19851),#7586,.T.) ;
#67137 = ADVANCED_FACE('',(#19852),#7587,.T.) ;
#67138 = ADVANCED_FACE('',(#19853),#7588,.T.) ;
#67139 = ADVANCED_FACE('',(#19854),#7589,.T.) ;
#67140 = ADVANCED_FACE('',(#19855),#4699,.T.) ;
#67141 = ADVANCED_FACE('',(#19856),#7590,.T.) ;
#67142 = ADVANCED_FACE('',(#19857),#7591,.T.) ;
#67143 = ADVANCED_FACE('',(#19858),#7592,.T.) ;
#67144 = ADVANCED_FACE('',(#19859),#4700,.T.) ;
#67145 = ADVANCED_FACE('',(#19860),#4701,.T.) ;
#67146 = ADVANCED_FACE('',(#19861),#7593,.T.) ;
#67147 = ADVANCED_FACE('',(#19862),#7594,.T.) ;
#67148 = ADVANCED_FACE('',(#19863),#7595,.T.) ;
#67149 = ADVANCED_FACE('',(#19864),#4702,.T.) ;
#67150 = ADVANCED_FACE('',(#19865),#7596,.T.) ;
#67151 = ADVANCED_FACE('',(#19866),#7597,.T.) ;
#67152 = ADVANCED_FACE('',(#19867),#7598,.T.) ;
#67153 = ADVANCED_FACE('',(#19868),#7599,.T.) ;
#67154 = ADVANCED_FACE('',(#19869),#4703,.T.) ;
#67155 = ADVANCED_FACE('',(#19870),#7600,.T.) ;
#67156 = ADVANCED_FACE('',(#19871),#7601,.T.) ;
#67157 = ADVANCED_FACE('',(#19872),#7602,.T.) ;
#67158 = ADVANCED_FACE('',(#19873),#4704,.T.) ;
#67159 = ADVANCED_FACE('',(#19874),#4705,.T.) ;
#67160 = ADVANCED_FACE('',(#19875),#7603,.T.) ;
#67161 = ADVANCED_FACE('',(#19876),#7604,.T.) ;
#67162 = ADVANCED_FACE('',(#19877),#7605,.T.) ;
#67163 = ADVANCED_FACE('',(#19878),#4706,.T.) ;
#67164 = ADVANCED_FACE('',(#19879),#7606,.T.) ;
#67165 = ADVANCED_FACE('',(#19880),#7607,.T.) ;
#67166 = ADVANCED_FACE('',(#19881),#7608,.T.) ;
#67167 = ADVANCED_FACE('',(#19882),#7609,.T.) ;
#67168 = ADVANCED_FACE('',(#19883),#4707,.T.) ;
#67169 = ADVANCED_FACE('',(#19884),#7610,.T.) ;
#67170 = ADVANCED_FACE('',(#19885),#7611,.T.) ;
#67171 = ADVANCED_FACE('',(#19886),#7612,.T.) ;
#67172 = ADVANCED_FACE('',(#19887),#4708,.T.) ;
#67173 = ADVANCED_FACE('',(#19888),#4709,.T.) ;
#67174 = ADVANCED_FACE('',(#19889),#7613,.T.) ;
#67175 = ADVANCED_FACE('',(#19890),#7614,.T.) ;
#67176 = ADVANCED_FACE('',(#19891),#7615,.T.) ;
#67177 = ADVANCED_FACE('',(#19892),#4710,.T.) ;
#67178 = ADVANCED_FACE('',(#19893),#7616,.T.) ;
#67179 = ADVANCED_FACE('',(#19894),#7617,.T.) ;
#67180 = ADVANCED_FACE('',(#19895),#7618,.T.) ;
#67181 = ADVANCED_FACE('',(#19896),#7619,.T.) ;
#67182 = ADVANCED_FACE('',(#19897),#4711,.T.) ;
#67183 = ADVANCED_FACE('',(#19898),#7620,.T.) ;
#67184 = ADVANCED_FACE('',(#19899),#7621,.T.) ;
#67185 = ADVANCED_FACE('',(#19900),#7622,.T.) ;
#67186 = ADVANCED_FACE('',(#19901),#4712,.T.) ;
#67187 = ADVANCED_FACE('',(#19902),#4713,.T.) ;
#67188 = ADVANCED_FACE('',(#19903),#7623,.T.) ;
#67189 = ADVANCED_FACE('',(#19904),#7624,.T.) ;
#67190 = ADVANCED_FACE('',(#19905),#7625,.T.) ;
#67191 = ADVANCED_FACE('',(#19906),#4714,.T.) ;
#67192 = ADVANCED_FACE('',(#19907),#7626,.T.) ;
#67193 = ADVANCED_FACE('',(#19908),#7627,.T.) ;
#67194 = ADVANCED_FACE('',(#19909),#7628,.T.) ;
#67195 = ADVANCED_FACE('',(#19910),#7629,.T.) ;
#67196 = ADVANCED_FACE('',(#19911),#4715,.T.) ;
#67197 = ADVANCED_FACE('',(#19912),#7630,.T.) ;
#67198 = ADVANCED_FACE('',(#19913),#7631,.T.) ;
#67199 = ADVANCED_FACE('',(#19914),#7632,.T.) ;
#67200 = ADVANCED_FACE('',(#19915),#4716,.T.) ;
#67201 = ADVANCED_FACE('',(#19916),#4717,.T.) ;
#67202 = ADVANCED_FACE('',(#19917),#7633,.T.) ;
#67203 = ADVANCED_FACE('',(#19918),#7634,.T.) ;
#67204 = ADVANCED_FACE('',(#19919),#7635,.T.) ;
#67205 = ADVANCED_FACE('',(#19920),#4718,.T.) ;
#67206 = ADVANCED_FACE('',(#19921),#7636,.T.) ;
#67207 = ADVANCED_FACE('',(#19922),#7637,.T.) ;
#67208 = ADVANCED_FACE('',(#19923),#7638,.T.) ;
#67209 = ADVANCED_FACE('',(#19924),#7639,.T.) ;
#67210 = ADVANCED_FACE('',(#19925),#4719,.T.) ;
#67211 = ADVANCED_FACE('',(#19926),#7640,.T.) ;
#67212 = ADVANCED_FACE('',(#19927),#7641,.T.) ;
#67213 = ADVANCED_FACE('',(#19928),#7642,.T.) ;
#67214 = ADVANCED_FACE('',(#19929),#4720,.T.) ;
#67215 = ADVANCED_FACE('',(#19930),#4721,.T.) ;
#67216 = ADVANCED_FACE('',(#19931),#7643,.T.) ;
#67217 = ADVANCED_FACE('',(#19932),#7644,.T.) ;
#67218 = ADVANCED_FACE('',(#19933),#7645,.T.) ;
#67219 = ADVANCED_FACE('',(#19934),#4722,.T.) ;
#67220 = ADVANCED_FACE('',(#19935),#7646,.T.) ;
#67221 = ADVANCED_FACE('',(#19936),#7647,.T.) ;
#67222 = ADVANCED_FACE('',(#19937),#7648,.T.) ;
#67223 = ADVANCED_FACE('',(#19938),#7649,.T.) ;
#67224 = ADVANCED_FACE('',(#19939),#4723,.T.) ;
#67225 = ADVANCED_FACE('',(#19940),#7650,.T.) ;
#67226 = ADVANCED_FACE('',(#19941),#7651,.T.) ;
#67227 = ADVANCED_FACE('',(#19942),#7652,.T.) ;
#67228 = ADVANCED_FACE('',(#19943),#4724,.T.) ;
#67229 = ADVANCED_FACE('',(#19944),#4725,.T.) ;
#67230 = ADVANCED_FACE('',(#19945),#7653,.T.) ;
#67231 = ADVANCED_FACE('',(#19946),#7654,.T.) ;
#67232 = ADVANCED_FACE('',(#19947),#7655,.T.) ;
#67233 = ADVANCED_FACE('',(#19948),#4726,.T.) ;
#67234 = ADVANCED_FACE('',(#19949),#7656,.T.) ;
#67235 = ADVANCED_FACE('',(#19950),#7657,.T.) ;
#67236 = ADVANCED_FACE('',(#19951),#7658,.T.) ;
#67237 = ADVANCED_FACE('',(#19952),#7659,.T.) ;
#67238 = ADVANCED_FACE('',(#19953),#4727,.T.) ;
#67239 = ADVANCED_FACE('',(#19954),#7660,.T.) ;
#67240 = ADVANCED_FACE('',(#19955),#7661,.T.) ;
#67241 = ADVANCED_FACE('',(#19956),#7662,.T.) ;
#67242 = ADVANCED_FACE('',(#19957),#4728,.T.) ;
#67243 = ADVANCED_FACE('',(#19958),#4729,.T.) ;
#67244 = ADVANCED_FACE('',(#19959),#7663,.T.) ;
#67245 = ADVANCED_FACE('',(#19960),#7664,.T.) ;
#67246 = ADVANCED_FACE('',(#19961),#7665,.T.) ;
#67247 = ADVANCED_FACE('',(#19962),#4730,.T.) ;
#67248 = ADVANCED_FACE('',(#19963),#7666,.T.) ;
#67249 = ADVANCED_FACE('',(#19964),#7667,.T.) ;
#67250 = ADVANCED_FACE('',(#19965),#7668,.T.) ;
#67251 = ADVANCED_FACE('',(#19966),#7669,.T.) ;
#67252 = ADVANCED_FACE('',(#19967),#4731,.T.) ;
#67253 = ADVANCED_FACE('',(#19968),#7670,.T.) ;
#67254 = ADVANCED_FACE('',(#19969),#7671,.T.) ;
#67255 = ADVANCED_FACE('',(#19970),#7672,.T.) ;
#67256 = ADVANCED_FACE('',(#19971),#4732,.T.) ;
#67257 = ADVANCED_FACE('',(#19972),#4733,.T.) ;
#67258 = ADVANCED_FACE('',(#19973),#7673,.T.) ;
#67259 = ADVANCED_FACE('',(#19974),#7674,.T.) ;
#67260 = ADVANCED_FACE('',(#19975),#7675,.T.) ;
#67261 = ADVANCED_FACE('',(#19976),#4734,.T.) ;
#67262 = ADVANCED_FACE('',(#19977),#7676,.T.) ;
#67263 = ADVANCED_FACE('',(#19978),#7677,.T.) ;
#67264 = ADVANCED_FACE('',(#19979),#7678,.T.) ;
#67265 = ADVANCED_FACE('',(#19980),#7679,.T.) ;
#67266 = ADVANCED_FACE('',(#19981),#4735,.T.) ;
#67267 = ADVANCED_FACE('',(#19982),#7680,.T.) ;
#67268 = ADVANCED_FACE('',(#19983),#7681,.T.) ;
#67269 = ADVANCED_FACE('',(#19984),#7682,.T.) ;
#67270 = ADVANCED_FACE('',(#19985),#4736,.T.) ;
#67271 = ADVANCED_FACE('',(#19986),#4737,.T.) ;
#67272 = ADVANCED_FACE('',(#19987),#7683,.T.) ;
#67273 = ADVANCED_FACE('',(#19988),#7684,.T.) ;
#67274 = ADVANCED_FACE('',(#19989),#7685,.T.) ;
#67275 = ADVANCED_FACE('',(#19990),#4738,.T.) ;
#67276 = ADVANCED_FACE('',(#19991),#7686,.T.) ;
#67277 = ADVANCED_FACE('',(#19992),#7687,.T.) ;
#67278 = ADVANCED_FACE('',(#19993),#7688,.T.) ;
#67279 = ADVANCED_FACE('',(#19994),#7689,.T.) ;
#67280 = ADVANCED_FACE('',(#19995),#4739,.T.) ;
#67281 = ADVANCED_FACE('',(#19996),#7690,.T.) ;
#67282 = ADVANCED_FACE('',(#19997),#7691,.T.) ;
#67283 = ADVANCED_FACE('',(#19998),#7692,.T.) ;
#67284 = ADVANCED_FACE('',(#19999),#4740,.T.) ;
#67285 = ADVANCED_FACE('',(#20000),#4741,.T.) ;
#67286 = ADVANCED_FACE('',(#20001),#7693,.T.) ;
#67287 = ADVANCED_FACE('',(#20002),#7694,.T.) ;
#67288 = ADVANCED_FACE('',(#20003),#7695,.T.) ;
#67289 = ADVANCED_FACE('',(#20004),#4742,.T.) ;
#67290 = ADVANCED_FACE('',(#20005),#7696,.T.) ;
#67291 = ADVANCED_FACE('',(#20006),#7697,.T.) ;
#67292 = ADVANCED_FACE('',(#20007),#7698,.T.) ;
#67293 = ADVANCED_FACE('',(#20008),#7699,.T.) ;
#67294 = ADVANCED_FACE('',(#20009),#4743,.T.) ;
#67295 = ADVANCED_FACE('',(#20010),#7700,.T.) ;
#67296 = ADVANCED_FACE('',(#20011),#7701,.T.) ;
#67297 = ADVANCED_FACE('',(#20012),#7702,.T.) ;
#67298 = ADVANCED_FACE('',(#20013),#4744,.T.) ;
#67299 = ADVANCED_FACE('',(#20014),#4745,.T.) ;
#67300 = ADVANCED_FACE('',(#20015),#7703,.T.) ;
#67301 = ADVANCED_FACE('',(#20016),#7704,.T.) ;
#67302 = ADVANCED_FACE('',(#20017),#7705,.T.) ;
#67303 = ADVANCED_FACE('',(#20018),#4746,.T.) ;
#67304 = ADVANCED_FACE('',(#20019),#7706,.T.) ;
#67305 = ADVANCED_FACE('',(#20020),#7707,.T.) ;
#67306 = ADVANCED_FACE('',(#20021),#7708,.T.) ;
#67307 = ADVANCED_FACE('',(#20022),#7709,.T.) ;
#67308 = ADVANCED_FACE('',(#20023),#4747,.T.) ;
#67309 = ADVANCED_FACE('',(#20024),#7710,.T.) ;
#67310 = ADVANCED_FACE('',(#20025),#7711,.T.) ;
#67311 = ADVANCED_FACE('',(#20026),#7712,.T.) ;
#67312 = ADVANCED_FACE('',(#20027),#4748,.T.) ;
#67313 = ADVANCED_FACE('',(#20028),#4749,.T.) ;
#67314 = ADVANCED_FACE('',(#20029),#7713,.T.) ;
#67315 = ADVANCED_FACE('',(#20030),#7714,.T.) ;
#67316 = ADVANCED_FACE('',(#20031),#7715,.T.) ;
#67317 = ADVANCED_FACE('',(#20032),#4750,.T.) ;
#67318 = ADVANCED_FACE('',(#20033),#7716,.T.) ;
#67319 = ADVANCED_FACE('',(#20034),#7717,.T.) ;
#67320 = ADVANCED_FACE('',(#20035),#7718,.T.) ;
#67321 = ADVANCED_FACE('',(#20036),#7719,.T.) ;
#67322 = ADVANCED_FACE('',(#20037),#4751,.T.) ;
#67323 = ADVANCED_FACE('',(#20038),#7720,.T.) ;
#67324 = ADVANCED_FACE('',(#20039),#7721,.T.) ;
#67325 = ADVANCED_FACE('',(#20040),#7722,.T.) ;
#67326 = ADVANCED_FACE('',(#20041),#4752,.T.) ;
#67327 = ADVANCED_FACE('',(#20042),#4753,.T.) ;
#67328 = ADVANCED_FACE('',(#20043),#7723,.T.) ;
#67329 = ADVANCED_FACE('',(#20044),#7724,.T.) ;
#67330 = ADVANCED_FACE('',(#20045),#7725,.T.) ;
#67331 = ADVANCED_FACE('',(#20046),#4754,.T.) ;
#67332 = ADVANCED_FACE('',(#20047),#7726,.T.) ;
#67333 = ADVANCED_FACE('',(#20048),#7727,.T.) ;
#67334 = ADVANCED_FACE('',(#20049),#7728,.T.) ;
#67335 = ADVANCED_FACE('',(#20050),#7729,.T.) ;
#67336 = ADVANCED_FACE('',(#20051),#4755,.T.) ;
#67337 = ADVANCED_FACE('',(#20052),#7730,.T.) ;
#67338 = ADVANCED_FACE('',(#20053),#7731,.T.) ;
#67339 = ADVANCED_FACE('',(#20054),#7732,.T.) ;
#67340 = ADVANCED_FACE('',(#20055),#4756,.T.) ;
#67341 = ADVANCED_FACE('',(#20056),#4757,.T.) ;
#67342 = ADVANCED_FACE('',(#20057),#7733,.T.) ;
#67343 = ADVANCED_FACE('',(#20058),#7734,.T.) ;
#67344 = ADVANCED_FACE('',(#20059),#7735,.T.) ;
#67345 = ADVANCED_FACE('',(#20060),#4758,.T.) ;
#67346 = ADVANCED_FACE('',(#20061),#7736,.T.) ;
#67347 = ADVANCED_FACE('',(#20062),#7737,.T.) ;
#67348 = ADVANCED_FACE('',(#20063),#7738,.T.) ;
#67349 = ADVANCED_FACE('',(#20064),#7739,.T.) ;
#67350 = ADVANCED_FACE('',(#20065),#4759,.T.) ;
#67351 = ADVANCED_FACE('',(#20066),#7740,.T.) ;
#67352 = ADVANCED_FACE('',(#20067),#7741,.T.) ;
#67353 = ADVANCED_FACE('',(#20068),#7742,.T.) ;
#67354 = ADVANCED_FACE('',(#20069),#4760,.T.) ;
#67355 = ADVANCED_FACE('',(#20070),#4761,.T.) ;
#67356 = ADVANCED_FACE('',(#20071),#7743,.T.) ;
#67357 = ADVANCED_FACE('',(#20072),#7744,.T.) ;
#67358 = ADVANCED_FACE('',(#20073),#7745,.T.) ;
#67359 = ADVANCED_FACE('',(#20074),#4762,.T.) ;
#67360 = ADVANCED_FACE('',(#20075),#7746,.T.) ;
#67361 = ADVANCED_FACE('',(#20076),#7747,.T.) ;
#67362 = ADVANCED_FACE('',(#20077),#7748,.T.) ;
#67363 = ADVANCED_FACE('',(#20078),#7749,.T.) ;
#67364 = ADVANCED_FACE('',(#20079),#4763,.T.) ;
#67365 = ADVANCED_FACE('',(#20080),#7750,.T.) ;
#67366 = ADVANCED_FACE('',(#20081),#7751,.T.) ;
#67367 = ADVANCED_FACE('',(#20082),#7752,.T.) ;
#67368 = ADVANCED_FACE('',(#20083),#4764,.T.) ;
#67369 = ADVANCED_FACE('',(#20084),#4765,.T.) ;
#67370 = ADVANCED_FACE('',(#20085),#7753,.T.) ;
#67371 = ADVANCED_FACE('',(#20086),#7754,.T.) ;
#67372 = ADVANCED_FACE('',(#20087),#7755,.T.) ;
#67373 = ADVANCED_FACE('',(#20088),#4766,.T.) ;
#67374 = ADVANCED_FACE('',(#20089),#7756,.T.) ;
#67375 = ADVANCED_FACE('',(#20090),#7757,.T.) ;
#67376 = ADVANCED_FACE('',(#20091),#63405,.T.) ;
#67377 = ADVANCED_FACE('',(#20092),#7758,.T.) ;
#67378 = ADVANCED_FACE('',(#20093),#4767,.T.) ;
#67379 = ADVANCED_FACE('',(#20094),#7759,.T.) ;
#67380 = ADVANCED_FACE('',(#20095),#4768,.T.) ;
#67381 = ADVANCED_FACE('',(#20096),#7760,.T.) ;
#67382 = ADVANCED_FACE('',(#20097),#63406,.T.) ;
#67383 = ADVANCED_FACE('',(#20098),#63407,.T.) ;
#67384 = ADVANCED_FACE('',(#20099),#7761,.T.) ;
#67385 = ADVANCED_FACE('',(#20100),#4769,.T.) ;
#67386 = ADVANCED_FACE('',(#20101),#7762,.T.) ;
#67387 = ADVANCED_FACE('',(#20102),#4770,.T.) ;
#67388 = ADVANCED_FACE('',(#20103),#7763,.T.) ;
#67389 = ADVANCED_FACE('',(#20104),#63408,.T.) ;
#67390 = ADVANCED_FACE('',(#20105),#7764,.T.) ;
#67391 = ADVANCED_FACE('',(#20106),#4771,.T.) ;
#67392 = ADVANCED_FACE('',(#20107),#7765,.T.) ;
#67393 = ADVANCED_FACE('',(#20108),#4772,.T.) ;
#67394 = ADVANCED_FACE('',(#20109),#7766,.T.) ;
#67395 = ADVANCED_FACE('',(#20110),#7767,.T.) ;
#67396 = ADVANCED_FACE('',(#20111),#4773,.T.) ;
#67397 = ADVANCED_FACE('',(#20112),#7768,.T.) ;
#67398 = ADVANCED_FACE('',(#20113),#7769,.T.) ;
#67399 = ADVANCED_FACE('',(#20114),#4774,.T.) ;
#67400 = ADVANCED_FACE('',(#20115),#63409,.T.) ;
#67401 = ADVANCED_FACE('',(#20116),#7770,.T.) ;
#67402 = ADVANCED_FACE('',(#20117),#4775,.T.) ;
#67403 = ADVANCED_FACE('',(#20118),#7771,.T.) ;
#67404 = ADVANCED_FACE('',(#20119),#4776,.T.) ;
#67405 = ADVANCED_FACE('',(#20120),#7772,.T.) ;
#67406 = ADVANCED_FACE('',(#20121),#63410,.T.) ;
#67407 = ADVANCED_FACE('',(#20122),#63411,.T.) ;
#67408 = ADVANCED_FACE('',(#20123),#7773,.T.) ;
#67409 = ADVANCED_FACE('',(#20124),#4777,.T.) ;
#67410 = ADVANCED_FACE('',(#20125),#7774,.T.) ;
#67411 = ADVANCED_FACE('',(#20126),#4778,.T.) ;
#67412 = ADVANCED_FACE('',(#20127),#7775,.T.) ;
#67413 = ADVANCED_FACE('',(#20128),#63412,.T.) ;
#67414 = ADVANCED_FACE('',(#20129),#7776,.T.) ;
#67415 = ADVANCED_FACE('',(#20130),#4779,.T.) ;
#67416 = ADVANCED_FACE('',(#20131),#7777,.T.) ;
#67417 = ADVANCED_FACE('',(#20132),#4780,.T.) ;
#67418 = ADVANCED_FACE('',(#20133),#7778,.T.) ;
#67419 = ADVANCED_FACE('',(#20134),#7779,.T.) ;
#67420 = ADVANCED_FACE('',(#20135),#4781,.T.) ;
#67421 = ADVANCED_FACE('',(#20136),#7780,.T.) ;
#67422 = ADVANCED_FACE('',(#20137),#7781,.T.) ;
#67423 = ADVANCED_FACE('',(#20138),#4782,.T.) ;
#67424 = ADVANCED_FACE('',(#20139),#63413,.T.) ;
#67425 = ADVANCED_FACE('',(#20140),#7782,.T.) ;
#67426 = ADVANCED_FACE('',(#20141),#4783,.T.) ;
#67427 = ADVANCED_FACE('',(#20142),#7783,.T.) ;
#67428 = ADVANCED_FACE('',(#20143),#4784,.T.) ;
#67429 = ADVANCED_FACE('',(#20144),#7784,.T.) ;
#67430 = ADVANCED_FACE('',(#20145),#63414,.T.) ;
#67431 = ADVANCED_FACE('',(#20146),#63415,.T.) ;
#67432 = ADVANCED_FACE('',(#20147),#7785,.T.) ;
#67433 = ADVANCED_FACE('',(#20148),#4785,.T.) ;
#67434 = ADVANCED_FACE('',(#20149),#7786,.T.) ;
#67435 = ADVANCED_FACE('',(#20150),#4786,.T.) ;
#67436 = ADVANCED_FACE('',(#20151),#7787,.T.) ;
#67437 = ADVANCED_FACE('',(#20152),#63416,.T.) ;
#67438 = ADVANCED_FACE('',(#20153),#7788,.T.) ;
#67439 = ADVANCED_FACE('',(#20154),#4787,.T.) ;
#67440 = ADVANCED_FACE('',(#20155),#7789,.T.) ;
#67441 = ADVANCED_FACE('',(#20156),#4788,.T.) ;
#67442 = ADVANCED_FACE('',(#20157),#7790,.T.) ;
#67443 = ADVANCED_FACE('',(#20158),#7791,.T.) ;
#67444 = ADVANCED_FACE('',(#20159),#4789,.T.) ;
#67445 = ADVANCED_FACE('',(#20160),#7792,.T.) ;
#67446 = ADVANCED_FACE('',(#20161),#7793,.T.) ;
#67447 = ADVANCED_FACE('',(#20162),#4790,.T.) ;
#67448 = ADVANCED_FACE('',(#20163),#63417,.T.) ;
#67449 = ADVANCED_FACE('',(#20164),#7794,.T.) ;
#67450 = ADVANCED_FACE('',(#20165),#4791,.T.) ;
#67451 = ADVANCED_FACE('',(#20166),#7795,.T.) ;
#67452 = ADVANCED_FACE('',(#20167),#4792,.T.) ;
#67453 = ADVANCED_FACE('',(#20168),#7796,.T.) ;
#67454 = ADVANCED_FACE('',(#20169),#63418,.T.) ;
#67455 = ADVANCED_FACE('',(#20170),#63419,.T.) ;
#67456 = ADVANCED_FACE('',(#20171),#7797,.T.) ;
#67457 = ADVANCED_FACE('',(#20172),#4793,.T.) ;
#67458 = ADVANCED_FACE('',(#20173),#7798,.T.) ;
#67459 = ADVANCED_FACE('',(#20174),#4794,.T.) ;
#67460 = ADVANCED_FACE('',(#20175),#7799,.T.) ;
#67461 = ADVANCED_FACE('',(#20176),#63420,.T.) ;
#67462 = ADVANCED_FACE('',(#20177),#7800,.T.) ;
#67463 = ADVANCED_FACE('',(#20178),#4795,.T.) ;
#67464 = ADVANCED_FACE('',(#20179),#7801,.T.) ;
#67465 = ADVANCED_FACE('',(#20180),#4796,.T.) ;
#67466 = ADVANCED_FACE('',(#20181),#7802,.T.) ;
#67467 = ADVANCED_FACE('',(#20182),#7803,.T.) ;
#67468 = ADVANCED_FACE('',(#20183),#4797,.T.) ;
#67469 = ADVANCED_FACE('',(#20184),#7804,.T.) ;
#67470 = ADVANCED_FACE('',(#20185),#7805,.T.) ;
#67471 = ADVANCED_FACE('',(#20186),#4798,.T.) ;
#67472 = ADVANCED_FACE('',(#20187),#63421,.T.) ;
#67473 = ADVANCED_FACE('',(#20188),#7806,.T.) ;
#67474 = ADVANCED_FACE('',(#20189),#4799,.T.) ;
#67475 = ADVANCED_FACE('',(#20190),#7807,.T.) ;
#67476 = ADVANCED_FACE('',(#20191),#4800,.T.) ;
#67477 = ADVANCED_FACE('',(#20192),#7808,.T.) ;
#67478 = ADVANCED_FACE('',(#20193),#63422,.T.) ;
#67479 = ADVANCED_FACE('',(#20194),#63423,.T.) ;
#67480 = ADVANCED_FACE('',(#20195),#7809,.T.) ;
#67481 = ADVANCED_FACE('',(#20196),#4801,.T.) ;
#67482 = ADVANCED_FACE('',(#20197),#7810,.T.) ;
#67483 = ADVANCED_FACE('',(#20198),#4802,.T.) ;
#67484 = ADVANCED_FACE('',(#20199),#7811,.T.) ;
#67485 = ADVANCED_FACE('',(#20200),#63424,.T.) ;
#67486 = ADVANCED_FACE('',(#20201),#7812,.T.) ;
#67487 = ADVANCED_FACE('',(#20202),#4803,.T.) ;
#67488 = ADVANCED_FACE('',(#20203),#7813,.T.) ;
#67489 = ADVANCED_FACE('',(#20204),#4804,.T.) ;
#67490 = ADVANCED_FACE('',(#20205),#7814,.T.) ;
#67491 = ADVANCED_FACE('',(#20206),#7815,.T.) ;
#67492 = ADVANCED_FACE('',(#20207),#4805,.T.) ;
#67493 = ADVANCED_FACE('',(#20208),#7816,.T.) ;
#67494 = ADVANCED_FACE('',(#20209),#7817,.T.) ;
#67495 = ADVANCED_FACE('',(#20210),#4806,.T.) ;
#67496 = ADVANCED_FACE('',(#20211),#63425,.T.) ;
#67497 = ADVANCED_FACE('',(#20212),#7818,.T.) ;
#67498 = ADVANCED_FACE('',(#20213),#4807,.T.) ;
#67499 = ADVANCED_FACE('',(#20214),#7819,.T.) ;
#67500 = ADVANCED_FACE('',(#20215),#4808,.T.) ;
#67501 = ADVANCED_FACE('',(#20216),#7820,.T.) ;
#67502 = ADVANCED_FACE('',(#20217),#63426,.T.) ;
#67503 = ADVANCED_FACE('',(#20218),#63427,.T.) ;
#67504 = ADVANCED_FACE('',(#20219),#7821,.T.) ;
#67505 = ADVANCED_FACE('',(#20220),#4809,.T.) ;
#67506 = ADVANCED_FACE('',(#20221),#7822,.T.) ;
#67507 = ADVANCED_FACE('',(#20222),#4810,.T.) ;
#67508 = ADVANCED_FACE('',(#20223),#7823,.T.) ;
#67509 = ADVANCED_FACE('',(#20224),#63428,.T.) ;
#67510 = ADVANCED_FACE('',(#20225),#7824,.T.) ;
#67511 = ADVANCED_FACE('',(#20226),#4811,.T.) ;
#67512 = ADVANCED_FACE('',(#20227),#7825,.T.) ;
#67513 = ADVANCED_FACE('',(#20228),#4812,.T.) ;
#67514 = ADVANCED_FACE('',(#20229),#7826,.T.) ;
#67515 = ADVANCED_FACE('',(#20230),#7827,.T.) ;
#67516 = ADVANCED_FACE('',(#20231),#4813,.T.) ;
#67517 = ADVANCED_FACE('',(#20232),#7828,.T.) ;
#67518 = ADVANCED_FACE('',(#20233),#7829,.T.) ;
#67519 = ADVANCED_FACE('',(#20234),#4814,.T.) ;
#67520 = ADVANCED_FACE('',(#20235),#63429,.T.) ;
#67521 = ADVANCED_FACE('',(#20236),#7830,.T.) ;
#67522 = ADVANCED_FACE('',(#20237),#4815,.T.) ;
#67523 = ADVANCED_FACE('',(#20238),#7831,.T.) ;
#67524 = ADVANCED_FACE('',(#20239),#4816,.T.) ;
#67525 = ADVANCED_FACE('',(#20240),#7832,.T.) ;
#67526 = ADVANCED_FACE('',(#20241),#63430,.T.) ;
#67527 = ADVANCED_FACE('',(#20242),#63431,.T.) ;
#67528 = ADVANCED_FACE('',(#20243),#7833,.T.) ;
#67529 = ADVANCED_FACE('',(#20244),#4817,.T.) ;
#67530 = ADVANCED_FACE('',(#20245),#7834,.T.) ;
#67531 = ADVANCED_FACE('',(#20246),#4818,.T.) ;
#67532 = ADVANCED_FACE('',(#20247),#7835,.T.) ;
#67533 = ADVANCED_FACE('',(#20248),#63432,.T.) ;
#67534 = ADVANCED_FACE('',(#20249),#7836,.T.) ;
#67535 = ADVANCED_FACE('',(#20250),#4819,.T.) ;
#67536 = ADVANCED_FACE('',(#20251),#7837,.T.) ;
#67537 = ADVANCED_FACE('',(#20252),#4820,.T.) ;
#67538 = ADVANCED_FACE('',(#20253),#7838,.T.) ;
#67539 = ADVANCED_FACE('',(#20254),#7839,.T.) ;
#67540 = ADVANCED_FACE('',(#20255),#4821,.T.) ;
#67541 = ADVANCED_FACE('',(#20256),#7840,.T.) ;
#67542 = ADVANCED_FACE('',(#20257),#7841,.T.) ;
#67543 = ADVANCED_FACE('',(#20258),#4822,.T.) ;
#67544 = ADVANCED_FACE('',(#20259),#63433,.T.) ;
#67545 = ADVANCED_FACE('',(#20260),#7842,.T.) ;
#67546 = ADVANCED_FACE('',(#20261),#4823,.T.) ;
#67547 = ADVANCED_FACE('',(#20262),#7843,.T.) ;
#67548 = ADVANCED_FACE('',(#20263),#4824,.T.) ;
#67549 = ADVANCED_FACE('',(#20264),#7844,.T.) ;
#67550 = ADVANCED_FACE('',(#20265),#63434,.T.) ;
#67551 = ADVANCED_FACE('',(#20266),#63435,.T.) ;
#67552 = ADVANCED_FACE('',(#20267),#7845,.T.) ;
#67553 = ADVANCED_FACE('',(#20268),#4825,.T.) ;
#67554 = ADVANCED_FACE('',(#20269),#7846,.T.) ;
#67555 = ADVANCED_FACE('',(#20270),#4826,.T.) ;
#67556 = ADVANCED_FACE('',(#20271),#7847,.T.) ;
#67557 = ADVANCED_FACE('',(#20272),#63436,.T.) ;
#67558 = ADVANCED_FACE('',(#20273),#7848,.T.) ;
#67559 = ADVANCED_FACE('',(#20274),#4827,.T.) ;
#67560 = ADVANCED_FACE('',(#20275),#7849,.T.) ;
#67561 = ADVANCED_FACE('',(#20276),#4828,.T.) ;
#67562 = ADVANCED_FACE('',(#20277),#7850,.T.) ;
#67563 = ADVANCED_FACE('',(#20278),#7851,.T.) ;
#67564 = ADVANCED_FACE('',(#20279),#4829,.T.) ;
#67565 = ADVANCED_FACE('',(#20280),#7852,.T.) ;
#67566 = ADVANCED_FACE('',(#20281),#7853,.T.) ;
#67567 = ADVANCED_FACE('',(#20282),#4830,.T.) ;
#67568 = ADVANCED_FACE('',(#20283),#63437,.T.) ;
#67569 = ADVANCED_FACE('',(#20284),#7854,.T.) ;
#67570 = ADVANCED_FACE('',(#20285),#4831,.T.) ;
#67571 = ADVANCED_FACE('',(#20286),#7855,.T.) ;
#67572 = ADVANCED_FACE('',(#20287),#4832,.T.) ;
#67573 = ADVANCED_FACE('',(#20288),#7856,.T.) ;
#67574 = ADVANCED_FACE('',(#20289),#63438,.T.) ;
#67575 = ADVANCED_FACE('',(#20290),#63439,.T.) ;
#67576 = ADVANCED_FACE('',(#20291),#7857,.T.) ;
#67577 = ADVANCED_FACE('',(#20292),#4833,.T.) ;
#67578 = ADVANCED_FACE('',(#20293),#7858,.T.) ;
#67579 = ADVANCED_FACE('',(#20294),#4834,.T.) ;
#67580 = ADVANCED_FACE('',(#20295),#7859,.T.) ;
#67581 = ADVANCED_FACE('',(#20296),#63440,.T.) ;
#67582 = ADVANCED_FACE('',(#20297),#7860,.T.) ;
#67583 = ADVANCED_FACE('',(#20298),#4835,.T.) ;
#67584 = ADVANCED_FACE('',(#20299),#7861,.T.) ;
#67585 = ADVANCED_FACE('',(#20300),#4836,.T.) ;
#67586 = ADVANCED_FACE('',(#20301),#7862,.T.) ;
#67587 = ADVANCED_FACE('',(#20302),#7863,.T.) ;
#67588 = ADVANCED_FACE('',(#20303),#4837,.T.) ;
#67589 = ADVANCED_FACE('',(#20304),#7864,.T.) ;
#67590 = ADVANCED_FACE('',(#20305),#7865,.T.) ;
#67591 = ADVANCED_FACE('',(#20306),#4838,.T.) ;
#67592 = ADVANCED_FACE('',(#20307),#7866,.T.) ;
#67593 = ADVANCED_FACE('',(#20308),#7867,.T.) ;
#67594 = ADVANCED_FACE('',(#20309),#7868,.T.) ;
#67595 = ADVANCED_FACE('',(#20310),#7869,.T.) ;
#67596 = ADVANCED_FACE('',(#20311),#7870,.T.) ;
#67597 = ADVANCED_FACE('',(#20312),#7871,.T.) ;
#67598 = ADVANCED_FACE('',(#20313),#7872,.T.) ;
#67599 = ADVANCED_FACE('',(#20314),#7873,.T.) ;
#67600 = ADVANCED_FACE('',(#20315),#7874,.T.) ;
#67601 = ADVANCED_FACE('',(#20316),#7875,.T.) ;
#67602 = ADVANCED_FACE('',(#20317),#7876,.T.) ;
#67603 = ADVANCED_FACE('',(#20318),#7877,.T.) ;
#67604 = ADVANCED_FACE('',(#20319),#7878,.T.) ;
#67605 = ADVANCED_FACE('',(#20320),#7879,.T.) ;
#67606 = ADVANCED_FACE('',(#20321),#7880,.T.) ;
#67607 = ADVANCED_FACE('',(#20322),#7881,.T.) ;
#67608 = ADVANCED_FACE('',(#20323),#7882,.T.) ;
#67609 = ADVANCED_FACE('',(#20324),#7883,.T.) ;
#67610 = ADVANCED_FACE('',(#20325),#7884,.T.) ;
#67611 = ADVANCED_FACE('',(#20326),#7885,.T.) ;
#67612 = ADVANCED_FACE('',(#20327),#7886,.T.) ;
#67613 = ADVANCED_FACE('',(#20328),#16135,.F.) ;
#67614 = ADVANCED_FACE('',(#20329),#7887,.F.) ;
#67615 = ADVANCED_FACE('',(#20330),#16136,.F.) ;
#67616 = ADVANCED_FACE('',(#20331),#63441,.F.) ;
#67617 = ADVANCED_FACE('',(#20332),#16137,.T.) ;
#67618 = ADVANCED_FACE('',(#20333),#7888,.T.) ;
#67619 = ADVANCED_FACE('',(#20334),#7889,.T.) ;
#67620 = ADVANCED_FACE('',(#20335),#7890,.T.) ;
#67621 = ADVANCED_FACE('',(#20336),#7891,.T.) ;
#67622 = ADVANCED_FACE('',(#20337),#7892,.T.) ;
#67623 = ADVANCED_FACE('',(#20338),#7893,.T.) ;
#67624 = ADVANCED_FACE('',(#20339),#16138,.T.) ;
#67625 = ADVANCED_FACE('',(#20340),#16139,.T.) ;
#67626 = ADVANCED_FACE('',(#20341),#16140,.T.) ;
#67627 = ADVANCED_FACE('',(#20342),#16141,.T.) ;
#67628 = ADVANCED_FACE('',(#20343),#16142,.T.) ;
#67629 = ADVANCED_FACE('',(#20344),#16143,.T.) ;
#67630 = ADVANCED_FACE('',(#20345),#16144,.T.) ;
#67631 = ADVANCED_FACE('',(#20346),#16145,.T.) ;
#67632 = ADVANCED_FACE('',(#20347),#16146,.T.) ;
#67633 = ADVANCED_FACE('',(#20348),#16147,.T.) ;
#67634 = ADVANCED_FACE('',(#20349),#16148,.T.) ;
#67635 = ADVANCED_FACE('',(#20350),#16149,.T.) ;
#67636 = ADVANCED_FACE('',(#20351,#5061),#5913,.T.) ;
#67637 = ADVANCED_FACE('',(#20352,#5062),#5914,.F.) ;
#67638 = ADVANCED_FACE('',(#20353),#5915,.T.) ;
#67639 = ADVANCED_FACE('',(#20354),#5916,.T.) ;
#67640 = ADVANCED_FACE('',(#20355),#5917,.T.) ;
#67641 = ADVANCED_FACE('',(#20356),#5918,.T.) ;
#67642 = ADVANCED_FACE('',(#20357),#5919,.T.) ;
#67643 = ADVANCED_FACE('',(#20358),#5920,.T.) ;
#67644 = ADVANCED_FACE('',(#20359),#5921,.T.) ;
#67645 = ADVANCED_FACE('',(#20360),#467,.T.) ;
#67646 = ADVANCED_FACE('',(#20361),#468,.T.) ;
#67647 = ADVANCED_FACE('',(#20362),#5922,.F.) ;
#67648 = ADVANCED_FACE('',(#20363),#5923,.F.) ;
#67649 = ADVANCED_FACE('',(#20364),#5924,.F.) ;
#67650 = ADVANCED_FACE('',(#20365),#16150,.F.) ;
#67651 = ADVANCED_FACE('',(#20366),#16151,.F.) ;
#67652 = ADVANCED_FACE('',(#20367),#63442,.F.) ;
#67653 = ADVANCED_FACE('',(#20368),#63443,.T.) ;
#67654 = ADVANCED_FACE('',(#20369),#7894,.T.) ;
#67655 = ADVANCED_FACE('',(#20370),#7895,.T.) ;
#67656 = ADVANCED_FACE('',(#20371,#5063),#4839,.T.) ;
#67657 = ADVANCED_FACE('',(#20372),#5925,.T.) ;
#67658 = ADVANCED_FACE('',(#20373),#5926,.T.) ;
#67659 = ADVANCED_FACE('',(#20374),#5927,.T.) ;
#67660 = ADVANCED_FACE('',(#20375),#5928,.T.) ;
#67661 = ADVANCED_FACE('',(#20376),#5929,.F.) ;
#67662 = ADVANCED_FACE('',(#20377),#5930,.F.) ;
#67663 = ADVANCED_FACE('',(#20378),#5931,.T.) ;
#67664 = ADVANCED_FACE('',(#20379),#5932,.T.) ;
#67665 = ADVANCED_FACE('',(#20380),#5933,.T.) ;
#67666 = ADVANCED_FACE('',(#20381),#5934,.T.) ;
#67667 = ADVANCED_FACE('',(#20382),#5935,.T.) ;
#67668 = ADVANCED_FACE('',(#20383),#5936,.T.) ;
#67669 = ADVANCED_FACE('',(#20384),#5937,.T.) ;
#67670 = ADVANCED_FACE('',(#20385),#5938,.T.) ;
#67671 = ADVANCED_FACE('',(#20386),#5939,.T.) ;
#67672 = ADVANCED_FACE('',(#20387),#5940,.F.) ;
#67673 = ADVANCED_FACE('',(#20388),#5941,.F.) ;
#67674 = ADVANCED_FACE('',(#20389),#5942,.T.) ;
#67675 = ADVANCED_FACE('',(#20390),#5943,.T.) ;
#67676 = ADVANCED_FACE('',(#20391,#5064),#5944,.F.) ;
#67677 = ADVANCED_FACE('',(#20392),#5945,.T.) ;
#67678 = ADVANCED_FACE('',(#20393),#5946,.T.) ;
#67679 = ADVANCED_FACE('',(#20394),#16152,.F.) ;
#67680 = ADVANCED_FACE('',(#20395),#16153,.F.) ;
#67681 = ADVANCED_FACE('',(#20396),#16154,.F.) ;
#67682 = ADVANCED_FACE('',(#20397),#16155,.F.) ;
#67683 = ADVANCED_FACE('',(#20398),#16156,.F.) ;
#67684 = ADVANCED_FACE('',(#20399),#16157,.F.) ;
#67685 = ADVANCED_FACE('',(#20400),#16158,.F.) ;
#67686 = CLOSED_SHELL('',(#63444,#63445,#63446,#63447,#63448,#63449,#63450,
#63451,#63452,#63453,#63454,#63455,#63456,#63457,#63458,#63459,#63460,#63461,
#63462,#63463,#63464,#63465,#63466,#63467,#63468,#63469,#63470,#63471,#63472,
#63473,#63474,#63475,#63476,#63477,#63478,#63479,#63480,#63481,#63482,#63483,
#63484,#63485,#63486,#63487,#63488,#63489,#63490,#63491,#63492,#63493,#63494,
#63495,#63496,#63497,#63498,#63499,#63500,#63501,#63502,#63503,#63504,#63505,
#63506,#63507,#63508,#63509,#63510,#63511,#63512,#63513,#63514,#63515,#63516,
#63517,#63518,#63519,#63520,#63521,#63522,#63523,#63524,#63525,#63526,#63527,
#63528,#63529,#63530,#63531,#63532,#63533,#63534,#63535,#63536,#63537,#63538,
#63539,#63540,#63541,#63542,#63543,#63544,#63545,#63546,#63547,#63548,#63549,
#63550,#63551,#63552,#63553,#63554,#63555,#63556,#63557,#63558,#63559,#63560,
#63561,#63562,#63563,#63564,#63565,#63566,#63567,#63568,#63569,#63570,#63571,
#63572,#63573,#63574,#63575,#63576,#63577,#63578,#63579,#63580,#63581,#63582,
#63583,#63584,#63585,#63586,#63587,#63588,#63589,#63590,#63591,#63592,#63593,
#63594,#63595,#63596,#63597,#63598,#63599,#63600,#63601,#63602,#63603,#63604,
#63605,#63606,#63607,#63608,#63609,#63610,#63611,#63612,#63613,#63614,#63615,
#63616,#63617,#63618,#63619,#63620,#63621,#63622,#63623,#63624,#63625,#63626,
#63627,#63628,#63629,#63630,#63631,#63632,#63633,#63634,#63635,#63636,#63637,
#63638,#63639,#63640,#63641,#63642,#63643,#63644,#63645,#63646,#63647,#63648,
#63649,#63650,#63651,#63652,#63653,#63654,#63655,#63656,#63657,#63658,#63659,
#63660,#63661,#63662,#63663,#63664,#63665,#63666,#63667,#63668,#63669,#63670,
#63671,#63672,#63673,#63674,#63675,#63676,#63677,#63678,#63679,#63680,#63681,
#63682,#63683,#63684,#63685,#63686,#63687,#63688,#63689,#63690,#63691,#63692,
#63693,#63694,#63695,#63696,#63697,#63698,#63699,#63700,#63701,#63702,#63703,
#63704,#63705,#63706,#63707,#63708,#63709,#63710,#63711,#63712,#63713,#63714,
#63715,#63716,#63717,#63718,#63719,#63720,#63721,#63722,#63723,#63724,#63725,
#63726,#63727,#63728,#63729,#63730,#63731,#63732,#63733,#63734,#63735,#63736,
#63737,#63738,#63739,#63740,#63741,#63742,#63743,#63744,#63745,#63746,#63747,
#63748,#63749,#63750,#63751,#63752,#63753,#63754,#63755,#63756,#63757,#63758,
#63759,#63760,#63761,#63762,#63763,#63764,#63765,#63766,#63767,#63768,#63769,
#63770,#63771,#63772,#63773,#63774,#63775,#63776,#63777,#63778,#63779,#63780,
#63781,#63782,#63783,#63784,#63785,#63786,#63787,#63788,#63789,#63790,#63791,
#63792,#63793,#63794,#63795,#63796,#63797,#63798,#63799,#63800,#63801,#63802,
#63803,#63804,#63805,#63806,#63807,#63808,#63809,#63810,#63811,#63812,#63813,
#63814,#63815,#63816,#63817,#63818,#63819,#63820,#63821,#63822,#63823,#63824,
#63825,#63826,#63827,#63828,#63829,#63830,#63831,#63832,#63833,#63834,#63835,
#63836,#63837,#63838,#63839,#63840,#63841,#63842,#63843,#63844,#63845,#63846,
#63847,#63848,#63849,#63850,#63851,#63852,#63853,#63854,#63855,#63856,#63857,
#63858,#63859,#63860,#63861,#63862,#63863,#63864,#63865,#63866,#63867,#63868,
#63869,#63870,#63871,#63872,#63873,#63874,#63875,#63876,#63877,#63878,#63879,
#63880,#63881,#63882,#63883,#63884,#63885,#63886,#63887,#63888,#63889,#63890,
#63891,#63892,#63893,#63894)) ;
#67687 = CLOSED_SHELL('',(#63895,#63896,#63897,#63898,#63899,#63900,#63901,
#63902,#63903,#63904,#63905,#63906,#63907,#63908,#63909,#63910,#63911,#63912,
#63913,#63914,#63915,#63916,#63917,#63918,#63919,#63920,#63921,#63922,#63923,
#63924,#63925,#63926,#63927,#63928,#63929,#63930,#63931,#63932,#63933,#63934,
#63935,#63936,#63937,#63938,#63939,#63940,#63941,#63942,#63943,#63944,#63945,
#63946,#63947,#63948,#63949,#63950,#63951,#63952,#63953,#63954,#63955,#63956,
#63957,#63958,#63959,#63960,#63961,#63962,#63963,#63964,#63965,#63966,#63967,
#63968,#63969,#63970,#63971,#63972,#63973,#63974,#63975,#63976,#63977,#63978,
#63979,#63980,#63981,#63982,#63983,#63984,#63985,#63986,#63987,#63988,#63989,
#63990,#63991,#63992,#63993,#63994,#63995,#63996,#63997,#63998,#63999,#64000,
#64001,#64002,#64003,#64004,#64005,#64006,#64007,#64008,#64009,#64010,#64011,
#64012,#64013,#64014,#64015,#64016,#64017,#64018,#64019,#64020,#64021,#64022,
#64023,#64024,#64025,#64026,#64027,#64028,#64029,#64030,#64031,#64032,#64033,
#64034,#64035,#64036,#64037,#64038,#64039,#64040,#64041,#64042,#64043,#64044,
#64045,#64046,#64047,#64048,#64049,#64050,#64051,#64052,#64053,#64054,#64055,
#64056,#64057,#64058,#64059,#64060,#64061,#64062,#64063,#64064,#64065,#64066,
#64067,#64068,#64069,#64070,#64071,#64072,#64073,#64074,#64075,#64076,#64077,
#64078,#64079,#64080,#64081,#64082,#64083,#64084,#64085,#64086,#64087,#64088,
#64089,#64090,#64091,#64092,#64093,#64094,#64095,#64096,#64097,#64098,#64099,
#64100,#64101,#64102,#64103,#64104,#64105,#64106,#64107,#64108,#64109,#64110,
#64111,#64112,#64113,#64114,#64115,#64116,#64117,#64118,#64119,#64120,#64121,
#64122,#64123,#64124,#64125,#64126,#64127,#64128,#64129,#64130,#64131,#64132,
#64133,#64134,#64135,#64136,#64137,#64138,#64139,#64140,#64141,#64142,#64143,
#64144,#64145,#64146,#64147,#64148,#64149,#64150,#64151,#64152,#64153,#64154,
#64155,#64156,#64157,#64158,#64159,#64160,#64161,#64162,#64163,#64164,#64165,
#64166,#64167,#64168,#64169,#64170,#64171,#64172,#64173,#64174,#64175,#64176,
#64177,#64178,#64179,#64180,#64181,#64182,#64183)) ;
#67688 = CLOSED_SHELL('',(#64184,#64185,#64186,#64187,#64188,#64189,#64190,
#64191,#64192,#64193,#64194,#64195,#64196,#64197,#64198,#64199,#64200,#64201,
#64202,#64203,#64204,#64205,#64206,#64207,#64208,#64209,#64210,#64211,#64212,
#64213,#64214,#64215,#64216,#64217,#64218,#64219,#64220,#64221,#64222,#64223,
#64224,#64225,#64226,#64227,#64228,#64229,#64230,#64231,#64232,#64233,#64234,
#64235,#64236,#64237,#64238,#64239,#64240,#64241,#64242,#64243,#64244,#64245,
#64246,#64247,#64248,#64249,#64250,#64251,#64252,#64253,#64254,#64255,#64256,
#64257,#64258,#64259,#64260,#64261,#64262,#64263,#64264,#64265,#64266,#64267,
#64268,#64269,#64270,#64271,#64272,#64273,#64274,#64275,#64276,#64277,#64278,
#64279,#64280,#64281,#64282,#64283,#64284,#64285,#64286,#64287,#64288,#64289,
#64290,#64291,#64292,#64293,#64294,#64295,#64296,#64297,#64298,#64299,#64300,
#64301,#64302,#64303,#64304,#64305,#64306,#64307,#64308,#64309,#64310,#64311,
#64312,#64313,#64314,#64315,#64316,#64317,#64318,#64319,#64320,#64321,#64322,
#64323,#64324,#64325,#64326,#64327,#64328,#64329,#64330,#64331,#64332,#64333,
#64334,#64335,#64336,#64337,#64338,#64339,#64340,#64341,#64342,#64343,#64344,
#64345,#64346,#64347,#64348,#64349,#64350,#64351,#64352,#64353,#64354,#64355,
#64356,#64357,#64358,#64359,#64360,#64361,#64362,#64363,#64364,#64365,#64366,
#64367,#64368,#64369,#64370,#64371,#64372,#64373,#64374,#64375,#64376,#64377,
#64378,#64379,#64380,#64381,#64382,#64383,#64384,#64385,#64386,#64387,#64388,
#64389,#64390,#64391,#64392,#64393,#64394,#64395,#64396,#64397,#64398,#64399,
#64400,#64401,#64402,#64403,#64404,#64405,#64406,#64407,#64408,#64409,#64410,
#64411,#64412,#64413,#64414,#64415,#64416,#64417,#64418,#64419,#64420,#64421,
#64422,#64423,#64424,#64425,#64426,#64427,#64428,#64429,#64430,#64431,#64432,
#64433,#64434,#64435,#64436,#64437,#64438,#64439,#64440,#64441,#64442,#64443,
#64444,#64445,#64446,#64447,#64448,#64449,#64450,#64451,#64452,#64453,#64454,
#64455,#64456,#64457,#64458,#64459,#64460,#64461,#64462,#64463,#64464,#64465,
#64466,#64467,#64468,#64469,#64470,#64471,#64472)) ;
#67689 = CLOSED_SHELL('',(#64473,#64474,#64475,#64476,#64477,#64478,#64479,
#64480,#64481,#64482,#64483,#64484,#64485,#64486,#64487,#64488,#64489,#64490,
#64491,#64492,#64493,#64494,#64495,#64496,#64497,#64498,#64499,#64500,#64501,
#64502,#64503,#64504,#64505,#64506,#64507,#64508,#64509,#64510,#64511,#64512,
#64513,#64514,#64515,#64516,#64517,#64518,#64519,#64520,#64521,#64522,#64523,
#64524,#64525,#64526,#64527,#64528,#64529,#64530,#64531,#64532,#64533,#64534,
#64535,#64536,#64537,#64538,#64539,#64540,#64541,#64542,#64543,#64544,#64545,
#64546,#64547,#64548,#64549,#64550,#64551,#64552,#64553,#64554,#64555,#64556,
#64557,#64558,#64559,#64560,#64561,#64562,#64563,#64564,#64565,#64566,#64567,
#64568,#64569,#64570,#64571,#64572,#64573,#64574,#64575,#64576,#64577,#64578,
#64579,#64580,#64581,#64582,#64583,#64584,#64585,#64586,#64587,#64588,#64589,
#64590,#64591,#64592,#64593,#64594,#64595,#64596,#64597,#64598,#64599,#64600,
#64601,#64602,#64603,#64604,#64605,#64606,#64607,#64608,#64609,#64610,#64611,
#64612,#64613,#64614,#64615,#64616,#64617,#64618,#64619,#64620,#64621,#64622,
#64623,#64624,#64625,#64626,#64627,#64628,#64629,#64630,#64631,#64632,#64633,
#64634,#64635,#64636,#64637,#64638,#64639,#64640,#64641,#64642,#64643,#64644,
#64645,#64646,#64647,#64648,#64649,#64650,#64651,#64652,#64653,#64654,#64655,
#64656,#64657,#64658,#64659,#64660,#64661,#64662,#64663,#64664,#64665,#64666,
#64667,#64668,#64669,#64670,#64671,#64672,#64673,#64674,#64675,#64676,#64677,
#64678,#64679,#64680,#64681,#64682,#64683,#64684,#64685,#64686,#64687,#64688,
#64689,#64690,#64691,#64692,#64693,#64694,#64695,#64696,#64697,#64698,#64699,
#64700,#64701,#64702,#64703,#64704,#64705,#64706,#64707,#64708,#64709,#64710,
#64711,#64712,#64713,#64714,#64715,#64716,#64717,#64718,#64719,#64720,#64721,
#64722,#64723,#64724,#64725,#64726,#64727,#64728,#64729,#64730,#64731,#64732,
#64733,#64734,#64735,#64736,#64737,#64738,#64739,#64740,#64741,#64742,#64743,
#64744,#64745,#64746,#64747,#64748,#64749,#64750,#64751,#64752,#64753,#64754,
#64755,#64756,#64757,#64758,#64759,#64760,#64761)) ;
#67690 = CLOSED_SHELL('',(#64762,#64763,#64764,#64765,#64766,#64767,#64768,
#64769,#64770,#64771,#64772,#64773,#64774,#64775,#64776,#64777,#64778,#64779,
#64780,#64781,#64782,#64783,#64784,#64785,#64786,#64787,#64788,#64789,#64790,
#64791,#64792,#64793,#64794,#64795,#64796,#64797,#64798,#64799,#64800,#64801,
#64802,#64803,#64804,#64805,#64806,#64807,#64808,#64809,#64810,#64811,#64812,
#64813,#64814,#64815,#64816,#64817,#64818,#64819,#64820,#64821,#64822,#64823,
#64824,#64825,#64826,#64827,#64828,#64829,#64830,#64831,#64832,#64833,#64834,
#64835,#64836,#64837,#64838,#64839,#64840,#64841,#64842,#64843,#64844,#64845,
#64846,#64847,#64848,#64849,#64850,#64851,#64852,#64853,#64854,#64855,#64856,
#64857,#64858,#64859,#64860,#64861,#64862,#64863,#64864,#64865,#64866,#64867,
#64868,#64869,#64870,#64871,#64872,#64873,#64874,#64875,#64876,#64877,#64878,
#64879,#64880,#64881,#64882,#64883,#64884,#64885,#64886,#64887,#64888,#64889,
#64890,#64891,#64892,#64893,#64894,#64895,#64896,#64897,#64898,#64899,#64900,
#64901,#64902,#64903,#64904,#64905,#64906,#64907,#64908,#64909,#64910,#64911,
#64912,#64913,#64914,#64915,#64916,#64917,#64918,#64919,#64920,#64921,#64922,
#64923,#64924,#64925,#64926,#64927,#64928,#64929,#64930,#64931,#64932,#64933,
#64934,#64935,#64936,#64937,#64938,#64939,#64940,#64941,#64942,#64943,#64944,
#64945,#64946,#64947,#64948,#64949,#64950,#64951,#64952,#64953,#64954,#64955,
#64956,#64957,#64958,#64959,#64960,#64961,#64962,#64963,#64964,#64965,#64966,
#64967,#64968,#64969,#64970,#64971,#64972,#64973,#64974,#64975,#64976,#64977,
#64978,#64979,#64980,#64981,#64982,#64983,#64984,#64985,#64986,#64987,#64988,
#64989,#64990,#64991,#64992,#64993,#64994,#64995,#64996,#64997,#64998,#64999,
#65000,#65001,#65002,#65003,#65004,#65005,#65006,#65007,#65008,#65009,#65010,
#65011,#65012,#65013,#65014,#65015,#65016,#65017,#65018,#65019,#65020,#65021,
#65022,#65023,#65024,#65025,#65026,#65027,#65028,#65029,#65030,#65031,#65032,
#65033,#65034,#65035,#65036,#65037,#65038,#65039,#65040,#65041,#65042,#65043,
#65044,#65045,#65046,#65047,#65048,#65049,#65050)) ;
#67691 = CLOSED_SHELL('',(#65051,#65052,#65053,#65054,#65055,#65056,#65057,
#65058,#65059,#65060,#65061,#65062,#65063,#65064,#65065,#65066,#65067,#65068,
#65069,#65070,#65071,#65072,#65073,#65074,#65075,#65076,#65077,#65078,#65079,
#65080,#65081,#65082,#65083,#65084,#65085,#65086,#65087,#65088,#65089,#65090,
#65091,#65092,#65093,#65094,#65095,#65096,#65097,#65098,#65099,#65100,#65101,
#65102,#65103,#65104,#65105,#65106,#65107,#65108,#65109,#65110,#65111,#65112,
#65113,#65114,#65115,#65116,#65117,#65118,#65119,#65120,#65121,#65122,#65123,
#65124,#65125,#65126,#65127,#65128,#65129,#65130,#65131,#65132,#65133,#65134,
#65135,#65136,#65137,#65138,#65139,#65140,#65141,#65142,#65143,#65144,#65145,
#65146,#65147,#65148,#65149,#65150,#65151,#65152,#65153,#65154,#65155,#65156,
#65157,#65158,#65159,#65160,#65161,#65162,#65163,#65164,#65165,#65166,#65167,
#65168,#65169,#65170,#65171,#65172,#65173,#65174,#65175,#65176,#65177,#65178,
#65179,#65180,#65181,#65182,#65183,#65184,#65185,#65186,#65187,#65188,#65189,
#65190,#65191,#65192,#65193,#65194,#65195,#65196,#65197,#65198,#65199,#65200,
#65201,#65202,#65203,#65204,#65205,#65206,#65207,#65208,#65209,#65210,#65211,
#65212,#65213,#65214,#65215,#65216,#65217,#65218,#65219,#65220,#65221,#65222,
#65223,#65224,#65225,#65226,#65227,#65228,#65229,#65230,#65231,#65232,#65233,
#65234,#65235,#65236,#65237,#65238,#65239,#65240,#65241,#65242,#65243,#65244,
#65245,#65246,#65247,#65248,#65249,#65250,#65251,#65252,#65253,#65254,#65255,
#65256,#65257,#65258,#65259,#65260,#65261,#65262,#65263,#65264,#65265,#65266,
#65267,#65268,#65269,#65270,#65271,#65272,#65273,#65274,#65275,#65276,#65277,
#65278,#65279,#65280,#65281,#65282,#65283,#65284,#65285,#65286,#65287,#65288,
#65289,#65290,#65291,#65292,#65293,#65294,#65295,#65296,#65297,#65298,#65299,
#65300,#65301,#65302,#65303,#65304,#65305,#65306,#65307,#65308,#65309,#65310,
#65311,#65312,#65313,#65314,#65315,#65316,#65317,#65318,#65319,#65320,#65321,
#65322,#65323,#65324,#65325,#65326,#65327,#65328,#65329,#65330,#65331,#65332,
#65333,#65334,#65335,#65336,#65337,#65338,#65339)) ;
#67692 = CLOSED_SHELL('',(#65340,#65341,#65342,#65343,#65344,#65345,#65346,
#65347,#65348,#65349,#65350,#65351,#65352,#65353,#65354,#65355,#65356,#65357,
#65358,#65359,#65360,#65361)) ;
#67693 = CLOSED_SHELL('',(#65362,#65363,#65364,#65365,#65366,#65367,#65368,
#65369,#65370,#65371,#65372,#65373,#65374,#65375,#65376,#65377,#65378,#65379,
#65380,#65381,#65382,#65383,#65384,#65385,#65386,#65387,#65388,#65389,#65390,
#65391,#65392,#65393,#65394,#65395,#65396,#65397,#65398,#65399,#65400,#65401,
#65402,#65403,#65404,#65405,#65406,#65407,#65408,#65409,#65410,#65411,#65412,
#65413,#65414,#65415,#65416,#65417,#65418,#65419,#65420,#65421,#65422,#65423,
#65424,#65425,#65426,#65427,#65428,#65429,#65430,#65431,#65432,#65433,#65434,
#65435,#65436,#65437,#65438,#65439,#65440,#65441,#65442,#65443,#65444,#65445,
#65446,#65447,#65448,#65449,#65450,#65451,#65452,#65453,#65454,#65455,#65456,
#65457,#65458,#65459,#65460,#65461,#65462,#65463,#65464,#65465,#65466,#65467,
#65468,#65469,#65470,#65471,#65472,#65473,#65474,#65475,#65476,#65477,#65478,
#65479,#65480,#65481,#65482,#65483,#65484,#65485,#65486,#65487,#65488,#65489,
#65490,#65491,#65492,#65493,#65494,#65495,#65496,#65497,#65498,#65499,#65500,
#65501,#65502,#65503,#65504,#65505,#65506,#65507,#65508,#65509,#65510,#65511,
#65512,#65513,#65514,#65515,#65516,#65517,#65518,#65519,#65520,#65521,#65522,
#65523,#65524,#65525,#65526,#65527,#65528,#65529,#65530,#65531,#65532,#65533,
#65534,#65535,#65536,#65537,#65538,#65539,#65540,#65541,#65542,#65543,#65544,
#65545,#65546,#65547,#65548,#65549,#65550,#65551,#65552,#65553,#65554,#65555,
#65556,#65557,#65558,#65559,#65560,#65561,#65562,#65563,#65564,#65565,#65566,
#65567,#65568,#65569,#65570,#65571,#65572,#65573,#65574,#65575,#65576,#65577,
#65578,#65579,#65580,#65581,#65582,#65583,#65584,#65585,#65586,#65587,#65588,
#65589,#65590,#65591,#65592,#65593,#65594,#65595,#65596,#65597,#65598,#65599,
#65600,#65601,#65602,#65603,#65604,#65605,#65606,#65607,#65608,#65609,#65610,
#65611,#65612,#65613,#65614,#65615,#65616,#65617,#65618,#65619,#65620,#65621,
#65622,#65623,#65624,#65625,#65626,#65627,#65628,#65629,#65630,#65631,#65632,
#65633,#65634,#65635,#65636,#65637,#65638,#65639,#65640,#65641,#65642,#65643,
#65644,#65645,#65646,#65647,#65648,#65649,#65650,#65651,#65652,#65653,#65654,
#65655,#65656,#65657,#65658,#65659,#65660,#65661,#65662,#65663,#65664,#65665,
#65666,#65667,#65668,#65669,#65670,#65671,#65672,#65673,#65674,#65675,#65676,
#65677,#65678,#65679,#65680,#65681,#65682,#65683,#65684,#65685,#65686,#65687,
#65688,#65689,#65690,#65691,#65692,#65693,#65694,#65695,#65696,#65697,#65698,
#65699,#65700,#65701,#65702,#65703,#65704,#65705,#65706,#65707,#65708,#65709,
#65710,#65711,#65712,#65713,#65714,#65715,#65716,#65717,#65718,#65719,#65720,
#65721,#65722,#65723,#65724,#65725,#65726,#65727,#65728,#65729,#65730,#65731,
#65732,#65733,#65734,#65735,#65736,#65737,#65738,#65739,#65740,#65741,#65742,
#65743,#65744,#65745,#65746,#65747,#65748,#65749,#65750,#65751,#65752,#65753,
#65754,#65755,#65756,#65757,#65758,#65759,#65760,#65761,#65762,#65763,#65764,
#65765,#65766,#65767,#65768,#65769,#65770,#65771,#65772,#65773,#65774,#65775,
#65776,#65777,#65778,#65779,#65780,#65781,#65782,#65783,#65784,#65785,#65786,
#65787,#65788,#65789,#65790,#65791,#65792,#65793,#65794,#65795,#65796,#65797,
#65798,#65799,#65800,#65801,#65802,#65803,#65804,#65805,#65806,#65807,#65808,
#65809,#65810,#65811,#65812,#65813,#65814,#65815,#65816,#65817,#65818,#65819,
#65820,#65821,#65822,#65823,#65824,#65825,#65826,#65827,#65828,#65829,#65830,
#65831,#65832,#65833,#65834,#65835,#65836,#65837,#65838,#65839,#65840,#65841,
#65842,#65843,#65844,#65845,#65846,#65847,#65848,#65849,#65850,#65851,#65852,
#65853,#65854,#65855,#65856,#65857,#65858,#65859,#65860,#65861,#65862,#65863,
#65864,#65865,#65866,#65867,#65868,#65869,#65870,#65871,#65872,#65873,#65874,
#65875,#65876,#65877,#65878,#65879,#65880,#65881,#65882,#65883,#65884,#65885,
#65886,#65887,#65888,#65889,#65890,#65891,#65892,#65893,#65894,#65895,#65896,
#65897,#65898,#65899,#65900,#65901,#65902,#65903,#65904,#65905,#65906,#65907,
#65908,#65909,#65910,#65911,#65912,#65913,#65914,#65915,#65916,#65917,#65918,
#65919,#65920,#65921,#65922,#65923,#65924,#65925,#65926,#65927,#65928,#65929,
#65930,#65931,#65932,#65933,#65934,#65935,#65936,#65937,#65938,#65939,#65940,
#65941,#65942,#65943,#65944,#65945,#65946,#65947,#65948,#65949,#65950,#65951,
#65952,#65953,#65954,#65955,#65956,#65957,#65958,#65959,#65960,#65961,#65962,
#65963,#65964,#65965,#65966,#65967,#65968,#65969,#65970,#65971,#65972,#65973,
#65974,#65975,#65976,#65977,#65978,#65979,#65980,#65981,#65982,#65983,#65984,
#65985,#65986,#65987,#65988,#65989,#65990,#65991,#65992,#65993,#65994,#65995,
#65996,#65997,#65998,#65999,#66000,#66001,#66002,#66003,#66004,#66005,#66006,
#66007,#66008,#66009,#66010,#66011,#66012,#66013,#66014,#66015,#66016,#66017,
#66018,#66019,#66020,#66021,#66022,#66023,#66024,#66025,#66026,#66027,#66028,
#66029,#66030,#66031,#66032,#66033,#66034,#66035,#66036,#66037,#66038,#66039,
#66040,#66041,#66042,#66043,#66044,#66045,#66046,#66047,#66048,#66049,#66050,
#66051,#66052,#66053,#66054,#66055,#66056,#66057,#66058,#66059,#66060,#66061,
#66062,#66063,#66064,#66065,#66066,#66067,#66068,#66069,#66070,#66071,#66072,
#66073,#66074,#66075,#66076,#66077,#66078,#66079,#66080,#66081,#66082,#66083,
#66084,#66085,#66086,#66087,#66088,#66089,#66090,#66091,#66092,#66093,#66094,
#66095,#66096,#66097,#66098,#66099,#66100,#66101,#66102,#66103,#66104,#66105,
#66106,#66107,#66108,#66109,#66110,#66111,#66112,#66113,#66114,#66115,#66116,
#66117,#66118,#66119,#66120,#66121,#66122,#66123,#66124,#66125,#66126,#66127,
#66128,#66129,#66130,#66131,#66132,#66133,#66134,#66135,#66136,#66137,#66138,
#66139,#66140,#66141,#66142,#66143,#66144,#66145,#66146,#66147,#66148,#66149,
#66150,#66151,#66152,#66153,#66154,#66155,#66156,#66157,#66158,#66159,#66160,
#66161,#66162,#66163,#66164,#66165,#66166,#66167,#66168,#66169,#66170,#66171,
#66172,#66173,#66174,#66175,#66176,#66177,#66178,#66179,#66180,#66181,#66182,
#66183,#66184,#66185,#66186,#66187,#66188,#66189,#66190,#66191,#66192,#66193,
#66194,#66195,#66196,#66197,#66198,#66199,#66200,#66201,#66202,#66203,#66204,
#66205,#66206,#66207,#66208,#66209,#66210,#66211,#66212,#66213,#66214,#66215,
#66216,#66217,#66218,#66219,#66220,#66221,#66222,#66223,#66224,#66225,#66226,
#66227,#66228,#66229,#66230,#66231,#66232,#66233,#66234,#66235,#66236,#66237,
#66238,#66239,#66240,#66241,#66242,#66243,#66244,#66245,#66246,#66247,#66248,
#66249,#66250,#66251,#66252,#66253,#66254,#66255,#66256,#66257,#66258,#66259,
#66260,#66261,#66262,#66263,#66264,#66265,#66266,#66267,#66268,#66269,#66270,
#66271,#66272,#66273,#66274,#66275,#66276,#66277,#66278,#66279,#66280,#66281,
#66282,#66283,#66284,#66285,#66286,#66287,#66288,#66289,#66290,#66291,#66292,
#66293,#66294,#66295,#66296,#66297,#66298,#66299,#66300,#66301,#66302,#66303,
#66304,#66305,#66306,#66307,#66308,#66309,#66310,#66311,#66312,#66313,#66314,
#66315,#66316,#66317,#66318,#66319,#66320,#66321,#66322,#66323,#66324,#66325,
#66326,#66327,#66328,#66329,#66330,#66331,#66332,#66333,#66334,#66335,#66336,
#66337,#66338,#66339,#66340,#66341,#66342,#66343,#66344,#66345,#66346,#66347,
#66348,#66349,#66350,#66351,#66352,#66353,#66354,#66355,#66356,#66357,#66358,
#66359,#66360,#66361,#66362,#66363,#66364,#66365,#66366,#66367,#66368,#66369,
#66370,#66371,#66372,#66373,#66374,#66375,#66376,#66377,#66378,#66379,#66380,
#66381,#66382,#66383,#66384,#66385,#66386,#66387,#66388,#66389,#66390,#66391,
#66392,#66393,#66394,#66395,#66396,#66397,#66398,#66399,#66400,#66401,#66402,
#66403,#66404,#66405,#66406,#66407,#66408,#66409,#66410,#66411,#66412,#66413,
#66414,#66415,#66416,#66417,#66418,#66419,#66420,#66421,#66422,#66423,#66424,
#66425,#66426,#66427,#66428,#66429,#66430,#66431,#66432,#66433,#66434,#66435,
#66436,#66437,#66438,#66439,#66440,#66441,#66442,#66443,#66444,#66445,#66446,
#66447,#66448,#66449,#66450,#66451,#66452,#66453,#66454,#66455,#66456,#66457,
#66458,#66459,#66460,#66461,#66462,#66463,#66464,#66465,#66466,#66467,#66468,
#66469,#66470,#66471,#66472,#66473,#66474,#66475,#66476,#66477,#66478,#66479,
#66480,#66481,#66482,#66483,#66484,#66485,#66486,#66487,#66488,#66489,#66490,
#66491,#66492,#66493,#66494,#66495,#66496,#66497,#66498,#66499,#66500,#66501,
#66502,#66503,#66504,#66505,#66506,#66507,#66508,#66509,#66510,#66511,#66512,
#66513,#66514,#66515,#66516,#66517,#66518,#66519,#66520,#66521,#66522,#66523,
#66524,#66525,#66526,#66527,#66528,#66529,#66530,#66531,#66532,#66533,#66534,
#66535,#66536,#66537,#66538,#66539,#66540,#66541,#66542,#66543,#66544,#66545,
#66546,#66547,#66548,#66549,#66550,#66551,#66552,#66553,#66554,#66555,#66556,
#66557,#66558,#66559,#66560,#66561,#66562,#66563,#66564,#66565,#66566,#66567,
#66568,#66569,#66570,#66571,#66572,#66573,#66574,#66575,#66576,#66577,#66578,
#66579,#66580,#66581,#66582,#66583,#66584,#66585,#66586,#66587,#66588,#66589,
#66590,#66591,#66592,#66593,#66594,#66595,#66596,#66597,#66598,#66599,#66600,
#66601,#66602,#66603,#66604,#66605,#66606,#66607,#66608,#66609,#66610,#66611,
#66612,#66613,#66614,#66615,#66616,#66617,#66618,#66619,#66620,#66621,#66622,
#66623,#66624,#66625,#66626,#66627,#66628,#66629,#66630,#66631,#66632,#66633,
#66634,#66635,#66636,#66637,#66638,#66639,#66640,#66641,#66642,#66643,#66644,
#66645,#66646,#66647,#66648,#66649,#66650,#66651,#66652,#66653,#66654,#66655,
#66656,#66657,#66658,#66659,#66660,#66661,#66662,#66663,#66664,#66665,#66666,
#66667,#66668,#66669,#66670,#66671,#66672,#66673,#66674,#66675,#66676,#66677,
#66678,#66679,#66680,#66681,#66682,#66683,#66684,#66685,#66686,#66687,#66688,
#66689,#66690,#66691,#66692,#66693,#66694,#66695,#66696,#66697,#66698,#66699,
#66700,#66701,#66702,#66703,#66704,#66705,#66706,#66707,#66708,#66709,#66710,
#66711,#66712,#66713,#66714,#66715,#66716,#66717,#66718,#66719,#66720,#66721,
#66722,#66723,#66724,#66725,#66726,#66727,#66728,#66729,#66730,#66731,#66732,
#66733,#66734,#66735,#66736,#66737,#66738,#66739,#66740,#66741,#66742,#66743,
#66744,#66745,#66746,#66747,#66748,#66749,#66750,#66751,#66752,#66753,#66754,
#66755,#66756,#66757,#66758,#66759,#66760,#66761,#66762,#66763,#66764,#66765,
#66766,#66767,#66768,#66769,#66770,#66771,#66772,#66773,#66774,#66775,#66776,
#66777,#66778,#66779,#66780,#66781,#66782,#66783,#66784,#66785,#66786,#66787,
#66788,#66789,#66790,#66791,#66792,#66793,#66794,#66795,#66796,#66797,#66798,
#66799,#66800,#66801,#66802,#66803,#66804,#66805,#66806,#66807,#66808,#66809,
#66810,#66811,#66812,#66813,#66814,#66815,#66816,#66817,#66818,#66819,#66820,
#66821,#66822,#66823,#66824,#66825,#66826,#66827,#66828,#66829,#66830,#66831,
#66832,#66833,#66834,#66835,#66836,#66837,#66838,#66839,#66840,#66841,#66842,
#66843,#66844,#66845,#66846,#66847,#66848,#66849,#66850,#66851,#66852,#66853,
#66854,#66855,#66856,#66857,#66858,#66859,#66860,#66861,#66862,#66863,#66864,
#66865,#66866,#66867,#66868,#66869,#66870,#66871,#66872,#66873,#66874,#66875,
#66876,#66877,#66878,#66879,#66880,#66881,#66882,#66883,#66884,#66885,#66886,
#66887,#66888,#66889,#66890,#66891,#66892,#66893,#66894,#66895,#66896,#66897,
#66898,#66899,#66900,#66901,#66902,#66903,#66904,#66905,#66906,#66907,#66908,
#66909,#66910,#66911,#66912,#66913,#66914,#66915,#66916,#66917,#66918,#66919,
#66920,#66921,#66922,#66923,#66924,#66925,#66926,#66927,#66928,#66929,#66930,
#66931,#66932,#66933,#66934,#66935,#66936,#66937,#66938,#66939,#66940,#66941,
#66942,#66943,#66944,#66945,#66946,#66947,#66948,#66949,#66950,#66951,#66952,
#66953,#66954,#66955,#66956,#66957,#66958,#66959,#66960,#66961,#66962,#66963,
#66964,#66965,#66966,#66967,#66968,#66969,#66970,#66971,#66972,#66973,#66974,
#66975,#66976,#66977,#66978,#66979,#66980,#66981,#66982,#66983,#66984,#66985,
#66986,#66987,#66988,#66989,#66990,#66991,#66992,#66993,#66994,#66995,#66996,
#66997,#66998,#66999,#67000,#67001,#67002,#67003,#67004,#67005,#67006,#67007,
#67008,#67009,#67010,#67011,#67012,#67013,#67014,#67015,#67016,#67017,#67018,
#67019,#67020,#67021,#67022,#67023,#67024,#67025,#67026,#67027,#67028,#67029,
#67030,#67031,#67032,#67033,#67034,#67035,#67036,#67037,#67038,#67039,#67040,
#67041,#67042,#67043,#67044,#67045,#67046,#67047,#67048,#67049,#67050,#67051,
#67052,#67053,#67054,#67055,#67056,#67057,#67058,#67059,#67060,#67061,#67062,
#67063,#67064,#67065,#67066,#67067,#67068,#67069,#67070,#67071,#67072,#67073,
#67074,#67075,#67076,#67077,#67078,#67079,#67080,#67081,#67082,#67083,#67084,
#67085,#67086,#67087,#67088,#67089,#67090,#67091,#67092,#67093,#67094,#67095,
#67096,#67097,#67098,#67099,#67100,#67101,#67102,#67103,#67104,#67105,#67106,
#67107,#67108,#67109,#67110,#67111,#67112,#67113,#67114,#67115,#67116,#67117,
#67118,#67119,#67120,#67121,#67122,#67123,#67124,#67125,#67126,#67127,#67128,
#67129,#67130,#67131,#67132,#67133,#67134,#67135,#67136,#67137,#67138,#67139,
#67140,#67141,#67142,#67143,#67144,#67145,#67146,#67147,#67148,#67149,#67150,
#67151,#67152,#67153,#67154,#67155,#67156,#67157,#67158,#67159,#67160,#67161,
#67162,#67163,#67164,#67165,#67166,#67167,#67168,#67169,#67170,#67171,#67172,
#67173,#67174,#67175,#67176,#67177,#67178,#67179,#67180,#67181,#67182,#67183,
#67184,#67185,#67186,#67187,#67188,#67189,#67190,#67191,#67192,#67193,#67194,
#67195,#67196,#67197,#67198,#67199,#67200,#67201,#67202,#67203,#67204,#67205,
#67206,#67207,#67208,#67209,#67210,#67211,#67212,#67213,#67214,#67215,#67216,
#67217,#67218,#67219,#67220,#67221,#67222,#67223,#67224,#67225,#67226,#67227,
#67228,#67229,#67230,#67231,#67232,#67233,#67234,#67235,#67236,#67237,#67238,
#67239,#67240,#67241,#67242,#67243,#67244,#67245,#67246,#67247,#67248,#67249,
#67250,#67251,#67252,#67253,#67254,#67255,#67256,#67257,#67258,#67259,#67260,
#67261,#67262,#67263,#67264,#67265,#67266,#67267,#67268,#67269,#67270,#67271,
#67272,#67273,#67274,#67275,#67276,#67277,#67278,#67279,#67280,#67281,#67282,
#67283,#67284,#67285,#67286,#67287,#67288,#67289,#67290,#67291,#67292,#67293,
#67294,#67295,#67296,#67297,#67298,#67299,#67300,#67301,#67302,#67303,#67304,
#67305,#67306,#67307,#67308,#67309,#67310,#67311,#67312,#67313,#67314,#67315,
#67316,#67317,#67318,#67319,#67320,#67321,#67322,#67323,#67324,#67325,#67326,
#67327,#67328,#67329,#67330,#67331,#67332,#67333,#67334,#67335,#67336,#67337,
#67338,#67339,#67340,#67341,#67342,#67343,#67344,#67345,#67346,#67347,#67348,
#67349,#67350,#67351,#67352,#67353,#67354,#67355,#67356,#67357,#67358,#67359,
#67360,#67361,#67362,#67363,#67364,#67365,#67366,#67367,#67368,#67369,#67370,
#67371,#67372,#67373,#67374,#67375,#67376,#67377,#67378,#67379,#67380,#67381,
#67382,#67383,#67384,#67385,#67386,#67387,#67388,#67389,#67390,#67391,#67392,
#67393,#67394,#67395,#67396,#67397,#67398,#67399,#67400,#67401,#67402,#67403,
#67404,#67405,#67406,#67407,#67408,#67409,#67410,#67411,#67412,#67413,#67414,
#67415,#67416,#67417,#67418,#67419,#67420,#67421,#67422,#67423,#67424,#67425,
#67426,#67427,#67428,#67429,#67430,#67431,#67432,#67433,#67434,#67435,#67436,
#67437,#67438,#67439,#67440,#67441,#67442,#67443,#67444,#67445,#67446,#67447,
#67448,#67449,#67450,#67451,#67452,#67453,#67454,#67455,#67456,#67457,#67458,
#67459,#67460,#67461,#67462,#67463,#67464,#67465,#67466,#67467,#67468,#67469,
#67470,#67471,#67472,#67473,#67474,#67475,#67476,#67477,#67478,#67479,#67480,
#67481,#67482,#67483,#67484,#67485,#67486,#67487,#67488,#67489,#67490,#67491,
#67492,#67493,#67494,#67495,#67496,#67497,#67498,#67499,#67500,#67501,#67502,
#67503,#67504,#67505,#67506,#67507,#67508,#67509,#67510,#67511,#67512,#67513,
#67514,#67515,#67516,#67517,#67518,#67519,#67520,#67521,#67522,#67523,#67524,
#67525,#67526,#67527,#67528,#67529,#67530,#67531,#67532,#67533,#67534,#67535,
#67536,#67537,#67538,#67539,#67540,#67541,#67542,#67543,#67544,#67545,#67546,
#67547,#67548,#67549,#67550,#67551,#67552,#67553,#67554,#67555,#67556,#67557,
#67558,#67559,#67560,#67561,#67562,#67563,#67564,#67565,#67566,#67567,#67568,
#67569,#67570,#67571,#67572,#67573,#67574,#67575,#67576,#67577,#67578,#67579,
#67580,#67581,#67582,#67583,#67584,#67585,#67586,#67587,#67588,#67589,#67590,
#67591)) ;
#67694 = CLOSED_SHELL('',(#67592,#67593,#67594,#67595,#67596,#67597,#67598,
#67599,#67600,#67601,#67602,#67603,#67604,#67605,#67606,#67607,#67608,#67609,
#67610,#67611,#67612,#67613,#67614,#67615,#67616,#67617,#67618,#67619,#67620,
#67621,#67622,#67623,#67624,#67625,#67626,#67627,#67628,#67629,#67630,#67631,
#67632,#67633,#67634,#67635,#67636,#67637,#67638,#67639,#67640,#67641,#67642,
#67643,#67644,#67645,#67646,#67647,#67648,#67649)) ;
#67695 = CLOSED_SHELL('',(#67650,#67651,#67652,#67653,#67654,#67655,#67656,
#67657,#67658,#67659,#67660,#67661,#67662,#67663,#67664,#67665,#67666,#67667,
#67668,#67669,#67670,#67671,#67672,#67673,#67674,#67675,#67676,#67677,#67678,
#67679,#67680,#67681,#67682,#67683,#67684,#67685)) ;
#67696 = DERIVED_UNIT_ELEMENT(#67708,1.) ;
#67697 = DERIVED_UNIT_ELEMENT(#126573,-3.) ;
#67698 = DERIVED_UNIT_ELEMENT(#67708,1.) ;
#67699 = DERIVED_UNIT_ELEMENT(#126573,-3.) ;
#67700 = DERIVED_UNIT_ELEMENT(#67708,1.) ;
#67701 = DERIVED_UNIT_ELEMENT(#126573,-3.) ;
#67702 = DERIVED_UNIT_ELEMENT(#67708,1.) ;
#67703 = DERIVED_UNIT_ELEMENT(#126573,-3.) ;
#67704 = DERIVED_UNIT_ELEMENT(#67708,1.) ;
#67705 = DERIVED_UNIT_ELEMENT(#126573,-3.) ;
#67706 = DERIVED_UNIT_ELEMENT(#67708,1.) ;
#67707 = DERIVED_UNIT_ELEMENT(#126573,-3.) ;
#67708 = (
MASS_UNIT()
NAMED_UNIT(*)
SI_UNIT(.KILO.,.GRAM.)
) ;
#67709 = DERIVED_UNIT((#67696,#67697)) ;
#67710 = DERIVED_UNIT((#67698,#67699)) ;
#67711 = DERIVED_UNIT((#67700,#67701)) ;
#67712 = DERIVED_UNIT((#67702,#67703)) ;
#67713 = DERIVED_UNIT((#67704,#67705)) ;
#67714 = DERIVED_UNIT((#67706,#67707)) ;
#67715 = MEASURE_REPRESENTATION_ITEM('density measure',
POSITIVE_RATIO_MEASURE(7850.),#67709) ;
#67716 = MEASURE_REPRESENTATION_ITEM('density measure',
POSITIVE_RATIO_MEASURE(7850.),#67710) ;
#67717 = MEASURE_REPRESENTATION_ITEM('density measure',
POSITIVE_RATIO_MEASURE(7850.),#67711) ;
#67718 = MEASURE_REPRESENTATION_ITEM('density measure',
POSITIVE_RATIO_MEASURE(7850.),#67712) ;
#67719 = MEASURE_REPRESENTATION_ITEM('density measure',
POSITIVE_RATIO_MEASURE(7850.),#67713) ;
#67720 = MEASURE_REPRESENTATION_ITEM('density measure',
POSITIVE_RATIO_MEASURE(7850.),#67714) ;
#67721 = PROPERTY_DEFINITION_REPRESENTATION(#67751,#67733) ;
#67722 = PROPERTY_DEFINITION_REPRESENTATION(#67752,#67734) ;
#67723 = PROPERTY_DEFINITION_REPRESENTATION(#67753,#67735) ;
#67724 = PROPERTY_DEFINITION_REPRESENTATION(#67754,#67736) ;
#67725 = PROPERTY_DEFINITION_REPRESENTATION(#67755,#67737) ;
#67726 = PROPERTY_DEFINITION_REPRESENTATION(#67756,#67738) ;
#67727 = PROPERTY_DEFINITION_REPRESENTATION(#67757,#67739) ;
#67728 = PROPERTY_DEFINITION_REPRESENTATION(#67758,#67740) ;
#67729 = PROPERTY_DEFINITION_REPRESENTATION(#67759,#67741) ;
#67730 = PROPERTY_DEFINITION_REPRESENTATION(#67760,#67742) ;
#67731 = PROPERTY_DEFINITION_REPRESENTATION(#67761,#67743) ;
#67732 = PROPERTY_DEFINITION_REPRESENTATION(#67762,#67744) ;
#67733 = REPRESENTATION('material name',(#67745),#126565) ;
#67734 = REPRESENTATION('density',(#67715),#126565) ;
#67735 = REPRESENTATION('material name',(#67746),#126566) ;
#67736 = REPRESENTATION('density',(#67716),#126566) ;
#67737 = REPRESENTATION('material name',(#67747),#126567) ;
#67738 = REPRESENTATION('density',(#67717),#126567) ;
#67739 = REPRESENTATION('material name',(#67748),#126568) ;
#67740 = REPRESENTATION('density',(#67718),#126568) ;
#67741 = REPRESENTATION('material name',(#67749),#126569) ;
#67742 = REPRESENTATION('density',(#67719),#126569) ;
#67743 = REPRESENTATION('material name',(#67750),#126570) ;
#67744 = REPRESENTATION('density',(#67720),#126570) ;
#67745 = DESCRIPTIVE_REPRESENTATION_ITEM('Steel','Steel') ;
#67746 = DESCRIPTIVE_REPRESENTATION_ITEM('Steel','Steel') ;
#67747 = DESCRIPTIVE_REPRESENTATION_ITEM('Steel','Steel') ;
#67748 = DESCRIPTIVE_REPRESENTATION_ITEM('Steel','Steel') ;
#67749 = DESCRIPTIVE_REPRESENTATION_ITEM('Steel','Steel') ;
#67750 = DESCRIPTIVE_REPRESENTATION_ITEM('Steel','Steel') ;
#67751 = PROPERTY_DEFINITION('material property','material name',#126607) ;
#67752 = PROPERTY_DEFINITION('material property','density of part',#126607) ;
#67753 = PROPERTY_DEFINITION('material property','material name',#126608) ;
#67754 = PROPERTY_DEFINITION('material property','density of part',#126608) ;
#67755 = PROPERTY_DEFINITION('material property','material name',#126609) ;
#67756 = PROPERTY_DEFINITION('material property','density of part',#126609) ;
#67757 = PROPERTY_DEFINITION('material property','material name',#126610) ;
#67758 = PROPERTY_DEFINITION('material property','density of part',#126610) ;
#67759 = PROPERTY_DEFINITION('material property','material name',#126611) ;
#67760 = PROPERTY_DEFINITION('material property','density of part',#126611) ;
#67761 = PROPERTY_DEFINITION('material property','material name',#126612) ;
#67762 = PROPERTY_DEFINITION('material property','density of part',#126612) ;
#67763 = AXIS2_PLACEMENT_3D('',#99146,#76852,#76853) ;
#67764 = AXIS2_PLACEMENT_3D('',#99147,#76854,#76855) ;
#67765 = AXIS2_PLACEMENT_3D('',#99148,#76856,#76857) ;
#67766 = AXIS2_PLACEMENT_3D('',#99151,#76858,#76859) ;
#67767 = AXIS2_PLACEMENT_3D('',#99152,#76860,#76861) ;
#67768 = AXIS2_PLACEMENT_3D('',#99154,#76862,#76863) ;
#67769 = AXIS2_PLACEMENT_3D('',#99155,#76864,#76865) ;
#67770 = AXIS2_PLACEMENT_3D('',#99156,#76866,#76867) ;
#67771 = AXIS2_PLACEMENT_3D('',#99158,#76868,#76869) ;
#67772 = AXIS2_PLACEMENT_3D('',#99160,#76870,#76871) ;
#67773 = AXIS2_PLACEMENT_3D('',#99162,#76872,#76873) ;
#67774 = AXIS2_PLACEMENT_3D('',#99163,#76874,#76875) ;
#67775 = AXIS2_PLACEMENT_3D('',#99164,#76876,#76877) ;
#67776 = AXIS2_PLACEMENT_3D('',#99167,#76878,#76879) ;
#67777 = AXIS2_PLACEMENT_3D('',#99168,#76880,#76881) ;
#67778 = AXIS2_PLACEMENT_3D('',#99170,#76882,#76883) ;
#67779 = AXIS2_PLACEMENT_3D('',#99172,#76884,#76885) ;
#67780 = AXIS2_PLACEMENT_3D('',#99173,#76886,#76887) ;
#67781 = AXIS2_PLACEMENT_3D('',#99174,#76888,#76889) ;
#67782 = AXIS2_PLACEMENT_3D('',#99176,#76890,#76891) ;
#67783 = AXIS2_PLACEMENT_3D('',#99178,#76892,#76893) ;
#67784 = AXIS2_PLACEMENT_3D('',#99179,#76894,#76895) ;
#67785 = AXIS2_PLACEMENT_3D('',#99180,#76896,#76897) ;
#67786 = AXIS2_PLACEMENT_3D('',#99183,#76898,#76899) ;
#67787 = AXIS2_PLACEMENT_3D('',#99184,#76900,#76901) ;
#67788 = AXIS2_PLACEMENT_3D('',#99186,#76902,#76903) ;
#67789 = AXIS2_PLACEMENT_3D('',#99188,#76904,#76905) ;
#67790 = AXIS2_PLACEMENT_3D('',#99189,#76906,#76907) ;
#67791 = AXIS2_PLACEMENT_3D('',#99190,#76908,#76909) ;
#67792 = AXIS2_PLACEMENT_3D('',#99192,#76910,#76911) ;
#67793 = AXIS2_PLACEMENT_3D('',#99194,#76912,#76913) ;
#67794 = AXIS2_PLACEMENT_3D('',#99195,#76914,#76915) ;
#67795 = AXIS2_PLACEMENT_3D('',#99196,#76916,#76917) ;
#67796 = AXIS2_PLACEMENT_3D('',#99199,#76919,#76920) ;
#67797 = AXIS2_PLACEMENT_3D('',#99200,#76921,#76922) ;
#67798 = AXIS2_PLACEMENT_3D('',#99202,#76924,#76925) ;
#67799 = AXIS2_PLACEMENT_3D('',#99205,#76927,#76928) ;
#67800 = AXIS2_PLACEMENT_3D('',#99206,#76929,#76930) ;
#67801 = AXIS2_PLACEMENT_3D('',#99208,#76932,#76933) ;
#67802 = AXIS2_PLACEMENT_3D('',#99210,#76935,#76936) ;
#67803 = AXIS2_PLACEMENT_3D('',#99225,#76943,#76944) ;
#67804 = AXIS2_PLACEMENT_3D('',#99229,#76946,#76947) ;
#67805 = AXIS2_PLACEMENT_3D('',#99233,#76949,#76950) ;
#67806 = AXIS2_PLACEMENT_3D('',#99237,#76952,#76953) ;
#67807 = AXIS2_PLACEMENT_3D('',#99239,#76955,#76956) ;
#67808 = AXIS2_PLACEMENT_3D('',#99254,#76963,#76964) ;
#67809 = AXIS2_PLACEMENT_3D('',#99258,#76966,#76967) ;
#67810 = AXIS2_PLACEMENT_3D('',#99262,#76969,#76970) ;
#67811 = AXIS2_PLACEMENT_3D('',#99266,#76972,#76973) ;
#67812 = AXIS2_PLACEMENT_3D('',#99268,#76975,#76976) ;
#67813 = AXIS2_PLACEMENT_3D('',#99271,#76977,#76978) ;
#67814 = AXIS2_PLACEMENT_3D('',#99285,#76985,#76986) ;
#67815 = AXIS2_PLACEMENT_3D('',#99293,#76990,#76991) ;
#67816 = AXIS2_PLACEMENT_3D('',#99297,#76993,#76994) ;
#67817 = AXIS2_PLACEMENT_3D('',#99301,#76996,#76997) ;
#67818 = AXIS2_PLACEMENT_3D('',#99305,#76999,#77000) ;
#67819 = AXIS2_PLACEMENT_3D('',#99309,#77002,#77003) ;
#67820 = AXIS2_PLACEMENT_3D('',#99313,#77005,#77006) ;
#67821 = AXIS2_PLACEMENT_3D('',#99317,#77008,#77009) ;
#67822 = AXIS2_PLACEMENT_3D('',#99321,#77011,#77012) ;
#67823 = AXIS2_PLACEMENT_3D('',#99325,#77014,#77015) ;
#67824 = AXIS2_PLACEMENT_3D('',#99329,#77017,#77018) ;
#67825 = AXIS2_PLACEMENT_3D('',#99333,#77020,#77021) ;
#67826 = AXIS2_PLACEMENT_3D('',#99337,#77023,#77024) ;
#67827 = AXIS2_PLACEMENT_3D('',#99341,#77026,#77027) ;
#67828 = AXIS2_PLACEMENT_3D('',#99345,#77029,#77030) ;
#67829 = AXIS2_PLACEMENT_3D('',#99349,#77032,#77033) ;
#67830 = AXIS2_PLACEMENT_3D('',#99353,#77035,#77036) ;
#67831 = AXIS2_PLACEMENT_3D('',#99355,#77038,#77039) ;
#67832 = AXIS2_PLACEMENT_3D('',#99362,#77042,#77043) ;
#67833 = AXIS2_PLACEMENT_3D('',#99370,#77047,#77048) ;
#67834 = AXIS2_PLACEMENT_3D('',#99380,#77053,#77054) ;
#67835 = AXIS2_PLACEMENT_3D('',#99384,#77056,#77057) ;
#67836 = AXIS2_PLACEMENT_3D('',#99388,#77059,#77060) ;
#67837 = AXIS2_PLACEMENT_3D('',#99392,#77062,#77063) ;
#67838 = AXIS2_PLACEMENT_3D('',#99396,#77065,#77066) ;
#67839 = AXIS2_PLACEMENT_3D('',#99400,#77068,#77069) ;
#67840 = AXIS2_PLACEMENT_3D('',#99404,#77071,#77072) ;
#67841 = AXIS2_PLACEMENT_3D('',#99408,#77074,#77075) ;
#67842 = AXIS2_PLACEMENT_3D('',#99412,#77077,#77078) ;
#67843 = AXIS2_PLACEMENT_3D('',#99416,#77080,#77081) ;
#67844 = AXIS2_PLACEMENT_3D('',#99420,#77083,#77084) ;
#67845 = AXIS2_PLACEMENT_3D('',#99424,#77086,#77087) ;
#67846 = AXIS2_PLACEMENT_3D('',#99428,#77089,#77090) ;
#67847 = AXIS2_PLACEMENT_3D('',#99432,#77092,#77093) ;
#67848 = AXIS2_PLACEMENT_3D('',#99436,#77095,#77096) ;
#67849 = AXIS2_PLACEMENT_3D('',#99440,#77098,#77099) ;
#67850 = AXIS2_PLACEMENT_3D('',#99442,#77101,#77102) ;
#67851 = AXIS2_PLACEMENT_3D('',#99449,#77105,#77106) ;
#67852 = AXIS2_PLACEMENT_3D('',#99457,#77110,#77111) ;
#67853 = AXIS2_PLACEMENT_3D('',#99467,#77116,#77117) ;
#67854 = AXIS2_PLACEMENT_3D('',#99471,#77119,#77120) ;
#67855 = AXIS2_PLACEMENT_3D('',#99475,#77122,#77123) ;
#67856 = AXIS2_PLACEMENT_3D('',#99479,#77125,#77126) ;
#67857 = AXIS2_PLACEMENT_3D('',#99483,#77128,#77129) ;
#67858 = AXIS2_PLACEMENT_3D('',#99487,#77131,#77132) ;
#67859 = AXIS2_PLACEMENT_3D('',#99491,#77134,#77135) ;
#67860 = AXIS2_PLACEMENT_3D('',#99495,#77137,#77138) ;
#67861 = AXIS2_PLACEMENT_3D('',#99499,#77140,#77141) ;
#67862 = AXIS2_PLACEMENT_3D('',#99503,#77143,#77144) ;
#67863 = AXIS2_PLACEMENT_3D('',#99507,#77146,#77147) ;
#67864 = AXIS2_PLACEMENT_3D('',#99511,#77149,#77150) ;
#67865 = AXIS2_PLACEMENT_3D('',#99515,#77152,#77153) ;
#67866 = AXIS2_PLACEMENT_3D('',#99519,#77155,#77156) ;
#67867 = AXIS2_PLACEMENT_3D('',#99523,#77158,#77159) ;
#67868 = AXIS2_PLACEMENT_3D('',#99527,#77161,#77162) ;
#67869 = AXIS2_PLACEMENT_3D('',#99531,#77164,#77165) ;
#67870 = AXIS2_PLACEMENT_3D('',#99535,#77167,#77168) ;
#67871 = AXIS2_PLACEMENT_3D('',#99539,#77170,#77171) ;
#67872 = AXIS2_PLACEMENT_3D('',#99543,#77173,#77174) ;
#67873 = AXIS2_PLACEMENT_3D('',#99547,#77176,#77177) ;
#67874 = AXIS2_PLACEMENT_3D('',#99551,#77179,#77180) ;
#67875 = AXIS2_PLACEMENT_3D('',#99555,#77182,#77183) ;
#67876 = AXIS2_PLACEMENT_3D('',#99559,#77185,#77186) ;
#67877 = AXIS2_PLACEMENT_3D('',#99563,#77188,#77189) ;
#67878 = AXIS2_PLACEMENT_3D('',#99567,#77191,#77192) ;
#67879 = AXIS2_PLACEMENT_3D('',#99571,#77194,#77195) ;
#67880 = AXIS2_PLACEMENT_3D('',#99575,#77197,#77198) ;
#67881 = AXIS2_PLACEMENT_3D('',#99577,#77200,#77201) ;
#67882 = AXIS2_PLACEMENT_3D('',#99580,#77202,#77203) ;
#67883 = AXIS2_PLACEMENT_3D('',#99594,#77210,#77211) ;
#67884 = AXIS2_PLACEMENT_3D('',#99602,#77215,#77216) ;
#67885 = AXIS2_PLACEMENT_3D('',#99606,#77218,#77219) ;
#67886 = AXIS2_PLACEMENT_3D('',#99610,#77221,#77222) ;
#67887 = AXIS2_PLACEMENT_3D('',#99614,#77224,#77225) ;
#67888 = AXIS2_PLACEMENT_3D('',#99618,#77227,#77228) ;
#67889 = AXIS2_PLACEMENT_3D('',#99622,#77230,#77231) ;
#67890 = AXIS2_PLACEMENT_3D('',#99626,#77233,#77234) ;
#67891 = AXIS2_PLACEMENT_3D('',#99630,#77236,#77237) ;
#67892 = AXIS2_PLACEMENT_3D('',#99634,#77239,#77240) ;
#67893 = AXIS2_PLACEMENT_3D('',#99638,#77242,#77243) ;
#67894 = AXIS2_PLACEMENT_3D('',#99642,#77245,#77246) ;
#67895 = AXIS2_PLACEMENT_3D('',#99646,#77248,#77249) ;
#67896 = AXIS2_PLACEMENT_3D('',#99650,#77251,#77252) ;
#67897 = AXIS2_PLACEMENT_3D('',#99654,#77254,#77255) ;
#67898 = AXIS2_PLACEMENT_3D('',#99658,#77257,#77258) ;
#67899 = AXIS2_PLACEMENT_3D('',#99662,#77260,#77261) ;
#67900 = AXIS2_PLACEMENT_3D('',#99666,#77263,#77264) ;
#67901 = AXIS2_PLACEMENT_3D('',#99670,#77266,#77267) ;
#67902 = AXIS2_PLACEMENT_3D('',#99674,#77269,#77270) ;
#67903 = AXIS2_PLACEMENT_3D('',#99678,#77272,#77273) ;
#67904 = AXIS2_PLACEMENT_3D('',#99682,#77275,#77276) ;
#67905 = AXIS2_PLACEMENT_3D('',#99686,#77278,#77279) ;
#67906 = AXIS2_PLACEMENT_3D('',#99690,#77281,#77282) ;
#67907 = AXIS2_PLACEMENT_3D('',#99694,#77284,#77285) ;
#67908 = AXIS2_PLACEMENT_3D('',#99698,#77287,#77288) ;
#67909 = AXIS2_PLACEMENT_3D('',#99702,#77290,#77291) ;
#67910 = AXIS2_PLACEMENT_3D('',#99706,#77293,#77294) ;
#67911 = AXIS2_PLACEMENT_3D('',#99710,#77296,#77297) ;
#67912 = AXIS2_PLACEMENT_3D('',#99712,#77299,#77300) ;
#67913 = AXIS2_PLACEMENT_3D('',#99715,#77301,#77302) ;
#67914 = AXIS2_PLACEMENT_3D('',#99727,#77308,#77309) ;
#67915 = AXIS2_PLACEMENT_3D('',#99733,#77313,#77314) ;
#67916 = AXIS2_PLACEMENT_3D('',#99740,#77317,#77318) ;
#67917 = AXIS2_PLACEMENT_3D('',#99748,#77322,#77323) ;
#67918 = AXIS2_PLACEMENT_3D('',#99754,#77327,#77328) ;
#67919 = AXIS2_PLACEMENT_3D('',#99763,#77333,#77334) ;
#67920 = AXIS2_PLACEMENT_3D('',#99772,#77339,#77340) ;
#67921 = AXIS2_PLACEMENT_3D('',#99781,#77345,#77346) ;
#67922 = AXIS2_PLACEMENT_3D('',#99790,#77351,#77352) ;
#67923 = AXIS2_PLACEMENT_3D('',#99799,#77357,#77358) ;
#67924 = AXIS2_PLACEMENT_3D('',#99801,#77359,#77360) ;
#67925 = AXIS2_PLACEMENT_3D('',#99804,#77362,#77363) ;
#67926 = AXIS2_PLACEMENT_3D('',#99805,#77364,#77365) ;
#67927 = AXIS2_PLACEMENT_3D('',#99806,#77366,#77367) ;
#67928 = AXIS2_PLACEMENT_3D('',#99808,#77369,#77370) ;
#67929 = AXIS2_PLACEMENT_3D('',#99810,#77372,#77373) ;
#67930 = AXIS2_PLACEMENT_3D('',#99811,#77374,#77375) ;
#67931 = AXIS2_PLACEMENT_3D('',#99812,#77376,#77377) ;
#67932 = AXIS2_PLACEMENT_3D('',#99813,#77378,#77379) ;
#67933 = AXIS2_PLACEMENT_3D('',#99814,#77380,#77381) ;
#67934 = AXIS2_PLACEMENT_3D('',#99823,#77386,#77387) ;
#67935 = AXIS2_PLACEMENT_3D('',#99832,#77392,#77393) ;
#67936 = AXIS2_PLACEMENT_3D('',#99841,#77398,#77399) ;
#67937 = AXIS2_PLACEMENT_3D('',#99850,#77404,#77405) ;
#67938 = AXIS2_PLACEMENT_3D('',#99859,#77410,#77411) ;
#67939 = AXIS2_PLACEMENT_3D('',#99868,#77416,#77417) ;
#67940 = AXIS2_PLACEMENT_3D('',#99874,#77421,#77422) ;
#67941 = AXIS2_PLACEMENT_3D('',#99876,#77424,#77425) ;
#67942 = AXIS2_PLACEMENT_3D('',#99885,#77430,#77431) ;
#67943 = AXIS2_PLACEMENT_3D('',#99894,#77436,#77437) ;
#67944 = AXIS2_PLACEMENT_3D('',#99903,#77442,#77443) ;
#67945 = AXIS2_PLACEMENT_3D('',#99906,#77446,#77447) ;
#67946 = AXIS2_PLACEMENT_3D('',#99909,#77450,#77451) ;
#67947 = AXIS2_PLACEMENT_3D('',#99910,#77452,#77453) ;
#67948 = AXIS2_PLACEMENT_3D('',#99912,#77455,#77456) ;
#67949 = AXIS2_PLACEMENT_3D('',#99913,#77457,#77458) ;
#67950 = AXIS2_PLACEMENT_3D('',#99914,#77459,#77460) ;
#67951 = AXIS2_PLACEMENT_3D('',#99915,#77461,#77462) ;
#67952 = AXIS2_PLACEMENT_3D('',#99916,#77463,#77464) ;
#67953 = AXIS2_PLACEMENT_3D('',#99917,#77465,#77466) ;
#67954 = AXIS2_PLACEMENT_3D('',#99918,#77467,#77468) ;
#67955 = AXIS2_PLACEMENT_3D('',#99922,#77470,#77471) ;
#67956 = AXIS2_PLACEMENT_3D('',#99923,#77472,#77473) ;
#67957 = AXIS2_PLACEMENT_3D('',#99924,#77474,#77475) ;
#67958 = AXIS2_PLACEMENT_3D('',#99925,#77476,#77477) ;
#67959 = AXIS2_PLACEMENT_3D('',#99927,#77479,#77480) ;
#67960 = AXIS2_PLACEMENT_3D('',#99928,#77481,#77482) ;
#67961 = AXIS2_PLACEMENT_3D('',#99929,#77483,#77484) ;
#67962 = AXIS2_PLACEMENT_3D('',#99930,#77485,#77486) ;
#67963 = AXIS2_PLACEMENT_3D('',#99931,#77487,#77488) ;
#67964 = AXIS2_PLACEMENT_3D('',#99932,#77489,#77490) ;
#67965 = AXIS2_PLACEMENT_3D('',#99941,#77495,#77496) ;
#67966 = AXIS2_PLACEMENT_3D('',#99950,#77501,#77502) ;
#67967 = AXIS2_PLACEMENT_3D('',#99959,#77507,#77508) ;
#67968 = AXIS2_PLACEMENT_3D('',#99968,#77513,#77514) ;
#67969 = AXIS2_PLACEMENT_3D('',#99977,#77519,#77520) ;
#67970 = AXIS2_PLACEMENT_3D('',#99986,#77525,#77526) ;
#67971 = AXIS2_PLACEMENT_3D('',#99988,#77528,#77529) ;
#67972 = AXIS2_PLACEMENT_3D('',#99994,#77533,#77534) ;
#67973 = AXIS2_PLACEMENT_3D('',#100003,#77539,#77540) ;
#67974 = AXIS2_PLACEMENT_3D('',#100012,#77545,#77546) ;
#67975 = AXIS2_PLACEMENT_3D('',#100021,#77551,#77552) ;
#67976 = AXIS2_PLACEMENT_3D('',#100030,#77557,#77558) ;
#67977 = AXIS2_PLACEMENT_3D('',#100039,#77563,#77564) ;
#67978 = AXIS2_PLACEMENT_3D('',#100048,#77569,#77570) ;
#67979 = AXIS2_PLACEMENT_3D('',#100057,#77575,#77576) ;
#67980 = AXIS2_PLACEMENT_3D('',#100066,#77581,#77582) ;
#67981 = AXIS2_PLACEMENT_3D('',#100075,#77587,#77588) ;
#67982 = AXIS2_PLACEMENT_3D('',#100084,#77593,#77594) ;
#67983 = AXIS2_PLACEMENT_3D('',#100093,#77599,#77600) ;
#67984 = AXIS2_PLACEMENT_3D('',#100102,#77605,#77606) ;
#67985 = AXIS2_PLACEMENT_3D('',#100111,#77611,#77612) ;
#67986 = AXIS2_PLACEMENT_3D('',#100120,#77617,#77618) ;
#67987 = AXIS2_PLACEMENT_3D('',#100129,#77623,#77624) ;
#67988 = AXIS2_PLACEMENT_3D('',#100138,#77629,#77630) ;
#67989 = AXIS2_PLACEMENT_3D('',#100147,#77635,#77636) ;
#67990 = AXIS2_PLACEMENT_3D('',#100156,#77641,#77642) ;
#67991 = AXIS2_PLACEMENT_3D('',#100165,#77647,#77648) ;
#67992 = AXIS2_PLACEMENT_3D('',#100174,#77653,#77654) ;
#67993 = AXIS2_PLACEMENT_3D('',#100183,#77659,#77660) ;
#67994 = AXIS2_PLACEMENT_3D('',#100192,#77665,#77666) ;
#67995 = AXIS2_PLACEMENT_3D('',#100201,#77671,#77672) ;
#67996 = AXIS2_PLACEMENT_3D('',#100210,#77677,#77678) ;
#67997 = AXIS2_PLACEMENT_3D('',#100219,#77683,#77684) ;
#67998 = AXIS2_PLACEMENT_3D('',#100228,#77689,#77690) ;
#67999 = AXIS2_PLACEMENT_3D('',#100237,#77695,#77696) ;
#68000 = AXIS2_PLACEMENT_3D('',#100246,#77701,#77702) ;
#68001 = AXIS2_PLACEMENT_3D('',#100255,#77707,#77708) ;
#68002 = AXIS2_PLACEMENT_3D('',#100264,#77713,#77714) ;
#68003 = AXIS2_PLACEMENT_3D('',#100273,#77719,#77720) ;
#68004 = AXIS2_PLACEMENT_3D('',#100282,#77725,#77726) ;
#68005 = AXIS2_PLACEMENT_3D('',#100291,#77731,#77732) ;
#68006 = AXIS2_PLACEMENT_3D('',#100300,#77737,#77738) ;
#68007 = AXIS2_PLACEMENT_3D('',#100309,#77743,#77744) ;
#68008 = AXIS2_PLACEMENT_3D('',#100318,#77749,#77750) ;
#68009 = AXIS2_PLACEMENT_3D('',#100327,#77755,#77756) ;
#68010 = AXIS2_PLACEMENT_3D('',#100336,#77761,#77762) ;
#68011 = AXIS2_PLACEMENT_3D('',#100345,#77767,#77768) ;
#68012 = AXIS2_PLACEMENT_3D('',#100354,#77773,#77774) ;
#68013 = AXIS2_PLACEMENT_3D('',#100363,#77779,#77780) ;
#68014 = AXIS2_PLACEMENT_3D('',#100372,#77785,#77786) ;
#68015 = AXIS2_PLACEMENT_3D('',#100381,#77791,#77792) ;
#68016 = AXIS2_PLACEMENT_3D('',#100390,#77797,#77798) ;
#68017 = AXIS2_PLACEMENT_3D('',#100399,#77803,#77804) ;
#68018 = AXIS2_PLACEMENT_3D('',#100408,#77809,#77810) ;
#68019 = AXIS2_PLACEMENT_3D('',#100417,#77815,#77816) ;
#68020 = AXIS2_PLACEMENT_3D('',#100426,#77821,#77822) ;
#68021 = AXIS2_PLACEMENT_3D('',#100427,#77823,#77824) ;
#68022 = AXIS2_PLACEMENT_3D('',#100428,#77825,#77826) ;
#68023 = AXIS2_PLACEMENT_3D('',#100429,#77827,#77828) ;
#68024 = AXIS2_PLACEMENT_3D('',#100430,#77829,#77830) ;
#68025 = AXIS2_PLACEMENT_3D('',#100431,#77831,#77832) ;
#68026 = AXIS2_PLACEMENT_3D('',#100432,#77833,#77834) ;
#68027 = AXIS2_PLACEMENT_3D('',#100433,#77835,#77836) ;
#68028 = AXIS2_PLACEMENT_3D('',#100434,#77837,#77838) ;
#68029 = AXIS2_PLACEMENT_3D('',#100435,#77839,#77840) ;
#68030 = AXIS2_PLACEMENT_3D('',#100436,#77841,#77842) ;
#68031 = AXIS2_PLACEMENT_3D('',#100437,#77843,#77844) ;
#68032 = AXIS2_PLACEMENT_3D('',#100438,#77845,#77846) ;
#68033 = AXIS2_PLACEMENT_3D('',#100439,#77847,#77848) ;
#68034 = AXIS2_PLACEMENT_3D('',#100440,#77849,#77850) ;
#68035 = AXIS2_PLACEMENT_3D('',#100441,#77851,#77852) ;
#68036 = AXIS2_PLACEMENT_3D('',#100442,#77853,#77854) ;
#68037 = AXIS2_PLACEMENT_3D('',#100443,#77855,#77856) ;
#68038 = AXIS2_PLACEMENT_3D('',#100444,#77857,#77858) ;
#68039 = AXIS2_PLACEMENT_3D('',#100445,#77859,#77860) ;
#68040 = AXIS2_PLACEMENT_3D('',#100446,#77861,#77862) ;
#68041 = AXIS2_PLACEMENT_3D('',#100447,#77863,#77864) ;
#68042 = AXIS2_PLACEMENT_3D('',#100448,#77865,#77866) ;
#68043 = AXIS2_PLACEMENT_3D('',#100449,#77867,#77868) ;
#68044 = AXIS2_PLACEMENT_3D('',#100450,#77869,#77870) ;
#68045 = AXIS2_PLACEMENT_3D('',#100451,#77871,#77872) ;
#68046 = AXIS2_PLACEMENT_3D('',#100452,#77873,#77874) ;
#68047 = AXIS2_PLACEMENT_3D('',#100453,#77875,#77876) ;
#68048 = AXIS2_PLACEMENT_3D('',#100454,#77877,#77878) ;
#68049 = AXIS2_PLACEMENT_3D('',#100455,#77879,#77880) ;
#68050 = AXIS2_PLACEMENT_3D('',#100456,#77881,#77882) ;
#68051 = AXIS2_PLACEMENT_3D('',#100457,#77883,#77884) ;
#68052 = AXIS2_PLACEMENT_3D('',#100458,#77885,#77886) ;
#68053 = AXIS2_PLACEMENT_3D('',#100459,#77887,#77888) ;
#68054 = AXIS2_PLACEMENT_3D('',#100460,#77889,#77890) ;
#68055 = AXIS2_PLACEMENT_3D('',#100461,#77891,#77892) ;
#68056 = AXIS2_PLACEMENT_3D('',#100462,#77893,#77894) ;
#68057 = AXIS2_PLACEMENT_3D('',#100463,#77895,#77896) ;
#68058 = AXIS2_PLACEMENT_3D('',#100464,#77897,#77898) ;
#68059 = AXIS2_PLACEMENT_3D('',#100465,#77899,#77900) ;
#68060 = AXIS2_PLACEMENT_3D('',#100466,#77901,#77902) ;
#68061 = AXIS2_PLACEMENT_3D('',#100467,#77903,#77904) ;
#68062 = AXIS2_PLACEMENT_3D('',#100468,#77905,#77906) ;
#68063 = AXIS2_PLACEMENT_3D('',#100469,#77907,#77908) ;
#68064 = AXIS2_PLACEMENT_3D('',#100470,#77909,#77910) ;
#68065 = AXIS2_PLACEMENT_3D('',#100471,#77911,#77912) ;
#68066 = AXIS2_PLACEMENT_3D('',#100472,#77913,#77914) ;
#68067 = AXIS2_PLACEMENT_3D('',#100473,#77915,#77916) ;
#68068 = AXIS2_PLACEMENT_3D('',#100474,#77917,#77918) ;
#68069 = AXIS2_PLACEMENT_3D('',#100475,#77919,#77920) ;
#68070 = AXIS2_PLACEMENT_3D('',#100476,#77921,#77922) ;
#68071 = AXIS2_PLACEMENT_3D('',#100477,#77923,#77924) ;
#68072 = AXIS2_PLACEMENT_3D('',#100478,#77925,#77926) ;
#68073 = AXIS2_PLACEMENT_3D('',#100479,#77927,#77928) ;
#68074 = AXIS2_PLACEMENT_3D('',#100480,#77929,#77930) ;
#68075 = AXIS2_PLACEMENT_3D('',#100481,#77931,#77932) ;
#68076 = AXIS2_PLACEMENT_3D('',#100482,#77933,#77934) ;
#68077 = AXIS2_PLACEMENT_3D('',#100483,#77935,#77936) ;
#68078 = AXIS2_PLACEMENT_3D('',#100484,#77937,#77938) ;
#68079 = AXIS2_PLACEMENT_3D('',#100485,#77939,#77940) ;
#68080 = AXIS2_PLACEMENT_3D('',#100486,#77941,#77942) ;
#68081 = AXIS2_PLACEMENT_3D('',#100487,#77943,#77944) ;
#68082 = AXIS2_PLACEMENT_3D('',#100488,#77945,#77946) ;
#68083 = AXIS2_PLACEMENT_3D('',#100489,#77947,#77948) ;
#68084 = AXIS2_PLACEMENT_3D('',#100490,#77949,#77950) ;
#68085 = AXIS2_PLACEMENT_3D('',#100491,#77951,#77952) ;
#68086 = AXIS2_PLACEMENT_3D('',#100492,#77953,#77954) ;
#68087 = AXIS2_PLACEMENT_3D('',#100493,#77955,#77956) ;
#68088 = AXIS2_PLACEMENT_3D('',#100494,#77957,#77958) ;
#68089 = AXIS2_PLACEMENT_3D('',#100495,#77959,#77960) ;
#68090 = AXIS2_PLACEMENT_3D('',#100496,#77961,#77962) ;
#68091 = AXIS2_PLACEMENT_3D('',#100497,#77963,#77964) ;
#68092 = AXIS2_PLACEMENT_3D('',#100498,#77965,#77966) ;
#68093 = AXIS2_PLACEMENT_3D('',#100499,#77967,#77968) ;
#68094 = AXIS2_PLACEMENT_3D('',#100500,#77969,#77970) ;
#68095 = AXIS2_PLACEMENT_3D('',#100501,#77971,#77972) ;
#68096 = AXIS2_PLACEMENT_3D('',#100502,#77973,#77974) ;
#68097 = AXIS2_PLACEMENT_3D('',#100503,#77975,#77976) ;
#68098 = AXIS2_PLACEMENT_3D('',#100504,#77977,#77978) ;
#68099 = AXIS2_PLACEMENT_3D('',#100505,#77979,#77980) ;
#68100 = AXIS2_PLACEMENT_3D('',#100506,#77981,#77982) ;
#68101 = AXIS2_PLACEMENT_3D('',#100507,#77983,#77984) ;
#68102 = AXIS2_PLACEMENT_3D('',#100508,#77985,#77986) ;
#68103 = AXIS2_PLACEMENT_3D('',#100509,#77987,#77988) ;
#68104 = AXIS2_PLACEMENT_3D('',#100510,#77989,#77990) ;
#68105 = AXIS2_PLACEMENT_3D('',#100511,#77991,#77992) ;
#68106 = AXIS2_PLACEMENT_3D('',#100512,#77993,#77994) ;
#68107 = AXIS2_PLACEMENT_3D('',#100513,#77995,#77996) ;
#68108 = AXIS2_PLACEMENT_3D('',#100514,#77997,#77998) ;
#68109 = AXIS2_PLACEMENT_3D('',#100515,#77999,#78000) ;
#68110 = AXIS2_PLACEMENT_3D('',#100516,#78001,#78002) ;
#68111 = AXIS2_PLACEMENT_3D('',#100517,#78003,#78004) ;
#68112 = AXIS2_PLACEMENT_3D('',#100518,#78005,#78006) ;
#68113 = AXIS2_PLACEMENT_3D('',#100519,#78007,#78008) ;
#68114 = AXIS2_PLACEMENT_3D('',#100520,#78009,#78010) ;
#68115 = AXIS2_PLACEMENT_3D('',#100521,#78011,#78012) ;
#68116 = AXIS2_PLACEMENT_3D('',#100522,#78013,#78014) ;
#68117 = AXIS2_PLACEMENT_3D('',#100523,#78015,#78016) ;
#68118 = AXIS2_PLACEMENT_3D('',#100524,#78017,#78018) ;
#68119 = AXIS2_PLACEMENT_3D('',#100525,#78019,#78020) ;
#68120 = AXIS2_PLACEMENT_3D('',#100526,#78021,#78022) ;
#68121 = AXIS2_PLACEMENT_3D('',#100527,#78023,#78024) ;
#68122 = AXIS2_PLACEMENT_3D('',#100528,#78025,#78026) ;
#68123 = AXIS2_PLACEMENT_3D('',#100529,#78027,#78028) ;
#68124 = AXIS2_PLACEMENT_3D('',#100530,#78029,#78030) ;
#68125 = AXIS2_PLACEMENT_3D('',#100531,#78031,#78032) ;
#68126 = AXIS2_PLACEMENT_3D('',#100532,#78033,#78034) ;
#68127 = AXIS2_PLACEMENT_3D('',#100533,#78035,#78036) ;
#68128 = AXIS2_PLACEMENT_3D('',#100534,#78037,#78038) ;
#68129 = AXIS2_PLACEMENT_3D('',#100535,#78039,#78040) ;
#68130 = AXIS2_PLACEMENT_3D('',#100536,#78041,#78042) ;
#68131 = AXIS2_PLACEMENT_3D('',#100537,#78043,#78044) ;
#68132 = AXIS2_PLACEMENT_3D('',#100538,#78045,#78046) ;
#68133 = AXIS2_PLACEMENT_3D('',#100539,#78047,#78048) ;
#68134 = AXIS2_PLACEMENT_3D('',#100540,#78049,#78050) ;
#68135 = AXIS2_PLACEMENT_3D('',#100541,#78051,#78052) ;
#68136 = AXIS2_PLACEMENT_3D('',#100542,#78053,#78054) ;
#68137 = AXIS2_PLACEMENT_3D('',#100543,#78055,#78056) ;
#68138 = AXIS2_PLACEMENT_3D('',#100544,#78057,#78058) ;
#68139 = AXIS2_PLACEMENT_3D('',#100545,#78059,#78060) ;
#68140 = AXIS2_PLACEMENT_3D('',#100546,#78061,#78062) ;
#68141 = AXIS2_PLACEMENT_3D('',#100547,#78063,#78064) ;
#68142 = AXIS2_PLACEMENT_3D('',#100548,#78065,#78066) ;
#68143 = AXIS2_PLACEMENT_3D('',#100549,#78067,#78068) ;
#68144 = AXIS2_PLACEMENT_3D('',#100550,#78069,#78070) ;
#68145 = AXIS2_PLACEMENT_3D('',#100551,#78071,#78072) ;
#68146 = AXIS2_PLACEMENT_3D('',#100552,#78073,#78074) ;
#68147 = AXIS2_PLACEMENT_3D('',#100553,#78075,#78076) ;
#68148 = AXIS2_PLACEMENT_3D('',#100554,#78077,#78078) ;
#68149 = AXIS2_PLACEMENT_3D('',#100555,#78079,#78080) ;
#68150 = AXIS2_PLACEMENT_3D('',#100556,#78081,#78082) ;
#68151 = AXIS2_PLACEMENT_3D('',#100557,#78083,#78084) ;
#68152 = AXIS2_PLACEMENT_3D('',#100558,#78085,#78086) ;
#68153 = AXIS2_PLACEMENT_3D('',#100559,#78087,#78088) ;
#68154 = AXIS2_PLACEMENT_3D('',#100560,#78089,#78090) ;
#68155 = AXIS2_PLACEMENT_3D('',#100561,#78091,#78092) ;
#68156 = AXIS2_PLACEMENT_3D('',#100562,#78093,#78094) ;
#68157 = AXIS2_PLACEMENT_3D('',#100563,#78095,#78096) ;
#68158 = AXIS2_PLACEMENT_3D('',#100564,#78097,#78098) ;
#68159 = AXIS2_PLACEMENT_3D('',#100565,#78099,#78100) ;
#68160 = AXIS2_PLACEMENT_3D('',#100566,#78101,#78102) ;
#68161 = AXIS2_PLACEMENT_3D('',#100567,#78103,#78104) ;
#68162 = AXIS2_PLACEMENT_3D('',#100568,#78105,#78106) ;
#68163 = AXIS2_PLACEMENT_3D('',#100569,#78107,#78108) ;
#68164 = AXIS2_PLACEMENT_3D('',#100570,#78109,#78110) ;
#68165 = AXIS2_PLACEMENT_3D('',#100571,#78111,#78112) ;
#68166 = AXIS2_PLACEMENT_3D('',#100572,#78113,#78114) ;
#68167 = AXIS2_PLACEMENT_3D('',#100573,#78115,#78116) ;
#68168 = AXIS2_PLACEMENT_3D('',#100574,#78117,#78118) ;
#68169 = AXIS2_PLACEMENT_3D('',#100575,#78119,#78120) ;
#68170 = AXIS2_PLACEMENT_3D('',#100576,#78121,#78122) ;
#68171 = AXIS2_PLACEMENT_3D('',#100577,#78123,#78124) ;
#68172 = AXIS2_PLACEMENT_3D('',#100578,#78125,#78126) ;
#68173 = AXIS2_PLACEMENT_3D('',#100579,#78127,#78128) ;
#68174 = AXIS2_PLACEMENT_3D('',#100580,#78129,#78130) ;
#68175 = AXIS2_PLACEMENT_3D('',#100581,#78131,#78132) ;
#68176 = AXIS2_PLACEMENT_3D('',#100582,#78133,#78134) ;
#68177 = AXIS2_PLACEMENT_3D('',#100583,#78135,#78136) ;
#68178 = AXIS2_PLACEMENT_3D('',#100584,#78137,#78138) ;
#68179 = AXIS2_PLACEMENT_3D('',#100585,#78139,#78140) ;
#68180 = AXIS2_PLACEMENT_3D('',#100586,#78141,#78142) ;
#68181 = AXIS2_PLACEMENT_3D('',#100587,#78143,#78144) ;
#68182 = AXIS2_PLACEMENT_3D('',#100588,#78145,#78146) ;
#68183 = AXIS2_PLACEMENT_3D('',#100589,#78147,#78148) ;
#68184 = AXIS2_PLACEMENT_3D('',#100590,#78149,#78150) ;
#68185 = AXIS2_PLACEMENT_3D('',#100591,#78151,#78152) ;
#68186 = AXIS2_PLACEMENT_3D('',#100592,#78153,#78154) ;
#68187 = AXIS2_PLACEMENT_3D('',#100593,#78155,#78156) ;
#68188 = AXIS2_PLACEMENT_3D('',#100594,#78157,#78158) ;
#68189 = AXIS2_PLACEMENT_3D('',#100595,#78159,#78160) ;
#68190 = AXIS2_PLACEMENT_3D('',#100596,#78161,#78162) ;
#68191 = AXIS2_PLACEMENT_3D('',#100597,#78163,#78164) ;
#68192 = AXIS2_PLACEMENT_3D('',#100598,#78165,#78166) ;
#68193 = AXIS2_PLACEMENT_3D('',#100599,#78167,#78168) ;
#68194 = AXIS2_PLACEMENT_3D('',#100600,#78169,#78170) ;
#68195 = AXIS2_PLACEMENT_3D('',#100601,#78171,#78172) ;
#68196 = AXIS2_PLACEMENT_3D('',#100602,#78173,#78174) ;
#68197 = AXIS2_PLACEMENT_3D('',#100603,#78175,#78176) ;
#68198 = AXIS2_PLACEMENT_3D('',#100604,#78177,#78178) ;
#68199 = AXIS2_PLACEMENT_3D('',#100605,#78179,#78180) ;
#68200 = AXIS2_PLACEMENT_3D('',#100606,#78181,#78182) ;
#68201 = AXIS2_PLACEMENT_3D('',#100607,#78183,#78184) ;
#68202 = AXIS2_PLACEMENT_3D('',#100608,#78185,#78186) ;
#68203 = AXIS2_PLACEMENT_3D('',#100609,#78187,#78188) ;
#68204 = AXIS2_PLACEMENT_3D('',#100610,#78189,#78190) ;
#68205 = AXIS2_PLACEMENT_3D('',#100611,#78191,#78192) ;
#68206 = AXIS2_PLACEMENT_3D('',#100612,#78193,#78194) ;
#68207 = AXIS2_PLACEMENT_3D('',#100613,#78195,#78196) ;
#68208 = AXIS2_PLACEMENT_3D('',#100614,#78197,#78198) ;
#68209 = AXIS2_PLACEMENT_3D('',#100615,#78199,#78200) ;
#68210 = AXIS2_PLACEMENT_3D('',#100616,#78201,#78202) ;
#68211 = AXIS2_PLACEMENT_3D('',#100617,#78203,#78204) ;
#68212 = AXIS2_PLACEMENT_3D('',#100618,#78205,#78206) ;
#68213 = AXIS2_PLACEMENT_3D('',#100619,#78207,#78208) ;
#68214 = AXIS2_PLACEMENT_3D('',#100620,#78209,#78210) ;
#68215 = AXIS2_PLACEMENT_3D('',#100621,#78211,#78212) ;
#68216 = AXIS2_PLACEMENT_3D('',#100622,#78213,#78214) ;
#68217 = AXIS2_PLACEMENT_3D('',#100623,#78215,#78216) ;
#68218 = AXIS2_PLACEMENT_3D('',#100624,#78217,#78218) ;
#68219 = AXIS2_PLACEMENT_3D('',#100625,#78219,#78220) ;
#68220 = AXIS2_PLACEMENT_3D('',#100626,#78221,#78222) ;
#68221 = AXIS2_PLACEMENT_3D('',#100627,#78223,#78224) ;
#68222 = AXIS2_PLACEMENT_3D('',#100628,#78225,#78226) ;
#68223 = AXIS2_PLACEMENT_3D('',#100629,#78227,#78228) ;
#68224 = AXIS2_PLACEMENT_3D('',#100630,#78229,#78230) ;
#68225 = AXIS2_PLACEMENT_3D('',#100631,#78231,#78232) ;
#68226 = AXIS2_PLACEMENT_3D('',#100632,#78233,#78234) ;
#68227 = AXIS2_PLACEMENT_3D('',#100633,#78235,#78236) ;
#68228 = AXIS2_PLACEMENT_3D('',#100634,#78237,#78238) ;
#68229 = AXIS2_PLACEMENT_3D('',#100635,#78239,#78240) ;
#68230 = AXIS2_PLACEMENT_3D('',#100636,#78241,#78242) ;
#68231 = AXIS2_PLACEMENT_3D('',#100637,#78243,#78244) ;
#68232 = AXIS2_PLACEMENT_3D('',#100638,#78245,#78246) ;
#68233 = AXIS2_PLACEMENT_3D('',#100639,#78247,#78248) ;
#68234 = AXIS2_PLACEMENT_3D('',#100640,#78249,#78250) ;
#68235 = AXIS2_PLACEMENT_3D('',#100641,#78251,#78252) ;
#68236 = AXIS2_PLACEMENT_3D('',#100642,#78253,#78254) ;
#68237 = AXIS2_PLACEMENT_3D('',#100643,#78255,#78256) ;
#68238 = AXIS2_PLACEMENT_3D('',#100644,#78257,#78258) ;
#68239 = AXIS2_PLACEMENT_3D('',#100645,#78259,#78260) ;
#68240 = AXIS2_PLACEMENT_3D('',#100646,#78261,#78262) ;
#68241 = AXIS2_PLACEMENT_3D('',#100647,#78263,#78264) ;
#68242 = AXIS2_PLACEMENT_3D('',#100648,#78265,#78266) ;
#68243 = AXIS2_PLACEMENT_3D('',#100649,#78267,#78268) ;
#68244 = AXIS2_PLACEMENT_3D('',#100650,#78269,#78270) ;
#68245 = AXIS2_PLACEMENT_3D('',#100651,#78271,#78272) ;
#68246 = AXIS2_PLACEMENT_3D('',#100652,#78273,#78274) ;
#68247 = AXIS2_PLACEMENT_3D('',#100653,#78275,#78276) ;
#68248 = AXIS2_PLACEMENT_3D('',#100654,#78277,#78278) ;
#68249 = AXIS2_PLACEMENT_3D('',#100655,#78279,#78280) ;
#68250 = AXIS2_PLACEMENT_3D('',#100656,#78281,#78282) ;
#68251 = AXIS2_PLACEMENT_3D('',#100657,#78283,#78284) ;
#68252 = AXIS2_PLACEMENT_3D('',#100658,#78285,#78286) ;
#68253 = AXIS2_PLACEMENT_3D('',#100659,#78287,#78288) ;
#68254 = AXIS2_PLACEMENT_3D('',#100660,#78289,#78290) ;
#68255 = AXIS2_PLACEMENT_3D('',#100661,#78291,#78292) ;
#68256 = AXIS2_PLACEMENT_3D('',#100662,#78293,#78294) ;
#68257 = AXIS2_PLACEMENT_3D('',#100663,#78295,#78296) ;
#68258 = AXIS2_PLACEMENT_3D('',#100664,#78297,#78298) ;
#68259 = AXIS2_PLACEMENT_3D('',#100665,#78299,#78300) ;
#68260 = AXIS2_PLACEMENT_3D('',#100666,#78301,#78302) ;
#68261 = AXIS2_PLACEMENT_3D('',#100667,#78303,#78304) ;
#68262 = AXIS2_PLACEMENT_3D('',#100668,#78305,#78306) ;
#68263 = AXIS2_PLACEMENT_3D('',#100669,#78307,#78308) ;
#68264 = AXIS2_PLACEMENT_3D('',#100670,#78309,#78310) ;
#68265 = AXIS2_PLACEMENT_3D('',#100671,#78311,#78312) ;
#68266 = AXIS2_PLACEMENT_3D('',#100672,#78313,#78314) ;
#68267 = AXIS2_PLACEMENT_3D('',#100673,#78315,#78316) ;
#68268 = AXIS2_PLACEMENT_3D('',#100674,#78317,#78318) ;
#68269 = AXIS2_PLACEMENT_3D('',#100675,#78319,#78320) ;
#68270 = AXIS2_PLACEMENT_3D('',#100676,#78321,#78322) ;
#68271 = AXIS2_PLACEMENT_3D('',#100677,#78323,#78324) ;
#68272 = AXIS2_PLACEMENT_3D('',#100678,#78325,#78326) ;
#68273 = AXIS2_PLACEMENT_3D('',#100679,#78327,#78328) ;
#68274 = AXIS2_PLACEMENT_3D('',#100680,#78329,#78330) ;
#68275 = AXIS2_PLACEMENT_3D('',#100681,#78331,#78332) ;
#68276 = AXIS2_PLACEMENT_3D('',#100682,#78333,#78334) ;
#68277 = AXIS2_PLACEMENT_3D('',#100683,#78335,#78336) ;
#68278 = AXIS2_PLACEMENT_3D('',#100684,#78337,#78338) ;
#68279 = AXIS2_PLACEMENT_3D('',#100685,#78339,#78340) ;
#68280 = AXIS2_PLACEMENT_3D('',#100686,#78341,#78342) ;
#68281 = AXIS2_PLACEMENT_3D('',#100687,#78343,#78344) ;
#68282 = AXIS2_PLACEMENT_3D('',#100688,#78345,#78346) ;
#68283 = AXIS2_PLACEMENT_3D('',#100689,#78347,#78348) ;
#68284 = AXIS2_PLACEMENT_3D('',#100690,#78349,#78350) ;
#68285 = AXIS2_PLACEMENT_3D('',#100691,#78351,#78352) ;
#68286 = AXIS2_PLACEMENT_3D('',#100692,#78353,#78354) ;
#68287 = AXIS2_PLACEMENT_3D('',#100693,#78355,#78356) ;
#68288 = AXIS2_PLACEMENT_3D('',#100694,#78357,#78358) ;
#68289 = AXIS2_PLACEMENT_3D('',#100695,#78359,#78360) ;
#68290 = AXIS2_PLACEMENT_3D('',#100696,#78361,#78362) ;
#68291 = AXIS2_PLACEMENT_3D('',#100697,#78363,#78364) ;
#68292 = AXIS2_PLACEMENT_3D('',#100698,#78365,#78366) ;
#68293 = AXIS2_PLACEMENT_3D('',#100699,#78367,#78368) ;
#68294 = AXIS2_PLACEMENT_3D('',#100700,#78369,#78370) ;
#68295 = AXIS2_PLACEMENT_3D('',#100701,#78371,#78372) ;
#68296 = AXIS2_PLACEMENT_3D('',#100702,#78373,#78374) ;
#68297 = AXIS2_PLACEMENT_3D('',#100703,#78375,#78376) ;
#68298 = AXIS2_PLACEMENT_3D('',#100704,#78377,#78378) ;
#68299 = AXIS2_PLACEMENT_3D('',#100705,#78379,#78380) ;
#68300 = AXIS2_PLACEMENT_3D('',#100706,#78381,#78382) ;
#68301 = AXIS2_PLACEMENT_3D('',#100707,#78383,#78384) ;
#68302 = AXIS2_PLACEMENT_3D('',#100708,#78385,#78386) ;
#68303 = AXIS2_PLACEMENT_3D('',#100709,#78387,#78388) ;
#68304 = AXIS2_PLACEMENT_3D('',#100710,#78389,#78390) ;
#68305 = AXIS2_PLACEMENT_3D('',#100711,#78391,#78392) ;
#68306 = AXIS2_PLACEMENT_3D('',#100712,#78393,#78394) ;
#68307 = AXIS2_PLACEMENT_3D('',#100713,#78395,#78396) ;
#68308 = AXIS2_PLACEMENT_3D('',#100714,#78397,#78398) ;
#68309 = AXIS2_PLACEMENT_3D('',#100715,#78399,#78400) ;
#68310 = AXIS2_PLACEMENT_3D('',#100716,#78401,#78402) ;
#68311 = AXIS2_PLACEMENT_3D('',#100717,#78403,#78404) ;
#68312 = AXIS2_PLACEMENT_3D('',#100718,#78405,#78406) ;
#68313 = AXIS2_PLACEMENT_3D('',#100719,#78407,#78408) ;
#68314 = AXIS2_PLACEMENT_3D('',#100720,#78409,#78410) ;
#68315 = AXIS2_PLACEMENT_3D('',#100721,#78411,#78412) ;
#68316 = AXIS2_PLACEMENT_3D('',#100722,#78413,#78414) ;
#68317 = AXIS2_PLACEMENT_3D('',#100723,#78415,#78416) ;
#68318 = AXIS2_PLACEMENT_3D('',#100724,#78417,#78418) ;
#68319 = AXIS2_PLACEMENT_3D('',#100725,#78419,#78420) ;
#68320 = AXIS2_PLACEMENT_3D('',#100726,#78421,#78422) ;
#68321 = AXIS2_PLACEMENT_3D('',#100727,#78423,#78424) ;
#68322 = AXIS2_PLACEMENT_3D('',#100728,#78425,#78426) ;
#68323 = AXIS2_PLACEMENT_3D('',#100729,#78427,#78428) ;
#68324 = AXIS2_PLACEMENT_3D('',#100730,#78429,#78430) ;
#68325 = AXIS2_PLACEMENT_3D('',#100731,#78431,#78432) ;
#68326 = AXIS2_PLACEMENT_3D('',#100732,#78433,#78434) ;
#68327 = AXIS2_PLACEMENT_3D('',#100733,#78435,#78436) ;
#68328 = AXIS2_PLACEMENT_3D('',#100734,#78437,#78438) ;
#68329 = AXIS2_PLACEMENT_3D('',#100735,#78439,#78440) ;
#68330 = AXIS2_PLACEMENT_3D('',#100736,#78441,#78442) ;
#68331 = AXIS2_PLACEMENT_3D('',#100737,#78443,#78444) ;
#68332 = AXIS2_PLACEMENT_3D('',#100738,#78445,#78446) ;
#68333 = AXIS2_PLACEMENT_3D('',#100739,#78447,#78448) ;
#68334 = AXIS2_PLACEMENT_3D('',#100740,#78449,#78450) ;
#68335 = AXIS2_PLACEMENT_3D('',#100741,#78451,#78452) ;
#68336 = AXIS2_PLACEMENT_3D('',#100742,#78453,#78454) ;
#68337 = AXIS2_PLACEMENT_3D('',#100743,#78455,#78456) ;
#68338 = AXIS2_PLACEMENT_3D('',#100744,#78457,#78458) ;
#68339 = AXIS2_PLACEMENT_3D('',#100745,#78459,#78460) ;
#68340 = AXIS2_PLACEMENT_3D('',#100746,#78461,#78462) ;
#68341 = AXIS2_PLACEMENT_3D('',#100747,#78463,#78464) ;
#68342 = AXIS2_PLACEMENT_3D('',#100748,#78465,#78466) ;
#68343 = AXIS2_PLACEMENT_3D('',#100749,#78467,#78468) ;
#68344 = AXIS2_PLACEMENT_3D('',#100750,#78469,#78470) ;
#68345 = AXIS2_PLACEMENT_3D('',#100751,#78471,#78472) ;
#68346 = AXIS2_PLACEMENT_3D('',#100752,#78473,#78474) ;
#68347 = AXIS2_PLACEMENT_3D('',#100753,#78475,#78476) ;
#68348 = AXIS2_PLACEMENT_3D('',#100754,#78477,#78478) ;
#68349 = AXIS2_PLACEMENT_3D('',#100755,#78479,#78480) ;
#68350 = AXIS2_PLACEMENT_3D('',#100756,#78481,#78482) ;
#68351 = AXIS2_PLACEMENT_3D('',#100757,#78483,#78484) ;
#68352 = AXIS2_PLACEMENT_3D('',#100758,#78485,#78486) ;
#68353 = AXIS2_PLACEMENT_3D('',#100759,#78487,#78488) ;
#68354 = AXIS2_PLACEMENT_3D('',#100760,#78489,#78490) ;
#68355 = AXIS2_PLACEMENT_3D('',#100761,#78491,#78492) ;
#68356 = AXIS2_PLACEMENT_3D('',#100762,#78493,#78494) ;
#68357 = AXIS2_PLACEMENT_3D('',#100763,#78495,#78496) ;
#68358 = AXIS2_PLACEMENT_3D('',#100764,#78497,#78498) ;
#68359 = AXIS2_PLACEMENT_3D('',#100765,#78499,#78500) ;
#68360 = AXIS2_PLACEMENT_3D('',#100766,#78501,#78502) ;
#68361 = AXIS2_PLACEMENT_3D('',#100767,#78503,#78504) ;
#68362 = AXIS2_PLACEMENT_3D('',#100768,#78505,#78506) ;
#68363 = AXIS2_PLACEMENT_3D('',#100769,#78507,#78508) ;
#68364 = AXIS2_PLACEMENT_3D('',#100770,#78509,#78510) ;
#68365 = AXIS2_PLACEMENT_3D('',#100771,#78511,#78512) ;
#68366 = AXIS2_PLACEMENT_3D('',#100772,#78513,#78514) ;
#68367 = AXIS2_PLACEMENT_3D('',#100773,#78515,#78516) ;
#68368 = AXIS2_PLACEMENT_3D('',#100774,#78517,#78518) ;
#68369 = AXIS2_PLACEMENT_3D('',#100775,#78519,#78520) ;
#68370 = AXIS2_PLACEMENT_3D('',#100776,#78521,#78522) ;
#68371 = AXIS2_PLACEMENT_3D('',#100777,#78523,#78524) ;
#68372 = AXIS2_PLACEMENT_3D('',#100778,#78525,#78526) ;
#68373 = AXIS2_PLACEMENT_3D('',#100779,#78527,#78528) ;
#68374 = AXIS2_PLACEMENT_3D('',#100780,#78529,#78530) ;
#68375 = AXIS2_PLACEMENT_3D('',#100781,#78531,#78532) ;
#68376 = AXIS2_PLACEMENT_3D('',#100782,#78533,#78534) ;
#68377 = AXIS2_PLACEMENT_3D('',#100783,#78535,#78536) ;
#68378 = AXIS2_PLACEMENT_3D('',#100784,#78537,#78538) ;
#68379 = AXIS2_PLACEMENT_3D('',#100785,#78539,#78540) ;
#68380 = AXIS2_PLACEMENT_3D('',#100786,#78541,#78542) ;
#68381 = AXIS2_PLACEMENT_3D('',#100787,#78543,#78544) ;
#68382 = AXIS2_PLACEMENT_3D('',#100788,#78545,#78546) ;
#68383 = AXIS2_PLACEMENT_3D('',#100789,#78547,#78548) ;
#68384 = AXIS2_PLACEMENT_3D('',#100790,#78549,#78550) ;
#68385 = AXIS2_PLACEMENT_3D('',#100791,#78551,#78552) ;
#68386 = AXIS2_PLACEMENT_3D('',#100792,#78553,#78554) ;
#68387 = AXIS2_PLACEMENT_3D('',#100793,#78555,#78556) ;
#68388 = AXIS2_PLACEMENT_3D('',#100794,#78557,#78558) ;
#68389 = AXIS2_PLACEMENT_3D('',#100795,#78559,#78560) ;
#68390 = AXIS2_PLACEMENT_3D('',#100796,#78561,#78562) ;
#68391 = AXIS2_PLACEMENT_3D('',#100797,#78563,#78564) ;
#68392 = AXIS2_PLACEMENT_3D('',#100798,#78565,#78566) ;
#68393 = AXIS2_PLACEMENT_3D('',#100799,#78567,#78568) ;
#68394 = AXIS2_PLACEMENT_3D('',#100800,#78569,#78570) ;
#68395 = AXIS2_PLACEMENT_3D('',#100801,#78571,#78572) ;
#68396 = AXIS2_PLACEMENT_3D('',#100802,#78573,#78574) ;
#68397 = AXIS2_PLACEMENT_3D('',#100803,#78575,#78576) ;
#68398 = AXIS2_PLACEMENT_3D('',#100804,#78577,#78578) ;
#68399 = AXIS2_PLACEMENT_3D('',#100805,#78579,#78580) ;
#68400 = AXIS2_PLACEMENT_3D('',#100806,#78581,#78582) ;
#68401 = AXIS2_PLACEMENT_3D('',#100807,#78583,#78584) ;
#68402 = AXIS2_PLACEMENT_3D('',#100808,#78585,#78586) ;
#68403 = AXIS2_PLACEMENT_3D('',#100809,#78587,#78588) ;
#68404 = AXIS2_PLACEMENT_3D('',#100810,#78589,#78590) ;
#68405 = AXIS2_PLACEMENT_3D('',#100811,#78591,#78592) ;
#68406 = AXIS2_PLACEMENT_3D('',#100812,#78593,#78594) ;
#68407 = AXIS2_PLACEMENT_3D('',#100813,#78595,#78596) ;
#68408 = AXIS2_PLACEMENT_3D('',#100814,#78597,#78598) ;
#68409 = AXIS2_PLACEMENT_3D('',#100815,#78599,#78600) ;
#68410 = AXIS2_PLACEMENT_3D('',#100816,#78601,#78602) ;
#68411 = AXIS2_PLACEMENT_3D('',#100817,#78603,#78604) ;
#68412 = AXIS2_PLACEMENT_3D('',#100818,#78605,#78606) ;
#68413 = AXIS2_PLACEMENT_3D('',#100819,#78607,#78608) ;
#68414 = AXIS2_PLACEMENT_3D('',#100820,#78609,#78610) ;
#68415 = AXIS2_PLACEMENT_3D('',#100821,#78611,#78612) ;
#68416 = AXIS2_PLACEMENT_3D('',#100822,#78613,#78614) ;
#68417 = AXIS2_PLACEMENT_3D('',#100823,#78615,#78616) ;
#68418 = AXIS2_PLACEMENT_3D('',#100824,#78617,#78618) ;
#68419 = AXIS2_PLACEMENT_3D('',#100825,#78619,#78620) ;
#68420 = AXIS2_PLACEMENT_3D('',#100826,#78621,#78622) ;
#68421 = AXIS2_PLACEMENT_3D('',#100827,#78623,#78624) ;
#68422 = AXIS2_PLACEMENT_3D('',#100828,#78625,#78626) ;
#68423 = AXIS2_PLACEMENT_3D('',#100829,#78627,#78628) ;
#68424 = AXIS2_PLACEMENT_3D('',#100830,#78629,#78630) ;
#68425 = AXIS2_PLACEMENT_3D('',#100831,#78631,#78632) ;
#68426 = AXIS2_PLACEMENT_3D('',#100832,#78633,#78634) ;
#68427 = AXIS2_PLACEMENT_3D('',#100833,#78635,#78636) ;
#68428 = AXIS2_PLACEMENT_3D('',#100834,#78637,#78638) ;
#68429 = AXIS2_PLACEMENT_3D('',#100835,#78639,#78640) ;
#68430 = AXIS2_PLACEMENT_3D('',#100836,#78641,#78642) ;
#68431 = AXIS2_PLACEMENT_3D('',#100837,#78643,#78644) ;
#68432 = AXIS2_PLACEMENT_3D('',#100838,#78645,#78646) ;
#68433 = AXIS2_PLACEMENT_3D('',#100839,#78647,#78648) ;
#68434 = AXIS2_PLACEMENT_3D('',#100840,#78649,#78650) ;
#68435 = AXIS2_PLACEMENT_3D('',#100841,#78651,#78652) ;
#68436 = AXIS2_PLACEMENT_3D('',#100842,#78653,#78654) ;
#68437 = AXIS2_PLACEMENT_3D('',#100843,#78655,#78656) ;
#68438 = AXIS2_PLACEMENT_3D('',#100844,#78657,#78658) ;
#68439 = AXIS2_PLACEMENT_3D('',#100845,#78659,#78660) ;
#68440 = AXIS2_PLACEMENT_3D('',#100846,#78661,#78662) ;
#68441 = AXIS2_PLACEMENT_3D('',#100847,#78663,#78664) ;
#68442 = AXIS2_PLACEMENT_3D('',#100848,#78665,#78666) ;
#68443 = AXIS2_PLACEMENT_3D('',#100849,#78667,#78668) ;
#68444 = AXIS2_PLACEMENT_3D('',#100850,#78669,#78670) ;
#68445 = AXIS2_PLACEMENT_3D('',#100851,#78671,#78672) ;
#68446 = AXIS2_PLACEMENT_3D('',#100852,#78673,#78674) ;
#68447 = AXIS2_PLACEMENT_3D('',#100853,#78675,#78676) ;
#68448 = AXIS2_PLACEMENT_3D('',#100854,#78677,#78678) ;
#68449 = AXIS2_PLACEMENT_3D('',#100855,#78679,#78680) ;
#68450 = AXIS2_PLACEMENT_3D('',#100856,#78681,#78682) ;
#68451 = AXIS2_PLACEMENT_3D('',#100857,#78683,#78684) ;
#68452 = AXIS2_PLACEMENT_3D('',#100858,#78685,#78686) ;
#68453 = AXIS2_PLACEMENT_3D('',#100859,#78687,#78688) ;
#68454 = AXIS2_PLACEMENT_3D('',#100860,#78689,#78690) ;
#68455 = AXIS2_PLACEMENT_3D('',#100861,#78691,#78692) ;
#68456 = AXIS2_PLACEMENT_3D('',#100862,#78693,#78694) ;
#68457 = AXIS2_PLACEMENT_3D('',#100863,#78695,#78696) ;
#68458 = AXIS2_PLACEMENT_3D('',#100864,#78697,#78698) ;
#68459 = AXIS2_PLACEMENT_3D('',#100865,#78699,#78700) ;
#68460 = AXIS2_PLACEMENT_3D('',#100866,#78701,#78702) ;
#68461 = AXIS2_PLACEMENT_3D('',#100867,#78703,#78704) ;
#68462 = AXIS2_PLACEMENT_3D('',#100868,#78705,#78706) ;
#68463 = AXIS2_PLACEMENT_3D('',#100869,#78707,#78708) ;
#68464 = AXIS2_PLACEMENT_3D('',#100870,#78709,#78710) ;
#68465 = AXIS2_PLACEMENT_3D('',#100871,#78711,#78712) ;
#68466 = AXIS2_PLACEMENT_3D('',#100872,#78713,#78714) ;
#68467 = AXIS2_PLACEMENT_3D('',#100873,#78715,#78716) ;
#68468 = AXIS2_PLACEMENT_3D('',#100874,#78717,#78718) ;
#68469 = AXIS2_PLACEMENT_3D('',#100875,#78719,#78720) ;
#68470 = AXIS2_PLACEMENT_3D('',#100876,#78721,#78722) ;
#68471 = AXIS2_PLACEMENT_3D('',#100877,#78723,#78724) ;
#68472 = AXIS2_PLACEMENT_3D('',#100878,#78725,#78726) ;
#68473 = AXIS2_PLACEMENT_3D('',#100879,#78727,#78728) ;
#68474 = AXIS2_PLACEMENT_3D('',#100880,#78729,#78730) ;
#68475 = AXIS2_PLACEMENT_3D('',#100881,#78731,#78732) ;
#68476 = AXIS2_PLACEMENT_3D('',#100882,#78733,#78734) ;
#68477 = AXIS2_PLACEMENT_3D('',#100883,#78735,#78736) ;
#68478 = AXIS2_PLACEMENT_3D('',#100884,#78737,#78738) ;
#68479 = AXIS2_PLACEMENT_3D('',#100885,#78739,#78740) ;
#68480 = AXIS2_PLACEMENT_3D('',#100886,#78741,#78742) ;
#68481 = AXIS2_PLACEMENT_3D('',#100887,#78743,#78744) ;
#68482 = AXIS2_PLACEMENT_3D('',#100888,#78745,#78746) ;
#68483 = AXIS2_PLACEMENT_3D('',#100889,#78747,#78748) ;
#68484 = AXIS2_PLACEMENT_3D('',#100890,#78749,#78750) ;
#68485 = AXIS2_PLACEMENT_3D('',#100891,#78751,#78752) ;
#68486 = AXIS2_PLACEMENT_3D('',#100892,#78753,#78754) ;
#68487 = AXIS2_PLACEMENT_3D('',#100893,#78755,#78756) ;
#68488 = AXIS2_PLACEMENT_3D('',#100894,#78757,#78758) ;
#68489 = AXIS2_PLACEMENT_3D('',#100895,#78759,#78760) ;
#68490 = AXIS2_PLACEMENT_3D('',#100896,#78761,#78762) ;
#68491 = AXIS2_PLACEMENT_3D('',#100897,#78763,#78764) ;
#68492 = AXIS2_PLACEMENT_3D('',#100898,#78765,#78766) ;
#68493 = AXIS2_PLACEMENT_3D('',#100899,#78767,#78768) ;
#68494 = AXIS2_PLACEMENT_3D('',#100900,#78769,#78770) ;
#68495 = AXIS2_PLACEMENT_3D('',#100901,#78771,#78772) ;
#68496 = AXIS2_PLACEMENT_3D('',#100902,#78773,#78774) ;
#68497 = AXIS2_PLACEMENT_3D('',#100903,#78775,#78776) ;
#68498 = AXIS2_PLACEMENT_3D('',#100904,#78777,#78778) ;
#68499 = AXIS2_PLACEMENT_3D('',#100905,#78779,#78780) ;
#68500 = AXIS2_PLACEMENT_3D('',#100906,#78781,#78782) ;
#68501 = AXIS2_PLACEMENT_3D('',#100907,#78783,#78784) ;
#68502 = AXIS2_PLACEMENT_3D('',#100908,#78785,#78786) ;
#68503 = AXIS2_PLACEMENT_3D('',#100909,#78787,#78788) ;
#68504 = AXIS2_PLACEMENT_3D('',#100910,#78789,#78790) ;
#68505 = AXIS2_PLACEMENT_3D('',#100911,#78791,#78792) ;
#68506 = AXIS2_PLACEMENT_3D('',#100912,#78793,#78794) ;
#68507 = AXIS2_PLACEMENT_3D('',#100913,#78795,#78796) ;
#68508 = AXIS2_PLACEMENT_3D('',#100914,#78797,#78798) ;
#68509 = AXIS2_PLACEMENT_3D('',#100915,#78799,#78800) ;
#68510 = AXIS2_PLACEMENT_3D('',#100916,#78801,#78802) ;
#68511 = AXIS2_PLACEMENT_3D('',#100917,#78803,#78804) ;
#68512 = AXIS2_PLACEMENT_3D('',#100918,#78805,#78806) ;
#68513 = AXIS2_PLACEMENT_3D('',#100919,#78807,#78808) ;
#68514 = AXIS2_PLACEMENT_3D('',#100920,#78809,#78810) ;
#68515 = AXIS2_PLACEMENT_3D('',#100921,#78811,#78812) ;
#68516 = AXIS2_PLACEMENT_3D('',#100922,#78813,#78814) ;
#68517 = AXIS2_PLACEMENT_3D('',#100923,#78815,#78816) ;
#68518 = AXIS2_PLACEMENT_3D('',#100924,#78817,#78818) ;
#68519 = AXIS2_PLACEMENT_3D('',#100925,#78819,#78820) ;
#68520 = AXIS2_PLACEMENT_3D('',#100926,#78821,#78822) ;
#68521 = AXIS2_PLACEMENT_3D('',#100927,#78823,#78824) ;
#68522 = AXIS2_PLACEMENT_3D('',#100928,#78825,#78826) ;
#68523 = AXIS2_PLACEMENT_3D('',#100929,#78827,#78828) ;
#68524 = AXIS2_PLACEMENT_3D('',#100930,#78829,#78830) ;
#68525 = AXIS2_PLACEMENT_3D('',#100931,#78831,#78832) ;
#68526 = AXIS2_PLACEMENT_3D('',#100932,#78833,#78834) ;
#68527 = AXIS2_PLACEMENT_3D('',#100933,#78835,#78836) ;
#68528 = AXIS2_PLACEMENT_3D('',#100934,#78837,#78838) ;
#68529 = AXIS2_PLACEMENT_3D('',#100935,#78839,#78840) ;
#68530 = AXIS2_PLACEMENT_3D('',#100936,#78841,#78842) ;
#68531 = AXIS2_PLACEMENT_3D('',#100937,#78843,#78844) ;
#68532 = AXIS2_PLACEMENT_3D('',#100938,#78845,#78846) ;
#68533 = AXIS2_PLACEMENT_3D('',#100939,#78847,#78848) ;
#68534 = AXIS2_PLACEMENT_3D('',#100940,#78849,#78850) ;
#68535 = AXIS2_PLACEMENT_3D('',#100941,#78851,#78852) ;
#68536 = AXIS2_PLACEMENT_3D('',#100942,#78853,#78854) ;
#68537 = AXIS2_PLACEMENT_3D('',#100943,#78855,#78856) ;
#68538 = AXIS2_PLACEMENT_3D('',#100944,#78857,#78858) ;
#68539 = AXIS2_PLACEMENT_3D('',#100945,#78859,#78860) ;
#68540 = AXIS2_PLACEMENT_3D('',#100946,#78861,#78862) ;
#68541 = AXIS2_PLACEMENT_3D('',#100947,#78863,#78864) ;
#68542 = AXIS2_PLACEMENT_3D('',#100948,#78865,#78866) ;
#68543 = AXIS2_PLACEMENT_3D('',#100949,#78867,#78868) ;
#68544 = AXIS2_PLACEMENT_3D('',#100950,#78869,#78870) ;
#68545 = AXIS2_PLACEMENT_3D('',#100951,#78871,#78872) ;
#68546 = AXIS2_PLACEMENT_3D('',#100952,#78873,#78874) ;
#68547 = AXIS2_PLACEMENT_3D('',#100953,#78875,#78876) ;
#68548 = AXIS2_PLACEMENT_3D('',#100954,#78877,#78878) ;
#68549 = AXIS2_PLACEMENT_3D('',#100955,#78879,#78880) ;
#68550 = AXIS2_PLACEMENT_3D('',#100956,#78881,#78882) ;
#68551 = AXIS2_PLACEMENT_3D('',#100957,#78883,#78884) ;
#68552 = AXIS2_PLACEMENT_3D('',#100958,#78885,#78886) ;
#68553 = AXIS2_PLACEMENT_3D('',#100959,#78887,#78888) ;
#68554 = AXIS2_PLACEMENT_3D('',#100960,#78889,#78890) ;
#68555 = AXIS2_PLACEMENT_3D('',#100961,#78891,#78892) ;
#68556 = AXIS2_PLACEMENT_3D('',#100962,#78893,#78894) ;
#68557 = AXIS2_PLACEMENT_3D('',#100963,#78895,#78896) ;
#68558 = AXIS2_PLACEMENT_3D('',#100964,#78897,#78898) ;
#68559 = AXIS2_PLACEMENT_3D('',#100965,#78899,#78900) ;
#68560 = AXIS2_PLACEMENT_3D('',#100966,#78901,#78902) ;
#68561 = AXIS2_PLACEMENT_3D('',#100967,#78903,#78904) ;
#68562 = AXIS2_PLACEMENT_3D('',#100968,#78905,#78906) ;
#68563 = AXIS2_PLACEMENT_3D('',#100969,#78907,#78908) ;
#68564 = AXIS2_PLACEMENT_3D('',#100970,#78909,#78910) ;
#68565 = AXIS2_PLACEMENT_3D('',#100971,#78911,#78912) ;
#68566 = AXIS2_PLACEMENT_3D('',#100972,#78913,#78914) ;
#68567 = AXIS2_PLACEMENT_3D('',#100973,#78915,#78916) ;
#68568 = AXIS2_PLACEMENT_3D('',#100974,#78917,#78918) ;
#68569 = AXIS2_PLACEMENT_3D('',#100975,#78919,#78920) ;
#68570 = AXIS2_PLACEMENT_3D('',#100976,#78921,#78922) ;
#68571 = AXIS2_PLACEMENT_3D('',#100977,#78923,#78924) ;
#68572 = AXIS2_PLACEMENT_3D('',#100978,#78925,#78926) ;
#68573 = AXIS2_PLACEMENT_3D('',#100979,#78927,#78928) ;
#68574 = AXIS2_PLACEMENT_3D('',#100980,#78929,#78930) ;
#68575 = AXIS2_PLACEMENT_3D('',#100981,#78931,#78932) ;
#68576 = AXIS2_PLACEMENT_3D('',#100982,#78933,#78934) ;
#68577 = AXIS2_PLACEMENT_3D('',#100983,#78935,#78936) ;
#68578 = AXIS2_PLACEMENT_3D('',#100984,#78937,#78938) ;
#68579 = AXIS2_PLACEMENT_3D('',#100985,#78939,#78940) ;
#68580 = AXIS2_PLACEMENT_3D('',#100986,#78941,#78942) ;
#68581 = AXIS2_PLACEMENT_3D('',#100987,#78943,#78944) ;
#68582 = AXIS2_PLACEMENT_3D('',#100988,#78945,#78946) ;
#68583 = AXIS2_PLACEMENT_3D('',#100989,#78947,#78948) ;
#68584 = AXIS2_PLACEMENT_3D('',#100990,#78949,#78950) ;
#68585 = AXIS2_PLACEMENT_3D('',#100991,#78951,#78952) ;
#68586 = AXIS2_PLACEMENT_3D('',#100992,#78953,#78954) ;
#68587 = AXIS2_PLACEMENT_3D('',#100993,#78955,#78956) ;
#68588 = AXIS2_PLACEMENT_3D('',#100994,#78957,#78958) ;
#68589 = AXIS2_PLACEMENT_3D('',#100995,#78959,#78960) ;
#68590 = AXIS2_PLACEMENT_3D('',#100996,#78961,#78962) ;
#68591 = AXIS2_PLACEMENT_3D('',#100997,#78963,#78964) ;
#68592 = AXIS2_PLACEMENT_3D('',#100998,#78965,#78966) ;
#68593 = AXIS2_PLACEMENT_3D('',#100999,#78967,#78968) ;
#68594 = AXIS2_PLACEMENT_3D('',#101000,#78969,#78970) ;
#68595 = AXIS2_PLACEMENT_3D('',#101001,#78971,#78972) ;
#68596 = AXIS2_PLACEMENT_3D('',#101002,#78973,#78974) ;
#68597 = AXIS2_PLACEMENT_3D('',#101003,#78975,#78976) ;
#68598 = AXIS2_PLACEMENT_3D('',#101004,#78977,#78978) ;
#68599 = AXIS2_PLACEMENT_3D('',#101005,#78979,#78980) ;
#68600 = AXIS2_PLACEMENT_3D('',#101006,#78981,#78982) ;
#68601 = AXIS2_PLACEMENT_3D('',#101007,#78983,#78984) ;
#68602 = AXIS2_PLACEMENT_3D('',#101008,#78985,#78986) ;
#68603 = AXIS2_PLACEMENT_3D('',#101009,#78987,#78988) ;
#68604 = AXIS2_PLACEMENT_3D('',#101010,#78989,#78990) ;
#68605 = AXIS2_PLACEMENT_3D('',#101011,#78991,#78992) ;
#68606 = AXIS2_PLACEMENT_3D('',#101012,#78993,#78994) ;
#68607 = AXIS2_PLACEMENT_3D('',#101013,#78995,#78996) ;
#68608 = AXIS2_PLACEMENT_3D('',#101014,#78997,#78998) ;
#68609 = AXIS2_PLACEMENT_3D('',#101015,#78999,#79000) ;
#68610 = AXIS2_PLACEMENT_3D('',#101016,#79001,#79002) ;
#68611 = AXIS2_PLACEMENT_3D('',#101017,#79003,#79004) ;
#68612 = AXIS2_PLACEMENT_3D('',#101018,#79005,#79006) ;
#68613 = AXIS2_PLACEMENT_3D('',#101019,#79007,#79008) ;
#68614 = AXIS2_PLACEMENT_3D('',#101020,#79009,#79010) ;
#68615 = AXIS2_PLACEMENT_3D('',#101021,#79011,#79012) ;
#68616 = AXIS2_PLACEMENT_3D('',#101022,#79013,#79014) ;
#68617 = AXIS2_PLACEMENT_3D('',#101023,#79015,#79016) ;
#68618 = AXIS2_PLACEMENT_3D('',#101024,#79017,#79018) ;
#68619 = AXIS2_PLACEMENT_3D('',#101025,#79019,#79020) ;
#68620 = AXIS2_PLACEMENT_3D('',#101026,#79021,#79022) ;
#68621 = AXIS2_PLACEMENT_3D('',#101027,#79023,#79024) ;
#68622 = AXIS2_PLACEMENT_3D('',#101028,#79025,#79026) ;
#68623 = AXIS2_PLACEMENT_3D('',#101029,#79027,#79028) ;
#68624 = AXIS2_PLACEMENT_3D('',#101030,#79029,#79030) ;
#68625 = AXIS2_PLACEMENT_3D('',#101031,#79031,#79032) ;
#68626 = AXIS2_PLACEMENT_3D('',#101032,#79033,#79034) ;
#68627 = AXIS2_PLACEMENT_3D('',#101033,#79035,#79036) ;
#68628 = AXIS2_PLACEMENT_3D('',#101034,#79037,#79038) ;
#68629 = AXIS2_PLACEMENT_3D('',#101035,#79039,#79040) ;
#68630 = AXIS2_PLACEMENT_3D('',#101036,#79041,#79042) ;
#68631 = AXIS2_PLACEMENT_3D('',#101037,#79043,#79044) ;
#68632 = AXIS2_PLACEMENT_3D('',#101038,#79045,#79046) ;
#68633 = AXIS2_PLACEMENT_3D('',#101039,#79047,#79048) ;
#68634 = AXIS2_PLACEMENT_3D('',#101040,#79049,#79050) ;
#68635 = AXIS2_PLACEMENT_3D('',#101041,#79051,#79052) ;
#68636 = AXIS2_PLACEMENT_3D('',#101042,#79053,#79054) ;
#68637 = AXIS2_PLACEMENT_3D('',#101043,#79055,#79056) ;
#68638 = AXIS2_PLACEMENT_3D('',#101044,#79057,#79058) ;
#68639 = AXIS2_PLACEMENT_3D('',#101045,#79059,#79060) ;
#68640 = AXIS2_PLACEMENT_3D('',#101046,#79061,#79062) ;
#68641 = AXIS2_PLACEMENT_3D('',#101047,#79063,#79064) ;
#68642 = AXIS2_PLACEMENT_3D('',#101048,#79065,#79066) ;
#68643 = AXIS2_PLACEMENT_3D('',#101049,#79067,#79068) ;
#68644 = AXIS2_PLACEMENT_3D('',#101050,#79069,#79070) ;
#68645 = AXIS2_PLACEMENT_3D('',#101051,#79071,#79072) ;
#68646 = AXIS2_PLACEMENT_3D('',#101052,#79073,#79074) ;
#68647 = AXIS2_PLACEMENT_3D('',#101053,#79075,#79076) ;
#68648 = AXIS2_PLACEMENT_3D('',#101054,#79077,#79078) ;
#68649 = AXIS2_PLACEMENT_3D('',#101055,#79079,#79080) ;
#68650 = AXIS2_PLACEMENT_3D('',#101056,#79081,#79082) ;
#68651 = AXIS2_PLACEMENT_3D('',#101057,#79083,#79084) ;
#68652 = AXIS2_PLACEMENT_3D('',#101058,#79085,#79086) ;
#68653 = AXIS2_PLACEMENT_3D('',#101059,#79087,#79088) ;
#68654 = AXIS2_PLACEMENT_3D('',#101060,#79089,#79090) ;
#68655 = AXIS2_PLACEMENT_3D('',#101061,#79091,#79092) ;
#68656 = AXIS2_PLACEMENT_3D('',#101062,#79093,#79094) ;
#68657 = AXIS2_PLACEMENT_3D('',#101063,#79095,#79096) ;
#68658 = AXIS2_PLACEMENT_3D('',#101064,#79097,#79098) ;
#68659 = AXIS2_PLACEMENT_3D('',#101065,#79099,#79100) ;
#68660 = AXIS2_PLACEMENT_3D('',#101066,#79101,#79102) ;
#68661 = AXIS2_PLACEMENT_3D('',#101067,#79103,#79104) ;
#68662 = AXIS2_PLACEMENT_3D('',#101068,#79105,#79106) ;
#68663 = AXIS2_PLACEMENT_3D('',#101069,#79107,#79108) ;
#68664 = AXIS2_PLACEMENT_3D('',#101070,#79109,#79110) ;
#68665 = AXIS2_PLACEMENT_3D('',#101071,#79111,#79112) ;
#68666 = AXIS2_PLACEMENT_3D('',#101072,#79113,#79114) ;
#68667 = AXIS2_PLACEMENT_3D('',#101073,#79115,#79116) ;
#68668 = AXIS2_PLACEMENT_3D('',#101074,#79117,#79118) ;
#68669 = AXIS2_PLACEMENT_3D('',#101075,#79119,#79120) ;
#68670 = AXIS2_PLACEMENT_3D('',#101076,#79121,#79122) ;
#68671 = AXIS2_PLACEMENT_3D('',#101077,#79123,#79124) ;
#68672 = AXIS2_PLACEMENT_3D('',#101078,#79125,#79126) ;
#68673 = AXIS2_PLACEMENT_3D('',#101079,#79127,#79128) ;
#68674 = AXIS2_PLACEMENT_3D('',#101080,#79129,#79130) ;
#68675 = AXIS2_PLACEMENT_3D('',#101081,#79131,#79132) ;
#68676 = AXIS2_PLACEMENT_3D('',#101082,#79133,#79134) ;
#68677 = AXIS2_PLACEMENT_3D('',#101083,#79135,#79136) ;
#68678 = AXIS2_PLACEMENT_3D('',#101084,#79137,#79138) ;
#68679 = AXIS2_PLACEMENT_3D('',#101085,#79139,#79140) ;
#68680 = AXIS2_PLACEMENT_3D('',#101086,#79141,#79142) ;
#68681 = AXIS2_PLACEMENT_3D('',#101087,#79143,#79144) ;
#68682 = AXIS2_PLACEMENT_3D('',#101088,#79145,#79146) ;
#68683 = AXIS2_PLACEMENT_3D('',#101089,#79147,#79148) ;
#68684 = AXIS2_PLACEMENT_3D('',#101090,#79149,#79150) ;
#68685 = AXIS2_PLACEMENT_3D('',#101091,#79151,#79152) ;
#68686 = AXIS2_PLACEMENT_3D('',#101092,#79153,#79154) ;
#68687 = AXIS2_PLACEMENT_3D('',#101093,#79155,#79156) ;
#68688 = AXIS2_PLACEMENT_3D('',#101094,#79157,#79158) ;
#68689 = AXIS2_PLACEMENT_3D('',#101095,#79159,#79160) ;
#68690 = AXIS2_PLACEMENT_3D('',#101096,#79161,#79162) ;
#68691 = AXIS2_PLACEMENT_3D('',#101097,#79163,#79164) ;
#68692 = AXIS2_PLACEMENT_3D('',#101098,#79165,#79166) ;
#68693 = AXIS2_PLACEMENT_3D('',#101099,#79167,#79168) ;
#68694 = AXIS2_PLACEMENT_3D('',#101100,#79169,#79170) ;
#68695 = AXIS2_PLACEMENT_3D('',#101101,#79171,#79172) ;
#68696 = AXIS2_PLACEMENT_3D('',#101102,#79173,#79174) ;
#68697 = AXIS2_PLACEMENT_3D('',#101103,#79175,#79176) ;
#68698 = AXIS2_PLACEMENT_3D('',#101104,#79177,#79178) ;
#68699 = AXIS2_PLACEMENT_3D('',#101105,#79179,#79180) ;
#68700 = AXIS2_PLACEMENT_3D('',#101106,#79181,#79182) ;
#68701 = AXIS2_PLACEMENT_3D('',#101107,#79183,#79184) ;
#68702 = AXIS2_PLACEMENT_3D('',#101108,#79185,#79186) ;
#68703 = AXIS2_PLACEMENT_3D('',#101109,#79187,#79188) ;
#68704 = AXIS2_PLACEMENT_3D('',#101110,#79189,#79190) ;
#68705 = AXIS2_PLACEMENT_3D('',#101111,#79191,#79192) ;
#68706 = AXIS2_PLACEMENT_3D('',#101112,#79193,#79194) ;
#68707 = AXIS2_PLACEMENT_3D('',#101113,#79195,#79196) ;
#68708 = AXIS2_PLACEMENT_3D('',#101114,#79197,#79198) ;
#68709 = AXIS2_PLACEMENT_3D('',#101115,#79199,#79200) ;
#68710 = AXIS2_PLACEMENT_3D('',#101116,#79201,#79202) ;
#68711 = AXIS2_PLACEMENT_3D('',#101117,#79203,#79204) ;
#68712 = AXIS2_PLACEMENT_3D('',#101118,#79205,#79206) ;
#68713 = AXIS2_PLACEMENT_3D('',#101119,#79207,#79208) ;
#68714 = AXIS2_PLACEMENT_3D('',#101120,#79209,#79210) ;
#68715 = AXIS2_PLACEMENT_3D('',#101121,#79211,#79212) ;
#68716 = AXIS2_PLACEMENT_3D('',#101122,#79213,#79214) ;
#68717 = AXIS2_PLACEMENT_3D('',#101123,#79215,#79216) ;
#68718 = AXIS2_PLACEMENT_3D('',#101124,#79217,#79218) ;
#68719 = AXIS2_PLACEMENT_3D('',#101125,#79219,#79220) ;
#68720 = AXIS2_PLACEMENT_3D('',#101126,#79221,#79222) ;
#68721 = AXIS2_PLACEMENT_3D('',#101127,#79223,#79224) ;
#68722 = AXIS2_PLACEMENT_3D('',#101128,#79225,#79226) ;
#68723 = AXIS2_PLACEMENT_3D('',#101129,#79227,#79228) ;
#68724 = AXIS2_PLACEMENT_3D('',#101130,#79229,#79230) ;
#68725 = AXIS2_PLACEMENT_3D('',#101131,#79231,#79232) ;
#68726 = AXIS2_PLACEMENT_3D('',#101132,#79233,#79234) ;
#68727 = AXIS2_PLACEMENT_3D('',#101133,#79235,#79236) ;
#68728 = AXIS2_PLACEMENT_3D('',#101134,#79237,#79238) ;
#68729 = AXIS2_PLACEMENT_3D('',#101135,#79239,#79240) ;
#68730 = AXIS2_PLACEMENT_3D('',#101136,#79241,#79242) ;
#68731 = AXIS2_PLACEMENT_3D('',#101137,#79243,#79244) ;
#68732 = AXIS2_PLACEMENT_3D('',#101138,#79245,#79246) ;
#68733 = AXIS2_PLACEMENT_3D('',#101139,#79247,#79248) ;
#68734 = AXIS2_PLACEMENT_3D('',#101140,#79249,#79250) ;
#68735 = AXIS2_PLACEMENT_3D('',#101141,#79251,#79252) ;
#68736 = AXIS2_PLACEMENT_3D('',#101142,#79253,#79254) ;
#68737 = AXIS2_PLACEMENT_3D('',#101143,#79255,#79256) ;
#68738 = AXIS2_PLACEMENT_3D('',#101144,#79257,#79258) ;
#68739 = AXIS2_PLACEMENT_3D('',#101145,#79259,#79260) ;
#68740 = AXIS2_PLACEMENT_3D('',#101146,#79261,#79262) ;
#68741 = AXIS2_PLACEMENT_3D('',#101147,#79263,#79264) ;
#68742 = AXIS2_PLACEMENT_3D('',#101148,#79265,#79266) ;
#68743 = AXIS2_PLACEMENT_3D('',#101149,#79267,#79268) ;
#68744 = AXIS2_PLACEMENT_3D('',#101150,#79269,#79270) ;
#68745 = AXIS2_PLACEMENT_3D('',#101151,#79271,#79272) ;
#68746 = AXIS2_PLACEMENT_3D('',#101152,#79273,#79274) ;
#68747 = AXIS2_PLACEMENT_3D('',#101153,#79275,#79276) ;
#68748 = AXIS2_PLACEMENT_3D('',#101154,#79277,#79278) ;
#68749 = AXIS2_PLACEMENT_3D('',#101155,#79279,#79280) ;
#68750 = AXIS2_PLACEMENT_3D('',#101156,#79281,#79282) ;
#68751 = AXIS2_PLACEMENT_3D('',#101157,#79283,#79284) ;
#68752 = AXIS2_PLACEMENT_3D('',#101158,#79285,#79286) ;
#68753 = AXIS2_PLACEMENT_3D('',#101159,#79287,#79288) ;
#68754 = AXIS2_PLACEMENT_3D('',#101160,#79289,#79290) ;
#68755 = AXIS2_PLACEMENT_3D('',#101161,#79291,#79292) ;
#68756 = AXIS2_PLACEMENT_3D('',#101162,#79293,#79294) ;
#68757 = AXIS2_PLACEMENT_3D('',#101163,#79295,#79296) ;
#68758 = AXIS2_PLACEMENT_3D('',#101164,#79297,#79298) ;
#68759 = AXIS2_PLACEMENT_3D('',#101165,#79299,#79300) ;
#68760 = AXIS2_PLACEMENT_3D('',#101166,#79301,#79302) ;
#68761 = AXIS2_PLACEMENT_3D('',#101167,#79303,#79304) ;
#68762 = AXIS2_PLACEMENT_3D('',#101168,#79305,#79306) ;
#68763 = AXIS2_PLACEMENT_3D('',#101169,#79307,#79308) ;
#68764 = AXIS2_PLACEMENT_3D('',#101170,#79309,#79310) ;
#68765 = AXIS2_PLACEMENT_3D('',#101171,#79311,#79312) ;
#68766 = AXIS2_PLACEMENT_3D('',#101172,#79313,#79314) ;
#68767 = AXIS2_PLACEMENT_3D('',#101173,#79315,#79316) ;
#68768 = AXIS2_PLACEMENT_3D('',#101174,#79317,#79318) ;
#68769 = AXIS2_PLACEMENT_3D('',#101175,#79319,#79320) ;
#68770 = AXIS2_PLACEMENT_3D('',#101176,#79321,#79322) ;
#68771 = AXIS2_PLACEMENT_3D('',#101177,#79323,#79324) ;
#68772 = AXIS2_PLACEMENT_3D('',#101178,#79325,#79326) ;
#68773 = AXIS2_PLACEMENT_3D('',#101179,#79327,#79328) ;
#68774 = AXIS2_PLACEMENT_3D('',#101180,#79329,#79330) ;
#68775 = AXIS2_PLACEMENT_3D('',#101181,#79331,#79332) ;
#68776 = AXIS2_PLACEMENT_3D('',#101182,#79333,#79334) ;
#68777 = AXIS2_PLACEMENT_3D('',#101183,#79335,#79336) ;
#68778 = AXIS2_PLACEMENT_3D('',#101184,#79337,#79338) ;
#68779 = AXIS2_PLACEMENT_3D('',#101210,#79339,#79340) ;
#68780 = AXIS2_PLACEMENT_3D('',#101212,#79341,#79342) ;
#68781 = AXIS2_PLACEMENT_3D('',#101214,#79343,#79344) ;
#68782 = AXIS2_PLACEMENT_3D('',#101253,#79345,#79346) ;
#68783 = AXIS2_PLACEMENT_3D('',#101255,#79347,#79348) ;
#68784 = AXIS2_PLACEMENT_3D('',#101257,#79349,#79350) ;
#68785 = AXIS2_PLACEMENT_3D('',#101258,#79351,#79352) ;
#68786 = AXIS2_PLACEMENT_3D('',#101259,#79353,#79354) ;
#68787 = AXIS2_PLACEMENT_3D('',#101261,#79355,#79356) ;
#68788 = AXIS2_PLACEMENT_3D('',#101263,#79357,#79358) ;
#68789 = AXIS2_PLACEMENT_3D('',#101264,#79359,#79360) ;
#68790 = AXIS2_PLACEMENT_3D('',#101265,#79361,#79362) ;
#68791 = AXIS2_PLACEMENT_3D('',#101267,#79363,#79364) ;
#68792 = AXIS2_PLACEMENT_3D('',#101269,#79365,#79366) ;
#68793 = AXIS2_PLACEMENT_3D('',#101270,#79367,#79368) ;
#68794 = AXIS2_PLACEMENT_3D('',#101271,#79369,#79370) ;
#68795 = AXIS2_PLACEMENT_3D('',#101274,#79371,#79372) ;
#68796 = AXIS2_PLACEMENT_3D('',#101278,#79374,#79375) ;
#68797 = AXIS2_PLACEMENT_3D('',#101280,#79376,#79377) ;
#68798 = AXIS2_PLACEMENT_3D('',#101282,#79379,#79380) ;
#68799 = AXIS2_PLACEMENT_3D('',#101285,#79381,#79382) ;
#68800 = AXIS2_PLACEMENT_3D('',#101289,#79384,#79385) ;
#68801 = AXIS2_PLACEMENT_3D('',#101291,#79387,#79388) ;
#68802 = AXIS2_PLACEMENT_3D('',#101294,#79389,#79390) ;
#68803 = AXIS2_PLACEMENT_3D('',#101296,#79391,#79392) ;
#68804 = AXIS2_PLACEMENT_3D('',#101298,#79393,#79394) ;
#68805 = AXIS2_PLACEMENT_3D('',#101299,#79395,#79396) ;
#68806 = AXIS2_PLACEMENT_3D('',#101300,#79397,#79398) ;
#68807 = AXIS2_PLACEMENT_3D('',#101302,#79400,#79401) ;
#68808 = AXIS2_PLACEMENT_3D('',#101305,#79403,#79404) ;
#68809 = AXIS2_PLACEMENT_3D('',#101314,#79405,#79406) ;
#68810 = AXIS2_PLACEMENT_3D('',#101322,#79407,#79408) ;
#68811 = AXIS2_PLACEMENT_3D('',#101324,#79410,#79411) ;
#68812 = AXIS2_PLACEMENT_3D('',#101340,#79415,#79416) ;
#68813 = AXIS2_PLACEMENT_3D('',#101342,#79418,#79419) ;
#68814 = AXIS2_PLACEMENT_3D('',#101391,#79424,#79425) ;
#68815 = AXIS2_PLACEMENT_3D('',#101400,#79430,#79431) ;
#68816 = AXIS2_PLACEMENT_3D('',#101430,#79436,#79437) ;
#68817 = AXIS2_PLACEMENT_3D('',#101439,#79442,#79443) ;
#68818 = AXIS2_PLACEMENT_3D('',#101448,#79448,#79449) ;
#68819 = AXIS2_PLACEMENT_3D('',#101459,#79454,#79455) ;
#68820 = AXIS2_PLACEMENT_3D('',#101461,#79457,#79458) ;
#68821 = AXIS2_PLACEMENT_3D('',#101465,#79460,#79461) ;
#68822 = AXIS2_PLACEMENT_3D('',#101466,#79462,#79463) ;
#68823 = AXIS2_PLACEMENT_3D('',#101467,#79464,#79465) ;
#68824 = AXIS2_PLACEMENT_3D('',#101469,#79466,#79467) ;
#68825 = AXIS2_PLACEMENT_3D('',#101473,#79469,#79470) ;
#68826 = AXIS2_PLACEMENT_3D('',#101477,#79472,#79473) ;
#68827 = AXIS2_PLACEMENT_3D('',#101481,#79475,#79476) ;
#68828 = AXIS2_PLACEMENT_3D('',#101485,#79478,#79479) ;
#68829 = AXIS2_PLACEMENT_3D('',#101489,#79481,#79482) ;
#68830 = AXIS2_PLACEMENT_3D('',#101492,#79484,#79485) ;
#68831 = AXIS2_PLACEMENT_3D('',#101494,#79486,#79487) ;
#68832 = AXIS2_PLACEMENT_3D('',#101497,#79489,#79490) ;
#68833 = AXIS2_PLACEMENT_3D('',#101499,#79491,#79492) ;
#68834 = AXIS2_PLACEMENT_3D('',#101505,#79495,#79496) ;
#68835 = AXIS2_PLACEMENT_3D('',#101509,#79498,#79499) ;
#68836 = AXIS2_PLACEMENT_3D('',#101512,#79501,#79502) ;
#68837 = AXIS2_PLACEMENT_3D('',#101513,#79503,#79504) ;
#68838 = AXIS2_PLACEMENT_3D('',#101518,#79506,#79507) ;
#68839 = AXIS2_PLACEMENT_3D('',#101522,#79509,#79510) ;
#68840 = AXIS2_PLACEMENT_3D('',#101526,#79512,#79513) ;
#68841 = AXIS2_PLACEMENT_3D('',#101530,#79515,#79516) ;
#68842 = AXIS2_PLACEMENT_3D('',#101535,#79519,#79520) ;
#68843 = AXIS2_PLACEMENT_3D('',#101537,#79521,#79522) ;
#68844 = AXIS2_PLACEMENT_3D('',#101540,#79524,#79525) ;
#68845 = AXIS2_PLACEMENT_3D('',#101542,#79526,#79527) ;
#68846 = AXIS2_PLACEMENT_3D('',#101546,#79529,#79530) ;
#68847 = AXIS2_PLACEMENT_3D('',#101550,#79532,#79533) ;
#68848 = AXIS2_PLACEMENT_3D('',#101554,#79535,#79536) ;
#68849 = AXIS2_PLACEMENT_3D('',#101558,#79538,#79539) ;
#68850 = AXIS2_PLACEMENT_3D('',#101562,#79541,#79542) ;
#68851 = AXIS2_PLACEMENT_3D('',#101566,#79544,#79545) ;
#68852 = AXIS2_PLACEMENT_3D('',#101570,#79547,#79548) ;
#68853 = AXIS2_PLACEMENT_3D('',#101573,#79550,#79551) ;
#68854 = AXIS2_PLACEMENT_3D('',#101574,#79552,#79553) ;
#68855 = AXIS2_PLACEMENT_3D('',#101577,#79556,#79557) ;
#68856 = AXIS2_PLACEMENT_3D('',#101580,#79560,#79561) ;
#68857 = AXIS2_PLACEMENT_3D('',#101669,#79566,#79567) ;
#68858 = AXIS2_PLACEMENT_3D('',#101680,#79568,#79569) ;
#68859 = AXIS2_PLACEMENT_3D('',#101685,#79573,#79574) ;
#68860 = AXIS2_PLACEMENT_3D('',#101691,#79578,#79579) ;
#68861 = AXIS2_PLACEMENT_3D('',#101711,#79583,#79584) ;
#68862 = AXIS2_PLACEMENT_3D('',#101810,#79590,#79591) ;
#68863 = AXIS2_PLACEMENT_3D('',#101814,#79593,#79594) ;
#68864 = AXIS2_PLACEMENT_3D('',#101818,#79597,#79598) ;
#68865 = AXIS2_PLACEMENT_3D('',#101821,#79599,#79600) ;
#68866 = AXIS2_PLACEMENT_3D('',#101826,#79603,#79604) ;
#68867 = AXIS2_PLACEMENT_3D('',#101828,#79605,#79606) ;
#68868 = AXIS2_PLACEMENT_3D('',#101830,#79607,#79608) ;
#68869 = AXIS2_PLACEMENT_3D('',#101838,#79612,#79613) ;
#68870 = AXIS2_PLACEMENT_3D('',#101840,#79614,#79615) ;
#68871 = AXIS2_PLACEMENT_3D('',#101842,#79616,#79617) ;
#68872 = AXIS2_PLACEMENT_3D('',#101847,#79620,#79621) ;
#68873 = AXIS2_PLACEMENT_3D('',#101849,#79622,#79623) ;
#68874 = AXIS2_PLACEMENT_3D('',#101851,#79624,#79625) ;
#68875 = AXIS2_PLACEMENT_3D('',#101855,#79627,#79628) ;
#68876 = AXIS2_PLACEMENT_3D('',#101859,#79630,#79631) ;
#68877 = AXIS2_PLACEMENT_3D('',#101860,#79632,#79633) ;
#68878 = AXIS2_PLACEMENT_3D('',#101861,#79634,#79635) ;
#68879 = AXIS2_PLACEMENT_3D('',#101864,#79636,#79637) ;
#68880 = AXIS2_PLACEMENT_3D('',#101874,#79643,#79644) ;
#68881 = AXIS2_PLACEMENT_3D('',#101876,#79646,#79647) ;
#68882 = AXIS2_PLACEMENT_3D('',#101879,#79648,#79649) ;
#68883 = AXIS2_PLACEMENT_3D('',#101885,#79653,#79654) ;
#68884 = AXIS2_PLACEMENT_3D('',#101887,#79656,#79657) ;
#68885 = AXIS2_PLACEMENT_3D('',#101893,#79660,#79661) ;
#68886 = AXIS2_PLACEMENT_3D('',#101894,#79662,#79663) ;
#68887 = AXIS2_PLACEMENT_3D('',#101897,#79664,#79665) ;
#68888 = AXIS2_PLACEMENT_3D('',#101901,#79668,#79669) ;
#68889 = AXIS2_PLACEMENT_3D('',#101918,#79678,#79679) ;
#68890 = AXIS2_PLACEMENT_3D('',#101927,#79684,#79685) ;
#68891 = AXIS2_PLACEMENT_3D('',#101936,#79690,#79691) ;
#68892 = AXIS2_PLACEMENT_3D('',#101945,#79696,#79697) ;
#68893 = AXIS2_PLACEMENT_3D('',#101972,#79702,#79703) ;
#68894 = AXIS2_PLACEMENT_3D('',#101989,#79712,#79713) ;
#68895 = AXIS2_PLACEMENT_3D('',#101994,#79715,#79716) ;
#68896 = AXIS2_PLACEMENT_3D('',#101998,#79718,#79719) ;
#68897 = AXIS2_PLACEMENT_3D('',#102002,#79721,#79722) ;
#68898 = AXIS2_PLACEMENT_3D('',#102005,#79724,#79725) ;
#68899 = AXIS2_PLACEMENT_3D('',#102006,#79726,#79727) ;
#68900 = AXIS2_PLACEMENT_3D('',#102009,#79728,#79729) ;
#68901 = AXIS2_PLACEMENT_3D('',#102014,#79732,#79733) ;
#68902 = AXIS2_PLACEMENT_3D('',#102017,#79735,#79736) ;
#68903 = AXIS2_PLACEMENT_3D('',#102018,#79737,#79738) ;
#68904 = AXIS2_PLACEMENT_3D('',#102024,#79742,#79743) ;
#68905 = AXIS2_PLACEMENT_3D('',#102030,#79747,#79748) ;
#68906 = AXIS2_PLACEMENT_3D('',#102033,#79749,#79750) ;
#68907 = AXIS2_PLACEMENT_3D('',#102037,#79752,#79753) ;
#68908 = AXIS2_PLACEMENT_3D('',#102039,#79755,#79756) ;
#68909 = AXIS2_PLACEMENT_3D('',#102042,#79757,#79758) ;
#68910 = AXIS2_PLACEMENT_3D('',#102046,#79760,#79761) ;
#68911 = AXIS2_PLACEMENT_3D('',#102048,#79763,#79764) ;
#68912 = AXIS2_PLACEMENT_3D('',#102054,#79768,#79769) ;
#68913 = AXIS2_PLACEMENT_3D('',#102060,#79773,#79774) ;
#68914 = AXIS2_PLACEMENT_3D('',#102063,#79775,#79776) ;
#68915 = AXIS2_PLACEMENT_3D('',#102068,#79779,#79780) ;
#68916 = AXIS2_PLACEMENT_3D('',#102070,#79781,#79782) ;
#68917 = AXIS2_PLACEMENT_3D('',#102072,#79784,#79785) ;
#68918 = AXIS2_PLACEMENT_3D('',#102075,#79786,#79787) ;
#68919 = AXIS2_PLACEMENT_3D('',#102080,#79791,#79792) ;
#68920 = AXIS2_PLACEMENT_3D('',#102086,#79796,#79797) ;
#68921 = AXIS2_PLACEMENT_3D('',#102089,#79798,#79799) ;
#68922 = AXIS2_PLACEMENT_3D('',#102093,#79801,#79802) ;
#68923 = AXIS2_PLACEMENT_3D('',#102095,#79804,#79805) ;
#68924 = AXIS2_PLACEMENT_3D('',#102104,#79810,#79811) ;
#68925 = AXIS2_PLACEMENT_3D('',#102107,#79812,#79813) ;
#68926 = AXIS2_PLACEMENT_3D('',#102111,#79815,#79816) ;
#68927 = AXIS2_PLACEMENT_3D('',#102113,#79818,#79819) ;
#68928 = AXIS2_PLACEMENT_3D('',#102119,#79823,#79824) ;
#68929 = AXIS2_PLACEMENT_3D('',#102128,#79829,#79830) ;
#68930 = AXIS2_PLACEMENT_3D('',#102135,#79834,#79835) ;
#68931 = AXIS2_PLACEMENT_3D('',#102136,#79836,#79837) ;
#68932 = AXIS2_PLACEMENT_3D('',#102145,#79842,#79843) ;
#68933 = AXIS2_PLACEMENT_3D('',#102148,#79844,#79845) ;
#68934 = AXIS2_PLACEMENT_3D('',#102153,#79848,#79849) ;
#68935 = AXIS2_PLACEMENT_3D('',#102157,#79851,#79852) ;
#68936 = AXIS2_PLACEMENT_3D('',#102159,#79854,#79855) ;
#68937 = AXIS2_PLACEMENT_3D('',#102167,#79860,#79861) ;
#68938 = AXIS2_PLACEMENT_3D('',#102176,#79866,#79867) ;
#68939 = AXIS2_PLACEMENT_3D('',#102185,#79872,#79873) ;
#68940 = AXIS2_PLACEMENT_3D('',#102194,#79878,#79879) ;
#68941 = AXIS2_PLACEMENT_3D('',#102200,#79883,#79884) ;
#68942 = AXIS2_PLACEMENT_3D('',#102206,#79888,#79889) ;
#68943 = AXIS2_PLACEMENT_3D('',#102212,#79893,#79894) ;
#68944 = AXIS2_PLACEMENT_3D('',#102218,#79898,#79899) ;
#68945 = AXIS2_PLACEMENT_3D('',#102227,#79903,#79904) ;
#68946 = AXIS2_PLACEMENT_3D('',#102230,#79906,#79907) ;
#68947 = AXIS2_PLACEMENT_3D('',#102231,#79908,#79909) ;
#68948 = AXIS2_PLACEMENT_3D('',#102240,#79913,#79914) ;
#68949 = AXIS2_PLACEMENT_3D('',#102243,#79916,#79917) ;
#68950 = AXIS2_PLACEMENT_3D('',#102244,#79918,#79919) ;
#68951 = AXIS2_PLACEMENT_3D('',#102248,#79921,#79922) ;
#68952 = AXIS2_PLACEMENT_3D('',#102249,#79923,#79924) ;
#68953 = AXIS2_PLACEMENT_3D('',#102250,#79925,#79926) ;
#68954 = AXIS2_PLACEMENT_3D('',#102256,#79930,#79931) ;
#68955 = AXIS2_PLACEMENT_3D('',#102265,#79936,#79937) ;
#68956 = AXIS2_PLACEMENT_3D('',#102274,#79942,#79943) ;
#68957 = AXIS2_PLACEMENT_3D('',#102283,#79948,#79949) ;
#68958 = AXIS2_PLACEMENT_3D('',#102292,#79954,#79955) ;
#68959 = AXIS2_PLACEMENT_3D('',#102293,#79956,#79957) ;
#68960 = AXIS2_PLACEMENT_3D('',#102294,#79958,#79959) ;
#68961 = AXIS2_PLACEMENT_3D('',#102295,#79960,#79961) ;
#68962 = AXIS2_PLACEMENT_3D('',#102304,#79966,#79967) ;
#68963 = AXIS2_PLACEMENT_3D('',#102313,#79972,#79973) ;
#68964 = AXIS2_PLACEMENT_3D('',#102322,#79978,#79979) ;
#68965 = AXIS2_PLACEMENT_3D('',#102331,#79984,#79985) ;
#68966 = AXIS2_PLACEMENT_3D('',#102335,#79987,#79988) ;
#68967 = AXIS2_PLACEMENT_3D('',#102337,#79990,#79991) ;
#68968 = AXIS2_PLACEMENT_3D('',#102340,#79992,#79993) ;
#68969 = AXIS2_PLACEMENT_3D('',#102341,#79994,#79995) ;
#68970 = AXIS2_PLACEMENT_3D('',#102342,#79996,#79997) ;
#68971 = AXIS2_PLACEMENT_3D('',#102343,#79998,#79999) ;
#68972 = AXIS2_PLACEMENT_3D('',#102347,#80001,#80002) ;
#68973 = AXIS2_PLACEMENT_3D('',#102349,#80004,#80005) ;
#68974 = AXIS2_PLACEMENT_3D('',#102350,#80006,#80007) ;
#68975 = AXIS2_PLACEMENT_3D('',#102351,#80008,#80009) ;
#68976 = AXIS2_PLACEMENT_3D('',#102352,#80010,#80011) ;
#68977 = AXIS2_PLACEMENT_3D('',#102353,#80012,#80013) ;
#68978 = AXIS2_PLACEMENT_3D('',#102354,#80014,#80015) ;
#68979 = AXIS2_PLACEMENT_3D('',#102355,#80016,#80017) ;
#68980 = AXIS2_PLACEMENT_3D('',#102356,#80018,#80019) ;
#68981 = AXIS2_PLACEMENT_3D('',#102357,#80020,#80021) ;
#68982 = AXIS2_PLACEMENT_3D('',#102358,#80022,#80023) ;
#68983 = AXIS2_PLACEMENT_3D('',#102359,#80024,#80025) ;
#68984 = AXIS2_PLACEMENT_3D('',#102360,#80026,#80027) ;
#68985 = AXIS2_PLACEMENT_3D('',#102361,#80028,#80029) ;
#68986 = AXIS2_PLACEMENT_3D('',#102362,#80030,#80031) ;
#68987 = AXIS2_PLACEMENT_3D('',#102363,#80032,#80033) ;
#68988 = AXIS2_PLACEMENT_3D('',#102364,#80034,#80035) ;
#68989 = AXIS2_PLACEMENT_3D('',#102365,#80036,#80037) ;
#68990 = AXIS2_PLACEMENT_3D('',#102366,#80038,#80039) ;
#68991 = AXIS2_PLACEMENT_3D('',#102367,#80040,#80041) ;
#68992 = AXIS2_PLACEMENT_3D('',#102368,#80042,#80043) ;
#68993 = AXIS2_PLACEMENT_3D('',#102369,#80044,#80045) ;
#68994 = AXIS2_PLACEMENT_3D('',#102370,#80046,#80047) ;
#68995 = AXIS2_PLACEMENT_3D('',#102371,#80048,#80049) ;
#68996 = AXIS2_PLACEMENT_3D('',#102372,#80050,#80051) ;
#68997 = AXIS2_PLACEMENT_3D('',#102373,#80052,#80053) ;
#68998 = AXIS2_PLACEMENT_3D('',#102374,#80054,#80055) ;
#68999 = AXIS2_PLACEMENT_3D('',#102375,#80056,#80057) ;
#69000 = AXIS2_PLACEMENT_3D('',#102376,#80058,#80059) ;
#69001 = AXIS2_PLACEMENT_3D('',#102377,#80060,#80061) ;
#69002 = AXIS2_PLACEMENT_3D('',#102378,#80062,#80063) ;
#69003 = AXIS2_PLACEMENT_3D('',#102379,#80064,#80065) ;
#69004 = AXIS2_PLACEMENT_3D('',#102380,#80066,#80067) ;
#69005 = AXIS2_PLACEMENT_3D('',#102381,#80068,#80069) ;
#69006 = AXIS2_PLACEMENT_3D('',#102382,#80070,#80071) ;
#69007 = AXIS2_PLACEMENT_3D('',#102383,#80072,#80073) ;
#69008 = AXIS2_PLACEMENT_3D('',#102384,#80074,#80075) ;
#69009 = AXIS2_PLACEMENT_3D('',#102385,#80076,#80077) ;
#69010 = AXIS2_PLACEMENT_3D('',#102386,#80078,#80079) ;
#69011 = AXIS2_PLACEMENT_3D('',#102387,#80080,#80081) ;
#69012 = AXIS2_PLACEMENT_3D('',#102388,#80082,#80083) ;
#69013 = AXIS2_PLACEMENT_3D('',#102389,#80084,#80085) ;
#69014 = AXIS2_PLACEMENT_3D('',#102390,#80086,#80087) ;
#69015 = AXIS2_PLACEMENT_3D('',#102391,#80088,#80089) ;
#69016 = AXIS2_PLACEMENT_3D('',#102392,#80090,#80091) ;
#69017 = AXIS2_PLACEMENT_3D('',#102393,#80092,#80093) ;
#69018 = AXIS2_PLACEMENT_3D('',#102394,#80094,#80095) ;
#69019 = AXIS2_PLACEMENT_3D('',#102395,#80096,#80097) ;
#69020 = AXIS2_PLACEMENT_3D('',#102396,#80098,#80099) ;
#69021 = AXIS2_PLACEMENT_3D('',#102397,#80100,#80101) ;
#69022 = AXIS2_PLACEMENT_3D('',#102398,#80102,#80103) ;
#69023 = AXIS2_PLACEMENT_3D('',#102399,#80104,#80105) ;
#69024 = AXIS2_PLACEMENT_3D('',#102400,#80106,#80107) ;
#69025 = AXIS2_PLACEMENT_3D('',#102401,#80108,#80109) ;
#69026 = AXIS2_PLACEMENT_3D('',#102402,#80110,#80111) ;
#69027 = AXIS2_PLACEMENT_3D('',#102403,#80112,#80113) ;
#69028 = AXIS2_PLACEMENT_3D('',#102404,#80114,#80115) ;
#69029 = AXIS2_PLACEMENT_3D('',#102405,#80116,#80117) ;
#69030 = AXIS2_PLACEMENT_3D('',#102406,#80118,#80119) ;
#69031 = AXIS2_PLACEMENT_3D('',#102407,#80120,#80121) ;
#69032 = AXIS2_PLACEMENT_3D('',#102408,#80122,#80123) ;
#69033 = AXIS2_PLACEMENT_3D('',#102409,#80124,#80125) ;
#69034 = AXIS2_PLACEMENT_3D('',#102410,#80126,#80127) ;
#69035 = AXIS2_PLACEMENT_3D('',#102411,#80128,#80129) ;
#69036 = AXIS2_PLACEMENT_3D('',#102412,#80130,#80131) ;
#69037 = AXIS2_PLACEMENT_3D('',#102413,#80132,#80133) ;
#69038 = AXIS2_PLACEMENT_3D('',#102414,#80134,#80135) ;
#69039 = AXIS2_PLACEMENT_3D('',#102415,#80136,#80137) ;
#69040 = AXIS2_PLACEMENT_3D('',#102416,#80138,#80139) ;
#69041 = AXIS2_PLACEMENT_3D('',#102417,#80140,#80141) ;
#69042 = AXIS2_PLACEMENT_3D('',#102418,#80142,#80143) ;
#69043 = AXIS2_PLACEMENT_3D('',#102419,#80144,#80145) ;
#69044 = AXIS2_PLACEMENT_3D('',#102420,#80146,#80147) ;
#69045 = AXIS2_PLACEMENT_3D('',#102421,#80148,#80149) ;
#69046 = AXIS2_PLACEMENT_3D('',#102422,#80150,#80151) ;
#69047 = AXIS2_PLACEMENT_3D('',#102438,#80152,#80153) ;
#69048 = AXIS2_PLACEMENT_3D('',#102439,#80154,#80155) ;
#69049 = AXIS2_PLACEMENT_3D('',#102441,#80156,#80157) ;
#69050 = AXIS2_PLACEMENT_3D('',#102456,#80158,#80159) ;
#69051 = AXIS2_PLACEMENT_3D('',#102457,#80160,#80161) ;
#69052 = AXIS2_PLACEMENT_3D('',#102458,#80162,#80163) ;
#69053 = AXIS2_PLACEMENT_3D('',#102460,#80164,#80165) ;
#69054 = AXIS2_PLACEMENT_3D('',#102490,#80166,#80167) ;
#69055 = AXIS2_PLACEMENT_3D('',#102491,#80168,#80169) ;
#69056 = AXIS2_PLACEMENT_3D('',#102507,#80170,#80171) ;
#69057 = AXIS2_PLACEMENT_3D('',#102509,#80172,#80173) ;
#69058 = AXIS2_PLACEMENT_3D('',#102524,#80174,#80175) ;
#69059 = AXIS2_PLACEMENT_3D('',#102525,#80176,#80177) ;
#69060 = AXIS2_PLACEMENT_3D('',#102526,#80178,#80179) ;
#69061 = AXIS2_PLACEMENT_3D('',#102527,#80180,#80181) ;
#69062 = AXIS2_PLACEMENT_3D('',#102530,#80183,#80184) ;
#69063 = AXIS2_PLACEMENT_3D('',#102531,#80185,#80186) ;
#69064 = AXIS2_PLACEMENT_3D('',#102533,#80187,#80188) ;
#69065 = AXIS2_PLACEMENT_3D('',#102534,#80189,#80190) ;
#69066 = AXIS2_PLACEMENT_3D('',#102535,#80191,#80192) ;
#69067 = AXIS2_PLACEMENT_3D('',#102537,#80193,#80194) ;
#69068 = AXIS2_PLACEMENT_3D('',#102552,#80195,#80196) ;
#69069 = AXIS2_PLACEMENT_3D('',#102553,#80197,#80198) ;
#69070 = AXIS2_PLACEMENT_3D('',#102569,#80199,#80200) ;
#69071 = AXIS2_PLACEMENT_3D('',#102570,#80201,#80202) ;
#69072 = AXIS2_PLACEMENT_3D('',#102571,#80203,#80204) ;
#69073 = AXIS2_PLACEMENT_3D('',#102573,#80205,#80206) ;
#69074 = AXIS2_PLACEMENT_3D('',#102575,#80208,#80209) ;
#69075 = AXIS2_PLACEMENT_3D('',#102576,#80210,#80211) ;
#69076 = AXIS2_PLACEMENT_3D('',#102577,#80212,#80213) ;
#69077 = AXIS2_PLACEMENT_3D('',#102578,#80214,#80215) ;
#69078 = AXIS2_PLACEMENT_3D('',#102579,#80216,#80217) ;
#69079 = AXIS2_PLACEMENT_3D('',#102580,#80218,#80219) ;
#69080 = AXIS2_PLACEMENT_3D('',#102583,#80221,#80222) ;
#69081 = AXIS2_PLACEMENT_3D('',#102584,#80223,#80224) ;
#69082 = AXIS2_PLACEMENT_3D('',#102585,#80225,#80226) ;
#69083 = AXIS2_PLACEMENT_3D('',#102586,#80227,#80228) ;
#69084 = AXIS2_PLACEMENT_3D('',#102588,#80229,#80230) ;
#69085 = AXIS2_PLACEMENT_3D('',#102589,#80231,#80232) ;
#69086 = AXIS2_PLACEMENT_3D('',#102590,#80233,#80234) ;
#69087 = AXIS2_PLACEMENT_3D('',#102591,#80235,#80236) ;
#69088 = AXIS2_PLACEMENT_3D('',#102592,#80237,#80238) ;
#69089 = AXIS2_PLACEMENT_3D('',#102593,#80239,#80240) ;
#69090 = AXIS2_PLACEMENT_3D('',#102594,#80241,#80242) ;
#69091 = AXIS2_PLACEMENT_3D('',#102596,#80243,#80244) ;
#69092 = AXIS2_PLACEMENT_3D('',#102597,#80245,#80246) ;
#69093 = AXIS2_PLACEMENT_3D('',#102598,#80247,#80248) ;
#69094 = AXIS2_PLACEMENT_3D('',#102599,#80249,#80250) ;
#69095 = AXIS2_PLACEMENT_3D('',#102600,#80251,#80252) ;
#69096 = AXIS2_PLACEMENT_3D('',#102602,#80253,#80254) ;
#69097 = AXIS2_PLACEMENT_3D('',#102604,#80256,#80257) ;
#69098 = AXIS2_PLACEMENT_3D('',#102605,#80258,#80259) ;
#69099 = AXIS2_PLACEMENT_3D('',#102606,#80260,#80261) ;
#69100 = AXIS2_PLACEMENT_3D('',#102607,#80262,#80263) ;
#69101 = AXIS2_PLACEMENT_3D('',#102608,#80264,#80265) ;
#69102 = AXIS2_PLACEMENT_3D('',#102610,#80267,#80268) ;
#69103 = AXIS2_PLACEMENT_3D('',#102611,#80269,#80270) ;
#69104 = AXIS2_PLACEMENT_3D('',#102612,#80271,#80272) ;
#69105 = AXIS2_PLACEMENT_3D('',#102613,#80273,#80274) ;
#69106 = AXIS2_PLACEMENT_3D('',#102615,#80275,#80276) ;
#69107 = AXIS2_PLACEMENT_3D('',#102616,#80277,#80278) ;
#69108 = AXIS2_PLACEMENT_3D('',#102617,#80279,#80280) ;
#69109 = AXIS2_PLACEMENT_3D('',#102618,#80281,#80282) ;
#69110 = AXIS2_PLACEMENT_3D('',#102619,#80283,#80284) ;
#69111 = AXIS2_PLACEMENT_3D('',#102620,#80285,#80286) ;
#69112 = AXIS2_PLACEMENT_3D('',#102621,#80287,#80288) ;
#69113 = AXIS2_PLACEMENT_3D('',#102623,#80290,#80291) ;
#69114 = AXIS2_PLACEMENT_3D('',#102624,#80292,#80293) ;
#69115 = AXIS2_PLACEMENT_3D('',#102625,#80294,#80295) ;
#69116 = AXIS2_PLACEMENT_3D('',#102626,#80296,#80297) ;
#69117 = AXIS2_PLACEMENT_3D('',#102627,#80298,#80299) ;
#69118 = AXIS2_PLACEMENT_3D('',#102628,#80300,#80301) ;
#69119 = AXIS2_PLACEMENT_3D('',#102629,#80302,#80303) ;
#69120 = AXIS2_PLACEMENT_3D('',#102630,#80304,#80305) ;
#69121 = AXIS2_PLACEMENT_3D('',#102631,#80306,#80307) ;
#69122 = AXIS2_PLACEMENT_3D('',#102632,#80308,#80309) ;
#69123 = AXIS2_PLACEMENT_3D('',#102633,#80310,#80311) ;
#69124 = AXIS2_PLACEMENT_3D('',#102634,#80312,#80313) ;
#69125 = AXIS2_PLACEMENT_3D('',#102635,#80314,#80315) ;
#69126 = AXIS2_PLACEMENT_3D('',#102636,#80316,#80317) ;
#69127 = AXIS2_PLACEMENT_3D('',#102637,#80318,#80319) ;
#69128 = AXIS2_PLACEMENT_3D('',#102638,#80320,#80321) ;
#69129 = AXIS2_PLACEMENT_3D('',#102639,#80322,#80323) ;
#69130 = AXIS2_PLACEMENT_3D('',#102640,#80324,#80325) ;
#69131 = AXIS2_PLACEMENT_3D('',#102641,#80326,#80327) ;
#69132 = AXIS2_PLACEMENT_3D('',#102642,#80328,#80329) ;
#69133 = AXIS2_PLACEMENT_3D('',#102643,#80330,#80331) ;
#69134 = AXIS2_PLACEMENT_3D('',#102644,#80332,#80333) ;
#69135 = AXIS2_PLACEMENT_3D('',#102645,#80334,#80335) ;
#69136 = AXIS2_PLACEMENT_3D('',#102646,#80336,#80337) ;
#69137 = AXIS2_PLACEMENT_3D('',#102647,#80338,#80339) ;
#69138 = AXIS2_PLACEMENT_3D('',#102648,#80340,#80341) ;
#69139 = AXIS2_PLACEMENT_3D('',#102649,#80342,#80343) ;
#69140 = AXIS2_PLACEMENT_3D('',#102650,#80344,#80345) ;
#69141 = AXIS2_PLACEMENT_3D('',#102651,#80346,#80347) ;
#69142 = AXIS2_PLACEMENT_3D('',#102652,#80348,#80349) ;
#69143 = AXIS2_PLACEMENT_3D('',#102653,#80350,#80351) ;
#69144 = AXIS2_PLACEMENT_3D('',#102654,#80352,#80353) ;
#69145 = AXIS2_PLACEMENT_3D('',#102655,#80354,#80355) ;
#69146 = AXIS2_PLACEMENT_3D('',#102656,#80356,#80357) ;
#69147 = AXIS2_PLACEMENT_3D('',#102657,#80358,#80359) ;
#69148 = AXIS2_PLACEMENT_3D('',#102658,#80360,#80361) ;
#69149 = AXIS2_PLACEMENT_3D('',#102659,#80362,#80363) ;
#69150 = AXIS2_PLACEMENT_3D('',#102660,#80364,#80365) ;
#69151 = AXIS2_PLACEMENT_3D('',#102661,#80366,#80367) ;
#69152 = AXIS2_PLACEMENT_3D('',#102662,#80368,#80369) ;
#69153 = AXIS2_PLACEMENT_3D('',#102663,#80370,#80371) ;
#69154 = AXIS2_PLACEMENT_3D('',#102664,#80372,#80373) ;
#69155 = AXIS2_PLACEMENT_3D('',#102665,#80374,#80375) ;
#69156 = AXIS2_PLACEMENT_3D('',#102666,#80376,#80377) ;
#69157 = AXIS2_PLACEMENT_3D('',#102667,#80378,#80379) ;
#69158 = AXIS2_PLACEMENT_3D('',#102668,#80380,#80381) ;
#69159 = AXIS2_PLACEMENT_3D('',#102669,#80382,#80383) ;
#69160 = AXIS2_PLACEMENT_3D('',#102670,#80384,#80385) ;
#69161 = AXIS2_PLACEMENT_3D('',#102671,#80386,#80387) ;
#69162 = AXIS2_PLACEMENT_3D('',#102672,#80388,#80389) ;
#69163 = AXIS2_PLACEMENT_3D('',#102689,#80390,#80391) ;
#69164 = AXIS2_PLACEMENT_3D('',#102690,#80392,#80393) ;
#69165 = AXIS2_PLACEMENT_3D('',#102691,#80394,#80395) ;
#69166 = AXIS2_PLACEMENT_3D('',#102692,#80396,#80397) ;
#69167 = AXIS2_PLACEMENT_3D('',#102693,#80398,#80399) ;
#69168 = AXIS2_PLACEMENT_3D('',#102694,#80400,#80401) ;
#69169 = AXIS2_PLACEMENT_3D('',#102695,#80402,#80403) ;
#69170 = AXIS2_PLACEMENT_3D('',#102696,#80404,#80405) ;
#69171 = AXIS2_PLACEMENT_3D('',#102697,#80406,#80407) ;
#69172 = AXIS2_PLACEMENT_3D('',#102698,#80408,#80409) ;
#69173 = AXIS2_PLACEMENT_3D('',#102699,#80410,#80411) ;
#69174 = AXIS2_PLACEMENT_3D('',#102718,#80412,#80413) ;
#69175 = AXIS2_PLACEMENT_3D('',#102719,#80414,#80415) ;
#69176 = AXIS2_PLACEMENT_3D('',#102721,#80416,#80417) ;
#69177 = AXIS2_PLACEMENT_3D('',#102722,#80418,#80419) ;
#69178 = AXIS2_PLACEMENT_3D('',#102723,#80420,#80421) ;
#69179 = AXIS2_PLACEMENT_3D('',#102724,#80422,#80423) ;
#69180 = AXIS2_PLACEMENT_3D('',#102725,#80424,#80425) ;
#69181 = AXIS2_PLACEMENT_3D('',#102726,#80426,#80427) ;
#69182 = AXIS2_PLACEMENT_3D('',#102727,#80428,#80429) ;
#69183 = AXIS2_PLACEMENT_3D('',#102728,#80430,#80431) ;
#69184 = AXIS2_PLACEMENT_3D('',#102729,#80432,#80433) ;
#69185 = AXIS2_PLACEMENT_3D('',#102730,#80434,#80435) ;
#69186 = AXIS2_PLACEMENT_3D('',#102731,#80436,#80437) ;
#69187 = AXIS2_PLACEMENT_3D('',#102766,#80438,#80439) ;
#69188 = AXIS2_PLACEMENT_3D('',#102767,#80440,#80441) ;
#69189 = AXIS2_PLACEMENT_3D('',#102768,#80442,#80443) ;
#69190 = AXIS2_PLACEMENT_3D('',#102769,#80444,#80445) ;
#69191 = AXIS2_PLACEMENT_3D('',#102780,#80446,#80447) ;
#69192 = AXIS2_PLACEMENT_3D('',#102781,#80448,#80449) ;
#69193 = AXIS2_PLACEMENT_3D('',#102782,#80450,#80451) ;
#69194 = AXIS2_PLACEMENT_3D('',#102783,#80452,#80453) ;
#69195 = AXIS2_PLACEMENT_3D('',#102790,#80454,#80455) ;
#69196 = AXIS2_PLACEMENT_3D('',#102791,#80456,#80457) ;
#69197 = AXIS2_PLACEMENT_3D('',#102792,#80458,#80459) ;
#69198 = AXIS2_PLACEMENT_3D('',#102793,#80460,#80461) ;
#69199 = AXIS2_PLACEMENT_3D('',#102794,#80462,#80463) ;
#69200 = AXIS2_PLACEMENT_3D('',#102805,#80464,#80465) ;
#69201 = AXIS2_PLACEMENT_3D('',#102806,#80466,#80467) ;
#69202 = AXIS2_PLACEMENT_3D('',#102807,#80468,#80469) ;
#69203 = AXIS2_PLACEMENT_3D('',#102808,#80470,#80471) ;
#69204 = AXIS2_PLACEMENT_3D('',#102809,#80472,#80473) ;
#69205 = AXIS2_PLACEMENT_3D('',#102810,#80474,#80475) ;
#69206 = AXIS2_PLACEMENT_3D('',#102811,#80476,#80477) ;
#69207 = AXIS2_PLACEMENT_3D('',#102812,#80478,#80479) ;
#69208 = AXIS2_PLACEMENT_3D('',#102813,#80480,#80481) ;
#69209 = AXIS2_PLACEMENT_3D('',#102814,#80482,#80483) ;
#69210 = AXIS2_PLACEMENT_3D('',#102815,#80484,#80485) ;
#69211 = AXIS2_PLACEMENT_3D('',#102816,#80486,#80487) ;
#69212 = AXIS2_PLACEMENT_3D('',#102817,#80488,#80489) ;
#69213 = AXIS2_PLACEMENT_3D('',#102818,#80490,#80491) ;
#69214 = AXIS2_PLACEMENT_3D('',#102819,#80492,#80493) ;
#69215 = AXIS2_PLACEMENT_3D('',#102820,#80494,#80495) ;
#69216 = AXIS2_PLACEMENT_3D('',#102821,#80496,#80497) ;
#69217 = AXIS2_PLACEMENT_3D('',#102822,#80498,#80499) ;
#69218 = AXIS2_PLACEMENT_3D('',#102823,#80500,#80501) ;
#69219 = AXIS2_PLACEMENT_3D('',#102824,#80502,#80503) ;
#69220 = AXIS2_PLACEMENT_3D('',#102825,#80504,#80505) ;
#69221 = AXIS2_PLACEMENT_3D('',#102826,#80506,#80507) ;
#69222 = AXIS2_PLACEMENT_3D('',#102827,#80508,#80509) ;
#69223 = AXIS2_PLACEMENT_3D('',#102828,#80510,#80511) ;
#69224 = AXIS2_PLACEMENT_3D('',#102829,#80512,#80513) ;
#69225 = AXIS2_PLACEMENT_3D('',#102830,#80514,#80515) ;
#69226 = AXIS2_PLACEMENT_3D('',#102831,#80516,#80517) ;
#69227 = AXIS2_PLACEMENT_3D('',#102832,#80518,#80519) ;
#69228 = AXIS2_PLACEMENT_3D('',#102833,#80520,#80521) ;
#69229 = AXIS2_PLACEMENT_3D('',#102834,#80522,#80523) ;
#69230 = AXIS2_PLACEMENT_3D('',#102835,#80524,#80525) ;
#69231 = AXIS2_PLACEMENT_3D('',#102836,#80526,#80527) ;
#69232 = AXIS2_PLACEMENT_3D('',#102837,#80528,#80529) ;
#69233 = AXIS2_PLACEMENT_3D('',#102838,#80530,#80531) ;
#69234 = AXIS2_PLACEMENT_3D('',#102845,#80532,#80533) ;
#69235 = AXIS2_PLACEMENT_3D('',#102846,#80534,#80535) ;
#69236 = AXIS2_PLACEMENT_3D('',#102847,#80536,#80537) ;
#69237 = AXIS2_PLACEMENT_3D('',#102848,#80538,#80539) ;
#69238 = AXIS2_PLACEMENT_3D('',#102849,#80540,#80541) ;
#69239 = AXIS2_PLACEMENT_3D('',#102850,#80542,#80543) ;
#69240 = AXIS2_PLACEMENT_3D('',#102851,#80544,#80545) ;
#69241 = AXIS2_PLACEMENT_3D('',#102852,#80546,#80547) ;
#69242 = AXIS2_PLACEMENT_3D('',#102853,#80548,#80549) ;
#69243 = AXIS2_PLACEMENT_3D('',#102854,#80550,#80551) ;
#69244 = AXIS2_PLACEMENT_3D('',#102855,#80552,#80553) ;
#69245 = AXIS2_PLACEMENT_3D('',#102856,#80554,#80555) ;
#69246 = AXIS2_PLACEMENT_3D('',#102857,#80556,#80557) ;
#69247 = AXIS2_PLACEMENT_3D('',#102858,#80558,#80559) ;
#69248 = AXIS2_PLACEMENT_3D('',#102859,#80560,#80561) ;
#69249 = AXIS2_PLACEMENT_3D('',#102860,#80562,#80563) ;
#69250 = AXIS2_PLACEMENT_3D('',#102861,#80564,#80565) ;
#69251 = AXIS2_PLACEMENT_3D('',#102862,#80566,#80567) ;
#69252 = AXIS2_PLACEMENT_3D('',#102863,#80568,#80569) ;
#69253 = AXIS2_PLACEMENT_3D('',#102864,#80570,#80571) ;
#69254 = AXIS2_PLACEMENT_3D('',#102865,#80572,#80573) ;
#69255 = AXIS2_PLACEMENT_3D('',#102866,#80574,#80575) ;
#69256 = AXIS2_PLACEMENT_3D('',#102867,#80576,#80577) ;
#69257 = AXIS2_PLACEMENT_3D('',#102868,#80578,#80579) ;
#69258 = AXIS2_PLACEMENT_3D('',#102869,#80580,#80581) ;
#69259 = AXIS2_PLACEMENT_3D('',#102870,#80582,#80583) ;
#69260 = AXIS2_PLACEMENT_3D('',#102871,#80584,#80585) ;
#69261 = AXIS2_PLACEMENT_3D('',#102872,#80586,#80587) ;
#69262 = AXIS2_PLACEMENT_3D('',#102873,#80588,#80589) ;
#69263 = AXIS2_PLACEMENT_3D('',#102874,#80590,#80591) ;
#69264 = AXIS2_PLACEMENT_3D('',#102875,#80592,#80593) ;
#69265 = AXIS2_PLACEMENT_3D('',#102876,#80594,#80595) ;
#69266 = AXIS2_PLACEMENT_3D('',#102877,#80596,#80597) ;
#69267 = AXIS2_PLACEMENT_3D('',#102878,#80598,#80599) ;
#69268 = AXIS2_PLACEMENT_3D('',#102879,#80600,#80601) ;
#69269 = AXIS2_PLACEMENT_3D('',#102880,#80602,#80603) ;
#69270 = AXIS2_PLACEMENT_3D('',#102881,#80604,#80605) ;
#69271 = AXIS2_PLACEMENT_3D('',#102882,#80606,#80607) ;
#69272 = AXIS2_PLACEMENT_3D('',#102883,#80608,#80609) ;
#69273 = AXIS2_PLACEMENT_3D('',#102914,#80610,#80611) ;
#69274 = AXIS2_PLACEMENT_3D('',#102915,#80612,#80613) ;
#69275 = AXIS2_PLACEMENT_3D('',#102916,#80614,#80615) ;
#69276 = AXIS2_PLACEMENT_3D('',#102917,#80616,#80617) ;
#69277 = AXIS2_PLACEMENT_3D('',#102918,#80618,#80619) ;
#69278 = AXIS2_PLACEMENT_3D('',#102919,#80620,#80621) ;
#69279 = AXIS2_PLACEMENT_3D('',#102920,#80622,#80623) ;
#69280 = AXIS2_PLACEMENT_3D('',#102921,#80624,#80625) ;
#69281 = AXIS2_PLACEMENT_3D('',#102922,#80626,#80627) ;
#69282 = AXIS2_PLACEMENT_3D('',#102923,#80628,#80629) ;
#69283 = AXIS2_PLACEMENT_3D('',#102950,#80630,#80631) ;
#69284 = AXIS2_PLACEMENT_3D('',#102951,#80632,#80633) ;
#69285 = AXIS2_PLACEMENT_3D('',#102952,#80634,#80635) ;
#69286 = AXIS2_PLACEMENT_3D('',#102953,#80636,#80637) ;
#69287 = AXIS2_PLACEMENT_3D('',#102954,#80638,#80639) ;
#69288 = AXIS2_PLACEMENT_3D('',#102955,#80640,#80641) ;
#69289 = AXIS2_PLACEMENT_3D('',#102956,#80642,#80643) ;
#69290 = AXIS2_PLACEMENT_3D('',#102957,#80644,#80645) ;
#69291 = AXIS2_PLACEMENT_3D('',#102958,#80646,#80647) ;
#69292 = AXIS2_PLACEMENT_3D('',#102959,#80648,#80649) ;
#69293 = AXIS2_PLACEMENT_3D('',#102960,#80650,#80651) ;
#69294 = AXIS2_PLACEMENT_3D('',#102961,#80652,#80653) ;
#69295 = AXIS2_PLACEMENT_3D('',#102962,#80654,#80655) ;
#69296 = AXIS2_PLACEMENT_3D('',#102963,#80656,#80657) ;
#69297 = AXIS2_PLACEMENT_3D('',#102964,#80658,#80659) ;
#69298 = AXIS2_PLACEMENT_3D('',#102965,#80660,#80661) ;
#69299 = AXIS2_PLACEMENT_3D('',#102966,#80662,#80663) ;
#69300 = AXIS2_PLACEMENT_3D('',#102967,#80664,#80665) ;
#69301 = AXIS2_PLACEMENT_3D('',#102968,#80666,#80667) ;
#69302 = AXIS2_PLACEMENT_3D('',#102969,#80668,#80669) ;
#69303 = AXIS2_PLACEMENT_3D('',#102970,#80670,#80671) ;
#69304 = AXIS2_PLACEMENT_3D('',#102971,#80672,#80673) ;
#69305 = AXIS2_PLACEMENT_3D('',#102972,#80674,#80675) ;
#69306 = AXIS2_PLACEMENT_3D('',#102973,#80676,#80677) ;
#69307 = AXIS2_PLACEMENT_3D('',#102974,#80678,#80679) ;
#69308 = AXIS2_PLACEMENT_3D('',#102975,#80680,#80681) ;
#69309 = AXIS2_PLACEMENT_3D('',#102976,#80682,#80683) ;
#69310 = AXIS2_PLACEMENT_3D('',#102977,#80684,#80685) ;
#69311 = AXIS2_PLACEMENT_3D('',#102978,#80686,#80687) ;
#69312 = AXIS2_PLACEMENT_3D('',#103003,#80688,#80689) ;
#69313 = AXIS2_PLACEMENT_3D('',#103004,#80690,#80691) ;
#69314 = AXIS2_PLACEMENT_3D('',#103005,#80692,#80693) ;
#69315 = AXIS2_PLACEMENT_3D('',#103006,#80694,#80695) ;
#69316 = AXIS2_PLACEMENT_3D('',#103007,#80696,#80697) ;
#69317 = AXIS2_PLACEMENT_3D('',#103008,#80698,#80699) ;
#69318 = AXIS2_PLACEMENT_3D('',#103009,#80700,#80701) ;
#69319 = AXIS2_PLACEMENT_3D('',#103058,#80702,#80703) ;
#69320 = AXIS2_PLACEMENT_3D('',#103059,#80704,#80705) ;
#69321 = AXIS2_PLACEMENT_3D('',#103060,#80706,#80707) ;
#69322 = AXIS2_PLACEMENT_3D('',#103061,#80708,#80709) ;
#69323 = AXIS2_PLACEMENT_3D('',#103062,#80710,#80711) ;
#69324 = AXIS2_PLACEMENT_3D('',#103063,#80712,#80713) ;
#69325 = AXIS2_PLACEMENT_3D('',#103064,#80714,#80715) ;
#69326 = AXIS2_PLACEMENT_3D('',#103126,#80716,#80717) ;
#69327 = AXIS2_PLACEMENT_3D('',#103127,#80718,#80719) ;
#69328 = AXIS2_PLACEMENT_3D('',#103128,#80720,#80721) ;
#69329 = AXIS2_PLACEMENT_3D('',#103301,#80722,#80723) ;
#69330 = AXIS2_PLACEMENT_3D('',#103302,#80724,#80725) ;
#69331 = AXIS2_PLACEMENT_3D('',#103357,#80726,#80727) ;
#69332 = AXIS2_PLACEMENT_3D('',#103404,#80728,#80729) ;
#69333 = AXIS2_PLACEMENT_3D('',#103405,#80730,#80731) ;
#69334 = AXIS2_PLACEMENT_3D('',#103406,#80732,#80733) ;
#69335 = AXIS2_PLACEMENT_3D('',#103407,#80734,#80735) ;
#69336 = AXIS2_PLACEMENT_3D('',#103408,#80736,#80737) ;
#69337 = AXIS2_PLACEMENT_3D('',#103409,#80738,#80739) ;
#69338 = AXIS2_PLACEMENT_3D('',#103514,#80740,#80741) ;
#69339 = AXIS2_PLACEMENT_3D('',#103515,#80742,#80743) ;
#69340 = AXIS2_PLACEMENT_3D('',#103516,#80744,#80745) ;
#69341 = AXIS2_PLACEMENT_3D('',#103517,#80746,#80747) ;
#69342 = AXIS2_PLACEMENT_3D('',#103530,#80748,#80749) ;
#69343 = AXIS2_PLACEMENT_3D('',#103531,#80750,#80751) ;
#69344 = AXIS2_PLACEMENT_3D('',#103532,#80752,#80753) ;
#69345 = AXIS2_PLACEMENT_3D('',#103533,#80754,#80755) ;
#69346 = AXIS2_PLACEMENT_3D('',#103534,#80756,#80757) ;
#69347 = AXIS2_PLACEMENT_3D('',#103535,#80758,#80759) ;
#69348 = AXIS2_PLACEMENT_3D('',#103536,#80760,#80761) ;
#69349 = AXIS2_PLACEMENT_3D('',#103537,#80762,#80763) ;
#69350 = AXIS2_PLACEMENT_3D('',#103538,#80764,#80765) ;
#69351 = AXIS2_PLACEMENT_3D('',#103539,#80766,#80767) ;
#69352 = AXIS2_PLACEMENT_3D('',#103540,#80768,#80769) ;
#69353 = AXIS2_PLACEMENT_3D('',#103541,#80770,#80771) ;
#69354 = AXIS2_PLACEMENT_3D('',#103542,#80772,#80773) ;
#69355 = AXIS2_PLACEMENT_3D('',#103543,#80774,#80775) ;
#69356 = AXIS2_PLACEMENT_3D('',#103544,#80776,#80777) ;
#69357 = AXIS2_PLACEMENT_3D('',#103545,#80778,#80779) ;
#69358 = AXIS2_PLACEMENT_3D('',#103546,#80780,#80781) ;
#69359 = AXIS2_PLACEMENT_3D('',#103547,#80782,#80783) ;
#69360 = AXIS2_PLACEMENT_3D('',#103548,#80784,#80785) ;
#69361 = AXIS2_PLACEMENT_3D('',#103549,#80786,#80787) ;
#69362 = AXIS2_PLACEMENT_3D('',#103550,#80788,#80789) ;
#69363 = AXIS2_PLACEMENT_3D('',#103551,#80790,#80791) ;
#69364 = AXIS2_PLACEMENT_3D('',#103552,#80792,#80793) ;
#69365 = AXIS2_PLACEMENT_3D('',#103553,#80794,#80795) ;
#69366 = AXIS2_PLACEMENT_3D('',#103554,#80796,#80797) ;
#69367 = AXIS2_PLACEMENT_3D('',#103555,#80798,#80799) ;
#69368 = AXIS2_PLACEMENT_3D('',#103556,#80800,#80801) ;
#69369 = AXIS2_PLACEMENT_3D('',#103557,#80802,#80803) ;
#69370 = AXIS2_PLACEMENT_3D('',#103558,#80804,#80805) ;
#69371 = AXIS2_PLACEMENT_3D('',#103559,#80806,#80807) ;
#69372 = AXIS2_PLACEMENT_3D('',#103560,#80808,#80809) ;
#69373 = AXIS2_PLACEMENT_3D('',#103561,#80810,#80811) ;
#69374 = AXIS2_PLACEMENT_3D('',#103562,#80812,#80813) ;
#69375 = AXIS2_PLACEMENT_3D('',#103563,#80814,#80815) ;
#69376 = AXIS2_PLACEMENT_3D('',#103564,#80816,#80817) ;
#69377 = AXIS2_PLACEMENT_3D('',#103565,#80818,#80819) ;
#69378 = AXIS2_PLACEMENT_3D('',#103566,#80820,#80821) ;
#69379 = AXIS2_PLACEMENT_3D('',#103567,#80822,#80823) ;
#69380 = AXIS2_PLACEMENT_3D('',#103580,#80824,#80825) ;
#69381 = AXIS2_PLACEMENT_3D('',#103581,#80826,#80827) ;
#69382 = AXIS2_PLACEMENT_3D('',#103582,#80828,#80829) ;
#69383 = AXIS2_PLACEMENT_3D('',#103583,#80830,#80831) ;
#69384 = AXIS2_PLACEMENT_3D('',#103638,#80832,#80833) ;
#69385 = AXIS2_PLACEMENT_3D('',#103639,#80834,#80835) ;
#69386 = AXIS2_PLACEMENT_3D('',#103640,#80836,#80837) ;
#69387 = AXIS2_PLACEMENT_3D('',#103695,#80838,#80839) ;
#69388 = AXIS2_PLACEMENT_3D('',#103696,#80840,#80841) ;
#69389 = AXIS2_PLACEMENT_3D('',#103722,#80842,#80843) ;
#69390 = AXIS2_PLACEMENT_3D('',#103724,#80844,#80845) ;
#69391 = AXIS2_PLACEMENT_3D('',#103726,#80846,#80847) ;
#69392 = AXIS2_PLACEMENT_3D('',#103765,#80848,#80849) ;
#69393 = AXIS2_PLACEMENT_3D('',#103767,#80850,#80851) ;
#69394 = AXIS2_PLACEMENT_3D('',#103769,#80852,#80853) ;
#69395 = AXIS2_PLACEMENT_3D('',#103770,#80854,#80855) ;
#69396 = AXIS2_PLACEMENT_3D('',#103771,#80856,#80857) ;
#69397 = AXIS2_PLACEMENT_3D('',#103773,#80858,#80859) ;
#69398 = AXIS2_PLACEMENT_3D('',#103775,#80860,#80861) ;
#69399 = AXIS2_PLACEMENT_3D('',#103776,#80862,#80863) ;
#69400 = AXIS2_PLACEMENT_3D('',#103777,#80864,#80865) ;
#69401 = AXIS2_PLACEMENT_3D('',#103779,#80866,#80867) ;
#69402 = AXIS2_PLACEMENT_3D('',#103781,#80868,#80869) ;
#69403 = AXIS2_PLACEMENT_3D('',#103782,#80870,#80871) ;
#69404 = AXIS2_PLACEMENT_3D('',#103783,#80872,#80873) ;
#69405 = AXIS2_PLACEMENT_3D('',#103786,#80874,#80875) ;
#69406 = AXIS2_PLACEMENT_3D('',#103790,#80877,#80878) ;
#69407 = AXIS2_PLACEMENT_3D('',#103792,#80879,#80880) ;
#69408 = AXIS2_PLACEMENT_3D('',#103794,#80882,#80883) ;
#69409 = AXIS2_PLACEMENT_3D('',#103797,#80884,#80885) ;
#69410 = AXIS2_PLACEMENT_3D('',#103801,#80887,#80888) ;
#69411 = AXIS2_PLACEMENT_3D('',#103803,#80890,#80891) ;
#69412 = AXIS2_PLACEMENT_3D('',#103806,#80892,#80893) ;
#69413 = AXIS2_PLACEMENT_3D('',#103808,#80894,#80895) ;
#69414 = AXIS2_PLACEMENT_3D('',#103810,#80896,#80897) ;
#69415 = AXIS2_PLACEMENT_3D('',#103811,#80898,#80899) ;
#69416 = AXIS2_PLACEMENT_3D('',#103812,#80900,#80901) ;
#69417 = AXIS2_PLACEMENT_3D('',#103814,#80903,#80904) ;
#69418 = AXIS2_PLACEMENT_3D('',#103817,#80906,#80907) ;
#69419 = AXIS2_PLACEMENT_3D('',#103826,#80908,#80909) ;
#69420 = AXIS2_PLACEMENT_3D('',#103834,#80910,#80911) ;
#69421 = AXIS2_PLACEMENT_3D('',#103836,#80913,#80914) ;
#69422 = AXIS2_PLACEMENT_3D('',#103852,#80918,#80919) ;
#69423 = AXIS2_PLACEMENT_3D('',#103854,#80921,#80922) ;
#69424 = AXIS2_PLACEMENT_3D('',#103903,#80927,#80928) ;
#69425 = AXIS2_PLACEMENT_3D('',#103912,#80933,#80934) ;
#69426 = AXIS2_PLACEMENT_3D('',#103942,#80939,#80940) ;
#69427 = AXIS2_PLACEMENT_3D('',#103951,#80945,#80946) ;
#69428 = AXIS2_PLACEMENT_3D('',#103960,#80951,#80952) ;
#69429 = AXIS2_PLACEMENT_3D('',#103971,#80957,#80958) ;
#69430 = AXIS2_PLACEMENT_3D('',#103973,#80960,#80961) ;
#69431 = AXIS2_PLACEMENT_3D('',#103977,#80963,#80964) ;
#69432 = AXIS2_PLACEMENT_3D('',#103978,#80965,#80966) ;
#69433 = AXIS2_PLACEMENT_3D('',#103979,#80967,#80968) ;
#69434 = AXIS2_PLACEMENT_3D('',#103981,#80969,#80970) ;
#69435 = AXIS2_PLACEMENT_3D('',#103985,#80972,#80973) ;
#69436 = AXIS2_PLACEMENT_3D('',#103989,#80975,#80976) ;
#69437 = AXIS2_PLACEMENT_3D('',#103993,#80978,#80979) ;
#69438 = AXIS2_PLACEMENT_3D('',#103997,#80981,#80982) ;
#69439 = AXIS2_PLACEMENT_3D('',#104001,#80984,#80985) ;
#69440 = AXIS2_PLACEMENT_3D('',#104004,#80987,#80988) ;
#69441 = AXIS2_PLACEMENT_3D('',#104006,#80989,#80990) ;
#69442 = AXIS2_PLACEMENT_3D('',#104009,#80992,#80993) ;
#69443 = AXIS2_PLACEMENT_3D('',#104011,#80994,#80995) ;
#69444 = AXIS2_PLACEMENT_3D('',#104017,#80998,#80999) ;
#69445 = AXIS2_PLACEMENT_3D('',#104021,#81001,#81002) ;
#69446 = AXIS2_PLACEMENT_3D('',#104024,#81004,#81005) ;
#69447 = AXIS2_PLACEMENT_3D('',#104025,#81006,#81007) ;
#69448 = AXIS2_PLACEMENT_3D('',#104030,#81009,#81010) ;
#69449 = AXIS2_PLACEMENT_3D('',#104034,#81012,#81013) ;
#69450 = AXIS2_PLACEMENT_3D('',#104038,#81015,#81016) ;
#69451 = AXIS2_PLACEMENT_3D('',#104042,#81018,#81019) ;
#69452 = AXIS2_PLACEMENT_3D('',#104047,#81022,#81023) ;
#69453 = AXIS2_PLACEMENT_3D('',#104049,#81024,#81025) ;
#69454 = AXIS2_PLACEMENT_3D('',#104052,#81027,#81028) ;
#69455 = AXIS2_PLACEMENT_3D('',#104054,#81029,#81030) ;
#69456 = AXIS2_PLACEMENT_3D('',#104058,#81032,#81033) ;
#69457 = AXIS2_PLACEMENT_3D('',#104062,#81035,#81036) ;
#69458 = AXIS2_PLACEMENT_3D('',#104066,#81038,#81039) ;
#69459 = AXIS2_PLACEMENT_3D('',#104070,#81041,#81042) ;
#69460 = AXIS2_PLACEMENT_3D('',#104074,#81044,#81045) ;
#69461 = AXIS2_PLACEMENT_3D('',#104078,#81047,#81048) ;
#69462 = AXIS2_PLACEMENT_3D('',#104082,#81050,#81051) ;
#69463 = AXIS2_PLACEMENT_3D('',#104085,#81053,#81054) ;
#69464 = AXIS2_PLACEMENT_3D('',#104086,#81055,#81056) ;
#69465 = AXIS2_PLACEMENT_3D('',#104089,#81059,#81060) ;
#69466 = AXIS2_PLACEMENT_3D('',#104092,#81063,#81064) ;
#69467 = AXIS2_PLACEMENT_3D('',#104181,#81069,#81070) ;
#69468 = AXIS2_PLACEMENT_3D('',#104192,#81071,#81072) ;
#69469 = AXIS2_PLACEMENT_3D('',#104197,#81076,#81077) ;
#69470 = AXIS2_PLACEMENT_3D('',#104203,#81081,#81082) ;
#69471 = AXIS2_PLACEMENT_3D('',#104223,#81086,#81087) ;
#69472 = AXIS2_PLACEMENT_3D('',#104322,#81093,#81094) ;
#69473 = AXIS2_PLACEMENT_3D('',#104326,#81096,#81097) ;
#69474 = AXIS2_PLACEMENT_3D('',#104330,#81100,#81101) ;
#69475 = AXIS2_PLACEMENT_3D('',#104333,#81102,#81103) ;
#69476 = AXIS2_PLACEMENT_3D('',#104338,#81106,#81107) ;
#69477 = AXIS2_PLACEMENT_3D('',#104340,#81108,#81109) ;
#69478 = AXIS2_PLACEMENT_3D('',#104342,#81110,#81111) ;
#69479 = AXIS2_PLACEMENT_3D('',#104350,#81115,#81116) ;
#69480 = AXIS2_PLACEMENT_3D('',#104352,#81117,#81118) ;
#69481 = AXIS2_PLACEMENT_3D('',#104354,#81119,#81120) ;
#69482 = AXIS2_PLACEMENT_3D('',#104359,#81123,#81124) ;
#69483 = AXIS2_PLACEMENT_3D('',#104361,#81125,#81126) ;
#69484 = AXIS2_PLACEMENT_3D('',#104363,#81127,#81128) ;
#69485 = AXIS2_PLACEMENT_3D('',#104367,#81130,#81131) ;
#69486 = AXIS2_PLACEMENT_3D('',#104371,#81133,#81134) ;
#69487 = AXIS2_PLACEMENT_3D('',#104372,#81135,#81136) ;
#69488 = AXIS2_PLACEMENT_3D('',#104373,#81137,#81138) ;
#69489 = AXIS2_PLACEMENT_3D('',#104376,#81139,#81140) ;
#69490 = AXIS2_PLACEMENT_3D('',#104386,#81146,#81147) ;
#69491 = AXIS2_PLACEMENT_3D('',#104388,#81149,#81150) ;
#69492 = AXIS2_PLACEMENT_3D('',#104391,#81151,#81152) ;
#69493 = AXIS2_PLACEMENT_3D('',#104397,#81156,#81157) ;
#69494 = AXIS2_PLACEMENT_3D('',#104399,#81159,#81160) ;
#69495 = AXIS2_PLACEMENT_3D('',#104405,#81163,#81164) ;
#69496 = AXIS2_PLACEMENT_3D('',#104406,#81165,#81166) ;
#69497 = AXIS2_PLACEMENT_3D('',#104409,#81167,#81168) ;
#69498 = AXIS2_PLACEMENT_3D('',#104413,#81171,#81172) ;
#69499 = AXIS2_PLACEMENT_3D('',#104430,#81181,#81182) ;
#69500 = AXIS2_PLACEMENT_3D('',#104439,#81187,#81188) ;
#69501 = AXIS2_PLACEMENT_3D('',#104448,#81193,#81194) ;
#69502 = AXIS2_PLACEMENT_3D('',#104457,#81199,#81200) ;
#69503 = AXIS2_PLACEMENT_3D('',#104484,#81205,#81206) ;
#69504 = AXIS2_PLACEMENT_3D('',#104501,#81215,#81216) ;
#69505 = AXIS2_PLACEMENT_3D('',#104506,#81218,#81219) ;
#69506 = AXIS2_PLACEMENT_3D('',#104510,#81221,#81222) ;
#69507 = AXIS2_PLACEMENT_3D('',#104514,#81224,#81225) ;
#69508 = AXIS2_PLACEMENT_3D('',#104517,#81227,#81228) ;
#69509 = AXIS2_PLACEMENT_3D('',#104518,#81229,#81230) ;
#69510 = AXIS2_PLACEMENT_3D('',#104521,#81231,#81232) ;
#69511 = AXIS2_PLACEMENT_3D('',#104526,#81235,#81236) ;
#69512 = AXIS2_PLACEMENT_3D('',#104529,#81238,#81239) ;
#69513 = AXIS2_PLACEMENT_3D('',#104530,#81240,#81241) ;
#69514 = AXIS2_PLACEMENT_3D('',#104536,#81245,#81246) ;
#69515 = AXIS2_PLACEMENT_3D('',#104542,#81250,#81251) ;
#69516 = AXIS2_PLACEMENT_3D('',#104545,#81252,#81253) ;
#69517 = AXIS2_PLACEMENT_3D('',#104549,#81255,#81256) ;
#69518 = AXIS2_PLACEMENT_3D('',#104551,#81258,#81259) ;
#69519 = AXIS2_PLACEMENT_3D('',#104554,#81260,#81261) ;
#69520 = AXIS2_PLACEMENT_3D('',#104558,#81263,#81264) ;
#69521 = AXIS2_PLACEMENT_3D('',#104560,#81266,#81267) ;
#69522 = AXIS2_PLACEMENT_3D('',#104566,#81271,#81272) ;
#69523 = AXIS2_PLACEMENT_3D('',#104572,#81276,#81277) ;
#69524 = AXIS2_PLACEMENT_3D('',#104575,#81278,#81279) ;
#69525 = AXIS2_PLACEMENT_3D('',#104580,#81282,#81283) ;
#69526 = AXIS2_PLACEMENT_3D('',#104582,#81284,#81285) ;
#69527 = AXIS2_PLACEMENT_3D('',#104584,#81287,#81288) ;
#69528 = AXIS2_PLACEMENT_3D('',#104587,#81289,#81290) ;
#69529 = AXIS2_PLACEMENT_3D('',#104592,#81294,#81295) ;
#69530 = AXIS2_PLACEMENT_3D('',#104598,#81299,#81300) ;
#69531 = AXIS2_PLACEMENT_3D('',#104601,#81301,#81302) ;
#69532 = AXIS2_PLACEMENT_3D('',#104605,#81304,#81305) ;
#69533 = AXIS2_PLACEMENT_3D('',#104607,#81307,#81308) ;
#69534 = AXIS2_PLACEMENT_3D('',#104616,#81313,#81314) ;
#69535 = AXIS2_PLACEMENT_3D('',#104619,#81315,#81316) ;
#69536 = AXIS2_PLACEMENT_3D('',#104623,#81318,#81319) ;
#69537 = AXIS2_PLACEMENT_3D('',#104625,#81321,#81322) ;
#69538 = AXIS2_PLACEMENT_3D('',#104631,#81326,#81327) ;
#69539 = AXIS2_PLACEMENT_3D('',#104640,#81332,#81333) ;
#69540 = AXIS2_PLACEMENT_3D('',#104647,#81337,#81338) ;
#69541 = AXIS2_PLACEMENT_3D('',#104648,#81339,#81340) ;
#69542 = AXIS2_PLACEMENT_3D('',#104657,#81345,#81346) ;
#69543 = AXIS2_PLACEMENT_3D('',#104660,#81347,#81348) ;
#69544 = AXIS2_PLACEMENT_3D('',#104665,#81351,#81352) ;
#69545 = AXIS2_PLACEMENT_3D('',#104669,#81354,#81355) ;
#69546 = AXIS2_PLACEMENT_3D('',#104671,#81357,#81358) ;
#69547 = AXIS2_PLACEMENT_3D('',#104679,#81363,#81364) ;
#69548 = AXIS2_PLACEMENT_3D('',#104688,#81369,#81370) ;
#69549 = AXIS2_PLACEMENT_3D('',#104697,#81375,#81376) ;
#69550 = AXIS2_PLACEMENT_3D('',#104706,#81381,#81382) ;
#69551 = AXIS2_PLACEMENT_3D('',#104712,#81386,#81387) ;
#69552 = AXIS2_PLACEMENT_3D('',#104718,#81391,#81392) ;
#69553 = AXIS2_PLACEMENT_3D('',#104724,#81396,#81397) ;
#69554 = AXIS2_PLACEMENT_3D('',#104730,#81401,#81402) ;
#69555 = AXIS2_PLACEMENT_3D('',#104739,#81406,#81407) ;
#69556 = AXIS2_PLACEMENT_3D('',#104742,#81409,#81410) ;
#69557 = AXIS2_PLACEMENT_3D('',#104743,#81411,#81412) ;
#69558 = AXIS2_PLACEMENT_3D('',#104752,#81416,#81417) ;
#69559 = AXIS2_PLACEMENT_3D('',#104755,#81419,#81420) ;
#69560 = AXIS2_PLACEMENT_3D('',#104756,#81421,#81422) ;
#69561 = AXIS2_PLACEMENT_3D('',#104760,#81424,#81425) ;
#69562 = AXIS2_PLACEMENT_3D('',#104761,#81426,#81427) ;
#69563 = AXIS2_PLACEMENT_3D('',#104762,#81428,#81429) ;
#69564 = AXIS2_PLACEMENT_3D('',#104768,#81433,#81434) ;
#69565 = AXIS2_PLACEMENT_3D('',#104777,#81439,#81440) ;
#69566 = AXIS2_PLACEMENT_3D('',#104786,#81445,#81446) ;
#69567 = AXIS2_PLACEMENT_3D('',#104795,#81451,#81452) ;
#69568 = AXIS2_PLACEMENT_3D('',#104804,#81457,#81458) ;
#69569 = AXIS2_PLACEMENT_3D('',#104805,#81459,#81460) ;
#69570 = AXIS2_PLACEMENT_3D('',#104806,#81461,#81462) ;
#69571 = AXIS2_PLACEMENT_3D('',#104807,#81463,#81464) ;
#69572 = AXIS2_PLACEMENT_3D('',#104816,#81469,#81470) ;
#69573 = AXIS2_PLACEMENT_3D('',#104825,#81475,#81476) ;
#69574 = AXIS2_PLACEMENT_3D('',#104834,#81481,#81482) ;
#69575 = AXIS2_PLACEMENT_3D('',#104843,#81487,#81488) ;
#69576 = AXIS2_PLACEMENT_3D('',#104847,#81490,#81491) ;
#69577 = AXIS2_PLACEMENT_3D('',#104849,#81493,#81494) ;
#69578 = AXIS2_PLACEMENT_3D('',#104852,#81495,#81496) ;
#69579 = AXIS2_PLACEMENT_3D('',#104853,#81497,#81498) ;
#69580 = AXIS2_PLACEMENT_3D('',#104854,#81499,#81500) ;
#69581 = AXIS2_PLACEMENT_3D('',#104855,#81501,#81502) ;
#69582 = AXIS2_PLACEMENT_3D('',#104859,#81504,#81505) ;
#69583 = AXIS2_PLACEMENT_3D('',#104861,#81507,#81508) ;
#69584 = AXIS2_PLACEMENT_3D('',#104862,#81509,#81510) ;
#69585 = AXIS2_PLACEMENT_3D('',#104863,#81511,#81512) ;
#69586 = AXIS2_PLACEMENT_3D('',#104864,#81513,#81514) ;
#69587 = AXIS2_PLACEMENT_3D('',#104865,#81515,#81516) ;
#69588 = AXIS2_PLACEMENT_3D('',#104866,#81517,#81518) ;
#69589 = AXIS2_PLACEMENT_3D('',#104867,#81519,#81520) ;
#69590 = AXIS2_PLACEMENT_3D('',#104868,#81521,#81522) ;
#69591 = AXIS2_PLACEMENT_3D('',#104869,#81523,#81524) ;
#69592 = AXIS2_PLACEMENT_3D('',#104870,#81525,#81526) ;
#69593 = AXIS2_PLACEMENT_3D('',#104871,#81527,#81528) ;
#69594 = AXIS2_PLACEMENT_3D('',#104872,#81529,#81530) ;
#69595 = AXIS2_PLACEMENT_3D('',#104873,#81531,#81532) ;
#69596 = AXIS2_PLACEMENT_3D('',#104874,#81533,#81534) ;
#69597 = AXIS2_PLACEMENT_3D('',#104875,#81535,#81536) ;
#69598 = AXIS2_PLACEMENT_3D('',#104876,#81537,#81538) ;
#69599 = AXIS2_PLACEMENT_3D('',#104877,#81539,#81540) ;
#69600 = AXIS2_PLACEMENT_3D('',#104878,#81541,#81542) ;
#69601 = AXIS2_PLACEMENT_3D('',#104879,#81543,#81544) ;
#69602 = AXIS2_PLACEMENT_3D('',#104880,#81545,#81546) ;
#69603 = AXIS2_PLACEMENT_3D('',#104881,#81547,#81548) ;
#69604 = AXIS2_PLACEMENT_3D('',#104882,#81549,#81550) ;
#69605 = AXIS2_PLACEMENT_3D('',#104883,#81551,#81552) ;
#69606 = AXIS2_PLACEMENT_3D('',#104884,#81553,#81554) ;
#69607 = AXIS2_PLACEMENT_3D('',#104885,#81555,#81556) ;
#69608 = AXIS2_PLACEMENT_3D('',#104886,#81557,#81558) ;
#69609 = AXIS2_PLACEMENT_3D('',#104887,#81559,#81560) ;
#69610 = AXIS2_PLACEMENT_3D('',#104888,#81561,#81562) ;
#69611 = AXIS2_PLACEMENT_3D('',#104889,#81563,#81564) ;
#69612 = AXIS2_PLACEMENT_3D('',#104890,#81565,#81566) ;
#69613 = AXIS2_PLACEMENT_3D('',#104891,#81567,#81568) ;
#69614 = AXIS2_PLACEMENT_3D('',#104892,#81569,#81570) ;
#69615 = AXIS2_PLACEMENT_3D('',#104893,#81571,#81572) ;
#69616 = AXIS2_PLACEMENT_3D('',#104894,#81573,#81574) ;
#69617 = AXIS2_PLACEMENT_3D('',#104895,#81575,#81576) ;
#69618 = AXIS2_PLACEMENT_3D('',#104896,#81577,#81578) ;
#69619 = AXIS2_PLACEMENT_3D('',#104897,#81579,#81580) ;
#69620 = AXIS2_PLACEMENT_3D('',#104898,#81581,#81582) ;
#69621 = AXIS2_PLACEMENT_3D('',#104899,#81583,#81584) ;
#69622 = AXIS2_PLACEMENT_3D('',#104900,#81585,#81586) ;
#69623 = AXIS2_PLACEMENT_3D('',#104901,#81587,#81588) ;
#69624 = AXIS2_PLACEMENT_3D('',#104902,#81589,#81590) ;
#69625 = AXIS2_PLACEMENT_3D('',#104903,#81591,#81592) ;
#69626 = AXIS2_PLACEMENT_3D('',#104904,#81593,#81594) ;
#69627 = AXIS2_PLACEMENT_3D('',#104905,#81595,#81596) ;
#69628 = AXIS2_PLACEMENT_3D('',#104906,#81597,#81598) ;
#69629 = AXIS2_PLACEMENT_3D('',#104907,#81599,#81600) ;
#69630 = AXIS2_PLACEMENT_3D('',#104908,#81601,#81602) ;
#69631 = AXIS2_PLACEMENT_3D('',#104909,#81603,#81604) ;
#69632 = AXIS2_PLACEMENT_3D('',#104910,#81605,#81606) ;
#69633 = AXIS2_PLACEMENT_3D('',#104911,#81607,#81608) ;
#69634 = AXIS2_PLACEMENT_3D('',#104912,#81609,#81610) ;
#69635 = AXIS2_PLACEMENT_3D('',#104913,#81611,#81612) ;
#69636 = AXIS2_PLACEMENT_3D('',#104914,#81613,#81614) ;
#69637 = AXIS2_PLACEMENT_3D('',#104915,#81615,#81616) ;
#69638 = AXIS2_PLACEMENT_3D('',#104916,#81617,#81618) ;
#69639 = AXIS2_PLACEMENT_3D('',#104917,#81619,#81620) ;
#69640 = AXIS2_PLACEMENT_3D('',#104918,#81621,#81622) ;
#69641 = AXIS2_PLACEMENT_3D('',#104919,#81623,#81624) ;
#69642 = AXIS2_PLACEMENT_3D('',#104920,#81625,#81626) ;
#69643 = AXIS2_PLACEMENT_3D('',#104921,#81627,#81628) ;
#69644 = AXIS2_PLACEMENT_3D('',#104922,#81629,#81630) ;
#69645 = AXIS2_PLACEMENT_3D('',#104923,#81631,#81632) ;
#69646 = AXIS2_PLACEMENT_3D('',#104924,#81633,#81634) ;
#69647 = AXIS2_PLACEMENT_3D('',#104925,#81635,#81636) ;
#69648 = AXIS2_PLACEMENT_3D('',#104926,#81637,#81638) ;
#69649 = AXIS2_PLACEMENT_3D('',#104927,#81639,#81640) ;
#69650 = AXIS2_PLACEMENT_3D('',#104928,#81641,#81642) ;
#69651 = AXIS2_PLACEMENT_3D('',#104929,#81643,#81644) ;
#69652 = AXIS2_PLACEMENT_3D('',#104930,#81645,#81646) ;
#69653 = AXIS2_PLACEMENT_3D('',#104931,#81647,#81648) ;
#69654 = AXIS2_PLACEMENT_3D('',#104932,#81649,#81650) ;
#69655 = AXIS2_PLACEMENT_3D('',#104933,#81651,#81652) ;
#69656 = AXIS2_PLACEMENT_3D('',#104934,#81653,#81654) ;
#69657 = AXIS2_PLACEMENT_3D('',#104950,#81655,#81656) ;
#69658 = AXIS2_PLACEMENT_3D('',#104951,#81657,#81658) ;
#69659 = AXIS2_PLACEMENT_3D('',#104953,#81659,#81660) ;
#69660 = AXIS2_PLACEMENT_3D('',#104968,#81661,#81662) ;
#69661 = AXIS2_PLACEMENT_3D('',#104969,#81663,#81664) ;
#69662 = AXIS2_PLACEMENT_3D('',#104970,#81665,#81666) ;
#69663 = AXIS2_PLACEMENT_3D('',#104972,#81667,#81668) ;
#69664 = AXIS2_PLACEMENT_3D('',#105002,#81669,#81670) ;
#69665 = AXIS2_PLACEMENT_3D('',#105003,#81671,#81672) ;
#69666 = AXIS2_PLACEMENT_3D('',#105019,#81673,#81674) ;
#69667 = AXIS2_PLACEMENT_3D('',#105021,#81675,#81676) ;
#69668 = AXIS2_PLACEMENT_3D('',#105036,#81677,#81678) ;
#69669 = AXIS2_PLACEMENT_3D('',#105037,#81679,#81680) ;
#69670 = AXIS2_PLACEMENT_3D('',#105038,#81681,#81682) ;
#69671 = AXIS2_PLACEMENT_3D('',#105039,#81683,#81684) ;
#69672 = AXIS2_PLACEMENT_3D('',#105042,#81686,#81687) ;
#69673 = AXIS2_PLACEMENT_3D('',#105043,#81688,#81689) ;
#69674 = AXIS2_PLACEMENT_3D('',#105045,#81690,#81691) ;
#69675 = AXIS2_PLACEMENT_3D('',#105046,#81692,#81693) ;
#69676 = AXIS2_PLACEMENT_3D('',#105047,#81694,#81695) ;
#69677 = AXIS2_PLACEMENT_3D('',#105049,#81696,#81697) ;
#69678 = AXIS2_PLACEMENT_3D('',#105064,#81698,#81699) ;
#69679 = AXIS2_PLACEMENT_3D('',#105065,#81700,#81701) ;
#69680 = AXIS2_PLACEMENT_3D('',#105081,#81702,#81703) ;
#69681 = AXIS2_PLACEMENT_3D('',#105082,#81704,#81705) ;
#69682 = AXIS2_PLACEMENT_3D('',#105083,#81706,#81707) ;
#69683 = AXIS2_PLACEMENT_3D('',#105085,#81708,#81709) ;
#69684 = AXIS2_PLACEMENT_3D('',#105087,#81711,#81712) ;
#69685 = AXIS2_PLACEMENT_3D('',#105088,#81713,#81714) ;
#69686 = AXIS2_PLACEMENT_3D('',#105089,#81715,#81716) ;
#69687 = AXIS2_PLACEMENT_3D('',#105090,#81717,#81718) ;
#69688 = AXIS2_PLACEMENT_3D('',#105091,#81719,#81720) ;
#69689 = AXIS2_PLACEMENT_3D('',#105092,#81721,#81722) ;
#69690 = AXIS2_PLACEMENT_3D('',#105095,#81724,#81725) ;
#69691 = AXIS2_PLACEMENT_3D('',#105096,#81726,#81727) ;
#69692 = AXIS2_PLACEMENT_3D('',#105097,#81728,#81729) ;
#69693 = AXIS2_PLACEMENT_3D('',#105098,#81730,#81731) ;
#69694 = AXIS2_PLACEMENT_3D('',#105100,#81732,#81733) ;
#69695 = AXIS2_PLACEMENT_3D('',#105101,#81734,#81735) ;
#69696 = AXIS2_PLACEMENT_3D('',#105102,#81736,#81737) ;
#69697 = AXIS2_PLACEMENT_3D('',#105103,#81738,#81739) ;
#69698 = AXIS2_PLACEMENT_3D('',#105104,#81740,#81741) ;
#69699 = AXIS2_PLACEMENT_3D('',#105105,#81742,#81743) ;
#69700 = AXIS2_PLACEMENT_3D('',#105106,#81744,#81745) ;
#69701 = AXIS2_PLACEMENT_3D('',#105108,#81746,#81747) ;
#69702 = AXIS2_PLACEMENT_3D('',#105109,#81748,#81749) ;
#69703 = AXIS2_PLACEMENT_3D('',#105110,#81750,#81751) ;
#69704 = AXIS2_PLACEMENT_3D('',#105111,#81752,#81753) ;
#69705 = AXIS2_PLACEMENT_3D('',#105112,#81754,#81755) ;
#69706 = AXIS2_PLACEMENT_3D('',#105114,#81756,#81757) ;
#69707 = AXIS2_PLACEMENT_3D('',#105116,#81759,#81760) ;
#69708 = AXIS2_PLACEMENT_3D('',#105117,#81761,#81762) ;
#69709 = AXIS2_PLACEMENT_3D('',#105118,#81763,#81764) ;
#69710 = AXIS2_PLACEMENT_3D('',#105119,#81765,#81766) ;
#69711 = AXIS2_PLACEMENT_3D('',#105120,#81767,#81768) ;
#69712 = AXIS2_PLACEMENT_3D('',#105122,#81770,#81771) ;
#69713 = AXIS2_PLACEMENT_3D('',#105123,#81772,#81773) ;
#69714 = AXIS2_PLACEMENT_3D('',#105124,#81774,#81775) ;
#69715 = AXIS2_PLACEMENT_3D('',#105125,#81776,#81777) ;
#69716 = AXIS2_PLACEMENT_3D('',#105127,#81778,#81779) ;
#69717 = AXIS2_PLACEMENT_3D('',#105128,#81780,#81781) ;
#69718 = AXIS2_PLACEMENT_3D('',#105129,#81782,#81783) ;
#69719 = AXIS2_PLACEMENT_3D('',#105130,#81784,#81785) ;
#69720 = AXIS2_PLACEMENT_3D('',#105131,#81786,#81787) ;
#69721 = AXIS2_PLACEMENT_3D('',#105132,#81788,#81789) ;
#69722 = AXIS2_PLACEMENT_3D('',#105133,#81790,#81791) ;
#69723 = AXIS2_PLACEMENT_3D('',#105135,#81793,#81794) ;
#69724 = AXIS2_PLACEMENT_3D('',#105136,#81795,#81796) ;
#69725 = AXIS2_PLACEMENT_3D('',#105137,#81797,#81798) ;
#69726 = AXIS2_PLACEMENT_3D('',#105138,#81799,#81800) ;
#69727 = AXIS2_PLACEMENT_3D('',#105139,#81801,#81802) ;
#69728 = AXIS2_PLACEMENT_3D('',#105140,#81803,#81804) ;
#69729 = AXIS2_PLACEMENT_3D('',#105141,#81805,#81806) ;
#69730 = AXIS2_PLACEMENT_3D('',#105142,#81807,#81808) ;
#69731 = AXIS2_PLACEMENT_3D('',#105143,#81809,#81810) ;
#69732 = AXIS2_PLACEMENT_3D('',#105144,#81811,#81812) ;
#69733 = AXIS2_PLACEMENT_3D('',#105145,#81813,#81814) ;
#69734 = AXIS2_PLACEMENT_3D('',#105146,#81815,#81816) ;
#69735 = AXIS2_PLACEMENT_3D('',#105147,#81817,#81818) ;
#69736 = AXIS2_PLACEMENT_3D('',#105148,#81819,#81820) ;
#69737 = AXIS2_PLACEMENT_3D('',#105149,#81821,#81822) ;
#69738 = AXIS2_PLACEMENT_3D('',#105150,#81823,#81824) ;
#69739 = AXIS2_PLACEMENT_3D('',#105151,#81825,#81826) ;
#69740 = AXIS2_PLACEMENT_3D('',#105152,#81827,#81828) ;
#69741 = AXIS2_PLACEMENT_3D('',#105153,#81829,#81830) ;
#69742 = AXIS2_PLACEMENT_3D('',#105154,#81831,#81832) ;
#69743 = AXIS2_PLACEMENT_3D('',#105155,#81833,#81834) ;
#69744 = AXIS2_PLACEMENT_3D('',#105156,#81835,#81836) ;
#69745 = AXIS2_PLACEMENT_3D('',#105157,#81837,#81838) ;
#69746 = AXIS2_PLACEMENT_3D('',#105158,#81839,#81840) ;
#69747 = AXIS2_PLACEMENT_3D('',#105159,#81841,#81842) ;
#69748 = AXIS2_PLACEMENT_3D('',#105160,#81843,#81844) ;
#69749 = AXIS2_PLACEMENT_3D('',#105161,#81845,#81846) ;
#69750 = AXIS2_PLACEMENT_3D('',#105162,#81847,#81848) ;
#69751 = AXIS2_PLACEMENT_3D('',#105163,#81849,#81850) ;
#69752 = AXIS2_PLACEMENT_3D('',#105164,#81851,#81852) ;
#69753 = AXIS2_PLACEMENT_3D('',#105165,#81853,#81854) ;
#69754 = AXIS2_PLACEMENT_3D('',#105166,#81855,#81856) ;
#69755 = AXIS2_PLACEMENT_3D('',#105167,#81857,#81858) ;
#69756 = AXIS2_PLACEMENT_3D('',#105168,#81859,#81860) ;
#69757 = AXIS2_PLACEMENT_3D('',#105169,#81861,#81862) ;
#69758 = AXIS2_PLACEMENT_3D('',#105170,#81863,#81864) ;
#69759 = AXIS2_PLACEMENT_3D('',#105171,#81865,#81866) ;
#69760 = AXIS2_PLACEMENT_3D('',#105172,#81867,#81868) ;
#69761 = AXIS2_PLACEMENT_3D('',#105173,#81869,#81870) ;
#69762 = AXIS2_PLACEMENT_3D('',#105174,#81871,#81872) ;
#69763 = AXIS2_PLACEMENT_3D('',#105175,#81873,#81874) ;
#69764 = AXIS2_PLACEMENT_3D('',#105176,#81875,#81876) ;
#69765 = AXIS2_PLACEMENT_3D('',#105177,#81877,#81878) ;
#69766 = AXIS2_PLACEMENT_3D('',#105178,#81879,#81880) ;
#69767 = AXIS2_PLACEMENT_3D('',#105179,#81881,#81882) ;
#69768 = AXIS2_PLACEMENT_3D('',#105180,#81883,#81884) ;
#69769 = AXIS2_PLACEMENT_3D('',#105181,#81885,#81886) ;
#69770 = AXIS2_PLACEMENT_3D('',#105182,#81887,#81888) ;
#69771 = AXIS2_PLACEMENT_3D('',#105183,#81889,#81890) ;
#69772 = AXIS2_PLACEMENT_3D('',#105184,#81891,#81892) ;
#69773 = AXIS2_PLACEMENT_3D('',#105201,#81893,#81894) ;
#69774 = AXIS2_PLACEMENT_3D('',#105202,#81895,#81896) ;
#69775 = AXIS2_PLACEMENT_3D('',#105203,#81897,#81898) ;
#69776 = AXIS2_PLACEMENT_3D('',#105204,#81899,#81900) ;
#69777 = AXIS2_PLACEMENT_3D('',#105205,#81901,#81902) ;
#69778 = AXIS2_PLACEMENT_3D('',#105206,#81903,#81904) ;
#69779 = AXIS2_PLACEMENT_3D('',#105207,#81905,#81906) ;
#69780 = AXIS2_PLACEMENT_3D('',#105208,#81907,#81908) ;
#69781 = AXIS2_PLACEMENT_3D('',#105209,#81909,#81910) ;
#69782 = AXIS2_PLACEMENT_3D('',#105210,#81911,#81912) ;
#69783 = AXIS2_PLACEMENT_3D('',#105211,#81913,#81914) ;
#69784 = AXIS2_PLACEMENT_3D('',#105230,#81915,#81916) ;
#69785 = AXIS2_PLACEMENT_3D('',#105231,#81917,#81918) ;
#69786 = AXIS2_PLACEMENT_3D('',#105233,#81919,#81920) ;
#69787 = AXIS2_PLACEMENT_3D('',#105234,#81921,#81922) ;
#69788 = AXIS2_PLACEMENT_3D('',#105235,#81923,#81924) ;
#69789 = AXIS2_PLACEMENT_3D('',#105236,#81925,#81926) ;
#69790 = AXIS2_PLACEMENT_3D('',#105237,#81927,#81928) ;
#69791 = AXIS2_PLACEMENT_3D('',#105238,#81929,#81930) ;
#69792 = AXIS2_PLACEMENT_3D('',#105239,#81931,#81932) ;
#69793 = AXIS2_PLACEMENT_3D('',#105240,#81933,#81934) ;
#69794 = AXIS2_PLACEMENT_3D('',#105241,#81935,#81936) ;
#69795 = AXIS2_PLACEMENT_3D('',#105242,#81937,#81938) ;
#69796 = AXIS2_PLACEMENT_3D('',#105243,#81939,#81940) ;
#69797 = AXIS2_PLACEMENT_3D('',#105278,#81941,#81942) ;
#69798 = AXIS2_PLACEMENT_3D('',#105279,#81943,#81944) ;
#69799 = AXIS2_PLACEMENT_3D('',#105280,#81945,#81946) ;
#69800 = AXIS2_PLACEMENT_3D('',#105281,#81947,#81948) ;
#69801 = AXIS2_PLACEMENT_3D('',#105292,#81949,#81950) ;
#69802 = AXIS2_PLACEMENT_3D('',#105293,#81951,#81952) ;
#69803 = AXIS2_PLACEMENT_3D('',#105294,#81953,#81954) ;
#69804 = AXIS2_PLACEMENT_3D('',#105295,#81955,#81956) ;
#69805 = AXIS2_PLACEMENT_3D('',#105302,#81957,#81958) ;
#69806 = AXIS2_PLACEMENT_3D('',#105303,#81959,#81960) ;
#69807 = AXIS2_PLACEMENT_3D('',#105304,#81961,#81962) ;
#69808 = AXIS2_PLACEMENT_3D('',#105305,#81963,#81964) ;
#69809 = AXIS2_PLACEMENT_3D('',#105306,#81965,#81966) ;
#69810 = AXIS2_PLACEMENT_3D('',#105317,#81967,#81968) ;
#69811 = AXIS2_PLACEMENT_3D('',#105318,#81969,#81970) ;
#69812 = AXIS2_PLACEMENT_3D('',#105319,#81971,#81972) ;
#69813 = AXIS2_PLACEMENT_3D('',#105320,#81973,#81974) ;
#69814 = AXIS2_PLACEMENT_3D('',#105321,#81975,#81976) ;
#69815 = AXIS2_PLACEMENT_3D('',#105322,#81977,#81978) ;
#69816 = AXIS2_PLACEMENT_3D('',#105323,#81979,#81980) ;
#69817 = AXIS2_PLACEMENT_3D('',#105324,#81981,#81982) ;
#69818 = AXIS2_PLACEMENT_3D('',#105325,#81983,#81984) ;
#69819 = AXIS2_PLACEMENT_3D('',#105326,#81985,#81986) ;
#69820 = AXIS2_PLACEMENT_3D('',#105327,#81987,#81988) ;
#69821 = AXIS2_PLACEMENT_3D('',#105328,#81989,#81990) ;
#69822 = AXIS2_PLACEMENT_3D('',#105329,#81991,#81992) ;
#69823 = AXIS2_PLACEMENT_3D('',#105330,#81993,#81994) ;
#69824 = AXIS2_PLACEMENT_3D('',#105331,#81995,#81996) ;
#69825 = AXIS2_PLACEMENT_3D('',#105332,#81997,#81998) ;
#69826 = AXIS2_PLACEMENT_3D('',#105333,#81999,#82000) ;
#69827 = AXIS2_PLACEMENT_3D('',#105334,#82001,#82002) ;
#69828 = AXIS2_PLACEMENT_3D('',#105335,#82003,#82004) ;
#69829 = AXIS2_PLACEMENT_3D('',#105336,#82005,#82006) ;
#69830 = AXIS2_PLACEMENT_3D('',#105337,#82007,#82008) ;
#69831 = AXIS2_PLACEMENT_3D('',#105338,#82009,#82010) ;
#69832 = AXIS2_PLACEMENT_3D('',#105339,#82011,#82012) ;
#69833 = AXIS2_PLACEMENT_3D('',#105340,#82013,#82014) ;
#69834 = AXIS2_PLACEMENT_3D('',#105341,#82015,#82016) ;
#69835 = AXIS2_PLACEMENT_3D('',#105342,#82017,#82018) ;
#69836 = AXIS2_PLACEMENT_3D('',#105343,#82019,#82020) ;
#69837 = AXIS2_PLACEMENT_3D('',#105344,#82021,#82022) ;
#69838 = AXIS2_PLACEMENT_3D('',#105345,#82023,#82024) ;
#69839 = AXIS2_PLACEMENT_3D('',#105346,#82025,#82026) ;
#69840 = AXIS2_PLACEMENT_3D('',#105347,#82027,#82028) ;
#69841 = AXIS2_PLACEMENT_3D('',#105348,#82029,#82030) ;
#69842 = AXIS2_PLACEMENT_3D('',#105349,#82031,#82032) ;
#69843 = AXIS2_PLACEMENT_3D('',#105350,#82033,#82034) ;
#69844 = AXIS2_PLACEMENT_3D('',#105357,#82035,#82036) ;
#69845 = AXIS2_PLACEMENT_3D('',#105358,#82037,#82038) ;
#69846 = AXIS2_PLACEMENT_3D('',#105359,#82039,#82040) ;
#69847 = AXIS2_PLACEMENT_3D('',#105360,#82041,#82042) ;
#69848 = AXIS2_PLACEMENT_3D('',#105361,#82043,#82044) ;
#69849 = AXIS2_PLACEMENT_3D('',#105362,#82045,#82046) ;
#69850 = AXIS2_PLACEMENT_3D('',#105363,#82047,#82048) ;
#69851 = AXIS2_PLACEMENT_3D('',#105364,#82049,#82050) ;
#69852 = AXIS2_PLACEMENT_3D('',#105365,#82051,#82052) ;
#69853 = AXIS2_PLACEMENT_3D('',#105366,#82053,#82054) ;
#69854 = AXIS2_PLACEMENT_3D('',#105367,#82055,#82056) ;
#69855 = AXIS2_PLACEMENT_3D('',#105368,#82057,#82058) ;
#69856 = AXIS2_PLACEMENT_3D('',#105369,#82059,#82060) ;
#69857 = AXIS2_PLACEMENT_3D('',#105370,#82061,#82062) ;
#69858 = AXIS2_PLACEMENT_3D('',#105371,#82063,#82064) ;
#69859 = AXIS2_PLACEMENT_3D('',#105372,#82065,#82066) ;
#69860 = AXIS2_PLACEMENT_3D('',#105373,#82067,#82068) ;
#69861 = AXIS2_PLACEMENT_3D('',#105374,#82069,#82070) ;
#69862 = AXIS2_PLACEMENT_3D('',#105375,#82071,#82072) ;
#69863 = AXIS2_PLACEMENT_3D('',#105376,#82073,#82074) ;
#69864 = AXIS2_PLACEMENT_3D('',#105377,#82075,#82076) ;
#69865 = AXIS2_PLACEMENT_3D('',#105378,#82077,#82078) ;
#69866 = AXIS2_PLACEMENT_3D('',#105379,#82079,#82080) ;
#69867 = AXIS2_PLACEMENT_3D('',#105380,#82081,#82082) ;
#69868 = AXIS2_PLACEMENT_3D('',#105381,#82083,#82084) ;
#69869 = AXIS2_PLACEMENT_3D('',#105382,#82085,#82086) ;
#69870 = AXIS2_PLACEMENT_3D('',#105383,#82087,#82088) ;
#69871 = AXIS2_PLACEMENT_3D('',#105384,#82089,#82090) ;
#69872 = AXIS2_PLACEMENT_3D('',#105385,#82091,#82092) ;
#69873 = AXIS2_PLACEMENT_3D('',#105386,#82093,#82094) ;
#69874 = AXIS2_PLACEMENT_3D('',#105387,#82095,#82096) ;
#69875 = AXIS2_PLACEMENT_3D('',#105388,#82097,#82098) ;
#69876 = AXIS2_PLACEMENT_3D('',#105389,#82099,#82100) ;
#69877 = AXIS2_PLACEMENT_3D('',#105390,#82101,#82102) ;
#69878 = AXIS2_PLACEMENT_3D('',#105391,#82103,#82104) ;
#69879 = AXIS2_PLACEMENT_3D('',#105392,#82105,#82106) ;
#69880 = AXIS2_PLACEMENT_3D('',#105393,#82107,#82108) ;
#69881 = AXIS2_PLACEMENT_3D('',#105394,#82109,#82110) ;
#69882 = AXIS2_PLACEMENT_3D('',#105395,#82111,#82112) ;
#69883 = AXIS2_PLACEMENT_3D('',#105426,#82113,#82114) ;
#69884 = AXIS2_PLACEMENT_3D('',#105427,#82115,#82116) ;
#69885 = AXIS2_PLACEMENT_3D('',#105428,#82117,#82118) ;
#69886 = AXIS2_PLACEMENT_3D('',#105429,#82119,#82120) ;
#69887 = AXIS2_PLACEMENT_3D('',#105430,#82121,#82122) ;
#69888 = AXIS2_PLACEMENT_3D('',#105431,#82123,#82124) ;
#69889 = AXIS2_PLACEMENT_3D('',#105432,#82125,#82126) ;
#69890 = AXIS2_PLACEMENT_3D('',#105433,#82127,#82128) ;
#69891 = AXIS2_PLACEMENT_3D('',#105434,#82129,#82130) ;
#69892 = AXIS2_PLACEMENT_3D('',#105435,#82131,#82132) ;
#69893 = AXIS2_PLACEMENT_3D('',#105462,#82133,#82134) ;
#69894 = AXIS2_PLACEMENT_3D('',#105463,#82135,#82136) ;
#69895 = AXIS2_PLACEMENT_3D('',#105464,#82137,#82138) ;
#69896 = AXIS2_PLACEMENT_3D('',#105465,#82139,#82140) ;
#69897 = AXIS2_PLACEMENT_3D('',#105466,#82141,#82142) ;
#69898 = AXIS2_PLACEMENT_3D('',#105467,#82143,#82144) ;
#69899 = AXIS2_PLACEMENT_3D('',#105468,#82145,#82146) ;
#69900 = AXIS2_PLACEMENT_3D('',#105469,#82147,#82148) ;
#69901 = AXIS2_PLACEMENT_3D('',#105470,#82149,#82150) ;
#69902 = AXIS2_PLACEMENT_3D('',#105471,#82151,#82152) ;
#69903 = AXIS2_PLACEMENT_3D('',#105472,#82153,#82154) ;
#69904 = AXIS2_PLACEMENT_3D('',#105473,#82155,#82156) ;
#69905 = AXIS2_PLACEMENT_3D('',#105474,#82157,#82158) ;
#69906 = AXIS2_PLACEMENT_3D('',#105475,#82159,#82160) ;
#69907 = AXIS2_PLACEMENT_3D('',#105476,#82161,#82162) ;
#69908 = AXIS2_PLACEMENT_3D('',#105477,#82163,#82164) ;
#69909 = AXIS2_PLACEMENT_3D('',#105478,#82165,#82166) ;
#69910 = AXIS2_PLACEMENT_3D('',#105479,#82167,#82168) ;
#69911 = AXIS2_PLACEMENT_3D('',#105480,#82169,#82170) ;
#69912 = AXIS2_PLACEMENT_3D('',#105481,#82171,#82172) ;
#69913 = AXIS2_PLACEMENT_3D('',#105482,#82173,#82174) ;
#69914 = AXIS2_PLACEMENT_3D('',#105483,#82175,#82176) ;
#69915 = AXIS2_PLACEMENT_3D('',#105484,#82177,#82178) ;
#69916 = AXIS2_PLACEMENT_3D('',#105485,#82179,#82180) ;
#69917 = AXIS2_PLACEMENT_3D('',#105486,#82181,#82182) ;
#69918 = AXIS2_PLACEMENT_3D('',#105487,#82183,#82184) ;
#69919 = AXIS2_PLACEMENT_3D('',#105488,#82185,#82186) ;
#69920 = AXIS2_PLACEMENT_3D('',#105489,#82187,#82188) ;
#69921 = AXIS2_PLACEMENT_3D('',#105490,#82189,#82190) ;
#69922 = AXIS2_PLACEMENT_3D('',#105515,#82191,#82192) ;
#69923 = AXIS2_PLACEMENT_3D('',#105516,#82193,#82194) ;
#69924 = AXIS2_PLACEMENT_3D('',#105517,#82195,#82196) ;
#69925 = AXIS2_PLACEMENT_3D('',#105518,#82197,#82198) ;
#69926 = AXIS2_PLACEMENT_3D('',#105519,#82199,#82200) ;
#69927 = AXIS2_PLACEMENT_3D('',#105520,#82201,#82202) ;
#69928 = AXIS2_PLACEMENT_3D('',#105521,#82203,#82204) ;
#69929 = AXIS2_PLACEMENT_3D('',#105570,#82205,#82206) ;
#69930 = AXIS2_PLACEMENT_3D('',#105571,#82207,#82208) ;
#69931 = AXIS2_PLACEMENT_3D('',#105572,#82209,#82210) ;
#69932 = AXIS2_PLACEMENT_3D('',#105573,#82211,#82212) ;
#69933 = AXIS2_PLACEMENT_3D('',#105574,#82213,#82214) ;
#69934 = AXIS2_PLACEMENT_3D('',#105575,#82215,#82216) ;
#69935 = AXIS2_PLACEMENT_3D('',#105576,#82217,#82218) ;
#69936 = AXIS2_PLACEMENT_3D('',#105638,#82219,#82220) ;
#69937 = AXIS2_PLACEMENT_3D('',#105639,#82221,#82222) ;
#69938 = AXIS2_PLACEMENT_3D('',#105640,#82223,#82224) ;
#69939 = AXIS2_PLACEMENT_3D('',#105813,#82225,#82226) ;
#69940 = AXIS2_PLACEMENT_3D('',#105814,#82227,#82228) ;
#69941 = AXIS2_PLACEMENT_3D('',#105869,#82229,#82230) ;
#69942 = AXIS2_PLACEMENT_3D('',#105916,#82231,#82232) ;
#69943 = AXIS2_PLACEMENT_3D('',#105917,#82233,#82234) ;
#69944 = AXIS2_PLACEMENT_3D('',#105918,#82235,#82236) ;
#69945 = AXIS2_PLACEMENT_3D('',#105919,#82237,#82238) ;
#69946 = AXIS2_PLACEMENT_3D('',#105920,#82239,#82240) ;
#69947 = AXIS2_PLACEMENT_3D('',#105921,#82241,#82242) ;
#69948 = AXIS2_PLACEMENT_3D('',#106026,#82243,#82244) ;
#69949 = AXIS2_PLACEMENT_3D('',#106027,#82245,#82246) ;
#69950 = AXIS2_PLACEMENT_3D('',#106028,#82247,#82248) ;
#69951 = AXIS2_PLACEMENT_3D('',#106029,#82249,#82250) ;
#69952 = AXIS2_PLACEMENT_3D('',#106042,#82251,#82252) ;
#69953 = AXIS2_PLACEMENT_3D('',#106043,#82253,#82254) ;
#69954 = AXIS2_PLACEMENT_3D('',#106044,#82255,#82256) ;
#69955 = AXIS2_PLACEMENT_3D('',#106045,#82257,#82258) ;
#69956 = AXIS2_PLACEMENT_3D('',#106046,#82259,#82260) ;
#69957 = AXIS2_PLACEMENT_3D('',#106047,#82261,#82262) ;
#69958 = AXIS2_PLACEMENT_3D('',#106048,#82263,#82264) ;
#69959 = AXIS2_PLACEMENT_3D('',#106049,#82265,#82266) ;
#69960 = AXIS2_PLACEMENT_3D('',#106050,#82267,#82268) ;
#69961 = AXIS2_PLACEMENT_3D('',#106051,#82269,#82270) ;
#69962 = AXIS2_PLACEMENT_3D('',#106052,#82271,#82272) ;
#69963 = AXIS2_PLACEMENT_3D('',#106053,#82273,#82274) ;
#69964 = AXIS2_PLACEMENT_3D('',#106054,#82275,#82276) ;
#69965 = AXIS2_PLACEMENT_3D('',#106055,#82277,#82278) ;
#69966 = AXIS2_PLACEMENT_3D('',#106056,#82279,#82280) ;
#69967 = AXIS2_PLACEMENT_3D('',#106057,#82281,#82282) ;
#69968 = AXIS2_PLACEMENT_3D('',#106058,#82283,#82284) ;
#69969 = AXIS2_PLACEMENT_3D('',#106059,#82285,#82286) ;
#69970 = AXIS2_PLACEMENT_3D('',#106060,#82287,#82288) ;
#69971 = AXIS2_PLACEMENT_3D('',#106061,#82289,#82290) ;
#69972 = AXIS2_PLACEMENT_3D('',#106062,#82291,#82292) ;
#69973 = AXIS2_PLACEMENT_3D('',#106063,#82293,#82294) ;
#69974 = AXIS2_PLACEMENT_3D('',#106064,#82295,#82296) ;
#69975 = AXIS2_PLACEMENT_3D('',#106065,#82297,#82298) ;
#69976 = AXIS2_PLACEMENT_3D('',#106066,#82299,#82300) ;
#69977 = AXIS2_PLACEMENT_3D('',#106067,#82301,#82302) ;
#69978 = AXIS2_PLACEMENT_3D('',#106068,#82303,#82304) ;
#69979 = AXIS2_PLACEMENT_3D('',#106069,#82305,#82306) ;
#69980 = AXIS2_PLACEMENT_3D('',#106070,#82307,#82308) ;
#69981 = AXIS2_PLACEMENT_3D('',#106071,#82309,#82310) ;
#69982 = AXIS2_PLACEMENT_3D('',#106072,#82311,#82312) ;
#69983 = AXIS2_PLACEMENT_3D('',#106073,#82313,#82314) ;
#69984 = AXIS2_PLACEMENT_3D('',#106074,#82315,#82316) ;
#69985 = AXIS2_PLACEMENT_3D('',#106075,#82317,#82318) ;
#69986 = AXIS2_PLACEMENT_3D('',#106076,#82319,#82320) ;
#69987 = AXIS2_PLACEMENT_3D('',#106077,#82321,#82322) ;
#69988 = AXIS2_PLACEMENT_3D('',#106078,#82323,#82324) ;
#69989 = AXIS2_PLACEMENT_3D('',#106079,#82325,#82326) ;
#69990 = AXIS2_PLACEMENT_3D('',#106092,#82327,#82328) ;
#69991 = AXIS2_PLACEMENT_3D('',#106093,#82329,#82330) ;
#69992 = AXIS2_PLACEMENT_3D('',#106094,#82331,#82332) ;
#69993 = AXIS2_PLACEMENT_3D('',#106095,#82333,#82334) ;
#69994 = AXIS2_PLACEMENT_3D('',#106150,#82335,#82336) ;
#69995 = AXIS2_PLACEMENT_3D('',#106151,#82337,#82338) ;
#69996 = AXIS2_PLACEMENT_3D('',#106152,#82339,#82340) ;
#69997 = AXIS2_PLACEMENT_3D('',#106207,#82341,#82342) ;
#69998 = AXIS2_PLACEMENT_3D('',#106208,#82343,#82344) ;
#69999 = AXIS2_PLACEMENT_3D('',#106234,#82345,#82346) ;
#70000 = AXIS2_PLACEMENT_3D('',#106236,#82347,#82348) ;
#70001 = AXIS2_PLACEMENT_3D('',#106238,#82349,#82350) ;
#70002 = AXIS2_PLACEMENT_3D('',#106277,#82351,#82352) ;
#70003 = AXIS2_PLACEMENT_3D('',#106279,#82353,#82354) ;
#70004 = AXIS2_PLACEMENT_3D('',#106281,#82355,#82356) ;
#70005 = AXIS2_PLACEMENT_3D('',#106282,#82357,#82358) ;
#70006 = AXIS2_PLACEMENT_3D('',#106283,#82359,#82360) ;
#70007 = AXIS2_PLACEMENT_3D('',#106285,#82361,#82362) ;
#70008 = AXIS2_PLACEMENT_3D('',#106287,#82363,#82364) ;
#70009 = AXIS2_PLACEMENT_3D('',#106288,#82365,#82366) ;
#70010 = AXIS2_PLACEMENT_3D('',#106289,#82367,#82368) ;
#70011 = AXIS2_PLACEMENT_3D('',#106291,#82369,#82370) ;
#70012 = AXIS2_PLACEMENT_3D('',#106293,#82371,#82372) ;
#70013 = AXIS2_PLACEMENT_3D('',#106294,#82373,#82374) ;
#70014 = AXIS2_PLACEMENT_3D('',#106295,#82375,#82376) ;
#70015 = AXIS2_PLACEMENT_3D('',#106298,#82377,#82378) ;
#70016 = AXIS2_PLACEMENT_3D('',#106302,#82380,#82381) ;
#70017 = AXIS2_PLACEMENT_3D('',#106304,#82382,#82383) ;
#70018 = AXIS2_PLACEMENT_3D('',#106306,#82385,#82386) ;
#70019 = AXIS2_PLACEMENT_3D('',#106309,#82387,#82388) ;
#70020 = AXIS2_PLACEMENT_3D('',#106313,#82390,#82391) ;
#70021 = AXIS2_PLACEMENT_3D('',#106315,#82393,#82394) ;
#70022 = AXIS2_PLACEMENT_3D('',#106318,#82395,#82396) ;
#70023 = AXIS2_PLACEMENT_3D('',#106320,#82397,#82398) ;
#70024 = AXIS2_PLACEMENT_3D('',#106322,#82399,#82400) ;
#70025 = AXIS2_PLACEMENT_3D('',#106323,#82401,#82402) ;
#70026 = AXIS2_PLACEMENT_3D('',#106324,#82403,#82404) ;
#70027 = AXIS2_PLACEMENT_3D('',#106326,#82406,#82407) ;
#70028 = AXIS2_PLACEMENT_3D('',#106329,#82409,#82410) ;
#70029 = AXIS2_PLACEMENT_3D('',#106338,#82411,#82412) ;
#70030 = AXIS2_PLACEMENT_3D('',#106346,#82413,#82414) ;
#70031 = AXIS2_PLACEMENT_3D('',#106348,#82416,#82417) ;
#70032 = AXIS2_PLACEMENT_3D('',#106364,#82421,#82422) ;
#70033 = AXIS2_PLACEMENT_3D('',#106366,#82424,#82425) ;
#70034 = AXIS2_PLACEMENT_3D('',#106415,#82430,#82431) ;
#70035 = AXIS2_PLACEMENT_3D('',#106424,#82436,#82437) ;
#70036 = AXIS2_PLACEMENT_3D('',#106454,#82442,#82443) ;
#70037 = AXIS2_PLACEMENT_3D('',#106463,#82448,#82449) ;
#70038 = AXIS2_PLACEMENT_3D('',#106472,#82454,#82455) ;
#70039 = AXIS2_PLACEMENT_3D('',#106483,#82460,#82461) ;
#70040 = AXIS2_PLACEMENT_3D('',#106485,#82463,#82464) ;
#70041 = AXIS2_PLACEMENT_3D('',#106489,#82466,#82467) ;
#70042 = AXIS2_PLACEMENT_3D('',#106490,#82468,#82469) ;
#70043 = AXIS2_PLACEMENT_3D('',#106491,#82470,#82471) ;
#70044 = AXIS2_PLACEMENT_3D('',#106493,#82472,#82473) ;
#70045 = AXIS2_PLACEMENT_3D('',#106497,#82475,#82476) ;
#70046 = AXIS2_PLACEMENT_3D('',#106501,#82478,#82479) ;
#70047 = AXIS2_PLACEMENT_3D('',#106505,#82481,#82482) ;
#70048 = AXIS2_PLACEMENT_3D('',#106509,#82484,#82485) ;
#70049 = AXIS2_PLACEMENT_3D('',#106513,#82487,#82488) ;
#70050 = AXIS2_PLACEMENT_3D('',#106516,#82490,#82491) ;
#70051 = AXIS2_PLACEMENT_3D('',#106518,#82492,#82493) ;
#70052 = AXIS2_PLACEMENT_3D('',#106521,#82495,#82496) ;
#70053 = AXIS2_PLACEMENT_3D('',#106523,#82497,#82498) ;
#70054 = AXIS2_PLACEMENT_3D('',#106529,#82501,#82502) ;
#70055 = AXIS2_PLACEMENT_3D('',#106533,#82504,#82505) ;
#70056 = AXIS2_PLACEMENT_3D('',#106536,#82507,#82508) ;
#70057 = AXIS2_PLACEMENT_3D('',#106537,#82509,#82510) ;
#70058 = AXIS2_PLACEMENT_3D('',#106542,#82512,#82513) ;
#70059 = AXIS2_PLACEMENT_3D('',#106546,#82515,#82516) ;
#70060 = AXIS2_PLACEMENT_3D('',#106550,#82518,#82519) ;
#70061 = AXIS2_PLACEMENT_3D('',#106554,#82521,#82522) ;
#70062 = AXIS2_PLACEMENT_3D('',#106559,#82525,#82526) ;
#70063 = AXIS2_PLACEMENT_3D('',#106561,#82527,#82528) ;
#70064 = AXIS2_PLACEMENT_3D('',#106564,#82530,#82531) ;
#70065 = AXIS2_PLACEMENT_3D('',#106566,#82532,#82533) ;
#70066 = AXIS2_PLACEMENT_3D('',#106570,#82535,#82536) ;
#70067 = AXIS2_PLACEMENT_3D('',#106574,#82538,#82539) ;
#70068 = AXIS2_PLACEMENT_3D('',#106578,#82541,#82542) ;
#70069 = AXIS2_PLACEMENT_3D('',#106582,#82544,#82545) ;
#70070 = AXIS2_PLACEMENT_3D('',#106586,#82547,#82548) ;
#70071 = AXIS2_PLACEMENT_3D('',#106590,#82550,#82551) ;
#70072 = AXIS2_PLACEMENT_3D('',#106594,#82553,#82554) ;
#70073 = AXIS2_PLACEMENT_3D('',#106597,#82556,#82557) ;
#70074 = AXIS2_PLACEMENT_3D('',#106598,#82558,#82559) ;
#70075 = AXIS2_PLACEMENT_3D('',#106601,#82562,#82563) ;
#70076 = AXIS2_PLACEMENT_3D('',#106604,#82566,#82567) ;
#70077 = AXIS2_PLACEMENT_3D('',#106693,#82572,#82573) ;
#70078 = AXIS2_PLACEMENT_3D('',#106704,#82574,#82575) ;
#70079 = AXIS2_PLACEMENT_3D('',#106709,#82579,#82580) ;
#70080 = AXIS2_PLACEMENT_3D('',#106715,#82584,#82585) ;
#70081 = AXIS2_PLACEMENT_3D('',#106735,#82589,#82590) ;
#70082 = AXIS2_PLACEMENT_3D('',#106834,#82596,#82597) ;
#70083 = AXIS2_PLACEMENT_3D('',#106838,#82599,#82600) ;
#70084 = AXIS2_PLACEMENT_3D('',#106842,#82603,#82604) ;
#70085 = AXIS2_PLACEMENT_3D('',#106845,#82605,#82606) ;
#70086 = AXIS2_PLACEMENT_3D('',#106850,#82609,#82610) ;
#70087 = AXIS2_PLACEMENT_3D('',#106852,#82611,#82612) ;
#70088 = AXIS2_PLACEMENT_3D('',#106854,#82613,#82614) ;
#70089 = AXIS2_PLACEMENT_3D('',#106862,#82618,#82619) ;
#70090 = AXIS2_PLACEMENT_3D('',#106864,#82620,#82621) ;
#70091 = AXIS2_PLACEMENT_3D('',#106866,#82622,#82623) ;
#70092 = AXIS2_PLACEMENT_3D('',#106871,#82626,#82627) ;
#70093 = AXIS2_PLACEMENT_3D('',#106873,#82628,#82629) ;
#70094 = AXIS2_PLACEMENT_3D('',#106875,#82630,#82631) ;
#70095 = AXIS2_PLACEMENT_3D('',#106879,#82633,#82634) ;
#70096 = AXIS2_PLACEMENT_3D('',#106883,#82636,#82637) ;
#70097 = AXIS2_PLACEMENT_3D('',#106884,#82638,#82639) ;
#70098 = AXIS2_PLACEMENT_3D('',#106885,#82640,#82641) ;
#70099 = AXIS2_PLACEMENT_3D('',#106888,#82642,#82643) ;
#70100 = AXIS2_PLACEMENT_3D('',#106898,#82649,#82650) ;
#70101 = AXIS2_PLACEMENT_3D('',#106900,#82652,#82653) ;
#70102 = AXIS2_PLACEMENT_3D('',#106903,#82654,#82655) ;
#70103 = AXIS2_PLACEMENT_3D('',#106909,#82659,#82660) ;
#70104 = AXIS2_PLACEMENT_3D('',#106911,#82662,#82663) ;
#70105 = AXIS2_PLACEMENT_3D('',#106917,#82666,#82667) ;
#70106 = AXIS2_PLACEMENT_3D('',#106918,#82668,#82669) ;
#70107 = AXIS2_PLACEMENT_3D('',#106921,#82670,#82671) ;
#70108 = AXIS2_PLACEMENT_3D('',#106925,#82674,#82675) ;
#70109 = AXIS2_PLACEMENT_3D('',#106942,#82684,#82685) ;
#70110 = AXIS2_PLACEMENT_3D('',#106951,#82690,#82691) ;
#70111 = AXIS2_PLACEMENT_3D('',#106960,#82696,#82697) ;
#70112 = AXIS2_PLACEMENT_3D('',#106969,#82702,#82703) ;
#70113 = AXIS2_PLACEMENT_3D('',#106996,#82708,#82709) ;
#70114 = AXIS2_PLACEMENT_3D('',#107013,#82718,#82719) ;
#70115 = AXIS2_PLACEMENT_3D('',#107018,#82721,#82722) ;
#70116 = AXIS2_PLACEMENT_3D('',#107022,#82724,#82725) ;
#70117 = AXIS2_PLACEMENT_3D('',#107026,#82727,#82728) ;
#70118 = AXIS2_PLACEMENT_3D('',#107029,#82730,#82731) ;
#70119 = AXIS2_PLACEMENT_3D('',#107030,#82732,#82733) ;
#70120 = AXIS2_PLACEMENT_3D('',#107033,#82734,#82735) ;
#70121 = AXIS2_PLACEMENT_3D('',#107038,#82738,#82739) ;
#70122 = AXIS2_PLACEMENT_3D('',#107041,#82741,#82742) ;
#70123 = AXIS2_PLACEMENT_3D('',#107042,#82743,#82744) ;
#70124 = AXIS2_PLACEMENT_3D('',#107048,#82748,#82749) ;
#70125 = AXIS2_PLACEMENT_3D('',#107054,#82753,#82754) ;
#70126 = AXIS2_PLACEMENT_3D('',#107057,#82755,#82756) ;
#70127 = AXIS2_PLACEMENT_3D('',#107061,#82758,#82759) ;
#70128 = AXIS2_PLACEMENT_3D('',#107063,#82761,#82762) ;
#70129 = AXIS2_PLACEMENT_3D('',#107066,#82763,#82764) ;
#70130 = AXIS2_PLACEMENT_3D('',#107070,#82766,#82767) ;
#70131 = AXIS2_PLACEMENT_3D('',#107072,#82769,#82770) ;
#70132 = AXIS2_PLACEMENT_3D('',#107078,#82774,#82775) ;
#70133 = AXIS2_PLACEMENT_3D('',#107084,#82779,#82780) ;
#70134 = AXIS2_PLACEMENT_3D('',#107087,#82781,#82782) ;
#70135 = AXIS2_PLACEMENT_3D('',#107092,#82785,#82786) ;
#70136 = AXIS2_PLACEMENT_3D('',#107094,#82787,#82788) ;
#70137 = AXIS2_PLACEMENT_3D('',#107096,#82790,#82791) ;
#70138 = AXIS2_PLACEMENT_3D('',#107099,#82792,#82793) ;
#70139 = AXIS2_PLACEMENT_3D('',#107104,#82797,#82798) ;
#70140 = AXIS2_PLACEMENT_3D('',#107110,#82802,#82803) ;
#70141 = AXIS2_PLACEMENT_3D('',#107113,#82804,#82805) ;
#70142 = AXIS2_PLACEMENT_3D('',#107117,#82807,#82808) ;
#70143 = AXIS2_PLACEMENT_3D('',#107119,#82810,#82811) ;
#70144 = AXIS2_PLACEMENT_3D('',#107128,#82816,#82817) ;
#70145 = AXIS2_PLACEMENT_3D('',#107131,#82818,#82819) ;
#70146 = AXIS2_PLACEMENT_3D('',#107135,#82821,#82822) ;
#70147 = AXIS2_PLACEMENT_3D('',#107137,#82824,#82825) ;
#70148 = AXIS2_PLACEMENT_3D('',#107143,#82829,#82830) ;
#70149 = AXIS2_PLACEMENT_3D('',#107152,#82835,#82836) ;
#70150 = AXIS2_PLACEMENT_3D('',#107159,#82840,#82841) ;
#70151 = AXIS2_PLACEMENT_3D('',#107160,#82842,#82843) ;
#70152 = AXIS2_PLACEMENT_3D('',#107169,#82848,#82849) ;
#70153 = AXIS2_PLACEMENT_3D('',#107172,#82850,#82851) ;
#70154 = AXIS2_PLACEMENT_3D('',#107177,#82854,#82855) ;
#70155 = AXIS2_PLACEMENT_3D('',#107181,#82857,#82858) ;
#70156 = AXIS2_PLACEMENT_3D('',#107183,#82860,#82861) ;
#70157 = AXIS2_PLACEMENT_3D('',#107191,#82866,#82867) ;
#70158 = AXIS2_PLACEMENT_3D('',#107200,#82872,#82873) ;
#70159 = AXIS2_PLACEMENT_3D('',#107209,#82878,#82879) ;
#70160 = AXIS2_PLACEMENT_3D('',#107218,#82884,#82885) ;
#70161 = AXIS2_PLACEMENT_3D('',#107224,#82889,#82890) ;
#70162 = AXIS2_PLACEMENT_3D('',#107230,#82894,#82895) ;
#70163 = AXIS2_PLACEMENT_3D('',#107236,#82899,#82900) ;
#70164 = AXIS2_PLACEMENT_3D('',#107242,#82904,#82905) ;
#70165 = AXIS2_PLACEMENT_3D('',#107251,#82909,#82910) ;
#70166 = AXIS2_PLACEMENT_3D('',#107254,#82912,#82913) ;
#70167 = AXIS2_PLACEMENT_3D('',#107255,#82914,#82915) ;
#70168 = AXIS2_PLACEMENT_3D('',#107264,#82919,#82920) ;
#70169 = AXIS2_PLACEMENT_3D('',#107267,#82922,#82923) ;
#70170 = AXIS2_PLACEMENT_3D('',#107268,#82924,#82925) ;
#70171 = AXIS2_PLACEMENT_3D('',#107272,#82927,#82928) ;
#70172 = AXIS2_PLACEMENT_3D('',#107273,#82929,#82930) ;
#70173 = AXIS2_PLACEMENT_3D('',#107274,#82931,#82932) ;
#70174 = AXIS2_PLACEMENT_3D('',#107280,#82936,#82937) ;
#70175 = AXIS2_PLACEMENT_3D('',#107289,#82942,#82943) ;
#70176 = AXIS2_PLACEMENT_3D('',#107298,#82948,#82949) ;
#70177 = AXIS2_PLACEMENT_3D('',#107307,#82954,#82955) ;
#70178 = AXIS2_PLACEMENT_3D('',#107316,#82960,#82961) ;
#70179 = AXIS2_PLACEMENT_3D('',#107317,#82962,#82963) ;
#70180 = AXIS2_PLACEMENT_3D('',#107318,#82964,#82965) ;
#70181 = AXIS2_PLACEMENT_3D('',#107319,#82966,#82967) ;
#70182 = AXIS2_PLACEMENT_3D('',#107328,#82972,#82973) ;
#70183 = AXIS2_PLACEMENT_3D('',#107337,#82978,#82979) ;
#70184 = AXIS2_PLACEMENT_3D('',#107346,#82984,#82985) ;
#70185 = AXIS2_PLACEMENT_3D('',#107355,#82990,#82991) ;
#70186 = AXIS2_PLACEMENT_3D('',#107359,#82993,#82994) ;
#70187 = AXIS2_PLACEMENT_3D('',#107361,#82996,#82997) ;
#70188 = AXIS2_PLACEMENT_3D('',#107364,#82998,#82999) ;
#70189 = AXIS2_PLACEMENT_3D('',#107365,#83000,#83001) ;
#70190 = AXIS2_PLACEMENT_3D('',#107366,#83002,#83003) ;
#70191 = AXIS2_PLACEMENT_3D('',#107367,#83004,#83005) ;
#70192 = AXIS2_PLACEMENT_3D('',#107371,#83007,#83008) ;
#70193 = AXIS2_PLACEMENT_3D('',#107373,#83010,#83011) ;
#70194 = AXIS2_PLACEMENT_3D('',#107374,#83012,#83013) ;
#70195 = AXIS2_PLACEMENT_3D('',#107375,#83014,#83015) ;
#70196 = AXIS2_PLACEMENT_3D('',#107376,#83016,#83017) ;
#70197 = AXIS2_PLACEMENT_3D('',#107377,#83018,#83019) ;
#70198 = AXIS2_PLACEMENT_3D('',#107378,#83020,#83021) ;
#70199 = AXIS2_PLACEMENT_3D('',#107379,#83022,#83023) ;
#70200 = AXIS2_PLACEMENT_3D('',#107380,#83024,#83025) ;
#70201 = AXIS2_PLACEMENT_3D('',#107381,#83026,#83027) ;
#70202 = AXIS2_PLACEMENT_3D('',#107382,#83028,#83029) ;
#70203 = AXIS2_PLACEMENT_3D('',#107383,#83030,#83031) ;
#70204 = AXIS2_PLACEMENT_3D('',#107384,#83032,#83033) ;
#70205 = AXIS2_PLACEMENT_3D('',#107385,#83034,#83035) ;
#70206 = AXIS2_PLACEMENT_3D('',#107386,#83036,#83037) ;
#70207 = AXIS2_PLACEMENT_3D('',#107387,#83038,#83039) ;
#70208 = AXIS2_PLACEMENT_3D('',#107388,#83040,#83041) ;
#70209 = AXIS2_PLACEMENT_3D('',#107389,#83042,#83043) ;
#70210 = AXIS2_PLACEMENT_3D('',#107390,#83044,#83045) ;
#70211 = AXIS2_PLACEMENT_3D('',#107391,#83046,#83047) ;
#70212 = AXIS2_PLACEMENT_3D('',#107392,#83048,#83049) ;
#70213 = AXIS2_PLACEMENT_3D('',#107393,#83050,#83051) ;
#70214 = AXIS2_PLACEMENT_3D('',#107394,#83052,#83053) ;
#70215 = AXIS2_PLACEMENT_3D('',#107395,#83054,#83055) ;
#70216 = AXIS2_PLACEMENT_3D('',#107396,#83056,#83057) ;
#70217 = AXIS2_PLACEMENT_3D('',#107397,#83058,#83059) ;
#70218 = AXIS2_PLACEMENT_3D('',#107398,#83060,#83061) ;
#70219 = AXIS2_PLACEMENT_3D('',#107399,#83062,#83063) ;
#70220 = AXIS2_PLACEMENT_3D('',#107400,#83064,#83065) ;
#70221 = AXIS2_PLACEMENT_3D('',#107401,#83066,#83067) ;
#70222 = AXIS2_PLACEMENT_3D('',#107402,#83068,#83069) ;
#70223 = AXIS2_PLACEMENT_3D('',#107403,#83070,#83071) ;
#70224 = AXIS2_PLACEMENT_3D('',#107404,#83072,#83073) ;
#70225 = AXIS2_PLACEMENT_3D('',#107405,#83074,#83075) ;
#70226 = AXIS2_PLACEMENT_3D('',#107406,#83076,#83077) ;
#70227 = AXIS2_PLACEMENT_3D('',#107407,#83078,#83079) ;
#70228 = AXIS2_PLACEMENT_3D('',#107408,#83080,#83081) ;
#70229 = AXIS2_PLACEMENT_3D('',#107409,#83082,#83083) ;
#70230 = AXIS2_PLACEMENT_3D('',#107410,#83084,#83085) ;
#70231 = AXIS2_PLACEMENT_3D('',#107411,#83086,#83087) ;
#70232 = AXIS2_PLACEMENT_3D('',#107412,#83088,#83089) ;
#70233 = AXIS2_PLACEMENT_3D('',#107413,#83090,#83091) ;
#70234 = AXIS2_PLACEMENT_3D('',#107414,#83092,#83093) ;
#70235 = AXIS2_PLACEMENT_3D('',#107415,#83094,#83095) ;
#70236 = AXIS2_PLACEMENT_3D('',#107416,#83096,#83097) ;
#70237 = AXIS2_PLACEMENT_3D('',#107417,#83098,#83099) ;
#70238 = AXIS2_PLACEMENT_3D('',#107418,#83100,#83101) ;
#70239 = AXIS2_PLACEMENT_3D('',#107419,#83102,#83103) ;
#70240 = AXIS2_PLACEMENT_3D('',#107420,#83104,#83105) ;
#70241 = AXIS2_PLACEMENT_3D('',#107421,#83106,#83107) ;
#70242 = AXIS2_PLACEMENT_3D('',#107422,#83108,#83109) ;
#70243 = AXIS2_PLACEMENT_3D('',#107423,#83110,#83111) ;
#70244 = AXIS2_PLACEMENT_3D('',#107424,#83112,#83113) ;
#70245 = AXIS2_PLACEMENT_3D('',#107425,#83114,#83115) ;
#70246 = AXIS2_PLACEMENT_3D('',#107426,#83116,#83117) ;
#70247 = AXIS2_PLACEMENT_3D('',#107427,#83118,#83119) ;
#70248 = AXIS2_PLACEMENT_3D('',#107428,#83120,#83121) ;
#70249 = AXIS2_PLACEMENT_3D('',#107429,#83122,#83123) ;
#70250 = AXIS2_PLACEMENT_3D('',#107430,#83124,#83125) ;
#70251 = AXIS2_PLACEMENT_3D('',#107431,#83126,#83127) ;
#70252 = AXIS2_PLACEMENT_3D('',#107432,#83128,#83129) ;
#70253 = AXIS2_PLACEMENT_3D('',#107433,#83130,#83131) ;
#70254 = AXIS2_PLACEMENT_3D('',#107434,#83132,#83133) ;
#70255 = AXIS2_PLACEMENT_3D('',#107435,#83134,#83135) ;
#70256 = AXIS2_PLACEMENT_3D('',#107436,#83136,#83137) ;
#70257 = AXIS2_PLACEMENT_3D('',#107437,#83138,#83139) ;
#70258 = AXIS2_PLACEMENT_3D('',#107438,#83140,#83141) ;
#70259 = AXIS2_PLACEMENT_3D('',#107439,#83142,#83143) ;
#70260 = AXIS2_PLACEMENT_3D('',#107440,#83144,#83145) ;
#70261 = AXIS2_PLACEMENT_3D('',#107441,#83146,#83147) ;
#70262 = AXIS2_PLACEMENT_3D('',#107442,#83148,#83149) ;
#70263 = AXIS2_PLACEMENT_3D('',#107443,#83150,#83151) ;
#70264 = AXIS2_PLACEMENT_3D('',#107444,#83152,#83153) ;
#70265 = AXIS2_PLACEMENT_3D('',#107445,#83154,#83155) ;
#70266 = AXIS2_PLACEMENT_3D('',#107446,#83156,#83157) ;
#70267 = AXIS2_PLACEMENT_3D('',#107462,#83158,#83159) ;
#70268 = AXIS2_PLACEMENT_3D('',#107463,#83160,#83161) ;
#70269 = AXIS2_PLACEMENT_3D('',#107465,#83162,#83163) ;
#70270 = AXIS2_PLACEMENT_3D('',#107480,#83164,#83165) ;
#70271 = AXIS2_PLACEMENT_3D('',#107481,#83166,#83167) ;
#70272 = AXIS2_PLACEMENT_3D('',#107482,#83168,#83169) ;
#70273 = AXIS2_PLACEMENT_3D('',#107484,#83170,#83171) ;
#70274 = AXIS2_PLACEMENT_3D('',#107514,#83172,#83173) ;
#70275 = AXIS2_PLACEMENT_3D('',#107515,#83174,#83175) ;
#70276 = AXIS2_PLACEMENT_3D('',#107531,#83176,#83177) ;
#70277 = AXIS2_PLACEMENT_3D('',#107533,#83178,#83179) ;
#70278 = AXIS2_PLACEMENT_3D('',#107548,#83180,#83181) ;
#70279 = AXIS2_PLACEMENT_3D('',#107549,#83182,#83183) ;
#70280 = AXIS2_PLACEMENT_3D('',#107550,#83184,#83185) ;
#70281 = AXIS2_PLACEMENT_3D('',#107551,#83186,#83187) ;
#70282 = AXIS2_PLACEMENT_3D('',#107554,#83189,#83190) ;
#70283 = AXIS2_PLACEMENT_3D('',#107555,#83191,#83192) ;
#70284 = AXIS2_PLACEMENT_3D('',#107557,#83193,#83194) ;
#70285 = AXIS2_PLACEMENT_3D('',#107558,#83195,#83196) ;
#70286 = AXIS2_PLACEMENT_3D('',#107559,#83197,#83198) ;
#70287 = AXIS2_PLACEMENT_3D('',#107561,#83199,#83200) ;
#70288 = AXIS2_PLACEMENT_3D('',#107576,#83201,#83202) ;
#70289 = AXIS2_PLACEMENT_3D('',#107577,#83203,#83204) ;
#70290 = AXIS2_PLACEMENT_3D('',#107593,#83205,#83206) ;
#70291 = AXIS2_PLACEMENT_3D('',#107594,#83207,#83208) ;
#70292 = AXIS2_PLACEMENT_3D('',#107595,#83209,#83210) ;
#70293 = AXIS2_PLACEMENT_3D('',#107597,#83211,#83212) ;
#70294 = AXIS2_PLACEMENT_3D('',#107599,#83214,#83215) ;
#70295 = AXIS2_PLACEMENT_3D('',#107600,#83216,#83217) ;
#70296 = AXIS2_PLACEMENT_3D('',#107601,#83218,#83219) ;
#70297 = AXIS2_PLACEMENT_3D('',#107602,#83220,#83221) ;
#70298 = AXIS2_PLACEMENT_3D('',#107603,#83222,#83223) ;
#70299 = AXIS2_PLACEMENT_3D('',#107604,#83224,#83225) ;
#70300 = AXIS2_PLACEMENT_3D('',#107607,#83227,#83228) ;
#70301 = AXIS2_PLACEMENT_3D('',#107608,#83229,#83230) ;
#70302 = AXIS2_PLACEMENT_3D('',#107609,#83231,#83232) ;
#70303 = AXIS2_PLACEMENT_3D('',#107610,#83233,#83234) ;
#70304 = AXIS2_PLACEMENT_3D('',#107612,#83235,#83236) ;
#70305 = AXIS2_PLACEMENT_3D('',#107613,#83237,#83238) ;
#70306 = AXIS2_PLACEMENT_3D('',#107614,#83239,#83240) ;
#70307 = AXIS2_PLACEMENT_3D('',#107615,#83241,#83242) ;
#70308 = AXIS2_PLACEMENT_3D('',#107616,#83243,#83244) ;
#70309 = AXIS2_PLACEMENT_3D('',#107617,#83245,#83246) ;
#70310 = AXIS2_PLACEMENT_3D('',#107618,#83247,#83248) ;
#70311 = AXIS2_PLACEMENT_3D('',#107620,#83249,#83250) ;
#70312 = AXIS2_PLACEMENT_3D('',#107621,#83251,#83252) ;
#70313 = AXIS2_PLACEMENT_3D('',#107622,#83253,#83254) ;
#70314 = AXIS2_PLACEMENT_3D('',#107623,#83255,#83256) ;
#70315 = AXIS2_PLACEMENT_3D('',#107624,#83257,#83258) ;
#70316 = AXIS2_PLACEMENT_3D('',#107626,#83259,#83260) ;
#70317 = AXIS2_PLACEMENT_3D('',#107628,#83262,#83263) ;
#70318 = AXIS2_PLACEMENT_3D('',#107629,#83264,#83265) ;
#70319 = AXIS2_PLACEMENT_3D('',#107630,#83266,#83267) ;
#70320 = AXIS2_PLACEMENT_3D('',#107631,#83268,#83269) ;
#70321 = AXIS2_PLACEMENT_3D('',#107632,#83270,#83271) ;
#70322 = AXIS2_PLACEMENT_3D('',#107634,#83273,#83274) ;
#70323 = AXIS2_PLACEMENT_3D('',#107635,#83275,#83276) ;
#70324 = AXIS2_PLACEMENT_3D('',#107636,#83277,#83278) ;
#70325 = AXIS2_PLACEMENT_3D('',#107637,#83279,#83280) ;
#70326 = AXIS2_PLACEMENT_3D('',#107639,#83281,#83282) ;
#70327 = AXIS2_PLACEMENT_3D('',#107640,#83283,#83284) ;
#70328 = AXIS2_PLACEMENT_3D('',#107641,#83285,#83286) ;
#70329 = AXIS2_PLACEMENT_3D('',#107642,#83287,#83288) ;
#70330 = AXIS2_PLACEMENT_3D('',#107643,#83289,#83290) ;
#70331 = AXIS2_PLACEMENT_3D('',#107644,#83291,#83292) ;
#70332 = AXIS2_PLACEMENT_3D('',#107645,#83293,#83294) ;
#70333 = AXIS2_PLACEMENT_3D('',#107647,#83296,#83297) ;
#70334 = AXIS2_PLACEMENT_3D('',#107648,#83298,#83299) ;
#70335 = AXIS2_PLACEMENT_3D('',#107649,#83300,#83301) ;
#70336 = AXIS2_PLACEMENT_3D('',#107650,#83302,#83303) ;
#70337 = AXIS2_PLACEMENT_3D('',#107651,#83304,#83305) ;
#70338 = AXIS2_PLACEMENT_3D('',#107652,#83306,#83307) ;
#70339 = AXIS2_PLACEMENT_3D('',#107653,#83308,#83309) ;
#70340 = AXIS2_PLACEMENT_3D('',#107654,#83310,#83311) ;
#70341 = AXIS2_PLACEMENT_3D('',#107655,#83312,#83313) ;
#70342 = AXIS2_PLACEMENT_3D('',#107656,#83314,#83315) ;
#70343 = AXIS2_PLACEMENT_3D('',#107657,#83316,#83317) ;
#70344 = AXIS2_PLACEMENT_3D('',#107658,#83318,#83319) ;
#70345 = AXIS2_PLACEMENT_3D('',#107659,#83320,#83321) ;
#70346 = AXIS2_PLACEMENT_3D('',#107660,#83322,#83323) ;
#70347 = AXIS2_PLACEMENT_3D('',#107661,#83324,#83325) ;
#70348 = AXIS2_PLACEMENT_3D('',#107662,#83326,#83327) ;
#70349 = AXIS2_PLACEMENT_3D('',#107663,#83328,#83329) ;
#70350 = AXIS2_PLACEMENT_3D('',#107664,#83330,#83331) ;
#70351 = AXIS2_PLACEMENT_3D('',#107665,#83332,#83333) ;
#70352 = AXIS2_PLACEMENT_3D('',#107666,#83334,#83335) ;
#70353 = AXIS2_PLACEMENT_3D('',#107667,#83336,#83337) ;
#70354 = AXIS2_PLACEMENT_3D('',#107668,#83338,#83339) ;
#70355 = AXIS2_PLACEMENT_3D('',#107669,#83340,#83341) ;
#70356 = AXIS2_PLACEMENT_3D('',#107670,#83342,#83343) ;
#70357 = AXIS2_PLACEMENT_3D('',#107671,#83344,#83345) ;
#70358 = AXIS2_PLACEMENT_3D('',#107672,#83346,#83347) ;
#70359 = AXIS2_PLACEMENT_3D('',#107673,#83348,#83349) ;
#70360 = AXIS2_PLACEMENT_3D('',#107674,#83350,#83351) ;
#70361 = AXIS2_PLACEMENT_3D('',#107675,#83352,#83353) ;
#70362 = AXIS2_PLACEMENT_3D('',#107676,#83354,#83355) ;
#70363 = AXIS2_PLACEMENT_3D('',#107677,#83356,#83357) ;
#70364 = AXIS2_PLACEMENT_3D('',#107678,#83358,#83359) ;
#70365 = AXIS2_PLACEMENT_3D('',#107679,#83360,#83361) ;
#70366 = AXIS2_PLACEMENT_3D('',#107680,#83362,#83363) ;
#70367 = AXIS2_PLACEMENT_3D('',#107681,#83364,#83365) ;
#70368 = AXIS2_PLACEMENT_3D('',#107682,#83366,#83367) ;
#70369 = AXIS2_PLACEMENT_3D('',#107683,#83368,#83369) ;
#70370 = AXIS2_PLACEMENT_3D('',#107684,#83370,#83371) ;
#70371 = AXIS2_PLACEMENT_3D('',#107685,#83372,#83373) ;
#70372 = AXIS2_PLACEMENT_3D('',#107686,#83374,#83375) ;
#70373 = AXIS2_PLACEMENT_3D('',#107687,#83376,#83377) ;
#70374 = AXIS2_PLACEMENT_3D('',#107688,#83378,#83379) ;
#70375 = AXIS2_PLACEMENT_3D('',#107689,#83380,#83381) ;
#70376 = AXIS2_PLACEMENT_3D('',#107690,#83382,#83383) ;
#70377 = AXIS2_PLACEMENT_3D('',#107691,#83384,#83385) ;
#70378 = AXIS2_PLACEMENT_3D('',#107692,#83386,#83387) ;
#70379 = AXIS2_PLACEMENT_3D('',#107693,#83388,#83389) ;
#70380 = AXIS2_PLACEMENT_3D('',#107694,#83390,#83391) ;
#70381 = AXIS2_PLACEMENT_3D('',#107695,#83392,#83393) ;
#70382 = AXIS2_PLACEMENT_3D('',#107696,#83394,#83395) ;
#70383 = AXIS2_PLACEMENT_3D('',#107713,#83396,#83397) ;
#70384 = AXIS2_PLACEMENT_3D('',#107714,#83398,#83399) ;
#70385 = AXIS2_PLACEMENT_3D('',#107715,#83400,#83401) ;
#70386 = AXIS2_PLACEMENT_3D('',#107716,#83402,#83403) ;
#70387 = AXIS2_PLACEMENT_3D('',#107717,#83404,#83405) ;
#70388 = AXIS2_PLACEMENT_3D('',#107718,#83406,#83407) ;
#70389 = AXIS2_PLACEMENT_3D('',#107719,#83408,#83409) ;
#70390 = AXIS2_PLACEMENT_3D('',#107720,#83410,#83411) ;
#70391 = AXIS2_PLACEMENT_3D('',#107721,#83412,#83413) ;
#70392 = AXIS2_PLACEMENT_3D('',#107722,#83414,#83415) ;
#70393 = AXIS2_PLACEMENT_3D('',#107723,#83416,#83417) ;
#70394 = AXIS2_PLACEMENT_3D('',#107742,#83418,#83419) ;
#70395 = AXIS2_PLACEMENT_3D('',#107743,#83420,#83421) ;
#70396 = AXIS2_PLACEMENT_3D('',#107745,#83422,#83423) ;
#70397 = AXIS2_PLACEMENT_3D('',#107746,#83424,#83425) ;
#70398 = AXIS2_PLACEMENT_3D('',#107747,#83426,#83427) ;
#70399 = AXIS2_PLACEMENT_3D('',#107748,#83428,#83429) ;
#70400 = AXIS2_PLACEMENT_3D('',#107749,#83430,#83431) ;
#70401 = AXIS2_PLACEMENT_3D('',#107750,#83432,#83433) ;
#70402 = AXIS2_PLACEMENT_3D('',#107751,#83434,#83435) ;
#70403 = AXIS2_PLACEMENT_3D('',#107752,#83436,#83437) ;
#70404 = AXIS2_PLACEMENT_3D('',#107753,#83438,#83439) ;
#70405 = AXIS2_PLACEMENT_3D('',#107754,#83440,#83441) ;
#70406 = AXIS2_PLACEMENT_3D('',#107755,#83442,#83443) ;
#70407 = AXIS2_PLACEMENT_3D('',#107790,#83444,#83445) ;
#70408 = AXIS2_PLACEMENT_3D('',#107791,#83446,#83447) ;
#70409 = AXIS2_PLACEMENT_3D('',#107792,#83448,#83449) ;
#70410 = AXIS2_PLACEMENT_3D('',#107793,#83450,#83451) ;
#70411 = AXIS2_PLACEMENT_3D('',#107804,#83452,#83453) ;
#70412 = AXIS2_PLACEMENT_3D('',#107805,#83454,#83455) ;
#70413 = AXIS2_PLACEMENT_3D('',#107806,#83456,#83457) ;
#70414 = AXIS2_PLACEMENT_3D('',#107807,#83458,#83459) ;
#70415 = AXIS2_PLACEMENT_3D('',#107814,#83460,#83461) ;
#70416 = AXIS2_PLACEMENT_3D('',#107815,#83462,#83463) ;
#70417 = AXIS2_PLACEMENT_3D('',#107816,#83464,#83465) ;
#70418 = AXIS2_PLACEMENT_3D('',#107817,#83466,#83467) ;
#70419 = AXIS2_PLACEMENT_3D('',#107818,#83468,#83469) ;
#70420 = AXIS2_PLACEMENT_3D('',#107829,#83470,#83471) ;
#70421 = AXIS2_PLACEMENT_3D('',#107830,#83472,#83473) ;
#70422 = AXIS2_PLACEMENT_3D('',#107831,#83474,#83475) ;
#70423 = AXIS2_PLACEMENT_3D('',#107832,#83476,#83477) ;
#70424 = AXIS2_PLACEMENT_3D('',#107833,#83478,#83479) ;
#70425 = AXIS2_PLACEMENT_3D('',#107834,#83480,#83481) ;
#70426 = AXIS2_PLACEMENT_3D('',#107835,#83482,#83483) ;
#70427 = AXIS2_PLACEMENT_3D('',#107836,#83484,#83485) ;
#70428 = AXIS2_PLACEMENT_3D('',#107837,#83486,#83487) ;
#70429 = AXIS2_PLACEMENT_3D('',#107838,#83488,#83489) ;
#70430 = AXIS2_PLACEMENT_3D('',#107839,#83490,#83491) ;
#70431 = AXIS2_PLACEMENT_3D('',#107840,#83492,#83493) ;
#70432 = AXIS2_PLACEMENT_3D('',#107841,#83494,#83495) ;
#70433 = AXIS2_PLACEMENT_3D('',#107842,#83496,#83497) ;
#70434 = AXIS2_PLACEMENT_3D('',#107843,#83498,#83499) ;
#70435 = AXIS2_PLACEMENT_3D('',#107844,#83500,#83501) ;
#70436 = AXIS2_PLACEMENT_3D('',#107845,#83502,#83503) ;
#70437 = AXIS2_PLACEMENT_3D('',#107846,#83504,#83505) ;
#70438 = AXIS2_PLACEMENT_3D('',#107847,#83506,#83507) ;
#70439 = AXIS2_PLACEMENT_3D('',#107848,#83508,#83509) ;
#70440 = AXIS2_PLACEMENT_3D('',#107849,#83510,#83511) ;
#70441 = AXIS2_PLACEMENT_3D('',#107850,#83512,#83513) ;
#70442 = AXIS2_PLACEMENT_3D('',#107851,#83514,#83515) ;
#70443 = AXIS2_PLACEMENT_3D('',#107852,#83516,#83517) ;
#70444 = AXIS2_PLACEMENT_3D('',#107853,#83518,#83519) ;
#70445 = AXIS2_PLACEMENT_3D('',#107854,#83520,#83521) ;
#70446 = AXIS2_PLACEMENT_3D('',#107855,#83522,#83523) ;
#70447 = AXIS2_PLACEMENT_3D('',#107856,#83524,#83525) ;
#70448 = AXIS2_PLACEMENT_3D('',#107857,#83526,#83527) ;
#70449 = AXIS2_PLACEMENT_3D('',#107858,#83528,#83529) ;
#70450 = AXIS2_PLACEMENT_3D('',#107859,#83530,#83531) ;
#70451 = AXIS2_PLACEMENT_3D('',#107860,#83532,#83533) ;
#70452 = AXIS2_PLACEMENT_3D('',#107861,#83534,#83535) ;
#70453 = AXIS2_PLACEMENT_3D('',#107862,#83536,#83537) ;
#70454 = AXIS2_PLACEMENT_3D('',#107869,#83538,#83539) ;
#70455 = AXIS2_PLACEMENT_3D('',#107870,#83540,#83541) ;
#70456 = AXIS2_PLACEMENT_3D('',#107871,#83542,#83543) ;
#70457 = AXIS2_PLACEMENT_3D('',#107872,#83544,#83545) ;
#70458 = AXIS2_PLACEMENT_3D('',#107873,#83546,#83547) ;
#70459 = AXIS2_PLACEMENT_3D('',#107874,#83548,#83549) ;
#70460 = AXIS2_PLACEMENT_3D('',#107875,#83550,#83551) ;
#70461 = AXIS2_PLACEMENT_3D('',#107876,#83552,#83553) ;
#70462 = AXIS2_PLACEMENT_3D('',#107877,#83554,#83555) ;
#70463 = AXIS2_PLACEMENT_3D('',#107878,#83556,#83557) ;
#70464 = AXIS2_PLACEMENT_3D('',#107879,#83558,#83559) ;
#70465 = AXIS2_PLACEMENT_3D('',#107880,#83560,#83561) ;
#70466 = AXIS2_PLACEMENT_3D('',#107881,#83562,#83563) ;
#70467 = AXIS2_PLACEMENT_3D('',#107882,#83564,#83565) ;
#70468 = AXIS2_PLACEMENT_3D('',#107883,#83566,#83567) ;
#70469 = AXIS2_PLACEMENT_3D('',#107884,#83568,#83569) ;
#70470 = AXIS2_PLACEMENT_3D('',#107885,#83570,#83571) ;
#70471 = AXIS2_PLACEMENT_3D('',#107886,#83572,#83573) ;
#70472 = AXIS2_PLACEMENT_3D('',#107887,#83574,#83575) ;
#70473 = AXIS2_PLACEMENT_3D('',#107888,#83576,#83577) ;
#70474 = AXIS2_PLACEMENT_3D('',#107889,#83578,#83579) ;
#70475 = AXIS2_PLACEMENT_3D('',#107890,#83580,#83581) ;
#70476 = AXIS2_PLACEMENT_3D('',#107891,#83582,#83583) ;
#70477 = AXIS2_PLACEMENT_3D('',#107892,#83584,#83585) ;
#70478 = AXIS2_PLACEMENT_3D('',#107893,#83586,#83587) ;
#70479 = AXIS2_PLACEMENT_3D('',#107894,#83588,#83589) ;
#70480 = AXIS2_PLACEMENT_3D('',#107895,#83590,#83591) ;
#70481 = AXIS2_PLACEMENT_3D('',#107896,#83592,#83593) ;
#70482 = AXIS2_PLACEMENT_3D('',#107897,#83594,#83595) ;
#70483 = AXIS2_PLACEMENT_3D('',#107898,#83596,#83597) ;
#70484 = AXIS2_PLACEMENT_3D('',#107899,#83598,#83599) ;
#70485 = AXIS2_PLACEMENT_3D('',#107900,#83600,#83601) ;
#70486 = AXIS2_PLACEMENT_3D('',#107901,#83602,#83603) ;
#70487 = AXIS2_PLACEMENT_3D('',#107902,#83604,#83605) ;
#70488 = AXIS2_PLACEMENT_3D('',#107903,#83606,#83607) ;
#70489 = AXIS2_PLACEMENT_3D('',#107904,#83608,#83609) ;
#70490 = AXIS2_PLACEMENT_3D('',#107905,#83610,#83611) ;
#70491 = AXIS2_PLACEMENT_3D('',#107906,#83612,#83613) ;
#70492 = AXIS2_PLACEMENT_3D('',#107907,#83614,#83615) ;
#70493 = AXIS2_PLACEMENT_3D('',#107938,#83616,#83617) ;
#70494 = AXIS2_PLACEMENT_3D('',#107939,#83618,#83619) ;
#70495 = AXIS2_PLACEMENT_3D('',#107940,#83620,#83621) ;
#70496 = AXIS2_PLACEMENT_3D('',#107941,#83622,#83623) ;
#70497 = AXIS2_PLACEMENT_3D('',#107942,#83624,#83625) ;
#70498 = AXIS2_PLACEMENT_3D('',#107943,#83626,#83627) ;
#70499 = AXIS2_PLACEMENT_3D('',#107944,#83628,#83629) ;
#70500 = AXIS2_PLACEMENT_3D('',#107945,#83630,#83631) ;
#70501 = AXIS2_PLACEMENT_3D('',#107946,#83632,#83633) ;
#70502 = AXIS2_PLACEMENT_3D('',#107947,#83634,#83635) ;
#70503 = AXIS2_PLACEMENT_3D('',#107974,#83636,#83637) ;
#70504 = AXIS2_PLACEMENT_3D('',#107975,#83638,#83639) ;
#70505 = AXIS2_PLACEMENT_3D('',#107976,#83640,#83641) ;
#70506 = AXIS2_PLACEMENT_3D('',#107977,#83642,#83643) ;
#70507 = AXIS2_PLACEMENT_3D('',#107978,#83644,#83645) ;
#70508 = AXIS2_PLACEMENT_3D('',#107979,#83646,#83647) ;
#70509 = AXIS2_PLACEMENT_3D('',#107980,#83648,#83649) ;
#70510 = AXIS2_PLACEMENT_3D('',#107981,#83650,#83651) ;
#70511 = AXIS2_PLACEMENT_3D('',#107982,#83652,#83653) ;
#70512 = AXIS2_PLACEMENT_3D('',#107983,#83654,#83655) ;
#70513 = AXIS2_PLACEMENT_3D('',#107984,#83656,#83657) ;
#70514 = AXIS2_PLACEMENT_3D('',#107985,#83658,#83659) ;
#70515 = AXIS2_PLACEMENT_3D('',#107986,#83660,#83661) ;
#70516 = AXIS2_PLACEMENT_3D('',#107987,#83662,#83663) ;
#70517 = AXIS2_PLACEMENT_3D('',#107988,#83664,#83665) ;
#70518 = AXIS2_PLACEMENT_3D('',#107989,#83666,#83667) ;
#70519 = AXIS2_PLACEMENT_3D('',#107990,#83668,#83669) ;
#70520 = AXIS2_PLACEMENT_3D('',#107991,#83670,#83671) ;
#70521 = AXIS2_PLACEMENT_3D('',#107992,#83672,#83673) ;
#70522 = AXIS2_PLACEMENT_3D('',#107993,#83674,#83675) ;
#70523 = AXIS2_PLACEMENT_3D('',#107994,#83676,#83677) ;
#70524 = AXIS2_PLACEMENT_3D('',#107995,#83678,#83679) ;
#70525 = AXIS2_PLACEMENT_3D('',#107996,#83680,#83681) ;
#70526 = AXIS2_PLACEMENT_3D('',#107997,#83682,#83683) ;
#70527 = AXIS2_PLACEMENT_3D('',#107998,#83684,#83685) ;
#70528 = AXIS2_PLACEMENT_3D('',#107999,#83686,#83687) ;
#70529 = AXIS2_PLACEMENT_3D('',#108000,#83688,#83689) ;
#70530 = AXIS2_PLACEMENT_3D('',#108001,#83690,#83691) ;
#70531 = AXIS2_PLACEMENT_3D('',#108002,#83692,#83693) ;
#70532 = AXIS2_PLACEMENT_3D('',#108027,#83694,#83695) ;
#70533 = AXIS2_PLACEMENT_3D('',#108028,#83696,#83697) ;
#70534 = AXIS2_PLACEMENT_3D('',#108029,#83698,#83699) ;
#70535 = AXIS2_PLACEMENT_3D('',#108030,#83700,#83701) ;
#70536 = AXIS2_PLACEMENT_3D('',#108031,#83702,#83703) ;
#70537 = AXIS2_PLACEMENT_3D('',#108032,#83704,#83705) ;
#70538 = AXIS2_PLACEMENT_3D('',#108033,#83706,#83707) ;
#70539 = AXIS2_PLACEMENT_3D('',#108082,#83708,#83709) ;
#70540 = AXIS2_PLACEMENT_3D('',#108083,#83710,#83711) ;
#70541 = AXIS2_PLACEMENT_3D('',#108084,#83712,#83713) ;
#70542 = AXIS2_PLACEMENT_3D('',#108085,#83714,#83715) ;
#70543 = AXIS2_PLACEMENT_3D('',#108086,#83716,#83717) ;
#70544 = AXIS2_PLACEMENT_3D('',#108087,#83718,#83719) ;
#70545 = AXIS2_PLACEMENT_3D('',#108088,#83720,#83721) ;
#70546 = AXIS2_PLACEMENT_3D('',#108150,#83722,#83723) ;
#70547 = AXIS2_PLACEMENT_3D('',#108151,#83724,#83725) ;
#70548 = AXIS2_PLACEMENT_3D('',#108152,#83726,#83727) ;
#70549 = AXIS2_PLACEMENT_3D('',#108325,#83728,#83729) ;
#70550 = AXIS2_PLACEMENT_3D('',#108326,#83730,#83731) ;
#70551 = AXIS2_PLACEMENT_3D('',#108381,#83732,#83733) ;
#70552 = AXIS2_PLACEMENT_3D('',#108428,#83734,#83735) ;
#70553 = AXIS2_PLACEMENT_3D('',#108429,#83736,#83737) ;
#70554 = AXIS2_PLACEMENT_3D('',#108430,#83738,#83739) ;
#70555 = AXIS2_PLACEMENT_3D('',#108431,#83740,#83741) ;
#70556 = AXIS2_PLACEMENT_3D('',#108432,#83742,#83743) ;
#70557 = AXIS2_PLACEMENT_3D('',#108433,#83744,#83745) ;
#70558 = AXIS2_PLACEMENT_3D('',#108538,#83746,#83747) ;
#70559 = AXIS2_PLACEMENT_3D('',#108539,#83748,#83749) ;
#70560 = AXIS2_PLACEMENT_3D('',#108540,#83750,#83751) ;
#70561 = AXIS2_PLACEMENT_3D('',#108541,#83752,#83753) ;
#70562 = AXIS2_PLACEMENT_3D('',#108554,#83754,#83755) ;
#70563 = AXIS2_PLACEMENT_3D('',#108555,#83756,#83757) ;
#70564 = AXIS2_PLACEMENT_3D('',#108556,#83758,#83759) ;
#70565 = AXIS2_PLACEMENT_3D('',#108557,#83760,#83761) ;
#70566 = AXIS2_PLACEMENT_3D('',#108558,#83762,#83763) ;
#70567 = AXIS2_PLACEMENT_3D('',#108559,#83764,#83765) ;
#70568 = AXIS2_PLACEMENT_3D('',#108560,#83766,#83767) ;
#70569 = AXIS2_PLACEMENT_3D('',#108561,#83768,#83769) ;
#70570 = AXIS2_PLACEMENT_3D('',#108562,#83770,#83771) ;
#70571 = AXIS2_PLACEMENT_3D('',#108563,#83772,#83773) ;
#70572 = AXIS2_PLACEMENT_3D('',#108564,#83774,#83775) ;
#70573 = AXIS2_PLACEMENT_3D('',#108565,#83776,#83777) ;
#70574 = AXIS2_PLACEMENT_3D('',#108566,#83778,#83779) ;
#70575 = AXIS2_PLACEMENT_3D('',#108567,#83780,#83781) ;
#70576 = AXIS2_PLACEMENT_3D('',#108568,#83782,#83783) ;
#70577 = AXIS2_PLACEMENT_3D('',#108569,#83784,#83785) ;
#70578 = AXIS2_PLACEMENT_3D('',#108570,#83786,#83787) ;
#70579 = AXIS2_PLACEMENT_3D('',#108571,#83788,#83789) ;
#70580 = AXIS2_PLACEMENT_3D('',#108572,#83790,#83791) ;
#70581 = AXIS2_PLACEMENT_3D('',#108573,#83792,#83793) ;
#70582 = AXIS2_PLACEMENT_3D('',#108574,#83794,#83795) ;
#70583 = AXIS2_PLACEMENT_3D('',#108575,#83796,#83797) ;
#70584 = AXIS2_PLACEMENT_3D('',#108576,#83798,#83799) ;
#70585 = AXIS2_PLACEMENT_3D('',#108577,#83800,#83801) ;
#70586 = AXIS2_PLACEMENT_3D('',#108578,#83802,#83803) ;
#70587 = AXIS2_PLACEMENT_3D('',#108579,#83804,#83805) ;
#70588 = AXIS2_PLACEMENT_3D('',#108580,#83806,#83807) ;
#70589 = AXIS2_PLACEMENT_3D('',#108581,#83808,#83809) ;
#70590 = AXIS2_PLACEMENT_3D('',#108582,#83810,#83811) ;
#70591 = AXIS2_PLACEMENT_3D('',#108583,#83812,#83813) ;
#70592 = AXIS2_PLACEMENT_3D('',#108584,#83814,#83815) ;
#70593 = AXIS2_PLACEMENT_3D('',#108585,#83816,#83817) ;
#70594 = AXIS2_PLACEMENT_3D('',#108586,#83818,#83819) ;
#70595 = AXIS2_PLACEMENT_3D('',#108587,#83820,#83821) ;
#70596 = AXIS2_PLACEMENT_3D('',#108588,#83822,#83823) ;
#70597 = AXIS2_PLACEMENT_3D('',#108589,#83824,#83825) ;
#70598 = AXIS2_PLACEMENT_3D('',#108590,#83826,#83827) ;
#70599 = AXIS2_PLACEMENT_3D('',#108591,#83828,#83829) ;
#70600 = AXIS2_PLACEMENT_3D('',#108604,#83830,#83831) ;
#70601 = AXIS2_PLACEMENT_3D('',#108605,#83832,#83833) ;
#70602 = AXIS2_PLACEMENT_3D('',#108606,#83834,#83835) ;
#70603 = AXIS2_PLACEMENT_3D('',#108607,#83836,#83837) ;
#70604 = AXIS2_PLACEMENT_3D('',#108662,#83838,#83839) ;
#70605 = AXIS2_PLACEMENT_3D('',#108663,#83840,#83841) ;
#70606 = AXIS2_PLACEMENT_3D('',#108664,#83842,#83843) ;
#70607 = AXIS2_PLACEMENT_3D('',#108719,#83844,#83845) ;
#70608 = AXIS2_PLACEMENT_3D('',#108720,#83846,#83847) ;
#70609 = AXIS2_PLACEMENT_3D('',#108746,#83848,#83849) ;
#70610 = AXIS2_PLACEMENT_3D('',#108748,#83850,#83851) ;
#70611 = AXIS2_PLACEMENT_3D('',#108750,#83852,#83853) ;
#70612 = AXIS2_PLACEMENT_3D('',#108789,#83854,#83855) ;
#70613 = AXIS2_PLACEMENT_3D('',#108791,#83856,#83857) ;
#70614 = AXIS2_PLACEMENT_3D('',#108793,#83858,#83859) ;
#70615 = AXIS2_PLACEMENT_3D('',#108794,#83860,#83861) ;
#70616 = AXIS2_PLACEMENT_3D('',#108795,#83862,#83863) ;
#70617 = AXIS2_PLACEMENT_3D('',#108797,#83864,#83865) ;
#70618 = AXIS2_PLACEMENT_3D('',#108799,#83866,#83867) ;
#70619 = AXIS2_PLACEMENT_3D('',#108800,#83868,#83869) ;
#70620 = AXIS2_PLACEMENT_3D('',#108801,#83870,#83871) ;
#70621 = AXIS2_PLACEMENT_3D('',#108803,#83872,#83873) ;
#70622 = AXIS2_PLACEMENT_3D('',#108805,#83874,#83875) ;
#70623 = AXIS2_PLACEMENT_3D('',#108806,#83876,#83877) ;
#70624 = AXIS2_PLACEMENT_3D('',#108807,#83878,#83879) ;
#70625 = AXIS2_PLACEMENT_3D('',#108810,#83880,#83881) ;
#70626 = AXIS2_PLACEMENT_3D('',#108814,#83883,#83884) ;
#70627 = AXIS2_PLACEMENT_3D('',#108816,#83885,#83886) ;
#70628 = AXIS2_PLACEMENT_3D('',#108818,#83888,#83889) ;
#70629 = AXIS2_PLACEMENT_3D('',#108821,#83890,#83891) ;
#70630 = AXIS2_PLACEMENT_3D('',#108825,#83893,#83894) ;
#70631 = AXIS2_PLACEMENT_3D('',#108827,#83896,#83897) ;
#70632 = AXIS2_PLACEMENT_3D('',#108830,#83898,#83899) ;
#70633 = AXIS2_PLACEMENT_3D('',#108832,#83900,#83901) ;
#70634 = AXIS2_PLACEMENT_3D('',#108834,#83902,#83903) ;
#70635 = AXIS2_PLACEMENT_3D('',#108835,#83904,#83905) ;
#70636 = AXIS2_PLACEMENT_3D('',#108836,#83906,#83907) ;
#70637 = AXIS2_PLACEMENT_3D('',#108838,#83909,#83910) ;
#70638 = AXIS2_PLACEMENT_3D('',#108841,#83912,#83913) ;
#70639 = AXIS2_PLACEMENT_3D('',#108850,#83914,#83915) ;
#70640 = AXIS2_PLACEMENT_3D('',#108858,#83916,#83917) ;
#70641 = AXIS2_PLACEMENT_3D('',#108860,#83919,#83920) ;
#70642 = AXIS2_PLACEMENT_3D('',#108876,#83924,#83925) ;
#70643 = AXIS2_PLACEMENT_3D('',#108878,#83927,#83928) ;
#70644 = AXIS2_PLACEMENT_3D('',#108927,#83933,#83934) ;
#70645 = AXIS2_PLACEMENT_3D('',#108936,#83939,#83940) ;
#70646 = AXIS2_PLACEMENT_3D('',#108966,#83945,#83946) ;
#70647 = AXIS2_PLACEMENT_3D('',#108975,#83951,#83952) ;
#70648 = AXIS2_PLACEMENT_3D('',#108984,#83957,#83958) ;
#70649 = AXIS2_PLACEMENT_3D('',#108995,#83963,#83964) ;
#70650 = AXIS2_PLACEMENT_3D('',#108997,#83966,#83967) ;
#70651 = AXIS2_PLACEMENT_3D('',#109001,#83969,#83970) ;
#70652 = AXIS2_PLACEMENT_3D('',#109002,#83971,#83972) ;
#70653 = AXIS2_PLACEMENT_3D('',#109003,#83973,#83974) ;
#70654 = AXIS2_PLACEMENT_3D('',#109005,#83975,#83976) ;
#70655 = AXIS2_PLACEMENT_3D('',#109009,#83978,#83979) ;
#70656 = AXIS2_PLACEMENT_3D('',#109013,#83981,#83982) ;
#70657 = AXIS2_PLACEMENT_3D('',#109017,#83984,#83985) ;
#70658 = AXIS2_PLACEMENT_3D('',#109021,#83987,#83988) ;
#70659 = AXIS2_PLACEMENT_3D('',#109025,#83990,#83991) ;
#70660 = AXIS2_PLACEMENT_3D('',#109028,#83993,#83994) ;
#70661 = AXIS2_PLACEMENT_3D('',#109030,#83995,#83996) ;
#70662 = AXIS2_PLACEMENT_3D('',#109033,#83998,#83999) ;
#70663 = AXIS2_PLACEMENT_3D('',#109035,#84000,#84001) ;
#70664 = AXIS2_PLACEMENT_3D('',#109041,#84004,#84005) ;
#70665 = AXIS2_PLACEMENT_3D('',#109045,#84007,#84008) ;
#70666 = AXIS2_PLACEMENT_3D('',#109048,#84010,#84011) ;
#70667 = AXIS2_PLACEMENT_3D('',#109049,#84012,#84013) ;
#70668 = AXIS2_PLACEMENT_3D('',#109054,#84015,#84016) ;
#70669 = AXIS2_PLACEMENT_3D('',#109058,#84018,#84019) ;
#70670 = AXIS2_PLACEMENT_3D('',#109062,#84021,#84022) ;
#70671 = AXIS2_PLACEMENT_3D('',#109066,#84024,#84025) ;
#70672 = AXIS2_PLACEMENT_3D('',#109071,#84028,#84029) ;
#70673 = AXIS2_PLACEMENT_3D('',#109073,#84030,#84031) ;
#70674 = AXIS2_PLACEMENT_3D('',#109076,#84033,#84034) ;
#70675 = AXIS2_PLACEMENT_3D('',#109078,#84035,#84036) ;
#70676 = AXIS2_PLACEMENT_3D('',#109082,#84038,#84039) ;
#70677 = AXIS2_PLACEMENT_3D('',#109086,#84041,#84042) ;
#70678 = AXIS2_PLACEMENT_3D('',#109090,#84044,#84045) ;
#70679 = AXIS2_PLACEMENT_3D('',#109094,#84047,#84048) ;
#70680 = AXIS2_PLACEMENT_3D('',#109098,#84050,#84051) ;
#70681 = AXIS2_PLACEMENT_3D('',#109102,#84053,#84054) ;
#70682 = AXIS2_PLACEMENT_3D('',#109106,#84056,#84057) ;
#70683 = AXIS2_PLACEMENT_3D('',#109109,#84059,#84060) ;
#70684 = AXIS2_PLACEMENT_3D('',#109110,#84061,#84062) ;
#70685 = AXIS2_PLACEMENT_3D('',#109113,#84065,#84066) ;
#70686 = AXIS2_PLACEMENT_3D('',#109116,#84069,#84070) ;
#70687 = AXIS2_PLACEMENT_3D('',#109205,#84075,#84076) ;
#70688 = AXIS2_PLACEMENT_3D('',#109216,#84077,#84078) ;
#70689 = AXIS2_PLACEMENT_3D('',#109221,#84082,#84083) ;
#70690 = AXIS2_PLACEMENT_3D('',#109227,#84087,#84088) ;
#70691 = AXIS2_PLACEMENT_3D('',#109247,#84092,#84093) ;
#70692 = AXIS2_PLACEMENT_3D('',#109346,#84099,#84100) ;
#70693 = AXIS2_PLACEMENT_3D('',#109350,#84102,#84103) ;
#70694 = AXIS2_PLACEMENT_3D('',#109354,#84106,#84107) ;
#70695 = AXIS2_PLACEMENT_3D('',#109357,#84108,#84109) ;
#70696 = AXIS2_PLACEMENT_3D('',#109362,#84112,#84113) ;
#70697 = AXIS2_PLACEMENT_3D('',#109364,#84114,#84115) ;
#70698 = AXIS2_PLACEMENT_3D('',#109366,#84116,#84117) ;
#70699 = AXIS2_PLACEMENT_3D('',#109374,#84121,#84122) ;
#70700 = AXIS2_PLACEMENT_3D('',#109376,#84123,#84124) ;
#70701 = AXIS2_PLACEMENT_3D('',#109378,#84125,#84126) ;
#70702 = AXIS2_PLACEMENT_3D('',#109383,#84129,#84130) ;
#70703 = AXIS2_PLACEMENT_3D('',#109385,#84131,#84132) ;
#70704 = AXIS2_PLACEMENT_3D('',#109387,#84133,#84134) ;
#70705 = AXIS2_PLACEMENT_3D('',#109391,#84136,#84137) ;
#70706 = AXIS2_PLACEMENT_3D('',#109395,#84139,#84140) ;
#70707 = AXIS2_PLACEMENT_3D('',#109396,#84141,#84142) ;
#70708 = AXIS2_PLACEMENT_3D('',#109397,#84143,#84144) ;
#70709 = AXIS2_PLACEMENT_3D('',#109400,#84145,#84146) ;
#70710 = AXIS2_PLACEMENT_3D('',#109410,#84152,#84153) ;
#70711 = AXIS2_PLACEMENT_3D('',#109412,#84155,#84156) ;
#70712 = AXIS2_PLACEMENT_3D('',#109415,#84157,#84158) ;
#70713 = AXIS2_PLACEMENT_3D('',#109421,#84162,#84163) ;
#70714 = AXIS2_PLACEMENT_3D('',#109423,#84165,#84166) ;
#70715 = AXIS2_PLACEMENT_3D('',#109429,#84169,#84170) ;
#70716 = AXIS2_PLACEMENT_3D('',#109430,#84171,#84172) ;
#70717 = AXIS2_PLACEMENT_3D('',#109433,#84173,#84174) ;
#70718 = AXIS2_PLACEMENT_3D('',#109437,#84177,#84178) ;
#70719 = AXIS2_PLACEMENT_3D('',#109454,#84187,#84188) ;
#70720 = AXIS2_PLACEMENT_3D('',#109463,#84193,#84194) ;
#70721 = AXIS2_PLACEMENT_3D('',#109472,#84199,#84200) ;
#70722 = AXIS2_PLACEMENT_3D('',#109481,#84205,#84206) ;
#70723 = AXIS2_PLACEMENT_3D('',#109508,#84211,#84212) ;
#70724 = AXIS2_PLACEMENT_3D('',#109525,#84221,#84222) ;
#70725 = AXIS2_PLACEMENT_3D('',#109530,#84224,#84225) ;
#70726 = AXIS2_PLACEMENT_3D('',#109534,#84227,#84228) ;
#70727 = AXIS2_PLACEMENT_3D('',#109538,#84230,#84231) ;
#70728 = AXIS2_PLACEMENT_3D('',#109541,#84233,#84234) ;
#70729 = AXIS2_PLACEMENT_3D('',#109542,#84235,#84236) ;
#70730 = AXIS2_PLACEMENT_3D('',#109545,#84237,#84238) ;
#70731 = AXIS2_PLACEMENT_3D('',#109550,#84241,#84242) ;
#70732 = AXIS2_PLACEMENT_3D('',#109553,#84244,#84245) ;
#70733 = AXIS2_PLACEMENT_3D('',#109554,#84246,#84247) ;
#70734 = AXIS2_PLACEMENT_3D('',#109560,#84251,#84252) ;
#70735 = AXIS2_PLACEMENT_3D('',#109566,#84256,#84257) ;
#70736 = AXIS2_PLACEMENT_3D('',#109569,#84258,#84259) ;
#70737 = AXIS2_PLACEMENT_3D('',#109573,#84261,#84262) ;
#70738 = AXIS2_PLACEMENT_3D('',#109575,#84264,#84265) ;
#70739 = AXIS2_PLACEMENT_3D('',#109578,#84266,#84267) ;
#70740 = AXIS2_PLACEMENT_3D('',#109582,#84269,#84270) ;
#70741 = AXIS2_PLACEMENT_3D('',#109584,#84272,#84273) ;
#70742 = AXIS2_PLACEMENT_3D('',#109590,#84277,#84278) ;
#70743 = AXIS2_PLACEMENT_3D('',#109596,#84282,#84283) ;
#70744 = AXIS2_PLACEMENT_3D('',#109599,#84284,#84285) ;
#70745 = AXIS2_PLACEMENT_3D('',#109604,#84288,#84289) ;
#70746 = AXIS2_PLACEMENT_3D('',#109606,#84290,#84291) ;
#70747 = AXIS2_PLACEMENT_3D('',#109608,#84293,#84294) ;
#70748 = AXIS2_PLACEMENT_3D('',#109611,#84295,#84296) ;
#70749 = AXIS2_PLACEMENT_3D('',#109616,#84300,#84301) ;
#70750 = AXIS2_PLACEMENT_3D('',#109622,#84305,#84306) ;
#70751 = AXIS2_PLACEMENT_3D('',#109625,#84307,#84308) ;
#70752 = AXIS2_PLACEMENT_3D('',#109629,#84310,#84311) ;
#70753 = AXIS2_PLACEMENT_3D('',#109631,#84313,#84314) ;
#70754 = AXIS2_PLACEMENT_3D('',#109640,#84319,#84320) ;
#70755 = AXIS2_PLACEMENT_3D('',#109643,#84321,#84322) ;
#70756 = AXIS2_PLACEMENT_3D('',#109647,#84324,#84325) ;
#70757 = AXIS2_PLACEMENT_3D('',#109649,#84327,#84328) ;
#70758 = AXIS2_PLACEMENT_3D('',#109655,#84332,#84333) ;
#70759 = AXIS2_PLACEMENT_3D('',#109664,#84338,#84339) ;
#70760 = AXIS2_PLACEMENT_3D('',#109671,#84343,#84344) ;
#70761 = AXIS2_PLACEMENT_3D('',#109672,#84345,#84346) ;
#70762 = AXIS2_PLACEMENT_3D('',#109681,#84351,#84352) ;
#70763 = AXIS2_PLACEMENT_3D('',#109684,#84353,#84354) ;
#70764 = AXIS2_PLACEMENT_3D('',#109689,#84357,#84358) ;
#70765 = AXIS2_PLACEMENT_3D('',#109693,#84360,#84361) ;
#70766 = AXIS2_PLACEMENT_3D('',#109695,#84363,#84364) ;
#70767 = AXIS2_PLACEMENT_3D('',#109703,#84369,#84370) ;
#70768 = AXIS2_PLACEMENT_3D('',#109712,#84375,#84376) ;
#70769 = AXIS2_PLACEMENT_3D('',#109721,#84381,#84382) ;
#70770 = AXIS2_PLACEMENT_3D('',#109730,#84387,#84388) ;
#70771 = AXIS2_PLACEMENT_3D('',#109736,#84392,#84393) ;
#70772 = AXIS2_PLACEMENT_3D('',#109742,#84397,#84398) ;
#70773 = AXIS2_PLACEMENT_3D('',#109748,#84402,#84403) ;
#70774 = AXIS2_PLACEMENT_3D('',#109754,#84407,#84408) ;
#70775 = AXIS2_PLACEMENT_3D('',#109763,#84412,#84413) ;
#70776 = AXIS2_PLACEMENT_3D('',#109766,#84415,#84416) ;
#70777 = AXIS2_PLACEMENT_3D('',#109767,#84417,#84418) ;
#70778 = AXIS2_PLACEMENT_3D('',#109776,#84422,#84423) ;
#70779 = AXIS2_PLACEMENT_3D('',#109779,#84425,#84426) ;
#70780 = AXIS2_PLACEMENT_3D('',#109780,#84427,#84428) ;
#70781 = AXIS2_PLACEMENT_3D('',#109784,#84430,#84431) ;
#70782 = AXIS2_PLACEMENT_3D('',#109785,#84432,#84433) ;
#70783 = AXIS2_PLACEMENT_3D('',#109786,#84434,#84435) ;
#70784 = AXIS2_PLACEMENT_3D('',#109792,#84439,#84440) ;
#70785 = AXIS2_PLACEMENT_3D('',#109801,#84445,#84446) ;
#70786 = AXIS2_PLACEMENT_3D('',#109810,#84451,#84452) ;
#70787 = AXIS2_PLACEMENT_3D('',#109819,#84457,#84458) ;
#70788 = AXIS2_PLACEMENT_3D('',#109828,#84463,#84464) ;
#70789 = AXIS2_PLACEMENT_3D('',#109829,#84465,#84466) ;
#70790 = AXIS2_PLACEMENT_3D('',#109830,#84467,#84468) ;
#70791 = AXIS2_PLACEMENT_3D('',#109831,#84469,#84470) ;
#70792 = AXIS2_PLACEMENT_3D('',#109840,#84475,#84476) ;
#70793 = AXIS2_PLACEMENT_3D('',#109849,#84481,#84482) ;
#70794 = AXIS2_PLACEMENT_3D('',#109858,#84487,#84488) ;
#70795 = AXIS2_PLACEMENT_3D('',#109867,#84493,#84494) ;
#70796 = AXIS2_PLACEMENT_3D('',#109871,#84496,#84497) ;
#70797 = AXIS2_PLACEMENT_3D('',#109873,#84499,#84500) ;
#70798 = AXIS2_PLACEMENT_3D('',#109876,#84501,#84502) ;
#70799 = AXIS2_PLACEMENT_3D('',#109877,#84503,#84504) ;
#70800 = AXIS2_PLACEMENT_3D('',#109878,#84505,#84506) ;
#70801 = AXIS2_PLACEMENT_3D('',#109879,#84507,#84508) ;
#70802 = AXIS2_PLACEMENT_3D('',#109883,#84510,#84511) ;
#70803 = AXIS2_PLACEMENT_3D('',#109885,#84513,#84514) ;
#70804 = AXIS2_PLACEMENT_3D('',#109886,#84515,#84516) ;
#70805 = AXIS2_PLACEMENT_3D('',#109887,#84517,#84518) ;
#70806 = AXIS2_PLACEMENT_3D('',#109888,#84519,#84520) ;
#70807 = AXIS2_PLACEMENT_3D('',#109889,#84521,#84522) ;
#70808 = AXIS2_PLACEMENT_3D('',#109890,#84523,#84524) ;
#70809 = AXIS2_PLACEMENT_3D('',#109891,#84525,#84526) ;
#70810 = AXIS2_PLACEMENT_3D('',#109892,#84527,#84528) ;
#70811 = AXIS2_PLACEMENT_3D('',#109893,#84529,#84530) ;
#70812 = AXIS2_PLACEMENT_3D('',#109894,#84531,#84532) ;
#70813 = AXIS2_PLACEMENT_3D('',#109895,#84533,#84534) ;
#70814 = AXIS2_PLACEMENT_3D('',#109896,#84535,#84536) ;
#70815 = AXIS2_PLACEMENT_3D('',#109897,#84537,#84538) ;
#70816 = AXIS2_PLACEMENT_3D('',#109898,#84539,#84540) ;
#70817 = AXIS2_PLACEMENT_3D('',#109899,#84541,#84542) ;
#70818 = AXIS2_PLACEMENT_3D('',#109900,#84543,#84544) ;
#70819 = AXIS2_PLACEMENT_3D('',#109901,#84545,#84546) ;
#70820 = AXIS2_PLACEMENT_3D('',#109902,#84547,#84548) ;
#70821 = AXIS2_PLACEMENT_3D('',#109903,#84549,#84550) ;
#70822 = AXIS2_PLACEMENT_3D('',#109904,#84551,#84552) ;
#70823 = AXIS2_PLACEMENT_3D('',#109905,#84553,#84554) ;
#70824 = AXIS2_PLACEMENT_3D('',#109906,#84555,#84556) ;
#70825 = AXIS2_PLACEMENT_3D('',#109907,#84557,#84558) ;
#70826 = AXIS2_PLACEMENT_3D('',#109908,#84559,#84560) ;
#70827 = AXIS2_PLACEMENT_3D('',#109909,#84561,#84562) ;
#70828 = AXIS2_PLACEMENT_3D('',#109910,#84563,#84564) ;
#70829 = AXIS2_PLACEMENT_3D('',#109911,#84565,#84566) ;
#70830 = AXIS2_PLACEMENT_3D('',#109912,#84567,#84568) ;
#70831 = AXIS2_PLACEMENT_3D('',#109913,#84569,#84570) ;
#70832 = AXIS2_PLACEMENT_3D('',#109914,#84571,#84572) ;
#70833 = AXIS2_PLACEMENT_3D('',#109915,#84573,#84574) ;
#70834 = AXIS2_PLACEMENT_3D('',#109916,#84575,#84576) ;
#70835 = AXIS2_PLACEMENT_3D('',#109917,#84577,#84578) ;
#70836 = AXIS2_PLACEMENT_3D('',#109918,#84579,#84580) ;
#70837 = AXIS2_PLACEMENT_3D('',#109919,#84581,#84582) ;
#70838 = AXIS2_PLACEMENT_3D('',#109920,#84583,#84584) ;
#70839 = AXIS2_PLACEMENT_3D('',#109921,#84585,#84586) ;
#70840 = AXIS2_PLACEMENT_3D('',#109922,#84587,#84588) ;
#70841 = AXIS2_PLACEMENT_3D('',#109923,#84589,#84590) ;
#70842 = AXIS2_PLACEMENT_3D('',#109924,#84591,#84592) ;
#70843 = AXIS2_PLACEMENT_3D('',#109925,#84593,#84594) ;
#70844 = AXIS2_PLACEMENT_3D('',#109926,#84595,#84596) ;
#70845 = AXIS2_PLACEMENT_3D('',#109927,#84597,#84598) ;
#70846 = AXIS2_PLACEMENT_3D('',#109928,#84599,#84600) ;
#70847 = AXIS2_PLACEMENT_3D('',#109929,#84601,#84602) ;
#70848 = AXIS2_PLACEMENT_3D('',#109930,#84603,#84604) ;
#70849 = AXIS2_PLACEMENT_3D('',#109931,#84605,#84606) ;
#70850 = AXIS2_PLACEMENT_3D('',#109932,#84607,#84608) ;
#70851 = AXIS2_PLACEMENT_3D('',#109933,#84609,#84610) ;
#70852 = AXIS2_PLACEMENT_3D('',#109934,#84611,#84612) ;
#70853 = AXIS2_PLACEMENT_3D('',#109935,#84613,#84614) ;
#70854 = AXIS2_PLACEMENT_3D('',#109936,#84615,#84616) ;
#70855 = AXIS2_PLACEMENT_3D('',#109937,#84617,#84618) ;
#70856 = AXIS2_PLACEMENT_3D('',#109938,#84619,#84620) ;
#70857 = AXIS2_PLACEMENT_3D('',#109939,#84621,#84622) ;
#70858 = AXIS2_PLACEMENT_3D('',#109940,#84623,#84624) ;
#70859 = AXIS2_PLACEMENT_3D('',#109941,#84625,#84626) ;
#70860 = AXIS2_PLACEMENT_3D('',#109942,#84627,#84628) ;
#70861 = AXIS2_PLACEMENT_3D('',#109943,#84629,#84630) ;
#70862 = AXIS2_PLACEMENT_3D('',#109944,#84631,#84632) ;
#70863 = AXIS2_PLACEMENT_3D('',#109945,#84633,#84634) ;
#70864 = AXIS2_PLACEMENT_3D('',#109946,#84635,#84636) ;
#70865 = AXIS2_PLACEMENT_3D('',#109947,#84637,#84638) ;
#70866 = AXIS2_PLACEMENT_3D('',#109948,#84639,#84640) ;
#70867 = AXIS2_PLACEMENT_3D('',#109949,#84641,#84642) ;
#70868 = AXIS2_PLACEMENT_3D('',#109950,#84643,#84644) ;
#70869 = AXIS2_PLACEMENT_3D('',#109951,#84645,#84646) ;
#70870 = AXIS2_PLACEMENT_3D('',#109952,#84647,#84648) ;
#70871 = AXIS2_PLACEMENT_3D('',#109953,#84649,#84650) ;
#70872 = AXIS2_PLACEMENT_3D('',#109954,#84651,#84652) ;
#70873 = AXIS2_PLACEMENT_3D('',#109955,#84653,#84654) ;
#70874 = AXIS2_PLACEMENT_3D('',#109956,#84655,#84656) ;
#70875 = AXIS2_PLACEMENT_3D('',#109957,#84657,#84658) ;
#70876 = AXIS2_PLACEMENT_3D('',#109958,#84659,#84660) ;
#70877 = AXIS2_PLACEMENT_3D('',#109974,#84661,#84662) ;
#70878 = AXIS2_PLACEMENT_3D('',#109975,#84663,#84664) ;
#70879 = AXIS2_PLACEMENT_3D('',#109977,#84665,#84666) ;
#70880 = AXIS2_PLACEMENT_3D('',#109992,#84667,#84668) ;
#70881 = AXIS2_PLACEMENT_3D('',#109993,#84669,#84670) ;
#70882 = AXIS2_PLACEMENT_3D('',#109994,#84671,#84672) ;
#70883 = AXIS2_PLACEMENT_3D('',#109996,#84673,#84674) ;
#70884 = AXIS2_PLACEMENT_3D('',#110026,#84675,#84676) ;
#70885 = AXIS2_PLACEMENT_3D('',#110027,#84677,#84678) ;
#70886 = AXIS2_PLACEMENT_3D('',#110043,#84679,#84680) ;
#70887 = AXIS2_PLACEMENT_3D('',#110045,#84681,#84682) ;
#70888 = AXIS2_PLACEMENT_3D('',#110060,#84683,#84684) ;
#70889 = AXIS2_PLACEMENT_3D('',#110061,#84685,#84686) ;
#70890 = AXIS2_PLACEMENT_3D('',#110062,#84687,#84688) ;
#70891 = AXIS2_PLACEMENT_3D('',#110063,#84689,#84690) ;
#70892 = AXIS2_PLACEMENT_3D('',#110066,#84692,#84693) ;
#70893 = AXIS2_PLACEMENT_3D('',#110067,#84694,#84695) ;
#70894 = AXIS2_PLACEMENT_3D('',#110069,#84696,#84697) ;
#70895 = AXIS2_PLACEMENT_3D('',#110070,#84698,#84699) ;
#70896 = AXIS2_PLACEMENT_3D('',#110071,#84700,#84701) ;
#70897 = AXIS2_PLACEMENT_3D('',#110073,#84702,#84703) ;
#70898 = AXIS2_PLACEMENT_3D('',#110088,#84704,#84705) ;
#70899 = AXIS2_PLACEMENT_3D('',#110089,#84706,#84707) ;
#70900 = AXIS2_PLACEMENT_3D('',#110105,#84708,#84709) ;
#70901 = AXIS2_PLACEMENT_3D('',#110106,#84710,#84711) ;
#70902 = AXIS2_PLACEMENT_3D('',#110107,#84712,#84713) ;
#70903 = AXIS2_PLACEMENT_3D('',#110109,#84714,#84715) ;
#70904 = AXIS2_PLACEMENT_3D('',#110111,#84717,#84718) ;
#70905 = AXIS2_PLACEMENT_3D('',#110112,#84719,#84720) ;
#70906 = AXIS2_PLACEMENT_3D('',#110113,#84721,#84722) ;
#70907 = AXIS2_PLACEMENT_3D('',#110114,#84723,#84724) ;
#70908 = AXIS2_PLACEMENT_3D('',#110115,#84725,#84726) ;
#70909 = AXIS2_PLACEMENT_3D('',#110116,#84727,#84728) ;
#70910 = AXIS2_PLACEMENT_3D('',#110119,#84730,#84731) ;
#70911 = AXIS2_PLACEMENT_3D('',#110120,#84732,#84733) ;
#70912 = AXIS2_PLACEMENT_3D('',#110121,#84734,#84735) ;
#70913 = AXIS2_PLACEMENT_3D('',#110122,#84736,#84737) ;
#70914 = AXIS2_PLACEMENT_3D('',#110124,#84738,#84739) ;
#70915 = AXIS2_PLACEMENT_3D('',#110125,#84740,#84741) ;
#70916 = AXIS2_PLACEMENT_3D('',#110126,#84742,#84743) ;
#70917 = AXIS2_PLACEMENT_3D('',#110127,#84744,#84745) ;
#70918 = AXIS2_PLACEMENT_3D('',#110128,#84746,#84747) ;
#70919 = AXIS2_PLACEMENT_3D('',#110129,#84748,#84749) ;
#70920 = AXIS2_PLACEMENT_3D('',#110130,#84750,#84751) ;
#70921 = AXIS2_PLACEMENT_3D('',#110132,#84752,#84753) ;
#70922 = AXIS2_PLACEMENT_3D('',#110133,#84754,#84755) ;
#70923 = AXIS2_PLACEMENT_3D('',#110134,#84756,#84757) ;
#70924 = AXIS2_PLACEMENT_3D('',#110135,#84758,#84759) ;
#70925 = AXIS2_PLACEMENT_3D('',#110136,#84760,#84761) ;
#70926 = AXIS2_PLACEMENT_3D('',#110138,#84762,#84763) ;
#70927 = AXIS2_PLACEMENT_3D('',#110140,#84765,#84766) ;
#70928 = AXIS2_PLACEMENT_3D('',#110141,#84767,#84768) ;
#70929 = AXIS2_PLACEMENT_3D('',#110142,#84769,#84770) ;
#70930 = AXIS2_PLACEMENT_3D('',#110143,#84771,#84772) ;
#70931 = AXIS2_PLACEMENT_3D('',#110144,#84773,#84774) ;
#70932 = AXIS2_PLACEMENT_3D('',#110146,#84776,#84777) ;
#70933 = AXIS2_PLACEMENT_3D('',#110147,#84778,#84779) ;
#70934 = AXIS2_PLACEMENT_3D('',#110148,#84780,#84781) ;
#70935 = AXIS2_PLACEMENT_3D('',#110149,#84782,#84783) ;
#70936 = AXIS2_PLACEMENT_3D('',#110151,#84784,#84785) ;
#70937 = AXIS2_PLACEMENT_3D('',#110152,#84786,#84787) ;
#70938 = AXIS2_PLACEMENT_3D('',#110153,#84788,#84789) ;
#70939 = AXIS2_PLACEMENT_3D('',#110154,#84790,#84791) ;
#70940 = AXIS2_PLACEMENT_3D('',#110155,#84792,#84793) ;
#70941 = AXIS2_PLACEMENT_3D('',#110156,#84794,#84795) ;
#70942 = AXIS2_PLACEMENT_3D('',#110157,#84796,#84797) ;
#70943 = AXIS2_PLACEMENT_3D('',#110159,#84799,#84800) ;
#70944 = AXIS2_PLACEMENT_3D('',#110160,#84801,#84802) ;
#70945 = AXIS2_PLACEMENT_3D('',#110161,#84803,#84804) ;
#70946 = AXIS2_PLACEMENT_3D('',#110162,#84805,#84806) ;
#70947 = AXIS2_PLACEMENT_3D('',#110163,#84807,#84808) ;
#70948 = AXIS2_PLACEMENT_3D('',#110164,#84809,#84810) ;
#70949 = AXIS2_PLACEMENT_3D('',#110165,#84811,#84812) ;
#70950 = AXIS2_PLACEMENT_3D('',#110166,#84813,#84814) ;
#70951 = AXIS2_PLACEMENT_3D('',#110167,#84815,#84816) ;
#70952 = AXIS2_PLACEMENT_3D('',#110168,#84817,#84818) ;
#70953 = AXIS2_PLACEMENT_3D('',#110169,#84819,#84820) ;
#70954 = AXIS2_PLACEMENT_3D('',#110170,#84821,#84822) ;
#70955 = AXIS2_PLACEMENT_3D('',#110171,#84823,#84824) ;
#70956 = AXIS2_PLACEMENT_3D('',#110172,#84825,#84826) ;
#70957 = AXIS2_PLACEMENT_3D('',#110173,#84827,#84828) ;
#70958 = AXIS2_PLACEMENT_3D('',#110174,#84829,#84830) ;
#70959 = AXIS2_PLACEMENT_3D('',#110175,#84831,#84832) ;
#70960 = AXIS2_PLACEMENT_3D('',#110176,#84833,#84834) ;
#70961 = AXIS2_PLACEMENT_3D('',#110177,#84835,#84836) ;
#70962 = AXIS2_PLACEMENT_3D('',#110178,#84837,#84838) ;
#70963 = AXIS2_PLACEMENT_3D('',#110179,#84839,#84840) ;
#70964 = AXIS2_PLACEMENT_3D('',#110180,#84841,#84842) ;
#70965 = AXIS2_PLACEMENT_3D('',#110181,#84843,#84844) ;
#70966 = AXIS2_PLACEMENT_3D('',#110182,#84845,#84846) ;
#70967 = AXIS2_PLACEMENT_3D('',#110183,#84847,#84848) ;
#70968 = AXIS2_PLACEMENT_3D('',#110184,#84849,#84850) ;
#70969 = AXIS2_PLACEMENT_3D('',#110185,#84851,#84852) ;
#70970 = AXIS2_PLACEMENT_3D('',#110186,#84853,#84854) ;
#70971 = AXIS2_PLACEMENT_3D('',#110187,#84855,#84856) ;
#70972 = AXIS2_PLACEMENT_3D('',#110188,#84857,#84858) ;
#70973 = AXIS2_PLACEMENT_3D('',#110189,#84859,#84860) ;
#70974 = AXIS2_PLACEMENT_3D('',#110190,#84861,#84862) ;
#70975 = AXIS2_PLACEMENT_3D('',#110191,#84863,#84864) ;
#70976 = AXIS2_PLACEMENT_3D('',#110192,#84865,#84866) ;
#70977 = AXIS2_PLACEMENT_3D('',#110193,#84867,#84868) ;
#70978 = AXIS2_PLACEMENT_3D('',#110194,#84869,#84870) ;
#70979 = AXIS2_PLACEMENT_3D('',#110195,#84871,#84872) ;
#70980 = AXIS2_PLACEMENT_3D('',#110196,#84873,#84874) ;
#70981 = AXIS2_PLACEMENT_3D('',#110197,#84875,#84876) ;
#70982 = AXIS2_PLACEMENT_3D('',#110198,#84877,#84878) ;
#70983 = AXIS2_PLACEMENT_3D('',#110199,#84879,#84880) ;
#70984 = AXIS2_PLACEMENT_3D('',#110200,#84881,#84882) ;
#70985 = AXIS2_PLACEMENT_3D('',#110201,#84883,#84884) ;
#70986 = AXIS2_PLACEMENT_3D('',#110202,#84885,#84886) ;
#70987 = AXIS2_PLACEMENT_3D('',#110203,#84887,#84888) ;
#70988 = AXIS2_PLACEMENT_3D('',#110204,#84889,#84890) ;
#70989 = AXIS2_PLACEMENT_3D('',#110205,#84891,#84892) ;
#70990 = AXIS2_PLACEMENT_3D('',#110206,#84893,#84894) ;
#70991 = AXIS2_PLACEMENT_3D('',#110207,#84895,#84896) ;
#70992 = AXIS2_PLACEMENT_3D('',#110208,#84897,#84898) ;
#70993 = AXIS2_PLACEMENT_3D('',#110225,#84899,#84900) ;
#70994 = AXIS2_PLACEMENT_3D('',#110226,#84901,#84902) ;
#70995 = AXIS2_PLACEMENT_3D('',#110227,#84903,#84904) ;
#70996 = AXIS2_PLACEMENT_3D('',#110228,#84905,#84906) ;
#70997 = AXIS2_PLACEMENT_3D('',#110229,#84907,#84908) ;
#70998 = AXIS2_PLACEMENT_3D('',#110230,#84909,#84910) ;
#70999 = AXIS2_PLACEMENT_3D('',#110231,#84911,#84912) ;
#71000 = AXIS2_PLACEMENT_3D('',#110232,#84913,#84914) ;
#71001 = AXIS2_PLACEMENT_3D('',#110233,#84915,#84916) ;
#71002 = AXIS2_PLACEMENT_3D('',#110234,#84917,#84918) ;
#71003 = AXIS2_PLACEMENT_3D('',#110235,#84919,#84920) ;
#71004 = AXIS2_PLACEMENT_3D('',#110254,#84921,#84922) ;
#71005 = AXIS2_PLACEMENT_3D('',#110255,#84923,#84924) ;
#71006 = AXIS2_PLACEMENT_3D('',#110257,#84925,#84926) ;
#71007 = AXIS2_PLACEMENT_3D('',#110258,#84927,#84928) ;
#71008 = AXIS2_PLACEMENT_3D('',#110259,#84929,#84930) ;
#71009 = AXIS2_PLACEMENT_3D('',#110260,#84931,#84932) ;
#71010 = AXIS2_PLACEMENT_3D('',#110261,#84933,#84934) ;
#71011 = AXIS2_PLACEMENT_3D('',#110262,#84935,#84936) ;
#71012 = AXIS2_PLACEMENT_3D('',#110263,#84937,#84938) ;
#71013 = AXIS2_PLACEMENT_3D('',#110264,#84939,#84940) ;
#71014 = AXIS2_PLACEMENT_3D('',#110265,#84941,#84942) ;
#71015 = AXIS2_PLACEMENT_3D('',#110266,#84943,#84944) ;
#71016 = AXIS2_PLACEMENT_3D('',#110267,#84945,#84946) ;
#71017 = AXIS2_PLACEMENT_3D('',#110302,#84947,#84948) ;
#71018 = AXIS2_PLACEMENT_3D('',#110303,#84949,#84950) ;
#71019 = AXIS2_PLACEMENT_3D('',#110304,#84951,#84952) ;
#71020 = AXIS2_PLACEMENT_3D('',#110305,#84953,#84954) ;
#71021 = AXIS2_PLACEMENT_3D('',#110316,#84955,#84956) ;
#71022 = AXIS2_PLACEMENT_3D('',#110317,#84957,#84958) ;
#71023 = AXIS2_PLACEMENT_3D('',#110318,#84959,#84960) ;
#71024 = AXIS2_PLACEMENT_3D('',#110319,#84961,#84962) ;
#71025 = AXIS2_PLACEMENT_3D('',#110326,#84963,#84964) ;
#71026 = AXIS2_PLACEMENT_3D('',#110327,#84965,#84966) ;
#71027 = AXIS2_PLACEMENT_3D('',#110328,#84967,#84968) ;
#71028 = AXIS2_PLACEMENT_3D('',#110329,#84969,#84970) ;
#71029 = AXIS2_PLACEMENT_3D('',#110330,#84971,#84972) ;
#71030 = AXIS2_PLACEMENT_3D('',#110341,#84973,#84974) ;
#71031 = AXIS2_PLACEMENT_3D('',#110342,#84975,#84976) ;
#71032 = AXIS2_PLACEMENT_3D('',#110343,#84977,#84978) ;
#71033 = AXIS2_PLACEMENT_3D('',#110344,#84979,#84980) ;
#71034 = AXIS2_PLACEMENT_3D('',#110345,#84981,#84982) ;
#71035 = AXIS2_PLACEMENT_3D('',#110346,#84983,#84984) ;
#71036 = AXIS2_PLACEMENT_3D('',#110347,#84985,#84986) ;
#71037 = AXIS2_PLACEMENT_3D('',#110348,#84987,#84988) ;
#71038 = AXIS2_PLACEMENT_3D('',#110349,#84989,#84990) ;
#71039 = AXIS2_PLACEMENT_3D('',#110350,#84991,#84992) ;
#71040 = AXIS2_PLACEMENT_3D('',#110351,#84993,#84994) ;
#71041 = AXIS2_PLACEMENT_3D('',#110352,#84995,#84996) ;
#71042 = AXIS2_PLACEMENT_3D('',#110353,#84997,#84998) ;
#71043 = AXIS2_PLACEMENT_3D('',#110354,#84999,#85000) ;
#71044 = AXIS2_PLACEMENT_3D('',#110355,#85001,#85002) ;
#71045 = AXIS2_PLACEMENT_3D('',#110356,#85003,#85004) ;
#71046 = AXIS2_PLACEMENT_3D('',#110357,#85005,#85006) ;
#71047 = AXIS2_PLACEMENT_3D('',#110358,#85007,#85008) ;
#71048 = AXIS2_PLACEMENT_3D('',#110359,#85009,#85010) ;
#71049 = AXIS2_PLACEMENT_3D('',#110360,#85011,#85012) ;
#71050 = AXIS2_PLACEMENT_3D('',#110361,#85013,#85014) ;
#71051 = AXIS2_PLACEMENT_3D('',#110362,#85015,#85016) ;
#71052 = AXIS2_PLACEMENT_3D('',#110363,#85017,#85018) ;
#71053 = AXIS2_PLACEMENT_3D('',#110364,#85019,#85020) ;
#71054 = AXIS2_PLACEMENT_3D('',#110365,#85021,#85022) ;
#71055 = AXIS2_PLACEMENT_3D('',#110366,#85023,#85024) ;
#71056 = AXIS2_PLACEMENT_3D('',#110367,#85025,#85026) ;
#71057 = AXIS2_PLACEMENT_3D('',#110368,#85027,#85028) ;
#71058 = AXIS2_PLACEMENT_3D('',#110369,#85029,#85030) ;
#71059 = AXIS2_PLACEMENT_3D('',#110370,#85031,#85032) ;
#71060 = AXIS2_PLACEMENT_3D('',#110371,#85033,#85034) ;
#71061 = AXIS2_PLACEMENT_3D('',#110372,#85035,#85036) ;
#71062 = AXIS2_PLACEMENT_3D('',#110373,#85037,#85038) ;
#71063 = AXIS2_PLACEMENT_3D('',#110374,#85039,#85040) ;
#71064 = AXIS2_PLACEMENT_3D('',#110381,#85041,#85042) ;
#71065 = AXIS2_PLACEMENT_3D('',#110382,#85043,#85044) ;
#71066 = AXIS2_PLACEMENT_3D('',#110383,#85045,#85046) ;
#71067 = AXIS2_PLACEMENT_3D('',#110384,#85047,#85048) ;
#71068 = AXIS2_PLACEMENT_3D('',#110385,#85049,#85050) ;
#71069 = AXIS2_PLACEMENT_3D('',#110386,#85051,#85052) ;
#71070 = AXIS2_PLACEMENT_3D('',#110387,#85053,#85054) ;
#71071 = AXIS2_PLACEMENT_3D('',#110388,#85055,#85056) ;
#71072 = AXIS2_PLACEMENT_3D('',#110389,#85057,#85058) ;
#71073 = AXIS2_PLACEMENT_3D('',#110390,#85059,#85060) ;
#71074 = AXIS2_PLACEMENT_3D('',#110391,#85061,#85062) ;
#71075 = AXIS2_PLACEMENT_3D('',#110392,#85063,#85064) ;
#71076 = AXIS2_PLACEMENT_3D('',#110393,#85065,#85066) ;
#71077 = AXIS2_PLACEMENT_3D('',#110394,#85067,#85068) ;
#71078 = AXIS2_PLACEMENT_3D('',#110395,#85069,#85070) ;
#71079 = AXIS2_PLACEMENT_3D('',#110396,#85071,#85072) ;
#71080 = AXIS2_PLACEMENT_3D('',#110397,#85073,#85074) ;
#71081 = AXIS2_PLACEMENT_3D('',#110398,#85075,#85076) ;
#71082 = AXIS2_PLACEMENT_3D('',#110399,#85077,#85078) ;
#71083 = AXIS2_PLACEMENT_3D('',#110400,#85079,#85080) ;
#71084 = AXIS2_PLACEMENT_3D('',#110401,#85081,#85082) ;
#71085 = AXIS2_PLACEMENT_3D('',#110402,#85083,#85084) ;
#71086 = AXIS2_PLACEMENT_3D('',#110403,#85085,#85086) ;
#71087 = AXIS2_PLACEMENT_3D('',#110404,#85087,#85088) ;
#71088 = AXIS2_PLACEMENT_3D('',#110405,#85089,#85090) ;
#71089 = AXIS2_PLACEMENT_3D('',#110406,#85091,#85092) ;
#71090 = AXIS2_PLACEMENT_3D('',#110407,#85093,#85094) ;
#71091 = AXIS2_PLACEMENT_3D('',#110408,#85095,#85096) ;
#71092 = AXIS2_PLACEMENT_3D('',#110409,#85097,#85098) ;
#71093 = AXIS2_PLACEMENT_3D('',#110410,#85099,#85100) ;
#71094 = AXIS2_PLACEMENT_3D('',#110411,#85101,#85102) ;
#71095 = AXIS2_PLACEMENT_3D('',#110412,#85103,#85104) ;
#71096 = AXIS2_PLACEMENT_3D('',#110413,#85105,#85106) ;
#71097 = AXIS2_PLACEMENT_3D('',#110414,#85107,#85108) ;
#71098 = AXIS2_PLACEMENT_3D('',#110415,#85109,#85110) ;
#71099 = AXIS2_PLACEMENT_3D('',#110416,#85111,#85112) ;
#71100 = AXIS2_PLACEMENT_3D('',#110417,#85113,#85114) ;
#71101 = AXIS2_PLACEMENT_3D('',#110418,#85115,#85116) ;
#71102 = AXIS2_PLACEMENT_3D('',#110419,#85117,#85118) ;
#71103 = AXIS2_PLACEMENT_3D('',#110450,#85119,#85120) ;
#71104 = AXIS2_PLACEMENT_3D('',#110451,#85121,#85122) ;
#71105 = AXIS2_PLACEMENT_3D('',#110452,#85123,#85124) ;
#71106 = AXIS2_PLACEMENT_3D('',#110453,#85125,#85126) ;
#71107 = AXIS2_PLACEMENT_3D('',#110454,#85127,#85128) ;
#71108 = AXIS2_PLACEMENT_3D('',#110455,#85129,#85130) ;
#71109 = AXIS2_PLACEMENT_3D('',#110456,#85131,#85132) ;
#71110 = AXIS2_PLACEMENT_3D('',#110457,#85133,#85134) ;
#71111 = AXIS2_PLACEMENT_3D('',#110458,#85135,#85136) ;
#71112 = AXIS2_PLACEMENT_3D('',#110459,#85137,#85138) ;
#71113 = AXIS2_PLACEMENT_3D('',#110486,#85139,#85140) ;
#71114 = AXIS2_PLACEMENT_3D('',#110487,#85141,#85142) ;
#71115 = AXIS2_PLACEMENT_3D('',#110488,#85143,#85144) ;
#71116 = AXIS2_PLACEMENT_3D('',#110489,#85145,#85146) ;
#71117 = AXIS2_PLACEMENT_3D('',#110490,#85147,#85148) ;
#71118 = AXIS2_PLACEMENT_3D('',#110491,#85149,#85150) ;
#71119 = AXIS2_PLACEMENT_3D('',#110492,#85151,#85152) ;
#71120 = AXIS2_PLACEMENT_3D('',#110493,#85153,#85154) ;
#71121 = AXIS2_PLACEMENT_3D('',#110494,#85155,#85156) ;
#71122 = AXIS2_PLACEMENT_3D('',#110495,#85157,#85158) ;
#71123 = AXIS2_PLACEMENT_3D('',#110496,#85159,#85160) ;
#71124 = AXIS2_PLACEMENT_3D('',#110497,#85161,#85162) ;
#71125 = AXIS2_PLACEMENT_3D('',#110498,#85163,#85164) ;
#71126 = AXIS2_PLACEMENT_3D('',#110499,#85165,#85166) ;
#71127 = AXIS2_PLACEMENT_3D('',#110500,#85167,#85168) ;
#71128 = AXIS2_PLACEMENT_3D('',#110501,#85169,#85170) ;
#71129 = AXIS2_PLACEMENT_3D('',#110502,#85171,#85172) ;
#71130 = AXIS2_PLACEMENT_3D('',#110503,#85173,#85174) ;
#71131 = AXIS2_PLACEMENT_3D('',#110504,#85175,#85176) ;
#71132 = AXIS2_PLACEMENT_3D('',#110505,#85177,#85178) ;
#71133 = AXIS2_PLACEMENT_3D('',#110506,#85179,#85180) ;
#71134 = AXIS2_PLACEMENT_3D('',#110507,#85181,#85182) ;
#71135 = AXIS2_PLACEMENT_3D('',#110508,#85183,#85184) ;
#71136 = AXIS2_PLACEMENT_3D('',#110509,#85185,#85186) ;
#71137 = AXIS2_PLACEMENT_3D('',#110510,#85187,#85188) ;
#71138 = AXIS2_PLACEMENT_3D('',#110511,#85189,#85190) ;
#71139 = AXIS2_PLACEMENT_3D('',#110512,#85191,#85192) ;
#71140 = AXIS2_PLACEMENT_3D('',#110513,#85193,#85194) ;
#71141 = AXIS2_PLACEMENT_3D('',#110514,#85195,#85196) ;
#71142 = AXIS2_PLACEMENT_3D('',#110539,#85197,#85198) ;
#71143 = AXIS2_PLACEMENT_3D('',#110540,#85199,#85200) ;
#71144 = AXIS2_PLACEMENT_3D('',#110541,#85201,#85202) ;
#71145 = AXIS2_PLACEMENT_3D('',#110542,#85203,#85204) ;
#71146 = AXIS2_PLACEMENT_3D('',#110543,#85205,#85206) ;
#71147 = AXIS2_PLACEMENT_3D('',#110544,#85207,#85208) ;
#71148 = AXIS2_PLACEMENT_3D('',#110545,#85209,#85210) ;
#71149 = AXIS2_PLACEMENT_3D('',#110594,#85211,#85212) ;
#71150 = AXIS2_PLACEMENT_3D('',#110595,#85213,#85214) ;
#71151 = AXIS2_PLACEMENT_3D('',#110596,#85215,#85216) ;
#71152 = AXIS2_PLACEMENT_3D('',#110597,#85217,#85218) ;
#71153 = AXIS2_PLACEMENT_3D('',#110598,#85219,#85220) ;
#71154 = AXIS2_PLACEMENT_3D('',#110599,#85221,#85222) ;
#71155 = AXIS2_PLACEMENT_3D('',#110600,#85223,#85224) ;
#71156 = AXIS2_PLACEMENT_3D('',#110662,#85225,#85226) ;
#71157 = AXIS2_PLACEMENT_3D('',#110663,#85227,#85228) ;
#71158 = AXIS2_PLACEMENT_3D('',#110664,#85229,#85230) ;
#71159 = AXIS2_PLACEMENT_3D('',#110837,#85231,#85232) ;
#71160 = AXIS2_PLACEMENT_3D('',#110838,#85233,#85234) ;
#71161 = AXIS2_PLACEMENT_3D('',#110893,#85235,#85236) ;
#71162 = AXIS2_PLACEMENT_3D('',#110940,#85237,#85238) ;
#71163 = AXIS2_PLACEMENT_3D('',#110941,#85239,#85240) ;
#71164 = AXIS2_PLACEMENT_3D('',#110942,#85241,#85242) ;
#71165 = AXIS2_PLACEMENT_3D('',#110943,#85243,#85244) ;
#71166 = AXIS2_PLACEMENT_3D('',#110944,#85245,#85246) ;
#71167 = AXIS2_PLACEMENT_3D('',#110945,#85247,#85248) ;
#71168 = AXIS2_PLACEMENT_3D('',#111050,#85249,#85250) ;
#71169 = AXIS2_PLACEMENT_3D('',#111051,#85251,#85252) ;
#71170 = AXIS2_PLACEMENT_3D('',#111052,#85253,#85254) ;
#71171 = AXIS2_PLACEMENT_3D('',#111053,#85255,#85256) ;
#71172 = AXIS2_PLACEMENT_3D('',#111066,#85257,#85258) ;
#71173 = AXIS2_PLACEMENT_3D('',#111067,#85259,#85260) ;
#71174 = AXIS2_PLACEMENT_3D('',#111068,#85261,#85262) ;
#71175 = AXIS2_PLACEMENT_3D('',#111069,#85263,#85264) ;
#71176 = AXIS2_PLACEMENT_3D('',#111070,#85265,#85266) ;
#71177 = AXIS2_PLACEMENT_3D('',#111071,#85267,#85268) ;
#71178 = AXIS2_PLACEMENT_3D('',#111072,#85269,#85270) ;
#71179 = AXIS2_PLACEMENT_3D('',#111073,#85271,#85272) ;
#71180 = AXIS2_PLACEMENT_3D('',#111074,#85273,#85274) ;
#71181 = AXIS2_PLACEMENT_3D('',#111075,#85275,#85276) ;
#71182 = AXIS2_PLACEMENT_3D('',#111076,#85277,#85278) ;
#71183 = AXIS2_PLACEMENT_3D('',#111077,#85279,#85280) ;
#71184 = AXIS2_PLACEMENT_3D('',#111078,#85281,#85282) ;
#71185 = AXIS2_PLACEMENT_3D('',#111079,#85283,#85284) ;
#71186 = AXIS2_PLACEMENT_3D('',#111080,#85285,#85286) ;
#71187 = AXIS2_PLACEMENT_3D('',#111081,#85287,#85288) ;
#71188 = AXIS2_PLACEMENT_3D('',#111082,#85289,#85290) ;
#71189 = AXIS2_PLACEMENT_3D('',#111083,#85291,#85292) ;
#71190 = AXIS2_PLACEMENT_3D('',#111084,#85293,#85294) ;
#71191 = AXIS2_PLACEMENT_3D('',#111085,#85295,#85296) ;
#71192 = AXIS2_PLACEMENT_3D('',#111086,#85297,#85298) ;
#71193 = AXIS2_PLACEMENT_3D('',#111087,#85299,#85300) ;
#71194 = AXIS2_PLACEMENT_3D('',#111088,#85301,#85302) ;
#71195 = AXIS2_PLACEMENT_3D('',#111089,#85303,#85304) ;
#71196 = AXIS2_PLACEMENT_3D('',#111090,#85305,#85306) ;
#71197 = AXIS2_PLACEMENT_3D('',#111091,#85307,#85308) ;
#71198 = AXIS2_PLACEMENT_3D('',#111092,#85309,#85310) ;
#71199 = AXIS2_PLACEMENT_3D('',#111093,#85311,#85312) ;
#71200 = AXIS2_PLACEMENT_3D('',#111094,#85313,#85314) ;
#71201 = AXIS2_PLACEMENT_3D('',#111095,#85315,#85316) ;
#71202 = AXIS2_PLACEMENT_3D('',#111096,#85317,#85318) ;
#71203 = AXIS2_PLACEMENT_3D('',#111097,#85319,#85320) ;
#71204 = AXIS2_PLACEMENT_3D('',#111098,#85321,#85322) ;
#71205 = AXIS2_PLACEMENT_3D('',#111099,#85323,#85324) ;
#71206 = AXIS2_PLACEMENT_3D('',#111100,#85325,#85326) ;
#71207 = AXIS2_PLACEMENT_3D('',#111101,#85327,#85328) ;
#71208 = AXIS2_PLACEMENT_3D('',#111102,#85329,#85330) ;
#71209 = AXIS2_PLACEMENT_3D('',#111103,#85331,#85332) ;
#71210 = AXIS2_PLACEMENT_3D('',#111116,#85333,#85334) ;
#71211 = AXIS2_PLACEMENT_3D('',#111117,#85335,#85336) ;
#71212 = AXIS2_PLACEMENT_3D('',#111118,#85337,#85338) ;
#71213 = AXIS2_PLACEMENT_3D('',#111119,#85339,#85340) ;
#71214 = AXIS2_PLACEMENT_3D('',#111174,#85341,#85342) ;
#71215 = AXIS2_PLACEMENT_3D('',#111175,#85343,#85344) ;
#71216 = AXIS2_PLACEMENT_3D('',#111176,#85345,#85346) ;
#71217 = AXIS2_PLACEMENT_3D('',#111231,#85347,#85348) ;
#71218 = AXIS2_PLACEMENT_3D('',#111232,#85349,#85350) ;
#71219 = AXIS2_PLACEMENT_3D('',#111258,#85351,#85352) ;
#71220 = AXIS2_PLACEMENT_3D('',#111260,#85353,#85354) ;
#71221 = AXIS2_PLACEMENT_3D('',#111262,#85355,#85356) ;
#71222 = AXIS2_PLACEMENT_3D('',#111301,#85357,#85358) ;
#71223 = AXIS2_PLACEMENT_3D('',#111303,#85359,#85360) ;
#71224 = AXIS2_PLACEMENT_3D('',#111305,#85361,#85362) ;
#71225 = AXIS2_PLACEMENT_3D('',#111306,#85363,#85364) ;
#71226 = AXIS2_PLACEMENT_3D('',#111307,#85365,#85366) ;
#71227 = AXIS2_PLACEMENT_3D('',#111309,#85367,#85368) ;
#71228 = AXIS2_PLACEMENT_3D('',#111311,#85369,#85370) ;
#71229 = AXIS2_PLACEMENT_3D('',#111312,#85371,#85372) ;
#71230 = AXIS2_PLACEMENT_3D('',#111313,#85373,#85374) ;
#71231 = AXIS2_PLACEMENT_3D('',#111315,#85375,#85376) ;
#71232 = AXIS2_PLACEMENT_3D('',#111317,#85377,#85378) ;
#71233 = AXIS2_PLACEMENT_3D('',#111318,#85379,#85380) ;
#71234 = AXIS2_PLACEMENT_3D('',#111319,#85381,#85382) ;
#71235 = AXIS2_PLACEMENT_3D('',#111322,#85383,#85384) ;
#71236 = AXIS2_PLACEMENT_3D('',#111326,#85386,#85387) ;
#71237 = AXIS2_PLACEMENT_3D('',#111328,#85388,#85389) ;
#71238 = AXIS2_PLACEMENT_3D('',#111330,#85391,#85392) ;
#71239 = AXIS2_PLACEMENT_3D('',#111333,#85393,#85394) ;
#71240 = AXIS2_PLACEMENT_3D('',#111337,#85396,#85397) ;
#71241 = AXIS2_PLACEMENT_3D('',#111339,#85399,#85400) ;
#71242 = AXIS2_PLACEMENT_3D('',#111342,#85401,#85402) ;
#71243 = AXIS2_PLACEMENT_3D('',#111344,#85403,#85404) ;
#71244 = AXIS2_PLACEMENT_3D('',#111346,#85405,#85406) ;
#71245 = AXIS2_PLACEMENT_3D('',#111347,#85407,#85408) ;
#71246 = AXIS2_PLACEMENT_3D('',#111348,#85409,#85410) ;
#71247 = AXIS2_PLACEMENT_3D('',#111350,#85412,#85413) ;
#71248 = AXIS2_PLACEMENT_3D('',#111353,#85415,#85416) ;
#71249 = AXIS2_PLACEMENT_3D('',#111362,#85417,#85418) ;
#71250 = AXIS2_PLACEMENT_3D('',#111370,#85419,#85420) ;
#71251 = AXIS2_PLACEMENT_3D('',#111372,#85422,#85423) ;
#71252 = AXIS2_PLACEMENT_3D('',#111388,#85427,#85428) ;
#71253 = AXIS2_PLACEMENT_3D('',#111390,#85430,#85431) ;
#71254 = AXIS2_PLACEMENT_3D('',#111439,#85436,#85437) ;
#71255 = AXIS2_PLACEMENT_3D('',#111448,#85442,#85443) ;
#71256 = AXIS2_PLACEMENT_3D('',#111478,#85448,#85449) ;
#71257 = AXIS2_PLACEMENT_3D('',#111487,#85454,#85455) ;
#71258 = AXIS2_PLACEMENT_3D('',#111496,#85460,#85461) ;
#71259 = AXIS2_PLACEMENT_3D('',#111507,#85466,#85467) ;
#71260 = AXIS2_PLACEMENT_3D('',#111509,#85469,#85470) ;
#71261 = AXIS2_PLACEMENT_3D('',#111513,#85472,#85473) ;
#71262 = AXIS2_PLACEMENT_3D('',#111514,#85474,#85475) ;
#71263 = AXIS2_PLACEMENT_3D('',#111515,#85476,#85477) ;
#71264 = AXIS2_PLACEMENT_3D('',#111517,#85478,#85479) ;
#71265 = AXIS2_PLACEMENT_3D('',#111521,#85481,#85482) ;
#71266 = AXIS2_PLACEMENT_3D('',#111525,#85484,#85485) ;
#71267 = AXIS2_PLACEMENT_3D('',#111529,#85487,#85488) ;
#71268 = AXIS2_PLACEMENT_3D('',#111533,#85490,#85491) ;
#71269 = AXIS2_PLACEMENT_3D('',#111537,#85493,#85494) ;
#71270 = AXIS2_PLACEMENT_3D('',#111540,#85496,#85497) ;
#71271 = AXIS2_PLACEMENT_3D('',#111542,#85498,#85499) ;
#71272 = AXIS2_PLACEMENT_3D('',#111545,#85501,#85502) ;
#71273 = AXIS2_PLACEMENT_3D('',#111547,#85503,#85504) ;
#71274 = AXIS2_PLACEMENT_3D('',#111553,#85507,#85508) ;
#71275 = AXIS2_PLACEMENT_3D('',#111557,#85510,#85511) ;
#71276 = AXIS2_PLACEMENT_3D('',#111560,#85513,#85514) ;
#71277 = AXIS2_PLACEMENT_3D('',#111561,#85515,#85516) ;
#71278 = AXIS2_PLACEMENT_3D('',#111566,#85518,#85519) ;
#71279 = AXIS2_PLACEMENT_3D('',#111570,#85521,#85522) ;
#71280 = AXIS2_PLACEMENT_3D('',#111574,#85524,#85525) ;
#71281 = AXIS2_PLACEMENT_3D('',#111578,#85527,#85528) ;
#71282 = AXIS2_PLACEMENT_3D('',#111583,#85531,#85532) ;
#71283 = AXIS2_PLACEMENT_3D('',#111585,#85533,#85534) ;
#71284 = AXIS2_PLACEMENT_3D('',#111588,#85536,#85537) ;
#71285 = AXIS2_PLACEMENT_3D('',#111590,#85538,#85539) ;
#71286 = AXIS2_PLACEMENT_3D('',#111594,#85541,#85542) ;
#71287 = AXIS2_PLACEMENT_3D('',#111598,#85544,#85545) ;
#71288 = AXIS2_PLACEMENT_3D('',#111602,#85547,#85548) ;
#71289 = AXIS2_PLACEMENT_3D('',#111606,#85550,#85551) ;
#71290 = AXIS2_PLACEMENT_3D('',#111610,#85553,#85554) ;
#71291 = AXIS2_PLACEMENT_3D('',#111614,#85556,#85557) ;
#71292 = AXIS2_PLACEMENT_3D('',#111618,#85559,#85560) ;
#71293 = AXIS2_PLACEMENT_3D('',#111621,#85562,#85563) ;
#71294 = AXIS2_PLACEMENT_3D('',#111622,#85564,#85565) ;
#71295 = AXIS2_PLACEMENT_3D('',#111625,#85568,#85569) ;
#71296 = AXIS2_PLACEMENT_3D('',#111628,#85572,#85573) ;
#71297 = AXIS2_PLACEMENT_3D('',#111717,#85578,#85579) ;
#71298 = AXIS2_PLACEMENT_3D('',#111728,#85580,#85581) ;
#71299 = AXIS2_PLACEMENT_3D('',#111733,#85585,#85586) ;
#71300 = AXIS2_PLACEMENT_3D('',#111739,#85590,#85591) ;
#71301 = AXIS2_PLACEMENT_3D('',#111759,#85595,#85596) ;
#71302 = AXIS2_PLACEMENT_3D('',#111858,#85602,#85603) ;
#71303 = AXIS2_PLACEMENT_3D('',#111862,#85605,#85606) ;
#71304 = AXIS2_PLACEMENT_3D('',#111866,#85609,#85610) ;
#71305 = AXIS2_PLACEMENT_3D('',#111869,#85611,#85612) ;
#71306 = AXIS2_PLACEMENT_3D('',#111874,#85615,#85616) ;
#71307 = AXIS2_PLACEMENT_3D('',#111876,#85617,#85618) ;
#71308 = AXIS2_PLACEMENT_3D('',#111878,#85619,#85620) ;
#71309 = AXIS2_PLACEMENT_3D('',#111886,#85624,#85625) ;
#71310 = AXIS2_PLACEMENT_3D('',#111888,#85626,#85627) ;
#71311 = AXIS2_PLACEMENT_3D('',#111890,#85628,#85629) ;
#71312 = AXIS2_PLACEMENT_3D('',#111895,#85632,#85633) ;
#71313 = AXIS2_PLACEMENT_3D('',#111897,#85634,#85635) ;
#71314 = AXIS2_PLACEMENT_3D('',#111899,#85636,#85637) ;
#71315 = AXIS2_PLACEMENT_3D('',#111903,#85639,#85640) ;
#71316 = AXIS2_PLACEMENT_3D('',#111907,#85642,#85643) ;
#71317 = AXIS2_PLACEMENT_3D('',#111908,#85644,#85645) ;
#71318 = AXIS2_PLACEMENT_3D('',#111909,#85646,#85647) ;
#71319 = AXIS2_PLACEMENT_3D('',#111912,#85648,#85649) ;
#71320 = AXIS2_PLACEMENT_3D('',#111922,#85655,#85656) ;
#71321 = AXIS2_PLACEMENT_3D('',#111924,#85658,#85659) ;
#71322 = AXIS2_PLACEMENT_3D('',#111927,#85660,#85661) ;
#71323 = AXIS2_PLACEMENT_3D('',#111933,#85665,#85666) ;
#71324 = AXIS2_PLACEMENT_3D('',#111935,#85668,#85669) ;
#71325 = AXIS2_PLACEMENT_3D('',#111941,#85672,#85673) ;
#71326 = AXIS2_PLACEMENT_3D('',#111942,#85674,#85675) ;
#71327 = AXIS2_PLACEMENT_3D('',#111945,#85676,#85677) ;
#71328 = AXIS2_PLACEMENT_3D('',#111949,#85680,#85681) ;
#71329 = AXIS2_PLACEMENT_3D('',#111966,#85690,#85691) ;
#71330 = AXIS2_PLACEMENT_3D('',#111975,#85696,#85697) ;
#71331 = AXIS2_PLACEMENT_3D('',#111984,#85702,#85703) ;
#71332 = AXIS2_PLACEMENT_3D('',#111993,#85708,#85709) ;
#71333 = AXIS2_PLACEMENT_3D('',#112020,#85714,#85715) ;
#71334 = AXIS2_PLACEMENT_3D('',#112037,#85724,#85725) ;
#71335 = AXIS2_PLACEMENT_3D('',#112042,#85727,#85728) ;
#71336 = AXIS2_PLACEMENT_3D('',#112046,#85730,#85731) ;
#71337 = AXIS2_PLACEMENT_3D('',#112050,#85733,#85734) ;
#71338 = AXIS2_PLACEMENT_3D('',#112053,#85736,#85737) ;
#71339 = AXIS2_PLACEMENT_3D('',#112054,#85738,#85739) ;
#71340 = AXIS2_PLACEMENT_3D('',#112057,#85740,#85741) ;
#71341 = AXIS2_PLACEMENT_3D('',#112062,#85744,#85745) ;
#71342 = AXIS2_PLACEMENT_3D('',#112065,#85747,#85748) ;
#71343 = AXIS2_PLACEMENT_3D('',#112066,#85749,#85750) ;
#71344 = AXIS2_PLACEMENT_3D('',#112072,#85754,#85755) ;
#71345 = AXIS2_PLACEMENT_3D('',#112078,#85759,#85760) ;
#71346 = AXIS2_PLACEMENT_3D('',#112081,#85761,#85762) ;
#71347 = AXIS2_PLACEMENT_3D('',#112085,#85764,#85765) ;
#71348 = AXIS2_PLACEMENT_3D('',#112087,#85767,#85768) ;
#71349 = AXIS2_PLACEMENT_3D('',#112090,#85769,#85770) ;
#71350 = AXIS2_PLACEMENT_3D('',#112094,#85772,#85773) ;
#71351 = AXIS2_PLACEMENT_3D('',#112096,#85775,#85776) ;
#71352 = AXIS2_PLACEMENT_3D('',#112102,#85780,#85781) ;
#71353 = AXIS2_PLACEMENT_3D('',#112108,#85785,#85786) ;
#71354 = AXIS2_PLACEMENT_3D('',#112111,#85787,#85788) ;
#71355 = AXIS2_PLACEMENT_3D('',#112116,#85791,#85792) ;
#71356 = AXIS2_PLACEMENT_3D('',#112118,#85793,#85794) ;
#71357 = AXIS2_PLACEMENT_3D('',#112120,#85796,#85797) ;
#71358 = AXIS2_PLACEMENT_3D('',#112123,#85798,#85799) ;
#71359 = AXIS2_PLACEMENT_3D('',#112128,#85803,#85804) ;
#71360 = AXIS2_PLACEMENT_3D('',#112134,#85808,#85809) ;
#71361 = AXIS2_PLACEMENT_3D('',#112137,#85810,#85811) ;
#71362 = AXIS2_PLACEMENT_3D('',#112141,#85813,#85814) ;
#71363 = AXIS2_PLACEMENT_3D('',#112143,#85816,#85817) ;
#71364 = AXIS2_PLACEMENT_3D('',#112152,#85822,#85823) ;
#71365 = AXIS2_PLACEMENT_3D('',#112155,#85824,#85825) ;
#71366 = AXIS2_PLACEMENT_3D('',#112159,#85827,#85828) ;
#71367 = AXIS2_PLACEMENT_3D('',#112161,#85830,#85831) ;
#71368 = AXIS2_PLACEMENT_3D('',#112167,#85835,#85836) ;
#71369 = AXIS2_PLACEMENT_3D('',#112176,#85841,#85842) ;
#71370 = AXIS2_PLACEMENT_3D('',#112183,#85846,#85847) ;
#71371 = AXIS2_PLACEMENT_3D('',#112184,#85848,#85849) ;
#71372 = AXIS2_PLACEMENT_3D('',#112193,#85854,#85855) ;
#71373 = AXIS2_PLACEMENT_3D('',#112196,#85856,#85857) ;
#71374 = AXIS2_PLACEMENT_3D('',#112201,#85860,#85861) ;
#71375 = AXIS2_PLACEMENT_3D('',#112205,#85863,#85864) ;
#71376 = AXIS2_PLACEMENT_3D('',#112207,#85866,#85867) ;
#71377 = AXIS2_PLACEMENT_3D('',#112215,#85872,#85873) ;
#71378 = AXIS2_PLACEMENT_3D('',#112224,#85878,#85879) ;
#71379 = AXIS2_PLACEMENT_3D('',#112233,#85884,#85885) ;
#71380 = AXIS2_PLACEMENT_3D('',#112242,#85890,#85891) ;
#71381 = AXIS2_PLACEMENT_3D('',#112248,#85895,#85896) ;
#71382 = AXIS2_PLACEMENT_3D('',#112254,#85900,#85901) ;
#71383 = AXIS2_PLACEMENT_3D('',#112260,#85905,#85906) ;
#71384 = AXIS2_PLACEMENT_3D('',#112266,#85910,#85911) ;
#71385 = AXIS2_PLACEMENT_3D('',#112275,#85915,#85916) ;
#71386 = AXIS2_PLACEMENT_3D('',#112278,#85918,#85919) ;
#71387 = AXIS2_PLACEMENT_3D('',#112279,#85920,#85921) ;
#71388 = AXIS2_PLACEMENT_3D('',#112288,#85925,#85926) ;
#71389 = AXIS2_PLACEMENT_3D('',#112291,#85928,#85929) ;
#71390 = AXIS2_PLACEMENT_3D('',#112292,#85930,#85931) ;
#71391 = AXIS2_PLACEMENT_3D('',#112296,#85933,#85934) ;
#71392 = AXIS2_PLACEMENT_3D('',#112297,#85935,#85936) ;
#71393 = AXIS2_PLACEMENT_3D('',#112298,#85937,#85938) ;
#71394 = AXIS2_PLACEMENT_3D('',#112304,#85942,#85943) ;
#71395 = AXIS2_PLACEMENT_3D('',#112313,#85948,#85949) ;
#71396 = AXIS2_PLACEMENT_3D('',#112322,#85954,#85955) ;
#71397 = AXIS2_PLACEMENT_3D('',#112331,#85960,#85961) ;
#71398 = AXIS2_PLACEMENT_3D('',#112340,#85966,#85967) ;
#71399 = AXIS2_PLACEMENT_3D('',#112341,#85968,#85969) ;
#71400 = AXIS2_PLACEMENT_3D('',#112342,#85970,#85971) ;
#71401 = AXIS2_PLACEMENT_3D('',#112343,#85972,#85973) ;
#71402 = AXIS2_PLACEMENT_3D('',#112352,#85978,#85979) ;
#71403 = AXIS2_PLACEMENT_3D('',#112361,#85984,#85985) ;
#71404 = AXIS2_PLACEMENT_3D('',#112370,#85990,#85991) ;
#71405 = AXIS2_PLACEMENT_3D('',#112379,#85996,#85997) ;
#71406 = AXIS2_PLACEMENT_3D('',#112383,#85999,#86000) ;
#71407 = AXIS2_PLACEMENT_3D('',#112385,#86002,#86003) ;
#71408 = AXIS2_PLACEMENT_3D('',#112388,#86004,#86005) ;
#71409 = AXIS2_PLACEMENT_3D('',#112389,#86006,#86007) ;
#71410 = AXIS2_PLACEMENT_3D('',#112390,#86008,#86009) ;
#71411 = AXIS2_PLACEMENT_3D('',#112391,#86010,#86011) ;
#71412 = AXIS2_PLACEMENT_3D('',#112395,#86013,#86014) ;
#71413 = AXIS2_PLACEMENT_3D('',#112397,#86016,#86017) ;
#71414 = AXIS2_PLACEMENT_3D('',#112398,#86018,#86019) ;
#71415 = AXIS2_PLACEMENT_3D('',#112399,#86020,#86021) ;
#71416 = AXIS2_PLACEMENT_3D('',#112400,#86022,#86023) ;
#71417 = AXIS2_PLACEMENT_3D('',#112401,#86024,#86025) ;
#71418 = AXIS2_PLACEMENT_3D('',#112402,#86026,#86027) ;
#71419 = AXIS2_PLACEMENT_3D('',#112403,#86028,#86029) ;
#71420 = AXIS2_PLACEMENT_3D('',#112404,#86030,#86031) ;
#71421 = AXIS2_PLACEMENT_3D('',#112405,#86032,#86033) ;
#71422 = AXIS2_PLACEMENT_3D('',#112406,#86034,#86035) ;
#71423 = AXIS2_PLACEMENT_3D('',#112407,#86036,#86037) ;
#71424 = AXIS2_PLACEMENT_3D('',#112408,#86038,#86039) ;
#71425 = AXIS2_PLACEMENT_3D('',#112409,#86040,#86041) ;
#71426 = AXIS2_PLACEMENT_3D('',#112410,#86042,#86043) ;
#71427 = AXIS2_PLACEMENT_3D('',#112411,#86044,#86045) ;
#71428 = AXIS2_PLACEMENT_3D('',#112412,#86046,#86047) ;
#71429 = AXIS2_PLACEMENT_3D('',#112413,#86048,#86049) ;
#71430 = AXIS2_PLACEMENT_3D('',#112414,#86050,#86051) ;
#71431 = AXIS2_PLACEMENT_3D('',#112415,#86052,#86053) ;
#71432 = AXIS2_PLACEMENT_3D('',#112416,#86054,#86055) ;
#71433 = AXIS2_PLACEMENT_3D('',#112417,#86056,#86057) ;
#71434 = AXIS2_PLACEMENT_3D('',#112418,#86058,#86059) ;
#71435 = AXIS2_PLACEMENT_3D('',#112419,#86060,#86061) ;
#71436 = AXIS2_PLACEMENT_3D('',#112420,#86062,#86063) ;
#71437 = AXIS2_PLACEMENT_3D('',#112421,#86064,#86065) ;
#71438 = AXIS2_PLACEMENT_3D('',#112422,#86066,#86067) ;
#71439 = AXIS2_PLACEMENT_3D('',#112423,#86068,#86069) ;
#71440 = AXIS2_PLACEMENT_3D('',#112424,#86070,#86071) ;
#71441 = AXIS2_PLACEMENT_3D('',#112425,#86072,#86073) ;
#71442 = AXIS2_PLACEMENT_3D('',#112426,#86074,#86075) ;
#71443 = AXIS2_PLACEMENT_3D('',#112427,#86076,#86077) ;
#71444 = AXIS2_PLACEMENT_3D('',#112428,#86078,#86079) ;
#71445 = AXIS2_PLACEMENT_3D('',#112429,#86080,#86081) ;
#71446 = AXIS2_PLACEMENT_3D('',#112430,#86082,#86083) ;
#71447 = AXIS2_PLACEMENT_3D('',#112431,#86084,#86085) ;
#71448 = AXIS2_PLACEMENT_3D('',#112432,#86086,#86087) ;
#71449 = AXIS2_PLACEMENT_3D('',#112433,#86088,#86089) ;
#71450 = AXIS2_PLACEMENT_3D('',#112434,#86090,#86091) ;
#71451 = AXIS2_PLACEMENT_3D('',#112435,#86092,#86093) ;
#71452 = AXIS2_PLACEMENT_3D('',#112436,#86094,#86095) ;
#71453 = AXIS2_PLACEMENT_3D('',#112437,#86096,#86097) ;
#71454 = AXIS2_PLACEMENT_3D('',#112438,#86098,#86099) ;
#71455 = AXIS2_PLACEMENT_3D('',#112439,#86100,#86101) ;
#71456 = AXIS2_PLACEMENT_3D('',#112440,#86102,#86103) ;
#71457 = AXIS2_PLACEMENT_3D('',#112441,#86104,#86105) ;
#71458 = AXIS2_PLACEMENT_3D('',#112442,#86106,#86107) ;
#71459 = AXIS2_PLACEMENT_3D('',#112443,#86108,#86109) ;
#71460 = AXIS2_PLACEMENT_3D('',#112444,#86110,#86111) ;
#71461 = AXIS2_PLACEMENT_3D('',#112445,#86112,#86113) ;
#71462 = AXIS2_PLACEMENT_3D('',#112446,#86114,#86115) ;
#71463 = AXIS2_PLACEMENT_3D('',#112447,#86116,#86117) ;
#71464 = AXIS2_PLACEMENT_3D('',#112448,#86118,#86119) ;
#71465 = AXIS2_PLACEMENT_3D('',#112449,#86120,#86121) ;
#71466 = AXIS2_PLACEMENT_3D('',#112450,#86122,#86123) ;
#71467 = AXIS2_PLACEMENT_3D('',#112451,#86124,#86125) ;
#71468 = AXIS2_PLACEMENT_3D('',#112452,#86126,#86127) ;
#71469 = AXIS2_PLACEMENT_3D('',#112453,#86128,#86129) ;
#71470 = AXIS2_PLACEMENT_3D('',#112454,#86130,#86131) ;
#71471 = AXIS2_PLACEMENT_3D('',#112455,#86132,#86133) ;
#71472 = AXIS2_PLACEMENT_3D('',#112456,#86134,#86135) ;
#71473 = AXIS2_PLACEMENT_3D('',#112457,#86136,#86137) ;
#71474 = AXIS2_PLACEMENT_3D('',#112458,#86138,#86139) ;
#71475 = AXIS2_PLACEMENT_3D('',#112459,#86140,#86141) ;
#71476 = AXIS2_PLACEMENT_3D('',#112460,#86142,#86143) ;
#71477 = AXIS2_PLACEMENT_3D('',#112461,#86144,#86145) ;
#71478 = AXIS2_PLACEMENT_3D('',#112462,#86146,#86147) ;
#71479 = AXIS2_PLACEMENT_3D('',#112463,#86148,#86149) ;
#71480 = AXIS2_PLACEMENT_3D('',#112464,#86150,#86151) ;
#71481 = AXIS2_PLACEMENT_3D('',#112465,#86152,#86153) ;
#71482 = AXIS2_PLACEMENT_3D('',#112466,#86154,#86155) ;
#71483 = AXIS2_PLACEMENT_3D('',#112467,#86156,#86157) ;
#71484 = AXIS2_PLACEMENT_3D('',#112468,#86158,#86159) ;
#71485 = AXIS2_PLACEMENT_3D('',#112469,#86160,#86161) ;
#71486 = AXIS2_PLACEMENT_3D('',#112470,#86162,#86163) ;
#71487 = AXIS2_PLACEMENT_3D('',#112486,#86164,#86165) ;
#71488 = AXIS2_PLACEMENT_3D('',#112487,#86166,#86167) ;
#71489 = AXIS2_PLACEMENT_3D('',#112489,#86168,#86169) ;
#71490 = AXIS2_PLACEMENT_3D('',#112504,#86170,#86171) ;
#71491 = AXIS2_PLACEMENT_3D('',#112505,#86172,#86173) ;
#71492 = AXIS2_PLACEMENT_3D('',#112506,#86174,#86175) ;
#71493 = AXIS2_PLACEMENT_3D('',#112508,#86176,#86177) ;
#71494 = AXIS2_PLACEMENT_3D('',#112538,#86178,#86179) ;
#71495 = AXIS2_PLACEMENT_3D('',#112539,#86180,#86181) ;
#71496 = AXIS2_PLACEMENT_3D('',#112555,#86182,#86183) ;
#71497 = AXIS2_PLACEMENT_3D('',#112557,#86184,#86185) ;
#71498 = AXIS2_PLACEMENT_3D('',#112572,#86186,#86187) ;
#71499 = AXIS2_PLACEMENT_3D('',#112573,#86188,#86189) ;
#71500 = AXIS2_PLACEMENT_3D('',#112574,#86190,#86191) ;
#71501 = AXIS2_PLACEMENT_3D('',#112575,#86192,#86193) ;
#71502 = AXIS2_PLACEMENT_3D('',#112578,#86195,#86196) ;
#71503 = AXIS2_PLACEMENT_3D('',#112579,#86197,#86198) ;
#71504 = AXIS2_PLACEMENT_3D('',#112581,#86199,#86200) ;
#71505 = AXIS2_PLACEMENT_3D('',#112582,#86201,#86202) ;
#71506 = AXIS2_PLACEMENT_3D('',#112583,#86203,#86204) ;
#71507 = AXIS2_PLACEMENT_3D('',#112585,#86205,#86206) ;
#71508 = AXIS2_PLACEMENT_3D('',#112600,#86207,#86208) ;
#71509 = AXIS2_PLACEMENT_3D('',#112601,#86209,#86210) ;
#71510 = AXIS2_PLACEMENT_3D('',#112617,#86211,#86212) ;
#71511 = AXIS2_PLACEMENT_3D('',#112618,#86213,#86214) ;
#71512 = AXIS2_PLACEMENT_3D('',#112619,#86215,#86216) ;
#71513 = AXIS2_PLACEMENT_3D('',#112621,#86217,#86218) ;
#71514 = AXIS2_PLACEMENT_3D('',#112623,#86220,#86221) ;
#71515 = AXIS2_PLACEMENT_3D('',#112624,#86222,#86223) ;
#71516 = AXIS2_PLACEMENT_3D('',#112625,#86224,#86225) ;
#71517 = AXIS2_PLACEMENT_3D('',#112626,#86226,#86227) ;
#71518 = AXIS2_PLACEMENT_3D('',#112627,#86228,#86229) ;
#71519 = AXIS2_PLACEMENT_3D('',#112628,#86230,#86231) ;
#71520 = AXIS2_PLACEMENT_3D('',#112631,#86233,#86234) ;
#71521 = AXIS2_PLACEMENT_3D('',#112632,#86235,#86236) ;
#71522 = AXIS2_PLACEMENT_3D('',#112633,#86237,#86238) ;
#71523 = AXIS2_PLACEMENT_3D('',#112634,#86239,#86240) ;
#71524 = AXIS2_PLACEMENT_3D('',#112636,#86241,#86242) ;
#71525 = AXIS2_PLACEMENT_3D('',#112637,#86243,#86244) ;
#71526 = AXIS2_PLACEMENT_3D('',#112638,#86245,#86246) ;
#71527 = AXIS2_PLACEMENT_3D('',#112639,#86247,#86248) ;
#71528 = AXIS2_PLACEMENT_3D('',#112640,#86249,#86250) ;
#71529 = AXIS2_PLACEMENT_3D('',#112641,#86251,#86252) ;
#71530 = AXIS2_PLACEMENT_3D('',#112642,#86253,#86254) ;
#71531 = AXIS2_PLACEMENT_3D('',#112644,#86255,#86256) ;
#71532 = AXIS2_PLACEMENT_3D('',#112645,#86257,#86258) ;
#71533 = AXIS2_PLACEMENT_3D('',#112646,#86259,#86260) ;
#71534 = AXIS2_PLACEMENT_3D('',#112647,#86261,#86262) ;
#71535 = AXIS2_PLACEMENT_3D('',#112648,#86263,#86264) ;
#71536 = AXIS2_PLACEMENT_3D('',#112650,#86265,#86266) ;
#71537 = AXIS2_PLACEMENT_3D('',#112652,#86268,#86269) ;
#71538 = AXIS2_PLACEMENT_3D('',#112653,#86270,#86271) ;
#71539 = AXIS2_PLACEMENT_3D('',#112654,#86272,#86273) ;
#71540 = AXIS2_PLACEMENT_3D('',#112655,#86274,#86275) ;
#71541 = AXIS2_PLACEMENT_3D('',#112656,#86276,#86277) ;
#71542 = AXIS2_PLACEMENT_3D('',#112658,#86279,#86280) ;
#71543 = AXIS2_PLACEMENT_3D('',#112659,#86281,#86282) ;
#71544 = AXIS2_PLACEMENT_3D('',#112660,#86283,#86284) ;
#71545 = AXIS2_PLACEMENT_3D('',#112661,#86285,#86286) ;
#71546 = AXIS2_PLACEMENT_3D('',#112663,#86287,#86288) ;
#71547 = AXIS2_PLACEMENT_3D('',#112664,#86289,#86290) ;
#71548 = AXIS2_PLACEMENT_3D('',#112665,#86291,#86292) ;
#71549 = AXIS2_PLACEMENT_3D('',#112666,#86293,#86294) ;
#71550 = AXIS2_PLACEMENT_3D('',#112667,#86295,#86296) ;
#71551 = AXIS2_PLACEMENT_3D('',#112668,#86297,#86298) ;
#71552 = AXIS2_PLACEMENT_3D('',#112669,#86299,#86300) ;
#71553 = AXIS2_PLACEMENT_3D('',#112671,#86302,#86303) ;
#71554 = AXIS2_PLACEMENT_3D('',#112672,#86304,#86305) ;
#71555 = AXIS2_PLACEMENT_3D('',#112673,#86306,#86307) ;
#71556 = AXIS2_PLACEMENT_3D('',#112674,#86308,#86309) ;
#71557 = AXIS2_PLACEMENT_3D('',#112675,#86310,#86311) ;
#71558 = AXIS2_PLACEMENT_3D('',#112676,#86312,#86313) ;
#71559 = AXIS2_PLACEMENT_3D('',#112677,#86314,#86315) ;
#71560 = AXIS2_PLACEMENT_3D('',#112678,#86316,#86317) ;
#71561 = AXIS2_PLACEMENT_3D('',#112679,#86318,#86319) ;
#71562 = AXIS2_PLACEMENT_3D('',#112680,#86320,#86321) ;
#71563 = AXIS2_PLACEMENT_3D('',#112681,#86322,#86323) ;
#71564 = AXIS2_PLACEMENT_3D('',#112682,#86324,#86325) ;
#71565 = AXIS2_PLACEMENT_3D('',#112683,#86326,#86327) ;
#71566 = AXIS2_PLACEMENT_3D('',#112684,#86328,#86329) ;
#71567 = AXIS2_PLACEMENT_3D('',#112685,#86330,#86331) ;
#71568 = AXIS2_PLACEMENT_3D('',#112686,#86332,#86333) ;
#71569 = AXIS2_PLACEMENT_3D('',#112687,#86334,#86335) ;
#71570 = AXIS2_PLACEMENT_3D('',#112688,#86336,#86337) ;
#71571 = AXIS2_PLACEMENT_3D('',#112689,#86338,#86339) ;
#71572 = AXIS2_PLACEMENT_3D('',#112690,#86340,#86341) ;
#71573 = AXIS2_PLACEMENT_3D('',#112691,#86342,#86343) ;
#71574 = AXIS2_PLACEMENT_3D('',#112692,#86344,#86345) ;
#71575 = AXIS2_PLACEMENT_3D('',#112693,#86346,#86347) ;
#71576 = AXIS2_PLACEMENT_3D('',#112694,#86348,#86349) ;
#71577 = AXIS2_PLACEMENT_3D('',#112695,#86350,#86351) ;
#71578 = AXIS2_PLACEMENT_3D('',#112696,#86352,#86353) ;
#71579 = AXIS2_PLACEMENT_3D('',#112697,#86354,#86355) ;
#71580 = AXIS2_PLACEMENT_3D('',#112698,#86356,#86357) ;
#71581 = AXIS2_PLACEMENT_3D('',#112699,#86358,#86359) ;
#71582 = AXIS2_PLACEMENT_3D('',#112700,#86360,#86361) ;
#71583 = AXIS2_PLACEMENT_3D('',#112701,#86362,#86363) ;
#71584 = AXIS2_PLACEMENT_3D('',#112702,#86364,#86365) ;
#71585 = AXIS2_PLACEMENT_3D('',#112703,#86366,#86367) ;
#71586 = AXIS2_PLACEMENT_3D('',#112704,#86368,#86369) ;
#71587 = AXIS2_PLACEMENT_3D('',#112705,#86370,#86371) ;
#71588 = AXIS2_PLACEMENT_3D('',#112706,#86372,#86373) ;
#71589 = AXIS2_PLACEMENT_3D('',#112707,#86374,#86375) ;
#71590 = AXIS2_PLACEMENT_3D('',#112708,#86376,#86377) ;
#71591 = AXIS2_PLACEMENT_3D('',#112709,#86378,#86379) ;
#71592 = AXIS2_PLACEMENT_3D('',#112710,#86380,#86381) ;
#71593 = AXIS2_PLACEMENT_3D('',#112711,#86382,#86383) ;
#71594 = AXIS2_PLACEMENT_3D('',#112712,#86384,#86385) ;
#71595 = AXIS2_PLACEMENT_3D('',#112713,#86386,#86387) ;
#71596 = AXIS2_PLACEMENT_3D('',#112714,#86388,#86389) ;
#71597 = AXIS2_PLACEMENT_3D('',#112715,#86390,#86391) ;
#71598 = AXIS2_PLACEMENT_3D('',#112716,#86392,#86393) ;
#71599 = AXIS2_PLACEMENT_3D('',#112717,#86394,#86395) ;
#71600 = AXIS2_PLACEMENT_3D('',#112718,#86396,#86397) ;
#71601 = AXIS2_PLACEMENT_3D('',#112719,#86398,#86399) ;
#71602 = AXIS2_PLACEMENT_3D('',#112720,#86400,#86401) ;
#71603 = AXIS2_PLACEMENT_3D('',#112737,#86402,#86403) ;
#71604 = AXIS2_PLACEMENT_3D('',#112738,#86404,#86405) ;
#71605 = AXIS2_PLACEMENT_3D('',#112739,#86406,#86407) ;
#71606 = AXIS2_PLACEMENT_3D('',#112740,#86408,#86409) ;
#71607 = AXIS2_PLACEMENT_3D('',#112741,#86410,#86411) ;
#71608 = AXIS2_PLACEMENT_3D('',#112742,#86412,#86413) ;
#71609 = AXIS2_PLACEMENT_3D('',#112743,#86414,#86415) ;
#71610 = AXIS2_PLACEMENT_3D('',#112744,#86416,#86417) ;
#71611 = AXIS2_PLACEMENT_3D('',#112745,#86418,#86419) ;
#71612 = AXIS2_PLACEMENT_3D('',#112746,#86420,#86421) ;
#71613 = AXIS2_PLACEMENT_3D('',#112747,#86422,#86423) ;
#71614 = AXIS2_PLACEMENT_3D('',#112766,#86424,#86425) ;
#71615 = AXIS2_PLACEMENT_3D('',#112767,#86426,#86427) ;
#71616 = AXIS2_PLACEMENT_3D('',#112769,#86428,#86429) ;
#71617 = AXIS2_PLACEMENT_3D('',#112770,#86430,#86431) ;
#71618 = AXIS2_PLACEMENT_3D('',#112771,#86432,#86433) ;
#71619 = AXIS2_PLACEMENT_3D('',#112772,#86434,#86435) ;
#71620 = AXIS2_PLACEMENT_3D('',#112773,#86436,#86437) ;
#71621 = AXIS2_PLACEMENT_3D('',#112774,#86438,#86439) ;
#71622 = AXIS2_PLACEMENT_3D('',#112775,#86440,#86441) ;
#71623 = AXIS2_PLACEMENT_3D('',#112776,#86442,#86443) ;
#71624 = AXIS2_PLACEMENT_3D('',#112777,#86444,#86445) ;
#71625 = AXIS2_PLACEMENT_3D('',#112778,#86446,#86447) ;
#71626 = AXIS2_PLACEMENT_3D('',#112779,#86448,#86449) ;
#71627 = AXIS2_PLACEMENT_3D('',#112814,#86450,#86451) ;
#71628 = AXIS2_PLACEMENT_3D('',#112815,#86452,#86453) ;
#71629 = AXIS2_PLACEMENT_3D('',#112816,#86454,#86455) ;
#71630 = AXIS2_PLACEMENT_3D('',#112817,#86456,#86457) ;
#71631 = AXIS2_PLACEMENT_3D('',#112828,#86458,#86459) ;
#71632 = AXIS2_PLACEMENT_3D('',#112829,#86460,#86461) ;
#71633 = AXIS2_PLACEMENT_3D('',#112830,#86462,#86463) ;
#71634 = AXIS2_PLACEMENT_3D('',#112831,#86464,#86465) ;
#71635 = AXIS2_PLACEMENT_3D('',#112838,#86466,#86467) ;
#71636 = AXIS2_PLACEMENT_3D('',#112839,#86468,#86469) ;
#71637 = AXIS2_PLACEMENT_3D('',#112840,#86470,#86471) ;
#71638 = AXIS2_PLACEMENT_3D('',#112841,#86472,#86473) ;
#71639 = AXIS2_PLACEMENT_3D('',#112842,#86474,#86475) ;
#71640 = AXIS2_PLACEMENT_3D('',#112853,#86476,#86477) ;
#71641 = AXIS2_PLACEMENT_3D('',#112854,#86478,#86479) ;
#71642 = AXIS2_PLACEMENT_3D('',#112855,#86480,#86481) ;
#71643 = AXIS2_PLACEMENT_3D('',#112856,#86482,#86483) ;
#71644 = AXIS2_PLACEMENT_3D('',#112857,#86484,#86485) ;
#71645 = AXIS2_PLACEMENT_3D('',#112858,#86486,#86487) ;
#71646 = AXIS2_PLACEMENT_3D('',#112859,#86488,#86489) ;
#71647 = AXIS2_PLACEMENT_3D('',#112860,#86490,#86491) ;
#71648 = AXIS2_PLACEMENT_3D('',#112861,#86492,#86493) ;
#71649 = AXIS2_PLACEMENT_3D('',#112862,#86494,#86495) ;
#71650 = AXIS2_PLACEMENT_3D('',#112863,#86496,#86497) ;
#71651 = AXIS2_PLACEMENT_3D('',#112864,#86498,#86499) ;
#71652 = AXIS2_PLACEMENT_3D('',#112865,#86500,#86501) ;
#71653 = AXIS2_PLACEMENT_3D('',#112866,#86502,#86503) ;
#71654 = AXIS2_PLACEMENT_3D('',#112867,#86504,#86505) ;
#71655 = AXIS2_PLACEMENT_3D('',#112868,#86506,#86507) ;
#71656 = AXIS2_PLACEMENT_3D('',#112869,#86508,#86509) ;
#71657 = AXIS2_PLACEMENT_3D('',#112870,#86510,#86511) ;
#71658 = AXIS2_PLACEMENT_3D('',#112871,#86512,#86513) ;
#71659 = AXIS2_PLACEMENT_3D('',#112872,#86514,#86515) ;
#71660 = AXIS2_PLACEMENT_3D('',#112873,#86516,#86517) ;
#71661 = AXIS2_PLACEMENT_3D('',#112874,#86518,#86519) ;
#71662 = AXIS2_PLACEMENT_3D('',#112875,#86520,#86521) ;
#71663 = AXIS2_PLACEMENT_3D('',#112876,#86522,#86523) ;
#71664 = AXIS2_PLACEMENT_3D('',#112877,#86524,#86525) ;
#71665 = AXIS2_PLACEMENT_3D('',#112878,#86526,#86527) ;
#71666 = AXIS2_PLACEMENT_3D('',#112879,#86528,#86529) ;
#71667 = AXIS2_PLACEMENT_3D('',#112880,#86530,#86531) ;
#71668 = AXIS2_PLACEMENT_3D('',#112881,#86532,#86533) ;
#71669 = AXIS2_PLACEMENT_3D('',#112882,#86534,#86535) ;
#71670 = AXIS2_PLACEMENT_3D('',#112883,#86536,#86537) ;
#71671 = AXIS2_PLACEMENT_3D('',#112884,#86538,#86539) ;
#71672 = AXIS2_PLACEMENT_3D('',#112885,#86540,#86541) ;
#71673 = AXIS2_PLACEMENT_3D('',#112886,#86542,#86543) ;
#71674 = AXIS2_PLACEMENT_3D('',#112893,#86544,#86545) ;
#71675 = AXIS2_PLACEMENT_3D('',#112894,#86546,#86547) ;
#71676 = AXIS2_PLACEMENT_3D('',#112895,#86548,#86549) ;
#71677 = AXIS2_PLACEMENT_3D('',#112896,#86550,#86551) ;
#71678 = AXIS2_PLACEMENT_3D('',#112897,#86552,#86553) ;
#71679 = AXIS2_PLACEMENT_3D('',#112898,#86554,#86555) ;
#71680 = AXIS2_PLACEMENT_3D('',#112899,#86556,#86557) ;
#71681 = AXIS2_PLACEMENT_3D('',#112900,#86558,#86559) ;
#71682 = AXIS2_PLACEMENT_3D('',#112901,#86560,#86561) ;
#71683 = AXIS2_PLACEMENT_3D('',#112902,#86562,#86563) ;
#71684 = AXIS2_PLACEMENT_3D('',#112903,#86564,#86565) ;
#71685 = AXIS2_PLACEMENT_3D('',#112904,#86566,#86567) ;
#71686 = AXIS2_PLACEMENT_3D('',#112905,#86568,#86569) ;
#71687 = AXIS2_PLACEMENT_3D('',#112906,#86570,#86571) ;
#71688 = AXIS2_PLACEMENT_3D('',#112907,#86572,#86573) ;
#71689 = AXIS2_PLACEMENT_3D('',#112908,#86574,#86575) ;
#71690 = AXIS2_PLACEMENT_3D('',#112909,#86576,#86577) ;
#71691 = AXIS2_PLACEMENT_3D('',#112910,#86578,#86579) ;
#71692 = AXIS2_PLACEMENT_3D('',#112911,#86580,#86581) ;
#71693 = AXIS2_PLACEMENT_3D('',#112912,#86582,#86583) ;
#71694 = AXIS2_PLACEMENT_3D('',#112913,#86584,#86585) ;
#71695 = AXIS2_PLACEMENT_3D('',#112914,#86586,#86587) ;
#71696 = AXIS2_PLACEMENT_3D('',#112915,#86588,#86589) ;
#71697 = AXIS2_PLACEMENT_3D('',#112916,#86590,#86591) ;
#71698 = AXIS2_PLACEMENT_3D('',#112917,#86592,#86593) ;
#71699 = AXIS2_PLACEMENT_3D('',#112918,#86594,#86595) ;
#71700 = AXIS2_PLACEMENT_3D('',#112919,#86596,#86597) ;
#71701 = AXIS2_PLACEMENT_3D('',#112920,#86598,#86599) ;
#71702 = AXIS2_PLACEMENT_3D('',#112921,#86600,#86601) ;
#71703 = AXIS2_PLACEMENT_3D('',#112922,#86602,#86603) ;
#71704 = AXIS2_PLACEMENT_3D('',#112923,#86604,#86605) ;
#71705 = AXIS2_PLACEMENT_3D('',#112924,#86606,#86607) ;
#71706 = AXIS2_PLACEMENT_3D('',#112925,#86608,#86609) ;
#71707 = AXIS2_PLACEMENT_3D('',#112926,#86610,#86611) ;
#71708 = AXIS2_PLACEMENT_3D('',#112927,#86612,#86613) ;
#71709 = AXIS2_PLACEMENT_3D('',#112928,#86614,#86615) ;
#71710 = AXIS2_PLACEMENT_3D('',#112929,#86616,#86617) ;
#71711 = AXIS2_PLACEMENT_3D('',#112930,#86618,#86619) ;
#71712 = AXIS2_PLACEMENT_3D('',#112931,#86620,#86621) ;
#71713 = AXIS2_PLACEMENT_3D('',#112962,#86622,#86623) ;
#71714 = AXIS2_PLACEMENT_3D('',#112963,#86624,#86625) ;
#71715 = AXIS2_PLACEMENT_3D('',#112964,#86626,#86627) ;
#71716 = AXIS2_PLACEMENT_3D('',#112965,#86628,#86629) ;
#71717 = AXIS2_PLACEMENT_3D('',#112966,#86630,#86631) ;
#71718 = AXIS2_PLACEMENT_3D('',#112967,#86632,#86633) ;
#71719 = AXIS2_PLACEMENT_3D('',#112968,#86634,#86635) ;
#71720 = AXIS2_PLACEMENT_3D('',#112969,#86636,#86637) ;
#71721 = AXIS2_PLACEMENT_3D('',#112970,#86638,#86639) ;
#71722 = AXIS2_PLACEMENT_3D('',#112971,#86640,#86641) ;
#71723 = AXIS2_PLACEMENT_3D('',#112998,#86642,#86643) ;
#71724 = AXIS2_PLACEMENT_3D('',#112999,#86644,#86645) ;
#71725 = AXIS2_PLACEMENT_3D('',#113000,#86646,#86647) ;
#71726 = AXIS2_PLACEMENT_3D('',#113001,#86648,#86649) ;
#71727 = AXIS2_PLACEMENT_3D('',#113002,#86650,#86651) ;
#71728 = AXIS2_PLACEMENT_3D('',#113003,#86652,#86653) ;
#71729 = AXIS2_PLACEMENT_3D('',#113004,#86654,#86655) ;
#71730 = AXIS2_PLACEMENT_3D('',#113005,#86656,#86657) ;
#71731 = AXIS2_PLACEMENT_3D('',#113006,#86658,#86659) ;
#71732 = AXIS2_PLACEMENT_3D('',#113007,#86660,#86661) ;
#71733 = AXIS2_PLACEMENT_3D('',#113008,#86662,#86663) ;
#71734 = AXIS2_PLACEMENT_3D('',#113009,#86664,#86665) ;
#71735 = AXIS2_PLACEMENT_3D('',#113010,#86666,#86667) ;
#71736 = AXIS2_PLACEMENT_3D('',#113011,#86668,#86669) ;
#71737 = AXIS2_PLACEMENT_3D('',#113012,#86670,#86671) ;
#71738 = AXIS2_PLACEMENT_3D('',#113013,#86672,#86673) ;
#71739 = AXIS2_PLACEMENT_3D('',#113014,#86674,#86675) ;
#71740 = AXIS2_PLACEMENT_3D('',#113015,#86676,#86677) ;
#71741 = AXIS2_PLACEMENT_3D('',#113016,#86678,#86679) ;
#71742 = AXIS2_PLACEMENT_3D('',#113017,#86680,#86681) ;
#71743 = AXIS2_PLACEMENT_3D('',#113018,#86682,#86683) ;
#71744 = AXIS2_PLACEMENT_3D('',#113019,#86684,#86685) ;
#71745 = AXIS2_PLACEMENT_3D('',#113020,#86686,#86687) ;
#71746 = AXIS2_PLACEMENT_3D('',#113021,#86688,#86689) ;
#71747 = AXIS2_PLACEMENT_3D('',#113022,#86690,#86691) ;
#71748 = AXIS2_PLACEMENT_3D('',#113023,#86692,#86693) ;
#71749 = AXIS2_PLACEMENT_3D('',#113024,#86694,#86695) ;
#71750 = AXIS2_PLACEMENT_3D('',#113025,#86696,#86697) ;
#71751 = AXIS2_PLACEMENT_3D('',#113026,#86698,#86699) ;
#71752 = AXIS2_PLACEMENT_3D('',#113051,#86700,#86701) ;
#71753 = AXIS2_PLACEMENT_3D('',#113052,#86702,#86703) ;
#71754 = AXIS2_PLACEMENT_3D('',#113053,#86704,#86705) ;
#71755 = AXIS2_PLACEMENT_3D('',#113054,#86706,#86707) ;
#71756 = AXIS2_PLACEMENT_3D('',#113055,#86708,#86709) ;
#71757 = AXIS2_PLACEMENT_3D('',#113056,#86710,#86711) ;
#71758 = AXIS2_PLACEMENT_3D('',#113057,#86712,#86713) ;
#71759 = AXIS2_PLACEMENT_3D('',#113106,#86714,#86715) ;
#71760 = AXIS2_PLACEMENT_3D('',#113107,#86716,#86717) ;
#71761 = AXIS2_PLACEMENT_3D('',#113108,#86718,#86719) ;
#71762 = AXIS2_PLACEMENT_3D('',#113109,#86720,#86721) ;
#71763 = AXIS2_PLACEMENT_3D('',#113110,#86722,#86723) ;
#71764 = AXIS2_PLACEMENT_3D('',#113111,#86724,#86725) ;
#71765 = AXIS2_PLACEMENT_3D('',#113112,#86726,#86727) ;
#71766 = AXIS2_PLACEMENT_3D('',#113174,#86728,#86729) ;
#71767 = AXIS2_PLACEMENT_3D('',#113175,#86730,#86731) ;
#71768 = AXIS2_PLACEMENT_3D('',#113176,#86732,#86733) ;
#71769 = AXIS2_PLACEMENT_3D('',#113349,#86734,#86735) ;
#71770 = AXIS2_PLACEMENT_3D('',#113350,#86736,#86737) ;
#71771 = AXIS2_PLACEMENT_3D('',#113405,#86738,#86739) ;
#71772 = AXIS2_PLACEMENT_3D('',#113452,#86740,#86741) ;
#71773 = AXIS2_PLACEMENT_3D('',#113453,#86742,#86743) ;
#71774 = AXIS2_PLACEMENT_3D('',#113454,#86744,#86745) ;
#71775 = AXIS2_PLACEMENT_3D('',#113455,#86746,#86747) ;
#71776 = AXIS2_PLACEMENT_3D('',#113456,#86748,#86749) ;
#71777 = AXIS2_PLACEMENT_3D('',#113457,#86750,#86751) ;
#71778 = AXIS2_PLACEMENT_3D('',#113562,#86752,#86753) ;
#71779 = AXIS2_PLACEMENT_3D('',#113563,#86754,#86755) ;
#71780 = AXIS2_PLACEMENT_3D('',#113564,#86756,#86757) ;
#71781 = AXIS2_PLACEMENT_3D('',#113565,#86758,#86759) ;
#71782 = AXIS2_PLACEMENT_3D('',#113578,#86760,#86761) ;
#71783 = AXIS2_PLACEMENT_3D('',#113579,#86762,#86763) ;
#71784 = AXIS2_PLACEMENT_3D('',#113580,#86764,#86765) ;
#71785 = AXIS2_PLACEMENT_3D('',#113581,#86766,#86767) ;
#71786 = AXIS2_PLACEMENT_3D('',#113582,#86768,#86769) ;
#71787 = AXIS2_PLACEMENT_3D('',#113583,#86770,#86771) ;
#71788 = AXIS2_PLACEMENT_3D('',#113584,#86772,#86773) ;
#71789 = AXIS2_PLACEMENT_3D('',#113585,#86774,#86775) ;
#71790 = AXIS2_PLACEMENT_3D('',#113586,#86776,#86777) ;
#71791 = AXIS2_PLACEMENT_3D('',#113587,#86778,#86779) ;
#71792 = AXIS2_PLACEMENT_3D('',#113588,#86780,#86781) ;
#71793 = AXIS2_PLACEMENT_3D('',#113589,#86782,#86783) ;
#71794 = AXIS2_PLACEMENT_3D('',#113590,#86784,#86785) ;
#71795 = AXIS2_PLACEMENT_3D('',#113591,#86786,#86787) ;
#71796 = AXIS2_PLACEMENT_3D('',#113592,#86788,#86789) ;
#71797 = AXIS2_PLACEMENT_3D('',#113593,#86790,#86791) ;
#71798 = AXIS2_PLACEMENT_3D('',#113594,#86792,#86793) ;
#71799 = AXIS2_PLACEMENT_3D('',#113595,#86794,#86795) ;
#71800 = AXIS2_PLACEMENT_3D('',#113596,#86796,#86797) ;
#71801 = AXIS2_PLACEMENT_3D('',#113597,#86798,#86799) ;
#71802 = AXIS2_PLACEMENT_3D('',#113598,#86800,#86801) ;
#71803 = AXIS2_PLACEMENT_3D('',#113599,#86802,#86803) ;
#71804 = AXIS2_PLACEMENT_3D('',#113600,#86804,#86805) ;
#71805 = AXIS2_PLACEMENT_3D('',#113601,#86806,#86807) ;
#71806 = AXIS2_PLACEMENT_3D('',#113602,#86808,#86809) ;
#71807 = AXIS2_PLACEMENT_3D('',#113603,#86810,#86811) ;
#71808 = AXIS2_PLACEMENT_3D('',#113604,#86812,#86813) ;
#71809 = AXIS2_PLACEMENT_3D('',#113605,#86814,#86815) ;
#71810 = AXIS2_PLACEMENT_3D('',#113606,#86816,#86817) ;
#71811 = AXIS2_PLACEMENT_3D('',#113607,#86818,#86819) ;
#71812 = AXIS2_PLACEMENT_3D('',#113608,#86820,#86821) ;
#71813 = AXIS2_PLACEMENT_3D('',#113609,#86822,#86823) ;
#71814 = AXIS2_PLACEMENT_3D('',#113610,#86824,#86825) ;
#71815 = AXIS2_PLACEMENT_3D('',#113611,#86826,#86827) ;
#71816 = AXIS2_PLACEMENT_3D('',#113612,#86828,#86829) ;
#71817 = AXIS2_PLACEMENT_3D('',#113613,#86830,#86831) ;
#71818 = AXIS2_PLACEMENT_3D('',#113614,#86832,#86833) ;
#71819 = AXIS2_PLACEMENT_3D('',#113615,#86834,#86835) ;
#71820 = AXIS2_PLACEMENT_3D('',#113628,#86836,#86837) ;
#71821 = AXIS2_PLACEMENT_3D('',#113629,#86838,#86839) ;
#71822 = AXIS2_PLACEMENT_3D('',#113630,#86840,#86841) ;
#71823 = AXIS2_PLACEMENT_3D('',#113631,#86842,#86843) ;
#71824 = AXIS2_PLACEMENT_3D('',#113686,#86844,#86845) ;
#71825 = AXIS2_PLACEMENT_3D('',#113687,#86846,#86847) ;
#71826 = AXIS2_PLACEMENT_3D('',#113688,#86848,#86849) ;
#71827 = AXIS2_PLACEMENT_3D('',#113743,#86850,#86851) ;
#71828 = AXIS2_PLACEMENT_3D('',#113744,#86852,#86853) ;
#71829 = AXIS2_PLACEMENT_3D('',#113745,#86854,#86855) ;
#71830 = AXIS2_PLACEMENT_3D('',#113746,#86856,#86857) ;
#71831 = AXIS2_PLACEMENT_3D('',#113748,#86858,#86859) ;
#71832 = AXIS2_PLACEMENT_3D('',#113752,#86861,#86862) ;
#71833 = AXIS2_PLACEMENT_3D('',#113753,#86863,#86864) ;
#71834 = AXIS2_PLACEMENT_3D('',#113754,#86865,#86866) ;
#71835 = AXIS2_PLACEMENT_3D('',#113757,#86867,#86868) ;
#71836 = AXIS2_PLACEMENT_3D('',#113761,#86870,#86871) ;
#71837 = AXIS2_PLACEMENT_3D('',#113763,#86873,#86874) ;
#71838 = AXIS2_PLACEMENT_3D('',#113766,#86875,#86876) ;
#71839 = AXIS2_PLACEMENT_3D('',#113772,#86879,#86880) ;
#71840 = AXIS2_PLACEMENT_3D('',#113778,#86884,#86885) ;
#71841 = AXIS2_PLACEMENT_3D('',#113785,#86888,#86889) ;
#71842 = AXIS2_PLACEMENT_3D('',#113792,#86893,#86894) ;
#71843 = AXIS2_PLACEMENT_3D('',#113793,#86895,#86896) ;
#71844 = AXIS2_PLACEMENT_3D('',#113796,#86899,#86900) ;
#71845 = AXIS2_PLACEMENT_3D('',#113803,#86903,#86904) ;
#71846 = AXIS2_PLACEMENT_3D('',#113810,#86908,#86909) ;
#71847 = AXIS2_PLACEMENT_3D('',#113811,#86910,#86911) ;
#71848 = AXIS2_PLACEMENT_3D('',#113817,#86915,#86916) ;
#71849 = AXIS2_PLACEMENT_3D('',#113820,#86917,#86918) ;
#71850 = AXIS2_PLACEMENT_3D('',#113825,#86921,#86922) ;
#71851 = AXIS2_PLACEMENT_3D('',#113829,#86925,#86926) ;
#71852 = AXIS2_PLACEMENT_3D('',#113832,#86929,#86930) ;
#71853 = AXIS2_PLACEMENT_3D('',#113833,#86931,#86932) ;
#71854 = AXIS2_PLACEMENT_3D('',#113836,#86935,#86936) ;
#71855 = AXIS2_PLACEMENT_3D('',#113837,#86937,#86938) ;
#71856 = AXIS2_PLACEMENT_3D('',#113839,#86940,#86941) ;
#71857 = AXIS2_PLACEMENT_3D('',#113841,#86943,#86944) ;
#71858 = AXIS2_PLACEMENT_3D('',#113843,#86946,#86947) ;
#71859 = AXIS2_PLACEMENT_3D('',#113845,#86949,#86950) ;
#71860 = AXIS2_PLACEMENT_3D('',#113849,#86954,#86955) ;
#71861 = AXIS2_PLACEMENT_3D('',#113852,#86958,#86959) ;
#71862 = AXIS2_PLACEMENT_3D('',#113853,#86960,#86961) ;
#71863 = AXIS2_PLACEMENT_3D('',#113855,#86962,#86963) ;
#71864 = AXIS2_PLACEMENT_3D('',#113856,#86964,#86965) ;
#71865 = AXIS2_PLACEMENT_3D('',#113857,#86966,#86967) ;
#71866 = AXIS2_PLACEMENT_3D('',#113858,#86968,#86969) ;
#71867 = AXIS2_PLACEMENT_3D('',#113859,#86970,#86971) ;
#71868 = AXIS2_PLACEMENT_3D('',#113861,#86972,#86973) ;
#71869 = AXIS2_PLACEMENT_3D('',#113863,#86974,#86975) ;
#71870 = AXIS2_PLACEMENT_3D('',#113865,#86976,#86977) ;
#71871 = AXIS2_PLACEMENT_3D('',#113866,#86978,#86979) ;
#71872 = AXIS2_PLACEMENT_3D('',#113867,#86980,#86981) ;
#71873 = AXIS2_PLACEMENT_3D('',#113869,#86982,#86983) ;
#71874 = AXIS2_PLACEMENT_3D('',#113871,#86984,#86985) ;
#71875 = AXIS2_PLACEMENT_3D('',#113872,#86986,#86987) ;
#71876 = AXIS2_PLACEMENT_3D('',#113873,#86988,#86989) ;
#71877 = AXIS2_PLACEMENT_3D('',#113876,#86990,#86991) ;
#71878 = AXIS2_PLACEMENT_3D('',#113878,#86992,#86993) ;
#71879 = AXIS2_PLACEMENT_3D('',#113879,#86994,#86995) ;
#71880 = AXIS2_PLACEMENT_3D('',#113880,#86996,#86997) ;
#71881 = AXIS2_PLACEMENT_3D('',#113883,#86998,#86999) ;
#71882 = AXIS2_PLACEMENT_3D('',#113885,#87000,#87001) ;
#71883 = AXIS2_PLACEMENT_3D('',#113889,#87003,#87004) ;
#71884 = AXIS2_PLACEMENT_3D('',#113902,#87007,#87008) ;
#71885 = AXIS2_PLACEMENT_3D('',#113904,#87009,#87010) ;
#71886 = AXIS2_PLACEMENT_3D('',#113906,#87011,#87012) ;
#71887 = AXIS2_PLACEMENT_3D('',#113908,#87013,#87014) ;
#71888 = AXIS2_PLACEMENT_3D('',#113909,#87015,#87016) ;
#71889 = AXIS2_PLACEMENT_3D('',#113910,#87017,#87018) ;
#71890 = AXIS2_PLACEMENT_3D('',#113912,#87019,#87020) ;
#71891 = AXIS2_PLACEMENT_3D('',#113914,#87021,#87022) ;
#71892 = AXIS2_PLACEMENT_3D('',#113915,#87023,#87024) ;
#71893 = AXIS2_PLACEMENT_3D('',#113916,#87025,#87026) ;
#71894 = AXIS2_PLACEMENT_3D('',#113919,#87027,#87028) ;
#71895 = AXIS2_PLACEMENT_3D('',#113921,#87029,#87030) ;
#71896 = AXIS2_PLACEMENT_3D('',#113922,#87031,#87032) ;
#71897 = AXIS2_PLACEMENT_3D('',#113923,#87033,#87034) ;
#71898 = AXIS2_PLACEMENT_3D('',#113926,#87035,#87036) ;
#71899 = AXIS2_PLACEMENT_3D('',#113928,#87037,#87038) ;
#71900 = AXIS2_PLACEMENT_3D('',#113932,#87040,#87041) ;
#71901 = AXIS2_PLACEMENT_3D('',#113945,#87044,#87045) ;
#71902 = AXIS2_PLACEMENT_3D('',#113947,#87046,#87047) ;
#71903 = AXIS2_PLACEMENT_3D('',#113949,#87048,#87049) ;
#71904 = AXIS2_PLACEMENT_3D('',#113951,#87050,#87051) ;
#71905 = AXIS2_PLACEMENT_3D('',#113952,#87052,#87053) ;
#71906 = AXIS2_PLACEMENT_3D('',#113953,#87054,#87055) ;
#71907 = AXIS2_PLACEMENT_3D('',#113955,#87056,#87057) ;
#71908 = AXIS2_PLACEMENT_3D('',#113957,#87058,#87059) ;
#71909 = AXIS2_PLACEMENT_3D('',#113958,#87060,#87061) ;
#71910 = AXIS2_PLACEMENT_3D('',#113959,#87062,#87063) ;
#71911 = AXIS2_PLACEMENT_3D('',#113962,#87064,#87065) ;
#71912 = AXIS2_PLACEMENT_3D('',#113964,#87066,#87067) ;
#71913 = AXIS2_PLACEMENT_3D('',#113965,#87068,#87069) ;
#71914 = AXIS2_PLACEMENT_3D('',#113966,#87070,#87071) ;
#71915 = AXIS2_PLACEMENT_3D('',#113969,#87072,#87073) ;
#71916 = AXIS2_PLACEMENT_3D('',#113971,#87074,#87075) ;
#71917 = AXIS2_PLACEMENT_3D('',#113975,#87077,#87078) ;
#71918 = AXIS2_PLACEMENT_3D('',#113988,#87081,#87082) ;
#71919 = AXIS2_PLACEMENT_3D('',#113990,#87083,#87084) ;
#71920 = AXIS2_PLACEMENT_3D('',#113992,#87085,#87086) ;
#71921 = AXIS2_PLACEMENT_3D('',#113994,#87087,#87088) ;
#71922 = AXIS2_PLACEMENT_3D('',#113995,#87089,#87090) ;
#71923 = AXIS2_PLACEMENT_3D('',#113996,#87091,#87092) ;
#71924 = AXIS2_PLACEMENT_3D('',#113998,#87093,#87094) ;
#71925 = AXIS2_PLACEMENT_3D('',#114000,#87095,#87096) ;
#71926 = AXIS2_PLACEMENT_3D('',#114001,#87097,#87098) ;
#71927 = AXIS2_PLACEMENT_3D('',#114002,#87099,#87100) ;
#71928 = AXIS2_PLACEMENT_3D('',#114005,#87101,#87102) ;
#71929 = AXIS2_PLACEMENT_3D('',#114007,#87103,#87104) ;
#71930 = AXIS2_PLACEMENT_3D('',#114008,#87105,#87106) ;
#71931 = AXIS2_PLACEMENT_3D('',#114009,#87107,#87108) ;
#71932 = AXIS2_PLACEMENT_3D('',#114012,#87109,#87110) ;
#71933 = AXIS2_PLACEMENT_3D('',#114014,#87111,#87112) ;
#71934 = AXIS2_PLACEMENT_3D('',#114018,#87114,#87115) ;
#71935 = AXIS2_PLACEMENT_3D('',#114031,#87118,#87119) ;
#71936 = AXIS2_PLACEMENT_3D('',#114033,#87120,#87121) ;
#71937 = AXIS2_PLACEMENT_3D('',#114035,#87122,#87123) ;
#71938 = AXIS2_PLACEMENT_3D('',#114037,#87124,#87125) ;
#71939 = AXIS2_PLACEMENT_3D('',#114038,#87126,#87127) ;
#71940 = AXIS2_PLACEMENT_3D('',#114039,#87128,#87129) ;
#71941 = AXIS2_PLACEMENT_3D('',#114041,#87130,#87131) ;
#71942 = AXIS2_PLACEMENT_3D('',#114043,#87132,#87133) ;
#71943 = AXIS2_PLACEMENT_3D('',#114044,#87134,#87135) ;
#71944 = AXIS2_PLACEMENT_3D('',#114045,#87136,#87137) ;
#71945 = AXIS2_PLACEMENT_3D('',#114048,#87138,#87139) ;
#71946 = AXIS2_PLACEMENT_3D('',#114050,#87140,#87141) ;
#71947 = AXIS2_PLACEMENT_3D('',#114051,#87142,#87143) ;
#71948 = AXIS2_PLACEMENT_3D('',#114052,#87144,#87145) ;
#71949 = AXIS2_PLACEMENT_3D('',#114055,#87146,#87147) ;
#71950 = AXIS2_PLACEMENT_3D('',#114057,#87148,#87149) ;
#71951 = AXIS2_PLACEMENT_3D('',#114061,#87151,#87152) ;
#71952 = AXIS2_PLACEMENT_3D('',#114074,#87155,#87156) ;
#71953 = AXIS2_PLACEMENT_3D('',#114076,#87157,#87158) ;
#71954 = AXIS2_PLACEMENT_3D('',#114078,#87159,#87160) ;
#71955 = AXIS2_PLACEMENT_3D('',#114080,#87161,#87162) ;
#71956 = AXIS2_PLACEMENT_3D('',#114081,#87163,#87164) ;
#71957 = AXIS2_PLACEMENT_3D('',#114082,#87165,#87166) ;
#71958 = AXIS2_PLACEMENT_3D('',#114084,#87167,#87168) ;
#71959 = AXIS2_PLACEMENT_3D('',#114086,#87169,#87170) ;
#71960 = AXIS2_PLACEMENT_3D('',#114087,#87171,#87172) ;
#71961 = AXIS2_PLACEMENT_3D('',#114088,#87173,#87174) ;
#71962 = AXIS2_PLACEMENT_3D('',#114091,#87175,#87176) ;
#71963 = AXIS2_PLACEMENT_3D('',#114093,#87177,#87178) ;
#71964 = AXIS2_PLACEMENT_3D('',#114094,#87179,#87180) ;
#71965 = AXIS2_PLACEMENT_3D('',#114095,#87181,#87182) ;
#71966 = AXIS2_PLACEMENT_3D('',#114098,#87183,#87184) ;
#71967 = AXIS2_PLACEMENT_3D('',#114100,#87185,#87186) ;
#71968 = AXIS2_PLACEMENT_3D('',#114104,#87188,#87189) ;
#71969 = AXIS2_PLACEMENT_3D('',#114117,#87192,#87193) ;
#71970 = AXIS2_PLACEMENT_3D('',#114119,#87194,#87195) ;
#71971 = AXIS2_PLACEMENT_3D('',#114121,#87196,#87197) ;
#71972 = AXIS2_PLACEMENT_3D('',#114123,#87198,#87199) ;
#71973 = AXIS2_PLACEMENT_3D('',#114124,#87200,#87201) ;
#71974 = AXIS2_PLACEMENT_3D('',#114125,#87202,#87203) ;
#71975 = AXIS2_PLACEMENT_3D('',#114127,#87204,#87205) ;
#71976 = AXIS2_PLACEMENT_3D('',#114129,#87206,#87207) ;
#71977 = AXIS2_PLACEMENT_3D('',#114130,#87208,#87209) ;
#71978 = AXIS2_PLACEMENT_3D('',#114131,#87210,#87211) ;
#71979 = AXIS2_PLACEMENT_3D('',#114134,#87212,#87213) ;
#71980 = AXIS2_PLACEMENT_3D('',#114136,#87214,#87215) ;
#71981 = AXIS2_PLACEMENT_3D('',#114137,#87216,#87217) ;
#71982 = AXIS2_PLACEMENT_3D('',#114138,#87218,#87219) ;
#71983 = AXIS2_PLACEMENT_3D('',#114141,#87220,#87221) ;
#71984 = AXIS2_PLACEMENT_3D('',#114143,#87222,#87223) ;
#71985 = AXIS2_PLACEMENT_3D('',#114147,#87225,#87226) ;
#71986 = AXIS2_PLACEMENT_3D('',#114160,#87229,#87230) ;
#71987 = AXIS2_PLACEMENT_3D('',#114162,#87231,#87232) ;
#71988 = AXIS2_PLACEMENT_3D('',#114164,#87233,#87234) ;
#71989 = AXIS2_PLACEMENT_3D('',#114166,#87235,#87236) ;
#71990 = AXIS2_PLACEMENT_3D('',#114167,#87237,#87238) ;
#71991 = AXIS2_PLACEMENT_3D('',#114168,#87239,#87240) ;
#71992 = AXIS2_PLACEMENT_3D('',#114170,#87241,#87242) ;
#71993 = AXIS2_PLACEMENT_3D('',#114172,#87243,#87244) ;
#71994 = AXIS2_PLACEMENT_3D('',#114173,#87245,#87246) ;
#71995 = AXIS2_PLACEMENT_3D('',#114174,#87247,#87248) ;
#71996 = AXIS2_PLACEMENT_3D('',#114177,#87249,#87250) ;
#71997 = AXIS2_PLACEMENT_3D('',#114179,#87251,#87252) ;
#71998 = AXIS2_PLACEMENT_3D('',#114180,#87253,#87254) ;
#71999 = AXIS2_PLACEMENT_3D('',#114181,#87255,#87256) ;
#72000 = AXIS2_PLACEMENT_3D('',#114184,#87257,#87258) ;
#72001 = AXIS2_PLACEMENT_3D('',#114186,#87259,#87260) ;
#72002 = AXIS2_PLACEMENT_3D('',#114190,#87262,#87263) ;
#72003 = AXIS2_PLACEMENT_3D('',#114203,#87266,#87267) ;
#72004 = AXIS2_PLACEMENT_3D('',#114205,#87268,#87269) ;
#72005 = AXIS2_PLACEMENT_3D('',#114207,#87270,#87271) ;
#72006 = AXIS2_PLACEMENT_3D('',#114209,#87272,#87273) ;
#72007 = AXIS2_PLACEMENT_3D('',#114210,#87274,#87275) ;
#72008 = AXIS2_PLACEMENT_3D('',#114211,#87276,#87277) ;
#72009 = AXIS2_PLACEMENT_3D('',#114214,#87278,#87279) ;
#72010 = AXIS2_PLACEMENT_3D('',#114216,#87280,#87281) ;
#72011 = AXIS2_PLACEMENT_3D('',#114218,#87282,#87283) ;
#72012 = AXIS2_PLACEMENT_3D('',#114219,#87284,#87285) ;
#72013 = AXIS2_PLACEMENT_3D('',#114220,#87286,#87287) ;
#72014 = AXIS2_PLACEMENT_3D('',#114223,#87288,#87289) ;
#72015 = AXIS2_PLACEMENT_3D('',#114225,#87290,#87291) ;
#72016 = AXIS2_PLACEMENT_3D('',#114227,#87292,#87293) ;
#72017 = AXIS2_PLACEMENT_3D('',#114228,#87294,#87295) ;
#72018 = AXIS2_PLACEMENT_3D('',#114229,#87296,#87297) ;
#72019 = AXIS2_PLACEMENT_3D('',#114232,#87298,#87299) ;
#72020 = AXIS2_PLACEMENT_3D('',#114234,#87300,#87301) ;
#72021 = AXIS2_PLACEMENT_3D('',#114236,#87302,#87303) ;
#72022 = AXIS2_PLACEMENT_3D('',#114237,#87304,#87305) ;
#72023 = AXIS2_PLACEMENT_3D('',#114238,#87306,#87307) ;
#72024 = AXIS2_PLACEMENT_3D('',#114241,#87308,#87309) ;
#72025 = AXIS2_PLACEMENT_3D('',#114243,#87310,#87311) ;
#72026 = AXIS2_PLACEMENT_3D('',#114245,#87312,#87313) ;
#72027 = AXIS2_PLACEMENT_3D('',#114246,#87314,#87315) ;
#72028 = AXIS2_PLACEMENT_3D('',#114247,#87316,#87317) ;
#72029 = AXIS2_PLACEMENT_3D('',#114250,#87318,#87319) ;
#72030 = AXIS2_PLACEMENT_3D('',#114252,#87320,#87321) ;
#72031 = AXIS2_PLACEMENT_3D('',#114254,#87322,#87323) ;
#72032 = AXIS2_PLACEMENT_3D('',#114255,#87324,#87325) ;
#72033 = AXIS2_PLACEMENT_3D('',#114256,#87326,#87327) ;
#72034 = AXIS2_PLACEMENT_3D('',#114259,#87328,#87329) ;
#72035 = AXIS2_PLACEMENT_3D('',#114261,#87330,#87331) ;
#72036 = AXIS2_PLACEMENT_3D('',#114263,#87332,#87333) ;
#72037 = AXIS2_PLACEMENT_3D('',#114264,#87334,#87335) ;
#72038 = AXIS2_PLACEMENT_3D('',#114265,#87336,#87337) ;
#72039 = AXIS2_PLACEMENT_3D('',#114268,#87338,#87339) ;
#72040 = AXIS2_PLACEMENT_3D('',#114270,#87340,#87341) ;
#72041 = AXIS2_PLACEMENT_3D('',#114272,#87342,#87343) ;
#72042 = AXIS2_PLACEMENT_3D('',#114273,#87344,#87345) ;
#72043 = AXIS2_PLACEMENT_3D('',#114274,#87346,#87347) ;
#72044 = AXIS2_PLACEMENT_3D('',#114277,#87348,#87349) ;
#72045 = AXIS2_PLACEMENT_3D('',#114279,#87350,#87351) ;
#72046 = AXIS2_PLACEMENT_3D('',#114281,#87352,#87353) ;
#72047 = AXIS2_PLACEMENT_3D('',#114282,#87354,#87355) ;
#72048 = AXIS2_PLACEMENT_3D('',#114283,#87356,#87357) ;
#72049 = AXIS2_PLACEMENT_3D('',#114286,#87358,#87359) ;
#72050 = AXIS2_PLACEMENT_3D('',#114288,#87360,#87361) ;
#72051 = AXIS2_PLACEMENT_3D('',#114290,#87362,#87363) ;
#72052 = AXIS2_PLACEMENT_3D('',#114291,#87364,#87365) ;
#72053 = AXIS2_PLACEMENT_3D('',#114292,#87366,#87367) ;
#72054 = AXIS2_PLACEMENT_3D('',#114294,#87368,#87369) ;
#72055 = AXIS2_PLACEMENT_3D('',#114296,#87370,#87371) ;
#72056 = AXIS2_PLACEMENT_3D('',#114297,#87372,#87373) ;
#72057 = AXIS2_PLACEMENT_3D('',#114298,#87374,#87375) ;
#72058 = AXIS2_PLACEMENT_3D('',#114301,#87376,#87377) ;
#72059 = AXIS2_PLACEMENT_3D('',#114303,#87378,#87379) ;
#72060 = AXIS2_PLACEMENT_3D('',#114304,#87380,#87381) ;
#72061 = AXIS2_PLACEMENT_3D('',#114305,#87382,#87383) ;
#72062 = AXIS2_PLACEMENT_3D('',#114308,#87384,#87385) ;
#72063 = AXIS2_PLACEMENT_3D('',#114310,#87386,#87387) ;
#72064 = AXIS2_PLACEMENT_3D('',#114314,#87389,#87390) ;
#72065 = AXIS2_PLACEMENT_3D('',#114327,#87393,#87394) ;
#72066 = AXIS2_PLACEMENT_3D('',#114329,#87396,#87397) ;
#72067 = AXIS2_PLACEMENT_3D('',#114331,#87399,#87400) ;
#72068 = AXIS2_PLACEMENT_3D('',#114333,#87402,#87403) ;
#72069 = AXIS2_PLACEMENT_3D('',#114335,#87405,#87406) ;
#72070 = AXIS2_PLACEMENT_3D('',#114337,#87408,#87409) ;
#72071 = AXIS2_PLACEMENT_3D('',#114339,#87411,#87412) ;
#72072 = AXIS2_PLACEMENT_3D('',#114341,#87414,#87415) ;
#72073 = AXIS2_PLACEMENT_3D('',#114343,#87417,#87418) ;
#72074 = AXIS2_PLACEMENT_3D('',#114345,#87420,#87421) ;
#72075 = AXIS2_PLACEMENT_3D('',#114348,#87422,#87423) ;
#72076 = AXIS2_PLACEMENT_3D('',#114351,#87426,#87427) ;
#72077 = AXIS2_PLACEMENT_3D('',#114354,#87428,#87429) ;
#72078 = AXIS2_PLACEMENT_3D('',#114357,#87432,#87433) ;
#72079 = AXIS2_PLACEMENT_3D('',#114360,#87434,#87435) ;
#72080 = AXIS2_PLACEMENT_3D('',#114363,#87438,#87439) ;
#72081 = AXIS2_PLACEMENT_3D('',#114366,#87440,#87441) ;
#72082 = AXIS2_PLACEMENT_3D('',#114369,#87444,#87445) ;
#72083 = AXIS2_PLACEMENT_3D('',#114372,#87446,#87447) ;
#72084 = AXIS2_PLACEMENT_3D('',#114375,#87450,#87451) ;
#72085 = AXIS2_PLACEMENT_3D('',#114378,#87452,#87453) ;
#72086 = AXIS2_PLACEMENT_3D('',#114381,#87456,#87457) ;
#72087 = AXIS2_PLACEMENT_3D('',#114384,#87458,#87459) ;
#72088 = AXIS2_PLACEMENT_3D('',#114387,#87462,#87463) ;
#72089 = AXIS2_PLACEMENT_3D('',#114390,#87464,#87465) ;
#72090 = AXIS2_PLACEMENT_3D('',#114393,#87468,#87469) ;
#72091 = AXIS2_PLACEMENT_3D('',#114396,#87470,#87471) ;
#72092 = AXIS2_PLACEMENT_3D('',#114399,#87474,#87475) ;
#72093 = AXIS2_PLACEMENT_3D('',#114401,#87476,#87477) ;
#72094 = AXIS2_PLACEMENT_3D('',#114403,#87478,#87479) ;
#72095 = AXIS2_PLACEMENT_3D('',#114405,#87480,#87481) ;
#72096 = AXIS2_PLACEMENT_3D('',#114406,#87482,#87483) ;
#72097 = AXIS2_PLACEMENT_3D('',#114407,#87484,#87485) ;
#72098 = AXIS2_PLACEMENT_3D('',#114410,#87486,#87487) ;
#72099 = AXIS2_PLACEMENT_3D('',#114412,#87488,#87489) ;
#72100 = AXIS2_PLACEMENT_3D('',#114414,#87490,#87491) ;
#72101 = AXIS2_PLACEMENT_3D('',#114415,#87492,#87493) ;
#72102 = AXIS2_PLACEMENT_3D('',#114416,#87494,#87495) ;
#72103 = AXIS2_PLACEMENT_3D('',#114418,#87496,#87497) ;
#72104 = AXIS2_PLACEMENT_3D('',#114420,#87498,#87499) ;
#72105 = AXIS2_PLACEMENT_3D('',#114421,#87500,#87501) ;
#72106 = AXIS2_PLACEMENT_3D('',#114422,#87502,#87503) ;
#72107 = AXIS2_PLACEMENT_3D('',#114425,#87504,#87505) ;
#72108 = AXIS2_PLACEMENT_3D('',#114427,#87506,#87507) ;
#72109 = AXIS2_PLACEMENT_3D('',#114428,#87508,#87509) ;
#72110 = AXIS2_PLACEMENT_3D('',#114429,#87510,#87511) ;
#72111 = AXIS2_PLACEMENT_3D('',#114432,#87512,#87513) ;
#72112 = AXIS2_PLACEMENT_3D('',#114434,#87514,#87515) ;
#72113 = AXIS2_PLACEMENT_3D('',#114438,#87517,#87518) ;
#72114 = AXIS2_PLACEMENT_3D('',#114451,#87521,#87522) ;
#72115 = AXIS2_PLACEMENT_3D('',#114453,#87524,#87525) ;
#72116 = AXIS2_PLACEMENT_3D('',#114456,#87526,#87527) ;
#72117 = AXIS2_PLACEMENT_3D('',#114459,#87530,#87531) ;
#72118 = AXIS2_PLACEMENT_3D('',#114464,#87533,#87534) ;
#72119 = AXIS2_PLACEMENT_3D('',#114467,#87536,#87537) ;
#72120 = AXIS2_PLACEMENT_3D('',#114469,#87538,#87539) ;
#72121 = AXIS2_PLACEMENT_3D('',#114480,#87545,#87546) ;
#72122 = AXIS2_PLACEMENT_3D('',#114481,#87547,#87548) ;
#72123 = AXIS2_PLACEMENT_3D('',#114486,#87550,#87551) ;
#72124 = AXIS2_PLACEMENT_3D('',#114489,#87553,#87554) ;
#72125 = AXIS2_PLACEMENT_3D('',#114491,#87555,#87556) ;
#72126 = AXIS2_PLACEMENT_3D('',#114502,#87562,#87563) ;
#72127 = AXIS2_PLACEMENT_3D('',#114503,#87564,#87565) ;
#72128 = AXIS2_PLACEMENT_3D('',#114508,#87567,#87568) ;
#72129 = AXIS2_PLACEMENT_3D('',#114511,#87570,#87571) ;
#72130 = AXIS2_PLACEMENT_3D('',#114513,#87572,#87573) ;
#72131 = AXIS2_PLACEMENT_3D('',#114524,#87579,#87580) ;
#72132 = AXIS2_PLACEMENT_3D('',#114525,#87581,#87582) ;
#72133 = AXIS2_PLACEMENT_3D('',#114530,#87584,#87585) ;
#72134 = AXIS2_PLACEMENT_3D('',#114533,#87587,#87588) ;
#72135 = AXIS2_PLACEMENT_3D('',#114535,#87589,#87590) ;
#72136 = AXIS2_PLACEMENT_3D('',#114546,#87596,#87597) ;
#72137 = AXIS2_PLACEMENT_3D('',#114547,#87598,#87599) ;
#72138 = AXIS2_PLACEMENT_3D('',#114552,#87601,#87602) ;
#72139 = AXIS2_PLACEMENT_3D('',#114555,#87604,#87605) ;
#72140 = AXIS2_PLACEMENT_3D('',#114557,#87606,#87607) ;
#72141 = AXIS2_PLACEMENT_3D('',#114568,#87613,#87614) ;
#72142 = AXIS2_PLACEMENT_3D('',#114569,#87615,#87616) ;
#72143 = AXIS2_PLACEMENT_3D('',#114574,#87618,#87619) ;
#72144 = AXIS2_PLACEMENT_3D('',#114577,#87621,#87622) ;
#72145 = AXIS2_PLACEMENT_3D('',#114579,#87623,#87624) ;
#72146 = AXIS2_PLACEMENT_3D('',#114590,#87630,#87631) ;
#72147 = AXIS2_PLACEMENT_3D('',#114591,#87632,#87633) ;
#72148 = AXIS2_PLACEMENT_3D('',#114596,#87635,#87636) ;
#72149 = AXIS2_PLACEMENT_3D('',#114599,#87638,#87639) ;
#72150 = AXIS2_PLACEMENT_3D('',#114601,#87640,#87641) ;
#72151 = AXIS2_PLACEMENT_3D('',#114612,#87647,#87648) ;
#72152 = AXIS2_PLACEMENT_3D('',#114613,#87649,#87650) ;
#72153 = AXIS2_PLACEMENT_3D('',#114618,#87652,#87653) ;
#72154 = AXIS2_PLACEMENT_3D('',#114621,#87655,#87656) ;
#72155 = AXIS2_PLACEMENT_3D('',#114623,#87657,#87658) ;
#72156 = AXIS2_PLACEMENT_3D('',#114634,#87664,#87665) ;
#72157 = AXIS2_PLACEMENT_3D('',#114635,#87666,#87667) ;
#72158 = AXIS2_PLACEMENT_3D('',#114640,#87669,#87670) ;
#72159 = AXIS2_PLACEMENT_3D('',#114643,#87672,#87673) ;
#72160 = AXIS2_PLACEMENT_3D('',#114645,#87674,#87675) ;
#72161 = AXIS2_PLACEMENT_3D('',#114656,#87681,#87682) ;
#72162 = AXIS2_PLACEMENT_3D('',#114657,#87683,#87684) ;
#72163 = AXIS2_PLACEMENT_3D('',#114660,#87685,#87686) ;
#72164 = AXIS2_PLACEMENT_3D('',#114668,#87691,#87692) ;
#72165 = AXIS2_PLACEMENT_3D('',#114671,#87693,#87694) ;
#72166 = AXIS2_PLACEMENT_3D('',#114679,#87699,#87700) ;
#72167 = AXIS2_PLACEMENT_3D('',#114682,#87701,#87702) ;
#72168 = AXIS2_PLACEMENT_3D('',#114690,#87707,#87708) ;
#72169 = AXIS2_PLACEMENT_3D('',#114693,#87709,#87710) ;
#72170 = AXIS2_PLACEMENT_3D('',#114701,#87715,#87716) ;
#72171 = AXIS2_PLACEMENT_3D('',#114704,#87717,#87718) ;
#72172 = AXIS2_PLACEMENT_3D('',#114712,#87723,#87724) ;
#72173 = AXIS2_PLACEMENT_3D('',#114715,#87725,#87726) ;
#72174 = AXIS2_PLACEMENT_3D('',#114723,#87731,#87732) ;
#72175 = AXIS2_PLACEMENT_3D('',#114726,#87733,#87734) ;
#72176 = AXIS2_PLACEMENT_3D('',#114734,#87739,#87740) ;
#72177 = AXIS2_PLACEMENT_3D('',#114737,#87741,#87742) ;
#72178 = AXIS2_PLACEMENT_3D('',#114745,#87747,#87748) ;
#72179 = AXIS2_PLACEMENT_3D('',#114748,#87749,#87750) ;
#72180 = AXIS2_PLACEMENT_3D('',#114756,#87755,#87756) ;
#72181 = AXIS2_PLACEMENT_3D('',#114759,#87757,#87758) ;
#72182 = AXIS2_PLACEMENT_3D('',#114767,#87763,#87764) ;
#72183 = AXIS2_PLACEMENT_3D('',#114770,#87765,#87766) ;
#72184 = AXIS2_PLACEMENT_3D('',#114778,#87771,#87772) ;
#72185 = AXIS2_PLACEMENT_3D('',#114781,#87773,#87774) ;
#72186 = AXIS2_PLACEMENT_3D('',#114789,#87779,#87780) ;
#72187 = AXIS2_PLACEMENT_3D('',#114792,#87781,#87782) ;
#72188 = AXIS2_PLACEMENT_3D('',#114800,#87787,#87788) ;
#72189 = AXIS2_PLACEMENT_3D('',#114803,#87789,#87790) ;
#72190 = AXIS2_PLACEMENT_3D('',#114811,#87795,#87796) ;
#72191 = AXIS2_PLACEMENT_3D('',#114814,#87797,#87798) ;
#72192 = AXIS2_PLACEMENT_3D('',#114822,#87803,#87804) ;
#72193 = AXIS2_PLACEMENT_3D('',#114825,#87805,#87806) ;
#72194 = AXIS2_PLACEMENT_3D('',#114833,#87811,#87812) ;
#72195 = AXIS2_PLACEMENT_3D('',#114836,#87813,#87814) ;
#72196 = AXIS2_PLACEMENT_3D('',#114844,#87819,#87820) ;
#72197 = AXIS2_PLACEMENT_3D('',#114847,#87821,#87822) ;
#72198 = AXIS2_PLACEMENT_3D('',#114855,#87827,#87828) ;
#72199 = AXIS2_PLACEMENT_3D('',#114860,#87830,#87831) ;
#72200 = AXIS2_PLACEMENT_3D('',#114863,#87833,#87834) ;
#72201 = AXIS2_PLACEMENT_3D('',#114864,#87835,#87836) ;
#72202 = AXIS2_PLACEMENT_3D('',#114869,#87838,#87839) ;
#72203 = AXIS2_PLACEMENT_3D('',#114872,#87841,#87842) ;
#72204 = AXIS2_PLACEMENT_3D('',#114873,#87843,#87844) ;
#72205 = AXIS2_PLACEMENT_3D('',#114878,#87846,#87847) ;
#72206 = AXIS2_PLACEMENT_3D('',#114881,#87849,#87850) ;
#72207 = AXIS2_PLACEMENT_3D('',#114882,#87851,#87852) ;
#72208 = AXIS2_PLACEMENT_3D('',#114887,#87854,#87855) ;
#72209 = AXIS2_PLACEMENT_3D('',#114890,#87857,#87858) ;
#72210 = AXIS2_PLACEMENT_3D('',#114891,#87859,#87860) ;
#72211 = AXIS2_PLACEMENT_3D('',#114896,#87862,#87863) ;
#72212 = AXIS2_PLACEMENT_3D('',#114899,#87865,#87866) ;
#72213 = AXIS2_PLACEMENT_3D('',#114900,#87867,#87868) ;
#72214 = AXIS2_PLACEMENT_3D('',#114905,#87870,#87871) ;
#72215 = AXIS2_PLACEMENT_3D('',#114908,#87873,#87874) ;
#72216 = AXIS2_PLACEMENT_3D('',#114909,#87875,#87876) ;
#72217 = AXIS2_PLACEMENT_3D('',#114914,#87878,#87879) ;
#72218 = AXIS2_PLACEMENT_3D('',#114917,#87881,#87882) ;
#72219 = AXIS2_PLACEMENT_3D('',#114918,#87883,#87884) ;
#72220 = AXIS2_PLACEMENT_3D('',#114923,#87886,#87887) ;
#72221 = AXIS2_PLACEMENT_3D('',#114926,#87889,#87890) ;
#72222 = AXIS2_PLACEMENT_3D('',#114927,#87891,#87892) ;
#72223 = AXIS2_PLACEMENT_3D('',#114932,#87894,#87895) ;
#72224 = AXIS2_PLACEMENT_3D('',#114935,#87897,#87898) ;
#72225 = AXIS2_PLACEMENT_3D('',#114936,#87899,#87900) ;
#72226 = AXIS2_PLACEMENT_3D('',#114941,#87902,#87903) ;
#72227 = AXIS2_PLACEMENT_3D('',#114944,#87905,#87906) ;
#72228 = AXIS2_PLACEMENT_3D('',#114946,#87907,#87908) ;
#72229 = AXIS2_PLACEMENT_3D('',#114957,#87914,#87915) ;
#72230 = AXIS2_PLACEMENT_3D('',#114958,#87916,#87917) ;
#72231 = AXIS2_PLACEMENT_3D('',#114961,#87918,#87919) ;
#72232 = AXIS2_PLACEMENT_3D('',#114969,#87924,#87925) ;
#72233 = AXIS2_PLACEMENT_3D('',#114972,#87926,#87927) ;
#72234 = AXIS2_PLACEMENT_3D('',#114980,#87932,#87933) ;
#72235 = AXIS2_PLACEMENT_3D('',#114985,#87935,#87936) ;
#72236 = AXIS2_PLACEMENT_3D('',#114988,#87938,#87939) ;
#72237 = AXIS2_PLACEMENT_3D('',#114989,#87940,#87941) ;
#72238 = AXIS2_PLACEMENT_3D('',#114994,#87943,#87944) ;
#72239 = AXIS2_PLACEMENT_3D('',#114997,#87946,#87947) ;
#72240 = AXIS2_PLACEMENT_3D('',#114998,#87948,#87949) ;
#72241 = AXIS2_PLACEMENT_3D('',#115001,#87950,#87951) ;
#72242 = AXIS2_PLACEMENT_3D('',#115011,#87957,#87958) ;
#72243 = AXIS2_PLACEMENT_3D('',#115015,#87960,#87961) ;
#72244 = AXIS2_PLACEMENT_3D('',#115020,#87964,#87965) ;
#72245 = AXIS2_PLACEMENT_3D('',#115024,#87967,#87968) ;
#72246 = AXIS2_PLACEMENT_3D('',#115029,#87971,#87972) ;
#72247 = AXIS2_PLACEMENT_3D('',#115033,#87974,#87975) ;
#72248 = AXIS2_PLACEMENT_3D('',#115038,#87978,#87979) ;
#72249 = AXIS2_PLACEMENT_3D('',#115042,#87981,#87982) ;
#72250 = AXIS2_PLACEMENT_3D('',#115047,#87985,#87986) ;
#72251 = AXIS2_PLACEMENT_3D('',#115051,#87988,#87989) ;
#72252 = AXIS2_PLACEMENT_3D('',#115056,#87992,#87993) ;
#72253 = AXIS2_PLACEMENT_3D('',#115060,#87995,#87996) ;
#72254 = AXIS2_PLACEMENT_3D('',#115065,#87999,#88000) ;
#72255 = AXIS2_PLACEMENT_3D('',#115069,#88002,#88003) ;
#72256 = AXIS2_PLACEMENT_3D('',#115074,#88006,#88007) ;
#72257 = AXIS2_PLACEMENT_3D('',#115078,#88009,#88010) ;
#72258 = AXIS2_PLACEMENT_3D('',#115083,#88013,#88014) ;
#72259 = AXIS2_PLACEMENT_3D('',#115087,#88016,#88017) ;
#72260 = AXIS2_PLACEMENT_3D('',#115092,#88020,#88021) ;
#72261 = AXIS2_PLACEMENT_3D('',#115094,#88023,#88024) ;
#72262 = AXIS2_PLACEMENT_3D('',#115096,#88025,#88026) ;
#72263 = AXIS2_PLACEMENT_3D('',#115099,#88028,#88029) ;
#72264 = AXIS2_PLACEMENT_3D('',#115100,#88030,#88031) ;
#72265 = AXIS2_PLACEMENT_3D('',#115103,#88032,#88033) ;
#72266 = AXIS2_PLACEMENT_3D('',#115108,#88036,#88037) ;
#72267 = AXIS2_PLACEMENT_3D('',#115112,#88039,#88040) ;
#72268 = AXIS2_PLACEMENT_3D('',#115117,#88043,#88044) ;
#72269 = AXIS2_PLACEMENT_3D('',#115121,#88046,#88047) ;
#72270 = AXIS2_PLACEMENT_3D('',#115126,#88050,#88051) ;
#72271 = AXIS2_PLACEMENT_3D('',#115130,#88053,#88054) ;
#72272 = AXIS2_PLACEMENT_3D('',#115135,#88057,#88058) ;
#72273 = AXIS2_PLACEMENT_3D('',#115139,#88060,#88061) ;
#72274 = AXIS2_PLACEMENT_3D('',#115144,#88064,#88065) ;
#72275 = AXIS2_PLACEMENT_3D('',#115148,#88067,#88068) ;
#72276 = AXIS2_PLACEMENT_3D('',#115153,#88071,#88072) ;
#72277 = AXIS2_PLACEMENT_3D('',#115157,#88074,#88075) ;
#72278 = AXIS2_PLACEMENT_3D('',#115162,#88078,#88079) ;
#72279 = AXIS2_PLACEMENT_3D('',#115166,#88081,#88082) ;
#72280 = AXIS2_PLACEMENT_3D('',#115171,#88085,#88086) ;
#72281 = AXIS2_PLACEMENT_3D('',#115175,#88088,#88089) ;
#72282 = AXIS2_PLACEMENT_3D('',#115180,#88092,#88093) ;
#72283 = AXIS2_PLACEMENT_3D('',#115184,#88095,#88096) ;
#72284 = AXIS2_PLACEMENT_3D('',#115194,#88102,#88103) ;
#72285 = AXIS2_PLACEMENT_3D('',#115196,#88105,#88106) ;
#72286 = AXIS2_PLACEMENT_3D('',#115200,#88108,#88109) ;
#72287 = AXIS2_PLACEMENT_3D('',#115201,#88110,#88111) ;
#72288 = AXIS2_PLACEMENT_3D('',#115202,#88112,#88113) ;
#72289 = AXIS2_PLACEMENT_3D('',#115208,#88117,#88118) ;
#72290 = AXIS2_PLACEMENT_3D('',#115212,#88120,#88121) ;
#72291 = AXIS2_PLACEMENT_3D('',#115213,#88122,#88123) ;
#72292 = AXIS2_PLACEMENT_3D('',#115214,#88124,#88125) ;
#72293 = AXIS2_PLACEMENT_3D('',#115220,#88129,#88130) ;
#72294 = AXIS2_PLACEMENT_3D('',#115224,#88132,#88133) ;
#72295 = AXIS2_PLACEMENT_3D('',#115225,#88134,#88135) ;
#72296 = AXIS2_PLACEMENT_3D('',#115226,#88136,#88137) ;
#72297 = AXIS2_PLACEMENT_3D('',#115232,#88141,#88142) ;
#72298 = AXIS2_PLACEMENT_3D('',#115236,#88144,#88145) ;
#72299 = AXIS2_PLACEMENT_3D('',#115237,#88146,#88147) ;
#72300 = AXIS2_PLACEMENT_3D('',#115238,#88148,#88149) ;
#72301 = AXIS2_PLACEMENT_3D('',#115244,#88153,#88154) ;
#72302 = AXIS2_PLACEMENT_3D('',#115248,#88156,#88157) ;
#72303 = AXIS2_PLACEMENT_3D('',#115249,#88158,#88159) ;
#72304 = AXIS2_PLACEMENT_3D('',#115250,#88160,#88161) ;
#72305 = AXIS2_PLACEMENT_3D('',#115256,#88165,#88166) ;
#72306 = AXIS2_PLACEMENT_3D('',#115260,#88168,#88169) ;
#72307 = AXIS2_PLACEMENT_3D('',#115261,#88170,#88171) ;
#72308 = AXIS2_PLACEMENT_3D('',#115262,#88172,#88173) ;
#72309 = AXIS2_PLACEMENT_3D('',#115267,#88176,#88177) ;
#72310 = AXIS2_PLACEMENT_3D('',#115275,#88181,#88182) ;
#72311 = AXIS2_PLACEMENT_3D('',#115279,#88184,#88185) ;
#72312 = AXIS2_PLACEMENT_3D('',#115284,#88188,#88189) ;
#72313 = AXIS2_PLACEMENT_3D('',#115292,#88193,#88194) ;
#72314 = AXIS2_PLACEMENT_3D('',#115296,#88196,#88197) ;
#72315 = AXIS2_PLACEMENT_3D('',#115300,#88199,#88200) ;
#72316 = AXIS2_PLACEMENT_3D('',#115302,#88201,#88202) ;
#72317 = AXIS2_PLACEMENT_3D('',#115304,#88203,#88204) ;
#72318 = AXIS2_PLACEMENT_3D('',#115308,#88206,#88207) ;
#72319 = AXIS2_PLACEMENT_3D('',#115312,#88209,#88210) ;
#72320 = AXIS2_PLACEMENT_3D('',#115320,#88214,#88215) ;
#72321 = AXIS2_PLACEMENT_3D('',#115324,#88217,#88218) ;
#72322 = AXIS2_PLACEMENT_3D('',#115329,#88221,#88222) ;
#72323 = AXIS2_PLACEMENT_3D('',#115337,#88226,#88227) ;
#72324 = AXIS2_PLACEMENT_3D('',#115341,#88229,#88230) ;
#72325 = AXIS2_PLACEMENT_3D('',#115345,#88232,#88233) ;
#72326 = AXIS2_PLACEMENT_3D('',#115347,#88234,#88235) ;
#72327 = AXIS2_PLACEMENT_3D('',#115349,#88236,#88237) ;
#72328 = AXIS2_PLACEMENT_3D('',#115353,#88239,#88240) ;
#72329 = AXIS2_PLACEMENT_3D('',#115357,#88242,#88243) ;
#72330 = AXIS2_PLACEMENT_3D('',#115365,#88247,#88248) ;
#72331 = AXIS2_PLACEMENT_3D('',#115369,#88250,#88251) ;
#72332 = AXIS2_PLACEMENT_3D('',#115374,#88254,#88255) ;
#72333 = AXIS2_PLACEMENT_3D('',#115382,#88259,#88260) ;
#72334 = AXIS2_PLACEMENT_3D('',#115386,#88262,#88263) ;
#72335 = AXIS2_PLACEMENT_3D('',#115390,#88265,#88266) ;
#72336 = AXIS2_PLACEMENT_3D('',#115392,#88267,#88268) ;
#72337 = AXIS2_PLACEMENT_3D('',#115394,#88269,#88270) ;
#72338 = AXIS2_PLACEMENT_3D('',#115398,#88272,#88273) ;
#72339 = AXIS2_PLACEMENT_3D('',#115402,#88275,#88276) ;
#72340 = AXIS2_PLACEMENT_3D('',#115410,#88280,#88281) ;
#72341 = AXIS2_PLACEMENT_3D('',#115414,#88283,#88284) ;
#72342 = AXIS2_PLACEMENT_3D('',#115419,#88287,#88288) ;
#72343 = AXIS2_PLACEMENT_3D('',#115427,#88292,#88293) ;
#72344 = AXIS2_PLACEMENT_3D('',#115431,#88295,#88296) ;
#72345 = AXIS2_PLACEMENT_3D('',#115435,#88298,#88299) ;
#72346 = AXIS2_PLACEMENT_3D('',#115437,#88300,#88301) ;
#72347 = AXIS2_PLACEMENT_3D('',#115439,#88302,#88303) ;
#72348 = AXIS2_PLACEMENT_3D('',#115443,#88305,#88306) ;
#72349 = AXIS2_PLACEMENT_3D('',#115447,#88308,#88309) ;
#72350 = AXIS2_PLACEMENT_3D('',#115455,#88313,#88314) ;
#72351 = AXIS2_PLACEMENT_3D('',#115459,#88316,#88317) ;
#72352 = AXIS2_PLACEMENT_3D('',#115464,#88320,#88321) ;
#72353 = AXIS2_PLACEMENT_3D('',#115472,#88325,#88326) ;
#72354 = AXIS2_PLACEMENT_3D('',#115476,#88328,#88329) ;
#72355 = AXIS2_PLACEMENT_3D('',#115480,#88331,#88332) ;
#72356 = AXIS2_PLACEMENT_3D('',#115482,#88333,#88334) ;
#72357 = AXIS2_PLACEMENT_3D('',#115484,#88335,#88336) ;
#72358 = AXIS2_PLACEMENT_3D('',#115488,#88338,#88339) ;
#72359 = AXIS2_PLACEMENT_3D('',#115492,#88341,#88342) ;
#72360 = AXIS2_PLACEMENT_3D('',#115500,#88346,#88347) ;
#72361 = AXIS2_PLACEMENT_3D('',#115504,#88349,#88350) ;
#72362 = AXIS2_PLACEMENT_3D('',#115509,#88353,#88354) ;
#72363 = AXIS2_PLACEMENT_3D('',#115517,#88358,#88359) ;
#72364 = AXIS2_PLACEMENT_3D('',#115521,#88361,#88362) ;
#72365 = AXIS2_PLACEMENT_3D('',#115525,#88364,#88365) ;
#72366 = AXIS2_PLACEMENT_3D('',#115527,#88366,#88367) ;
#72367 = AXIS2_PLACEMENT_3D('',#115529,#88368,#88369) ;
#72368 = AXIS2_PLACEMENT_3D('',#115533,#88371,#88372) ;
#72369 = AXIS2_PLACEMENT_3D('',#115537,#88374,#88375) ;
#72370 = AXIS2_PLACEMENT_3D('',#115545,#88379,#88380) ;
#72371 = AXIS2_PLACEMENT_3D('',#115549,#88382,#88383) ;
#72372 = AXIS2_PLACEMENT_3D('',#115554,#88386,#88387) ;
#72373 = AXIS2_PLACEMENT_3D('',#115562,#88391,#88392) ;
#72374 = AXIS2_PLACEMENT_3D('',#115566,#88394,#88395) ;
#72375 = AXIS2_PLACEMENT_3D('',#115570,#88397,#88398) ;
#72376 = AXIS2_PLACEMENT_3D('',#115572,#88399,#88400) ;
#72377 = AXIS2_PLACEMENT_3D('',#115574,#88401,#88402) ;
#72378 = AXIS2_PLACEMENT_3D('',#115578,#88404,#88405) ;
#72379 = AXIS2_PLACEMENT_3D('',#115582,#88407,#88408) ;
#72380 = AXIS2_PLACEMENT_3D('',#115590,#88412,#88413) ;
#72381 = AXIS2_PLACEMENT_3D('',#115594,#88415,#88416) ;
#72382 = AXIS2_PLACEMENT_3D('',#115599,#88419,#88420) ;
#72383 = AXIS2_PLACEMENT_3D('',#115607,#88424,#88425) ;
#72384 = AXIS2_PLACEMENT_3D('',#115611,#88427,#88428) ;
#72385 = AXIS2_PLACEMENT_3D('',#115615,#88430,#88431) ;
#72386 = AXIS2_PLACEMENT_3D('',#115617,#88432,#88433) ;
#72387 = AXIS2_PLACEMENT_3D('',#115619,#88434,#88435) ;
#72388 = AXIS2_PLACEMENT_3D('',#115623,#88437,#88438) ;
#72389 = AXIS2_PLACEMENT_3D('',#115627,#88440,#88441) ;
#72390 = AXIS2_PLACEMENT_3D('',#115635,#88445,#88446) ;
#72391 = AXIS2_PLACEMENT_3D('',#115639,#88448,#88449) ;
#72392 = AXIS2_PLACEMENT_3D('',#115644,#88452,#88453) ;
#72393 = AXIS2_PLACEMENT_3D('',#115652,#88457,#88458) ;
#72394 = AXIS2_PLACEMENT_3D('',#115656,#88460,#88461) ;
#72395 = AXIS2_PLACEMENT_3D('',#115660,#88463,#88464) ;
#72396 = AXIS2_PLACEMENT_3D('',#115662,#88465,#88466) ;
#72397 = AXIS2_PLACEMENT_3D('',#115664,#88467,#88468) ;
#72398 = AXIS2_PLACEMENT_3D('',#115668,#88470,#88471) ;
#72399 = AXIS2_PLACEMENT_3D('',#115672,#88473,#88474) ;
#72400 = AXIS2_PLACEMENT_3D('',#115680,#88478,#88479) ;
#72401 = AXIS2_PLACEMENT_3D('',#115684,#88481,#88482) ;
#72402 = AXIS2_PLACEMENT_3D('',#115689,#88485,#88486) ;
#72403 = AXIS2_PLACEMENT_3D('',#115697,#88490,#88491) ;
#72404 = AXIS2_PLACEMENT_3D('',#115701,#88493,#88494) ;
#72405 = AXIS2_PLACEMENT_3D('',#115705,#88496,#88497) ;
#72406 = AXIS2_PLACEMENT_3D('',#115707,#88498,#88499) ;
#72407 = AXIS2_PLACEMENT_3D('',#115709,#88500,#88501) ;
#72408 = AXIS2_PLACEMENT_3D('',#115713,#88503,#88504) ;
#72409 = AXIS2_PLACEMENT_3D('',#115715,#88506,#88507) ;
#72410 = AXIS2_PLACEMENT_3D('',#115726,#88512,#88513) ;
#72411 = AXIS2_PLACEMENT_3D('',#115734,#88517,#88518) ;
#72412 = AXIS2_PLACEMENT_3D('',#115736,#88520,#88521) ;
#72413 = AXIS2_PLACEMENT_3D('',#115747,#88526,#88527) ;
#72414 = AXIS2_PLACEMENT_3D('',#115755,#88531,#88532) ;
#72415 = AXIS2_PLACEMENT_3D('',#115757,#88534,#88535) ;
#72416 = AXIS2_PLACEMENT_3D('',#115772,#88542,#88543) ;
#72417 = AXIS2_PLACEMENT_3D('',#115776,#88545,#88546) ;
#72418 = AXIS2_PLACEMENT_3D('',#115778,#88548,#88549) ;
#72419 = AXIS2_PLACEMENT_3D('',#115787,#88554,#88555) ;
#72420 = AXIS2_PLACEMENT_3D('',#115793,#88559,#88560) ;
#72421 = AXIS2_PLACEMENT_3D('',#115802,#88565,#88566) ;
#72422 = AXIS2_PLACEMENT_3D('',#115811,#88571,#88572) ;
#72423 = AXIS2_PLACEMENT_3D('',#115820,#88577,#88578) ;
#72424 = AXIS2_PLACEMENT_3D('',#115825,#88580,#88581) ;
#72425 = AXIS2_PLACEMENT_3D('',#115828,#88583,#88584) ;
#72426 = AXIS2_PLACEMENT_3D('',#115829,#88585,#88586) ;
#72427 = AXIS2_PLACEMENT_3D('',#115835,#88590,#88591) ;
#72428 = AXIS2_PLACEMENT_3D('',#115837,#88592,#88593) ;
#72429 = AXIS2_PLACEMENT_3D('',#115840,#88595,#88596) ;
#72430 = AXIS2_PLACEMENT_3D('',#115841,#88597,#88598) ;
#72431 = AXIS2_PLACEMENT_3D('',#115847,#88602,#88603) ;
#72432 = AXIS2_PLACEMENT_3D('',#115849,#88604,#88605) ;
#72433 = AXIS2_PLACEMENT_3D('',#115852,#88607,#88608) ;
#72434 = AXIS2_PLACEMENT_3D('',#115853,#88609,#88610) ;
#72435 = AXIS2_PLACEMENT_3D('',#115858,#88614,#88615) ;
#72436 = AXIS2_PLACEMENT_3D('',#115861,#88617,#88618) ;
#72437 = AXIS2_PLACEMENT_3D('',#115862,#88619,#88620) ;
#72438 = AXIS2_PLACEMENT_3D('',#115865,#88623,#88624) ;
#72439 = AXIS2_PLACEMENT_3D('',#115871,#88628,#88629) ;
#72440 = AXIS2_PLACEMENT_3D('',#115873,#88630,#88631) ;
#72441 = AXIS2_PLACEMENT_3D('',#115876,#88633,#88634) ;
#72442 = AXIS2_PLACEMENT_3D('',#115877,#88635,#88636) ;
#72443 = AXIS2_PLACEMENT_3D('',#115883,#88640,#88641) ;
#72444 = AXIS2_PLACEMENT_3D('',#115885,#88642,#88643) ;
#72445 = AXIS2_PLACEMENT_3D('',#115888,#88645,#88646) ;
#72446 = AXIS2_PLACEMENT_3D('',#115889,#88647,#88648) ;
#72447 = AXIS2_PLACEMENT_3D('',#115895,#88652,#88653) ;
#72448 = AXIS2_PLACEMENT_3D('',#115897,#88654,#88655) ;
#72449 = AXIS2_PLACEMENT_3D('',#115900,#88657,#88658) ;
#72450 = AXIS2_PLACEMENT_3D('',#115901,#88659,#88660) ;
#72451 = AXIS2_PLACEMENT_3D('',#115907,#88664,#88665) ;
#72452 = AXIS2_PLACEMENT_3D('',#115909,#88666,#88667) ;
#72453 = AXIS2_PLACEMENT_3D('',#115912,#88669,#88670) ;
#72454 = AXIS2_PLACEMENT_3D('',#115913,#88671,#88672) ;
#72455 = AXIS2_PLACEMENT_3D('',#115919,#88676,#88677) ;
#72456 = AXIS2_PLACEMENT_3D('',#115921,#88678,#88679) ;
#72457 = AXIS2_PLACEMENT_3D('',#115924,#88681,#88682) ;
#72458 = AXIS2_PLACEMENT_3D('',#115925,#88683,#88684) ;
#72459 = AXIS2_PLACEMENT_3D('',#115931,#88688,#88689) ;
#72460 = AXIS2_PLACEMENT_3D('',#115933,#88690,#88691) ;
#72461 = AXIS2_PLACEMENT_3D('',#115936,#88693,#88694) ;
#72462 = AXIS2_PLACEMENT_3D('',#115937,#88695,#88696) ;
#72463 = AXIS2_PLACEMENT_3D('',#115939,#88697,#88698) ;
#72464 = AXIS2_PLACEMENT_3D('',#115942,#88700,#88701) ;
#72465 = AXIS2_PLACEMENT_3D('',#115943,#88702,#88703) ;
#72466 = AXIS2_PLACEMENT_3D('',#115945,#88704,#88705) ;
#72467 = AXIS2_PLACEMENT_3D('',#115948,#88707,#88708) ;
#72468 = AXIS2_PLACEMENT_3D('',#115949,#88709,#88710) ;
#72469 = AXIS2_PLACEMENT_3D('',#115955,#88714,#88715) ;
#72470 = AXIS2_PLACEMENT_3D('',#115957,#88716,#88717) ;
#72471 = AXIS2_PLACEMENT_3D('',#115960,#88719,#88720) ;
#72472 = AXIS2_PLACEMENT_3D('',#115961,#88721,#88722) ;
#72473 = AXIS2_PLACEMENT_3D('',#115967,#88726,#88727) ;
#72474 = AXIS2_PLACEMENT_3D('',#115969,#88728,#88729) ;
#72475 = AXIS2_PLACEMENT_3D('',#115972,#88731,#88732) ;
#72476 = AXIS2_PLACEMENT_3D('',#115973,#88733,#88734) ;
#72477 = AXIS2_PLACEMENT_3D('',#115976,#88737,#88738) ;
#72478 = AXIS2_PLACEMENT_3D('',#115979,#88739,#88740) ;
#72479 = AXIS2_PLACEMENT_3D('',#115983,#88742,#88743) ;
#72480 = AXIS2_PLACEMENT_3D('',#115991,#88747,#88748) ;
#72481 = AXIS2_PLACEMENT_3D('',#115999,#88752,#88753) ;
#72482 = AXIS2_PLACEMENT_3D('',#116003,#88755,#88756) ;
#72483 = AXIS2_PLACEMENT_3D('',#116012,#88762,#88763) ;
#72484 = AXIS2_PLACEMENT_3D('',#116017,#88765,#88766) ;
#72485 = AXIS2_PLACEMENT_3D('',#116021,#88768,#88769) ;
#72486 = AXIS2_PLACEMENT_3D('',#116025,#88771,#88772) ;
#72487 = AXIS2_PLACEMENT_3D('',#116028,#88774,#88775) ;
#72488 = AXIS2_PLACEMENT_3D('',#116029,#88776,#88777) ;
#72489 = AXIS2_PLACEMENT_3D('',#116030,#88778,#88779) ;
#72490 = AXIS2_PLACEMENT_3D('',#116031,#88780,#88781) ;
#72491 = AXIS2_PLACEMENT_3D('',#116032,#88782,#88783) ;
#72492 = AXIS2_PLACEMENT_3D('',#116033,#88784,#88785) ;
#72493 = AXIS2_PLACEMENT_3D('',#116034,#88786,#88787) ;
#72494 = AXIS2_PLACEMENT_3D('',#116035,#88788,#88789) ;
#72495 = AXIS2_PLACEMENT_3D('',#116037,#88790,#88791) ;
#72496 = AXIS2_PLACEMENT_3D('',#116038,#88792,#88793) ;
#72497 = AXIS2_PLACEMENT_3D('',#116039,#88794,#88795) ;
#72498 = AXIS2_PLACEMENT_3D('',#116040,#88796,#88797) ;
#72499 = AXIS2_PLACEMENT_3D('',#116041,#88798,#88799) ;
#72500 = AXIS2_PLACEMENT_3D('',#116042,#88800,#88801) ;
#72501 = AXIS2_PLACEMENT_3D('',#116043,#88802,#88803) ;
#72502 = AXIS2_PLACEMENT_3D('',#116044,#88804,#88805) ;
#72503 = AXIS2_PLACEMENT_3D('',#116045,#88806,#88807) ;
#72504 = AXIS2_PLACEMENT_3D('',#116056,#88809,#88810) ;
#72505 = AXIS2_PLACEMENT_3D('',#116113,#88812,#88813) ;
#72506 = AXIS2_PLACEMENT_3D('',#116114,#88814,#88815) ;
#72507 = AXIS2_PLACEMENT_3D('',#116115,#88816,#88817) ;
#72508 = AXIS2_PLACEMENT_3D('',#116116,#88818,#88819) ;
#72509 = AXIS2_PLACEMENT_3D('',#116117,#88820,#88821) ;
#72510 = AXIS2_PLACEMENT_3D('',#116118,#88822,#88823) ;
#72511 = AXIS2_PLACEMENT_3D('',#116119,#88824,#88825) ;
#72512 = AXIS2_PLACEMENT_3D('',#116120,#88826,#88827) ;
#72513 = AXIS2_PLACEMENT_3D('',#116121,#88828,#88829) ;
#72514 = AXIS2_PLACEMENT_3D('',#116122,#88830,#88831) ;
#72515 = AXIS2_PLACEMENT_3D('',#116123,#88832,#88833) ;
#72516 = AXIS2_PLACEMENT_3D('',#116124,#88834,#88835) ;
#72517 = AXIS2_PLACEMENT_3D('',#116125,#88836,#88837) ;
#72518 = AXIS2_PLACEMENT_3D('',#116126,#88838,#88839) ;
#72519 = AXIS2_PLACEMENT_3D('',#116127,#88840,#88841) ;
#72520 = AXIS2_PLACEMENT_3D('',#116128,#88842,#88843) ;
#72521 = AXIS2_PLACEMENT_3D('',#116129,#88844,#88845) ;
#72522 = AXIS2_PLACEMENT_3D('',#116130,#88846,#88847) ;
#72523 = AXIS2_PLACEMENT_3D('',#116131,#88848,#88849) ;
#72524 = AXIS2_PLACEMENT_3D('',#116132,#88850,#88851) ;
#72525 = AXIS2_PLACEMENT_3D('',#116133,#88852,#88853) ;
#72526 = AXIS2_PLACEMENT_3D('',#116134,#88854,#88855) ;
#72527 = AXIS2_PLACEMENT_3D('',#116135,#88856,#88857) ;
#72528 = AXIS2_PLACEMENT_3D('',#116138,#88859,#88860) ;
#72529 = AXIS2_PLACEMENT_3D('',#116139,#88861,#88862) ;
#72530 = AXIS2_PLACEMENT_3D('',#116140,#88863,#88864) ;
#72531 = AXIS2_PLACEMENT_3D('',#116141,#88865,#88866) ;
#72532 = AXIS2_PLACEMENT_3D('',#116142,#88867,#88868) ;
#72533 = AXIS2_PLACEMENT_3D('',#116143,#88869,#88870) ;
#72534 = AXIS2_PLACEMENT_3D('',#116144,#88871,#88872) ;
#72535 = AXIS2_PLACEMENT_3D('',#116145,#88873,#88874) ;
#72536 = AXIS2_PLACEMENT_3D('',#116146,#88875,#88876) ;
#72537 = AXIS2_PLACEMENT_3D('',#116147,#88877,#88878) ;
#72538 = AXIS2_PLACEMENT_3D('',#116148,#88879,#88880) ;
#72539 = AXIS2_PLACEMENT_3D('',#116149,#88881,#88882) ;
#72540 = AXIS2_PLACEMENT_3D('',#116150,#88883,#88884) ;
#72541 = AXIS2_PLACEMENT_3D('',#116151,#88885,#88886) ;
#72542 = AXIS2_PLACEMENT_3D('',#116152,#88887,#88888) ;
#72543 = AXIS2_PLACEMENT_3D('',#116153,#88889,#88890) ;
#72544 = AXIS2_PLACEMENT_3D('',#116155,#88891,#88892) ;
#72545 = AXIS2_PLACEMENT_3D('',#116156,#88893,#88894) ;
#72546 = AXIS2_PLACEMENT_3D('',#116157,#88895,#88896) ;
#72547 = AXIS2_PLACEMENT_3D('',#116158,#88897,#88898) ;
#72548 = AXIS2_PLACEMENT_3D('',#116159,#88899,#88900) ;
#72549 = AXIS2_PLACEMENT_3D('',#116160,#88901,#88902) ;
#72550 = AXIS2_PLACEMENT_3D('',#116161,#88903,#88904) ;
#72551 = AXIS2_PLACEMENT_3D('',#116162,#88905,#88906) ;
#72552 = AXIS2_PLACEMENT_3D('',#116163,#88907,#88908) ;
#72553 = AXIS2_PLACEMENT_3D('',#116164,#88909,#88910) ;
#72554 = AXIS2_PLACEMENT_3D('',#116165,#88911,#88912) ;
#72555 = AXIS2_PLACEMENT_3D('',#116166,#88913,#88914) ;
#72556 = AXIS2_PLACEMENT_3D('',#116167,#88915,#88916) ;
#72557 = AXIS2_PLACEMENT_3D('',#116170,#88918,#88919) ;
#72558 = AXIS2_PLACEMENT_3D('',#116171,#88920,#88921) ;
#72559 = AXIS2_PLACEMENT_3D('',#116172,#88922,#88923) ;
#72560 = AXIS2_PLACEMENT_3D('',#116173,#88924,#88925) ;
#72561 = AXIS2_PLACEMENT_3D('',#116174,#88926,#88927) ;
#72562 = AXIS2_PLACEMENT_3D('',#116175,#88928,#88929) ;
#72563 = AXIS2_PLACEMENT_3D('',#116176,#88930,#88931) ;
#72564 = AXIS2_PLACEMENT_3D('',#116177,#88932,#88933) ;
#72565 = AXIS2_PLACEMENT_3D('',#116178,#88934,#88935) ;
#72566 = AXIS2_PLACEMENT_3D('',#116179,#88936,#88937) ;
#72567 = AXIS2_PLACEMENT_3D('',#116180,#88938,#88939) ;
#72568 = AXIS2_PLACEMENT_3D('',#116181,#88940,#88941) ;
#72569 = AXIS2_PLACEMENT_3D('',#116182,#88942,#88943) ;
#72570 = AXIS2_PLACEMENT_3D('',#116184,#88944,#88945) ;
#72571 = AXIS2_PLACEMENT_3D('',#116185,#88946,#88947) ;
#72572 = AXIS2_PLACEMENT_3D('',#116186,#88948,#88949) ;
#72573 = AXIS2_PLACEMENT_3D('',#116187,#88950,#88951) ;
#72574 = AXIS2_PLACEMENT_3D('',#116188,#88952,#88953) ;
#72575 = AXIS2_PLACEMENT_3D('',#116189,#88954,#88955) ;
#72576 = AXIS2_PLACEMENT_3D('',#116190,#88956,#88957) ;
#72577 = AXIS2_PLACEMENT_3D('',#116191,#88958,#88959) ;
#72578 = AXIS2_PLACEMENT_3D('',#116192,#88960,#88961) ;
#72579 = AXIS2_PLACEMENT_3D('',#116193,#88962,#88963) ;
#72580 = AXIS2_PLACEMENT_3D('',#116194,#88964,#88965) ;
#72581 = AXIS2_PLACEMENT_3D('',#116196,#88967,#88968) ;
#72582 = AXIS2_PLACEMENT_3D('',#116197,#88969,#88970) ;
#72583 = AXIS2_PLACEMENT_3D('',#116198,#88971,#88972) ;
#72584 = AXIS2_PLACEMENT_3D('',#116199,#88973,#88974) ;
#72585 = AXIS2_PLACEMENT_3D('',#116200,#88975,#88976) ;
#72586 = AXIS2_PLACEMENT_3D('',#116201,#88977,#88978) ;
#72587 = AXIS2_PLACEMENT_3D('',#116202,#88979,#88980) ;
#72588 = AXIS2_PLACEMENT_3D('',#116203,#88981,#88982) ;
#72589 = AXIS2_PLACEMENT_3D('',#116204,#88983,#88984) ;
#72590 = AXIS2_PLACEMENT_3D('',#116205,#88985,#88986) ;
#72591 = AXIS2_PLACEMENT_3D('',#116206,#88987,#88988) ;
#72592 = AXIS2_PLACEMENT_3D('',#116207,#88989,#88990) ;
#72593 = AXIS2_PLACEMENT_3D('',#116208,#88991,#88992) ;
#72594 = AXIS2_PLACEMENT_3D('',#116209,#88993,#88994) ;
#72595 = AXIS2_PLACEMENT_3D('',#116210,#88995,#88996) ;
#72596 = AXIS2_PLACEMENT_3D('',#116211,#88997,#88998) ;
#72597 = AXIS2_PLACEMENT_3D('',#116212,#88999,#89000) ;
#72598 = AXIS2_PLACEMENT_3D('',#116213,#89001,#89002) ;
#72599 = AXIS2_PLACEMENT_3D('',#116214,#89003,#89004) ;
#72600 = AXIS2_PLACEMENT_3D('',#116215,#89005,#89006) ;
#72601 = AXIS2_PLACEMENT_3D('',#116216,#89007,#89008) ;
#72602 = AXIS2_PLACEMENT_3D('',#116217,#89009,#89010) ;
#72603 = AXIS2_PLACEMENT_3D('',#116218,#89011,#89012) ;
#72604 = AXIS2_PLACEMENT_3D('',#116219,#89013,#89014) ;
#72605 = AXIS2_PLACEMENT_3D('',#116220,#89015,#89016) ;
#72606 = AXIS2_PLACEMENT_3D('',#116221,#89017,#89018) ;
#72607 = AXIS2_PLACEMENT_3D('',#116222,#89019,#89020) ;
#72608 = AXIS2_PLACEMENT_3D('',#116223,#89021,#89022) ;
#72609 = AXIS2_PLACEMENT_3D('',#116224,#89023,#89024) ;
#72610 = AXIS2_PLACEMENT_3D('',#116225,#89025,#89026) ;
#72611 = AXIS2_PLACEMENT_3D('',#116226,#89027,#89028) ;
#72612 = AXIS2_PLACEMENT_3D('',#116227,#89029,#89030) ;
#72613 = AXIS2_PLACEMENT_3D('',#116228,#89031,#89032) ;
#72614 = AXIS2_PLACEMENT_3D('',#116229,#89033,#89034) ;
#72615 = AXIS2_PLACEMENT_3D('',#116230,#89035,#89036) ;
#72616 = AXIS2_PLACEMENT_3D('',#116231,#89037,#89038) ;
#72617 = AXIS2_PLACEMENT_3D('',#116232,#89039,#89040) ;
#72618 = AXIS2_PLACEMENT_3D('',#116233,#89041,#89042) ;
#72619 = AXIS2_PLACEMENT_3D('',#116234,#89043,#89044) ;
#72620 = AXIS2_PLACEMENT_3D('',#116235,#89045,#89046) ;
#72621 = AXIS2_PLACEMENT_3D('',#116236,#89047,#89048) ;
#72622 = AXIS2_PLACEMENT_3D('',#116237,#89049,#89050) ;
#72623 = AXIS2_PLACEMENT_3D('',#116238,#89051,#89052) ;
#72624 = AXIS2_PLACEMENT_3D('',#116239,#89053,#89054) ;
#72625 = AXIS2_PLACEMENT_3D('',#116240,#89055,#89056) ;
#72626 = AXIS2_PLACEMENT_3D('',#116241,#89057,#89058) ;
#72627 = AXIS2_PLACEMENT_3D('',#116242,#89059,#89060) ;
#72628 = AXIS2_PLACEMENT_3D('',#116243,#89061,#89062) ;
#72629 = AXIS2_PLACEMENT_3D('',#116244,#89063,#89064) ;
#72630 = AXIS2_PLACEMENT_3D('',#116245,#89065,#89066) ;
#72631 = AXIS2_PLACEMENT_3D('',#116246,#89067,#89068) ;
#72632 = AXIS2_PLACEMENT_3D('',#116247,#89069,#89070) ;
#72633 = AXIS2_PLACEMENT_3D('',#116248,#89071,#89072) ;
#72634 = AXIS2_PLACEMENT_3D('',#116249,#89073,#89074) ;
#72635 = AXIS2_PLACEMENT_3D('',#116250,#89075,#89076) ;
#72636 = AXIS2_PLACEMENT_3D('',#116251,#89077,#89078) ;
#72637 = AXIS2_PLACEMENT_3D('',#116252,#89079,#89080) ;
#72638 = AXIS2_PLACEMENT_3D('',#116253,#89081,#89082) ;
#72639 = AXIS2_PLACEMENT_3D('',#116254,#89083,#89084) ;
#72640 = AXIS2_PLACEMENT_3D('',#116255,#89085,#89086) ;
#72641 = AXIS2_PLACEMENT_3D('',#116256,#89087,#89088) ;
#72642 = AXIS2_PLACEMENT_3D('',#116257,#89089,#89090) ;
#72643 = AXIS2_PLACEMENT_3D('',#116258,#89091,#89092) ;
#72644 = AXIS2_PLACEMENT_3D('',#116259,#89093,#89094) ;
#72645 = AXIS2_PLACEMENT_3D('',#116260,#89095,#89096) ;
#72646 = AXIS2_PLACEMENT_3D('',#116261,#89097,#89098) ;
#72647 = AXIS2_PLACEMENT_3D('',#116262,#89099,#89100) ;
#72648 = AXIS2_PLACEMENT_3D('',#116263,#89101,#89102) ;
#72649 = AXIS2_PLACEMENT_3D('',#116264,#89103,#89104) ;
#72650 = AXIS2_PLACEMENT_3D('',#116265,#89105,#89106) ;
#72651 = AXIS2_PLACEMENT_3D('',#116266,#89107,#89108) ;
#72652 = AXIS2_PLACEMENT_3D('',#116267,#89109,#89110) ;
#72653 = AXIS2_PLACEMENT_3D('',#116268,#89111,#89112) ;
#72654 = AXIS2_PLACEMENT_3D('',#116269,#89113,#89114) ;
#72655 = AXIS2_PLACEMENT_3D('',#116270,#89115,#89116) ;
#72656 = AXIS2_PLACEMENT_3D('',#116271,#89117,#89118) ;
#72657 = AXIS2_PLACEMENT_3D('',#116272,#89119,#89120) ;
#72658 = AXIS2_PLACEMENT_3D('',#116273,#89121,#89122) ;
#72659 = AXIS2_PLACEMENT_3D('',#116274,#89123,#89124) ;
#72660 = AXIS2_PLACEMENT_3D('',#116275,#89125,#89126) ;
#72661 = AXIS2_PLACEMENT_3D('',#116276,#89127,#89128) ;
#72662 = AXIS2_PLACEMENT_3D('',#116277,#89129,#89130) ;
#72663 = AXIS2_PLACEMENT_3D('',#116278,#89131,#89132) ;
#72664 = AXIS2_PLACEMENT_3D('',#116279,#89133,#89134) ;
#72665 = AXIS2_PLACEMENT_3D('',#116280,#89135,#89136) ;
#72666 = AXIS2_PLACEMENT_3D('',#116281,#89137,#89138) ;
#72667 = AXIS2_PLACEMENT_3D('',#116282,#89139,#89140) ;
#72668 = AXIS2_PLACEMENT_3D('',#116283,#89141,#89142) ;
#72669 = AXIS2_PLACEMENT_3D('',#116284,#89143,#89144) ;
#72670 = AXIS2_PLACEMENT_3D('',#116285,#89145,#89146) ;
#72671 = AXIS2_PLACEMENT_3D('',#116286,#89147,#89148) ;
#72672 = AXIS2_PLACEMENT_3D('',#116287,#89149,#89150) ;
#72673 = AXIS2_PLACEMENT_3D('',#116288,#89151,#89152) ;
#72674 = AXIS2_PLACEMENT_3D('',#116289,#89153,#89154) ;
#72675 = AXIS2_PLACEMENT_3D('',#116290,#89155,#89156) ;
#72676 = AXIS2_PLACEMENT_3D('',#116291,#89157,#89158) ;
#72677 = AXIS2_PLACEMENT_3D('',#116292,#89159,#89160) ;
#72678 = AXIS2_PLACEMENT_3D('',#116293,#89161,#89162) ;
#72679 = AXIS2_PLACEMENT_3D('',#116294,#89163,#89164) ;
#72680 = AXIS2_PLACEMENT_3D('',#116295,#89165,#89166) ;
#72681 = AXIS2_PLACEMENT_3D('',#116296,#89167,#89168) ;
#72682 = AXIS2_PLACEMENT_3D('',#116297,#89169,#89170) ;
#72683 = AXIS2_PLACEMENT_3D('',#116298,#89171,#89172) ;
#72684 = AXIS2_PLACEMENT_3D('',#116299,#89173,#89174) ;
#72685 = AXIS2_PLACEMENT_3D('',#116300,#89175,#89176) ;
#72686 = AXIS2_PLACEMENT_3D('',#116301,#89177,#89178) ;
#72687 = AXIS2_PLACEMENT_3D('',#116302,#89179,#89180) ;
#72688 = AXIS2_PLACEMENT_3D('',#116303,#89181,#89182) ;
#72689 = AXIS2_PLACEMENT_3D('',#116304,#89183,#89184) ;
#72690 = AXIS2_PLACEMENT_3D('',#116305,#89185,#89186) ;
#72691 = AXIS2_PLACEMENT_3D('',#116306,#89187,#89188) ;
#72692 = AXIS2_PLACEMENT_3D('',#116307,#89189,#89190) ;
#72693 = AXIS2_PLACEMENT_3D('',#116308,#89191,#89192) ;
#72694 = AXIS2_PLACEMENT_3D('',#116309,#89193,#89194) ;
#72695 = AXIS2_PLACEMENT_3D('',#116310,#89195,#89196) ;
#72696 = AXIS2_PLACEMENT_3D('',#116311,#89197,#89198) ;
#72697 = AXIS2_PLACEMENT_3D('',#116312,#89199,#89200) ;
#72698 = AXIS2_PLACEMENT_3D('',#116313,#89201,#89202) ;
#72699 = AXIS2_PLACEMENT_3D('',#116314,#89203,#89204) ;
#72700 = AXIS2_PLACEMENT_3D('',#116315,#89205,#89206) ;
#72701 = AXIS2_PLACEMENT_3D('',#116316,#89207,#89208) ;
#72702 = AXIS2_PLACEMENT_3D('',#116317,#89209,#89210) ;
#72703 = AXIS2_PLACEMENT_3D('',#116318,#89211,#89212) ;
#72704 = AXIS2_PLACEMENT_3D('',#116319,#89213,#89214) ;
#72705 = AXIS2_PLACEMENT_3D('',#116320,#89215,#89216) ;
#72706 = AXIS2_PLACEMENT_3D('',#116321,#89217,#89218) ;
#72707 = AXIS2_PLACEMENT_3D('',#116322,#89219,#89220) ;
#72708 = AXIS2_PLACEMENT_3D('',#116323,#89221,#89222) ;
#72709 = AXIS2_PLACEMENT_3D('',#116324,#89223,#89224) ;
#72710 = AXIS2_PLACEMENT_3D('',#116325,#89225,#89226) ;
#72711 = AXIS2_PLACEMENT_3D('',#116326,#89227,#89228) ;
#72712 = AXIS2_PLACEMENT_3D('',#116327,#89229,#89230) ;
#72713 = AXIS2_PLACEMENT_3D('',#116328,#89231,#89232) ;
#72714 = AXIS2_PLACEMENT_3D('',#116329,#89233,#89234) ;
#72715 = AXIS2_PLACEMENT_3D('',#116330,#89235,#89236) ;
#72716 = AXIS2_PLACEMENT_3D('',#116331,#89237,#89238) ;
#72717 = AXIS2_PLACEMENT_3D('',#116332,#89239,#89240) ;
#72718 = AXIS2_PLACEMENT_3D('',#116333,#89241,#89242) ;
#72719 = AXIS2_PLACEMENT_3D('',#116334,#89243,#89244) ;
#72720 = AXIS2_PLACEMENT_3D('',#116335,#89245,#89246) ;
#72721 = AXIS2_PLACEMENT_3D('',#116336,#89247,#89248) ;
#72722 = AXIS2_PLACEMENT_3D('',#116337,#89249,#89250) ;
#72723 = AXIS2_PLACEMENT_3D('',#116338,#89251,#89252) ;
#72724 = AXIS2_PLACEMENT_3D('',#116339,#89253,#89254) ;
#72725 = AXIS2_PLACEMENT_3D('',#116340,#89255,#89256) ;
#72726 = AXIS2_PLACEMENT_3D('',#116341,#89257,#89258) ;
#72727 = AXIS2_PLACEMENT_3D('',#116342,#89259,#89260) ;
#72728 = AXIS2_PLACEMENT_3D('',#116343,#89261,#89262) ;
#72729 = AXIS2_PLACEMENT_3D('',#116344,#89263,#89264) ;
#72730 = AXIS2_PLACEMENT_3D('',#116345,#89265,#89266) ;
#72731 = AXIS2_PLACEMENT_3D('',#116346,#89267,#89268) ;
#72732 = AXIS2_PLACEMENT_3D('',#116347,#89269,#89270) ;
#72733 = AXIS2_PLACEMENT_3D('',#116348,#89271,#89272) ;
#72734 = AXIS2_PLACEMENT_3D('',#116349,#89273,#89274) ;
#72735 = AXIS2_PLACEMENT_3D('',#116350,#89275,#89276) ;
#72736 = AXIS2_PLACEMENT_3D('',#116351,#89277,#89278) ;
#72737 = AXIS2_PLACEMENT_3D('',#116352,#89279,#89280) ;
#72738 = AXIS2_PLACEMENT_3D('',#116353,#89281,#89282) ;
#72739 = AXIS2_PLACEMENT_3D('',#116354,#89283,#89284) ;
#72740 = AXIS2_PLACEMENT_3D('',#116355,#89285,#89286) ;
#72741 = AXIS2_PLACEMENT_3D('',#116356,#89287,#89288) ;
#72742 = AXIS2_PLACEMENT_3D('',#116357,#89289,#89290) ;
#72743 = AXIS2_PLACEMENT_3D('',#116358,#89291,#89292) ;
#72744 = AXIS2_PLACEMENT_3D('',#116359,#89293,#89294) ;
#72745 = AXIS2_PLACEMENT_3D('',#116360,#89295,#89296) ;
#72746 = AXIS2_PLACEMENT_3D('',#116361,#89297,#89298) ;
#72747 = AXIS2_PLACEMENT_3D('',#116362,#89299,#89300) ;
#72748 = AXIS2_PLACEMENT_3D('',#116363,#89301,#89302) ;
#72749 = AXIS2_PLACEMENT_3D('',#116364,#89303,#89304) ;
#72750 = AXIS2_PLACEMENT_3D('',#116365,#89305,#89306) ;
#72751 = AXIS2_PLACEMENT_3D('',#116366,#89307,#89308) ;
#72752 = AXIS2_PLACEMENT_3D('',#116367,#89309,#89310) ;
#72753 = AXIS2_PLACEMENT_3D('',#116368,#89311,#89312) ;
#72754 = AXIS2_PLACEMENT_3D('',#116369,#89313,#89314) ;
#72755 = AXIS2_PLACEMENT_3D('',#116370,#89315,#89316) ;
#72756 = AXIS2_PLACEMENT_3D('',#116371,#89317,#89318) ;
#72757 = AXIS2_PLACEMENT_3D('',#116372,#89319,#89320) ;
#72758 = AXIS2_PLACEMENT_3D('',#116373,#89321,#89322) ;
#72759 = AXIS2_PLACEMENT_3D('',#116382,#89327,#89328) ;
#72760 = AXIS2_PLACEMENT_3D('',#116391,#89333,#89334) ;
#72761 = AXIS2_PLACEMENT_3D('',#116400,#89339,#89340) ;
#72762 = AXIS2_PLACEMENT_3D('',#116409,#89345,#89346) ;
#72763 = AXIS2_PLACEMENT_3D('',#116418,#89351,#89352) ;
#72764 = AXIS2_PLACEMENT_3D('',#116422,#89354,#89355) ;
#72765 = AXIS2_PLACEMENT_3D('',#116424,#89356,#89357) ;
#72766 = AXIS2_PLACEMENT_3D('',#116428,#89360,#89361) ;
#72767 = AXIS2_PLACEMENT_3D('',#116432,#89363,#89364) ;
#72768 = AXIS2_PLACEMENT_3D('',#116434,#89365,#89366) ;
#72769 = AXIS2_PLACEMENT_3D('',#116438,#89369,#89370) ;
#72770 = AXIS2_PLACEMENT_3D('',#116439,#89371,#89372) ;
#72771 = AXIS2_PLACEMENT_3D('',#116440,#89373,#89374) ;
#72772 = AXIS2_PLACEMENT_3D('',#116441,#89375,#89376) ;
#72773 = AXIS2_PLACEMENT_3D('',#116442,#89377,#89378) ;
#72774 = AXIS2_PLACEMENT_3D('',#116443,#89379,#89380) ;
#72775 = AXIS2_PLACEMENT_3D('',#116444,#89381,#89382) ;
#72776 = AXIS2_PLACEMENT_3D('',#116453,#89387,#89388) ;
#72777 = AXIS2_PLACEMENT_3D('',#116459,#89392,#89393) ;
#72778 = AXIS2_PLACEMENT_3D('',#116465,#89397,#89398) ;
#72779 = AXIS2_PLACEMENT_3D('',#116474,#89403,#89404) ;
#72780 = AXIS2_PLACEMENT_3D('',#116483,#89409,#89410) ;
#72781 = AXIS2_PLACEMENT_3D('',#116489,#89414,#89415) ;
#72782 = AXIS2_PLACEMENT_3D('',#116495,#89419,#89420) ;
#72783 = AXIS2_PLACEMENT_3D('',#116504,#89425,#89426) ;
#72784 = AXIS2_PLACEMENT_3D('',#116513,#89431,#89432) ;
#72785 = AXIS2_PLACEMENT_3D('',#116522,#89437,#89438) ;
#72786 = AXIS2_PLACEMENT_3D('',#116531,#89443,#89444) ;
#72787 = AXIS2_PLACEMENT_3D('',#116532,#89445,#89446) ;
#72788 = AXIS2_PLACEMENT_3D('',#116533,#89447,#89448) ;
#72789 = AXIS2_PLACEMENT_3D('',#116534,#89449,#89450) ;
#72790 = AXIS2_PLACEMENT_3D('',#116535,#89451,#89452) ;
#72791 = AXIS2_PLACEMENT_3D('',#116536,#89453,#89454) ;
#72792 = AXIS2_PLACEMENT_3D('',#116537,#89455,#89456) ;
#72793 = AXIS2_PLACEMENT_3D('',#116538,#89457,#89458) ;
#72794 = AXIS2_PLACEMENT_3D('',#116539,#89459,#89460) ;
#72795 = AXIS2_PLACEMENT_3D('',#116540,#89461,#89462) ;
#72796 = AXIS2_PLACEMENT_3D('',#116541,#89463,#89464) ;
#72797 = AXIS2_PLACEMENT_3D('',#116542,#89465,#89466) ;
#72798 = AXIS2_PLACEMENT_3D('',#116543,#89467,#89468) ;
#72799 = AXIS2_PLACEMENT_3D('',#116544,#89469,#89470) ;
#72800 = AXIS2_PLACEMENT_3D('',#116545,#89471,#89472) ;
#72801 = AXIS2_PLACEMENT_3D('',#116546,#89473,#89474) ;
#72802 = AXIS2_PLACEMENT_3D('',#116547,#89475,#89476) ;
#72803 = AXIS2_PLACEMENT_3D('',#116548,#89477,#89478) ;
#72804 = AXIS2_PLACEMENT_3D('',#116549,#89479,#89480) ;
#72805 = AXIS2_PLACEMENT_3D('',#116550,#89481,#89482) ;
#72806 = AXIS2_PLACEMENT_3D('',#116551,#89483,#89484) ;
#72807 = AXIS2_PLACEMENT_3D('',#116552,#89485,#89486) ;
#72808 = AXIS2_PLACEMENT_3D('',#116553,#89487,#89488) ;
#72809 = AXIS2_PLACEMENT_3D('',#116554,#89489,#89490) ;
#72810 = AXIS2_PLACEMENT_3D('',#116555,#89491,#89492) ;
#72811 = AXIS2_PLACEMENT_3D('',#116556,#89493,#89494) ;
#72812 = AXIS2_PLACEMENT_3D('',#116557,#89495,#89496) ;
#72813 = AXIS2_PLACEMENT_3D('',#116558,#89497,#89498) ;
#72814 = AXIS2_PLACEMENT_3D('',#116559,#89499,#89500) ;
#72815 = AXIS2_PLACEMENT_3D('',#116560,#89501,#89502) ;
#72816 = AXIS2_PLACEMENT_3D('',#116561,#89503,#89504) ;
#72817 = AXIS2_PLACEMENT_3D('',#116562,#89505,#89506) ;
#72818 = AXIS2_PLACEMENT_3D('',#116563,#89507,#89508) ;
#72819 = AXIS2_PLACEMENT_3D('',#116564,#89509,#89510) ;
#72820 = AXIS2_PLACEMENT_3D('',#116565,#89511,#89512) ;
#72821 = AXIS2_PLACEMENT_3D('',#116566,#89513,#89514) ;
#72822 = AXIS2_PLACEMENT_3D('',#116567,#89515,#89516) ;
#72823 = AXIS2_PLACEMENT_3D('',#116568,#89517,#89518) ;
#72824 = AXIS2_PLACEMENT_3D('',#116569,#89519,#89520) ;
#72825 = AXIS2_PLACEMENT_3D('',#116570,#89521,#89522) ;
#72826 = AXIS2_PLACEMENT_3D('',#116571,#89523,#89524) ;
#72827 = AXIS2_PLACEMENT_3D('',#116572,#89525,#89526) ;
#72828 = AXIS2_PLACEMENT_3D('',#116573,#89527,#89528) ;
#72829 = AXIS2_PLACEMENT_3D('',#116574,#89529,#89530) ;
#72830 = AXIS2_PLACEMENT_3D('',#116575,#89531,#89532) ;
#72831 = AXIS2_PLACEMENT_3D('',#116576,#89533,#89534) ;
#72832 = AXIS2_PLACEMENT_3D('',#116577,#89535,#89536) ;
#72833 = AXIS2_PLACEMENT_3D('',#116578,#89537,#89538) ;
#72834 = AXIS2_PLACEMENT_3D('',#116579,#89539,#89540) ;
#72835 = AXIS2_PLACEMENT_3D('',#116580,#89541,#89542) ;
#72836 = AXIS2_PLACEMENT_3D('',#116581,#89543,#89544) ;
#72837 = AXIS2_PLACEMENT_3D('',#116582,#89545,#89546) ;
#72838 = AXIS2_PLACEMENT_3D('',#116583,#89547,#89548) ;
#72839 = AXIS2_PLACEMENT_3D('',#116584,#89549,#89550) ;
#72840 = AXIS2_PLACEMENT_3D('',#116585,#89551,#89552) ;
#72841 = AXIS2_PLACEMENT_3D('',#116586,#89553,#89554) ;
#72842 = AXIS2_PLACEMENT_3D('',#116587,#89555,#89556) ;
#72843 = AXIS2_PLACEMENT_3D('',#116588,#89557,#89558) ;
#72844 = AXIS2_PLACEMENT_3D('',#116589,#89559,#89560) ;
#72845 = AXIS2_PLACEMENT_3D('',#116590,#89561,#89562) ;
#72846 = AXIS2_PLACEMENT_3D('',#116591,#89563,#89564) ;
#72847 = AXIS2_PLACEMENT_3D('',#116592,#89565,#89566) ;
#72848 = AXIS2_PLACEMENT_3D('',#116593,#89567,#89568) ;
#72849 = AXIS2_PLACEMENT_3D('',#116594,#89569,#89570) ;
#72850 = AXIS2_PLACEMENT_3D('',#116595,#89571,#89572) ;
#72851 = AXIS2_PLACEMENT_3D('',#116596,#89573,#89574) ;
#72852 = AXIS2_PLACEMENT_3D('',#116597,#89575,#89576) ;
#72853 = AXIS2_PLACEMENT_3D('',#116598,#89577,#89578) ;
#72854 = AXIS2_PLACEMENT_3D('',#116599,#89579,#89580) ;
#72855 = AXIS2_PLACEMENT_3D('',#116600,#89581,#89582) ;
#72856 = AXIS2_PLACEMENT_3D('',#116601,#89583,#89584) ;
#72857 = AXIS2_PLACEMENT_3D('',#116602,#89585,#89586) ;
#72858 = AXIS2_PLACEMENT_3D('',#116603,#89587,#89588) ;
#72859 = AXIS2_PLACEMENT_3D('',#116604,#89589,#89590) ;
#72860 = AXIS2_PLACEMENT_3D('',#116605,#89591,#89592) ;
#72861 = AXIS2_PLACEMENT_3D('',#116606,#89593,#89594) ;
#72862 = AXIS2_PLACEMENT_3D('',#116607,#89595,#89596) ;
#72863 = AXIS2_PLACEMENT_3D('',#116608,#89597,#89598) ;
#72864 = AXIS2_PLACEMENT_3D('',#116609,#89599,#89600) ;
#72865 = AXIS2_PLACEMENT_3D('',#116610,#89601,#89602) ;
#72866 = AXIS2_PLACEMENT_3D('',#116611,#89603,#89604) ;
#72867 = AXIS2_PLACEMENT_3D('',#116612,#89605,#89606) ;
#72868 = AXIS2_PLACEMENT_3D('',#116613,#89607,#89608) ;
#72869 = AXIS2_PLACEMENT_3D('',#116614,#89609,#89610) ;
#72870 = AXIS2_PLACEMENT_3D('',#116615,#89611,#89612) ;
#72871 = AXIS2_PLACEMENT_3D('',#116616,#89613,#89614) ;
#72872 = AXIS2_PLACEMENT_3D('',#116617,#89615,#89616) ;
#72873 = AXIS2_PLACEMENT_3D('',#116618,#89617,#89618) ;
#72874 = AXIS2_PLACEMENT_3D('',#116619,#89619,#89620) ;
#72875 = AXIS2_PLACEMENT_3D('',#116620,#89621,#89622) ;
#72876 = AXIS2_PLACEMENT_3D('',#116621,#89623,#89624) ;
#72877 = AXIS2_PLACEMENT_3D('',#116622,#89625,#89626) ;
#72878 = AXIS2_PLACEMENT_3D('',#116623,#89627,#89628) ;
#72879 = AXIS2_PLACEMENT_3D('',#116624,#89629,#89630) ;
#72880 = AXIS2_PLACEMENT_3D('',#116625,#89631,#89632) ;
#72881 = AXIS2_PLACEMENT_3D('',#116626,#89633,#89634) ;
#72882 = AXIS2_PLACEMENT_3D('',#116627,#89635,#89636) ;
#72883 = AXIS2_PLACEMENT_3D('',#116628,#89637,#89638) ;
#72884 = AXIS2_PLACEMENT_3D('',#116629,#89639,#89640) ;
#72885 = AXIS2_PLACEMENT_3D('',#116630,#89641,#89642) ;
#72886 = AXIS2_PLACEMENT_3D('',#116631,#89643,#89644) ;
#72887 = AXIS2_PLACEMENT_3D('',#116632,#89645,#89646) ;
#72888 = AXIS2_PLACEMENT_3D('',#116633,#89647,#89648) ;
#72889 = AXIS2_PLACEMENT_3D('',#116634,#89649,#89650) ;
#72890 = AXIS2_PLACEMENT_3D('',#116635,#89651,#89652) ;
#72891 = AXIS2_PLACEMENT_3D('',#116636,#89653,#89654) ;
#72892 = AXIS2_PLACEMENT_3D('',#116637,#89655,#89656) ;
#72893 = AXIS2_PLACEMENT_3D('',#116638,#89657,#89658) ;
#72894 = AXIS2_PLACEMENT_3D('',#116639,#89659,#89660) ;
#72895 = AXIS2_PLACEMENT_3D('',#116640,#89661,#89662) ;
#72896 = AXIS2_PLACEMENT_3D('',#116641,#89663,#89664) ;
#72897 = AXIS2_PLACEMENT_3D('',#116642,#89665,#89666) ;
#72898 = AXIS2_PLACEMENT_3D('',#116643,#89667,#89668) ;
#72899 = AXIS2_PLACEMENT_3D('',#116658,#89675,#89676) ;
#72900 = AXIS2_PLACEMENT_3D('',#116662,#89678,#89679) ;
#72901 = AXIS2_PLACEMENT_3D('',#116664,#89681,#89682) ;
#72902 = AXIS2_PLACEMENT_3D('',#116679,#89689,#89690) ;
#72903 = AXIS2_PLACEMENT_3D('',#116683,#89692,#89693) ;
#72904 = AXIS2_PLACEMENT_3D('',#116685,#89695,#89696) ;
#72905 = AXIS2_PLACEMENT_3D('',#116700,#89703,#89704) ;
#72906 = AXIS2_PLACEMENT_3D('',#116704,#89706,#89707) ;
#72907 = AXIS2_PLACEMENT_3D('',#116706,#89709,#89710) ;
#72908 = AXIS2_PLACEMENT_3D('',#116721,#89717,#89718) ;
#72909 = AXIS2_PLACEMENT_3D('',#116725,#89720,#89721) ;
#72910 = AXIS2_PLACEMENT_3D('',#116727,#89723,#89724) ;
#72911 = AXIS2_PLACEMENT_3D('',#116742,#89731,#89732) ;
#72912 = AXIS2_PLACEMENT_3D('',#116746,#89734,#89735) ;
#72913 = AXIS2_PLACEMENT_3D('',#116748,#89737,#89738) ;
#72914 = AXIS2_PLACEMENT_3D('',#116763,#89745,#89746) ;
#72915 = AXIS2_PLACEMENT_3D('',#116767,#89748,#89749) ;
#72916 = AXIS2_PLACEMENT_3D('',#116769,#89751,#89752) ;
#72917 = AXIS2_PLACEMENT_3D('',#116784,#89759,#89760) ;
#72918 = AXIS2_PLACEMENT_3D('',#116788,#89762,#89763) ;
#72919 = AXIS2_PLACEMENT_3D('',#116790,#89765,#89766) ;
#72920 = AXIS2_PLACEMENT_3D('',#116805,#89773,#89774) ;
#72921 = AXIS2_PLACEMENT_3D('',#116809,#89776,#89777) ;
#72922 = AXIS2_PLACEMENT_3D('',#116811,#89779,#89780) ;
#72923 = AXIS2_PLACEMENT_3D('',#116826,#89787,#89788) ;
#72924 = AXIS2_PLACEMENT_3D('',#116830,#89790,#89791) ;
#72925 = AXIS2_PLACEMENT_3D('',#116832,#89793,#89794) ;
#72926 = AXIS2_PLACEMENT_3D('',#116841,#89799,#89800) ;
#72927 = AXIS2_PLACEMENT_3D('',#116847,#89804,#89805) ;
#72928 = AXIS2_PLACEMENT_3D('',#116856,#89810,#89811) ;
#72929 = AXIS2_PLACEMENT_3D('',#116865,#89816,#89817) ;
#72930 = AXIS2_PLACEMENT_3D('',#116874,#89822,#89823) ;
#72931 = AXIS2_PLACEMENT_3D('',#116883,#89828,#89829) ;
#72932 = AXIS2_PLACEMENT_3D('',#116889,#89833,#89834) ;
#72933 = AXIS2_PLACEMENT_3D('',#116898,#89839,#89840) ;
#72934 = AXIS2_PLACEMENT_3D('',#116907,#89845,#89846) ;
#72935 = AXIS2_PLACEMENT_3D('',#116916,#89851,#89852) ;
#72936 = AXIS2_PLACEMENT_3D('',#116925,#89857,#89858) ;
#72937 = AXIS2_PLACEMENT_3D('',#116931,#89862,#89863) ;
#72938 = AXIS2_PLACEMENT_3D('',#116940,#89868,#89869) ;
#72939 = AXIS2_PLACEMENT_3D('',#116949,#89874,#89875) ;
#72940 = AXIS2_PLACEMENT_3D('',#116958,#89880,#89881) ;
#72941 = AXIS2_PLACEMENT_3D('',#116967,#89886,#89887) ;
#72942 = AXIS2_PLACEMENT_3D('',#116973,#89891,#89892) ;
#72943 = AXIS2_PLACEMENT_3D('',#116982,#89897,#89898) ;
#72944 = AXIS2_PLACEMENT_3D('',#116991,#89903,#89904) ;
#72945 = AXIS2_PLACEMENT_3D('',#117000,#89909,#89910) ;
#72946 = AXIS2_PLACEMENT_3D('',#117009,#89915,#89916) ;
#72947 = AXIS2_PLACEMENT_3D('',#117015,#89920,#89921) ;
#72948 = AXIS2_PLACEMENT_3D('',#117024,#89926,#89927) ;
#72949 = AXIS2_PLACEMENT_3D('',#117033,#89932,#89933) ;
#72950 = AXIS2_PLACEMENT_3D('',#117042,#89938,#89939) ;
#72951 = AXIS2_PLACEMENT_3D('',#117051,#89944,#89945) ;
#72952 = AXIS2_PLACEMENT_3D('',#117057,#89949,#89950) ;
#72953 = AXIS2_PLACEMENT_3D('',#117066,#89955,#89956) ;
#72954 = AXIS2_PLACEMENT_3D('',#117075,#89961,#89962) ;
#72955 = AXIS2_PLACEMENT_3D('',#117084,#89967,#89968) ;
#72956 = AXIS2_PLACEMENT_3D('',#117093,#89973,#89974) ;
#72957 = AXIS2_PLACEMENT_3D('',#117099,#89978,#89979) ;
#72958 = AXIS2_PLACEMENT_3D('',#117108,#89984,#89985) ;
#72959 = AXIS2_PLACEMENT_3D('',#117117,#89990,#89991) ;
#72960 = AXIS2_PLACEMENT_3D('',#117126,#89996,#89997) ;
#72961 = AXIS2_PLACEMENT_3D('',#117135,#90002,#90003) ;
#72962 = AXIS2_PLACEMENT_3D('',#117141,#90007,#90008) ;
#72963 = AXIS2_PLACEMENT_3D('',#117150,#90013,#90014) ;
#72964 = AXIS2_PLACEMENT_3D('',#117159,#90019,#90020) ;
#72965 = AXIS2_PLACEMENT_3D('',#117168,#90025,#90026) ;
#72966 = AXIS2_PLACEMENT_3D('',#117177,#90031,#90032) ;
#72967 = AXIS2_PLACEMENT_3D('',#117183,#90036,#90037) ;
#72968 = AXIS2_PLACEMENT_3D('',#117192,#90042,#90043) ;
#72969 = AXIS2_PLACEMENT_3D('',#117201,#90048,#90049) ;
#72970 = AXIS2_PLACEMENT_3D('',#117210,#90054,#90055) ;
#72971 = AXIS2_PLACEMENT_3D('',#117215,#90057,#90058) ;
#72972 = AXIS2_PLACEMENT_3D('',#117218,#90060,#90061) ;
#72973 = AXIS2_PLACEMENT_3D('',#117219,#90062,#90063) ;
#72974 = AXIS2_PLACEMENT_3D('',#117225,#90067,#90068) ;
#72975 = AXIS2_PLACEMENT_3D('',#117227,#90069,#90070) ;
#72976 = AXIS2_PLACEMENT_3D('',#117230,#90072,#90073) ;
#72977 = AXIS2_PLACEMENT_3D('',#117231,#90074,#90075) ;
#72978 = AXIS2_PLACEMENT_3D('',#117237,#90079,#90080) ;
#72979 = AXIS2_PLACEMENT_3D('',#117239,#90081,#90082) ;
#72980 = AXIS2_PLACEMENT_3D('',#117242,#90084,#90085) ;
#72981 = AXIS2_PLACEMENT_3D('',#117243,#90086,#90087) ;
#72982 = AXIS2_PLACEMENT_3D('',#117248,#90091,#90092) ;
#72983 = AXIS2_PLACEMENT_3D('',#117251,#90094,#90095) ;
#72984 = AXIS2_PLACEMENT_3D('',#117252,#90096,#90097) ;
#72985 = AXIS2_PLACEMENT_3D('',#117255,#90100,#90101) ;
#72986 = AXIS2_PLACEMENT_3D('',#117261,#90105,#90106) ;
#72987 = AXIS2_PLACEMENT_3D('',#117263,#90107,#90108) ;
#72988 = AXIS2_PLACEMENT_3D('',#117266,#90110,#90111) ;
#72989 = AXIS2_PLACEMENT_3D('',#117267,#90112,#90113) ;
#72990 = AXIS2_PLACEMENT_3D('',#117273,#90117,#90118) ;
#72991 = AXIS2_PLACEMENT_3D('',#117275,#90119,#90120) ;
#72992 = AXIS2_PLACEMENT_3D('',#117278,#90122,#90123) ;
#72993 = AXIS2_PLACEMENT_3D('',#117279,#90124,#90125) ;
#72994 = AXIS2_PLACEMENT_3D('',#117285,#90129,#90130) ;
#72995 = AXIS2_PLACEMENT_3D('',#117287,#90131,#90132) ;
#72996 = AXIS2_PLACEMENT_3D('',#117290,#90134,#90135) ;
#72997 = AXIS2_PLACEMENT_3D('',#117291,#90136,#90137) ;
#72998 = AXIS2_PLACEMENT_3D('',#117297,#90141,#90142) ;
#72999 = AXIS2_PLACEMENT_3D('',#117299,#90143,#90144) ;
#73000 = AXIS2_PLACEMENT_3D('',#117302,#90146,#90147) ;
#73001 = AXIS2_PLACEMENT_3D('',#117303,#90148,#90149) ;
#73002 = AXIS2_PLACEMENT_3D('',#117309,#90153,#90154) ;
#73003 = AXIS2_PLACEMENT_3D('',#117311,#90155,#90156) ;
#73004 = AXIS2_PLACEMENT_3D('',#117314,#90158,#90159) ;
#73005 = AXIS2_PLACEMENT_3D('',#117315,#90160,#90161) ;
#73006 = AXIS2_PLACEMENT_3D('',#117321,#90165,#90166) ;
#73007 = AXIS2_PLACEMENT_3D('',#117323,#90167,#90168) ;
#73008 = AXIS2_PLACEMENT_3D('',#117326,#90170,#90171) ;
#73009 = AXIS2_PLACEMENT_3D('',#117327,#90172,#90173) ;
#73010 = AXIS2_PLACEMENT_3D('',#117329,#90174,#90175) ;
#73011 = AXIS2_PLACEMENT_3D('',#117332,#90177,#90178) ;
#73012 = AXIS2_PLACEMENT_3D('',#117333,#90179,#90180) ;
#73013 = AXIS2_PLACEMENT_3D('',#117335,#90181,#90182) ;
#73014 = AXIS2_PLACEMENT_3D('',#117338,#90184,#90185) ;
#73015 = AXIS2_PLACEMENT_3D('',#117339,#90186,#90187) ;
#73016 = AXIS2_PLACEMENT_3D('',#117345,#90191,#90192) ;
#73017 = AXIS2_PLACEMENT_3D('',#117347,#90193,#90194) ;
#73018 = AXIS2_PLACEMENT_3D('',#117350,#90196,#90197) ;
#73019 = AXIS2_PLACEMENT_3D('',#117351,#90198,#90199) ;
#73020 = AXIS2_PLACEMENT_3D('',#117357,#90203,#90204) ;
#73021 = AXIS2_PLACEMENT_3D('',#117359,#90205,#90206) ;
#73022 = AXIS2_PLACEMENT_3D('',#117362,#90208,#90209) ;
#73023 = AXIS2_PLACEMENT_3D('',#117363,#90210,#90211) ;
#73024 = AXIS2_PLACEMENT_3D('',#117366,#90214,#90215) ;
#73025 = AXIS2_PLACEMENT_3D('',#117369,#90216,#90217) ;
#73026 = AXIS2_PLACEMENT_3D('',#117373,#90219,#90220) ;
#73027 = AXIS2_PLACEMENT_3D('',#117381,#90224,#90225) ;
#73028 = AXIS2_PLACEMENT_3D('',#117389,#90229,#90230) ;
#73029 = AXIS2_PLACEMENT_3D('',#117393,#90232,#90233) ;
#73030 = AXIS2_PLACEMENT_3D('',#117402,#90239,#90240) ;
#73031 = AXIS2_PLACEMENT_3D('',#117407,#90242,#90243) ;
#73032 = AXIS2_PLACEMENT_3D('',#117410,#90245,#90246) ;
#73033 = AXIS2_PLACEMENT_3D('',#117411,#90247,#90248) ;
#73034 = AXIS2_PLACEMENT_3D('',#117417,#90252,#90253) ;
#73035 = AXIS2_PLACEMENT_3D('',#117419,#90254,#90255) ;
#73036 = AXIS2_PLACEMENT_3D('',#117422,#90257,#90258) ;
#73037 = AXIS2_PLACEMENT_3D('',#117423,#90259,#90260) ;
#73038 = AXIS2_PLACEMENT_3D('',#117429,#90264,#90265) ;
#73039 = AXIS2_PLACEMENT_3D('',#117431,#90266,#90267) ;
#73040 = AXIS2_PLACEMENT_3D('',#117434,#90269,#90270) ;
#73041 = AXIS2_PLACEMENT_3D('',#117435,#90271,#90272) ;
#73042 = AXIS2_PLACEMENT_3D('',#117440,#90276,#90277) ;
#73043 = AXIS2_PLACEMENT_3D('',#117443,#90279,#90280) ;
#73044 = AXIS2_PLACEMENT_3D('',#117444,#90281,#90282) ;
#73045 = AXIS2_PLACEMENT_3D('',#117447,#90285,#90286) ;
#73046 = AXIS2_PLACEMENT_3D('',#117453,#90290,#90291) ;
#73047 = AXIS2_PLACEMENT_3D('',#117455,#90292,#90293) ;
#73048 = AXIS2_PLACEMENT_3D('',#117458,#90295,#90296) ;
#73049 = AXIS2_PLACEMENT_3D('',#117459,#90297,#90298) ;
#73050 = AXIS2_PLACEMENT_3D('',#117465,#90302,#90303) ;
#73051 = AXIS2_PLACEMENT_3D('',#117467,#90304,#90305) ;
#73052 = AXIS2_PLACEMENT_3D('',#117470,#90307,#90308) ;
#73053 = AXIS2_PLACEMENT_3D('',#117471,#90309,#90310) ;
#73054 = AXIS2_PLACEMENT_3D('',#117477,#90314,#90315) ;
#73055 = AXIS2_PLACEMENT_3D('',#117479,#90316,#90317) ;
#73056 = AXIS2_PLACEMENT_3D('',#117482,#90319,#90320) ;
#73057 = AXIS2_PLACEMENT_3D('',#117483,#90321,#90322) ;
#73058 = AXIS2_PLACEMENT_3D('',#117489,#90326,#90327) ;
#73059 = AXIS2_PLACEMENT_3D('',#117491,#90328,#90329) ;
#73060 = AXIS2_PLACEMENT_3D('',#117494,#90331,#90332) ;
#73061 = AXIS2_PLACEMENT_3D('',#117495,#90333,#90334) ;
#73062 = AXIS2_PLACEMENT_3D('',#117501,#90338,#90339) ;
#73063 = AXIS2_PLACEMENT_3D('',#117503,#90340,#90341) ;
#73064 = AXIS2_PLACEMENT_3D('',#117506,#90343,#90344) ;
#73065 = AXIS2_PLACEMENT_3D('',#117507,#90345,#90346) ;
#73066 = AXIS2_PLACEMENT_3D('',#117513,#90350,#90351) ;
#73067 = AXIS2_PLACEMENT_3D('',#117515,#90352,#90353) ;
#73068 = AXIS2_PLACEMENT_3D('',#117518,#90355,#90356) ;
#73069 = AXIS2_PLACEMENT_3D('',#117519,#90357,#90358) ;
#73070 = AXIS2_PLACEMENT_3D('',#117521,#90359,#90360) ;
#73071 = AXIS2_PLACEMENT_3D('',#117524,#90362,#90363) ;
#73072 = AXIS2_PLACEMENT_3D('',#117525,#90364,#90365) ;
#73073 = AXIS2_PLACEMENT_3D('',#117527,#90366,#90367) ;
#73074 = AXIS2_PLACEMENT_3D('',#117530,#90369,#90370) ;
#73075 = AXIS2_PLACEMENT_3D('',#117531,#90371,#90372) ;
#73076 = AXIS2_PLACEMENT_3D('',#117537,#90376,#90377) ;
#73077 = AXIS2_PLACEMENT_3D('',#117539,#90378,#90379) ;
#73078 = AXIS2_PLACEMENT_3D('',#117542,#90381,#90382) ;
#73079 = AXIS2_PLACEMENT_3D('',#117543,#90383,#90384) ;
#73080 = AXIS2_PLACEMENT_3D('',#117549,#90388,#90389) ;
#73081 = AXIS2_PLACEMENT_3D('',#117551,#90390,#90391) ;
#73082 = AXIS2_PLACEMENT_3D('',#117554,#90393,#90394) ;
#73083 = AXIS2_PLACEMENT_3D('',#117555,#90395,#90396) ;
#73084 = AXIS2_PLACEMENT_3D('',#117558,#90399,#90400) ;
#73085 = AXIS2_PLACEMENT_3D('',#117561,#90401,#90402) ;
#73086 = AXIS2_PLACEMENT_3D('',#117565,#90404,#90405) ;
#73087 = AXIS2_PLACEMENT_3D('',#117573,#90409,#90410) ;
#73088 = AXIS2_PLACEMENT_3D('',#117581,#90414,#90415) ;
#73089 = AXIS2_PLACEMENT_3D('',#117585,#90417,#90418) ;
#73090 = AXIS2_PLACEMENT_3D('',#117594,#90424,#90425) ;
#73091 = AXIS2_PLACEMENT_3D('',#117599,#90427,#90428) ;
#73092 = AXIS2_PLACEMENT_3D('',#117602,#90430,#90431) ;
#73093 = AXIS2_PLACEMENT_3D('',#117603,#90432,#90433) ;
#73094 = AXIS2_PLACEMENT_3D('',#117609,#90437,#90438) ;
#73095 = AXIS2_PLACEMENT_3D('',#117611,#90439,#90440) ;
#73096 = AXIS2_PLACEMENT_3D('',#117614,#90442,#90443) ;
#73097 = AXIS2_PLACEMENT_3D('',#117615,#90444,#90445) ;
#73098 = AXIS2_PLACEMENT_3D('',#117621,#90449,#90450) ;
#73099 = AXIS2_PLACEMENT_3D('',#117623,#90451,#90452) ;
#73100 = AXIS2_PLACEMENT_3D('',#117626,#90454,#90455) ;
#73101 = AXIS2_PLACEMENT_3D('',#117627,#90456,#90457) ;
#73102 = AXIS2_PLACEMENT_3D('',#117632,#90461,#90462) ;
#73103 = AXIS2_PLACEMENT_3D('',#117635,#90464,#90465) ;
#73104 = AXIS2_PLACEMENT_3D('',#117636,#90466,#90467) ;
#73105 = AXIS2_PLACEMENT_3D('',#117639,#90470,#90471) ;
#73106 = AXIS2_PLACEMENT_3D('',#117645,#90475,#90476) ;
#73107 = AXIS2_PLACEMENT_3D('',#117647,#90477,#90478) ;
#73108 = AXIS2_PLACEMENT_3D('',#117650,#90480,#90481) ;
#73109 = AXIS2_PLACEMENT_3D('',#117651,#90482,#90483) ;
#73110 = AXIS2_PLACEMENT_3D('',#117657,#90487,#90488) ;
#73111 = AXIS2_PLACEMENT_3D('',#117659,#90489,#90490) ;
#73112 = AXIS2_PLACEMENT_3D('',#117662,#90492,#90493) ;
#73113 = AXIS2_PLACEMENT_3D('',#117663,#90494,#90495) ;
#73114 = AXIS2_PLACEMENT_3D('',#117669,#90499,#90500) ;
#73115 = AXIS2_PLACEMENT_3D('',#117671,#90501,#90502) ;
#73116 = AXIS2_PLACEMENT_3D('',#117674,#90504,#90505) ;
#73117 = AXIS2_PLACEMENT_3D('',#117675,#90506,#90507) ;
#73118 = AXIS2_PLACEMENT_3D('',#117681,#90511,#90512) ;
#73119 = AXIS2_PLACEMENT_3D('',#117683,#90513,#90514) ;
#73120 = AXIS2_PLACEMENT_3D('',#117686,#90516,#90517) ;
#73121 = AXIS2_PLACEMENT_3D('',#117687,#90518,#90519) ;
#73122 = AXIS2_PLACEMENT_3D('',#117693,#90523,#90524) ;
#73123 = AXIS2_PLACEMENT_3D('',#117695,#90525,#90526) ;
#73124 = AXIS2_PLACEMENT_3D('',#117698,#90528,#90529) ;
#73125 = AXIS2_PLACEMENT_3D('',#117699,#90530,#90531) ;
#73126 = AXIS2_PLACEMENT_3D('',#117705,#90535,#90536) ;
#73127 = AXIS2_PLACEMENT_3D('',#117707,#90537,#90538) ;
#73128 = AXIS2_PLACEMENT_3D('',#117710,#90540,#90541) ;
#73129 = AXIS2_PLACEMENT_3D('',#117711,#90542,#90543) ;
#73130 = AXIS2_PLACEMENT_3D('',#117713,#90544,#90545) ;
#73131 = AXIS2_PLACEMENT_3D('',#117716,#90547,#90548) ;
#73132 = AXIS2_PLACEMENT_3D('',#117717,#90549,#90550) ;
#73133 = AXIS2_PLACEMENT_3D('',#117719,#90551,#90552) ;
#73134 = AXIS2_PLACEMENT_3D('',#117722,#90554,#90555) ;
#73135 = AXIS2_PLACEMENT_3D('',#117723,#90556,#90557) ;
#73136 = AXIS2_PLACEMENT_3D('',#117729,#90561,#90562) ;
#73137 = AXIS2_PLACEMENT_3D('',#117731,#90563,#90564) ;
#73138 = AXIS2_PLACEMENT_3D('',#117734,#90566,#90567) ;
#73139 = AXIS2_PLACEMENT_3D('',#117735,#90568,#90569) ;
#73140 = AXIS2_PLACEMENT_3D('',#117741,#90573,#90574) ;
#73141 = AXIS2_PLACEMENT_3D('',#117743,#90575,#90576) ;
#73142 = AXIS2_PLACEMENT_3D('',#117746,#90578,#90579) ;
#73143 = AXIS2_PLACEMENT_3D('',#117747,#90580,#90581) ;
#73144 = AXIS2_PLACEMENT_3D('',#117750,#90584,#90585) ;
#73145 = AXIS2_PLACEMENT_3D('',#117753,#90586,#90587) ;
#73146 = AXIS2_PLACEMENT_3D('',#117757,#90589,#90590) ;
#73147 = AXIS2_PLACEMENT_3D('',#117765,#90594,#90595) ;
#73148 = AXIS2_PLACEMENT_3D('',#117773,#90599,#90600) ;
#73149 = AXIS2_PLACEMENT_3D('',#117777,#90602,#90603) ;
#73150 = AXIS2_PLACEMENT_3D('',#117786,#90609,#90610) ;
#73151 = AXIS2_PLACEMENT_3D('',#117791,#90612,#90613) ;
#73152 = AXIS2_PLACEMENT_3D('',#117794,#90615,#90616) ;
#73153 = AXIS2_PLACEMENT_3D('',#117795,#90617,#90618) ;
#73154 = AXIS2_PLACEMENT_3D('',#117801,#90622,#90623) ;
#73155 = AXIS2_PLACEMENT_3D('',#117803,#90624,#90625) ;
#73156 = AXIS2_PLACEMENT_3D('',#117806,#90627,#90628) ;
#73157 = AXIS2_PLACEMENT_3D('',#117807,#90629,#90630) ;
#73158 = AXIS2_PLACEMENT_3D('',#117813,#90634,#90635) ;
#73159 = AXIS2_PLACEMENT_3D('',#117815,#90636,#90637) ;
#73160 = AXIS2_PLACEMENT_3D('',#117818,#90639,#90640) ;
#73161 = AXIS2_PLACEMENT_3D('',#117819,#90641,#90642) ;
#73162 = AXIS2_PLACEMENT_3D('',#117824,#90646,#90647) ;
#73163 = AXIS2_PLACEMENT_3D('',#117827,#90649,#90650) ;
#73164 = AXIS2_PLACEMENT_3D('',#117828,#90651,#90652) ;
#73165 = AXIS2_PLACEMENT_3D('',#117831,#90655,#90656) ;
#73166 = AXIS2_PLACEMENT_3D('',#117837,#90660,#90661) ;
#73167 = AXIS2_PLACEMENT_3D('',#117839,#90662,#90663) ;
#73168 = AXIS2_PLACEMENT_3D('',#117842,#90665,#90666) ;
#73169 = AXIS2_PLACEMENT_3D('',#117843,#90667,#90668) ;
#73170 = AXIS2_PLACEMENT_3D('',#117849,#90672,#90673) ;
#73171 = AXIS2_PLACEMENT_3D('',#117851,#90674,#90675) ;
#73172 = AXIS2_PLACEMENT_3D('',#117854,#90677,#90678) ;
#73173 = AXIS2_PLACEMENT_3D('',#117855,#90679,#90680) ;
#73174 = AXIS2_PLACEMENT_3D('',#117861,#90684,#90685) ;
#73175 = AXIS2_PLACEMENT_3D('',#117863,#90686,#90687) ;
#73176 = AXIS2_PLACEMENT_3D('',#117866,#90689,#90690) ;
#73177 = AXIS2_PLACEMENT_3D('',#117867,#90691,#90692) ;
#73178 = AXIS2_PLACEMENT_3D('',#117873,#90696,#90697) ;
#73179 = AXIS2_PLACEMENT_3D('',#117875,#90698,#90699) ;
#73180 = AXIS2_PLACEMENT_3D('',#117878,#90701,#90702) ;
#73181 = AXIS2_PLACEMENT_3D('',#117879,#90703,#90704) ;
#73182 = AXIS2_PLACEMENT_3D('',#117885,#90708,#90709) ;
#73183 = AXIS2_PLACEMENT_3D('',#117887,#90710,#90711) ;
#73184 = AXIS2_PLACEMENT_3D('',#117890,#90713,#90714) ;
#73185 = AXIS2_PLACEMENT_3D('',#117891,#90715,#90716) ;
#73186 = AXIS2_PLACEMENT_3D('',#117897,#90720,#90721) ;
#73187 = AXIS2_PLACEMENT_3D('',#117899,#90722,#90723) ;
#73188 = AXIS2_PLACEMENT_3D('',#117902,#90725,#90726) ;
#73189 = AXIS2_PLACEMENT_3D('',#117903,#90727,#90728) ;
#73190 = AXIS2_PLACEMENT_3D('',#117905,#90729,#90730) ;
#73191 = AXIS2_PLACEMENT_3D('',#117908,#90732,#90733) ;
#73192 = AXIS2_PLACEMENT_3D('',#117909,#90734,#90735) ;
#73193 = AXIS2_PLACEMENT_3D('',#117911,#90736,#90737) ;
#73194 = AXIS2_PLACEMENT_3D('',#117914,#90739,#90740) ;
#73195 = AXIS2_PLACEMENT_3D('',#117915,#90741,#90742) ;
#73196 = AXIS2_PLACEMENT_3D('',#117921,#90746,#90747) ;
#73197 = AXIS2_PLACEMENT_3D('',#117923,#90748,#90749) ;
#73198 = AXIS2_PLACEMENT_3D('',#117926,#90751,#90752) ;
#73199 = AXIS2_PLACEMENT_3D('',#117927,#90753,#90754) ;
#73200 = AXIS2_PLACEMENT_3D('',#117933,#90758,#90759) ;
#73201 = AXIS2_PLACEMENT_3D('',#117935,#90760,#90761) ;
#73202 = AXIS2_PLACEMENT_3D('',#117938,#90763,#90764) ;
#73203 = AXIS2_PLACEMENT_3D('',#117939,#90765,#90766) ;
#73204 = AXIS2_PLACEMENT_3D('',#117942,#90769,#90770) ;
#73205 = AXIS2_PLACEMENT_3D('',#117945,#90771,#90772) ;
#73206 = AXIS2_PLACEMENT_3D('',#117949,#90774,#90775) ;
#73207 = AXIS2_PLACEMENT_3D('',#117957,#90779,#90780) ;
#73208 = AXIS2_PLACEMENT_3D('',#117965,#90784,#90785) ;
#73209 = AXIS2_PLACEMENT_3D('',#117969,#90787,#90788) ;
#73210 = AXIS2_PLACEMENT_3D('',#117978,#90794,#90795) ;
#73211 = AXIS2_PLACEMENT_3D('',#117983,#90797,#90798) ;
#73212 = AXIS2_PLACEMENT_3D('',#117986,#90800,#90801) ;
#73213 = AXIS2_PLACEMENT_3D('',#117987,#90802,#90803) ;
#73214 = AXIS2_PLACEMENT_3D('',#117993,#90807,#90808) ;
#73215 = AXIS2_PLACEMENT_3D('',#117995,#90809,#90810) ;
#73216 = AXIS2_PLACEMENT_3D('',#117998,#90812,#90813) ;
#73217 = AXIS2_PLACEMENT_3D('',#117999,#90814,#90815) ;
#73218 = AXIS2_PLACEMENT_3D('',#118005,#90819,#90820) ;
#73219 = AXIS2_PLACEMENT_3D('',#118007,#90821,#90822) ;
#73220 = AXIS2_PLACEMENT_3D('',#118010,#90824,#90825) ;
#73221 = AXIS2_PLACEMENT_3D('',#118011,#90826,#90827) ;
#73222 = AXIS2_PLACEMENT_3D('',#118016,#90831,#90832) ;
#73223 = AXIS2_PLACEMENT_3D('',#118019,#90834,#90835) ;
#73224 = AXIS2_PLACEMENT_3D('',#118020,#90836,#90837) ;
#73225 = AXIS2_PLACEMENT_3D('',#118023,#90840,#90841) ;
#73226 = AXIS2_PLACEMENT_3D('',#118029,#90845,#90846) ;
#73227 = AXIS2_PLACEMENT_3D('',#118031,#90847,#90848) ;
#73228 = AXIS2_PLACEMENT_3D('',#118034,#90850,#90851) ;
#73229 = AXIS2_PLACEMENT_3D('',#118035,#90852,#90853) ;
#73230 = AXIS2_PLACEMENT_3D('',#118041,#90857,#90858) ;
#73231 = AXIS2_PLACEMENT_3D('',#118043,#90859,#90860) ;
#73232 = AXIS2_PLACEMENT_3D('',#118046,#90862,#90863) ;
#73233 = AXIS2_PLACEMENT_3D('',#118047,#90864,#90865) ;
#73234 = AXIS2_PLACEMENT_3D('',#118053,#90869,#90870) ;
#73235 = AXIS2_PLACEMENT_3D('',#118055,#90871,#90872) ;
#73236 = AXIS2_PLACEMENT_3D('',#118058,#90874,#90875) ;
#73237 = AXIS2_PLACEMENT_3D('',#118059,#90876,#90877) ;
#73238 = AXIS2_PLACEMENT_3D('',#118065,#90881,#90882) ;
#73239 = AXIS2_PLACEMENT_3D('',#118067,#90883,#90884) ;
#73240 = AXIS2_PLACEMENT_3D('',#118070,#90886,#90887) ;
#73241 = AXIS2_PLACEMENT_3D('',#118071,#90888,#90889) ;
#73242 = AXIS2_PLACEMENT_3D('',#118077,#90893,#90894) ;
#73243 = AXIS2_PLACEMENT_3D('',#118079,#90895,#90896) ;
#73244 = AXIS2_PLACEMENT_3D('',#118082,#90898,#90899) ;
#73245 = AXIS2_PLACEMENT_3D('',#118083,#90900,#90901) ;
#73246 = AXIS2_PLACEMENT_3D('',#118089,#90905,#90906) ;
#73247 = AXIS2_PLACEMENT_3D('',#118091,#90907,#90908) ;
#73248 = AXIS2_PLACEMENT_3D('',#118094,#90910,#90911) ;
#73249 = AXIS2_PLACEMENT_3D('',#118095,#90912,#90913) ;
#73250 = AXIS2_PLACEMENT_3D('',#118097,#90914,#90915) ;
#73251 = AXIS2_PLACEMENT_3D('',#118100,#90917,#90918) ;
#73252 = AXIS2_PLACEMENT_3D('',#118101,#90919,#90920) ;
#73253 = AXIS2_PLACEMENT_3D('',#118103,#90921,#90922) ;
#73254 = AXIS2_PLACEMENT_3D('',#118106,#90924,#90925) ;
#73255 = AXIS2_PLACEMENT_3D('',#118107,#90926,#90927) ;
#73256 = AXIS2_PLACEMENT_3D('',#118113,#90931,#90932) ;
#73257 = AXIS2_PLACEMENT_3D('',#118115,#90933,#90934) ;
#73258 = AXIS2_PLACEMENT_3D('',#118118,#90936,#90937) ;
#73259 = AXIS2_PLACEMENT_3D('',#118119,#90938,#90939) ;
#73260 = AXIS2_PLACEMENT_3D('',#118125,#90943,#90944) ;
#73261 = AXIS2_PLACEMENT_3D('',#118127,#90945,#90946) ;
#73262 = AXIS2_PLACEMENT_3D('',#118130,#90948,#90949) ;
#73263 = AXIS2_PLACEMENT_3D('',#118131,#90950,#90951) ;
#73264 = AXIS2_PLACEMENT_3D('',#118134,#90954,#90955) ;
#73265 = AXIS2_PLACEMENT_3D('',#118137,#90956,#90957) ;
#73266 = AXIS2_PLACEMENT_3D('',#118141,#90959,#90960) ;
#73267 = AXIS2_PLACEMENT_3D('',#118149,#90964,#90965) ;
#73268 = AXIS2_PLACEMENT_3D('',#118157,#90969,#90970) ;
#73269 = AXIS2_PLACEMENT_3D('',#118161,#90972,#90973) ;
#73270 = AXIS2_PLACEMENT_3D('',#118170,#90979,#90980) ;
#73271 = AXIS2_PLACEMENT_3D('',#118175,#90982,#90983) ;
#73272 = AXIS2_PLACEMENT_3D('',#118178,#90985,#90986) ;
#73273 = AXIS2_PLACEMENT_3D('',#118179,#90987,#90988) ;
#73274 = AXIS2_PLACEMENT_3D('',#118185,#90992,#90993) ;
#73275 = AXIS2_PLACEMENT_3D('',#118187,#90994,#90995) ;
#73276 = AXIS2_PLACEMENT_3D('',#118190,#90997,#90998) ;
#73277 = AXIS2_PLACEMENT_3D('',#118191,#90999,#91000) ;
#73278 = AXIS2_PLACEMENT_3D('',#118197,#91004,#91005) ;
#73279 = AXIS2_PLACEMENT_3D('',#118199,#91006,#91007) ;
#73280 = AXIS2_PLACEMENT_3D('',#118202,#91009,#91010) ;
#73281 = AXIS2_PLACEMENT_3D('',#118203,#91011,#91012) ;
#73282 = AXIS2_PLACEMENT_3D('',#118208,#91016,#91017) ;
#73283 = AXIS2_PLACEMENT_3D('',#118211,#91019,#91020) ;
#73284 = AXIS2_PLACEMENT_3D('',#118212,#91021,#91022) ;
#73285 = AXIS2_PLACEMENT_3D('',#118215,#91025,#91026) ;
#73286 = AXIS2_PLACEMENT_3D('',#118221,#91030,#91031) ;
#73287 = AXIS2_PLACEMENT_3D('',#118223,#91032,#91033) ;
#73288 = AXIS2_PLACEMENT_3D('',#118226,#91035,#91036) ;
#73289 = AXIS2_PLACEMENT_3D('',#118227,#91037,#91038) ;
#73290 = AXIS2_PLACEMENT_3D('',#118233,#91042,#91043) ;
#73291 = AXIS2_PLACEMENT_3D('',#118235,#91044,#91045) ;
#73292 = AXIS2_PLACEMENT_3D('',#118238,#91047,#91048) ;
#73293 = AXIS2_PLACEMENT_3D('',#118239,#91049,#91050) ;
#73294 = AXIS2_PLACEMENT_3D('',#118245,#91054,#91055) ;
#73295 = AXIS2_PLACEMENT_3D('',#118247,#91056,#91057) ;
#73296 = AXIS2_PLACEMENT_3D('',#118250,#91059,#91060) ;
#73297 = AXIS2_PLACEMENT_3D('',#118251,#91061,#91062) ;
#73298 = AXIS2_PLACEMENT_3D('',#118257,#91066,#91067) ;
#73299 = AXIS2_PLACEMENT_3D('',#118259,#91068,#91069) ;
#73300 = AXIS2_PLACEMENT_3D('',#118262,#91071,#91072) ;
#73301 = AXIS2_PLACEMENT_3D('',#118263,#91073,#91074) ;
#73302 = AXIS2_PLACEMENT_3D('',#118269,#91078,#91079) ;
#73303 = AXIS2_PLACEMENT_3D('',#118271,#91080,#91081) ;
#73304 = AXIS2_PLACEMENT_3D('',#118274,#91083,#91084) ;
#73305 = AXIS2_PLACEMENT_3D('',#118275,#91085,#91086) ;
#73306 = AXIS2_PLACEMENT_3D('',#118281,#91090,#91091) ;
#73307 = AXIS2_PLACEMENT_3D('',#118283,#91092,#91093) ;
#73308 = AXIS2_PLACEMENT_3D('',#118286,#91095,#91096) ;
#73309 = AXIS2_PLACEMENT_3D('',#118287,#91097,#91098) ;
#73310 = AXIS2_PLACEMENT_3D('',#118289,#91099,#91100) ;
#73311 = AXIS2_PLACEMENT_3D('',#118292,#91102,#91103) ;
#73312 = AXIS2_PLACEMENT_3D('',#118293,#91104,#91105) ;
#73313 = AXIS2_PLACEMENT_3D('',#118295,#91106,#91107) ;
#73314 = AXIS2_PLACEMENT_3D('',#118298,#91109,#91110) ;
#73315 = AXIS2_PLACEMENT_3D('',#118299,#91111,#91112) ;
#73316 = AXIS2_PLACEMENT_3D('',#118305,#91116,#91117) ;
#73317 = AXIS2_PLACEMENT_3D('',#118307,#91118,#91119) ;
#73318 = AXIS2_PLACEMENT_3D('',#118310,#91121,#91122) ;
#73319 = AXIS2_PLACEMENT_3D('',#118311,#91123,#91124) ;
#73320 = AXIS2_PLACEMENT_3D('',#118317,#91128,#91129) ;
#73321 = AXIS2_PLACEMENT_3D('',#118319,#91130,#91131) ;
#73322 = AXIS2_PLACEMENT_3D('',#118322,#91133,#91134) ;
#73323 = AXIS2_PLACEMENT_3D('',#118323,#91135,#91136) ;
#73324 = AXIS2_PLACEMENT_3D('',#118326,#91139,#91140) ;
#73325 = AXIS2_PLACEMENT_3D('',#118329,#91141,#91142) ;
#73326 = AXIS2_PLACEMENT_3D('',#118333,#91144,#91145) ;
#73327 = AXIS2_PLACEMENT_3D('',#118341,#91149,#91150) ;
#73328 = AXIS2_PLACEMENT_3D('',#118349,#91154,#91155) ;
#73329 = AXIS2_PLACEMENT_3D('',#118353,#91157,#91158) ;
#73330 = AXIS2_PLACEMENT_3D('',#118362,#91164,#91165) ;
#73331 = AXIS2_PLACEMENT_3D('',#118367,#91167,#91168) ;
#73332 = AXIS2_PLACEMENT_3D('',#118370,#91170,#91171) ;
#73333 = AXIS2_PLACEMENT_3D('',#118371,#91172,#91173) ;
#73334 = AXIS2_PLACEMENT_3D('',#118377,#91177,#91178) ;
#73335 = AXIS2_PLACEMENT_3D('',#118379,#91179,#91180) ;
#73336 = AXIS2_PLACEMENT_3D('',#118382,#91182,#91183) ;
#73337 = AXIS2_PLACEMENT_3D('',#118383,#91184,#91185) ;
#73338 = AXIS2_PLACEMENT_3D('',#118389,#91189,#91190) ;
#73339 = AXIS2_PLACEMENT_3D('',#118391,#91191,#91192) ;
#73340 = AXIS2_PLACEMENT_3D('',#118394,#91194,#91195) ;
#73341 = AXIS2_PLACEMENT_3D('',#118395,#91196,#91197) ;
#73342 = AXIS2_PLACEMENT_3D('',#118400,#91201,#91202) ;
#73343 = AXIS2_PLACEMENT_3D('',#118403,#91204,#91205) ;
#73344 = AXIS2_PLACEMENT_3D('',#118404,#91206,#91207) ;
#73345 = AXIS2_PLACEMENT_3D('',#118407,#91210,#91211) ;
#73346 = AXIS2_PLACEMENT_3D('',#118413,#91215,#91216) ;
#73347 = AXIS2_PLACEMENT_3D('',#118415,#91217,#91218) ;
#73348 = AXIS2_PLACEMENT_3D('',#118418,#91220,#91221) ;
#73349 = AXIS2_PLACEMENT_3D('',#118419,#91222,#91223) ;
#73350 = AXIS2_PLACEMENT_3D('',#118425,#91227,#91228) ;
#73351 = AXIS2_PLACEMENT_3D('',#118427,#91229,#91230) ;
#73352 = AXIS2_PLACEMENT_3D('',#118430,#91232,#91233) ;
#73353 = AXIS2_PLACEMENT_3D('',#118431,#91234,#91235) ;
#73354 = AXIS2_PLACEMENT_3D('',#118437,#91239,#91240) ;
#73355 = AXIS2_PLACEMENT_3D('',#118439,#91241,#91242) ;
#73356 = AXIS2_PLACEMENT_3D('',#118442,#91244,#91245) ;
#73357 = AXIS2_PLACEMENT_3D('',#118443,#91246,#91247) ;
#73358 = AXIS2_PLACEMENT_3D('',#118449,#91251,#91252) ;
#73359 = AXIS2_PLACEMENT_3D('',#118451,#91253,#91254) ;
#73360 = AXIS2_PLACEMENT_3D('',#118454,#91256,#91257) ;
#73361 = AXIS2_PLACEMENT_3D('',#118455,#91258,#91259) ;
#73362 = AXIS2_PLACEMENT_3D('',#118461,#91263,#91264) ;
#73363 = AXIS2_PLACEMENT_3D('',#118463,#91265,#91266) ;
#73364 = AXIS2_PLACEMENT_3D('',#118466,#91268,#91269) ;
#73365 = AXIS2_PLACEMENT_3D('',#118467,#91270,#91271) ;
#73366 = AXIS2_PLACEMENT_3D('',#118473,#91275,#91276) ;
#73367 = AXIS2_PLACEMENT_3D('',#118475,#91277,#91278) ;
#73368 = AXIS2_PLACEMENT_3D('',#118478,#91280,#91281) ;
#73369 = AXIS2_PLACEMENT_3D('',#118479,#91282,#91283) ;
#73370 = AXIS2_PLACEMENT_3D('',#118481,#91284,#91285) ;
#73371 = AXIS2_PLACEMENT_3D('',#118484,#91287,#91288) ;
#73372 = AXIS2_PLACEMENT_3D('',#118485,#91289,#91290) ;
#73373 = AXIS2_PLACEMENT_3D('',#118487,#91291,#91292) ;
#73374 = AXIS2_PLACEMENT_3D('',#118490,#91294,#91295) ;
#73375 = AXIS2_PLACEMENT_3D('',#118491,#91296,#91297) ;
#73376 = AXIS2_PLACEMENT_3D('',#118497,#91301,#91302) ;
#73377 = AXIS2_PLACEMENT_3D('',#118499,#91303,#91304) ;
#73378 = AXIS2_PLACEMENT_3D('',#118502,#91306,#91307) ;
#73379 = AXIS2_PLACEMENT_3D('',#118503,#91308,#91309) ;
#73380 = AXIS2_PLACEMENT_3D('',#118509,#91313,#91314) ;
#73381 = AXIS2_PLACEMENT_3D('',#118511,#91315,#91316) ;
#73382 = AXIS2_PLACEMENT_3D('',#118514,#91318,#91319) ;
#73383 = AXIS2_PLACEMENT_3D('',#118515,#91320,#91321) ;
#73384 = AXIS2_PLACEMENT_3D('',#118518,#91324,#91325) ;
#73385 = AXIS2_PLACEMENT_3D('',#118521,#91326,#91327) ;
#73386 = AXIS2_PLACEMENT_3D('',#118525,#91329,#91330) ;
#73387 = AXIS2_PLACEMENT_3D('',#118533,#91334,#91335) ;
#73388 = AXIS2_PLACEMENT_3D('',#118541,#91339,#91340) ;
#73389 = AXIS2_PLACEMENT_3D('',#118545,#91342,#91343) ;
#73390 = AXIS2_PLACEMENT_3D('',#118554,#91349,#91350) ;
#73391 = AXIS2_PLACEMENT_3D('',#118559,#91352,#91353) ;
#73392 = AXIS2_PLACEMENT_3D('',#118562,#91355,#91356) ;
#73393 = AXIS2_PLACEMENT_3D('',#118563,#91357,#91358) ;
#73394 = AXIS2_PLACEMENT_3D('',#118569,#91362,#91363) ;
#73395 = AXIS2_PLACEMENT_3D('',#118571,#91364,#91365) ;
#73396 = AXIS2_PLACEMENT_3D('',#118574,#91367,#91368) ;
#73397 = AXIS2_PLACEMENT_3D('',#118575,#91369,#91370) ;
#73398 = AXIS2_PLACEMENT_3D('',#118581,#91374,#91375) ;
#73399 = AXIS2_PLACEMENT_3D('',#118583,#91376,#91377) ;
#73400 = AXIS2_PLACEMENT_3D('',#118586,#91379,#91380) ;
#73401 = AXIS2_PLACEMENT_3D('',#118587,#91381,#91382) ;
#73402 = AXIS2_PLACEMENT_3D('',#118592,#91386,#91387) ;
#73403 = AXIS2_PLACEMENT_3D('',#118595,#91389,#91390) ;
#73404 = AXIS2_PLACEMENT_3D('',#118596,#91391,#91392) ;
#73405 = AXIS2_PLACEMENT_3D('',#118599,#91395,#91396) ;
#73406 = AXIS2_PLACEMENT_3D('',#118605,#91400,#91401) ;
#73407 = AXIS2_PLACEMENT_3D('',#118607,#91402,#91403) ;
#73408 = AXIS2_PLACEMENT_3D('',#118610,#91405,#91406) ;
#73409 = AXIS2_PLACEMENT_3D('',#118611,#91407,#91408) ;
#73410 = AXIS2_PLACEMENT_3D('',#118617,#91412,#91413) ;
#73411 = AXIS2_PLACEMENT_3D('',#118619,#91414,#91415) ;
#73412 = AXIS2_PLACEMENT_3D('',#118622,#91417,#91418) ;
#73413 = AXIS2_PLACEMENT_3D('',#118623,#91419,#91420) ;
#73414 = AXIS2_PLACEMENT_3D('',#118629,#91424,#91425) ;
#73415 = AXIS2_PLACEMENT_3D('',#118631,#91426,#91427) ;
#73416 = AXIS2_PLACEMENT_3D('',#118634,#91429,#91430) ;
#73417 = AXIS2_PLACEMENT_3D('',#118635,#91431,#91432) ;
#73418 = AXIS2_PLACEMENT_3D('',#118641,#91436,#91437) ;
#73419 = AXIS2_PLACEMENT_3D('',#118643,#91438,#91439) ;
#73420 = AXIS2_PLACEMENT_3D('',#118646,#91441,#91442) ;
#73421 = AXIS2_PLACEMENT_3D('',#118647,#91443,#91444) ;
#73422 = AXIS2_PLACEMENT_3D('',#118653,#91448,#91449) ;
#73423 = AXIS2_PLACEMENT_3D('',#118655,#91450,#91451) ;
#73424 = AXIS2_PLACEMENT_3D('',#118658,#91453,#91454) ;
#73425 = AXIS2_PLACEMENT_3D('',#118659,#91455,#91456) ;
#73426 = AXIS2_PLACEMENT_3D('',#118665,#91460,#91461) ;
#73427 = AXIS2_PLACEMENT_3D('',#118667,#91462,#91463) ;
#73428 = AXIS2_PLACEMENT_3D('',#118670,#91465,#91466) ;
#73429 = AXIS2_PLACEMENT_3D('',#118671,#91467,#91468) ;
#73430 = AXIS2_PLACEMENT_3D('',#118673,#91469,#91470) ;
#73431 = AXIS2_PLACEMENT_3D('',#118676,#91472,#91473) ;
#73432 = AXIS2_PLACEMENT_3D('',#118677,#91474,#91475) ;
#73433 = AXIS2_PLACEMENT_3D('',#118679,#91476,#91477) ;
#73434 = AXIS2_PLACEMENT_3D('',#118682,#91479,#91480) ;
#73435 = AXIS2_PLACEMENT_3D('',#118683,#91481,#91482) ;
#73436 = AXIS2_PLACEMENT_3D('',#118689,#91486,#91487) ;
#73437 = AXIS2_PLACEMENT_3D('',#118691,#91488,#91489) ;
#73438 = AXIS2_PLACEMENT_3D('',#118694,#91491,#91492) ;
#73439 = AXIS2_PLACEMENT_3D('',#118695,#91493,#91494) ;
#73440 = AXIS2_PLACEMENT_3D('',#118701,#91498,#91499) ;
#73441 = AXIS2_PLACEMENT_3D('',#118703,#91500,#91501) ;
#73442 = AXIS2_PLACEMENT_3D('',#118706,#91503,#91504) ;
#73443 = AXIS2_PLACEMENT_3D('',#118707,#91505,#91506) ;
#73444 = AXIS2_PLACEMENT_3D('',#118710,#91509,#91510) ;
#73445 = AXIS2_PLACEMENT_3D('',#118713,#91511,#91512) ;
#73446 = AXIS2_PLACEMENT_3D('',#118717,#91514,#91515) ;
#73447 = AXIS2_PLACEMENT_3D('',#118725,#91519,#91520) ;
#73448 = AXIS2_PLACEMENT_3D('',#118733,#91524,#91525) ;
#73449 = AXIS2_PLACEMENT_3D('',#118737,#91527,#91528) ;
#73450 = AXIS2_PLACEMENT_3D('',#118746,#91534,#91535) ;
#73451 = AXIS2_PLACEMENT_3D('',#118751,#91537,#91538) ;
#73452 = AXIS2_PLACEMENT_3D('',#118754,#91540,#91541) ;
#73453 = AXIS2_PLACEMENT_3D('',#118755,#91542,#91543) ;
#73454 = AXIS2_PLACEMENT_3D('',#118761,#91547,#91548) ;
#73455 = AXIS2_PLACEMENT_3D('',#118763,#91549,#91550) ;
#73456 = AXIS2_PLACEMENT_3D('',#118766,#91552,#91553) ;
#73457 = AXIS2_PLACEMENT_3D('',#118767,#91554,#91555) ;
#73458 = AXIS2_PLACEMENT_3D('',#118773,#91559,#91560) ;
#73459 = AXIS2_PLACEMENT_3D('',#118775,#91561,#91562) ;
#73460 = AXIS2_PLACEMENT_3D('',#118778,#91564,#91565) ;
#73461 = AXIS2_PLACEMENT_3D('',#118779,#91566,#91567) ;
#73462 = AXIS2_PLACEMENT_3D('',#118784,#91571,#91572) ;
#73463 = AXIS2_PLACEMENT_3D('',#118787,#91574,#91575) ;
#73464 = AXIS2_PLACEMENT_3D('',#118788,#91576,#91577) ;
#73465 = AXIS2_PLACEMENT_3D('',#118791,#91580,#91581) ;
#73466 = AXIS2_PLACEMENT_3D('',#118797,#91585,#91586) ;
#73467 = AXIS2_PLACEMENT_3D('',#118799,#91587,#91588) ;
#73468 = AXIS2_PLACEMENT_3D('',#118802,#91590,#91591) ;
#73469 = AXIS2_PLACEMENT_3D('',#118803,#91592,#91593) ;
#73470 = AXIS2_PLACEMENT_3D('',#118809,#91597,#91598) ;
#73471 = AXIS2_PLACEMENT_3D('',#118811,#91599,#91600) ;
#73472 = AXIS2_PLACEMENT_3D('',#118814,#91602,#91603) ;
#73473 = AXIS2_PLACEMENT_3D('',#118815,#91604,#91605) ;
#73474 = AXIS2_PLACEMENT_3D('',#118821,#91609,#91610) ;
#73475 = AXIS2_PLACEMENT_3D('',#118823,#91611,#91612) ;
#73476 = AXIS2_PLACEMENT_3D('',#118826,#91614,#91615) ;
#73477 = AXIS2_PLACEMENT_3D('',#118827,#91616,#91617) ;
#73478 = AXIS2_PLACEMENT_3D('',#118833,#91621,#91622) ;
#73479 = AXIS2_PLACEMENT_3D('',#118835,#91623,#91624) ;
#73480 = AXIS2_PLACEMENT_3D('',#118838,#91626,#91627) ;
#73481 = AXIS2_PLACEMENT_3D('',#118839,#91628,#91629) ;
#73482 = AXIS2_PLACEMENT_3D('',#118845,#91633,#91634) ;
#73483 = AXIS2_PLACEMENT_3D('',#118847,#91635,#91636) ;
#73484 = AXIS2_PLACEMENT_3D('',#118850,#91638,#91639) ;
#73485 = AXIS2_PLACEMENT_3D('',#118851,#91640,#91641) ;
#73486 = AXIS2_PLACEMENT_3D('',#118857,#91645,#91646) ;
#73487 = AXIS2_PLACEMENT_3D('',#118859,#91647,#91648) ;
#73488 = AXIS2_PLACEMENT_3D('',#118862,#91650,#91651) ;
#73489 = AXIS2_PLACEMENT_3D('',#118863,#91652,#91653) ;
#73490 = AXIS2_PLACEMENT_3D('',#118865,#91654,#91655) ;
#73491 = AXIS2_PLACEMENT_3D('',#118868,#91657,#91658) ;
#73492 = AXIS2_PLACEMENT_3D('',#118869,#91659,#91660) ;
#73493 = AXIS2_PLACEMENT_3D('',#118871,#91661,#91662) ;
#73494 = AXIS2_PLACEMENT_3D('',#118874,#91664,#91665) ;
#73495 = AXIS2_PLACEMENT_3D('',#118875,#91666,#91667) ;
#73496 = AXIS2_PLACEMENT_3D('',#118881,#91671,#91672) ;
#73497 = AXIS2_PLACEMENT_3D('',#118883,#91673,#91674) ;
#73498 = AXIS2_PLACEMENT_3D('',#118886,#91676,#91677) ;
#73499 = AXIS2_PLACEMENT_3D('',#118887,#91678,#91679) ;
#73500 = AXIS2_PLACEMENT_3D('',#118893,#91683,#91684) ;
#73501 = AXIS2_PLACEMENT_3D('',#118895,#91685,#91686) ;
#73502 = AXIS2_PLACEMENT_3D('',#118898,#91688,#91689) ;
#73503 = AXIS2_PLACEMENT_3D('',#118899,#91690,#91691) ;
#73504 = AXIS2_PLACEMENT_3D('',#118902,#91694,#91695) ;
#73505 = AXIS2_PLACEMENT_3D('',#118905,#91696,#91697) ;
#73506 = AXIS2_PLACEMENT_3D('',#118909,#91699,#91700) ;
#73507 = AXIS2_PLACEMENT_3D('',#118917,#91704,#91705) ;
#73508 = AXIS2_PLACEMENT_3D('',#118925,#91709,#91710) ;
#73509 = AXIS2_PLACEMENT_3D('',#118929,#91712,#91713) ;
#73510 = AXIS2_PLACEMENT_3D('',#118938,#91719,#91720) ;
#73511 = AXIS2_PLACEMENT_3D('',#118943,#91722,#91723) ;
#73512 = AXIS2_PLACEMENT_3D('',#118947,#91725,#91726) ;
#73513 = AXIS2_PLACEMENT_3D('',#118951,#91728,#91729) ;
#73514 = AXIS2_PLACEMENT_3D('',#118954,#91731,#91732) ;
#73515 = AXIS2_PLACEMENT_3D('',#118955,#91733,#91734) ;
#73516 = AXIS2_PLACEMENT_3D('',#118960,#91736,#91737) ;
#73517 = AXIS2_PLACEMENT_3D('',#118964,#91739,#91740) ;
#73518 = AXIS2_PLACEMENT_3D('',#118968,#91742,#91743) ;
#73519 = AXIS2_PLACEMENT_3D('',#118971,#91745,#91746) ;
#73520 = AXIS2_PLACEMENT_3D('',#118972,#91747,#91748) ;
#73521 = AXIS2_PLACEMENT_3D('',#118977,#91750,#91751) ;
#73522 = AXIS2_PLACEMENT_3D('',#118981,#91753,#91754) ;
#73523 = AXIS2_PLACEMENT_3D('',#118985,#91756,#91757) ;
#73524 = AXIS2_PLACEMENT_3D('',#118988,#91759,#91760) ;
#73525 = AXIS2_PLACEMENT_3D('',#118989,#91761,#91762) ;
#73526 = AXIS2_PLACEMENT_3D('',#118994,#91764,#91765) ;
#73527 = AXIS2_PLACEMENT_3D('',#118998,#91767,#91768) ;
#73528 = AXIS2_PLACEMENT_3D('',#119002,#91770,#91771) ;
#73529 = AXIS2_PLACEMENT_3D('',#119005,#91773,#91774) ;
#73530 = AXIS2_PLACEMENT_3D('',#119006,#91775,#91776) ;
#73531 = AXIS2_PLACEMENT_3D('',#119011,#91778,#91779) ;
#73532 = AXIS2_PLACEMENT_3D('',#119015,#91781,#91782) ;
#73533 = AXIS2_PLACEMENT_3D('',#119019,#91784,#91785) ;
#73534 = AXIS2_PLACEMENT_3D('',#119022,#91787,#91788) ;
#73535 = AXIS2_PLACEMENT_3D('',#119023,#91789,#91790) ;
#73536 = AXIS2_PLACEMENT_3D('',#119028,#91792,#91793) ;
#73537 = AXIS2_PLACEMENT_3D('',#119032,#91795,#91796) ;
#73538 = AXIS2_PLACEMENT_3D('',#119036,#91798,#91799) ;
#73539 = AXIS2_PLACEMENT_3D('',#119039,#91801,#91802) ;
#73540 = AXIS2_PLACEMENT_3D('',#119040,#91803,#91804) ;
#73541 = AXIS2_PLACEMENT_3D('',#119045,#91806,#91807) ;
#73542 = AXIS2_PLACEMENT_3D('',#119049,#91809,#91810) ;
#73543 = AXIS2_PLACEMENT_3D('',#119053,#91812,#91813) ;
#73544 = AXIS2_PLACEMENT_3D('',#119056,#91815,#91816) ;
#73545 = AXIS2_PLACEMENT_3D('',#119057,#91817,#91818) ;
#73546 = AXIS2_PLACEMENT_3D('',#119062,#91820,#91821) ;
#73547 = AXIS2_PLACEMENT_3D('',#119066,#91823,#91824) ;
#73548 = AXIS2_PLACEMENT_3D('',#119070,#91826,#91827) ;
#73549 = AXIS2_PLACEMENT_3D('',#119073,#91829,#91830) ;
#73550 = AXIS2_PLACEMENT_3D('',#119074,#91831,#91832) ;
#73551 = AXIS2_PLACEMENT_3D('',#119079,#91834,#91835) ;
#73552 = AXIS2_PLACEMENT_3D('',#119083,#91837,#91838) ;
#73553 = AXIS2_PLACEMENT_3D('',#119087,#91840,#91841) ;
#73554 = AXIS2_PLACEMENT_3D('',#119090,#91843,#91844) ;
#73555 = AXIS2_PLACEMENT_3D('',#119091,#91845,#91846) ;
#73556 = AXIS2_PLACEMENT_3D('',#119092,#91847,#91848) ;
#73557 = AXIS2_PLACEMENT_3D('',#119093,#91849,#91850) ;
#73558 = AXIS2_PLACEMENT_3D('',#119094,#91851,#91852) ;
#73559 = AXIS2_PLACEMENT_3D('',#119095,#91853,#91854) ;
#73560 = AXIS2_PLACEMENT_3D('',#119096,#91855,#91856) ;
#73561 = AXIS2_PLACEMENT_3D('',#119097,#91857,#91858) ;
#73562 = AXIS2_PLACEMENT_3D('',#119099,#91859,#91860) ;
#73563 = AXIS2_PLACEMENT_3D('',#119100,#91861,#91862) ;
#73564 = AXIS2_PLACEMENT_3D('',#119101,#91863,#91864) ;
#73565 = AXIS2_PLACEMENT_3D('',#119102,#91865,#91866) ;
#73566 = AXIS2_PLACEMENT_3D('',#119103,#91867,#91868) ;
#73567 = AXIS2_PLACEMENT_3D('',#119104,#91869,#91870) ;
#73568 = AXIS2_PLACEMENT_3D('',#119105,#91871,#91872) ;
#73569 = AXIS2_PLACEMENT_3D('',#119106,#91873,#91874) ;
#73570 = AXIS2_PLACEMENT_3D('',#119107,#91875,#91876) ;
#73571 = AXIS2_PLACEMENT_3D('',#119118,#91878,#91879) ;
#73572 = AXIS2_PLACEMENT_3D('',#119175,#91881,#91882) ;
#73573 = AXIS2_PLACEMENT_3D('',#119176,#91883,#91884) ;
#73574 = AXIS2_PLACEMENT_3D('',#119177,#91885,#91886) ;
#73575 = AXIS2_PLACEMENT_3D('',#119178,#91887,#91888) ;
#73576 = AXIS2_PLACEMENT_3D('',#119179,#91889,#91890) ;
#73577 = AXIS2_PLACEMENT_3D('',#119180,#91891,#91892) ;
#73578 = AXIS2_PLACEMENT_3D('',#119181,#91893,#91894) ;
#73579 = AXIS2_PLACEMENT_3D('',#119182,#91895,#91896) ;
#73580 = AXIS2_PLACEMENT_3D('',#119183,#91897,#91898) ;
#73581 = AXIS2_PLACEMENT_3D('',#119184,#91899,#91900) ;
#73582 = AXIS2_PLACEMENT_3D('',#119185,#91901,#91902) ;
#73583 = AXIS2_PLACEMENT_3D('',#119186,#91903,#91904) ;
#73584 = AXIS2_PLACEMENT_3D('',#119187,#91905,#91906) ;
#73585 = AXIS2_PLACEMENT_3D('',#119188,#91907,#91908) ;
#73586 = AXIS2_PLACEMENT_3D('',#119189,#91909,#91910) ;
#73587 = AXIS2_PLACEMENT_3D('',#119190,#91911,#91912) ;
#73588 = AXIS2_PLACEMENT_3D('',#119191,#91913,#91914) ;
#73589 = AXIS2_PLACEMENT_3D('',#119192,#91915,#91916) ;
#73590 = AXIS2_PLACEMENT_3D('',#119193,#91917,#91918) ;
#73591 = AXIS2_PLACEMENT_3D('',#119194,#91919,#91920) ;
#73592 = AXIS2_PLACEMENT_3D('',#119195,#91921,#91922) ;
#73593 = AXIS2_PLACEMENT_3D('',#119196,#91923,#91924) ;
#73594 = AXIS2_PLACEMENT_3D('',#119197,#91925,#91926) ;
#73595 = AXIS2_PLACEMENT_3D('',#119200,#91928,#91929) ;
#73596 = AXIS2_PLACEMENT_3D('',#119201,#91930,#91931) ;
#73597 = AXIS2_PLACEMENT_3D('',#119202,#91932,#91933) ;
#73598 = AXIS2_PLACEMENT_3D('',#119203,#91934,#91935) ;
#73599 = AXIS2_PLACEMENT_3D('',#119204,#91936,#91937) ;
#73600 = AXIS2_PLACEMENT_3D('',#119205,#91938,#91939) ;
#73601 = AXIS2_PLACEMENT_3D('',#119206,#91940,#91941) ;
#73602 = AXIS2_PLACEMENT_3D('',#119207,#91942,#91943) ;
#73603 = AXIS2_PLACEMENT_3D('',#119208,#91944,#91945) ;
#73604 = AXIS2_PLACEMENT_3D('',#119209,#91946,#91947) ;
#73605 = AXIS2_PLACEMENT_3D('',#119210,#91948,#91949) ;
#73606 = AXIS2_PLACEMENT_3D('',#119211,#91950,#91951) ;
#73607 = AXIS2_PLACEMENT_3D('',#119212,#91952,#91953) ;
#73608 = AXIS2_PLACEMENT_3D('',#119213,#91954,#91955) ;
#73609 = AXIS2_PLACEMENT_3D('',#119214,#91956,#91957) ;
#73610 = AXIS2_PLACEMENT_3D('',#119215,#91958,#91959) ;
#73611 = AXIS2_PLACEMENT_3D('',#119217,#91960,#91961) ;
#73612 = AXIS2_PLACEMENT_3D('',#119218,#91962,#91963) ;
#73613 = AXIS2_PLACEMENT_3D('',#119219,#91964,#91965) ;
#73614 = AXIS2_PLACEMENT_3D('',#119220,#91966,#91967) ;
#73615 = AXIS2_PLACEMENT_3D('',#119221,#91968,#91969) ;
#73616 = AXIS2_PLACEMENT_3D('',#119222,#91970,#91971) ;
#73617 = AXIS2_PLACEMENT_3D('',#119223,#91972,#91973) ;
#73618 = AXIS2_PLACEMENT_3D('',#119224,#91974,#91975) ;
#73619 = AXIS2_PLACEMENT_3D('',#119225,#91976,#91977) ;
#73620 = AXIS2_PLACEMENT_3D('',#119226,#91978,#91979) ;
#73621 = AXIS2_PLACEMENT_3D('',#119227,#91980,#91981) ;
#73622 = AXIS2_PLACEMENT_3D('',#119228,#91982,#91983) ;
#73623 = AXIS2_PLACEMENT_3D('',#119229,#91984,#91985) ;
#73624 = AXIS2_PLACEMENT_3D('',#119232,#91987,#91988) ;
#73625 = AXIS2_PLACEMENT_3D('',#119233,#91989,#91990) ;
#73626 = AXIS2_PLACEMENT_3D('',#119234,#91991,#91992) ;
#73627 = AXIS2_PLACEMENT_3D('',#119235,#91993,#91994) ;
#73628 = AXIS2_PLACEMENT_3D('',#119236,#91995,#91996) ;
#73629 = AXIS2_PLACEMENT_3D('',#119237,#91997,#91998) ;
#73630 = AXIS2_PLACEMENT_3D('',#119238,#91999,#92000) ;
#73631 = AXIS2_PLACEMENT_3D('',#119239,#92001,#92002) ;
#73632 = AXIS2_PLACEMENT_3D('',#119240,#92003,#92004) ;
#73633 = AXIS2_PLACEMENT_3D('',#119241,#92005,#92006) ;
#73634 = AXIS2_PLACEMENT_3D('',#119242,#92007,#92008) ;
#73635 = AXIS2_PLACEMENT_3D('',#119243,#92009,#92010) ;
#73636 = AXIS2_PLACEMENT_3D('',#119244,#92011,#92012) ;
#73637 = AXIS2_PLACEMENT_3D('',#119246,#92013,#92014) ;
#73638 = AXIS2_PLACEMENT_3D('',#119247,#92015,#92016) ;
#73639 = AXIS2_PLACEMENT_3D('',#119248,#92017,#92018) ;
#73640 = AXIS2_PLACEMENT_3D('',#119249,#92019,#92020) ;
#73641 = AXIS2_PLACEMENT_3D('',#119250,#92021,#92022) ;
#73642 = AXIS2_PLACEMENT_3D('',#119251,#92023,#92024) ;
#73643 = AXIS2_PLACEMENT_3D('',#119252,#92025,#92026) ;
#73644 = AXIS2_PLACEMENT_3D('',#119253,#92027,#92028) ;
#73645 = AXIS2_PLACEMENT_3D('',#119254,#92029,#92030) ;
#73646 = AXIS2_PLACEMENT_3D('',#119255,#92031,#92032) ;
#73647 = AXIS2_PLACEMENT_3D('',#119256,#92033,#92034) ;
#73648 = AXIS2_PLACEMENT_3D('',#119258,#92036,#92037) ;
#73649 = AXIS2_PLACEMENT_3D('',#119259,#92038,#92039) ;
#73650 = AXIS2_PLACEMENT_3D('',#119260,#92040,#92041) ;
#73651 = AXIS2_PLACEMENT_3D('',#119261,#92042,#92043) ;
#73652 = AXIS2_PLACEMENT_3D('',#119262,#92044,#92045) ;
#73653 = AXIS2_PLACEMENT_3D('',#119263,#92046,#92047) ;
#73654 = AXIS2_PLACEMENT_3D('',#119264,#92048,#92049) ;
#73655 = AXIS2_PLACEMENT_3D('',#119265,#92050,#92051) ;
#73656 = AXIS2_PLACEMENT_3D('',#119266,#92052,#92053) ;
#73657 = AXIS2_PLACEMENT_3D('',#119267,#92054,#92055) ;
#73658 = AXIS2_PLACEMENT_3D('',#119268,#92056,#92057) ;
#73659 = AXIS2_PLACEMENT_3D('',#119269,#92058,#92059) ;
#73660 = AXIS2_PLACEMENT_3D('',#119270,#92060,#92061) ;
#73661 = AXIS2_PLACEMENT_3D('',#119271,#92062,#92063) ;
#73662 = AXIS2_PLACEMENT_3D('',#119272,#92064,#92065) ;
#73663 = AXIS2_PLACEMENT_3D('',#119273,#92066,#92067) ;
#73664 = AXIS2_PLACEMENT_3D('',#119274,#92068,#92069) ;
#73665 = AXIS2_PLACEMENT_3D('',#119275,#92070,#92071) ;
#73666 = AXIS2_PLACEMENT_3D('',#119276,#92072,#92073) ;
#73667 = AXIS2_PLACEMENT_3D('',#119277,#92074,#92075) ;
#73668 = AXIS2_PLACEMENT_3D('',#119278,#92076,#92077) ;
#73669 = AXIS2_PLACEMENT_3D('',#119279,#92078,#92079) ;
#73670 = AXIS2_PLACEMENT_3D('',#119280,#92080,#92081) ;
#73671 = AXIS2_PLACEMENT_3D('',#119281,#92082,#92083) ;
#73672 = AXIS2_PLACEMENT_3D('',#119282,#92084,#92085) ;
#73673 = AXIS2_PLACEMENT_3D('',#119283,#92086,#92087) ;
#73674 = AXIS2_PLACEMENT_3D('',#119284,#92088,#92089) ;
#73675 = AXIS2_PLACEMENT_3D('',#119285,#92090,#92091) ;
#73676 = AXIS2_PLACEMENT_3D('',#119286,#92092,#92093) ;
#73677 = AXIS2_PLACEMENT_3D('',#119287,#92094,#92095) ;
#73678 = AXIS2_PLACEMENT_3D('',#119288,#92096,#92097) ;
#73679 = AXIS2_PLACEMENT_3D('',#119289,#92098,#92099) ;
#73680 = AXIS2_PLACEMENT_3D('',#119290,#92100,#92101) ;
#73681 = AXIS2_PLACEMENT_3D('',#119291,#92102,#92103) ;
#73682 = AXIS2_PLACEMENT_3D('',#119292,#92104,#92105) ;
#73683 = AXIS2_PLACEMENT_3D('',#119293,#92106,#92107) ;
#73684 = AXIS2_PLACEMENT_3D('',#119294,#92108,#92109) ;
#73685 = AXIS2_PLACEMENT_3D('',#119295,#92110,#92111) ;
#73686 = AXIS2_PLACEMENT_3D('',#119296,#92112,#92113) ;
#73687 = AXIS2_PLACEMENT_3D('',#119297,#92114,#92115) ;
#73688 = AXIS2_PLACEMENT_3D('',#119298,#92116,#92117) ;
#73689 = AXIS2_PLACEMENT_3D('',#119299,#92118,#92119) ;
#73690 = AXIS2_PLACEMENT_3D('',#119300,#92120,#92121) ;
#73691 = AXIS2_PLACEMENT_3D('',#119301,#92122,#92123) ;
#73692 = AXIS2_PLACEMENT_3D('',#119302,#92124,#92125) ;
#73693 = AXIS2_PLACEMENT_3D('',#119303,#92126,#92127) ;
#73694 = AXIS2_PLACEMENT_3D('',#119304,#92128,#92129) ;
#73695 = AXIS2_PLACEMENT_3D('',#119305,#92130,#92131) ;
#73696 = AXIS2_PLACEMENT_3D('',#119306,#92132,#92133) ;
#73697 = AXIS2_PLACEMENT_3D('',#119307,#92134,#92135) ;
#73698 = AXIS2_PLACEMENT_3D('',#119308,#92136,#92137) ;
#73699 = AXIS2_PLACEMENT_3D('',#119309,#92138,#92139) ;
#73700 = AXIS2_PLACEMENT_3D('',#119310,#92140,#92141) ;
#73701 = AXIS2_PLACEMENT_3D('',#119311,#92142,#92143) ;
#73702 = AXIS2_PLACEMENT_3D('',#119312,#92144,#92145) ;
#73703 = AXIS2_PLACEMENT_3D('',#119313,#92146,#92147) ;
#73704 = AXIS2_PLACEMENT_3D('',#119314,#92148,#92149) ;
#73705 = AXIS2_PLACEMENT_3D('',#119315,#92150,#92151) ;
#73706 = AXIS2_PLACEMENT_3D('',#119316,#92152,#92153) ;
#73707 = AXIS2_PLACEMENT_3D('',#119317,#92154,#92155) ;
#73708 = AXIS2_PLACEMENT_3D('',#119318,#92156,#92157) ;
#73709 = AXIS2_PLACEMENT_3D('',#119319,#92158,#92159) ;
#73710 = AXIS2_PLACEMENT_3D('',#119320,#92160,#92161) ;
#73711 = AXIS2_PLACEMENT_3D('',#119321,#92162,#92163) ;
#73712 = AXIS2_PLACEMENT_3D('',#119322,#92164,#92165) ;
#73713 = AXIS2_PLACEMENT_3D('',#119323,#92166,#92167) ;
#73714 = AXIS2_PLACEMENT_3D('',#119324,#92168,#92169) ;
#73715 = AXIS2_PLACEMENT_3D('',#119325,#92170,#92171) ;
#73716 = AXIS2_PLACEMENT_3D('',#119326,#92172,#92173) ;
#73717 = AXIS2_PLACEMENT_3D('',#119327,#92174,#92175) ;
#73718 = AXIS2_PLACEMENT_3D('',#119328,#92176,#92177) ;
#73719 = AXIS2_PLACEMENT_3D('',#119329,#92178,#92179) ;
#73720 = AXIS2_PLACEMENT_3D('',#119330,#92180,#92181) ;
#73721 = AXIS2_PLACEMENT_3D('',#119331,#92182,#92183) ;
#73722 = AXIS2_PLACEMENT_3D('',#119332,#92184,#92185) ;
#73723 = AXIS2_PLACEMENT_3D('',#119333,#92186,#92187) ;
#73724 = AXIS2_PLACEMENT_3D('',#119334,#92188,#92189) ;
#73725 = AXIS2_PLACEMENT_3D('',#119335,#92190,#92191) ;
#73726 = AXIS2_PLACEMENT_3D('',#119336,#92192,#92193) ;
#73727 = AXIS2_PLACEMENT_3D('',#119337,#92194,#92195) ;
#73728 = AXIS2_PLACEMENT_3D('',#119338,#92196,#92197) ;
#73729 = AXIS2_PLACEMENT_3D('',#119339,#92198,#92199) ;
#73730 = AXIS2_PLACEMENT_3D('',#119340,#92200,#92201) ;
#73731 = AXIS2_PLACEMENT_3D('',#119341,#92202,#92203) ;
#73732 = AXIS2_PLACEMENT_3D('',#119342,#92204,#92205) ;
#73733 = AXIS2_PLACEMENT_3D('',#119343,#92206,#92207) ;
#73734 = AXIS2_PLACEMENT_3D('',#119344,#92208,#92209) ;
#73735 = AXIS2_PLACEMENT_3D('',#119345,#92210,#92211) ;
#73736 = AXIS2_PLACEMENT_3D('',#119346,#92212,#92213) ;
#73737 = AXIS2_PLACEMENT_3D('',#119347,#92214,#92215) ;
#73738 = AXIS2_PLACEMENT_3D('',#119348,#92216,#92217) ;
#73739 = AXIS2_PLACEMENT_3D('',#119349,#92218,#92219) ;
#73740 = AXIS2_PLACEMENT_3D('',#119350,#92220,#92221) ;
#73741 = AXIS2_PLACEMENT_3D('',#119351,#92222,#92223) ;
#73742 = AXIS2_PLACEMENT_3D('',#119352,#92224,#92225) ;
#73743 = AXIS2_PLACEMENT_3D('',#119353,#92226,#92227) ;
#73744 = AXIS2_PLACEMENT_3D('',#119354,#92228,#92229) ;
#73745 = AXIS2_PLACEMENT_3D('',#119355,#92230,#92231) ;
#73746 = AXIS2_PLACEMENT_3D('',#119356,#92232,#92233) ;
#73747 = AXIS2_PLACEMENT_3D('',#119357,#92234,#92235) ;
#73748 = AXIS2_PLACEMENT_3D('',#119358,#92236,#92237) ;
#73749 = AXIS2_PLACEMENT_3D('',#119359,#92238,#92239) ;
#73750 = AXIS2_PLACEMENT_3D('',#119360,#92240,#92241) ;
#73751 = AXIS2_PLACEMENT_3D('',#119361,#92242,#92243) ;
#73752 = AXIS2_PLACEMENT_3D('',#119362,#92244,#92245) ;
#73753 = AXIS2_PLACEMENT_3D('',#119363,#92246,#92247) ;
#73754 = AXIS2_PLACEMENT_3D('',#119364,#92248,#92249) ;
#73755 = AXIS2_PLACEMENT_3D('',#119365,#92250,#92251) ;
#73756 = AXIS2_PLACEMENT_3D('',#119366,#92252,#92253) ;
#73757 = AXIS2_PLACEMENT_3D('',#119367,#92254,#92255) ;
#73758 = AXIS2_PLACEMENT_3D('',#119368,#92256,#92257) ;
#73759 = AXIS2_PLACEMENT_3D('',#119369,#92258,#92259) ;
#73760 = AXIS2_PLACEMENT_3D('',#119370,#92260,#92261) ;
#73761 = AXIS2_PLACEMENT_3D('',#119371,#92262,#92263) ;
#73762 = AXIS2_PLACEMENT_3D('',#119372,#92264,#92265) ;
#73763 = AXIS2_PLACEMENT_3D('',#119373,#92266,#92267) ;
#73764 = AXIS2_PLACEMENT_3D('',#119374,#92268,#92269) ;
#73765 = AXIS2_PLACEMENT_3D('',#119375,#92270,#92271) ;
#73766 = AXIS2_PLACEMENT_3D('',#119376,#92272,#92273) ;
#73767 = AXIS2_PLACEMENT_3D('',#119377,#92274,#92275) ;
#73768 = AXIS2_PLACEMENT_3D('',#119378,#92276,#92277) ;
#73769 = AXIS2_PLACEMENT_3D('',#119379,#92278,#92279) ;
#73770 = AXIS2_PLACEMENT_3D('',#119380,#92280,#92281) ;
#73771 = AXIS2_PLACEMENT_3D('',#119381,#92282,#92283) ;
#73772 = AXIS2_PLACEMENT_3D('',#119382,#92284,#92285) ;
#73773 = AXIS2_PLACEMENT_3D('',#119383,#92286,#92287) ;
#73774 = AXIS2_PLACEMENT_3D('',#119384,#92288,#92289) ;
#73775 = AXIS2_PLACEMENT_3D('',#119385,#92290,#92291) ;
#73776 = AXIS2_PLACEMENT_3D('',#119386,#92292,#92293) ;
#73777 = AXIS2_PLACEMENT_3D('',#119387,#92294,#92295) ;
#73778 = AXIS2_PLACEMENT_3D('',#119388,#92296,#92297) ;
#73779 = AXIS2_PLACEMENT_3D('',#119389,#92298,#92299) ;
#73780 = AXIS2_PLACEMENT_3D('',#119390,#92300,#92301) ;
#73781 = AXIS2_PLACEMENT_3D('',#119391,#92302,#92303) ;
#73782 = AXIS2_PLACEMENT_3D('',#119392,#92304,#92305) ;
#73783 = AXIS2_PLACEMENT_3D('',#119393,#92306,#92307) ;
#73784 = AXIS2_PLACEMENT_3D('',#119394,#92308,#92309) ;
#73785 = AXIS2_PLACEMENT_3D('',#119395,#92310,#92311) ;
#73786 = AXIS2_PLACEMENT_3D('',#119396,#92312,#92313) ;
#73787 = AXIS2_PLACEMENT_3D('',#119397,#92314,#92315) ;
#73788 = AXIS2_PLACEMENT_3D('',#119398,#92316,#92317) ;
#73789 = AXIS2_PLACEMENT_3D('',#119399,#92318,#92319) ;
#73790 = AXIS2_PLACEMENT_3D('',#119400,#92320,#92321) ;
#73791 = AXIS2_PLACEMENT_3D('',#119401,#92322,#92323) ;
#73792 = AXIS2_PLACEMENT_3D('',#119402,#92324,#92325) ;
#73793 = AXIS2_PLACEMENT_3D('',#119403,#92326,#92327) ;
#73794 = AXIS2_PLACEMENT_3D('',#119404,#92328,#92329) ;
#73795 = AXIS2_PLACEMENT_3D('',#119405,#92330,#92331) ;
#73796 = AXIS2_PLACEMENT_3D('',#119406,#92332,#92333) ;
#73797 = AXIS2_PLACEMENT_3D('',#119407,#92334,#92335) ;
#73798 = AXIS2_PLACEMENT_3D('',#119408,#92336,#92337) ;
#73799 = AXIS2_PLACEMENT_3D('',#119409,#92338,#92339) ;
#73800 = AXIS2_PLACEMENT_3D('',#119410,#92340,#92341) ;
#73801 = AXIS2_PLACEMENT_3D('',#119411,#92342,#92343) ;
#73802 = AXIS2_PLACEMENT_3D('',#119412,#92344,#92345) ;
#73803 = AXIS2_PLACEMENT_3D('',#119413,#92346,#92347) ;
#73804 = AXIS2_PLACEMENT_3D('',#119414,#92348,#92349) ;
#73805 = AXIS2_PLACEMENT_3D('',#119415,#92350,#92351) ;
#73806 = AXIS2_PLACEMENT_3D('',#119416,#92352,#92353) ;
#73807 = AXIS2_PLACEMENT_3D('',#119417,#92354,#92355) ;
#73808 = AXIS2_PLACEMENT_3D('',#119418,#92356,#92357) ;
#73809 = AXIS2_PLACEMENT_3D('',#119419,#92358,#92359) ;
#73810 = AXIS2_PLACEMENT_3D('',#119420,#92360,#92361) ;
#73811 = AXIS2_PLACEMENT_3D('',#119421,#92362,#92363) ;
#73812 = AXIS2_PLACEMENT_3D('',#119422,#92364,#92365) ;
#73813 = AXIS2_PLACEMENT_3D('',#119423,#92366,#92367) ;
#73814 = AXIS2_PLACEMENT_3D('',#119424,#92368,#92369) ;
#73815 = AXIS2_PLACEMENT_3D('',#119425,#92370,#92371) ;
#73816 = AXIS2_PLACEMENT_3D('',#119426,#92372,#92373) ;
#73817 = AXIS2_PLACEMENT_3D('',#119427,#92374,#92375) ;
#73818 = AXIS2_PLACEMENT_3D('',#119428,#92376,#92377) ;
#73819 = AXIS2_PLACEMENT_3D('',#119429,#92378,#92379) ;
#73820 = AXIS2_PLACEMENT_3D('',#119430,#92380,#92381) ;
#73821 = AXIS2_PLACEMENT_3D('',#119431,#92382,#92383) ;
#73822 = AXIS2_PLACEMENT_3D('',#119432,#92384,#92385) ;
#73823 = AXIS2_PLACEMENT_3D('',#119433,#92386,#92387) ;
#73824 = AXIS2_PLACEMENT_3D('',#119434,#92388,#92389) ;
#73825 = AXIS2_PLACEMENT_3D('',#119435,#92390,#92391) ;
#73826 = AXIS2_PLACEMENT_3D('',#119436,#92392,#92393) ;
#73827 = AXIS2_PLACEMENT_3D('',#119437,#92394,#92395) ;
#73828 = AXIS2_PLACEMENT_3D('',#119438,#92396,#92397) ;
#73829 = AXIS2_PLACEMENT_3D('',#119439,#92398,#92399) ;
#73830 = AXIS2_PLACEMENT_3D('',#119440,#92400,#92401) ;
#73831 = AXIS2_PLACEMENT_3D('',#119441,#92402,#92403) ;
#73832 = AXIS2_PLACEMENT_3D('',#119442,#92404,#92405) ;
#73833 = AXIS2_PLACEMENT_3D('',#119443,#92406,#92407) ;
#73834 = AXIS2_PLACEMENT_3D('',#119444,#92408,#92409) ;
#73835 = AXIS2_PLACEMENT_3D('',#119445,#92410,#92411) ;
#73836 = AXIS2_PLACEMENT_3D('',#119446,#92412,#92413) ;
#73837 = AXIS2_PLACEMENT_3D('',#119447,#92414,#92415) ;
#73838 = AXIS2_PLACEMENT_3D('',#119448,#92416,#92417) ;
#73839 = AXIS2_PLACEMENT_3D('',#119449,#92418,#92419) ;
#73840 = AXIS2_PLACEMENT_3D('',#119450,#92420,#92421) ;
#73841 = AXIS2_PLACEMENT_3D('',#119451,#92422,#92423) ;
#73842 = AXIS2_PLACEMENT_3D('',#119452,#92424,#92425) ;
#73843 = AXIS2_PLACEMENT_3D('',#119453,#92426,#92427) ;
#73844 = AXIS2_PLACEMENT_3D('',#119454,#92428,#92429) ;
#73845 = AXIS2_PLACEMENT_3D('',#119455,#92430,#92431) ;
#73846 = AXIS2_PLACEMENT_3D('',#119456,#92432,#92433) ;
#73847 = AXIS2_PLACEMENT_3D('',#119457,#92434,#92435) ;
#73848 = AXIS2_PLACEMENT_3D('',#119458,#92436,#92437) ;
#73849 = AXIS2_PLACEMENT_3D('',#119459,#92438,#92439) ;
#73850 = AXIS2_PLACEMENT_3D('',#119460,#92440,#92441) ;
#73851 = AXIS2_PLACEMENT_3D('',#119461,#92442,#92443) ;
#73852 = AXIS2_PLACEMENT_3D('',#119462,#92444,#92445) ;
#73853 = AXIS2_PLACEMENT_3D('',#119463,#92446,#92447) ;
#73854 = AXIS2_PLACEMENT_3D('',#119464,#92448,#92449) ;
#73855 = AXIS2_PLACEMENT_3D('',#119465,#92450,#92451) ;
#73856 = AXIS2_PLACEMENT_3D('',#119466,#92452,#92453) ;
#73857 = AXIS2_PLACEMENT_3D('',#119467,#92454,#92455) ;
#73858 = AXIS2_PLACEMENT_3D('',#119468,#92456,#92457) ;
#73859 = AXIS2_PLACEMENT_3D('',#119469,#92458,#92459) ;
#73860 = AXIS2_PLACEMENT_3D('',#119470,#92460,#92461) ;
#73861 = AXIS2_PLACEMENT_3D('',#119471,#92462,#92463) ;
#73862 = AXIS2_PLACEMENT_3D('',#119472,#92464,#92465) ;
#73863 = AXIS2_PLACEMENT_3D('',#119473,#92466,#92467) ;
#73864 = AXIS2_PLACEMENT_3D('',#119474,#92468,#92469) ;
#73865 = AXIS2_PLACEMENT_3D('',#119475,#92470,#92471) ;
#73866 = AXIS2_PLACEMENT_3D('',#119476,#92472,#92473) ;
#73867 = AXIS2_PLACEMENT_3D('',#119477,#92474,#92475) ;
#73868 = AXIS2_PLACEMENT_3D('',#119478,#92476,#92477) ;
#73869 = AXIS2_PLACEMENT_3D('',#119479,#92478,#92479) ;
#73870 = AXIS2_PLACEMENT_3D('',#119480,#92480,#92481) ;
#73871 = AXIS2_PLACEMENT_3D('',#119481,#92482,#92483) ;
#73872 = AXIS2_PLACEMENT_3D('',#119482,#92484,#92485) ;
#73873 = AXIS2_PLACEMENT_3D('',#119483,#92486,#92487) ;
#73874 = AXIS2_PLACEMENT_3D('',#119484,#92488,#92489) ;
#73875 = AXIS2_PLACEMENT_3D('',#119485,#92490,#92491) ;
#73876 = AXIS2_PLACEMENT_3D('',#119486,#92492,#92493) ;
#73877 = AXIS2_PLACEMENT_3D('',#119487,#92494,#92495) ;
#73878 = AXIS2_PLACEMENT_3D('',#119488,#92496,#92497) ;
#73879 = AXIS2_PLACEMENT_3D('',#119489,#92498,#92499) ;
#73880 = AXIS2_PLACEMENT_3D('',#119490,#92500,#92501) ;
#73881 = AXIS2_PLACEMENT_3D('',#119491,#92502,#92503) ;
#73882 = AXIS2_PLACEMENT_3D('',#119492,#92504,#92505) ;
#73883 = AXIS2_PLACEMENT_3D('',#119493,#92506,#92507) ;
#73884 = AXIS2_PLACEMENT_3D('',#119494,#92508,#92509) ;
#73885 = AXIS2_PLACEMENT_3D('',#119495,#92510,#92511) ;
#73886 = AXIS2_PLACEMENT_3D('',#119496,#92512,#92513) ;
#73887 = AXIS2_PLACEMENT_3D('',#119497,#92514,#92515) ;
#73888 = AXIS2_PLACEMENT_3D('',#119498,#92516,#92517) ;
#73889 = AXIS2_PLACEMENT_3D('',#119499,#92518,#92519) ;
#73890 = AXIS2_PLACEMENT_3D('',#119500,#92520,#92521) ;
#73891 = AXIS2_PLACEMENT_3D('',#119501,#92522,#92523) ;
#73892 = AXIS2_PLACEMENT_3D('',#119502,#92524,#92525) ;
#73893 = AXIS2_PLACEMENT_3D('',#119503,#92526,#92527) ;
#73894 = AXIS2_PLACEMENT_3D('',#119504,#92528,#92529) ;
#73895 = AXIS2_PLACEMENT_3D('',#119505,#92530,#92531) ;
#73896 = AXIS2_PLACEMENT_3D('',#119506,#92532,#92533) ;
#73897 = AXIS2_PLACEMENT_3D('',#119507,#92534,#92535) ;
#73898 = AXIS2_PLACEMENT_3D('',#119508,#92536,#92537) ;
#73899 = AXIS2_PLACEMENT_3D('',#119509,#92538,#92539) ;
#73900 = AXIS2_PLACEMENT_3D('',#119510,#92540,#92541) ;
#73901 = AXIS2_PLACEMENT_3D('',#119511,#92542,#92543) ;
#73902 = AXIS2_PLACEMENT_3D('',#119512,#92544,#92545) ;
#73903 = AXIS2_PLACEMENT_3D('',#119513,#92546,#92547) ;
#73904 = AXIS2_PLACEMENT_3D('',#119514,#92548,#92549) ;
#73905 = AXIS2_PLACEMENT_3D('',#119515,#92550,#92551) ;
#73906 = AXIS2_PLACEMENT_3D('',#119516,#92552,#92553) ;
#73907 = AXIS2_PLACEMENT_3D('',#119517,#92554,#92555) ;
#73908 = AXIS2_PLACEMENT_3D('',#119518,#92556,#92557) ;
#73909 = AXIS2_PLACEMENT_3D('',#119519,#92558,#92559) ;
#73910 = AXIS2_PLACEMENT_3D('',#119520,#92560,#92561) ;
#73911 = AXIS2_PLACEMENT_3D('',#119521,#92562,#92563) ;
#73912 = AXIS2_PLACEMENT_3D('',#119522,#92564,#92565) ;
#73913 = AXIS2_PLACEMENT_3D('',#119523,#92566,#92567) ;
#73914 = AXIS2_PLACEMENT_3D('',#119524,#92568,#92569) ;
#73915 = AXIS2_PLACEMENT_3D('',#119525,#92570,#92571) ;
#73916 = AXIS2_PLACEMENT_3D('',#119526,#92572,#92573) ;
#73917 = AXIS2_PLACEMENT_3D('',#119527,#92574,#92575) ;
#73918 = AXIS2_PLACEMENT_3D('',#119528,#92576,#92577) ;
#73919 = AXIS2_PLACEMENT_3D('',#119529,#92578,#92579) ;
#73920 = AXIS2_PLACEMENT_3D('',#119530,#92580,#92581) ;
#73921 = AXIS2_PLACEMENT_3D('',#119531,#92582,#92583) ;
#73922 = AXIS2_PLACEMENT_3D('',#119532,#92584,#92585) ;
#73923 = AXIS2_PLACEMENT_3D('',#119533,#92586,#92587) ;
#73924 = AXIS2_PLACEMENT_3D('',#119534,#92588,#92589) ;
#73925 = AXIS2_PLACEMENT_3D('',#119535,#92590,#92591) ;
#73926 = AXIS2_PLACEMENT_3D('',#119536,#92592,#92593) ;
#73927 = AXIS2_PLACEMENT_3D('',#119537,#92594,#92595) ;
#73928 = AXIS2_PLACEMENT_3D('',#119538,#92596,#92597) ;
#73929 = AXIS2_PLACEMENT_3D('',#119539,#92598,#92599) ;
#73930 = AXIS2_PLACEMENT_3D('',#119540,#92600,#92601) ;
#73931 = AXIS2_PLACEMENT_3D('',#119541,#92602,#92603) ;
#73932 = AXIS2_PLACEMENT_3D('',#119542,#92604,#92605) ;
#73933 = AXIS2_PLACEMENT_3D('',#119543,#92606,#92607) ;
#73934 = AXIS2_PLACEMENT_3D('',#119544,#92608,#92609) ;
#73935 = AXIS2_PLACEMENT_3D('',#119545,#92610,#92611) ;
#73936 = AXIS2_PLACEMENT_3D('',#119546,#92612,#92613) ;
#73937 = AXIS2_PLACEMENT_3D('',#119547,#92614,#92615) ;
#73938 = AXIS2_PLACEMENT_3D('',#119548,#92616,#92617) ;
#73939 = AXIS2_PLACEMENT_3D('',#119549,#92618,#92619) ;
#73940 = AXIS2_PLACEMENT_3D('',#119550,#92620,#92621) ;
#73941 = AXIS2_PLACEMENT_3D('',#119551,#92622,#92623) ;
#73942 = AXIS2_PLACEMENT_3D('',#119552,#92624,#92625) ;
#73943 = AXIS2_PLACEMENT_3D('',#119553,#92626,#92627) ;
#73944 = AXIS2_PLACEMENT_3D('',#119554,#92628,#92629) ;
#73945 = AXIS2_PLACEMENT_3D('',#119555,#92630,#92631) ;
#73946 = AXIS2_PLACEMENT_3D('',#119556,#92632,#92633) ;
#73947 = AXIS2_PLACEMENT_3D('',#119557,#92634,#92635) ;
#73948 = AXIS2_PLACEMENT_3D('',#119558,#92636,#92637) ;
#73949 = AXIS2_PLACEMENT_3D('',#119559,#92638,#92639) ;
#73950 = AXIS2_PLACEMENT_3D('',#119560,#92640,#92641) ;
#73951 = AXIS2_PLACEMENT_3D('',#119561,#92642,#92643) ;
#73952 = AXIS2_PLACEMENT_3D('',#119562,#92644,#92645) ;
#73953 = AXIS2_PLACEMENT_3D('',#119563,#92646,#92647) ;
#73954 = AXIS2_PLACEMENT_3D('',#119564,#92648,#92649) ;
#73955 = AXIS2_PLACEMENT_3D('',#119565,#92650,#92651) ;
#73956 = AXIS2_PLACEMENT_3D('',#119566,#92652,#92653) ;
#73957 = AXIS2_PLACEMENT_3D('',#119567,#92654,#92655) ;
#73958 = AXIS2_PLACEMENT_3D('',#119568,#92656,#92657) ;
#73959 = AXIS2_PLACEMENT_3D('',#119569,#92658,#92659) ;
#73960 = AXIS2_PLACEMENT_3D('',#119570,#92660,#92661) ;
#73961 = AXIS2_PLACEMENT_3D('',#119571,#92662,#92663) ;
#73962 = AXIS2_PLACEMENT_3D('',#119572,#92664,#92665) ;
#73963 = AXIS2_PLACEMENT_3D('',#119573,#92666,#92667) ;
#73964 = AXIS2_PLACEMENT_3D('',#119574,#92668,#92669) ;
#73965 = AXIS2_PLACEMENT_3D('',#119575,#92670,#92671) ;
#73966 = AXIS2_PLACEMENT_3D('',#119576,#92672,#92673) ;
#73967 = AXIS2_PLACEMENT_3D('',#119577,#92674,#92675) ;
#73968 = AXIS2_PLACEMENT_3D('',#119578,#92676,#92677) ;
#73969 = AXIS2_PLACEMENT_3D('',#119579,#92678,#92679) ;
#73970 = AXIS2_PLACEMENT_3D('',#119580,#92680,#92681) ;
#73971 = AXIS2_PLACEMENT_3D('',#119581,#92682,#92683) ;
#73972 = AXIS2_PLACEMENT_3D('',#119582,#92684,#92685) ;
#73973 = AXIS2_PLACEMENT_3D('',#119583,#92686,#92687) ;
#73974 = AXIS2_PLACEMENT_3D('',#119584,#92688,#92689) ;
#73975 = AXIS2_PLACEMENT_3D('',#119585,#92690,#92691) ;
#73976 = AXIS2_PLACEMENT_3D('',#119586,#92692,#92693) ;
#73977 = AXIS2_PLACEMENT_3D('',#119587,#92694,#92695) ;
#73978 = AXIS2_PLACEMENT_3D('',#119588,#92696,#92697) ;
#73979 = AXIS2_PLACEMENT_3D('',#119589,#92698,#92699) ;
#73980 = AXIS2_PLACEMENT_3D('',#119590,#92700,#92701) ;
#73981 = AXIS2_PLACEMENT_3D('',#119591,#92702,#92703) ;
#73982 = AXIS2_PLACEMENT_3D('',#119592,#92704,#92705) ;
#73983 = AXIS2_PLACEMENT_3D('',#119593,#92706,#92707) ;
#73984 = AXIS2_PLACEMENT_3D('',#119594,#92708,#92709) ;
#73985 = AXIS2_PLACEMENT_3D('',#119595,#92710,#92711) ;
#73986 = AXIS2_PLACEMENT_3D('',#119596,#92712,#92713) ;
#73987 = AXIS2_PLACEMENT_3D('',#119597,#92714,#92715) ;
#73988 = AXIS2_PLACEMENT_3D('',#119598,#92716,#92717) ;
#73989 = AXIS2_PLACEMENT_3D('',#119599,#92718,#92719) ;
#73990 = AXIS2_PLACEMENT_3D('',#119600,#92720,#92721) ;
#73991 = AXIS2_PLACEMENT_3D('',#119601,#92722,#92723) ;
#73992 = AXIS2_PLACEMENT_3D('',#119602,#92724,#92725) ;
#73993 = AXIS2_PLACEMENT_3D('',#119603,#92726,#92727) ;
#73994 = AXIS2_PLACEMENT_3D('',#119604,#92728,#92729) ;
#73995 = AXIS2_PLACEMENT_3D('',#119605,#92730,#92731) ;
#73996 = AXIS2_PLACEMENT_3D('',#119606,#92732,#92733) ;
#73997 = AXIS2_PLACEMENT_3D('',#119607,#92734,#92735) ;
#73998 = AXIS2_PLACEMENT_3D('',#119608,#92736,#92737) ;
#73999 = AXIS2_PLACEMENT_3D('',#119609,#92738,#92739) ;
#74000 = AXIS2_PLACEMENT_3D('',#119610,#92740,#92741) ;
#74001 = AXIS2_PLACEMENT_3D('',#119611,#92742,#92743) ;
#74002 = AXIS2_PLACEMENT_3D('',#119612,#92744,#92745) ;
#74003 = AXIS2_PLACEMENT_3D('',#119613,#92746,#92747) ;
#74004 = AXIS2_PLACEMENT_3D('',#119614,#92748,#92749) ;
#74005 = AXIS2_PLACEMENT_3D('',#119615,#92750,#92751) ;
#74006 = AXIS2_PLACEMENT_3D('',#119616,#92752,#92753) ;
#74007 = AXIS2_PLACEMENT_3D('',#119617,#92754,#92755) ;
#74008 = AXIS2_PLACEMENT_3D('',#119618,#92756,#92757) ;
#74009 = AXIS2_PLACEMENT_3D('',#119619,#92758,#92759) ;
#74010 = AXIS2_PLACEMENT_3D('',#119620,#92760,#92761) ;
#74011 = AXIS2_PLACEMENT_3D('',#119621,#92762,#92763) ;
#74012 = AXIS2_PLACEMENT_3D('',#119622,#92764,#92765) ;
#74013 = AXIS2_PLACEMENT_3D('',#119623,#92766,#92767) ;
#74014 = AXIS2_PLACEMENT_3D('',#119624,#92768,#92769) ;
#74015 = AXIS2_PLACEMENT_3D('',#119625,#92770,#92771) ;
#74016 = AXIS2_PLACEMENT_3D('',#119626,#92772,#92773) ;
#74017 = AXIS2_PLACEMENT_3D('',#119627,#92774,#92775) ;
#74018 = AXIS2_PLACEMENT_3D('',#119628,#92776,#92777) ;
#74019 = AXIS2_PLACEMENT_3D('',#119629,#92778,#92779) ;
#74020 = AXIS2_PLACEMENT_3D('',#119630,#92780,#92781) ;
#74021 = AXIS2_PLACEMENT_3D('',#119631,#92782,#92783) ;
#74022 = AXIS2_PLACEMENT_3D('',#119632,#92784,#92785) ;
#74023 = AXIS2_PLACEMENT_3D('',#119633,#92786,#92787) ;
#74024 = AXIS2_PLACEMENT_3D('',#119634,#92788,#92789) ;
#74025 = AXIS2_PLACEMENT_3D('',#119635,#92790,#92791) ;
#74026 = AXIS2_PLACEMENT_3D('',#119636,#92792,#92793) ;
#74027 = AXIS2_PLACEMENT_3D('',#119637,#92794,#92795) ;
#74028 = AXIS2_PLACEMENT_3D('',#119638,#92796,#92797) ;
#74029 = AXIS2_PLACEMENT_3D('',#119639,#92798,#92799) ;
#74030 = AXIS2_PLACEMENT_3D('',#119640,#92800,#92801) ;
#74031 = AXIS2_PLACEMENT_3D('',#119641,#92802,#92803) ;
#74032 = AXIS2_PLACEMENT_3D('',#119642,#92804,#92805) ;
#74033 = AXIS2_PLACEMENT_3D('',#119643,#92806,#92807) ;
#74034 = AXIS2_PLACEMENT_3D('',#119644,#92808,#92809) ;
#74035 = AXIS2_PLACEMENT_3D('',#119645,#92810,#92811) ;
#74036 = AXIS2_PLACEMENT_3D('',#119646,#92812,#92813) ;
#74037 = AXIS2_PLACEMENT_3D('',#119647,#92814,#92815) ;
#74038 = AXIS2_PLACEMENT_3D('',#119648,#92816,#92817) ;
#74039 = AXIS2_PLACEMENT_3D('',#119649,#92818,#92819) ;
#74040 = AXIS2_PLACEMENT_3D('',#119650,#92820,#92821) ;
#74041 = AXIS2_PLACEMENT_3D('',#119651,#92822,#92823) ;
#74042 = AXIS2_PLACEMENT_3D('',#119652,#92824,#92825) ;
#74043 = AXIS2_PLACEMENT_3D('',#119653,#92826,#92827) ;
#74044 = AXIS2_PLACEMENT_3D('',#119654,#92828,#92829) ;
#74045 = AXIS2_PLACEMENT_3D('',#119655,#92830,#92831) ;
#74046 = AXIS2_PLACEMENT_3D('',#119656,#92832,#92833) ;
#74047 = AXIS2_PLACEMENT_3D('',#119657,#92834,#92835) ;
#74048 = AXIS2_PLACEMENT_3D('',#119658,#92836,#92837) ;
#74049 = AXIS2_PLACEMENT_3D('',#119659,#92838,#92839) ;
#74050 = AXIS2_PLACEMENT_3D('',#119660,#92840,#92841) ;
#74051 = AXIS2_PLACEMENT_3D('',#119661,#92842,#92843) ;
#74052 = AXIS2_PLACEMENT_3D('',#119662,#92844,#92845) ;
#74053 = AXIS2_PLACEMENT_3D('',#119663,#92846,#92847) ;
#74054 = AXIS2_PLACEMENT_3D('',#119664,#92848,#92849) ;
#74055 = AXIS2_PLACEMENT_3D('',#119665,#92850,#92851) ;
#74056 = AXIS2_PLACEMENT_3D('',#119666,#92852,#92853) ;
#74057 = AXIS2_PLACEMENT_3D('',#119667,#92854,#92855) ;
#74058 = AXIS2_PLACEMENT_3D('',#119668,#92856,#92857) ;
#74059 = AXIS2_PLACEMENT_3D('',#119669,#92858,#92859) ;
#74060 = AXIS2_PLACEMENT_3D('',#119670,#92860,#92861) ;
#74061 = AXIS2_PLACEMENT_3D('',#119671,#92862,#92863) ;
#74062 = AXIS2_PLACEMENT_3D('',#119672,#92864,#92865) ;
#74063 = AXIS2_PLACEMENT_3D('',#119673,#92866,#92867) ;
#74064 = AXIS2_PLACEMENT_3D('',#119674,#92868,#92869) ;
#74065 = AXIS2_PLACEMENT_3D('',#119675,#92870,#92871) ;
#74066 = AXIS2_PLACEMENT_3D('',#119676,#92872,#92873) ;
#74067 = AXIS2_PLACEMENT_3D('',#119677,#92874,#92875) ;
#74068 = AXIS2_PLACEMENT_3D('',#119678,#92876,#92877) ;
#74069 = AXIS2_PLACEMENT_3D('',#119679,#92878,#92879) ;
#74070 = AXIS2_PLACEMENT_3D('',#119680,#92880,#92881) ;
#74071 = AXIS2_PLACEMENT_3D('',#119681,#92882,#92883) ;
#74072 = AXIS2_PLACEMENT_3D('',#119682,#92884,#92885) ;
#74073 = AXIS2_PLACEMENT_3D('',#119683,#92886,#92887) ;
#74074 = AXIS2_PLACEMENT_3D('',#119684,#92888,#92889) ;
#74075 = AXIS2_PLACEMENT_3D('',#119685,#92890,#92891) ;
#74076 = AXIS2_PLACEMENT_3D('',#119686,#92892,#92893) ;
#74077 = AXIS2_PLACEMENT_3D('',#119687,#92894,#92895) ;
#74078 = AXIS2_PLACEMENT_3D('',#119688,#92896,#92897) ;
#74079 = AXIS2_PLACEMENT_3D('',#119689,#92898,#92899) ;
#74080 = AXIS2_PLACEMENT_3D('',#119690,#92900,#92901) ;
#74081 = AXIS2_PLACEMENT_3D('',#119691,#92902,#92903) ;
#74082 = AXIS2_PLACEMENT_3D('',#119692,#92904,#92905) ;
#74083 = AXIS2_PLACEMENT_3D('',#119693,#92906,#92907) ;
#74084 = AXIS2_PLACEMENT_3D('',#119694,#92908,#92909) ;
#74085 = AXIS2_PLACEMENT_3D('',#119695,#92910,#92911) ;
#74086 = AXIS2_PLACEMENT_3D('',#119696,#92912,#92913) ;
#74087 = AXIS2_PLACEMENT_3D('',#119697,#92914,#92915) ;
#74088 = AXIS2_PLACEMENT_3D('',#119698,#92916,#92917) ;
#74089 = AXIS2_PLACEMENT_3D('',#119699,#92918,#92919) ;
#74090 = AXIS2_PLACEMENT_3D('',#119700,#92920,#92921) ;
#74091 = AXIS2_PLACEMENT_3D('',#119701,#92922,#92923) ;
#74092 = AXIS2_PLACEMENT_3D('',#119702,#92924,#92925) ;
#74093 = AXIS2_PLACEMENT_3D('',#119703,#92926,#92927) ;
#74094 = AXIS2_PLACEMENT_3D('',#119704,#92928,#92929) ;
#74095 = AXIS2_PLACEMENT_3D('',#119705,#92930,#92931) ;
#74096 = AXIS2_PLACEMENT_3D('',#119706,#92932,#92933) ;
#74097 = AXIS2_PLACEMENT_3D('',#119707,#92934,#92935) ;
#74098 = AXIS2_PLACEMENT_3D('',#119708,#92936,#92937) ;
#74099 = AXIS2_PLACEMENT_3D('',#119709,#92938,#92939) ;
#74100 = AXIS2_PLACEMENT_3D('',#119710,#92940,#92941) ;
#74101 = AXIS2_PLACEMENT_3D('',#119711,#92942,#92943) ;
#74102 = AXIS2_PLACEMENT_3D('',#119712,#92944,#92945) ;
#74103 = AXIS2_PLACEMENT_3D('',#119713,#92946,#92947) ;
#74104 = AXIS2_PLACEMENT_3D('',#119714,#92948,#92949) ;
#74105 = AXIS2_PLACEMENT_3D('',#119715,#92950,#92951) ;
#74106 = AXIS2_PLACEMENT_3D('',#119716,#92952,#92953) ;
#74107 = AXIS2_PLACEMENT_3D('',#119717,#92954,#92955) ;
#74108 = AXIS2_PLACEMENT_3D('',#119718,#92956,#92957) ;
#74109 = AXIS2_PLACEMENT_3D('',#119719,#92958,#92959) ;
#74110 = AXIS2_PLACEMENT_3D('',#119720,#92960,#92961) ;
#74111 = AXIS2_PLACEMENT_3D('',#119721,#92962,#92963) ;
#74112 = AXIS2_PLACEMENT_3D('',#119722,#92964,#92965) ;
#74113 = AXIS2_PLACEMENT_3D('',#119723,#92966,#92967) ;
#74114 = AXIS2_PLACEMENT_3D('',#119724,#92968,#92969) ;
#74115 = AXIS2_PLACEMENT_3D('',#119725,#92970,#92971) ;
#74116 = AXIS2_PLACEMENT_3D('',#119726,#92972,#92973) ;
#74117 = AXIS2_PLACEMENT_3D('',#119727,#92974,#92975) ;
#74118 = AXIS2_PLACEMENT_3D('',#119728,#92976,#92977) ;
#74119 = AXIS2_PLACEMENT_3D('',#119729,#92978,#92979) ;
#74120 = AXIS2_PLACEMENT_3D('',#119730,#92980,#92981) ;
#74121 = AXIS2_PLACEMENT_3D('',#119731,#92982,#92983) ;
#74122 = AXIS2_PLACEMENT_3D('',#119732,#92984,#92985) ;
#74123 = AXIS2_PLACEMENT_3D('',#119733,#92986,#92987) ;
#74124 = AXIS2_PLACEMENT_3D('',#119734,#92988,#92989) ;
#74125 = AXIS2_PLACEMENT_3D('',#119735,#92990,#92991) ;
#74126 = AXIS2_PLACEMENT_3D('',#119736,#92992,#92993) ;
#74127 = AXIS2_PLACEMENT_3D('',#119737,#92994,#92995) ;
#74128 = AXIS2_PLACEMENT_3D('',#119738,#92996,#92997) ;
#74129 = AXIS2_PLACEMENT_3D('',#119739,#92998,#92999) ;
#74130 = AXIS2_PLACEMENT_3D('',#119740,#93000,#93001) ;
#74131 = AXIS2_PLACEMENT_3D('',#119741,#93002,#93003) ;
#74132 = AXIS2_PLACEMENT_3D('',#119742,#93004,#93005) ;
#74133 = AXIS2_PLACEMENT_3D('',#119743,#93006,#93007) ;
#74134 = AXIS2_PLACEMENT_3D('',#119744,#93008,#93009) ;
#74135 = AXIS2_PLACEMENT_3D('',#119745,#93010,#93011) ;
#74136 = AXIS2_PLACEMENT_3D('',#119746,#93012,#93013) ;
#74137 = AXIS2_PLACEMENT_3D('',#119747,#93014,#93015) ;
#74138 = AXIS2_PLACEMENT_3D('',#119748,#93016,#93017) ;
#74139 = AXIS2_PLACEMENT_3D('',#119749,#93018,#93019) ;
#74140 = AXIS2_PLACEMENT_3D('',#119750,#93020,#93021) ;
#74141 = AXIS2_PLACEMENT_3D('',#119751,#93022,#93023) ;
#74142 = AXIS2_PLACEMENT_3D('',#119752,#93024,#93025) ;
#74143 = AXIS2_PLACEMENT_3D('',#119753,#93026,#93027) ;
#74144 = AXIS2_PLACEMENT_3D('',#119754,#93028,#93029) ;
#74145 = AXIS2_PLACEMENT_3D('',#119755,#93030,#93031) ;
#74146 = AXIS2_PLACEMENT_3D('',#119756,#93032,#93033) ;
#74147 = AXIS2_PLACEMENT_3D('',#119757,#93034,#93035) ;
#74148 = AXIS2_PLACEMENT_3D('',#119758,#93036,#93037) ;
#74149 = AXIS2_PLACEMENT_3D('',#119759,#93038,#93039) ;
#74150 = AXIS2_PLACEMENT_3D('',#119760,#93040,#93041) ;
#74151 = AXIS2_PLACEMENT_3D('',#119761,#93042,#93043) ;
#74152 = AXIS2_PLACEMENT_3D('',#119762,#93044,#93045) ;
#74153 = AXIS2_PLACEMENT_3D('',#119763,#93046,#93047) ;
#74154 = AXIS2_PLACEMENT_3D('',#119764,#93048,#93049) ;
#74155 = AXIS2_PLACEMENT_3D('',#119765,#93050,#93051) ;
#74156 = AXIS2_PLACEMENT_3D('',#119766,#93052,#93053) ;
#74157 = AXIS2_PLACEMENT_3D('',#119767,#93054,#93055) ;
#74158 = AXIS2_PLACEMENT_3D('',#119768,#93056,#93057) ;
#74159 = AXIS2_PLACEMENT_3D('',#119769,#93058,#93059) ;
#74160 = AXIS2_PLACEMENT_3D('',#119770,#93060,#93061) ;
#74161 = AXIS2_PLACEMENT_3D('',#119771,#93062,#93063) ;
#74162 = AXIS2_PLACEMENT_3D('',#119772,#93064,#93065) ;
#74163 = AXIS2_PLACEMENT_3D('',#119773,#93066,#93067) ;
#74164 = AXIS2_PLACEMENT_3D('',#119774,#93068,#93069) ;
#74165 = AXIS2_PLACEMENT_3D('',#119775,#93070,#93071) ;
#74166 = AXIS2_PLACEMENT_3D('',#119776,#93072,#93073) ;
#74167 = AXIS2_PLACEMENT_3D('',#119777,#93074,#93075) ;
#74168 = AXIS2_PLACEMENT_3D('',#119778,#93076,#93077) ;
#74169 = AXIS2_PLACEMENT_3D('',#119779,#93078,#93079) ;
#74170 = AXIS2_PLACEMENT_3D('',#119780,#93080,#93081) ;
#74171 = AXIS2_PLACEMENT_3D('',#119781,#93082,#93083) ;
#74172 = AXIS2_PLACEMENT_3D('',#119782,#93084,#93085) ;
#74173 = AXIS2_PLACEMENT_3D('',#119783,#93086,#93087) ;
#74174 = AXIS2_PLACEMENT_3D('',#119784,#93088,#93089) ;
#74175 = AXIS2_PLACEMENT_3D('',#119785,#93090,#93091) ;
#74176 = AXIS2_PLACEMENT_3D('',#119786,#93092,#93093) ;
#74177 = AXIS2_PLACEMENT_3D('',#119787,#93094,#93095) ;
#74178 = AXIS2_PLACEMENT_3D('',#119788,#93096,#93097) ;
#74179 = AXIS2_PLACEMENT_3D('',#119789,#93098,#93099) ;
#74180 = AXIS2_PLACEMENT_3D('',#119790,#93100,#93101) ;
#74181 = AXIS2_PLACEMENT_3D('',#119791,#93102,#93103) ;
#74182 = AXIS2_PLACEMENT_3D('',#119792,#93104,#93105) ;
#74183 = AXIS2_PLACEMENT_3D('',#119793,#93106,#93107) ;
#74184 = AXIS2_PLACEMENT_3D('',#119794,#93108,#93109) ;
#74185 = AXIS2_PLACEMENT_3D('',#119795,#93110,#93111) ;
#74186 = AXIS2_PLACEMENT_3D('',#119796,#93112,#93113) ;
#74187 = AXIS2_PLACEMENT_3D('',#119797,#93114,#93115) ;
#74188 = AXIS2_PLACEMENT_3D('',#119798,#93116,#93117) ;
#74189 = AXIS2_PLACEMENT_3D('',#119799,#93118,#93119) ;
#74190 = AXIS2_PLACEMENT_3D('',#119800,#93120,#93121) ;
#74191 = AXIS2_PLACEMENT_3D('',#119801,#93122,#93123) ;
#74192 = AXIS2_PLACEMENT_3D('',#119803,#93124,#93125) ;
#74193 = AXIS2_PLACEMENT_3D('',#119804,#93126,#93127) ;
#74194 = AXIS2_PLACEMENT_3D('',#119805,#93128,#93129) ;
#74195 = AXIS2_PLACEMENT_3D('',#119806,#93130,#93131) ;
#74196 = AXIS2_PLACEMENT_3D('',#119807,#93132,#93133) ;
#74197 = AXIS2_PLACEMENT_3D('',#119808,#93134,#93135) ;
#74198 = AXIS2_PLACEMENT_3D('',#119809,#93136,#93137) ;
#74199 = AXIS2_PLACEMENT_3D('',#119810,#93138,#93139) ;
#74200 = AXIS2_PLACEMENT_3D('',#119811,#93140,#93141) ;
#74201 = AXIS2_PLACEMENT_3D('',#119822,#93143,#93144) ;
#74202 = AXIS2_PLACEMENT_3D('',#119879,#93146,#93147) ;
#74203 = AXIS2_PLACEMENT_3D('',#119880,#93148,#93149) ;
#74204 = AXIS2_PLACEMENT_3D('',#119881,#93150,#93151) ;
#74205 = AXIS2_PLACEMENT_3D('',#119882,#93152,#93153) ;
#74206 = AXIS2_PLACEMENT_3D('',#119883,#93154,#93155) ;
#74207 = AXIS2_PLACEMENT_3D('',#119884,#93156,#93157) ;
#74208 = AXIS2_PLACEMENT_3D('',#119885,#93158,#93159) ;
#74209 = AXIS2_PLACEMENT_3D('',#119886,#93160,#93161) ;
#74210 = AXIS2_PLACEMENT_3D('',#119887,#93162,#93163) ;
#74211 = AXIS2_PLACEMENT_3D('',#119888,#93164,#93165) ;
#74212 = AXIS2_PLACEMENT_3D('',#119889,#93166,#93167) ;
#74213 = AXIS2_PLACEMENT_3D('',#119890,#93168,#93169) ;
#74214 = AXIS2_PLACEMENT_3D('',#119891,#93170,#93171) ;
#74215 = AXIS2_PLACEMENT_3D('',#119892,#93172,#93173) ;
#74216 = AXIS2_PLACEMENT_3D('',#119893,#93174,#93175) ;
#74217 = AXIS2_PLACEMENT_3D('',#119894,#93176,#93177) ;
#74218 = AXIS2_PLACEMENT_3D('',#119895,#93178,#93179) ;
#74219 = AXIS2_PLACEMENT_3D('',#119896,#93180,#93181) ;
#74220 = AXIS2_PLACEMENT_3D('',#119897,#93182,#93183) ;
#74221 = AXIS2_PLACEMENT_3D('',#119898,#93184,#93185) ;
#74222 = AXIS2_PLACEMENT_3D('',#119899,#93186,#93187) ;
#74223 = AXIS2_PLACEMENT_3D('',#119900,#93188,#93189) ;
#74224 = AXIS2_PLACEMENT_3D('',#119901,#93190,#93191) ;
#74225 = AXIS2_PLACEMENT_3D('',#119904,#93193,#93194) ;
#74226 = AXIS2_PLACEMENT_3D('',#119905,#93195,#93196) ;
#74227 = AXIS2_PLACEMENT_3D('',#119906,#93197,#93198) ;
#74228 = AXIS2_PLACEMENT_3D('',#119907,#93199,#93200) ;
#74229 = AXIS2_PLACEMENT_3D('',#119908,#93201,#93202) ;
#74230 = AXIS2_PLACEMENT_3D('',#119909,#93203,#93204) ;
#74231 = AXIS2_PLACEMENT_3D('',#119910,#93205,#93206) ;
#74232 = AXIS2_PLACEMENT_3D('',#119911,#93207,#93208) ;
#74233 = AXIS2_PLACEMENT_3D('',#119912,#93209,#93210) ;
#74234 = AXIS2_PLACEMENT_3D('',#119913,#93211,#93212) ;
#74235 = AXIS2_PLACEMENT_3D('',#119914,#93213,#93214) ;
#74236 = AXIS2_PLACEMENT_3D('',#119915,#93215,#93216) ;
#74237 = AXIS2_PLACEMENT_3D('',#119916,#93217,#93218) ;
#74238 = AXIS2_PLACEMENT_3D('',#119917,#93219,#93220) ;
#74239 = AXIS2_PLACEMENT_3D('',#119918,#93221,#93222) ;
#74240 = AXIS2_PLACEMENT_3D('',#119919,#93223,#93224) ;
#74241 = AXIS2_PLACEMENT_3D('',#119921,#93225,#93226) ;
#74242 = AXIS2_PLACEMENT_3D('',#119922,#93227,#93228) ;
#74243 = AXIS2_PLACEMENT_3D('',#119923,#93229,#93230) ;
#74244 = AXIS2_PLACEMENT_3D('',#119924,#93231,#93232) ;
#74245 = AXIS2_PLACEMENT_3D('',#119925,#93233,#93234) ;
#74246 = AXIS2_PLACEMENT_3D('',#119926,#93235,#93236) ;
#74247 = AXIS2_PLACEMENT_3D('',#119927,#93237,#93238) ;
#74248 = AXIS2_PLACEMENT_3D('',#119928,#93239,#93240) ;
#74249 = AXIS2_PLACEMENT_3D('',#119929,#93241,#93242) ;
#74250 = AXIS2_PLACEMENT_3D('',#119930,#93243,#93244) ;
#74251 = AXIS2_PLACEMENT_3D('',#119931,#93245,#93246) ;
#74252 = AXIS2_PLACEMENT_3D('',#119932,#93247,#93248) ;
#74253 = AXIS2_PLACEMENT_3D('',#119933,#93249,#93250) ;
#74254 = AXIS2_PLACEMENT_3D('',#119936,#93252,#93253) ;
#74255 = AXIS2_PLACEMENT_3D('',#119937,#93254,#93255) ;
#74256 = AXIS2_PLACEMENT_3D('',#119938,#93256,#93257) ;
#74257 = AXIS2_PLACEMENT_3D('',#119939,#93258,#93259) ;
#74258 = AXIS2_PLACEMENT_3D('',#119940,#93260,#93261) ;
#74259 = AXIS2_PLACEMENT_3D('',#119941,#93262,#93263) ;
#74260 = AXIS2_PLACEMENT_3D('',#119942,#93264,#93265) ;
#74261 = AXIS2_PLACEMENT_3D('',#119943,#93266,#93267) ;
#74262 = AXIS2_PLACEMENT_3D('',#119944,#93268,#93269) ;
#74263 = AXIS2_PLACEMENT_3D('',#119945,#93270,#93271) ;
#74264 = AXIS2_PLACEMENT_3D('',#119946,#93272,#93273) ;
#74265 = AXIS2_PLACEMENT_3D('',#119947,#93274,#93275) ;
#74266 = AXIS2_PLACEMENT_3D('',#119948,#93276,#93277) ;
#74267 = AXIS2_PLACEMENT_3D('',#119950,#93278,#93279) ;
#74268 = AXIS2_PLACEMENT_3D('',#119951,#93280,#93281) ;
#74269 = AXIS2_PLACEMENT_3D('',#119952,#93282,#93283) ;
#74270 = AXIS2_PLACEMENT_3D('',#119953,#93284,#93285) ;
#74271 = AXIS2_PLACEMENT_3D('',#119954,#93286,#93287) ;
#74272 = AXIS2_PLACEMENT_3D('',#119955,#93288,#93289) ;
#74273 = AXIS2_PLACEMENT_3D('',#119956,#93290,#93291) ;
#74274 = AXIS2_PLACEMENT_3D('',#119957,#93292,#93293) ;
#74275 = AXIS2_PLACEMENT_3D('',#119958,#93294,#93295) ;
#74276 = AXIS2_PLACEMENT_3D('',#119959,#93296,#93297) ;
#74277 = AXIS2_PLACEMENT_3D('',#119960,#93298,#93299) ;
#74278 = AXIS2_PLACEMENT_3D('',#119962,#93301,#93302) ;
#74279 = AXIS2_PLACEMENT_3D('',#119963,#93303,#93304) ;
#74280 = AXIS2_PLACEMENT_3D('',#119964,#93305,#93306) ;
#74281 = AXIS2_PLACEMENT_3D('',#119965,#93307,#93308) ;
#74282 = AXIS2_PLACEMENT_3D('',#119966,#93309,#93310) ;
#74283 = AXIS2_PLACEMENT_3D('',#119967,#93311,#93312) ;
#74284 = AXIS2_PLACEMENT_3D('',#119968,#93313,#93314) ;
#74285 = AXIS2_PLACEMENT_3D('',#119969,#93315,#93316) ;
#74286 = AXIS2_PLACEMENT_3D('',#119970,#93317,#93318) ;
#74287 = AXIS2_PLACEMENT_3D('',#119971,#93319,#93320) ;
#74288 = AXIS2_PLACEMENT_3D('',#119972,#93321,#93322) ;
#74289 = AXIS2_PLACEMENT_3D('',#119973,#93323,#93324) ;
#74290 = AXIS2_PLACEMENT_3D('',#119974,#93325,#93326) ;
#74291 = AXIS2_PLACEMENT_3D('',#119975,#93327,#93328) ;
#74292 = AXIS2_PLACEMENT_3D('',#119976,#93329,#93330) ;
#74293 = AXIS2_PLACEMENT_3D('',#119977,#93331,#93332) ;
#74294 = AXIS2_PLACEMENT_3D('',#119978,#93333,#93334) ;
#74295 = AXIS2_PLACEMENT_3D('',#119979,#93335,#93336) ;
#74296 = AXIS2_PLACEMENT_3D('',#119980,#93337,#93338) ;
#74297 = AXIS2_PLACEMENT_3D('',#119981,#93339,#93340) ;
#74298 = AXIS2_PLACEMENT_3D('',#119982,#93341,#93342) ;
#74299 = AXIS2_PLACEMENT_3D('',#119983,#93343,#93344) ;
#74300 = AXIS2_PLACEMENT_3D('',#119984,#93345,#93346) ;
#74301 = AXIS2_PLACEMENT_3D('',#119985,#93347,#93348) ;
#74302 = AXIS2_PLACEMENT_3D('',#119986,#93349,#93350) ;
#74303 = AXIS2_PLACEMENT_3D('',#119987,#93351,#93352) ;
#74304 = AXIS2_PLACEMENT_3D('',#119988,#93353,#93354) ;
#74305 = AXIS2_PLACEMENT_3D('',#119989,#93355,#93356) ;
#74306 = AXIS2_PLACEMENT_3D('',#119990,#93357,#93358) ;
#74307 = AXIS2_PLACEMENT_3D('',#119991,#93359,#93360) ;
#74308 = AXIS2_PLACEMENT_3D('',#119992,#93361,#93362) ;
#74309 = AXIS2_PLACEMENT_3D('',#119993,#93363,#93364) ;
#74310 = AXIS2_PLACEMENT_3D('',#119994,#93365,#93366) ;
#74311 = AXIS2_PLACEMENT_3D('',#119995,#93367,#93368) ;
#74312 = AXIS2_PLACEMENT_3D('',#119996,#93369,#93370) ;
#74313 = AXIS2_PLACEMENT_3D('',#119997,#93371,#93372) ;
#74314 = AXIS2_PLACEMENT_3D('',#119998,#93373,#93374) ;
#74315 = AXIS2_PLACEMENT_3D('',#119999,#93375,#93376) ;
#74316 = AXIS2_PLACEMENT_3D('',#120000,#93377,#93378) ;
#74317 = AXIS2_PLACEMENT_3D('',#120001,#93379,#93380) ;
#74318 = AXIS2_PLACEMENT_3D('',#120002,#93381,#93382) ;
#74319 = AXIS2_PLACEMENT_3D('',#120003,#93383,#93384) ;
#74320 = AXIS2_PLACEMENT_3D('',#120004,#93385,#93386) ;
#74321 = AXIS2_PLACEMENT_3D('',#120005,#93387,#93388) ;
#74322 = AXIS2_PLACEMENT_3D('',#120006,#93389,#93390) ;
#74323 = AXIS2_PLACEMENT_3D('',#120007,#93391,#93392) ;
#74324 = AXIS2_PLACEMENT_3D('',#120008,#93393,#93394) ;
#74325 = AXIS2_PLACEMENT_3D('',#120009,#93395,#93396) ;
#74326 = AXIS2_PLACEMENT_3D('',#120010,#93397,#93398) ;
#74327 = AXIS2_PLACEMENT_3D('',#120011,#93399,#93400) ;
#74328 = AXIS2_PLACEMENT_3D('',#120012,#93401,#93402) ;
#74329 = AXIS2_PLACEMENT_3D('',#120013,#93403,#93404) ;
#74330 = AXIS2_PLACEMENT_3D('',#120014,#93405,#93406) ;
#74331 = AXIS2_PLACEMENT_3D('',#120015,#93407,#93408) ;
#74332 = AXIS2_PLACEMENT_3D('',#120016,#93409,#93410) ;
#74333 = AXIS2_PLACEMENT_3D('',#120017,#93411,#93412) ;
#74334 = AXIS2_PLACEMENT_3D('',#120018,#93413,#93414) ;
#74335 = AXIS2_PLACEMENT_3D('',#120019,#93415,#93416) ;
#74336 = AXIS2_PLACEMENT_3D('',#120020,#93417,#93418) ;
#74337 = AXIS2_PLACEMENT_3D('',#120021,#93419,#93420) ;
#74338 = AXIS2_PLACEMENT_3D('',#120022,#93421,#93422) ;
#74339 = AXIS2_PLACEMENT_3D('',#120023,#93423,#93424) ;
#74340 = AXIS2_PLACEMENT_3D('',#120024,#93425,#93426) ;
#74341 = AXIS2_PLACEMENT_3D('',#120025,#93427,#93428) ;
#74342 = AXIS2_PLACEMENT_3D('',#120026,#93429,#93430) ;
#74343 = AXIS2_PLACEMENT_3D('',#120027,#93431,#93432) ;
#74344 = AXIS2_PLACEMENT_3D('',#120028,#93433,#93434) ;
#74345 = AXIS2_PLACEMENT_3D('',#120030,#93435,#93436) ;
#74346 = AXIS2_PLACEMENT_3D('',#120031,#93437,#93438) ;
#74347 = AXIS2_PLACEMENT_3D('',#120032,#93439,#93440) ;
#74348 = AXIS2_PLACEMENT_3D('',#120033,#93441,#93442) ;
#74349 = AXIS2_PLACEMENT_3D('',#120034,#93443,#93444) ;
#74350 = AXIS2_PLACEMENT_3D('',#120035,#93445,#93446) ;
#74351 = AXIS2_PLACEMENT_3D('',#120036,#93447,#93448) ;
#74352 = AXIS2_PLACEMENT_3D('',#120037,#93449,#93450) ;
#74353 = AXIS2_PLACEMENT_3D('',#120038,#93451,#93452) ;
#74354 = AXIS2_PLACEMENT_3D('',#120049,#93454,#93455) ;
#74355 = AXIS2_PLACEMENT_3D('',#120106,#93457,#93458) ;
#74356 = AXIS2_PLACEMENT_3D('',#120107,#93459,#93460) ;
#74357 = AXIS2_PLACEMENT_3D('',#120108,#93461,#93462) ;
#74358 = AXIS2_PLACEMENT_3D('',#120109,#93463,#93464) ;
#74359 = AXIS2_PLACEMENT_3D('',#120110,#93465,#93466) ;
#74360 = AXIS2_PLACEMENT_3D('',#120111,#93467,#93468) ;
#74361 = AXIS2_PLACEMENT_3D('',#120112,#93469,#93470) ;
#74362 = AXIS2_PLACEMENT_3D('',#120113,#93471,#93472) ;
#74363 = AXIS2_PLACEMENT_3D('',#120114,#93473,#93474) ;
#74364 = AXIS2_PLACEMENT_3D('',#120115,#93475,#93476) ;
#74365 = AXIS2_PLACEMENT_3D('',#120116,#93477,#93478) ;
#74366 = AXIS2_PLACEMENT_3D('',#120117,#93479,#93480) ;
#74367 = AXIS2_PLACEMENT_3D('',#120118,#93481,#93482) ;
#74368 = AXIS2_PLACEMENT_3D('',#120119,#93483,#93484) ;
#74369 = AXIS2_PLACEMENT_3D('',#120120,#93485,#93486) ;
#74370 = AXIS2_PLACEMENT_3D('',#120121,#93487,#93488) ;
#74371 = AXIS2_PLACEMENT_3D('',#120122,#93489,#93490) ;
#74372 = AXIS2_PLACEMENT_3D('',#120123,#93491,#93492) ;
#74373 = AXIS2_PLACEMENT_3D('',#120124,#93493,#93494) ;
#74374 = AXIS2_PLACEMENT_3D('',#120125,#93495,#93496) ;
#74375 = AXIS2_PLACEMENT_3D('',#120126,#93497,#93498) ;
#74376 = AXIS2_PLACEMENT_3D('',#120127,#93499,#93500) ;
#74377 = AXIS2_PLACEMENT_3D('',#120128,#93501,#93502) ;
#74378 = AXIS2_PLACEMENT_3D('',#120131,#93504,#93505) ;
#74379 = AXIS2_PLACEMENT_3D('',#120132,#93506,#93507) ;
#74380 = AXIS2_PLACEMENT_3D('',#120133,#93508,#93509) ;
#74381 = AXIS2_PLACEMENT_3D('',#120134,#93510,#93511) ;
#74382 = AXIS2_PLACEMENT_3D('',#120135,#93512,#93513) ;
#74383 = AXIS2_PLACEMENT_3D('',#120136,#93514,#93515) ;
#74384 = AXIS2_PLACEMENT_3D('',#120137,#93516,#93517) ;
#74385 = AXIS2_PLACEMENT_3D('',#120138,#93518,#93519) ;
#74386 = AXIS2_PLACEMENT_3D('',#120139,#93520,#93521) ;
#74387 = AXIS2_PLACEMENT_3D('',#120140,#93522,#93523) ;
#74388 = AXIS2_PLACEMENT_3D('',#120141,#93524,#93525) ;
#74389 = AXIS2_PLACEMENT_3D('',#120142,#93526,#93527) ;
#74390 = AXIS2_PLACEMENT_3D('',#120143,#93528,#93529) ;
#74391 = AXIS2_PLACEMENT_3D('',#120144,#93530,#93531) ;
#74392 = AXIS2_PLACEMENT_3D('',#120145,#93532,#93533) ;
#74393 = AXIS2_PLACEMENT_3D('',#120146,#93534,#93535) ;
#74394 = AXIS2_PLACEMENT_3D('',#120148,#93536,#93537) ;
#74395 = AXIS2_PLACEMENT_3D('',#120149,#93538,#93539) ;
#74396 = AXIS2_PLACEMENT_3D('',#120150,#93540,#93541) ;
#74397 = AXIS2_PLACEMENT_3D('',#120151,#93542,#93543) ;
#74398 = AXIS2_PLACEMENT_3D('',#120152,#93544,#93545) ;
#74399 = AXIS2_PLACEMENT_3D('',#120153,#93546,#93547) ;
#74400 = AXIS2_PLACEMENT_3D('',#120154,#93548,#93549) ;
#74401 = AXIS2_PLACEMENT_3D('',#120155,#93550,#93551) ;
#74402 = AXIS2_PLACEMENT_3D('',#120156,#93552,#93553) ;
#74403 = AXIS2_PLACEMENT_3D('',#120157,#93554,#93555) ;
#74404 = AXIS2_PLACEMENT_3D('',#120158,#93556,#93557) ;
#74405 = AXIS2_PLACEMENT_3D('',#120159,#93558,#93559) ;
#74406 = AXIS2_PLACEMENT_3D('',#120160,#93560,#93561) ;
#74407 = AXIS2_PLACEMENT_3D('',#120163,#93563,#93564) ;
#74408 = AXIS2_PLACEMENT_3D('',#120164,#93565,#93566) ;
#74409 = AXIS2_PLACEMENT_3D('',#120165,#93567,#93568) ;
#74410 = AXIS2_PLACEMENT_3D('',#120166,#93569,#93570) ;
#74411 = AXIS2_PLACEMENT_3D('',#120167,#93571,#93572) ;
#74412 = AXIS2_PLACEMENT_3D('',#120168,#93573,#93574) ;
#74413 = AXIS2_PLACEMENT_3D('',#120169,#93575,#93576) ;
#74414 = AXIS2_PLACEMENT_3D('',#120170,#93577,#93578) ;
#74415 = AXIS2_PLACEMENT_3D('',#120171,#93579,#93580) ;
#74416 = AXIS2_PLACEMENT_3D('',#120172,#93581,#93582) ;
#74417 = AXIS2_PLACEMENT_3D('',#120173,#93583,#93584) ;
#74418 = AXIS2_PLACEMENT_3D('',#120174,#93585,#93586) ;
#74419 = AXIS2_PLACEMENT_3D('',#120175,#93587,#93588) ;
#74420 = AXIS2_PLACEMENT_3D('',#120177,#93589,#93590) ;
#74421 = AXIS2_PLACEMENT_3D('',#120178,#93591,#93592) ;
#74422 = AXIS2_PLACEMENT_3D('',#120179,#93593,#93594) ;
#74423 = AXIS2_PLACEMENT_3D('',#120180,#93595,#93596) ;
#74424 = AXIS2_PLACEMENT_3D('',#120181,#93597,#93598) ;
#74425 = AXIS2_PLACEMENT_3D('',#120182,#93599,#93600) ;
#74426 = AXIS2_PLACEMENT_3D('',#120183,#93601,#93602) ;
#74427 = AXIS2_PLACEMENT_3D('',#120184,#93603,#93604) ;
#74428 = AXIS2_PLACEMENT_3D('',#120185,#93605,#93606) ;
#74429 = AXIS2_PLACEMENT_3D('',#120186,#93607,#93608) ;
#74430 = AXIS2_PLACEMENT_3D('',#120187,#93609,#93610) ;
#74431 = AXIS2_PLACEMENT_3D('',#120189,#93612,#93613) ;
#74432 = AXIS2_PLACEMENT_3D('',#120190,#93614,#93615) ;
#74433 = AXIS2_PLACEMENT_3D('',#120191,#93616,#93617) ;
#74434 = AXIS2_PLACEMENT_3D('',#120192,#93618,#93619) ;
#74435 = AXIS2_PLACEMENT_3D('',#120193,#93620,#93621) ;
#74436 = AXIS2_PLACEMENT_3D('',#120194,#93622,#93623) ;
#74437 = AXIS2_PLACEMENT_3D('',#120195,#93624,#93625) ;
#74438 = AXIS2_PLACEMENT_3D('',#120196,#93626,#93627) ;
#74439 = AXIS2_PLACEMENT_3D('',#120197,#93628,#93629) ;
#74440 = AXIS2_PLACEMENT_3D('',#120198,#93630,#93631) ;
#74441 = AXIS2_PLACEMENT_3D('',#120199,#93632,#93633) ;
#74442 = AXIS2_PLACEMENT_3D('',#120200,#93634,#93635) ;
#74443 = AXIS2_PLACEMENT_3D('',#120201,#93636,#93637) ;
#74444 = AXIS2_PLACEMENT_3D('',#120202,#93638,#93639) ;
#74445 = AXIS2_PLACEMENT_3D('',#120203,#93640,#93641) ;
#74446 = AXIS2_PLACEMENT_3D('',#120204,#93642,#93643) ;
#74447 = AXIS2_PLACEMENT_3D('',#120205,#93644,#93645) ;
#74448 = AXIS2_PLACEMENT_3D('',#120206,#93646,#93647) ;
#74449 = AXIS2_PLACEMENT_3D('',#120207,#93648,#93649) ;
#74450 = AXIS2_PLACEMENT_3D('',#120208,#93650,#93651) ;
#74451 = AXIS2_PLACEMENT_3D('',#120209,#93652,#93653) ;
#74452 = AXIS2_PLACEMENT_3D('',#120210,#93654,#93655) ;
#74453 = AXIS2_PLACEMENT_3D('',#120211,#93656,#93657) ;
#74454 = AXIS2_PLACEMENT_3D('',#120212,#93658,#93659) ;
#74455 = AXIS2_PLACEMENT_3D('',#120213,#93660,#93661) ;
#74456 = AXIS2_PLACEMENT_3D('',#120214,#93662,#93663) ;
#74457 = AXIS2_PLACEMENT_3D('',#120215,#93664,#93665) ;
#74458 = AXIS2_PLACEMENT_3D('',#120216,#93666,#93667) ;
#74459 = AXIS2_PLACEMENT_3D('',#120217,#93668,#93669) ;
#74460 = AXIS2_PLACEMENT_3D('',#120218,#93670,#93671) ;
#74461 = AXIS2_PLACEMENT_3D('',#120219,#93672,#93673) ;
#74462 = AXIS2_PLACEMENT_3D('',#120220,#93674,#93675) ;
#74463 = AXIS2_PLACEMENT_3D('',#120221,#93676,#93677) ;
#74464 = AXIS2_PLACEMENT_3D('',#120222,#93678,#93679) ;
#74465 = AXIS2_PLACEMENT_3D('',#120223,#93680,#93681) ;
#74466 = AXIS2_PLACEMENT_3D('',#120224,#93682,#93683) ;
#74467 = AXIS2_PLACEMENT_3D('',#120225,#93684,#93685) ;
#74468 = AXIS2_PLACEMENT_3D('',#120226,#93686,#93687) ;
#74469 = AXIS2_PLACEMENT_3D('',#120227,#93688,#93689) ;
#74470 = AXIS2_PLACEMENT_3D('',#120228,#93690,#93691) ;
#74471 = AXIS2_PLACEMENT_3D('',#120229,#93692,#93693) ;
#74472 = AXIS2_PLACEMENT_3D('',#120230,#93694,#93695) ;
#74473 = AXIS2_PLACEMENT_3D('',#120231,#93696,#93697) ;
#74474 = AXIS2_PLACEMENT_3D('',#120232,#93698,#93699) ;
#74475 = AXIS2_PLACEMENT_3D('',#120233,#93700,#93701) ;
#74476 = AXIS2_PLACEMENT_3D('',#120234,#93702,#93703) ;
#74477 = AXIS2_PLACEMENT_3D('',#120235,#93704,#93705) ;
#74478 = AXIS2_PLACEMENT_3D('',#120236,#93706,#93707) ;
#74479 = AXIS2_PLACEMENT_3D('',#120237,#93708,#93709) ;
#74480 = AXIS2_PLACEMENT_3D('',#120238,#93710,#93711) ;
#74481 = AXIS2_PLACEMENT_3D('',#120239,#93712,#93713) ;
#74482 = AXIS2_PLACEMENT_3D('',#120240,#93714,#93715) ;
#74483 = AXIS2_PLACEMENT_3D('',#120241,#93716,#93717) ;
#74484 = AXIS2_PLACEMENT_3D('',#120242,#93718,#93719) ;
#74485 = AXIS2_PLACEMENT_3D('',#120243,#93720,#93721) ;
#74486 = AXIS2_PLACEMENT_3D('',#120244,#93722,#93723) ;
#74487 = AXIS2_PLACEMENT_3D('',#120245,#93724,#93725) ;
#74488 = AXIS2_PLACEMENT_3D('',#120246,#93726,#93727) ;
#74489 = AXIS2_PLACEMENT_3D('',#120247,#93728,#93729) ;
#74490 = AXIS2_PLACEMENT_3D('',#120248,#93730,#93731) ;
#74491 = AXIS2_PLACEMENT_3D('',#120249,#93732,#93733) ;
#74492 = AXIS2_PLACEMENT_3D('',#120250,#93734,#93735) ;
#74493 = AXIS2_PLACEMENT_3D('',#120251,#93736,#93737) ;
#74494 = AXIS2_PLACEMENT_3D('',#120252,#93738,#93739) ;
#74495 = AXIS2_PLACEMENT_3D('',#120253,#93740,#93741) ;
#74496 = AXIS2_PLACEMENT_3D('',#120254,#93742,#93743) ;
#74497 = AXIS2_PLACEMENT_3D('',#120255,#93744,#93745) ;
#74498 = AXIS2_PLACEMENT_3D('',#120257,#93746,#93747) ;
#74499 = AXIS2_PLACEMENT_3D('',#120258,#93748,#93749) ;
#74500 = AXIS2_PLACEMENT_3D('',#120259,#93750,#93751) ;
#74501 = AXIS2_PLACEMENT_3D('',#120260,#93752,#93753) ;
#74502 = AXIS2_PLACEMENT_3D('',#120261,#93754,#93755) ;
#74503 = AXIS2_PLACEMENT_3D('',#120262,#93756,#93757) ;
#74504 = AXIS2_PLACEMENT_3D('',#120263,#93758,#93759) ;
#74505 = AXIS2_PLACEMENT_3D('',#120264,#93760,#93761) ;
#74506 = AXIS2_PLACEMENT_3D('',#120265,#93762,#93763) ;
#74507 = AXIS2_PLACEMENT_3D('',#120276,#93765,#93766) ;
#74508 = AXIS2_PLACEMENT_3D('',#120333,#93768,#93769) ;
#74509 = AXIS2_PLACEMENT_3D('',#120334,#93770,#93771) ;
#74510 = AXIS2_PLACEMENT_3D('',#120335,#93772,#93773) ;
#74511 = AXIS2_PLACEMENT_3D('',#120336,#93774,#93775) ;
#74512 = AXIS2_PLACEMENT_3D('',#120337,#93776,#93777) ;
#74513 = AXIS2_PLACEMENT_3D('',#120338,#93778,#93779) ;
#74514 = AXIS2_PLACEMENT_3D('',#120339,#93780,#93781) ;
#74515 = AXIS2_PLACEMENT_3D('',#120340,#93782,#93783) ;
#74516 = AXIS2_PLACEMENT_3D('',#120341,#93784,#93785) ;
#74517 = AXIS2_PLACEMENT_3D('',#120342,#93786,#93787) ;
#74518 = AXIS2_PLACEMENT_3D('',#120343,#93788,#93789) ;
#74519 = AXIS2_PLACEMENT_3D('',#120344,#93790,#93791) ;
#74520 = AXIS2_PLACEMENT_3D('',#120345,#93792,#93793) ;
#74521 = AXIS2_PLACEMENT_3D('',#120346,#93794,#93795) ;
#74522 = AXIS2_PLACEMENT_3D('',#120347,#93796,#93797) ;
#74523 = AXIS2_PLACEMENT_3D('',#120348,#93798,#93799) ;
#74524 = AXIS2_PLACEMENT_3D('',#120349,#93800,#93801) ;
#74525 = AXIS2_PLACEMENT_3D('',#120350,#93802,#93803) ;
#74526 = AXIS2_PLACEMENT_3D('',#120351,#93804,#93805) ;
#74527 = AXIS2_PLACEMENT_3D('',#120352,#93806,#93807) ;
#74528 = AXIS2_PLACEMENT_3D('',#120353,#93808,#93809) ;
#74529 = AXIS2_PLACEMENT_3D('',#120354,#93810,#93811) ;
#74530 = AXIS2_PLACEMENT_3D('',#120355,#93812,#93813) ;
#74531 = AXIS2_PLACEMENT_3D('',#120358,#93815,#93816) ;
#74532 = AXIS2_PLACEMENT_3D('',#120359,#93817,#93818) ;
#74533 = AXIS2_PLACEMENT_3D('',#120360,#93819,#93820) ;
#74534 = AXIS2_PLACEMENT_3D('',#120361,#93821,#93822) ;
#74535 = AXIS2_PLACEMENT_3D('',#120362,#93823,#93824) ;
#74536 = AXIS2_PLACEMENT_3D('',#120363,#93825,#93826) ;
#74537 = AXIS2_PLACEMENT_3D('',#120364,#93827,#93828) ;
#74538 = AXIS2_PLACEMENT_3D('',#120365,#93829,#93830) ;
#74539 = AXIS2_PLACEMENT_3D('',#120366,#93831,#93832) ;
#74540 = AXIS2_PLACEMENT_3D('',#120367,#93833,#93834) ;
#74541 = AXIS2_PLACEMENT_3D('',#120368,#93835,#93836) ;
#74542 = AXIS2_PLACEMENT_3D('',#120369,#93837,#93838) ;
#74543 = AXIS2_PLACEMENT_3D('',#120370,#93839,#93840) ;
#74544 = AXIS2_PLACEMENT_3D('',#120371,#93841,#93842) ;
#74545 = AXIS2_PLACEMENT_3D('',#120372,#93843,#93844) ;
#74546 = AXIS2_PLACEMENT_3D('',#120373,#93845,#93846) ;
#74547 = AXIS2_PLACEMENT_3D('',#120375,#93847,#93848) ;
#74548 = AXIS2_PLACEMENT_3D('',#120376,#93849,#93850) ;
#74549 = AXIS2_PLACEMENT_3D('',#120377,#93851,#93852) ;
#74550 = AXIS2_PLACEMENT_3D('',#120378,#93853,#93854) ;
#74551 = AXIS2_PLACEMENT_3D('',#120379,#93855,#93856) ;
#74552 = AXIS2_PLACEMENT_3D('',#120380,#93857,#93858) ;
#74553 = AXIS2_PLACEMENT_3D('',#120381,#93859,#93860) ;
#74554 = AXIS2_PLACEMENT_3D('',#120382,#93861,#93862) ;
#74555 = AXIS2_PLACEMENT_3D('',#120383,#93863,#93864) ;
#74556 = AXIS2_PLACEMENT_3D('',#120384,#93865,#93866) ;
#74557 = AXIS2_PLACEMENT_3D('',#120385,#93867,#93868) ;
#74558 = AXIS2_PLACEMENT_3D('',#120386,#93869,#93870) ;
#74559 = AXIS2_PLACEMENT_3D('',#120387,#93871,#93872) ;
#74560 = AXIS2_PLACEMENT_3D('',#120390,#93874,#93875) ;
#74561 = AXIS2_PLACEMENT_3D('',#120391,#93876,#93877) ;
#74562 = AXIS2_PLACEMENT_3D('',#120392,#93878,#93879) ;
#74563 = AXIS2_PLACEMENT_3D('',#120393,#93880,#93881) ;
#74564 = AXIS2_PLACEMENT_3D('',#120394,#93882,#93883) ;
#74565 = AXIS2_PLACEMENT_3D('',#120395,#93884,#93885) ;
#74566 = AXIS2_PLACEMENT_3D('',#120396,#93886,#93887) ;
#74567 = AXIS2_PLACEMENT_3D('',#120397,#93888,#93889) ;
#74568 = AXIS2_PLACEMENT_3D('',#120398,#93890,#93891) ;
#74569 = AXIS2_PLACEMENT_3D('',#120399,#93892,#93893) ;
#74570 = AXIS2_PLACEMENT_3D('',#120400,#93894,#93895) ;
#74571 = AXIS2_PLACEMENT_3D('',#120401,#93896,#93897) ;
#74572 = AXIS2_PLACEMENT_3D('',#120402,#93898,#93899) ;
#74573 = AXIS2_PLACEMENT_3D('',#120404,#93900,#93901) ;
#74574 = AXIS2_PLACEMENT_3D('',#120405,#93902,#93903) ;
#74575 = AXIS2_PLACEMENT_3D('',#120406,#93904,#93905) ;
#74576 = AXIS2_PLACEMENT_3D('',#120407,#93906,#93907) ;
#74577 = AXIS2_PLACEMENT_3D('',#120408,#93908,#93909) ;
#74578 = AXIS2_PLACEMENT_3D('',#120409,#93910,#93911) ;
#74579 = AXIS2_PLACEMENT_3D('',#120410,#93912,#93913) ;
#74580 = AXIS2_PLACEMENT_3D('',#120411,#93914,#93915) ;
#74581 = AXIS2_PLACEMENT_3D('',#120412,#93916,#93917) ;
#74582 = AXIS2_PLACEMENT_3D('',#120413,#93918,#93919) ;
#74583 = AXIS2_PLACEMENT_3D('',#120414,#93920,#93921) ;
#74584 = AXIS2_PLACEMENT_3D('',#120416,#93923,#93924) ;
#74585 = AXIS2_PLACEMENT_3D('',#120417,#93925,#93926) ;
#74586 = AXIS2_PLACEMENT_3D('',#120418,#93927,#93928) ;
#74587 = AXIS2_PLACEMENT_3D('',#120419,#93929,#93930) ;
#74588 = AXIS2_PLACEMENT_3D('',#120420,#93931,#93932) ;
#74589 = AXIS2_PLACEMENT_3D('',#120421,#93933,#93934) ;
#74590 = AXIS2_PLACEMENT_3D('',#120422,#93935,#93936) ;
#74591 = AXIS2_PLACEMENT_3D('',#120423,#93937,#93938) ;
#74592 = AXIS2_PLACEMENT_3D('',#120424,#93939,#93940) ;
#74593 = AXIS2_PLACEMENT_3D('',#120425,#93941,#93942) ;
#74594 = AXIS2_PLACEMENT_3D('',#120426,#93943,#93944) ;
#74595 = AXIS2_PLACEMENT_3D('',#120427,#93945,#93946) ;
#74596 = AXIS2_PLACEMENT_3D('',#120428,#93947,#93948) ;
#74597 = AXIS2_PLACEMENT_3D('',#120429,#93949,#93950) ;
#74598 = AXIS2_PLACEMENT_3D('',#120430,#93951,#93952) ;
#74599 = AXIS2_PLACEMENT_3D('',#120431,#93953,#93954) ;
#74600 = AXIS2_PLACEMENT_3D('',#120432,#93955,#93956) ;
#74601 = AXIS2_PLACEMENT_3D('',#120433,#93957,#93958) ;
#74602 = AXIS2_PLACEMENT_3D('',#120434,#93959,#93960) ;
#74603 = AXIS2_PLACEMENT_3D('',#120435,#93961,#93962) ;
#74604 = AXIS2_PLACEMENT_3D('',#120436,#93963,#93964) ;
#74605 = AXIS2_PLACEMENT_3D('',#120437,#93965,#93966) ;
#74606 = AXIS2_PLACEMENT_3D('',#120438,#93967,#93968) ;
#74607 = AXIS2_PLACEMENT_3D('',#120439,#93969,#93970) ;
#74608 = AXIS2_PLACEMENT_3D('',#120440,#93971,#93972) ;
#74609 = AXIS2_PLACEMENT_3D('',#120441,#93973,#93974) ;
#74610 = AXIS2_PLACEMENT_3D('',#120442,#93975,#93976) ;
#74611 = AXIS2_PLACEMENT_3D('',#120443,#93977,#93978) ;
#74612 = AXIS2_PLACEMENT_3D('',#120444,#93979,#93980) ;
#74613 = AXIS2_PLACEMENT_3D('',#120445,#93981,#93982) ;
#74614 = AXIS2_PLACEMENT_3D('',#120446,#93983,#93984) ;
#74615 = AXIS2_PLACEMENT_3D('',#120447,#93985,#93986) ;
#74616 = AXIS2_PLACEMENT_3D('',#120448,#93987,#93988) ;
#74617 = AXIS2_PLACEMENT_3D('',#120449,#93989,#93990) ;
#74618 = AXIS2_PLACEMENT_3D('',#120450,#93991,#93992) ;
#74619 = AXIS2_PLACEMENT_3D('',#120451,#93993,#93994) ;
#74620 = AXIS2_PLACEMENT_3D('',#120452,#93995,#93996) ;
#74621 = AXIS2_PLACEMENT_3D('',#120453,#93997,#93998) ;
#74622 = AXIS2_PLACEMENT_3D('',#120454,#93999,#94000) ;
#74623 = AXIS2_PLACEMENT_3D('',#120455,#94001,#94002) ;
#74624 = AXIS2_PLACEMENT_3D('',#120456,#94003,#94004) ;
#74625 = AXIS2_PLACEMENT_3D('',#120457,#94005,#94006) ;
#74626 = AXIS2_PLACEMENT_3D('',#120458,#94007,#94008) ;
#74627 = AXIS2_PLACEMENT_3D('',#120459,#94009,#94010) ;
#74628 = AXIS2_PLACEMENT_3D('',#120460,#94011,#94012) ;
#74629 = AXIS2_PLACEMENT_3D('',#120461,#94013,#94014) ;
#74630 = AXIS2_PLACEMENT_3D('',#120462,#94015,#94016) ;
#74631 = AXIS2_PLACEMENT_3D('',#120463,#94017,#94018) ;
#74632 = AXIS2_PLACEMENT_3D('',#120464,#94019,#94020) ;
#74633 = AXIS2_PLACEMENT_3D('',#120465,#94021,#94022) ;
#74634 = AXIS2_PLACEMENT_3D('',#120466,#94023,#94024) ;
#74635 = AXIS2_PLACEMENT_3D('',#120467,#94025,#94026) ;
#74636 = AXIS2_PLACEMENT_3D('',#120468,#94027,#94028) ;
#74637 = AXIS2_PLACEMENT_3D('',#120469,#94029,#94030) ;
#74638 = AXIS2_PLACEMENT_3D('',#120470,#94031,#94032) ;
#74639 = AXIS2_PLACEMENT_3D('',#120471,#94033,#94034) ;
#74640 = AXIS2_PLACEMENT_3D('',#120472,#94035,#94036) ;
#74641 = AXIS2_PLACEMENT_3D('',#120473,#94037,#94038) ;
#74642 = AXIS2_PLACEMENT_3D('',#120474,#94039,#94040) ;
#74643 = AXIS2_PLACEMENT_3D('',#120475,#94041,#94042) ;
#74644 = AXIS2_PLACEMENT_3D('',#120476,#94043,#94044) ;
#74645 = AXIS2_PLACEMENT_3D('',#120477,#94045,#94046) ;
#74646 = AXIS2_PLACEMENT_3D('',#120478,#94047,#94048) ;
#74647 = AXIS2_PLACEMENT_3D('',#120479,#94049,#94050) ;
#74648 = AXIS2_PLACEMENT_3D('',#120480,#94051,#94052) ;
#74649 = AXIS2_PLACEMENT_3D('',#120481,#94053,#94054) ;
#74650 = AXIS2_PLACEMENT_3D('',#120482,#94055,#94056) ;
#74651 = AXIS2_PLACEMENT_3D('',#120484,#94057,#94058) ;
#74652 = AXIS2_PLACEMENT_3D('',#120485,#94059,#94060) ;
#74653 = AXIS2_PLACEMENT_3D('',#120486,#94061,#94062) ;
#74654 = AXIS2_PLACEMENT_3D('',#120487,#94063,#94064) ;
#74655 = AXIS2_PLACEMENT_3D('',#120488,#94065,#94066) ;
#74656 = AXIS2_PLACEMENT_3D('',#120489,#94067,#94068) ;
#74657 = AXIS2_PLACEMENT_3D('',#120490,#94069,#94070) ;
#74658 = AXIS2_PLACEMENT_3D('',#120491,#94071,#94072) ;
#74659 = AXIS2_PLACEMENT_3D('',#120492,#94073,#94074) ;
#74660 = AXIS2_PLACEMENT_3D('',#120503,#94076,#94077) ;
#74661 = AXIS2_PLACEMENT_3D('',#120560,#94079,#94080) ;
#74662 = AXIS2_PLACEMENT_3D('',#120561,#94081,#94082) ;
#74663 = AXIS2_PLACEMENT_3D('',#120562,#94083,#94084) ;
#74664 = AXIS2_PLACEMENT_3D('',#120563,#94085,#94086) ;
#74665 = AXIS2_PLACEMENT_3D('',#120564,#94087,#94088) ;
#74666 = AXIS2_PLACEMENT_3D('',#120565,#94089,#94090) ;
#74667 = AXIS2_PLACEMENT_3D('',#120566,#94091,#94092) ;
#74668 = AXIS2_PLACEMENT_3D('',#120567,#94093,#94094) ;
#74669 = AXIS2_PLACEMENT_3D('',#120568,#94095,#94096) ;
#74670 = AXIS2_PLACEMENT_3D('',#120569,#94097,#94098) ;
#74671 = AXIS2_PLACEMENT_3D('',#120570,#94099,#94100) ;
#74672 = AXIS2_PLACEMENT_3D('',#120571,#94101,#94102) ;
#74673 = AXIS2_PLACEMENT_3D('',#120572,#94103,#94104) ;
#74674 = AXIS2_PLACEMENT_3D('',#120573,#94105,#94106) ;
#74675 = AXIS2_PLACEMENT_3D('',#120574,#94107,#94108) ;
#74676 = AXIS2_PLACEMENT_3D('',#120575,#94109,#94110) ;
#74677 = AXIS2_PLACEMENT_3D('',#120576,#94111,#94112) ;
#74678 = AXIS2_PLACEMENT_3D('',#120577,#94113,#94114) ;
#74679 = AXIS2_PLACEMENT_3D('',#120578,#94115,#94116) ;
#74680 = AXIS2_PLACEMENT_3D('',#120579,#94117,#94118) ;
#74681 = AXIS2_PLACEMENT_3D('',#120580,#94119,#94120) ;
#74682 = AXIS2_PLACEMENT_3D('',#120581,#94121,#94122) ;
#74683 = AXIS2_PLACEMENT_3D('',#120582,#94123,#94124) ;
#74684 = AXIS2_PLACEMENT_3D('',#120585,#94126,#94127) ;
#74685 = AXIS2_PLACEMENT_3D('',#120586,#94128,#94129) ;
#74686 = AXIS2_PLACEMENT_3D('',#120587,#94130,#94131) ;
#74687 = AXIS2_PLACEMENT_3D('',#120588,#94132,#94133) ;
#74688 = AXIS2_PLACEMENT_3D('',#120589,#94134,#94135) ;
#74689 = AXIS2_PLACEMENT_3D('',#120590,#94136,#94137) ;
#74690 = AXIS2_PLACEMENT_3D('',#120591,#94138,#94139) ;
#74691 = AXIS2_PLACEMENT_3D('',#120592,#94140,#94141) ;
#74692 = AXIS2_PLACEMENT_3D('',#120593,#94142,#94143) ;
#74693 = AXIS2_PLACEMENT_3D('',#120594,#94144,#94145) ;
#74694 = AXIS2_PLACEMENT_3D('',#120595,#94146,#94147) ;
#74695 = AXIS2_PLACEMENT_3D('',#120596,#94148,#94149) ;
#74696 = AXIS2_PLACEMENT_3D('',#120597,#94150,#94151) ;
#74697 = AXIS2_PLACEMENT_3D('',#120598,#94152,#94153) ;
#74698 = AXIS2_PLACEMENT_3D('',#120599,#94154,#94155) ;
#74699 = AXIS2_PLACEMENT_3D('',#120600,#94156,#94157) ;
#74700 = AXIS2_PLACEMENT_3D('',#120602,#94158,#94159) ;
#74701 = AXIS2_PLACEMENT_3D('',#120603,#94160,#94161) ;
#74702 = AXIS2_PLACEMENT_3D('',#120604,#94162,#94163) ;
#74703 = AXIS2_PLACEMENT_3D('',#120605,#94164,#94165) ;
#74704 = AXIS2_PLACEMENT_3D('',#120606,#94166,#94167) ;
#74705 = AXIS2_PLACEMENT_3D('',#120607,#94168,#94169) ;
#74706 = AXIS2_PLACEMENT_3D('',#120608,#94170,#94171) ;
#74707 = AXIS2_PLACEMENT_3D('',#120609,#94172,#94173) ;
#74708 = AXIS2_PLACEMENT_3D('',#120610,#94174,#94175) ;
#74709 = AXIS2_PLACEMENT_3D('',#120611,#94176,#94177) ;
#74710 = AXIS2_PLACEMENT_3D('',#120612,#94178,#94179) ;
#74711 = AXIS2_PLACEMENT_3D('',#120613,#94180,#94181) ;
#74712 = AXIS2_PLACEMENT_3D('',#120614,#94182,#94183) ;
#74713 = AXIS2_PLACEMENT_3D('',#120617,#94185,#94186) ;
#74714 = AXIS2_PLACEMENT_3D('',#120618,#94187,#94188) ;
#74715 = AXIS2_PLACEMENT_3D('',#120619,#94189,#94190) ;
#74716 = AXIS2_PLACEMENT_3D('',#120620,#94191,#94192) ;
#74717 = AXIS2_PLACEMENT_3D('',#120621,#94193,#94194) ;
#74718 = AXIS2_PLACEMENT_3D('',#120622,#94195,#94196) ;
#74719 = AXIS2_PLACEMENT_3D('',#120623,#94197,#94198) ;
#74720 = AXIS2_PLACEMENT_3D('',#120624,#94199,#94200) ;
#74721 = AXIS2_PLACEMENT_3D('',#120625,#94201,#94202) ;
#74722 = AXIS2_PLACEMENT_3D('',#120626,#94203,#94204) ;
#74723 = AXIS2_PLACEMENT_3D('',#120627,#94205,#94206) ;
#74724 = AXIS2_PLACEMENT_3D('',#120628,#94207,#94208) ;
#74725 = AXIS2_PLACEMENT_3D('',#120629,#94209,#94210) ;
#74726 = AXIS2_PLACEMENT_3D('',#120631,#94211,#94212) ;
#74727 = AXIS2_PLACEMENT_3D('',#120632,#94213,#94214) ;
#74728 = AXIS2_PLACEMENT_3D('',#120633,#94215,#94216) ;
#74729 = AXIS2_PLACEMENT_3D('',#120634,#94217,#94218) ;
#74730 = AXIS2_PLACEMENT_3D('',#120635,#94219,#94220) ;
#74731 = AXIS2_PLACEMENT_3D('',#120636,#94221,#94222) ;
#74732 = AXIS2_PLACEMENT_3D('',#120637,#94223,#94224) ;
#74733 = AXIS2_PLACEMENT_3D('',#120638,#94225,#94226) ;
#74734 = AXIS2_PLACEMENT_3D('',#120639,#94227,#94228) ;
#74735 = AXIS2_PLACEMENT_3D('',#120640,#94229,#94230) ;
#74736 = AXIS2_PLACEMENT_3D('',#120641,#94231,#94232) ;
#74737 = AXIS2_PLACEMENT_3D('',#120643,#94234,#94235) ;
#74738 = AXIS2_PLACEMENT_3D('',#120644,#94236,#94237) ;
#74739 = AXIS2_PLACEMENT_3D('',#120645,#94238,#94239) ;
#74740 = AXIS2_PLACEMENT_3D('',#120646,#94240,#94241) ;
#74741 = AXIS2_PLACEMENT_3D('',#120647,#94242,#94243) ;
#74742 = AXIS2_PLACEMENT_3D('',#120648,#94244,#94245) ;
#74743 = AXIS2_PLACEMENT_3D('',#120649,#94246,#94247) ;
#74744 = AXIS2_PLACEMENT_3D('',#120650,#94248,#94249) ;
#74745 = AXIS2_PLACEMENT_3D('',#120651,#94250,#94251) ;
#74746 = AXIS2_PLACEMENT_3D('',#120652,#94252,#94253) ;
#74747 = AXIS2_PLACEMENT_3D('',#120653,#94254,#94255) ;
#74748 = AXIS2_PLACEMENT_3D('',#120654,#94256,#94257) ;
#74749 = AXIS2_PLACEMENT_3D('',#120655,#94258,#94259) ;
#74750 = AXIS2_PLACEMENT_3D('',#120656,#94260,#94261) ;
#74751 = AXIS2_PLACEMENT_3D('',#120657,#94262,#94263) ;
#74752 = AXIS2_PLACEMENT_3D('',#120658,#94264,#94265) ;
#74753 = AXIS2_PLACEMENT_3D('',#120659,#94266,#94267) ;
#74754 = AXIS2_PLACEMENT_3D('',#120660,#94268,#94269) ;
#74755 = AXIS2_PLACEMENT_3D('',#120661,#94270,#94271) ;
#74756 = AXIS2_PLACEMENT_3D('',#120662,#94272,#94273) ;
#74757 = AXIS2_PLACEMENT_3D('',#120663,#94274,#94275) ;
#74758 = AXIS2_PLACEMENT_3D('',#120664,#94276,#94277) ;
#74759 = AXIS2_PLACEMENT_3D('',#120665,#94278,#94279) ;
#74760 = AXIS2_PLACEMENT_3D('',#120666,#94280,#94281) ;
#74761 = AXIS2_PLACEMENT_3D('',#120667,#94282,#94283) ;
#74762 = AXIS2_PLACEMENT_3D('',#120668,#94284,#94285) ;
#74763 = AXIS2_PLACEMENT_3D('',#120669,#94286,#94287) ;
#74764 = AXIS2_PLACEMENT_3D('',#120670,#94288,#94289) ;
#74765 = AXIS2_PLACEMENT_3D('',#120671,#94290,#94291) ;
#74766 = AXIS2_PLACEMENT_3D('',#120672,#94292,#94293) ;
#74767 = AXIS2_PLACEMENT_3D('',#120673,#94294,#94295) ;
#74768 = AXIS2_PLACEMENT_3D('',#120674,#94296,#94297) ;
#74769 = AXIS2_PLACEMENT_3D('',#120675,#94298,#94299) ;
#74770 = AXIS2_PLACEMENT_3D('',#120676,#94300,#94301) ;
#74771 = AXIS2_PLACEMENT_3D('',#120677,#94302,#94303) ;
#74772 = AXIS2_PLACEMENT_3D('',#120678,#94304,#94305) ;
#74773 = AXIS2_PLACEMENT_3D('',#120679,#94306,#94307) ;
#74774 = AXIS2_PLACEMENT_3D('',#120680,#94308,#94309) ;
#74775 = AXIS2_PLACEMENT_3D('',#120681,#94310,#94311) ;
#74776 = AXIS2_PLACEMENT_3D('',#120682,#94312,#94313) ;
#74777 = AXIS2_PLACEMENT_3D('',#120683,#94314,#94315) ;
#74778 = AXIS2_PLACEMENT_3D('',#120684,#94316,#94317) ;
#74779 = AXIS2_PLACEMENT_3D('',#120685,#94318,#94319) ;
#74780 = AXIS2_PLACEMENT_3D('',#120686,#94320,#94321) ;
#74781 = AXIS2_PLACEMENT_3D('',#120687,#94322,#94323) ;
#74782 = AXIS2_PLACEMENT_3D('',#120688,#94324,#94325) ;
#74783 = AXIS2_PLACEMENT_3D('',#120689,#94326,#94327) ;
#74784 = AXIS2_PLACEMENT_3D('',#120690,#94328,#94329) ;
#74785 = AXIS2_PLACEMENT_3D('',#120691,#94330,#94331) ;
#74786 = AXIS2_PLACEMENT_3D('',#120692,#94332,#94333) ;
#74787 = AXIS2_PLACEMENT_3D('',#120693,#94334,#94335) ;
#74788 = AXIS2_PLACEMENT_3D('',#120694,#94336,#94337) ;
#74789 = AXIS2_PLACEMENT_3D('',#120695,#94338,#94339) ;
#74790 = AXIS2_PLACEMENT_3D('',#120696,#94340,#94341) ;
#74791 = AXIS2_PLACEMENT_3D('',#120697,#94342,#94343) ;
#74792 = AXIS2_PLACEMENT_3D('',#120698,#94344,#94345) ;
#74793 = AXIS2_PLACEMENT_3D('',#120699,#94346,#94347) ;
#74794 = AXIS2_PLACEMENT_3D('',#120700,#94348,#94349) ;
#74795 = AXIS2_PLACEMENT_3D('',#120701,#94350,#94351) ;
#74796 = AXIS2_PLACEMENT_3D('',#120702,#94352,#94353) ;
#74797 = AXIS2_PLACEMENT_3D('',#120703,#94354,#94355) ;
#74798 = AXIS2_PLACEMENT_3D('',#120704,#94356,#94357) ;
#74799 = AXIS2_PLACEMENT_3D('',#120705,#94358,#94359) ;
#74800 = AXIS2_PLACEMENT_3D('',#120706,#94360,#94361) ;
#74801 = AXIS2_PLACEMENT_3D('',#120707,#94362,#94363) ;
#74802 = AXIS2_PLACEMENT_3D('',#120708,#94364,#94365) ;
#74803 = AXIS2_PLACEMENT_3D('',#120709,#94366,#94367) ;
#74804 = AXIS2_PLACEMENT_3D('',#120711,#94368,#94369) ;
#74805 = AXIS2_PLACEMENT_3D('',#120712,#94370,#94371) ;
#74806 = AXIS2_PLACEMENT_3D('',#120713,#94372,#94373) ;
#74807 = AXIS2_PLACEMENT_3D('',#120714,#94374,#94375) ;
#74808 = AXIS2_PLACEMENT_3D('',#120715,#94376,#94377) ;
#74809 = AXIS2_PLACEMENT_3D('',#120716,#94378,#94379) ;
#74810 = AXIS2_PLACEMENT_3D('',#120717,#94380,#94381) ;
#74811 = AXIS2_PLACEMENT_3D('',#120718,#94382,#94383) ;
#74812 = AXIS2_PLACEMENT_3D('',#120719,#94384,#94385) ;
#74813 = AXIS2_PLACEMENT_3D('',#120730,#94387,#94388) ;
#74814 = AXIS2_PLACEMENT_3D('',#120787,#94390,#94391) ;
#74815 = AXIS2_PLACEMENT_3D('',#120788,#94392,#94393) ;
#74816 = AXIS2_PLACEMENT_3D('',#120789,#94394,#94395) ;
#74817 = AXIS2_PLACEMENT_3D('',#120790,#94396,#94397) ;
#74818 = AXIS2_PLACEMENT_3D('',#120791,#94398,#94399) ;
#74819 = AXIS2_PLACEMENT_3D('',#120792,#94400,#94401) ;
#74820 = AXIS2_PLACEMENT_3D('',#120793,#94402,#94403) ;
#74821 = AXIS2_PLACEMENT_3D('',#120794,#94404,#94405) ;
#74822 = AXIS2_PLACEMENT_3D('',#120795,#94406,#94407) ;
#74823 = AXIS2_PLACEMENT_3D('',#120796,#94408,#94409) ;
#74824 = AXIS2_PLACEMENT_3D('',#120797,#94410,#94411) ;
#74825 = AXIS2_PLACEMENT_3D('',#120798,#94412,#94413) ;
#74826 = AXIS2_PLACEMENT_3D('',#120799,#94414,#94415) ;
#74827 = AXIS2_PLACEMENT_3D('',#120800,#94416,#94417) ;
#74828 = AXIS2_PLACEMENT_3D('',#120801,#94418,#94419) ;
#74829 = AXIS2_PLACEMENT_3D('',#120802,#94420,#94421) ;
#74830 = AXIS2_PLACEMENT_3D('',#120803,#94422,#94423) ;
#74831 = AXIS2_PLACEMENT_3D('',#120804,#94424,#94425) ;
#74832 = AXIS2_PLACEMENT_3D('',#120805,#94426,#94427) ;
#74833 = AXIS2_PLACEMENT_3D('',#120806,#94428,#94429) ;
#74834 = AXIS2_PLACEMENT_3D('',#120807,#94430,#94431) ;
#74835 = AXIS2_PLACEMENT_3D('',#120808,#94432,#94433) ;
#74836 = AXIS2_PLACEMENT_3D('',#120809,#94434,#94435) ;
#74837 = AXIS2_PLACEMENT_3D('',#120812,#94437,#94438) ;
#74838 = AXIS2_PLACEMENT_3D('',#120813,#94439,#94440) ;
#74839 = AXIS2_PLACEMENT_3D('',#120814,#94441,#94442) ;
#74840 = AXIS2_PLACEMENT_3D('',#120815,#94443,#94444) ;
#74841 = AXIS2_PLACEMENT_3D('',#120816,#94445,#94446) ;
#74842 = AXIS2_PLACEMENT_3D('',#120817,#94447,#94448) ;
#74843 = AXIS2_PLACEMENT_3D('',#120818,#94449,#94450) ;
#74844 = AXIS2_PLACEMENT_3D('',#120819,#94451,#94452) ;
#74845 = AXIS2_PLACEMENT_3D('',#120820,#94453,#94454) ;
#74846 = AXIS2_PLACEMENT_3D('',#120821,#94455,#94456) ;
#74847 = AXIS2_PLACEMENT_3D('',#120822,#94457,#94458) ;
#74848 = AXIS2_PLACEMENT_3D('',#120823,#94459,#94460) ;
#74849 = AXIS2_PLACEMENT_3D('',#120824,#94461,#94462) ;
#74850 = AXIS2_PLACEMENT_3D('',#120825,#94463,#94464) ;
#74851 = AXIS2_PLACEMENT_3D('',#120826,#94465,#94466) ;
#74852 = AXIS2_PLACEMENT_3D('',#120827,#94467,#94468) ;
#74853 = AXIS2_PLACEMENT_3D('',#120829,#94469,#94470) ;
#74854 = AXIS2_PLACEMENT_3D('',#120830,#94471,#94472) ;
#74855 = AXIS2_PLACEMENT_3D('',#120831,#94473,#94474) ;
#74856 = AXIS2_PLACEMENT_3D('',#120832,#94475,#94476) ;
#74857 = AXIS2_PLACEMENT_3D('',#120833,#94477,#94478) ;
#74858 = AXIS2_PLACEMENT_3D('',#120834,#94479,#94480) ;
#74859 = AXIS2_PLACEMENT_3D('',#120835,#94481,#94482) ;
#74860 = AXIS2_PLACEMENT_3D('',#120836,#94483,#94484) ;
#74861 = AXIS2_PLACEMENT_3D('',#120837,#94485,#94486) ;
#74862 = AXIS2_PLACEMENT_3D('',#120838,#94487,#94488) ;
#74863 = AXIS2_PLACEMENT_3D('',#120839,#94489,#94490) ;
#74864 = AXIS2_PLACEMENT_3D('',#120840,#94491,#94492) ;
#74865 = AXIS2_PLACEMENT_3D('',#120841,#94493,#94494) ;
#74866 = AXIS2_PLACEMENT_3D('',#120844,#94496,#94497) ;
#74867 = AXIS2_PLACEMENT_3D('',#120845,#94498,#94499) ;
#74868 = AXIS2_PLACEMENT_3D('',#120846,#94500,#94501) ;
#74869 = AXIS2_PLACEMENT_3D('',#120847,#94502,#94503) ;
#74870 = AXIS2_PLACEMENT_3D('',#120848,#94504,#94505) ;
#74871 = AXIS2_PLACEMENT_3D('',#120849,#94506,#94507) ;
#74872 = AXIS2_PLACEMENT_3D('',#120850,#94508,#94509) ;
#74873 = AXIS2_PLACEMENT_3D('',#120851,#94510,#94511) ;
#74874 = AXIS2_PLACEMENT_3D('',#120852,#94512,#94513) ;
#74875 = AXIS2_PLACEMENT_3D('',#120853,#94514,#94515) ;
#74876 = AXIS2_PLACEMENT_3D('',#120854,#94516,#94517) ;
#74877 = AXIS2_PLACEMENT_3D('',#120855,#94518,#94519) ;
#74878 = AXIS2_PLACEMENT_3D('',#120856,#94520,#94521) ;
#74879 = AXIS2_PLACEMENT_3D('',#120858,#94522,#94523) ;
#74880 = AXIS2_PLACEMENT_3D('',#120859,#94524,#94525) ;
#74881 = AXIS2_PLACEMENT_3D('',#120860,#94526,#94527) ;
#74882 = AXIS2_PLACEMENT_3D('',#120861,#94528,#94529) ;
#74883 = AXIS2_PLACEMENT_3D('',#120862,#94530,#94531) ;
#74884 = AXIS2_PLACEMENT_3D('',#120863,#94532,#94533) ;
#74885 = AXIS2_PLACEMENT_3D('',#120864,#94534,#94535) ;
#74886 = AXIS2_PLACEMENT_3D('',#120865,#94536,#94537) ;
#74887 = AXIS2_PLACEMENT_3D('',#120866,#94538,#94539) ;
#74888 = AXIS2_PLACEMENT_3D('',#120867,#94540,#94541) ;
#74889 = AXIS2_PLACEMENT_3D('',#120868,#94542,#94543) ;
#74890 = AXIS2_PLACEMENT_3D('',#120870,#94545,#94546) ;
#74891 = AXIS2_PLACEMENT_3D('',#120871,#94547,#94548) ;
#74892 = AXIS2_PLACEMENT_3D('',#120872,#94549,#94550) ;
#74893 = AXIS2_PLACEMENT_3D('',#120873,#94551,#94552) ;
#74894 = AXIS2_PLACEMENT_3D('',#120874,#94553,#94554) ;
#74895 = AXIS2_PLACEMENT_3D('',#120875,#94555,#94556) ;
#74896 = AXIS2_PLACEMENT_3D('',#120876,#94557,#94558) ;
#74897 = AXIS2_PLACEMENT_3D('',#120877,#94559,#94560) ;
#74898 = AXIS2_PLACEMENT_3D('',#120878,#94561,#94562) ;
#74899 = AXIS2_PLACEMENT_3D('',#120879,#94563,#94564) ;
#74900 = AXIS2_PLACEMENT_3D('',#120880,#94565,#94566) ;
#74901 = AXIS2_PLACEMENT_3D('',#120881,#94567,#94568) ;
#74902 = AXIS2_PLACEMENT_3D('',#120882,#94569,#94570) ;
#74903 = AXIS2_PLACEMENT_3D('',#120883,#94571,#94572) ;
#74904 = AXIS2_PLACEMENT_3D('',#120884,#94573,#94574) ;
#74905 = AXIS2_PLACEMENT_3D('',#120885,#94575,#94576) ;
#74906 = AXIS2_PLACEMENT_3D('',#120886,#94577,#94578) ;
#74907 = AXIS2_PLACEMENT_3D('',#120887,#94579,#94580) ;
#74908 = AXIS2_PLACEMENT_3D('',#120888,#94581,#94582) ;
#74909 = AXIS2_PLACEMENT_3D('',#120889,#94583,#94584) ;
#74910 = AXIS2_PLACEMENT_3D('',#120890,#94585,#94586) ;
#74911 = AXIS2_PLACEMENT_3D('',#120891,#94587,#94588) ;
#74912 = AXIS2_PLACEMENT_3D('',#120892,#94589,#94590) ;
#74913 = AXIS2_PLACEMENT_3D('',#120893,#94591,#94592) ;
#74914 = AXIS2_PLACEMENT_3D('',#120894,#94593,#94594) ;
#74915 = AXIS2_PLACEMENT_3D('',#120895,#94595,#94596) ;
#74916 = AXIS2_PLACEMENT_3D('',#120896,#94597,#94598) ;
#74917 = AXIS2_PLACEMENT_3D('',#120897,#94599,#94600) ;
#74918 = AXIS2_PLACEMENT_3D('',#120898,#94601,#94602) ;
#74919 = AXIS2_PLACEMENT_3D('',#120899,#94603,#94604) ;
#74920 = AXIS2_PLACEMENT_3D('',#120900,#94605,#94606) ;
#74921 = AXIS2_PLACEMENT_3D('',#120901,#94607,#94608) ;
#74922 = AXIS2_PLACEMENT_3D('',#120902,#94609,#94610) ;
#74923 = AXIS2_PLACEMENT_3D('',#120903,#94611,#94612) ;
#74924 = AXIS2_PLACEMENT_3D('',#120904,#94613,#94614) ;
#74925 = AXIS2_PLACEMENT_3D('',#120905,#94615,#94616) ;
#74926 = AXIS2_PLACEMENT_3D('',#120906,#94617,#94618) ;
#74927 = AXIS2_PLACEMENT_3D('',#120907,#94619,#94620) ;
#74928 = AXIS2_PLACEMENT_3D('',#120908,#94621,#94622) ;
#74929 = AXIS2_PLACEMENT_3D('',#120909,#94623,#94624) ;
#74930 = AXIS2_PLACEMENT_3D('',#120910,#94625,#94626) ;
#74931 = AXIS2_PLACEMENT_3D('',#120911,#94627,#94628) ;
#74932 = AXIS2_PLACEMENT_3D('',#120912,#94629,#94630) ;
#74933 = AXIS2_PLACEMENT_3D('',#120913,#94631,#94632) ;
#74934 = AXIS2_PLACEMENT_3D('',#120914,#94633,#94634) ;
#74935 = AXIS2_PLACEMENT_3D('',#120915,#94635,#94636) ;
#74936 = AXIS2_PLACEMENT_3D('',#120916,#94637,#94638) ;
#74937 = AXIS2_PLACEMENT_3D('',#120917,#94639,#94640) ;
#74938 = AXIS2_PLACEMENT_3D('',#120918,#94641,#94642) ;
#74939 = AXIS2_PLACEMENT_3D('',#120919,#94643,#94644) ;
#74940 = AXIS2_PLACEMENT_3D('',#120920,#94645,#94646) ;
#74941 = AXIS2_PLACEMENT_3D('',#120921,#94647,#94648) ;
#74942 = AXIS2_PLACEMENT_3D('',#120922,#94649,#94650) ;
#74943 = AXIS2_PLACEMENT_3D('',#120923,#94651,#94652) ;
#74944 = AXIS2_PLACEMENT_3D('',#120924,#94653,#94654) ;
#74945 = AXIS2_PLACEMENT_3D('',#120925,#94655,#94656) ;
#74946 = AXIS2_PLACEMENT_3D('',#120926,#94657,#94658) ;
#74947 = AXIS2_PLACEMENT_3D('',#120927,#94659,#94660) ;
#74948 = AXIS2_PLACEMENT_3D('',#120928,#94661,#94662) ;
#74949 = AXIS2_PLACEMENT_3D('',#120929,#94663,#94664) ;
#74950 = AXIS2_PLACEMENT_3D('',#120930,#94665,#94666) ;
#74951 = AXIS2_PLACEMENT_3D('',#120931,#94667,#94668) ;
#74952 = AXIS2_PLACEMENT_3D('',#120932,#94669,#94670) ;
#74953 = AXIS2_PLACEMENT_3D('',#120933,#94671,#94672) ;
#74954 = AXIS2_PLACEMENT_3D('',#120934,#94673,#94674) ;
#74955 = AXIS2_PLACEMENT_3D('',#120935,#94675,#94676) ;
#74956 = AXIS2_PLACEMENT_3D('',#120936,#94677,#94678) ;
#74957 = AXIS2_PLACEMENT_3D('',#120938,#94679,#94680) ;
#74958 = AXIS2_PLACEMENT_3D('',#120939,#94681,#94682) ;
#74959 = AXIS2_PLACEMENT_3D('',#120940,#94683,#94684) ;
#74960 = AXIS2_PLACEMENT_3D('',#120941,#94685,#94686) ;
#74961 = AXIS2_PLACEMENT_3D('',#120942,#94687,#94688) ;
#74962 = AXIS2_PLACEMENT_3D('',#120943,#94689,#94690) ;
#74963 = AXIS2_PLACEMENT_3D('',#120944,#94691,#94692) ;
#74964 = AXIS2_PLACEMENT_3D('',#120945,#94693,#94694) ;
#74965 = AXIS2_PLACEMENT_3D('',#120946,#94695,#94696) ;
#74966 = AXIS2_PLACEMENT_3D('',#120957,#94698,#94699) ;
#74967 = AXIS2_PLACEMENT_3D('',#121014,#94701,#94702) ;
#74968 = AXIS2_PLACEMENT_3D('',#121015,#94703,#94704) ;
#74969 = AXIS2_PLACEMENT_3D('',#121016,#94705,#94706) ;
#74970 = AXIS2_PLACEMENT_3D('',#121017,#94707,#94708) ;
#74971 = AXIS2_PLACEMENT_3D('',#121018,#94709,#94710) ;
#74972 = AXIS2_PLACEMENT_3D('',#121019,#94711,#94712) ;
#74973 = AXIS2_PLACEMENT_3D('',#121020,#94713,#94714) ;
#74974 = AXIS2_PLACEMENT_3D('',#121021,#94715,#94716) ;
#74975 = AXIS2_PLACEMENT_3D('',#121022,#94717,#94718) ;
#74976 = AXIS2_PLACEMENT_3D('',#121023,#94719,#94720) ;
#74977 = AXIS2_PLACEMENT_3D('',#121024,#94721,#94722) ;
#74978 = AXIS2_PLACEMENT_3D('',#121025,#94723,#94724) ;
#74979 = AXIS2_PLACEMENT_3D('',#121026,#94725,#94726) ;
#74980 = AXIS2_PLACEMENT_3D('',#121027,#94727,#94728) ;
#74981 = AXIS2_PLACEMENT_3D('',#121028,#94729,#94730) ;
#74982 = AXIS2_PLACEMENT_3D('',#121029,#94731,#94732) ;
#74983 = AXIS2_PLACEMENT_3D('',#121030,#94733,#94734) ;
#74984 = AXIS2_PLACEMENT_3D('',#121031,#94735,#94736) ;
#74985 = AXIS2_PLACEMENT_3D('',#121032,#94737,#94738) ;
#74986 = AXIS2_PLACEMENT_3D('',#121033,#94739,#94740) ;
#74987 = AXIS2_PLACEMENT_3D('',#121034,#94741,#94742) ;
#74988 = AXIS2_PLACEMENT_3D('',#121035,#94743,#94744) ;
#74989 = AXIS2_PLACEMENT_3D('',#121036,#94745,#94746) ;
#74990 = AXIS2_PLACEMENT_3D('',#121039,#94748,#94749) ;
#74991 = AXIS2_PLACEMENT_3D('',#121040,#94750,#94751) ;
#74992 = AXIS2_PLACEMENT_3D('',#121041,#94752,#94753) ;
#74993 = AXIS2_PLACEMENT_3D('',#121042,#94754,#94755) ;
#74994 = AXIS2_PLACEMENT_3D('',#121043,#94756,#94757) ;
#74995 = AXIS2_PLACEMENT_3D('',#121044,#94758,#94759) ;
#74996 = AXIS2_PLACEMENT_3D('',#121045,#94760,#94761) ;
#74997 = AXIS2_PLACEMENT_3D('',#121046,#94762,#94763) ;
#74998 = AXIS2_PLACEMENT_3D('',#121047,#94764,#94765) ;
#74999 = AXIS2_PLACEMENT_3D('',#121048,#94766,#94767) ;
#75000 = AXIS2_PLACEMENT_3D('',#121049,#94768,#94769) ;
#75001 = AXIS2_PLACEMENT_3D('',#121050,#94770,#94771) ;
#75002 = AXIS2_PLACEMENT_3D('',#121051,#94772,#94773) ;
#75003 = AXIS2_PLACEMENT_3D('',#121052,#94774,#94775) ;
#75004 = AXIS2_PLACEMENT_3D('',#121053,#94776,#94777) ;
#75005 = AXIS2_PLACEMENT_3D('',#121054,#94778,#94779) ;
#75006 = AXIS2_PLACEMENT_3D('',#121056,#94780,#94781) ;
#75007 = AXIS2_PLACEMENT_3D('',#121057,#94782,#94783) ;
#75008 = AXIS2_PLACEMENT_3D('',#121058,#94784,#94785) ;
#75009 = AXIS2_PLACEMENT_3D('',#121059,#94786,#94787) ;
#75010 = AXIS2_PLACEMENT_3D('',#121060,#94788,#94789) ;
#75011 = AXIS2_PLACEMENT_3D('',#121061,#94790,#94791) ;
#75012 = AXIS2_PLACEMENT_3D('',#121062,#94792,#94793) ;
#75013 = AXIS2_PLACEMENT_3D('',#121063,#94794,#94795) ;
#75014 = AXIS2_PLACEMENT_3D('',#121064,#94796,#94797) ;
#75015 = AXIS2_PLACEMENT_3D('',#121065,#94798,#94799) ;
#75016 = AXIS2_PLACEMENT_3D('',#121066,#94800,#94801) ;
#75017 = AXIS2_PLACEMENT_3D('',#121067,#94802,#94803) ;
#75018 = AXIS2_PLACEMENT_3D('',#121068,#94804,#94805) ;
#75019 = AXIS2_PLACEMENT_3D('',#121071,#94807,#94808) ;
#75020 = AXIS2_PLACEMENT_3D('',#121072,#94809,#94810) ;
#75021 = AXIS2_PLACEMENT_3D('',#121073,#94811,#94812) ;
#75022 = AXIS2_PLACEMENT_3D('',#121074,#94813,#94814) ;
#75023 = AXIS2_PLACEMENT_3D('',#121075,#94815,#94816) ;
#75024 = AXIS2_PLACEMENT_3D('',#121076,#94817,#94818) ;
#75025 = AXIS2_PLACEMENT_3D('',#121077,#94819,#94820) ;
#75026 = AXIS2_PLACEMENT_3D('',#121078,#94821,#94822) ;
#75027 = AXIS2_PLACEMENT_3D('',#121079,#94823,#94824) ;
#75028 = AXIS2_PLACEMENT_3D('',#121080,#94825,#94826) ;
#75029 = AXIS2_PLACEMENT_3D('',#121081,#94827,#94828) ;
#75030 = AXIS2_PLACEMENT_3D('',#121082,#94829,#94830) ;
#75031 = AXIS2_PLACEMENT_3D('',#121083,#94831,#94832) ;
#75032 = AXIS2_PLACEMENT_3D('',#121085,#94833,#94834) ;
#75033 = AXIS2_PLACEMENT_3D('',#121086,#94835,#94836) ;
#75034 = AXIS2_PLACEMENT_3D('',#121087,#94837,#94838) ;
#75035 = AXIS2_PLACEMENT_3D('',#121088,#94839,#94840) ;
#75036 = AXIS2_PLACEMENT_3D('',#121089,#94841,#94842) ;
#75037 = AXIS2_PLACEMENT_3D('',#121090,#94843,#94844) ;
#75038 = AXIS2_PLACEMENT_3D('',#121091,#94845,#94846) ;
#75039 = AXIS2_PLACEMENT_3D('',#121092,#94847,#94848) ;
#75040 = AXIS2_PLACEMENT_3D('',#121093,#94849,#94850) ;
#75041 = AXIS2_PLACEMENT_3D('',#121094,#94851,#94852) ;
#75042 = AXIS2_PLACEMENT_3D('',#121095,#94853,#94854) ;
#75043 = AXIS2_PLACEMENT_3D('',#121097,#94856,#94857) ;
#75044 = AXIS2_PLACEMENT_3D('',#121098,#94858,#94859) ;
#75045 = AXIS2_PLACEMENT_3D('',#121099,#94860,#94861) ;
#75046 = AXIS2_PLACEMENT_3D('',#121100,#94862,#94863) ;
#75047 = AXIS2_PLACEMENT_3D('',#121101,#94864,#94865) ;
#75048 = AXIS2_PLACEMENT_3D('',#121102,#94866,#94867) ;
#75049 = AXIS2_PLACEMENT_3D('',#121103,#94868,#94869) ;
#75050 = AXIS2_PLACEMENT_3D('',#121104,#94870,#94871) ;
#75051 = AXIS2_PLACEMENT_3D('',#121105,#94872,#94873) ;
#75052 = AXIS2_PLACEMENT_3D('',#121106,#94874,#94875) ;
#75053 = AXIS2_PLACEMENT_3D('',#121107,#94876,#94877) ;
#75054 = AXIS2_PLACEMENT_3D('',#121108,#94878,#94879) ;
#75055 = AXIS2_PLACEMENT_3D('',#121109,#94880,#94881) ;
#75056 = AXIS2_PLACEMENT_3D('',#121110,#94882,#94883) ;
#75057 = AXIS2_PLACEMENT_3D('',#121111,#94884,#94885) ;
#75058 = AXIS2_PLACEMENT_3D('',#121112,#94886,#94887) ;
#75059 = AXIS2_PLACEMENT_3D('',#121113,#94888,#94889) ;
#75060 = AXIS2_PLACEMENT_3D('',#121114,#94890,#94891) ;
#75061 = AXIS2_PLACEMENT_3D('',#121115,#94892,#94893) ;
#75062 = AXIS2_PLACEMENT_3D('',#121116,#94894,#94895) ;
#75063 = AXIS2_PLACEMENT_3D('',#121117,#94896,#94897) ;
#75064 = AXIS2_PLACEMENT_3D('',#121118,#94898,#94899) ;
#75065 = AXIS2_PLACEMENT_3D('',#121119,#94900,#94901) ;
#75066 = AXIS2_PLACEMENT_3D('',#121120,#94902,#94903) ;
#75067 = AXIS2_PLACEMENT_3D('',#121121,#94904,#94905) ;
#75068 = AXIS2_PLACEMENT_3D('',#121122,#94906,#94907) ;
#75069 = AXIS2_PLACEMENT_3D('',#121123,#94908,#94909) ;
#75070 = AXIS2_PLACEMENT_3D('',#121124,#94910,#94911) ;
#75071 = AXIS2_PLACEMENT_3D('',#121125,#94912,#94913) ;
#75072 = AXIS2_PLACEMENT_3D('',#121126,#94914,#94915) ;
#75073 = AXIS2_PLACEMENT_3D('',#121127,#94916,#94917) ;
#75074 = AXIS2_PLACEMENT_3D('',#121128,#94918,#94919) ;
#75075 = AXIS2_PLACEMENT_3D('',#121129,#94920,#94921) ;
#75076 = AXIS2_PLACEMENT_3D('',#121130,#94922,#94923) ;
#75077 = AXIS2_PLACEMENT_3D('',#121131,#94924,#94925) ;
#75078 = AXIS2_PLACEMENT_3D('',#121132,#94926,#94927) ;
#75079 = AXIS2_PLACEMENT_3D('',#121133,#94928,#94929) ;
#75080 = AXIS2_PLACEMENT_3D('',#121134,#94930,#94931) ;
#75081 = AXIS2_PLACEMENT_3D('',#121135,#94932,#94933) ;
#75082 = AXIS2_PLACEMENT_3D('',#121136,#94934,#94935) ;
#75083 = AXIS2_PLACEMENT_3D('',#121137,#94936,#94937) ;
#75084 = AXIS2_PLACEMENT_3D('',#121138,#94938,#94939) ;
#75085 = AXIS2_PLACEMENT_3D('',#121139,#94940,#94941) ;
#75086 = AXIS2_PLACEMENT_3D('',#121140,#94942,#94943) ;
#75087 = AXIS2_PLACEMENT_3D('',#121141,#94944,#94945) ;
#75088 = AXIS2_PLACEMENT_3D('',#121142,#94946,#94947) ;
#75089 = AXIS2_PLACEMENT_3D('',#121143,#94948,#94949) ;
#75090 = AXIS2_PLACEMENT_3D('',#121144,#94950,#94951) ;
#75091 = AXIS2_PLACEMENT_3D('',#121145,#94952,#94953) ;
#75092 = AXIS2_PLACEMENT_3D('',#121146,#94954,#94955) ;
#75093 = AXIS2_PLACEMENT_3D('',#121147,#94956,#94957) ;
#75094 = AXIS2_PLACEMENT_3D('',#121148,#94958,#94959) ;
#75095 = AXIS2_PLACEMENT_3D('',#121149,#94960,#94961) ;
#75096 = AXIS2_PLACEMENT_3D('',#121150,#94962,#94963) ;
#75097 = AXIS2_PLACEMENT_3D('',#121151,#94964,#94965) ;
#75098 = AXIS2_PLACEMENT_3D('',#121152,#94966,#94967) ;
#75099 = AXIS2_PLACEMENT_3D('',#121153,#94968,#94969) ;
#75100 = AXIS2_PLACEMENT_3D('',#121154,#94970,#94971) ;
#75101 = AXIS2_PLACEMENT_3D('',#121155,#94972,#94973) ;
#75102 = AXIS2_PLACEMENT_3D('',#121156,#94974,#94975) ;
#75103 = AXIS2_PLACEMENT_3D('',#121157,#94976,#94977) ;
#75104 = AXIS2_PLACEMENT_3D('',#121158,#94978,#94979) ;
#75105 = AXIS2_PLACEMENT_3D('',#121159,#94980,#94981) ;
#75106 = AXIS2_PLACEMENT_3D('',#121160,#94982,#94983) ;
#75107 = AXIS2_PLACEMENT_3D('',#121161,#94984,#94985) ;
#75108 = AXIS2_PLACEMENT_3D('',#121162,#94986,#94987) ;
#75109 = AXIS2_PLACEMENT_3D('',#121163,#94988,#94989) ;
#75110 = AXIS2_PLACEMENT_3D('',#121165,#94990,#94991) ;
#75111 = AXIS2_PLACEMENT_3D('',#121166,#94992,#94993) ;
#75112 = AXIS2_PLACEMENT_3D('',#121167,#94994,#94995) ;
#75113 = AXIS2_PLACEMENT_3D('',#121168,#94996,#94997) ;
#75114 = AXIS2_PLACEMENT_3D('',#121169,#94998,#94999) ;
#75115 = AXIS2_PLACEMENT_3D('',#121170,#95000,#95001) ;
#75116 = AXIS2_PLACEMENT_3D('',#121171,#95002,#95003) ;
#75117 = AXIS2_PLACEMENT_3D('',#121172,#95004,#95005) ;
#75118 = AXIS2_PLACEMENT_3D('',#121173,#95006,#95007) ;
#75119 = AXIS2_PLACEMENT_3D('',#121184,#95009,#95010) ;
#75120 = AXIS2_PLACEMENT_3D('',#121241,#95012,#95013) ;
#75121 = AXIS2_PLACEMENT_3D('',#121242,#95014,#95015) ;
#75122 = AXIS2_PLACEMENT_3D('',#121243,#95016,#95017) ;
#75123 = AXIS2_PLACEMENT_3D('',#121244,#95018,#95019) ;
#75124 = AXIS2_PLACEMENT_3D('',#121245,#95020,#95021) ;
#75125 = AXIS2_PLACEMENT_3D('',#121246,#95022,#95023) ;
#75126 = AXIS2_PLACEMENT_3D('',#121247,#95024,#95025) ;
#75127 = AXIS2_PLACEMENT_3D('',#121248,#95026,#95027) ;
#75128 = AXIS2_PLACEMENT_3D('',#121249,#95028,#95029) ;
#75129 = AXIS2_PLACEMENT_3D('',#121250,#95030,#95031) ;
#75130 = AXIS2_PLACEMENT_3D('',#121251,#95032,#95033) ;
#75131 = AXIS2_PLACEMENT_3D('',#121252,#95034,#95035) ;
#75132 = AXIS2_PLACEMENT_3D('',#121253,#95036,#95037) ;
#75133 = AXIS2_PLACEMENT_3D('',#121254,#95038,#95039) ;
#75134 = AXIS2_PLACEMENT_3D('',#121255,#95040,#95041) ;
#75135 = AXIS2_PLACEMENT_3D('',#121256,#95042,#95043) ;
#75136 = AXIS2_PLACEMENT_3D('',#121257,#95044,#95045) ;
#75137 = AXIS2_PLACEMENT_3D('',#121258,#95046,#95047) ;
#75138 = AXIS2_PLACEMENT_3D('',#121259,#95048,#95049) ;
#75139 = AXIS2_PLACEMENT_3D('',#121260,#95050,#95051) ;
#75140 = AXIS2_PLACEMENT_3D('',#121261,#95052,#95053) ;
#75141 = AXIS2_PLACEMENT_3D('',#121262,#95054,#95055) ;
#75142 = AXIS2_PLACEMENT_3D('',#121263,#95056,#95057) ;
#75143 = AXIS2_PLACEMENT_3D('',#121266,#95059,#95060) ;
#75144 = AXIS2_PLACEMENT_3D('',#121267,#95061,#95062) ;
#75145 = AXIS2_PLACEMENT_3D('',#121268,#95063,#95064) ;
#75146 = AXIS2_PLACEMENT_3D('',#121269,#95065,#95066) ;
#75147 = AXIS2_PLACEMENT_3D('',#121270,#95067,#95068) ;
#75148 = AXIS2_PLACEMENT_3D('',#121271,#95069,#95070) ;
#75149 = AXIS2_PLACEMENT_3D('',#121272,#95071,#95072) ;
#75150 = AXIS2_PLACEMENT_3D('',#121273,#95073,#95074) ;
#75151 = AXIS2_PLACEMENT_3D('',#121274,#95075,#95076) ;
#75152 = AXIS2_PLACEMENT_3D('',#121275,#95077,#95078) ;
#75153 = AXIS2_PLACEMENT_3D('',#121276,#95079,#95080) ;
#75154 = AXIS2_PLACEMENT_3D('',#121277,#95081,#95082) ;
#75155 = AXIS2_PLACEMENT_3D('',#121278,#95083,#95084) ;
#75156 = AXIS2_PLACEMENT_3D('',#121279,#95085,#95086) ;
#75157 = AXIS2_PLACEMENT_3D('',#121280,#95087,#95088) ;
#75158 = AXIS2_PLACEMENT_3D('',#121281,#95089,#95090) ;
#75159 = AXIS2_PLACEMENT_3D('',#121283,#95091,#95092) ;
#75160 = AXIS2_PLACEMENT_3D('',#121284,#95093,#95094) ;
#75161 = AXIS2_PLACEMENT_3D('',#121285,#95095,#95096) ;
#75162 = AXIS2_PLACEMENT_3D('',#121286,#95097,#95098) ;
#75163 = AXIS2_PLACEMENT_3D('',#121287,#95099,#95100) ;
#75164 = AXIS2_PLACEMENT_3D('',#121288,#95101,#95102) ;
#75165 = AXIS2_PLACEMENT_3D('',#121289,#95103,#95104) ;
#75166 = AXIS2_PLACEMENT_3D('',#121290,#95105,#95106) ;
#75167 = AXIS2_PLACEMENT_3D('',#121291,#95107,#95108) ;
#75168 = AXIS2_PLACEMENT_3D('',#121292,#95109,#95110) ;
#75169 = AXIS2_PLACEMENT_3D('',#121293,#95111,#95112) ;
#75170 = AXIS2_PLACEMENT_3D('',#121294,#95113,#95114) ;
#75171 = AXIS2_PLACEMENT_3D('',#121295,#95115,#95116) ;
#75172 = AXIS2_PLACEMENT_3D('',#121298,#95118,#95119) ;
#75173 = AXIS2_PLACEMENT_3D('',#121299,#95120,#95121) ;
#75174 = AXIS2_PLACEMENT_3D('',#121300,#95122,#95123) ;
#75175 = AXIS2_PLACEMENT_3D('',#121301,#95124,#95125) ;
#75176 = AXIS2_PLACEMENT_3D('',#121302,#95126,#95127) ;
#75177 = AXIS2_PLACEMENT_3D('',#121303,#95128,#95129) ;
#75178 = AXIS2_PLACEMENT_3D('',#121304,#95130,#95131) ;
#75179 = AXIS2_PLACEMENT_3D('',#121305,#95132,#95133) ;
#75180 = AXIS2_PLACEMENT_3D('',#121306,#95134,#95135) ;
#75181 = AXIS2_PLACEMENT_3D('',#121307,#95136,#95137) ;
#75182 = AXIS2_PLACEMENT_3D('',#121308,#95138,#95139) ;
#75183 = AXIS2_PLACEMENT_3D('',#121309,#95140,#95141) ;
#75184 = AXIS2_PLACEMENT_3D('',#121310,#95142,#95143) ;
#75185 = AXIS2_PLACEMENT_3D('',#121312,#95144,#95145) ;
#75186 = AXIS2_PLACEMENT_3D('',#121313,#95146,#95147) ;
#75187 = AXIS2_PLACEMENT_3D('',#121314,#95148,#95149) ;
#75188 = AXIS2_PLACEMENT_3D('',#121315,#95150,#95151) ;
#75189 = AXIS2_PLACEMENT_3D('',#121316,#95152,#95153) ;
#75190 = AXIS2_PLACEMENT_3D('',#121317,#95154,#95155) ;
#75191 = AXIS2_PLACEMENT_3D('',#121318,#95156,#95157) ;
#75192 = AXIS2_PLACEMENT_3D('',#121319,#95158,#95159) ;
#75193 = AXIS2_PLACEMENT_3D('',#121320,#95160,#95161) ;
#75194 = AXIS2_PLACEMENT_3D('',#121321,#95162,#95163) ;
#75195 = AXIS2_PLACEMENT_3D('',#121322,#95164,#95165) ;
#75196 = AXIS2_PLACEMENT_3D('',#121324,#95167,#95168) ;
#75197 = AXIS2_PLACEMENT_3D('',#121325,#95169,#95170) ;
#75198 = AXIS2_PLACEMENT_3D('',#121326,#95171,#95172) ;
#75199 = AXIS2_PLACEMENT_3D('',#121327,#95173,#95174) ;
#75200 = AXIS2_PLACEMENT_3D('',#121328,#95175,#95176) ;
#75201 = AXIS2_PLACEMENT_3D('',#121329,#95177,#95178) ;
#75202 = AXIS2_PLACEMENT_3D('',#121330,#95179,#95180) ;
#75203 = AXIS2_PLACEMENT_3D('',#121331,#95181,#95182) ;
#75204 = AXIS2_PLACEMENT_3D('',#121332,#95183,#95184) ;
#75205 = AXIS2_PLACEMENT_3D('',#121333,#95185,#95186) ;
#75206 = AXIS2_PLACEMENT_3D('',#121334,#95187,#95188) ;
#75207 = AXIS2_PLACEMENT_3D('',#121335,#95189,#95190) ;
#75208 = AXIS2_PLACEMENT_3D('',#121336,#95191,#95192) ;
#75209 = AXIS2_PLACEMENT_3D('',#121337,#95193,#95194) ;
#75210 = AXIS2_PLACEMENT_3D('',#121338,#95195,#95196) ;
#75211 = AXIS2_PLACEMENT_3D('',#121339,#95197,#95198) ;
#75212 = AXIS2_PLACEMENT_3D('',#121340,#95199,#95200) ;
#75213 = AXIS2_PLACEMENT_3D('',#121341,#95201,#95202) ;
#75214 = AXIS2_PLACEMENT_3D('',#121342,#95203,#95204) ;
#75215 = AXIS2_PLACEMENT_3D('',#121343,#95205,#95206) ;
#75216 = AXIS2_PLACEMENT_3D('',#121344,#95207,#95208) ;
#75217 = AXIS2_PLACEMENT_3D('',#121345,#95209,#95210) ;
#75218 = AXIS2_PLACEMENT_3D('',#121346,#95211,#95212) ;
#75219 = AXIS2_PLACEMENT_3D('',#121347,#95213,#95214) ;
#75220 = AXIS2_PLACEMENT_3D('',#121348,#95215,#95216) ;
#75221 = AXIS2_PLACEMENT_3D('',#121349,#95217,#95218) ;
#75222 = AXIS2_PLACEMENT_3D('',#121350,#95219,#95220) ;
#75223 = AXIS2_PLACEMENT_3D('',#121351,#95221,#95222) ;
#75224 = AXIS2_PLACEMENT_3D('',#121352,#95223,#95224) ;
#75225 = AXIS2_PLACEMENT_3D('',#121353,#95225,#95226) ;
#75226 = AXIS2_PLACEMENT_3D('',#121354,#95227,#95228) ;
#75227 = AXIS2_PLACEMENT_3D('',#121355,#95229,#95230) ;
#75228 = AXIS2_PLACEMENT_3D('',#121356,#95231,#95232) ;
#75229 = AXIS2_PLACEMENT_3D('',#121357,#95233,#95234) ;
#75230 = AXIS2_PLACEMENT_3D('',#121358,#95235,#95236) ;
#75231 = AXIS2_PLACEMENT_3D('',#121359,#95237,#95238) ;
#75232 = AXIS2_PLACEMENT_3D('',#121360,#95239,#95240) ;
#75233 = AXIS2_PLACEMENT_3D('',#121361,#95241,#95242) ;
#75234 = AXIS2_PLACEMENT_3D('',#121362,#95243,#95244) ;
#75235 = AXIS2_PLACEMENT_3D('',#121363,#95245,#95246) ;
#75236 = AXIS2_PLACEMENT_3D('',#121364,#95247,#95248) ;
#75237 = AXIS2_PLACEMENT_3D('',#121365,#95249,#95250) ;
#75238 = AXIS2_PLACEMENT_3D('',#121366,#95251,#95252) ;
#75239 = AXIS2_PLACEMENT_3D('',#121367,#95253,#95254) ;
#75240 = AXIS2_PLACEMENT_3D('',#121368,#95255,#95256) ;
#75241 = AXIS2_PLACEMENT_3D('',#121369,#95257,#95258) ;
#75242 = AXIS2_PLACEMENT_3D('',#121370,#95259,#95260) ;
#75243 = AXIS2_PLACEMENT_3D('',#121371,#95261,#95262) ;
#75244 = AXIS2_PLACEMENT_3D('',#121372,#95263,#95264) ;
#75245 = AXIS2_PLACEMENT_3D('',#121373,#95265,#95266) ;
#75246 = AXIS2_PLACEMENT_3D('',#121374,#95267,#95268) ;
#75247 = AXIS2_PLACEMENT_3D('',#121375,#95269,#95270) ;
#75248 = AXIS2_PLACEMENT_3D('',#121376,#95271,#95272) ;
#75249 = AXIS2_PLACEMENT_3D('',#121377,#95273,#95274) ;
#75250 = AXIS2_PLACEMENT_3D('',#121378,#95275,#95276) ;
#75251 = AXIS2_PLACEMENT_3D('',#121379,#95277,#95278) ;
#75252 = AXIS2_PLACEMENT_3D('',#121380,#95279,#95280) ;
#75253 = AXIS2_PLACEMENT_3D('',#121381,#95281,#95282) ;
#75254 = AXIS2_PLACEMENT_3D('',#121382,#95283,#95284) ;
#75255 = AXIS2_PLACEMENT_3D('',#121383,#95285,#95286) ;
#75256 = AXIS2_PLACEMENT_3D('',#121384,#95287,#95288) ;
#75257 = AXIS2_PLACEMENT_3D('',#121385,#95289,#95290) ;
#75258 = AXIS2_PLACEMENT_3D('',#121386,#95291,#95292) ;
#75259 = AXIS2_PLACEMENT_3D('',#121387,#95293,#95294) ;
#75260 = AXIS2_PLACEMENT_3D('',#121388,#95295,#95296) ;
#75261 = AXIS2_PLACEMENT_3D('',#121389,#95297,#95298) ;
#75262 = AXIS2_PLACEMENT_3D('',#121390,#95299,#95300) ;
#75263 = AXIS2_PLACEMENT_3D('',#121392,#95301,#95302) ;
#75264 = AXIS2_PLACEMENT_3D('',#121393,#95303,#95304) ;
#75265 = AXIS2_PLACEMENT_3D('',#121394,#95305,#95306) ;
#75266 = AXIS2_PLACEMENT_3D('',#121395,#95307,#95308) ;
#75267 = AXIS2_PLACEMENT_3D('',#121396,#95309,#95310) ;
#75268 = AXIS2_PLACEMENT_3D('',#121397,#95311,#95312) ;
#75269 = AXIS2_PLACEMENT_3D('',#121398,#95313,#95314) ;
#75270 = AXIS2_PLACEMENT_3D('',#121399,#95315,#95316) ;
#75271 = AXIS2_PLACEMENT_3D('',#121400,#95317,#95318) ;
#75272 = AXIS2_PLACEMENT_3D('',#121411,#95320,#95321) ;
#75273 = AXIS2_PLACEMENT_3D('',#121468,#95323,#95324) ;
#75274 = AXIS2_PLACEMENT_3D('',#121469,#95325,#95326) ;
#75275 = AXIS2_PLACEMENT_3D('',#121470,#95327,#95328) ;
#75276 = AXIS2_PLACEMENT_3D('',#121471,#95329,#95330) ;
#75277 = AXIS2_PLACEMENT_3D('',#121472,#95331,#95332) ;
#75278 = AXIS2_PLACEMENT_3D('',#121473,#95333,#95334) ;
#75279 = AXIS2_PLACEMENT_3D('',#121474,#95335,#95336) ;
#75280 = AXIS2_PLACEMENT_3D('',#121475,#95337,#95338) ;
#75281 = AXIS2_PLACEMENT_3D('',#121476,#95339,#95340) ;
#75282 = AXIS2_PLACEMENT_3D('',#121477,#95341,#95342) ;
#75283 = AXIS2_PLACEMENT_3D('',#121478,#95343,#95344) ;
#75284 = AXIS2_PLACEMENT_3D('',#121479,#95345,#95346) ;
#75285 = AXIS2_PLACEMENT_3D('',#121480,#95347,#95348) ;
#75286 = AXIS2_PLACEMENT_3D('',#121481,#95349,#95350) ;
#75287 = AXIS2_PLACEMENT_3D('',#121482,#95351,#95352) ;
#75288 = AXIS2_PLACEMENT_3D('',#121483,#95353,#95354) ;
#75289 = AXIS2_PLACEMENT_3D('',#121484,#95355,#95356) ;
#75290 = AXIS2_PLACEMENT_3D('',#121485,#95357,#95358) ;
#75291 = AXIS2_PLACEMENT_3D('',#121486,#95359,#95360) ;
#75292 = AXIS2_PLACEMENT_3D('',#121487,#95361,#95362) ;
#75293 = AXIS2_PLACEMENT_3D('',#121488,#95363,#95364) ;
#75294 = AXIS2_PLACEMENT_3D('',#121489,#95365,#95366) ;
#75295 = AXIS2_PLACEMENT_3D('',#121490,#95367,#95368) ;
#75296 = AXIS2_PLACEMENT_3D('',#121493,#95370,#95371) ;
#75297 = AXIS2_PLACEMENT_3D('',#121494,#95372,#95373) ;
#75298 = AXIS2_PLACEMENT_3D('',#121495,#95374,#95375) ;
#75299 = AXIS2_PLACEMENT_3D('',#121496,#95376,#95377) ;
#75300 = AXIS2_PLACEMENT_3D('',#121497,#95378,#95379) ;
#75301 = AXIS2_PLACEMENT_3D('',#121498,#95380,#95381) ;
#75302 = AXIS2_PLACEMENT_3D('',#121499,#95382,#95383) ;
#75303 = AXIS2_PLACEMENT_3D('',#121500,#95384,#95385) ;
#75304 = AXIS2_PLACEMENT_3D('',#121501,#95386,#95387) ;
#75305 = AXIS2_PLACEMENT_3D('',#121502,#95388,#95389) ;
#75306 = AXIS2_PLACEMENT_3D('',#121503,#95390,#95391) ;
#75307 = AXIS2_PLACEMENT_3D('',#121504,#95392,#95393) ;
#75308 = AXIS2_PLACEMENT_3D('',#121505,#95394,#95395) ;
#75309 = AXIS2_PLACEMENT_3D('',#121506,#95396,#95397) ;
#75310 = AXIS2_PLACEMENT_3D('',#121507,#95398,#95399) ;
#75311 = AXIS2_PLACEMENT_3D('',#121508,#95400,#95401) ;
#75312 = AXIS2_PLACEMENT_3D('',#121510,#95402,#95403) ;
#75313 = AXIS2_PLACEMENT_3D('',#121511,#95404,#95405) ;
#75314 = AXIS2_PLACEMENT_3D('',#121512,#95406,#95407) ;
#75315 = AXIS2_PLACEMENT_3D('',#121513,#95408,#95409) ;
#75316 = AXIS2_PLACEMENT_3D('',#121514,#95410,#95411) ;
#75317 = AXIS2_PLACEMENT_3D('',#121515,#95412,#95413) ;
#75318 = AXIS2_PLACEMENT_3D('',#121516,#95414,#95415) ;
#75319 = AXIS2_PLACEMENT_3D('',#121517,#95416,#95417) ;
#75320 = AXIS2_PLACEMENT_3D('',#121518,#95418,#95419) ;
#75321 = AXIS2_PLACEMENT_3D('',#121519,#95420,#95421) ;
#75322 = AXIS2_PLACEMENT_3D('',#121520,#95422,#95423) ;
#75323 = AXIS2_PLACEMENT_3D('',#121521,#95424,#95425) ;
#75324 = AXIS2_PLACEMENT_3D('',#121522,#95426,#95427) ;
#75325 = AXIS2_PLACEMENT_3D('',#121525,#95429,#95430) ;
#75326 = AXIS2_PLACEMENT_3D('',#121526,#95431,#95432) ;
#75327 = AXIS2_PLACEMENT_3D('',#121527,#95433,#95434) ;
#75328 = AXIS2_PLACEMENT_3D('',#121528,#95435,#95436) ;
#75329 = AXIS2_PLACEMENT_3D('',#121529,#95437,#95438) ;
#75330 = AXIS2_PLACEMENT_3D('',#121530,#95439,#95440) ;
#75331 = AXIS2_PLACEMENT_3D('',#121531,#95441,#95442) ;
#75332 = AXIS2_PLACEMENT_3D('',#121532,#95443,#95444) ;
#75333 = AXIS2_PLACEMENT_3D('',#121533,#95445,#95446) ;
#75334 = AXIS2_PLACEMENT_3D('',#121534,#95447,#95448) ;
#75335 = AXIS2_PLACEMENT_3D('',#121535,#95449,#95450) ;
#75336 = AXIS2_PLACEMENT_3D('',#121536,#95451,#95452) ;
#75337 = AXIS2_PLACEMENT_3D('',#121537,#95453,#95454) ;
#75338 = AXIS2_PLACEMENT_3D('',#121539,#95455,#95456) ;
#75339 = AXIS2_PLACEMENT_3D('',#121540,#95457,#95458) ;
#75340 = AXIS2_PLACEMENT_3D('',#121541,#95459,#95460) ;
#75341 = AXIS2_PLACEMENT_3D('',#121542,#95461,#95462) ;
#75342 = AXIS2_PLACEMENT_3D('',#121543,#95463,#95464) ;
#75343 = AXIS2_PLACEMENT_3D('',#121544,#95465,#95466) ;
#75344 = AXIS2_PLACEMENT_3D('',#121545,#95467,#95468) ;
#75345 = AXIS2_PLACEMENT_3D('',#121546,#95469,#95470) ;
#75346 = AXIS2_PLACEMENT_3D('',#121547,#95471,#95472) ;
#75347 = AXIS2_PLACEMENT_3D('',#121548,#95473,#95474) ;
#75348 = AXIS2_PLACEMENT_3D('',#121549,#95475,#95476) ;
#75349 = AXIS2_PLACEMENT_3D('',#121551,#95478,#95479) ;
#75350 = AXIS2_PLACEMENT_3D('',#121552,#95480,#95481) ;
#75351 = AXIS2_PLACEMENT_3D('',#121553,#95482,#95483) ;
#75352 = AXIS2_PLACEMENT_3D('',#121554,#95484,#95485) ;
#75353 = AXIS2_PLACEMENT_3D('',#121555,#95486,#95487) ;
#75354 = AXIS2_PLACEMENT_3D('',#121556,#95488,#95489) ;
#75355 = AXIS2_PLACEMENT_3D('',#121557,#95490,#95491) ;
#75356 = AXIS2_PLACEMENT_3D('',#121558,#95492,#95493) ;
#75357 = AXIS2_PLACEMENT_3D('',#121559,#95494,#95495) ;
#75358 = AXIS2_PLACEMENT_3D('',#121560,#95496,#95497) ;
#75359 = AXIS2_PLACEMENT_3D('',#121561,#95498,#95499) ;
#75360 = AXIS2_PLACEMENT_3D('',#121562,#95500,#95501) ;
#75361 = AXIS2_PLACEMENT_3D('',#121563,#95502,#95503) ;
#75362 = AXIS2_PLACEMENT_3D('',#121564,#95504,#95505) ;
#75363 = AXIS2_PLACEMENT_3D('',#121565,#95506,#95507) ;
#75364 = AXIS2_PLACEMENT_3D('',#121566,#95508,#95509) ;
#75365 = AXIS2_PLACEMENT_3D('',#121567,#95510,#95511) ;
#75366 = AXIS2_PLACEMENT_3D('',#121568,#95512,#95513) ;
#75367 = AXIS2_PLACEMENT_3D('',#121569,#95514,#95515) ;
#75368 = AXIS2_PLACEMENT_3D('',#121570,#95516,#95517) ;
#75369 = AXIS2_PLACEMENT_3D('',#121571,#95518,#95519) ;
#75370 = AXIS2_PLACEMENT_3D('',#121572,#95520,#95521) ;
#75371 = AXIS2_PLACEMENT_3D('',#121573,#95522,#95523) ;
#75372 = AXIS2_PLACEMENT_3D('',#121574,#95524,#95525) ;
#75373 = AXIS2_PLACEMENT_3D('',#121575,#95526,#95527) ;
#75374 = AXIS2_PLACEMENT_3D('',#121576,#95528,#95529) ;
#75375 = AXIS2_PLACEMENT_3D('',#121577,#95530,#95531) ;
#75376 = AXIS2_PLACEMENT_3D('',#121578,#95532,#95533) ;
#75377 = AXIS2_PLACEMENT_3D('',#121579,#95534,#95535) ;
#75378 = AXIS2_PLACEMENT_3D('',#121580,#95536,#95537) ;
#75379 = AXIS2_PLACEMENT_3D('',#121581,#95538,#95539) ;
#75380 = AXIS2_PLACEMENT_3D('',#121582,#95540,#95541) ;
#75381 = AXIS2_PLACEMENT_3D('',#121583,#95542,#95543) ;
#75382 = AXIS2_PLACEMENT_3D('',#121584,#95544,#95545) ;
#75383 = AXIS2_PLACEMENT_3D('',#121585,#95546,#95547) ;
#75384 = AXIS2_PLACEMENT_3D('',#121586,#95548,#95549) ;
#75385 = AXIS2_PLACEMENT_3D('',#121587,#95550,#95551) ;
#75386 = AXIS2_PLACEMENT_3D('',#121588,#95552,#95553) ;
#75387 = AXIS2_PLACEMENT_3D('',#121589,#95554,#95555) ;
#75388 = AXIS2_PLACEMENT_3D('',#121590,#95556,#95557) ;
#75389 = AXIS2_PLACEMENT_3D('',#121591,#95558,#95559) ;
#75390 = AXIS2_PLACEMENT_3D('',#121592,#95560,#95561) ;
#75391 = AXIS2_PLACEMENT_3D('',#121593,#95562,#95563) ;
#75392 = AXIS2_PLACEMENT_3D('',#121594,#95564,#95565) ;
#75393 = AXIS2_PLACEMENT_3D('',#121595,#95566,#95567) ;
#75394 = AXIS2_PLACEMENT_3D('',#121596,#95568,#95569) ;
#75395 = AXIS2_PLACEMENT_3D('',#121597,#95570,#95571) ;
#75396 = AXIS2_PLACEMENT_3D('',#121598,#95572,#95573) ;
#75397 = AXIS2_PLACEMENT_3D('',#121599,#95574,#95575) ;
#75398 = AXIS2_PLACEMENT_3D('',#121600,#95576,#95577) ;
#75399 = AXIS2_PLACEMENT_3D('',#121601,#95578,#95579) ;
#75400 = AXIS2_PLACEMENT_3D('',#121602,#95580,#95581) ;
#75401 = AXIS2_PLACEMENT_3D('',#121603,#95582,#95583) ;
#75402 = AXIS2_PLACEMENT_3D('',#121604,#95584,#95585) ;
#75403 = AXIS2_PLACEMENT_3D('',#121605,#95586,#95587) ;
#75404 = AXIS2_PLACEMENT_3D('',#121606,#95588,#95589) ;
#75405 = AXIS2_PLACEMENT_3D('',#121607,#95590,#95591) ;
#75406 = AXIS2_PLACEMENT_3D('',#121608,#95592,#95593) ;
#75407 = AXIS2_PLACEMENT_3D('',#121609,#95594,#95595) ;
#75408 = AXIS2_PLACEMENT_3D('',#121610,#95596,#95597) ;
#75409 = AXIS2_PLACEMENT_3D('',#121611,#95598,#95599) ;
#75410 = AXIS2_PLACEMENT_3D('',#121620,#95604,#95605) ;
#75411 = AXIS2_PLACEMENT_3D('',#121629,#95610,#95611) ;
#75412 = AXIS2_PLACEMENT_3D('',#121638,#95616,#95617) ;
#75413 = AXIS2_PLACEMENT_3D('',#121647,#95622,#95623) ;
#75414 = AXIS2_PLACEMENT_3D('',#121656,#95628,#95629) ;
#75415 = AXIS2_PLACEMENT_3D('',#121660,#95631,#95632) ;
#75416 = AXIS2_PLACEMENT_3D('',#121662,#95633,#95634) ;
#75417 = AXIS2_PLACEMENT_3D('',#121666,#95637,#95638) ;
#75418 = AXIS2_PLACEMENT_3D('',#121670,#95640,#95641) ;
#75419 = AXIS2_PLACEMENT_3D('',#121672,#95642,#95643) ;
#75420 = AXIS2_PLACEMENT_3D('',#121676,#95646,#95647) ;
#75421 = AXIS2_PLACEMENT_3D('',#121677,#95648,#95649) ;
#75422 = AXIS2_PLACEMENT_3D('',#121678,#95650,#95651) ;
#75423 = AXIS2_PLACEMENT_3D('',#121679,#95652,#95653) ;
#75424 = AXIS2_PLACEMENT_3D('',#121680,#95654,#95655) ;
#75425 = AXIS2_PLACEMENT_3D('',#121681,#95656,#95657) ;
#75426 = AXIS2_PLACEMENT_3D('',#121682,#95658,#95659) ;
#75427 = AXIS2_PLACEMENT_3D('',#121691,#95664,#95665) ;
#75428 = AXIS2_PLACEMENT_3D('',#121697,#95669,#95670) ;
#75429 = AXIS2_PLACEMENT_3D('',#121703,#95674,#95675) ;
#75430 = AXIS2_PLACEMENT_3D('',#121712,#95680,#95681) ;
#75431 = AXIS2_PLACEMENT_3D('',#121721,#95686,#95687) ;
#75432 = AXIS2_PLACEMENT_3D('',#121727,#95691,#95692) ;
#75433 = AXIS2_PLACEMENT_3D('',#121733,#95696,#95697) ;
#75434 = AXIS2_PLACEMENT_3D('',#121742,#95702,#95703) ;
#75435 = AXIS2_PLACEMENT_3D('',#121751,#95708,#95709) ;
#75436 = AXIS2_PLACEMENT_3D('',#121760,#95714,#95715) ;
#75437 = AXIS2_PLACEMENT_3D('',#121769,#95720,#95721) ;
#75438 = AXIS2_PLACEMENT_3D('',#121778,#95726,#95727) ;
#75439 = AXIS2_PLACEMENT_3D('',#121782,#95729,#95730) ;
#75440 = AXIS2_PLACEMENT_3D('',#121784,#95731,#95732) ;
#75441 = AXIS2_PLACEMENT_3D('',#121788,#95735,#95736) ;
#75442 = AXIS2_PLACEMENT_3D('',#121792,#95738,#95739) ;
#75443 = AXIS2_PLACEMENT_3D('',#121794,#95740,#95741) ;
#75444 = AXIS2_PLACEMENT_3D('',#121798,#95744,#95745) ;
#75445 = AXIS2_PLACEMENT_3D('',#121799,#95746,#95747) ;
#75446 = AXIS2_PLACEMENT_3D('',#121800,#95748,#95749) ;
#75447 = AXIS2_PLACEMENT_3D('',#121801,#95750,#95751) ;
#75448 = AXIS2_PLACEMENT_3D('',#121802,#95752,#95753) ;
#75449 = AXIS2_PLACEMENT_3D('',#121803,#95754,#95755) ;
#75450 = AXIS2_PLACEMENT_3D('',#121804,#95756,#95757) ;
#75451 = AXIS2_PLACEMENT_3D('',#121813,#95762,#95763) ;
#75452 = AXIS2_PLACEMENT_3D('',#121819,#95767,#95768) ;
#75453 = AXIS2_PLACEMENT_3D('',#121825,#95772,#95773) ;
#75454 = AXIS2_PLACEMENT_3D('',#121834,#95778,#95779) ;
#75455 = AXIS2_PLACEMENT_3D('',#121843,#95784,#95785) ;
#75456 = AXIS2_PLACEMENT_3D('',#121849,#95789,#95790) ;
#75457 = AXIS2_PLACEMENT_3D('',#121855,#95794,#95795) ;
#75458 = AXIS2_PLACEMENT_3D('',#121864,#95800,#95801) ;
#75459 = AXIS2_PLACEMENT_3D('',#121873,#95806,#95807) ;
#75460 = AXIS2_PLACEMENT_3D('',#121882,#95812,#95813) ;
#75461 = AXIS2_PLACEMENT_3D('',#121891,#95818,#95819) ;
#75462 = AXIS2_PLACEMENT_3D('',#121900,#95824,#95825) ;
#75463 = AXIS2_PLACEMENT_3D('',#121904,#95827,#95828) ;
#75464 = AXIS2_PLACEMENT_3D('',#121906,#95829,#95830) ;
#75465 = AXIS2_PLACEMENT_3D('',#121910,#95833,#95834) ;
#75466 = AXIS2_PLACEMENT_3D('',#121914,#95836,#95837) ;
#75467 = AXIS2_PLACEMENT_3D('',#121916,#95838,#95839) ;
#75468 = AXIS2_PLACEMENT_3D('',#121920,#95842,#95843) ;
#75469 = AXIS2_PLACEMENT_3D('',#121921,#95844,#95845) ;
#75470 = AXIS2_PLACEMENT_3D('',#121922,#95846,#95847) ;
#75471 = AXIS2_PLACEMENT_3D('',#121923,#95848,#95849) ;
#75472 = AXIS2_PLACEMENT_3D('',#121924,#95850,#95851) ;
#75473 = AXIS2_PLACEMENT_3D('',#121925,#95852,#95853) ;
#75474 = AXIS2_PLACEMENT_3D('',#121926,#95854,#95855) ;
#75475 = AXIS2_PLACEMENT_3D('',#121935,#95860,#95861) ;
#75476 = AXIS2_PLACEMENT_3D('',#121941,#95865,#95866) ;
#75477 = AXIS2_PLACEMENT_3D('',#121947,#95870,#95871) ;
#75478 = AXIS2_PLACEMENT_3D('',#121956,#95876,#95877) ;
#75479 = AXIS2_PLACEMENT_3D('',#121965,#95882,#95883) ;
#75480 = AXIS2_PLACEMENT_3D('',#121971,#95887,#95888) ;
#75481 = AXIS2_PLACEMENT_3D('',#121977,#95892,#95893) ;
#75482 = AXIS2_PLACEMENT_3D('',#121986,#95898,#95899) ;
#75483 = AXIS2_PLACEMENT_3D('',#121995,#95904,#95905) ;
#75484 = AXIS2_PLACEMENT_3D('',#122004,#95910,#95911) ;
#75485 = AXIS2_PLACEMENT_3D('',#122013,#95916,#95917) ;
#75486 = AXIS2_PLACEMENT_3D('',#122022,#95922,#95923) ;
#75487 = AXIS2_PLACEMENT_3D('',#122026,#95925,#95926) ;
#75488 = AXIS2_PLACEMENT_3D('',#122028,#95927,#95928) ;
#75489 = AXIS2_PLACEMENT_3D('',#122032,#95931,#95932) ;
#75490 = AXIS2_PLACEMENT_3D('',#122036,#95934,#95935) ;
#75491 = AXIS2_PLACEMENT_3D('',#122038,#95936,#95937) ;
#75492 = AXIS2_PLACEMENT_3D('',#122042,#95940,#95941) ;
#75493 = AXIS2_PLACEMENT_3D('',#122043,#95942,#95943) ;
#75494 = AXIS2_PLACEMENT_3D('',#122044,#95944,#95945) ;
#75495 = AXIS2_PLACEMENT_3D('',#122045,#95946,#95947) ;
#75496 = AXIS2_PLACEMENT_3D('',#122046,#95948,#95949) ;
#75497 = AXIS2_PLACEMENT_3D('',#122047,#95950,#95951) ;
#75498 = AXIS2_PLACEMENT_3D('',#122048,#95952,#95953) ;
#75499 = AXIS2_PLACEMENT_3D('',#122057,#95958,#95959) ;
#75500 = AXIS2_PLACEMENT_3D('',#122063,#95963,#95964) ;
#75501 = AXIS2_PLACEMENT_3D('',#122069,#95968,#95969) ;
#75502 = AXIS2_PLACEMENT_3D('',#122078,#95974,#95975) ;
#75503 = AXIS2_PLACEMENT_3D('',#122087,#95980,#95981) ;
#75504 = AXIS2_PLACEMENT_3D('',#122093,#95985,#95986) ;
#75505 = AXIS2_PLACEMENT_3D('',#122099,#95990,#95991) ;
#75506 = AXIS2_PLACEMENT_3D('',#122108,#95996,#95997) ;
#75507 = AXIS2_PLACEMENT_3D('',#122117,#96002,#96003) ;
#75508 = AXIS2_PLACEMENT_3D('',#122126,#96008,#96009) ;
#75509 = AXIS2_PLACEMENT_3D('',#122135,#96014,#96015) ;
#75510 = AXIS2_PLACEMENT_3D('',#122144,#96020,#96021) ;
#75511 = AXIS2_PLACEMENT_3D('',#122148,#96023,#96024) ;
#75512 = AXIS2_PLACEMENT_3D('',#122150,#96025,#96026) ;
#75513 = AXIS2_PLACEMENT_3D('',#122154,#96029,#96030) ;
#75514 = AXIS2_PLACEMENT_3D('',#122158,#96032,#96033) ;
#75515 = AXIS2_PLACEMENT_3D('',#122160,#96034,#96035) ;
#75516 = AXIS2_PLACEMENT_3D('',#122164,#96038,#96039) ;
#75517 = AXIS2_PLACEMENT_3D('',#122165,#96040,#96041) ;
#75518 = AXIS2_PLACEMENT_3D('',#122166,#96042,#96043) ;
#75519 = AXIS2_PLACEMENT_3D('',#122167,#96044,#96045) ;
#75520 = AXIS2_PLACEMENT_3D('',#122168,#96046,#96047) ;
#75521 = AXIS2_PLACEMENT_3D('',#122169,#96048,#96049) ;
#75522 = AXIS2_PLACEMENT_3D('',#122170,#96050,#96051) ;
#75523 = AXIS2_PLACEMENT_3D('',#122179,#96056,#96057) ;
#75524 = AXIS2_PLACEMENT_3D('',#122185,#96061,#96062) ;
#75525 = AXIS2_PLACEMENT_3D('',#122191,#96066,#96067) ;
#75526 = AXIS2_PLACEMENT_3D('',#122200,#96072,#96073) ;
#75527 = AXIS2_PLACEMENT_3D('',#122209,#96078,#96079) ;
#75528 = AXIS2_PLACEMENT_3D('',#122215,#96083,#96084) ;
#75529 = AXIS2_PLACEMENT_3D('',#122221,#96088,#96089) ;
#75530 = AXIS2_PLACEMENT_3D('',#122230,#96094,#96095) ;
#75531 = AXIS2_PLACEMENT_3D('',#122239,#96100,#96101) ;
#75532 = AXIS2_PLACEMENT_3D('',#122248,#96106,#96107) ;
#75533 = AXIS2_PLACEMENT_3D('',#122257,#96112,#96113) ;
#75534 = AXIS2_PLACEMENT_3D('',#122266,#96118,#96119) ;
#75535 = AXIS2_PLACEMENT_3D('',#122270,#96121,#96122) ;
#75536 = AXIS2_PLACEMENT_3D('',#122272,#96123,#96124) ;
#75537 = AXIS2_PLACEMENT_3D('',#122276,#96127,#96128) ;
#75538 = AXIS2_PLACEMENT_3D('',#122280,#96130,#96131) ;
#75539 = AXIS2_PLACEMENT_3D('',#122282,#96132,#96133) ;
#75540 = AXIS2_PLACEMENT_3D('',#122286,#96136,#96137) ;
#75541 = AXIS2_PLACEMENT_3D('',#122287,#96138,#96139) ;
#75542 = AXIS2_PLACEMENT_3D('',#122288,#96140,#96141) ;
#75543 = AXIS2_PLACEMENT_3D('',#122289,#96142,#96143) ;
#75544 = AXIS2_PLACEMENT_3D('',#122290,#96144,#96145) ;
#75545 = AXIS2_PLACEMENT_3D('',#122291,#96146,#96147) ;
#75546 = AXIS2_PLACEMENT_3D('',#122292,#96148,#96149) ;
#75547 = AXIS2_PLACEMENT_3D('',#122301,#96154,#96155) ;
#75548 = AXIS2_PLACEMENT_3D('',#122307,#96159,#96160) ;
#75549 = AXIS2_PLACEMENT_3D('',#122313,#96164,#96165) ;
#75550 = AXIS2_PLACEMENT_3D('',#122322,#96170,#96171) ;
#75551 = AXIS2_PLACEMENT_3D('',#122331,#96176,#96177) ;
#75552 = AXIS2_PLACEMENT_3D('',#122337,#96181,#96182) ;
#75553 = AXIS2_PLACEMENT_3D('',#122343,#96186,#96187) ;
#75554 = AXIS2_PLACEMENT_3D('',#122352,#96192,#96193) ;
#75555 = AXIS2_PLACEMENT_3D('',#122361,#96198,#96199) ;
#75556 = AXIS2_PLACEMENT_3D('',#122370,#96204,#96205) ;
#75557 = AXIS2_PLACEMENT_3D('',#122379,#96210,#96211) ;
#75558 = AXIS2_PLACEMENT_3D('',#122388,#96216,#96217) ;
#75559 = AXIS2_PLACEMENT_3D('',#122392,#96219,#96220) ;
#75560 = AXIS2_PLACEMENT_3D('',#122394,#96221,#96222) ;
#75561 = AXIS2_PLACEMENT_3D('',#122398,#96225,#96226) ;
#75562 = AXIS2_PLACEMENT_3D('',#122402,#96228,#96229) ;
#75563 = AXIS2_PLACEMENT_3D('',#122404,#96230,#96231) ;
#75564 = AXIS2_PLACEMENT_3D('',#122408,#96234,#96235) ;
#75565 = AXIS2_PLACEMENT_3D('',#122409,#96236,#96237) ;
#75566 = AXIS2_PLACEMENT_3D('',#122410,#96238,#96239) ;
#75567 = AXIS2_PLACEMENT_3D('',#122411,#96240,#96241) ;
#75568 = AXIS2_PLACEMENT_3D('',#122412,#96242,#96243) ;
#75569 = AXIS2_PLACEMENT_3D('',#122413,#96244,#96245) ;
#75570 = AXIS2_PLACEMENT_3D('',#122414,#96246,#96247) ;
#75571 = AXIS2_PLACEMENT_3D('',#122423,#96252,#96253) ;
#75572 = AXIS2_PLACEMENT_3D('',#122429,#96257,#96258) ;
#75573 = AXIS2_PLACEMENT_3D('',#122435,#96262,#96263) ;
#75574 = AXIS2_PLACEMENT_3D('',#122444,#96268,#96269) ;
#75575 = AXIS2_PLACEMENT_3D('',#122453,#96274,#96275) ;
#75576 = AXIS2_PLACEMENT_3D('',#122459,#96279,#96280) ;
#75577 = AXIS2_PLACEMENT_3D('',#122465,#96284,#96285) ;
#75578 = AXIS2_PLACEMENT_3D('',#122474,#96290,#96291) ;
#75579 = AXIS2_PLACEMENT_3D('',#122483,#96296,#96297) ;
#75580 = AXIS2_PLACEMENT_3D('',#122492,#96302,#96303) ;
#75581 = AXIS2_PLACEMENT_3D('',#122501,#96308,#96309) ;
#75582 = AXIS2_PLACEMENT_3D('',#122510,#96314,#96315) ;
#75583 = AXIS2_PLACEMENT_3D('',#122514,#96317,#96318) ;
#75584 = AXIS2_PLACEMENT_3D('',#122516,#96319,#96320) ;
#75585 = AXIS2_PLACEMENT_3D('',#122520,#96323,#96324) ;
#75586 = AXIS2_PLACEMENT_3D('',#122524,#96326,#96327) ;
#75587 = AXIS2_PLACEMENT_3D('',#122526,#96328,#96329) ;
#75588 = AXIS2_PLACEMENT_3D('',#122530,#96332,#96333) ;
#75589 = AXIS2_PLACEMENT_3D('',#122531,#96334,#96335) ;
#75590 = AXIS2_PLACEMENT_3D('',#122532,#96336,#96337) ;
#75591 = AXIS2_PLACEMENT_3D('',#122533,#96338,#96339) ;
#75592 = AXIS2_PLACEMENT_3D('',#122534,#96340,#96341) ;
#75593 = AXIS2_PLACEMENT_3D('',#122535,#96342,#96343) ;
#75594 = AXIS2_PLACEMENT_3D('',#122536,#96344,#96345) ;
#75595 = AXIS2_PLACEMENT_3D('',#122545,#96350,#96351) ;
#75596 = AXIS2_PLACEMENT_3D('',#122551,#96355,#96356) ;
#75597 = AXIS2_PLACEMENT_3D('',#122557,#96360,#96361) ;
#75598 = AXIS2_PLACEMENT_3D('',#122566,#96366,#96367) ;
#75599 = AXIS2_PLACEMENT_3D('',#122575,#96372,#96373) ;
#75600 = AXIS2_PLACEMENT_3D('',#122581,#96377,#96378) ;
#75601 = AXIS2_PLACEMENT_3D('',#122587,#96382,#96383) ;
#75602 = AXIS2_PLACEMENT_3D('',#122596,#96388,#96389) ;
#75603 = AXIS2_PLACEMENT_3D('',#122605,#96394,#96395) ;
#75604 = AXIS2_PLACEMENT_3D('',#122614,#96400,#96401) ;
#75605 = AXIS2_PLACEMENT_3D('',#122623,#96406,#96407) ;
#75606 = AXIS2_PLACEMENT_3D('',#122632,#96412,#96413) ;
#75607 = AXIS2_PLACEMENT_3D('',#122636,#96415,#96416) ;
#75608 = AXIS2_PLACEMENT_3D('',#122638,#96417,#96418) ;
#75609 = AXIS2_PLACEMENT_3D('',#122642,#96421,#96422) ;
#75610 = AXIS2_PLACEMENT_3D('',#122646,#96424,#96425) ;
#75611 = AXIS2_PLACEMENT_3D('',#122648,#96426,#96427) ;
#75612 = AXIS2_PLACEMENT_3D('',#122652,#96430,#96431) ;
#75613 = AXIS2_PLACEMENT_3D('',#122653,#96432,#96433) ;
#75614 = AXIS2_PLACEMENT_3D('',#122654,#96434,#96435) ;
#75615 = AXIS2_PLACEMENT_3D('',#122655,#96436,#96437) ;
#75616 = AXIS2_PLACEMENT_3D('',#122656,#96438,#96439) ;
#75617 = AXIS2_PLACEMENT_3D('',#122657,#96440,#96441) ;
#75618 = AXIS2_PLACEMENT_3D('',#122658,#96442,#96443) ;
#75619 = AXIS2_PLACEMENT_3D('',#122667,#96448,#96449) ;
#75620 = AXIS2_PLACEMENT_3D('',#122673,#96453,#96454) ;
#75621 = AXIS2_PLACEMENT_3D('',#122679,#96458,#96459) ;
#75622 = AXIS2_PLACEMENT_3D('',#122688,#96464,#96465) ;
#75623 = AXIS2_PLACEMENT_3D('',#122697,#96470,#96471) ;
#75624 = AXIS2_PLACEMENT_3D('',#122703,#96475,#96476) ;
#75625 = AXIS2_PLACEMENT_3D('',#122709,#96480,#96481) ;
#75626 = AXIS2_PLACEMENT_3D('',#122718,#96486,#96487) ;
#75627 = AXIS2_PLACEMENT_3D('',#122727,#96492,#96493) ;
#75628 = AXIS2_PLACEMENT_3D('',#122736,#96498,#96499) ;
#75629 = AXIS2_PLACEMENT_3D('',#122745,#96504,#96505) ;
#75630 = AXIS2_PLACEMENT_3D('',#122754,#96510,#96511) ;
#75631 = AXIS2_PLACEMENT_3D('',#122763,#96516,#96517) ;
#75632 = AXIS2_PLACEMENT_3D('',#122772,#96522,#96523) ;
#75633 = AXIS2_PLACEMENT_3D('',#122781,#96528,#96529) ;
#75634 = AXIS2_PLACEMENT_3D('',#122790,#96534,#96535) ;
#75635 = AXIS2_PLACEMENT_3D('',#122799,#96540,#96541) ;
#75636 = AXIS2_PLACEMENT_3D('',#122808,#96546,#96547) ;
#75637 = AXIS2_PLACEMENT_3D('',#122817,#96552,#96553) ;
#75638 = AXIS2_PLACEMENT_3D('',#122826,#96558,#96559) ;
#75639 = AXIS2_PLACEMENT_3D('',#122835,#96564,#96565) ;
#75640 = AXIS2_PLACEMENT_3D('',#122844,#96570,#96571) ;
#75641 = AXIS2_PLACEMENT_3D('',#122853,#96576,#96577) ;
#75642 = AXIS2_PLACEMENT_3D('',#122862,#96582,#96583) ;
#75643 = AXIS2_PLACEMENT_3D('',#122871,#96588,#96589) ;
#75644 = AXIS2_PLACEMENT_3D('',#122880,#96594,#96595) ;
#75645 = AXIS2_PLACEMENT_3D('',#122889,#96600,#96601) ;
#75646 = AXIS2_PLACEMENT_3D('',#122898,#96606,#96607) ;
#75647 = AXIS2_PLACEMENT_3D('',#122907,#96612,#96613) ;
#75648 = AXIS2_PLACEMENT_3D('',#122916,#96618,#96619) ;
#75649 = AXIS2_PLACEMENT_3D('',#122925,#96624,#96625) ;
#75650 = AXIS2_PLACEMENT_3D('',#122934,#96630,#96631) ;
#75651 = AXIS2_PLACEMENT_3D('',#122943,#96636,#96637) ;
#75652 = AXIS2_PLACEMENT_3D('',#122952,#96642,#96643) ;
#75653 = AXIS2_PLACEMENT_3D('',#122961,#96648,#96649) ;
#75654 = AXIS2_PLACEMENT_3D('',#122970,#96654,#96655) ;
#75655 = AXIS2_PLACEMENT_3D('',#122979,#96660,#96661) ;
#75656 = AXIS2_PLACEMENT_3D('',#122988,#96666,#96667) ;
#75657 = AXIS2_PLACEMENT_3D('',#122997,#96672,#96673) ;
#75658 = AXIS2_PLACEMENT_3D('',#123006,#96678,#96679) ;
#75659 = AXIS2_PLACEMENT_3D('',#123015,#96684,#96685) ;
#75660 = AXIS2_PLACEMENT_3D('',#123024,#96690,#96691) ;
#75661 = AXIS2_PLACEMENT_3D('',#123033,#96696,#96697) ;
#75662 = AXIS2_PLACEMENT_3D('',#123034,#96698,#96699) ;
#75663 = AXIS2_PLACEMENT_3D('',#123035,#96700,#96701) ;
#75664 = AXIS2_PLACEMENT_3D('',#123036,#96702,#96703) ;
#75665 = AXIS2_PLACEMENT_3D('',#123037,#96704,#96705) ;
#75666 = AXIS2_PLACEMENT_3D('',#123038,#96706,#96707) ;
#75667 = AXIS2_PLACEMENT_3D('',#123039,#96708,#96709) ;
#75668 = AXIS2_PLACEMENT_3D('',#123040,#96710,#96711) ;
#75669 = AXIS2_PLACEMENT_3D('',#123041,#96712,#96713) ;
#75670 = AXIS2_PLACEMENT_3D('',#123042,#96714,#96715) ;
#75671 = AXIS2_PLACEMENT_3D('',#123043,#96716,#96717) ;
#75672 = AXIS2_PLACEMENT_3D('',#123044,#96718,#96719) ;
#75673 = AXIS2_PLACEMENT_3D('',#123045,#96720,#96721) ;
#75674 = AXIS2_PLACEMENT_3D('',#123046,#96722,#96723) ;
#75675 = AXIS2_PLACEMENT_3D('',#123047,#96724,#96725) ;
#75676 = AXIS2_PLACEMENT_3D('',#123048,#96726,#96727) ;
#75677 = AXIS2_PLACEMENT_3D('',#123049,#96728,#96729) ;
#75678 = AXIS2_PLACEMENT_3D('',#123050,#96730,#96731) ;
#75679 = AXIS2_PLACEMENT_3D('',#123051,#96732,#96733) ;
#75680 = AXIS2_PLACEMENT_3D('',#123052,#96734,#96735) ;
#75681 = AXIS2_PLACEMENT_3D('',#123053,#96736,#96737) ;
#75682 = AXIS2_PLACEMENT_3D('',#123054,#96738,#96739) ;
#75683 = AXIS2_PLACEMENT_3D('',#123055,#96740,#96741) ;
#75684 = AXIS2_PLACEMENT_3D('',#123056,#96742,#96743) ;
#75685 = AXIS2_PLACEMENT_3D('',#123057,#96744,#96745) ;
#75686 = AXIS2_PLACEMENT_3D('',#123058,#96746,#96747) ;
#75687 = AXIS2_PLACEMENT_3D('',#123059,#96748,#96749) ;
#75688 = AXIS2_PLACEMENT_3D('',#123060,#96750,#96751) ;
#75689 = AXIS2_PLACEMENT_3D('',#123061,#96752,#96753) ;
#75690 = AXIS2_PLACEMENT_3D('',#123062,#96754,#96755) ;
#75691 = AXIS2_PLACEMENT_3D('',#123063,#96756,#96757) ;
#75692 = AXIS2_PLACEMENT_3D('',#123064,#96758,#96759) ;
#75693 = AXIS2_PLACEMENT_3D('',#123065,#96760,#96761) ;
#75694 = AXIS2_PLACEMENT_3D('',#123066,#96762,#96763) ;
#75695 = AXIS2_PLACEMENT_3D('',#123067,#96764,#96765) ;
#75696 = AXIS2_PLACEMENT_3D('',#123068,#96766,#96767) ;
#75697 = AXIS2_PLACEMENT_3D('',#123069,#96768,#96769) ;
#75698 = AXIS2_PLACEMENT_3D('',#123070,#96770,#96771) ;
#75699 = AXIS2_PLACEMENT_3D('',#123071,#96772,#96773) ;
#75700 = AXIS2_PLACEMENT_3D('',#123072,#96774,#96775) ;
#75701 = AXIS2_PLACEMENT_3D('',#123073,#96776,#96777) ;
#75702 = AXIS2_PLACEMENT_3D('',#123074,#96778,#96779) ;
#75703 = AXIS2_PLACEMENT_3D('',#123075,#96780,#96781) ;
#75704 = AXIS2_PLACEMENT_3D('',#123076,#96782,#96783) ;
#75705 = AXIS2_PLACEMENT_3D('',#123077,#96784,#96785) ;
#75706 = AXIS2_PLACEMENT_3D('',#123078,#96786,#96787) ;
#75707 = AXIS2_PLACEMENT_3D('',#123079,#96788,#96789) ;
#75708 = AXIS2_PLACEMENT_3D('',#123080,#96790,#96791) ;
#75709 = AXIS2_PLACEMENT_3D('',#123081,#96792,#96793) ;
#75710 = AXIS2_PLACEMENT_3D('',#123082,#96794,#96795) ;
#75711 = AXIS2_PLACEMENT_3D('',#123083,#96796,#96797) ;
#75712 = AXIS2_PLACEMENT_3D('',#123084,#96798,#96799) ;
#75713 = AXIS2_PLACEMENT_3D('',#123085,#96800,#96801) ;
#75714 = AXIS2_PLACEMENT_3D('',#123086,#96802,#96803) ;
#75715 = AXIS2_PLACEMENT_3D('',#123087,#96804,#96805) ;
#75716 = AXIS2_PLACEMENT_3D('',#123088,#96806,#96807) ;
#75717 = AXIS2_PLACEMENT_3D('',#123089,#96808,#96809) ;
#75718 = AXIS2_PLACEMENT_3D('',#123090,#96810,#96811) ;
#75719 = AXIS2_PLACEMENT_3D('',#123091,#96812,#96813) ;
#75720 = AXIS2_PLACEMENT_3D('',#123092,#96814,#96815) ;
#75721 = AXIS2_PLACEMENT_3D('',#123093,#96816,#96817) ;
#75722 = AXIS2_PLACEMENT_3D('',#123094,#96818,#96819) ;
#75723 = AXIS2_PLACEMENT_3D('',#123095,#96820,#96821) ;
#75724 = AXIS2_PLACEMENT_3D('',#123096,#96822,#96823) ;
#75725 = AXIS2_PLACEMENT_3D('',#123097,#96824,#96825) ;
#75726 = AXIS2_PLACEMENT_3D('',#123098,#96826,#96827) ;
#75727 = AXIS2_PLACEMENT_3D('',#123099,#96828,#96829) ;
#75728 = AXIS2_PLACEMENT_3D('',#123100,#96830,#96831) ;
#75729 = AXIS2_PLACEMENT_3D('',#123101,#96832,#96833) ;
#75730 = AXIS2_PLACEMENT_3D('',#123102,#96834,#96835) ;
#75731 = AXIS2_PLACEMENT_3D('',#123103,#96836,#96837) ;
#75732 = AXIS2_PLACEMENT_3D('',#123104,#96838,#96839) ;
#75733 = AXIS2_PLACEMENT_3D('',#123105,#96840,#96841) ;
#75734 = AXIS2_PLACEMENT_3D('',#123106,#96842,#96843) ;
#75735 = AXIS2_PLACEMENT_3D('',#123107,#96844,#96845) ;
#75736 = AXIS2_PLACEMENT_3D('',#123108,#96846,#96847) ;
#75737 = AXIS2_PLACEMENT_3D('',#123109,#96848,#96849) ;
#75738 = AXIS2_PLACEMENT_3D('',#123110,#96850,#96851) ;
#75739 = AXIS2_PLACEMENT_3D('',#123111,#96852,#96853) ;
#75740 = AXIS2_PLACEMENT_3D('',#123112,#96854,#96855) ;
#75741 = AXIS2_PLACEMENT_3D('',#123113,#96856,#96857) ;
#75742 = AXIS2_PLACEMENT_3D('',#123114,#96858,#96859) ;
#75743 = AXIS2_PLACEMENT_3D('',#123115,#96860,#96861) ;
#75744 = AXIS2_PLACEMENT_3D('',#123116,#96862,#96863) ;
#75745 = AXIS2_PLACEMENT_3D('',#123117,#96864,#96865) ;
#75746 = AXIS2_PLACEMENT_3D('',#123118,#96866,#96867) ;
#75747 = AXIS2_PLACEMENT_3D('',#123119,#96868,#96869) ;
#75748 = AXIS2_PLACEMENT_3D('',#123120,#96870,#96871) ;
#75749 = AXIS2_PLACEMENT_3D('',#123121,#96872,#96873) ;
#75750 = AXIS2_PLACEMENT_3D('',#123122,#96874,#96875) ;
#75751 = AXIS2_PLACEMENT_3D('',#123123,#96876,#96877) ;
#75752 = AXIS2_PLACEMENT_3D('',#123124,#96878,#96879) ;
#75753 = AXIS2_PLACEMENT_3D('',#123125,#96880,#96881) ;
#75754 = AXIS2_PLACEMENT_3D('',#123126,#96882,#96883) ;
#75755 = AXIS2_PLACEMENT_3D('',#123127,#96884,#96885) ;
#75756 = AXIS2_PLACEMENT_3D('',#123128,#96886,#96887) ;
#75757 = AXIS2_PLACEMENT_3D('',#123129,#96888,#96889) ;
#75758 = AXIS2_PLACEMENT_3D('',#123130,#96890,#96891) ;
#75759 = AXIS2_PLACEMENT_3D('',#123131,#96892,#96893) ;
#75760 = AXIS2_PLACEMENT_3D('',#123132,#96894,#96895) ;
#75761 = AXIS2_PLACEMENT_3D('',#123133,#96896,#96897) ;
#75762 = AXIS2_PLACEMENT_3D('',#123134,#96898,#96899) ;
#75763 = AXIS2_PLACEMENT_3D('',#123135,#96900,#96901) ;
#75764 = AXIS2_PLACEMENT_3D('',#123136,#96902,#96903) ;
#75765 = AXIS2_PLACEMENT_3D('',#123137,#96904,#96905) ;
#75766 = AXIS2_PLACEMENT_3D('',#123138,#96906,#96907) ;
#75767 = AXIS2_PLACEMENT_3D('',#123139,#96908,#96909) ;
#75768 = AXIS2_PLACEMENT_3D('',#123140,#96910,#96911) ;
#75769 = AXIS2_PLACEMENT_3D('',#123141,#96912,#96913) ;
#75770 = AXIS2_PLACEMENT_3D('',#123142,#96914,#96915) ;
#75771 = AXIS2_PLACEMENT_3D('',#123143,#96916,#96917) ;
#75772 = AXIS2_PLACEMENT_3D('',#123144,#96918,#96919) ;
#75773 = AXIS2_PLACEMENT_3D('',#123145,#96920,#96921) ;
#75774 = AXIS2_PLACEMENT_3D('',#123146,#96922,#96923) ;
#75775 = AXIS2_PLACEMENT_3D('',#123147,#96924,#96925) ;
#75776 = AXIS2_PLACEMENT_3D('',#123148,#96926,#96927) ;
#75777 = AXIS2_PLACEMENT_3D('',#123149,#96928,#96929) ;
#75778 = AXIS2_PLACEMENT_3D('',#123150,#96930,#96931) ;
#75779 = AXIS2_PLACEMENT_3D('',#123151,#96932,#96933) ;
#75780 = AXIS2_PLACEMENT_3D('',#123152,#96934,#96935) ;
#75781 = AXIS2_PLACEMENT_3D('',#123153,#96936,#96937) ;
#75782 = AXIS2_PLACEMENT_3D('',#123154,#96938,#96939) ;
#75783 = AXIS2_PLACEMENT_3D('',#123155,#96940,#96941) ;
#75784 = AXIS2_PLACEMENT_3D('',#123156,#96942,#96943) ;
#75785 = AXIS2_PLACEMENT_3D('',#123157,#96944,#96945) ;
#75786 = AXIS2_PLACEMENT_3D('',#123158,#96946,#96947) ;
#75787 = AXIS2_PLACEMENT_3D('',#123159,#96948,#96949) ;
#75788 = AXIS2_PLACEMENT_3D('',#123160,#96950,#96951) ;
#75789 = AXIS2_PLACEMENT_3D('',#123161,#96952,#96953) ;
#75790 = AXIS2_PLACEMENT_3D('',#123162,#96954,#96955) ;
#75791 = AXIS2_PLACEMENT_3D('',#123163,#96956,#96957) ;
#75792 = AXIS2_PLACEMENT_3D('',#123164,#96958,#96959) ;
#75793 = AXIS2_PLACEMENT_3D('',#123165,#96960,#96961) ;
#75794 = AXIS2_PLACEMENT_3D('',#123166,#96962,#96963) ;
#75795 = AXIS2_PLACEMENT_3D('',#123167,#96964,#96965) ;
#75796 = AXIS2_PLACEMENT_3D('',#123168,#96966,#96967) ;
#75797 = AXIS2_PLACEMENT_3D('',#123169,#96968,#96969) ;
#75798 = AXIS2_PLACEMENT_3D('',#123170,#96970,#96971) ;
#75799 = AXIS2_PLACEMENT_3D('',#123171,#96972,#96973) ;
#75800 = AXIS2_PLACEMENT_3D('',#123172,#96974,#96975) ;
#75801 = AXIS2_PLACEMENT_3D('',#123173,#96976,#96977) ;
#75802 = AXIS2_PLACEMENT_3D('',#123174,#96978,#96979) ;
#75803 = AXIS2_PLACEMENT_3D('',#123175,#96980,#96981) ;
#75804 = AXIS2_PLACEMENT_3D('',#123176,#96982,#96983) ;
#75805 = AXIS2_PLACEMENT_3D('',#123177,#96984,#96985) ;
#75806 = AXIS2_PLACEMENT_3D('',#123178,#96986,#96987) ;
#75807 = AXIS2_PLACEMENT_3D('',#123179,#96988,#96989) ;
#75808 = AXIS2_PLACEMENT_3D('',#123180,#96990,#96991) ;
#75809 = AXIS2_PLACEMENT_3D('',#123181,#96992,#96993) ;
#75810 = AXIS2_PLACEMENT_3D('',#123182,#96994,#96995) ;
#75811 = AXIS2_PLACEMENT_3D('',#123183,#96996,#96997) ;
#75812 = AXIS2_PLACEMENT_3D('',#123184,#96998,#96999) ;
#75813 = AXIS2_PLACEMENT_3D('',#123185,#97000,#97001) ;
#75814 = AXIS2_PLACEMENT_3D('',#123186,#97002,#97003) ;
#75815 = AXIS2_PLACEMENT_3D('',#123187,#97004,#97005) ;
#75816 = AXIS2_PLACEMENT_3D('',#123188,#97006,#97007) ;
#75817 = AXIS2_PLACEMENT_3D('',#123189,#97008,#97009) ;
#75818 = AXIS2_PLACEMENT_3D('',#123190,#97010,#97011) ;
#75819 = AXIS2_PLACEMENT_3D('',#123191,#97012,#97013) ;
#75820 = AXIS2_PLACEMENT_3D('',#123192,#97014,#97015) ;
#75821 = AXIS2_PLACEMENT_3D('',#123193,#97016,#97017) ;
#75822 = AXIS2_PLACEMENT_3D('',#123194,#97018,#97019) ;
#75823 = AXIS2_PLACEMENT_3D('',#123195,#97020,#97021) ;
#75824 = AXIS2_PLACEMENT_3D('',#123196,#97022,#97023) ;
#75825 = AXIS2_PLACEMENT_3D('',#123197,#97024,#97025) ;
#75826 = AXIS2_PLACEMENT_3D('',#123198,#97026,#97027) ;
#75827 = AXIS2_PLACEMENT_3D('',#123199,#97028,#97029) ;
#75828 = AXIS2_PLACEMENT_3D('',#123200,#97030,#97031) ;
#75829 = AXIS2_PLACEMENT_3D('',#123201,#97032,#97033) ;
#75830 = AXIS2_PLACEMENT_3D('',#123202,#97034,#97035) ;
#75831 = AXIS2_PLACEMENT_3D('',#123203,#97036,#97037) ;
#75832 = AXIS2_PLACEMENT_3D('',#123204,#97038,#97039) ;
#75833 = AXIS2_PLACEMENT_3D('',#123205,#97040,#97041) ;
#75834 = AXIS2_PLACEMENT_3D('',#123206,#97042,#97043) ;
#75835 = AXIS2_PLACEMENT_3D('',#123207,#97044,#97045) ;
#75836 = AXIS2_PLACEMENT_3D('',#123208,#97046,#97047) ;
#75837 = AXIS2_PLACEMENT_3D('',#123209,#97048,#97049) ;
#75838 = AXIS2_PLACEMENT_3D('',#123210,#97050,#97051) ;
#75839 = AXIS2_PLACEMENT_3D('',#123211,#97052,#97053) ;
#75840 = AXIS2_PLACEMENT_3D('',#123212,#97054,#97055) ;
#75841 = AXIS2_PLACEMENT_3D('',#123213,#97056,#97057) ;
#75842 = AXIS2_PLACEMENT_3D('',#123214,#97058,#97059) ;
#75843 = AXIS2_PLACEMENT_3D('',#123215,#97060,#97061) ;
#75844 = AXIS2_PLACEMENT_3D('',#123216,#97062,#97063) ;
#75845 = AXIS2_PLACEMENT_3D('',#123217,#97064,#97065) ;
#75846 = AXIS2_PLACEMENT_3D('',#123218,#97066,#97067) ;
#75847 = AXIS2_PLACEMENT_3D('',#123219,#97068,#97069) ;
#75848 = AXIS2_PLACEMENT_3D('',#123220,#97070,#97071) ;
#75849 = AXIS2_PLACEMENT_3D('',#123221,#97072,#97073) ;
#75850 = AXIS2_PLACEMENT_3D('',#123222,#97074,#97075) ;
#75851 = AXIS2_PLACEMENT_3D('',#123223,#97076,#97077) ;
#75852 = AXIS2_PLACEMENT_3D('',#123224,#97078,#97079) ;
#75853 = AXIS2_PLACEMENT_3D('',#123225,#97080,#97081) ;
#75854 = AXIS2_PLACEMENT_3D('',#123226,#97082,#97083) ;
#75855 = AXIS2_PLACEMENT_3D('',#123227,#97084,#97085) ;
#75856 = AXIS2_PLACEMENT_3D('',#123228,#97086,#97087) ;
#75857 = AXIS2_PLACEMENT_3D('',#123229,#97088,#97089) ;
#75858 = AXIS2_PLACEMENT_3D('',#123230,#97090,#97091) ;
#75859 = AXIS2_PLACEMENT_3D('',#123231,#97092,#97093) ;
#75860 = AXIS2_PLACEMENT_3D('',#123232,#97094,#97095) ;
#75861 = AXIS2_PLACEMENT_3D('',#123233,#97096,#97097) ;
#75862 = AXIS2_PLACEMENT_3D('',#123234,#97098,#97099) ;
#75863 = AXIS2_PLACEMENT_3D('',#123235,#97100,#97101) ;
#75864 = AXIS2_PLACEMENT_3D('',#123236,#97102,#97103) ;
#75865 = AXIS2_PLACEMENT_3D('',#123237,#97104,#97105) ;
#75866 = AXIS2_PLACEMENT_3D('',#123238,#97106,#97107) ;
#75867 = AXIS2_PLACEMENT_3D('',#123239,#97108,#97109) ;
#75868 = AXIS2_PLACEMENT_3D('',#123240,#97110,#97111) ;
#75869 = AXIS2_PLACEMENT_3D('',#123241,#97112,#97113) ;
#75870 = AXIS2_PLACEMENT_3D('',#123242,#97114,#97115) ;
#75871 = AXIS2_PLACEMENT_3D('',#123243,#97116,#97117) ;
#75872 = AXIS2_PLACEMENT_3D('',#123244,#97118,#97119) ;
#75873 = AXIS2_PLACEMENT_3D('',#123245,#97120,#97121) ;
#75874 = AXIS2_PLACEMENT_3D('',#123246,#97122,#97123) ;
#75875 = AXIS2_PLACEMENT_3D('',#123247,#97124,#97125) ;
#75876 = AXIS2_PLACEMENT_3D('',#123248,#97126,#97127) ;
#75877 = AXIS2_PLACEMENT_3D('',#123249,#97128,#97129) ;
#75878 = AXIS2_PLACEMENT_3D('',#123250,#97130,#97131) ;
#75879 = AXIS2_PLACEMENT_3D('',#123251,#97132,#97133) ;
#75880 = AXIS2_PLACEMENT_3D('',#123252,#97134,#97135) ;
#75881 = AXIS2_PLACEMENT_3D('',#123253,#97136,#97137) ;
#75882 = AXIS2_PLACEMENT_3D('',#123254,#97138,#97139) ;
#75883 = AXIS2_PLACEMENT_3D('',#123255,#97140,#97141) ;
#75884 = AXIS2_PLACEMENT_3D('',#123256,#97142,#97143) ;
#75885 = AXIS2_PLACEMENT_3D('',#123257,#97144,#97145) ;
#75886 = AXIS2_PLACEMENT_3D('',#123258,#97146,#97147) ;
#75887 = AXIS2_PLACEMENT_3D('',#123259,#97148,#97149) ;
#75888 = AXIS2_PLACEMENT_3D('',#123260,#97150,#97151) ;
#75889 = AXIS2_PLACEMENT_3D('',#123261,#97152,#97153) ;
#75890 = AXIS2_PLACEMENT_3D('',#123262,#97154,#97155) ;
#75891 = AXIS2_PLACEMENT_3D('',#123263,#97156,#97157) ;
#75892 = AXIS2_PLACEMENT_3D('',#123264,#97158,#97159) ;
#75893 = AXIS2_PLACEMENT_3D('',#123265,#97160,#97161) ;
#75894 = AXIS2_PLACEMENT_3D('',#123266,#97162,#97163) ;
#75895 = AXIS2_PLACEMENT_3D('',#123267,#97164,#97165) ;
#75896 = AXIS2_PLACEMENT_3D('',#123268,#97166,#97167) ;
#75897 = AXIS2_PLACEMENT_3D('',#123269,#97168,#97169) ;
#75898 = AXIS2_PLACEMENT_3D('',#123270,#97170,#97171) ;
#75899 = AXIS2_PLACEMENT_3D('',#123271,#97172,#97173) ;
#75900 = AXIS2_PLACEMENT_3D('',#123272,#97174,#97175) ;
#75901 = AXIS2_PLACEMENT_3D('',#123273,#97176,#97177) ;
#75902 = AXIS2_PLACEMENT_3D('',#123274,#97178,#97179) ;
#75903 = AXIS2_PLACEMENT_3D('',#123275,#97180,#97181) ;
#75904 = AXIS2_PLACEMENT_3D('',#123276,#97182,#97183) ;
#75905 = AXIS2_PLACEMENT_3D('',#123277,#97184,#97185) ;
#75906 = AXIS2_PLACEMENT_3D('',#123278,#97186,#97187) ;
#75907 = AXIS2_PLACEMENT_3D('',#123279,#97188,#97189) ;
#75908 = AXIS2_PLACEMENT_3D('',#123280,#97190,#97191) ;
#75909 = AXIS2_PLACEMENT_3D('',#123281,#97192,#97193) ;
#75910 = AXIS2_PLACEMENT_3D('',#123282,#97194,#97195) ;
#75911 = AXIS2_PLACEMENT_3D('',#123283,#97196,#97197) ;
#75912 = AXIS2_PLACEMENT_3D('',#123284,#97198,#97199) ;
#75913 = AXIS2_PLACEMENT_3D('',#123285,#97200,#97201) ;
#75914 = AXIS2_PLACEMENT_3D('',#123286,#97202,#97203) ;
#75915 = AXIS2_PLACEMENT_3D('',#123287,#97204,#97205) ;
#75916 = AXIS2_PLACEMENT_3D('',#123288,#97206,#97207) ;
#75917 = AXIS2_PLACEMENT_3D('',#123289,#97208,#97209) ;
#75918 = AXIS2_PLACEMENT_3D('',#123290,#97210,#97211) ;
#75919 = AXIS2_PLACEMENT_3D('',#123291,#97212,#97213) ;
#75920 = AXIS2_PLACEMENT_3D('',#123292,#97214,#97215) ;
#75921 = AXIS2_PLACEMENT_3D('',#123293,#97216,#97217) ;
#75922 = AXIS2_PLACEMENT_3D('',#123294,#97218,#97219) ;
#75923 = AXIS2_PLACEMENT_3D('',#123295,#97220,#97221) ;
#75924 = AXIS2_PLACEMENT_3D('',#123296,#97222,#97223) ;
#75925 = AXIS2_PLACEMENT_3D('',#123297,#97224,#97225) ;
#75926 = AXIS2_PLACEMENT_3D('',#123298,#97226,#97227) ;
#75927 = AXIS2_PLACEMENT_3D('',#123299,#97228,#97229) ;
#75928 = AXIS2_PLACEMENT_3D('',#123300,#97230,#97231) ;
#75929 = AXIS2_PLACEMENT_3D('',#123301,#97232,#97233) ;
#75930 = AXIS2_PLACEMENT_3D('',#123302,#97234,#97235) ;
#75931 = AXIS2_PLACEMENT_3D('',#123303,#97236,#97237) ;
#75932 = AXIS2_PLACEMENT_3D('',#123304,#97238,#97239) ;
#75933 = AXIS2_PLACEMENT_3D('',#123305,#97240,#97241) ;
#75934 = AXIS2_PLACEMENT_3D('',#123306,#97242,#97243) ;
#75935 = AXIS2_PLACEMENT_3D('',#123307,#97244,#97245) ;
#75936 = AXIS2_PLACEMENT_3D('',#123308,#97246,#97247) ;
#75937 = AXIS2_PLACEMENT_3D('',#123309,#97248,#97249) ;
#75938 = AXIS2_PLACEMENT_3D('',#123310,#97250,#97251) ;
#75939 = AXIS2_PLACEMENT_3D('',#123311,#97252,#97253) ;
#75940 = AXIS2_PLACEMENT_3D('',#123312,#97254,#97255) ;
#75941 = AXIS2_PLACEMENT_3D('',#123313,#97256,#97257) ;
#75942 = AXIS2_PLACEMENT_3D('',#123314,#97258,#97259) ;
#75943 = AXIS2_PLACEMENT_3D('',#123315,#97260,#97261) ;
#75944 = AXIS2_PLACEMENT_3D('',#123316,#97262,#97263) ;
#75945 = AXIS2_PLACEMENT_3D('',#123317,#97264,#97265) ;
#75946 = AXIS2_PLACEMENT_3D('',#123318,#97266,#97267) ;
#75947 = AXIS2_PLACEMENT_3D('',#123319,#97268,#97269) ;
#75948 = AXIS2_PLACEMENT_3D('',#123320,#97270,#97271) ;
#75949 = AXIS2_PLACEMENT_3D('',#123321,#97272,#97273) ;
#75950 = AXIS2_PLACEMENT_3D('',#123322,#97274,#97275) ;
#75951 = AXIS2_PLACEMENT_3D('',#123323,#97276,#97277) ;
#75952 = AXIS2_PLACEMENT_3D('',#123324,#97278,#97279) ;
#75953 = AXIS2_PLACEMENT_3D('',#123325,#97280,#97281) ;
#75954 = AXIS2_PLACEMENT_3D('',#123326,#97282,#97283) ;
#75955 = AXIS2_PLACEMENT_3D('',#123327,#97284,#97285) ;
#75956 = AXIS2_PLACEMENT_3D('',#123328,#97286,#97287) ;
#75957 = AXIS2_PLACEMENT_3D('',#123329,#97288,#97289) ;
#75958 = AXIS2_PLACEMENT_3D('',#123330,#97290,#97291) ;
#75959 = AXIS2_PLACEMENT_3D('',#123331,#97292,#97293) ;
#75960 = AXIS2_PLACEMENT_3D('',#123332,#97294,#97295) ;
#75961 = AXIS2_PLACEMENT_3D('',#123333,#97296,#97297) ;
#75962 = AXIS2_PLACEMENT_3D('',#123334,#97298,#97299) ;
#75963 = AXIS2_PLACEMENT_3D('',#123335,#97300,#97301) ;
#75964 = AXIS2_PLACEMENT_3D('',#123336,#97302,#97303) ;
#75965 = AXIS2_PLACEMENT_3D('',#123337,#97304,#97305) ;
#75966 = AXIS2_PLACEMENT_3D('',#123338,#97306,#97307) ;
#75967 = AXIS2_PLACEMENT_3D('',#123339,#97308,#97309) ;
#75968 = AXIS2_PLACEMENT_3D('',#123340,#97310,#97311) ;
#75969 = AXIS2_PLACEMENT_3D('',#123341,#97312,#97313) ;
#75970 = AXIS2_PLACEMENT_3D('',#123342,#97314,#97315) ;
#75971 = AXIS2_PLACEMENT_3D('',#123343,#97316,#97317) ;
#75972 = AXIS2_PLACEMENT_3D('',#123344,#97318,#97319) ;
#75973 = AXIS2_PLACEMENT_3D('',#123345,#97320,#97321) ;
#75974 = AXIS2_PLACEMENT_3D('',#123346,#97322,#97323) ;
#75975 = AXIS2_PLACEMENT_3D('',#123347,#97324,#97325) ;
#75976 = AXIS2_PLACEMENT_3D('',#123348,#97326,#97327) ;
#75977 = AXIS2_PLACEMENT_3D('',#123349,#97328,#97329) ;
#75978 = AXIS2_PLACEMENT_3D('',#123350,#97330,#97331) ;
#75979 = AXIS2_PLACEMENT_3D('',#123351,#97332,#97333) ;
#75980 = AXIS2_PLACEMENT_3D('',#123352,#97334,#97335) ;
#75981 = AXIS2_PLACEMENT_3D('',#123353,#97336,#97337) ;
#75982 = AXIS2_PLACEMENT_3D('',#123354,#97338,#97339) ;
#75983 = AXIS2_PLACEMENT_3D('',#123355,#97340,#97341) ;
#75984 = AXIS2_PLACEMENT_3D('',#123356,#97342,#97343) ;
#75985 = AXIS2_PLACEMENT_3D('',#123357,#97344,#97345) ;
#75986 = AXIS2_PLACEMENT_3D('',#123358,#97346,#97347) ;
#75987 = AXIS2_PLACEMENT_3D('',#123359,#97348,#97349) ;
#75988 = AXIS2_PLACEMENT_3D('',#123360,#97350,#97351) ;
#75989 = AXIS2_PLACEMENT_3D('',#123361,#97352,#97353) ;
#75990 = AXIS2_PLACEMENT_3D('',#123362,#97354,#97355) ;
#75991 = AXIS2_PLACEMENT_3D('',#123363,#97356,#97357) ;
#75992 = AXIS2_PLACEMENT_3D('',#123364,#97358,#97359) ;
#75993 = AXIS2_PLACEMENT_3D('',#123365,#97360,#97361) ;
#75994 = AXIS2_PLACEMENT_3D('',#123366,#97362,#97363) ;
#75995 = AXIS2_PLACEMENT_3D('',#123367,#97364,#97365) ;
#75996 = AXIS2_PLACEMENT_3D('',#123368,#97366,#97367) ;
#75997 = AXIS2_PLACEMENT_3D('',#123369,#97368,#97369) ;
#75998 = AXIS2_PLACEMENT_3D('',#123370,#97370,#97371) ;
#75999 = AXIS2_PLACEMENT_3D('',#123371,#97372,#97373) ;
#76000 = AXIS2_PLACEMENT_3D('',#123372,#97374,#97375) ;
#76001 = AXIS2_PLACEMENT_3D('',#123373,#97376,#97377) ;
#76002 = AXIS2_PLACEMENT_3D('',#123374,#97378,#97379) ;
#76003 = AXIS2_PLACEMENT_3D('',#123375,#97380,#97381) ;
#76004 = AXIS2_PLACEMENT_3D('',#123376,#97382,#97383) ;
#76005 = AXIS2_PLACEMENT_3D('',#123377,#97384,#97385) ;
#76006 = AXIS2_PLACEMENT_3D('',#123378,#97386,#97387) ;
#76007 = AXIS2_PLACEMENT_3D('',#123379,#97388,#97389) ;
#76008 = AXIS2_PLACEMENT_3D('',#123380,#97390,#97391) ;
#76009 = AXIS2_PLACEMENT_3D('',#123381,#97392,#97393) ;
#76010 = AXIS2_PLACEMENT_3D('',#123382,#97394,#97395) ;
#76011 = AXIS2_PLACEMENT_3D('',#123383,#97396,#97397) ;
#76012 = AXIS2_PLACEMENT_3D('',#123384,#97398,#97399) ;
#76013 = AXIS2_PLACEMENT_3D('',#123385,#97400,#97401) ;
#76014 = AXIS2_PLACEMENT_3D('',#123386,#97402,#97403) ;
#76015 = AXIS2_PLACEMENT_3D('',#123387,#97404,#97405) ;
#76016 = AXIS2_PLACEMENT_3D('',#123388,#97406,#97407) ;
#76017 = AXIS2_PLACEMENT_3D('',#123389,#97408,#97409) ;
#76018 = AXIS2_PLACEMENT_3D('',#123390,#97410,#97411) ;
#76019 = AXIS2_PLACEMENT_3D('',#123391,#97412,#97413) ;
#76020 = AXIS2_PLACEMENT_3D('',#123392,#97414,#97415) ;
#76021 = AXIS2_PLACEMENT_3D('',#123393,#97416,#97417) ;
#76022 = AXIS2_PLACEMENT_3D('',#123394,#97418,#97419) ;
#76023 = AXIS2_PLACEMENT_3D('',#123395,#97420,#97421) ;
#76024 = AXIS2_PLACEMENT_3D('',#123396,#97422,#97423) ;
#76025 = AXIS2_PLACEMENT_3D('',#123397,#97424,#97425) ;
#76026 = AXIS2_PLACEMENT_3D('',#123398,#97426,#97427) ;
#76027 = AXIS2_PLACEMENT_3D('',#123399,#97428,#97429) ;
#76028 = AXIS2_PLACEMENT_3D('',#123400,#97430,#97431) ;
#76029 = AXIS2_PLACEMENT_3D('',#123401,#97432,#97433) ;
#76030 = AXIS2_PLACEMENT_3D('',#123402,#97434,#97435) ;
#76031 = AXIS2_PLACEMENT_3D('',#123403,#97436,#97437) ;
#76032 = AXIS2_PLACEMENT_3D('',#123404,#97438,#97439) ;
#76033 = AXIS2_PLACEMENT_3D('',#123405,#97440,#97441) ;
#76034 = AXIS2_PLACEMENT_3D('',#123406,#97442,#97443) ;
#76035 = AXIS2_PLACEMENT_3D('',#123407,#97444,#97445) ;
#76036 = AXIS2_PLACEMENT_3D('',#123408,#97446,#97447) ;
#76037 = AXIS2_PLACEMENT_3D('',#123409,#97448,#97449) ;
#76038 = AXIS2_PLACEMENT_3D('',#123410,#97450,#97451) ;
#76039 = AXIS2_PLACEMENT_3D('',#123411,#97452,#97453) ;
#76040 = AXIS2_PLACEMENT_3D('',#123412,#97454,#97455) ;
#76041 = AXIS2_PLACEMENT_3D('',#123413,#97456,#97457) ;
#76042 = AXIS2_PLACEMENT_3D('',#123414,#97458,#97459) ;
#76043 = AXIS2_PLACEMENT_3D('',#123415,#97460,#97461) ;
#76044 = AXIS2_PLACEMENT_3D('',#123416,#97462,#97463) ;
#76045 = AXIS2_PLACEMENT_3D('',#123417,#97464,#97465) ;
#76046 = AXIS2_PLACEMENT_3D('',#123418,#97466,#97467) ;
#76047 = AXIS2_PLACEMENT_3D('',#123419,#97468,#97469) ;
#76048 = AXIS2_PLACEMENT_3D('',#123420,#97470,#97471) ;
#76049 = AXIS2_PLACEMENT_3D('',#123421,#97472,#97473) ;
#76050 = AXIS2_PLACEMENT_3D('',#123422,#97474,#97475) ;
#76051 = AXIS2_PLACEMENT_3D('',#123423,#97476,#97477) ;
#76052 = AXIS2_PLACEMENT_3D('',#123424,#97478,#97479) ;
#76053 = AXIS2_PLACEMENT_3D('',#123425,#97480,#97481) ;
#76054 = AXIS2_PLACEMENT_3D('',#123426,#97482,#97483) ;
#76055 = AXIS2_PLACEMENT_3D('',#123427,#97484,#97485) ;
#76056 = AXIS2_PLACEMENT_3D('',#123428,#97486,#97487) ;
#76057 = AXIS2_PLACEMENT_3D('',#123429,#97488,#97489) ;
#76058 = AXIS2_PLACEMENT_3D('',#123430,#97490,#97491) ;
#76059 = AXIS2_PLACEMENT_3D('',#123431,#97492,#97493) ;
#76060 = AXIS2_PLACEMENT_3D('',#123432,#97494,#97495) ;
#76061 = AXIS2_PLACEMENT_3D('',#123433,#97496,#97497) ;
#76062 = AXIS2_PLACEMENT_3D('',#123434,#97498,#97499) ;
#76063 = AXIS2_PLACEMENT_3D('',#123435,#97500,#97501) ;
#76064 = AXIS2_PLACEMENT_3D('',#123436,#97502,#97503) ;
#76065 = AXIS2_PLACEMENT_3D('',#123437,#97504,#97505) ;
#76066 = AXIS2_PLACEMENT_3D('',#123438,#97506,#97507) ;
#76067 = AXIS2_PLACEMENT_3D('',#123439,#97508,#97509) ;
#76068 = AXIS2_PLACEMENT_3D('',#123440,#97510,#97511) ;
#76069 = AXIS2_PLACEMENT_3D('',#123441,#97512,#97513) ;
#76070 = AXIS2_PLACEMENT_3D('',#123442,#97514,#97515) ;
#76071 = AXIS2_PLACEMENT_3D('',#123443,#97516,#97517) ;
#76072 = AXIS2_PLACEMENT_3D('',#123444,#97518,#97519) ;
#76073 = AXIS2_PLACEMENT_3D('',#123445,#97520,#97521) ;
#76074 = AXIS2_PLACEMENT_3D('',#123446,#97522,#97523) ;
#76075 = AXIS2_PLACEMENT_3D('',#123447,#97524,#97525) ;
#76076 = AXIS2_PLACEMENT_3D('',#123448,#97526,#97527) ;
#76077 = AXIS2_PLACEMENT_3D('',#123449,#97528,#97529) ;
#76078 = AXIS2_PLACEMENT_3D('',#123450,#97530,#97531) ;
#76079 = AXIS2_PLACEMENT_3D('',#123451,#97532,#97533) ;
#76080 = AXIS2_PLACEMENT_3D('',#123452,#97534,#97535) ;
#76081 = AXIS2_PLACEMENT_3D('',#123453,#97536,#97537) ;
#76082 = AXIS2_PLACEMENT_3D('',#123454,#97538,#97539) ;
#76083 = AXIS2_PLACEMENT_3D('',#123455,#97540,#97541) ;
#76084 = AXIS2_PLACEMENT_3D('',#123456,#97542,#97543) ;
#76085 = AXIS2_PLACEMENT_3D('',#123457,#97544,#97545) ;
#76086 = AXIS2_PLACEMENT_3D('',#123458,#97546,#97547) ;
#76087 = AXIS2_PLACEMENT_3D('',#123459,#97548,#97549) ;
#76088 = AXIS2_PLACEMENT_3D('',#123460,#97550,#97551) ;
#76089 = AXIS2_PLACEMENT_3D('',#123461,#97552,#97553) ;
#76090 = AXIS2_PLACEMENT_3D('',#123462,#97554,#97555) ;
#76091 = AXIS2_PLACEMENT_3D('',#123463,#97556,#97557) ;
#76092 = AXIS2_PLACEMENT_3D('',#123464,#97558,#97559) ;
#76093 = AXIS2_PLACEMENT_3D('',#123465,#97560,#97561) ;
#76094 = AXIS2_PLACEMENT_3D('',#123466,#97562,#97563) ;
#76095 = AXIS2_PLACEMENT_3D('',#123467,#97564,#97565) ;
#76096 = AXIS2_PLACEMENT_3D('',#123468,#97566,#97567) ;
#76097 = AXIS2_PLACEMENT_3D('',#123469,#97568,#97569) ;
#76098 = AXIS2_PLACEMENT_3D('',#123470,#97570,#97571) ;
#76099 = AXIS2_PLACEMENT_3D('',#123471,#97572,#97573) ;
#76100 = AXIS2_PLACEMENT_3D('',#123472,#97574,#97575) ;
#76101 = AXIS2_PLACEMENT_3D('',#123473,#97576,#97577) ;
#76102 = AXIS2_PLACEMENT_3D('',#123474,#97578,#97579) ;
#76103 = AXIS2_PLACEMENT_3D('',#123475,#97580,#97581) ;
#76104 = AXIS2_PLACEMENT_3D('',#123476,#97582,#97583) ;
#76105 = AXIS2_PLACEMENT_3D('',#123477,#97584,#97585) ;
#76106 = AXIS2_PLACEMENT_3D('',#123478,#97586,#97587) ;
#76107 = AXIS2_PLACEMENT_3D('',#123479,#97588,#97589) ;
#76108 = AXIS2_PLACEMENT_3D('',#123480,#97590,#97591) ;
#76109 = AXIS2_PLACEMENT_3D('',#123481,#97592,#97593) ;
#76110 = AXIS2_PLACEMENT_3D('',#123482,#97594,#97595) ;
#76111 = AXIS2_PLACEMENT_3D('',#123483,#97596,#97597) ;
#76112 = AXIS2_PLACEMENT_3D('',#123484,#97598,#97599) ;
#76113 = AXIS2_PLACEMENT_3D('',#123485,#97600,#97601) ;
#76114 = AXIS2_PLACEMENT_3D('',#123486,#97602,#97603) ;
#76115 = AXIS2_PLACEMENT_3D('',#123487,#97604,#97605) ;
#76116 = AXIS2_PLACEMENT_3D('',#123488,#97606,#97607) ;
#76117 = AXIS2_PLACEMENT_3D('',#123489,#97608,#97609) ;
#76118 = AXIS2_PLACEMENT_3D('',#123490,#97610,#97611) ;
#76119 = AXIS2_PLACEMENT_3D('',#123491,#97612,#97613) ;
#76120 = AXIS2_PLACEMENT_3D('',#123492,#97614,#97615) ;
#76121 = AXIS2_PLACEMENT_3D('',#123493,#97616,#97617) ;
#76122 = AXIS2_PLACEMENT_3D('',#123494,#97618,#97619) ;
#76123 = AXIS2_PLACEMENT_3D('',#123495,#97620,#97621) ;
#76124 = AXIS2_PLACEMENT_3D('',#123496,#97622,#97623) ;
#76125 = AXIS2_PLACEMENT_3D('',#123497,#97624,#97625) ;
#76126 = AXIS2_PLACEMENT_3D('',#123498,#97626,#97627) ;
#76127 = AXIS2_PLACEMENT_3D('',#123499,#97628,#97629) ;
#76128 = AXIS2_PLACEMENT_3D('',#123500,#97630,#97631) ;
#76129 = AXIS2_PLACEMENT_3D('',#123501,#97632,#97633) ;
#76130 = AXIS2_PLACEMENT_3D('',#123502,#97634,#97635) ;
#76131 = AXIS2_PLACEMENT_3D('',#123503,#97636,#97637) ;
#76132 = AXIS2_PLACEMENT_3D('',#123504,#97638,#97639) ;
#76133 = AXIS2_PLACEMENT_3D('',#123505,#97640,#97641) ;
#76134 = AXIS2_PLACEMENT_3D('',#123506,#97642,#97643) ;
#76135 = AXIS2_PLACEMENT_3D('',#123507,#97644,#97645) ;
#76136 = AXIS2_PLACEMENT_3D('',#123508,#97646,#97647) ;
#76137 = AXIS2_PLACEMENT_3D('',#123509,#97648,#97649) ;
#76138 = AXIS2_PLACEMENT_3D('',#123510,#97650,#97651) ;
#76139 = AXIS2_PLACEMENT_3D('',#123511,#97652,#97653) ;
#76140 = AXIS2_PLACEMENT_3D('',#123512,#97654,#97655) ;
#76141 = AXIS2_PLACEMENT_3D('',#123513,#97656,#97657) ;
#76142 = AXIS2_PLACEMENT_3D('',#123514,#97658,#97659) ;
#76143 = AXIS2_PLACEMENT_3D('',#123515,#97660,#97661) ;
#76144 = AXIS2_PLACEMENT_3D('',#123516,#97662,#97663) ;
#76145 = AXIS2_PLACEMENT_3D('',#123517,#97664,#97665) ;
#76146 = AXIS2_PLACEMENT_3D('',#123518,#97666,#97667) ;
#76147 = AXIS2_PLACEMENT_3D('',#123519,#97668,#97669) ;
#76148 = AXIS2_PLACEMENT_3D('',#123520,#97670,#97671) ;
#76149 = AXIS2_PLACEMENT_3D('',#123521,#97672,#97673) ;
#76150 = AXIS2_PLACEMENT_3D('',#123522,#97674,#97675) ;
#76151 = AXIS2_PLACEMENT_3D('',#123523,#97676,#97677) ;
#76152 = AXIS2_PLACEMENT_3D('',#123524,#97678,#97679) ;
#76153 = AXIS2_PLACEMENT_3D('',#123525,#97680,#97681) ;
#76154 = AXIS2_PLACEMENT_3D('',#123526,#97682,#97683) ;
#76155 = AXIS2_PLACEMENT_3D('',#123527,#97684,#97685) ;
#76156 = AXIS2_PLACEMENT_3D('',#123528,#97686,#97687) ;
#76157 = AXIS2_PLACEMENT_3D('',#123529,#97688,#97689) ;
#76158 = AXIS2_PLACEMENT_3D('',#123530,#97690,#97691) ;
#76159 = AXIS2_PLACEMENT_3D('',#123531,#97692,#97693) ;
#76160 = AXIS2_PLACEMENT_3D('',#123532,#97694,#97695) ;
#76161 = AXIS2_PLACEMENT_3D('',#123533,#97696,#97697) ;
#76162 = AXIS2_PLACEMENT_3D('',#123534,#97698,#97699) ;
#76163 = AXIS2_PLACEMENT_3D('',#123535,#97700,#97701) ;
#76164 = AXIS2_PLACEMENT_3D('',#123536,#97702,#97703) ;
#76165 = AXIS2_PLACEMENT_3D('',#123537,#97704,#97705) ;
#76166 = AXIS2_PLACEMENT_3D('',#123538,#97706,#97707) ;
#76167 = AXIS2_PLACEMENT_3D('',#123539,#97708,#97709) ;
#76168 = AXIS2_PLACEMENT_3D('',#123540,#97710,#97711) ;
#76169 = AXIS2_PLACEMENT_3D('',#123541,#97712,#97713) ;
#76170 = AXIS2_PLACEMENT_3D('',#123542,#97714,#97715) ;
#76171 = AXIS2_PLACEMENT_3D('',#123543,#97716,#97717) ;
#76172 = AXIS2_PLACEMENT_3D('',#123544,#97718,#97719) ;
#76173 = AXIS2_PLACEMENT_3D('',#123545,#97720,#97721) ;
#76174 = AXIS2_PLACEMENT_3D('',#123546,#97722,#97723) ;
#76175 = AXIS2_PLACEMENT_3D('',#123547,#97724,#97725) ;
#76176 = AXIS2_PLACEMENT_3D('',#123548,#97726,#97727) ;
#76177 = AXIS2_PLACEMENT_3D('',#123549,#97728,#97729) ;
#76178 = AXIS2_PLACEMENT_3D('',#123550,#97730,#97731) ;
#76179 = AXIS2_PLACEMENT_3D('',#123551,#97732,#97733) ;
#76180 = AXIS2_PLACEMENT_3D('',#123552,#97734,#97735) ;
#76181 = AXIS2_PLACEMENT_3D('',#123553,#97736,#97737) ;
#76182 = AXIS2_PLACEMENT_3D('',#123554,#97738,#97739) ;
#76183 = AXIS2_PLACEMENT_3D('',#123555,#97740,#97741) ;
#76184 = AXIS2_PLACEMENT_3D('',#123556,#97742,#97743) ;
#76185 = AXIS2_PLACEMENT_3D('',#123557,#97744,#97745) ;
#76186 = AXIS2_PLACEMENT_3D('',#123558,#97746,#97747) ;
#76187 = AXIS2_PLACEMENT_3D('',#123559,#97748,#97749) ;
#76188 = AXIS2_PLACEMENT_3D('',#123560,#97750,#97751) ;
#76189 = AXIS2_PLACEMENT_3D('',#123561,#97752,#97753) ;
#76190 = AXIS2_PLACEMENT_3D('',#123562,#97754,#97755) ;
#76191 = AXIS2_PLACEMENT_3D('',#123563,#97756,#97757) ;
#76192 = AXIS2_PLACEMENT_3D('',#123564,#97758,#97759) ;
#76193 = AXIS2_PLACEMENT_3D('',#123565,#97760,#97761) ;
#76194 = AXIS2_PLACEMENT_3D('',#123566,#97762,#97763) ;
#76195 = AXIS2_PLACEMENT_3D('',#123567,#97764,#97765) ;
#76196 = AXIS2_PLACEMENT_3D('',#123568,#97766,#97767) ;
#76197 = AXIS2_PLACEMENT_3D('',#123569,#97768,#97769) ;
#76198 = AXIS2_PLACEMENT_3D('',#123570,#97770,#97771) ;
#76199 = AXIS2_PLACEMENT_3D('',#123571,#97772,#97773) ;
#76200 = AXIS2_PLACEMENT_3D('',#123572,#97774,#97775) ;
#76201 = AXIS2_PLACEMENT_3D('',#123573,#97776,#97777) ;
#76202 = AXIS2_PLACEMENT_3D('',#123574,#97778,#97779) ;
#76203 = AXIS2_PLACEMENT_3D('',#123575,#97780,#97781) ;
#76204 = AXIS2_PLACEMENT_3D('',#123576,#97782,#97783) ;
#76205 = AXIS2_PLACEMENT_3D('',#123577,#97784,#97785) ;
#76206 = AXIS2_PLACEMENT_3D('',#123578,#97786,#97787) ;
#76207 = AXIS2_PLACEMENT_3D('',#123579,#97788,#97789) ;
#76208 = AXIS2_PLACEMENT_3D('',#123580,#97790,#97791) ;
#76209 = AXIS2_PLACEMENT_3D('',#123581,#97792,#97793) ;
#76210 = AXIS2_PLACEMENT_3D('',#123582,#97794,#97795) ;
#76211 = AXIS2_PLACEMENT_3D('',#123583,#97796,#97797) ;
#76212 = AXIS2_PLACEMENT_3D('',#123584,#97798,#97799) ;
#76213 = AXIS2_PLACEMENT_3D('',#123585,#97800,#97801) ;
#76214 = AXIS2_PLACEMENT_3D('',#123586,#97802,#97803) ;
#76215 = AXIS2_PLACEMENT_3D('',#123587,#97804,#97805) ;
#76216 = AXIS2_PLACEMENT_3D('',#123588,#97806,#97807) ;
#76217 = AXIS2_PLACEMENT_3D('',#123589,#97808,#97809) ;
#76218 = AXIS2_PLACEMENT_3D('',#123590,#97810,#97811) ;
#76219 = AXIS2_PLACEMENT_3D('',#123591,#97812,#97813) ;
#76220 = AXIS2_PLACEMENT_3D('',#123592,#97814,#97815) ;
#76221 = AXIS2_PLACEMENT_3D('',#123593,#97816,#97817) ;
#76222 = AXIS2_PLACEMENT_3D('',#123594,#97818,#97819) ;
#76223 = AXIS2_PLACEMENT_3D('',#123595,#97820,#97821) ;
#76224 = AXIS2_PLACEMENT_3D('',#123596,#97822,#97823) ;
#76225 = AXIS2_PLACEMENT_3D('',#123597,#97824,#97825) ;
#76226 = AXIS2_PLACEMENT_3D('',#123598,#97826,#97827) ;
#76227 = AXIS2_PLACEMENT_3D('',#123599,#97828,#97829) ;
#76228 = AXIS2_PLACEMENT_3D('',#123600,#97830,#97831) ;
#76229 = AXIS2_PLACEMENT_3D('',#123601,#97832,#97833) ;
#76230 = AXIS2_PLACEMENT_3D('',#123602,#97834,#97835) ;
#76231 = AXIS2_PLACEMENT_3D('',#123603,#97836,#97837) ;
#76232 = AXIS2_PLACEMENT_3D('',#123604,#97838,#97839) ;
#76233 = AXIS2_PLACEMENT_3D('',#123605,#97840,#97841) ;
#76234 = AXIS2_PLACEMENT_3D('',#123606,#97842,#97843) ;
#76235 = AXIS2_PLACEMENT_3D('',#123607,#97844,#97845) ;
#76236 = AXIS2_PLACEMENT_3D('',#123608,#97846,#97847) ;
#76237 = AXIS2_PLACEMENT_3D('',#123609,#97848,#97849) ;
#76238 = AXIS2_PLACEMENT_3D('',#123610,#97850,#97851) ;
#76239 = AXIS2_PLACEMENT_3D('',#123611,#97852,#97853) ;
#76240 = AXIS2_PLACEMENT_3D('',#123612,#97854,#97855) ;
#76241 = AXIS2_PLACEMENT_3D('',#123613,#97856,#97857) ;
#76242 = AXIS2_PLACEMENT_3D('',#123614,#97858,#97859) ;
#76243 = AXIS2_PLACEMENT_3D('',#123615,#97860,#97861) ;
#76244 = AXIS2_PLACEMENT_3D('',#123616,#97862,#97863) ;
#76245 = AXIS2_PLACEMENT_3D('',#123617,#97864,#97865) ;
#76246 = AXIS2_PLACEMENT_3D('',#123618,#97866,#97867) ;
#76247 = AXIS2_PLACEMENT_3D('',#123619,#97868,#97869) ;
#76248 = AXIS2_PLACEMENT_3D('',#123620,#97870,#97871) ;
#76249 = AXIS2_PLACEMENT_3D('',#123621,#97872,#97873) ;
#76250 = AXIS2_PLACEMENT_3D('',#123622,#97874,#97875) ;
#76251 = AXIS2_PLACEMENT_3D('',#123623,#97876,#97877) ;
#76252 = AXIS2_PLACEMENT_3D('',#123624,#97878,#97879) ;
#76253 = AXIS2_PLACEMENT_3D('',#123625,#97880,#97881) ;
#76254 = AXIS2_PLACEMENT_3D('',#123626,#97882,#97883) ;
#76255 = AXIS2_PLACEMENT_3D('',#123627,#97884,#97885) ;
#76256 = AXIS2_PLACEMENT_3D('',#123628,#97886,#97887) ;
#76257 = AXIS2_PLACEMENT_3D('',#123629,#97888,#97889) ;
#76258 = AXIS2_PLACEMENT_3D('',#123630,#97890,#97891) ;
#76259 = AXIS2_PLACEMENT_3D('',#123631,#97892,#97893) ;
#76260 = AXIS2_PLACEMENT_3D('',#123632,#97894,#97895) ;
#76261 = AXIS2_PLACEMENT_3D('',#123633,#97896,#97897) ;
#76262 = AXIS2_PLACEMENT_3D('',#123634,#97898,#97899) ;
#76263 = AXIS2_PLACEMENT_3D('',#123635,#97900,#97901) ;
#76264 = AXIS2_PLACEMENT_3D('',#123636,#97902,#97903) ;
#76265 = AXIS2_PLACEMENT_3D('',#123637,#97904,#97905) ;
#76266 = AXIS2_PLACEMENT_3D('',#123638,#97906,#97907) ;
#76267 = AXIS2_PLACEMENT_3D('',#123639,#97908,#97909) ;
#76268 = AXIS2_PLACEMENT_3D('',#123640,#97910,#97911) ;
#76269 = AXIS2_PLACEMENT_3D('',#123641,#97912,#97913) ;
#76270 = AXIS2_PLACEMENT_3D('',#123642,#97914,#97915) ;
#76271 = AXIS2_PLACEMENT_3D('',#123643,#97916,#97917) ;
#76272 = AXIS2_PLACEMENT_3D('',#123644,#97918,#97919) ;
#76273 = AXIS2_PLACEMENT_3D('',#123645,#97920,#97921) ;
#76274 = AXIS2_PLACEMENT_3D('',#123646,#97922,#97923) ;
#76275 = AXIS2_PLACEMENT_3D('',#123647,#97924,#97925) ;
#76276 = AXIS2_PLACEMENT_3D('',#123648,#97926,#97927) ;
#76277 = AXIS2_PLACEMENT_3D('',#123649,#97928,#97929) ;
#76278 = AXIS2_PLACEMENT_3D('',#123650,#97930,#97931) ;
#76279 = AXIS2_PLACEMENT_3D('',#123651,#97932,#97933) ;
#76280 = AXIS2_PLACEMENT_3D('',#123652,#97934,#97935) ;
#76281 = AXIS2_PLACEMENT_3D('',#123653,#97936,#97937) ;
#76282 = AXIS2_PLACEMENT_3D('',#123654,#97938,#97939) ;
#76283 = AXIS2_PLACEMENT_3D('',#123655,#97940,#97941) ;
#76284 = AXIS2_PLACEMENT_3D('',#123656,#97942,#97943) ;
#76285 = AXIS2_PLACEMENT_3D('',#123657,#97944,#97945) ;
#76286 = AXIS2_PLACEMENT_3D('',#123658,#97946,#97947) ;
#76287 = AXIS2_PLACEMENT_3D('',#123659,#97948,#97949) ;
#76288 = AXIS2_PLACEMENT_3D('',#123660,#97950,#97951) ;
#76289 = AXIS2_PLACEMENT_3D('',#123661,#97952,#97953) ;
#76290 = AXIS2_PLACEMENT_3D('',#123662,#97954,#97955) ;
#76291 = AXIS2_PLACEMENT_3D('',#123663,#97956,#97957) ;
#76292 = AXIS2_PLACEMENT_3D('',#123664,#97958,#97959) ;
#76293 = AXIS2_PLACEMENT_3D('',#123665,#97960,#97961) ;
#76294 = AXIS2_PLACEMENT_3D('',#123666,#97962,#97963) ;
#76295 = AXIS2_PLACEMENT_3D('',#123667,#97964,#97965) ;
#76296 = AXIS2_PLACEMENT_3D('',#123668,#97966,#97967) ;
#76297 = AXIS2_PLACEMENT_3D('',#123669,#97968,#97969) ;
#76298 = AXIS2_PLACEMENT_3D('',#123670,#97970,#97971) ;
#76299 = AXIS2_PLACEMENT_3D('',#123671,#97972,#97973) ;
#76300 = AXIS2_PLACEMENT_3D('',#123672,#97974,#97975) ;
#76301 = AXIS2_PLACEMENT_3D('',#123673,#97976,#97977) ;
#76302 = AXIS2_PLACEMENT_3D('',#123674,#97978,#97979) ;
#76303 = AXIS2_PLACEMENT_3D('',#123675,#97980,#97981) ;
#76304 = AXIS2_PLACEMENT_3D('',#123676,#97982,#97983) ;
#76305 = AXIS2_PLACEMENT_3D('',#123677,#97984,#97985) ;
#76306 = AXIS2_PLACEMENT_3D('',#123678,#97986,#97987) ;
#76307 = AXIS2_PLACEMENT_3D('',#123679,#97988,#97989) ;
#76308 = AXIS2_PLACEMENT_3D('',#123680,#97990,#97991) ;
#76309 = AXIS2_PLACEMENT_3D('',#123681,#97992,#97993) ;
#76310 = AXIS2_PLACEMENT_3D('',#123682,#97994,#97995) ;
#76311 = AXIS2_PLACEMENT_3D('',#123683,#97996,#97997) ;
#76312 = AXIS2_PLACEMENT_3D('',#123684,#97998,#97999) ;
#76313 = AXIS2_PLACEMENT_3D('',#123685,#98000,#98001) ;
#76314 = AXIS2_PLACEMENT_3D('',#123686,#98002,#98003) ;
#76315 = AXIS2_PLACEMENT_3D('',#123687,#98004,#98005) ;
#76316 = AXIS2_PLACEMENT_3D('',#123688,#98006,#98007) ;
#76317 = AXIS2_PLACEMENT_3D('',#123689,#98008,#98009) ;
#76318 = AXIS2_PLACEMENT_3D('',#123690,#98010,#98011) ;
#76319 = AXIS2_PLACEMENT_3D('',#123691,#98012,#98013) ;
#76320 = AXIS2_PLACEMENT_3D('',#123692,#98014,#98015) ;
#76321 = AXIS2_PLACEMENT_3D('',#123693,#98016,#98017) ;
#76322 = AXIS2_PLACEMENT_3D('',#123694,#98018,#98019) ;
#76323 = AXIS2_PLACEMENT_3D('',#123695,#98020,#98021) ;
#76324 = AXIS2_PLACEMENT_3D('',#123696,#98022,#98023) ;
#76325 = AXIS2_PLACEMENT_3D('',#123697,#98024,#98025) ;
#76326 = AXIS2_PLACEMENT_3D('',#123698,#98026,#98027) ;
#76327 = AXIS2_PLACEMENT_3D('',#123699,#98028,#98029) ;
#76328 = AXIS2_PLACEMENT_3D('',#123700,#98030,#98031) ;
#76329 = AXIS2_PLACEMENT_3D('',#123701,#98032,#98033) ;
#76330 = AXIS2_PLACEMENT_3D('',#123702,#98034,#98035) ;
#76331 = AXIS2_PLACEMENT_3D('',#123703,#98036,#98037) ;
#76332 = AXIS2_PLACEMENT_3D('',#123704,#98038,#98039) ;
#76333 = AXIS2_PLACEMENT_3D('',#123705,#98040,#98041) ;
#76334 = AXIS2_PLACEMENT_3D('',#123706,#98042,#98043) ;
#76335 = AXIS2_PLACEMENT_3D('',#123707,#98044,#98045) ;
#76336 = AXIS2_PLACEMENT_3D('',#123708,#98046,#98047) ;
#76337 = AXIS2_PLACEMENT_3D('',#123709,#98048,#98049) ;
#76338 = AXIS2_PLACEMENT_3D('',#123710,#98050,#98051) ;
#76339 = AXIS2_PLACEMENT_3D('',#123711,#98052,#98053) ;
#76340 = AXIS2_PLACEMENT_3D('',#123712,#98054,#98055) ;
#76341 = AXIS2_PLACEMENT_3D('',#123713,#98056,#98057) ;
#76342 = AXIS2_PLACEMENT_3D('',#123714,#98058,#98059) ;
#76343 = AXIS2_PLACEMENT_3D('',#123715,#98060,#98061) ;
#76344 = AXIS2_PLACEMENT_3D('',#123716,#98062,#98063) ;
#76345 = AXIS2_PLACEMENT_3D('',#123717,#98064,#98065) ;
#76346 = AXIS2_PLACEMENT_3D('',#123718,#98066,#98067) ;
#76347 = AXIS2_PLACEMENT_3D('',#123719,#98068,#98069) ;
#76348 = AXIS2_PLACEMENT_3D('',#123720,#98070,#98071) ;
#76349 = AXIS2_PLACEMENT_3D('',#123721,#98072,#98073) ;
#76350 = AXIS2_PLACEMENT_3D('',#123722,#98074,#98075) ;
#76351 = AXIS2_PLACEMENT_3D('',#123723,#98076,#98077) ;
#76352 = AXIS2_PLACEMENT_3D('',#123724,#98078,#98079) ;
#76353 = AXIS2_PLACEMENT_3D('',#123725,#98080,#98081) ;
#76354 = AXIS2_PLACEMENT_3D('',#123726,#98082,#98083) ;
#76355 = AXIS2_PLACEMENT_3D('',#123727,#98084,#98085) ;
#76356 = AXIS2_PLACEMENT_3D('',#123728,#98086,#98087) ;
#76357 = AXIS2_PLACEMENT_3D('',#123729,#98088,#98089) ;
#76358 = AXIS2_PLACEMENT_3D('',#123730,#98090,#98091) ;
#76359 = AXIS2_PLACEMENT_3D('',#123731,#98092,#98093) ;
#76360 = AXIS2_PLACEMENT_3D('',#123732,#98094,#98095) ;
#76361 = AXIS2_PLACEMENT_3D('',#123733,#98096,#98097) ;
#76362 = AXIS2_PLACEMENT_3D('',#123734,#98098,#98099) ;
#76363 = AXIS2_PLACEMENT_3D('',#123735,#98100,#98101) ;
#76364 = AXIS2_PLACEMENT_3D('',#123736,#98102,#98103) ;
#76365 = AXIS2_PLACEMENT_3D('',#123737,#98104,#98105) ;
#76366 = AXIS2_PLACEMENT_3D('',#123738,#98106,#98107) ;
#76367 = AXIS2_PLACEMENT_3D('',#123739,#98108,#98109) ;
#76368 = AXIS2_PLACEMENT_3D('',#123740,#98110,#98111) ;
#76369 = AXIS2_PLACEMENT_3D('',#123741,#98112,#98113) ;
#76370 = AXIS2_PLACEMENT_3D('',#123742,#98114,#98115) ;
#76371 = AXIS2_PLACEMENT_3D('',#123743,#98116,#98117) ;
#76372 = AXIS2_PLACEMENT_3D('',#123744,#98118,#98119) ;
#76373 = AXIS2_PLACEMENT_3D('',#123745,#98120,#98121) ;
#76374 = AXIS2_PLACEMENT_3D('',#123746,#98122,#98123) ;
#76375 = AXIS2_PLACEMENT_3D('',#123747,#98124,#98125) ;
#76376 = AXIS2_PLACEMENT_3D('',#123748,#98126,#98127) ;
#76377 = AXIS2_PLACEMENT_3D('',#123749,#98128,#98129) ;
#76378 = AXIS2_PLACEMENT_3D('',#123750,#98130,#98131) ;
#76379 = AXIS2_PLACEMENT_3D('',#123751,#98132,#98133) ;
#76380 = AXIS2_PLACEMENT_3D('',#123752,#98134,#98135) ;
#76381 = AXIS2_PLACEMENT_3D('',#123753,#98136,#98137) ;
#76382 = AXIS2_PLACEMENT_3D('',#123754,#98138,#98139) ;
#76383 = AXIS2_PLACEMENT_3D('',#123755,#98140,#98141) ;
#76384 = AXIS2_PLACEMENT_3D('',#123756,#98142,#98143) ;
#76385 = AXIS2_PLACEMENT_3D('',#123757,#98144,#98145) ;
#76386 = AXIS2_PLACEMENT_3D('',#123758,#98146,#98147) ;
#76387 = AXIS2_PLACEMENT_3D('',#123759,#98148,#98149) ;
#76388 = AXIS2_PLACEMENT_3D('',#123760,#98150,#98151) ;
#76389 = AXIS2_PLACEMENT_3D('',#123761,#98152,#98153) ;
#76390 = AXIS2_PLACEMENT_3D('',#123762,#98154,#98155) ;
#76391 = AXIS2_PLACEMENT_3D('',#123763,#98156,#98157) ;
#76392 = AXIS2_PLACEMENT_3D('',#123764,#98158,#98159) ;
#76393 = AXIS2_PLACEMENT_3D('',#123765,#98160,#98161) ;
#76394 = AXIS2_PLACEMENT_3D('',#123766,#98162,#98163) ;
#76395 = AXIS2_PLACEMENT_3D('',#123767,#98164,#98165) ;
#76396 = AXIS2_PLACEMENT_3D('',#123768,#98166,#98167) ;
#76397 = AXIS2_PLACEMENT_3D('',#123769,#98168,#98169) ;
#76398 = AXIS2_PLACEMENT_3D('',#123770,#98170,#98171) ;
#76399 = AXIS2_PLACEMENT_3D('',#123771,#98172,#98173) ;
#76400 = AXIS2_PLACEMENT_3D('',#123772,#98174,#98175) ;
#76401 = AXIS2_PLACEMENT_3D('',#123773,#98176,#98177) ;
#76402 = AXIS2_PLACEMENT_3D('',#123774,#98178,#98179) ;
#76403 = AXIS2_PLACEMENT_3D('',#123775,#98180,#98181) ;
#76404 = AXIS2_PLACEMENT_3D('',#123776,#98182,#98183) ;
#76405 = AXIS2_PLACEMENT_3D('',#123777,#98184,#98185) ;
#76406 = AXIS2_PLACEMENT_3D('',#123778,#98186,#98187) ;
#76407 = AXIS2_PLACEMENT_3D('',#123779,#98188,#98189) ;
#76408 = AXIS2_PLACEMENT_3D('',#123780,#98190,#98191) ;
#76409 = AXIS2_PLACEMENT_3D('',#123781,#98192,#98193) ;
#76410 = AXIS2_PLACEMENT_3D('',#123782,#98194,#98195) ;
#76411 = AXIS2_PLACEMENT_3D('',#123783,#98196,#98197) ;
#76412 = AXIS2_PLACEMENT_3D('',#123784,#98198,#98199) ;
#76413 = AXIS2_PLACEMENT_3D('',#123785,#98200,#98201) ;
#76414 = AXIS2_PLACEMENT_3D('',#123786,#98202,#98203) ;
#76415 = AXIS2_PLACEMENT_3D('',#123787,#98204,#98205) ;
#76416 = AXIS2_PLACEMENT_3D('',#123788,#98206,#98207) ;
#76417 = AXIS2_PLACEMENT_3D('',#123789,#98208,#98209) ;
#76418 = AXIS2_PLACEMENT_3D('',#123790,#98210,#98211) ;
#76419 = AXIS2_PLACEMENT_3D('',#123791,#98212,#98213) ;
#76420 = AXIS2_PLACEMENT_3D('',#123792,#98214,#98215) ;
#76421 = AXIS2_PLACEMENT_3D('',#123793,#98216,#98217) ;
#76422 = AXIS2_PLACEMENT_3D('',#123794,#98218,#98219) ;
#76423 = AXIS2_PLACEMENT_3D('',#123795,#98220,#98221) ;
#76424 = AXIS2_PLACEMENT_3D('',#123796,#98222,#98223) ;
#76425 = AXIS2_PLACEMENT_3D('',#123797,#98224,#98225) ;
#76426 = AXIS2_PLACEMENT_3D('',#123798,#98226,#98227) ;
#76427 = AXIS2_PLACEMENT_3D('',#123799,#98228,#98229) ;
#76428 = AXIS2_PLACEMENT_3D('',#123800,#98230,#98231) ;
#76429 = AXIS2_PLACEMENT_3D('',#123801,#98232,#98233) ;
#76430 = AXIS2_PLACEMENT_3D('',#123802,#98234,#98235) ;
#76431 = AXIS2_PLACEMENT_3D('',#123803,#98236,#98237) ;
#76432 = AXIS2_PLACEMENT_3D('',#123804,#98238,#98239) ;
#76433 = AXIS2_PLACEMENT_3D('',#123805,#98240,#98241) ;
#76434 = AXIS2_PLACEMENT_3D('',#123806,#98242,#98243) ;
#76435 = AXIS2_PLACEMENT_3D('',#123807,#98244,#98245) ;
#76436 = AXIS2_PLACEMENT_3D('',#123808,#98246,#98247) ;
#76437 = AXIS2_PLACEMENT_3D('',#123809,#98248,#98249) ;
#76438 = AXIS2_PLACEMENT_3D('',#123810,#98250,#98251) ;
#76439 = AXIS2_PLACEMENT_3D('',#123811,#98252,#98253) ;
#76440 = AXIS2_PLACEMENT_3D('',#123812,#98254,#98255) ;
#76441 = AXIS2_PLACEMENT_3D('',#123813,#98256,#98257) ;
#76442 = AXIS2_PLACEMENT_3D('',#123814,#98258,#98259) ;
#76443 = AXIS2_PLACEMENT_3D('',#123815,#98260,#98261) ;
#76444 = AXIS2_PLACEMENT_3D('',#123816,#98262,#98263) ;
#76445 = AXIS2_PLACEMENT_3D('',#123817,#98264,#98265) ;
#76446 = AXIS2_PLACEMENT_3D('',#123818,#98266,#98267) ;
#76447 = AXIS2_PLACEMENT_3D('',#123819,#98268,#98269) ;
#76448 = AXIS2_PLACEMENT_3D('',#123820,#98270,#98271) ;
#76449 = AXIS2_PLACEMENT_3D('',#123821,#98272,#98273) ;
#76450 = AXIS2_PLACEMENT_3D('',#123822,#98274,#98275) ;
#76451 = AXIS2_PLACEMENT_3D('',#123823,#98276,#98277) ;
#76452 = AXIS2_PLACEMENT_3D('',#123824,#98278,#98279) ;
#76453 = AXIS2_PLACEMENT_3D('',#123825,#98280,#98281) ;
#76454 = AXIS2_PLACEMENT_3D('',#123826,#98282,#98283) ;
#76455 = AXIS2_PLACEMENT_3D('',#123827,#98284,#98285) ;
#76456 = AXIS2_PLACEMENT_3D('',#123828,#98286,#98287) ;
#76457 = AXIS2_PLACEMENT_3D('',#123829,#98288,#98289) ;
#76458 = AXIS2_PLACEMENT_3D('',#123830,#98290,#98291) ;
#76459 = AXIS2_PLACEMENT_3D('',#123831,#98292,#98293) ;
#76460 = AXIS2_PLACEMENT_3D('',#123832,#98294,#98295) ;
#76461 = AXIS2_PLACEMENT_3D('',#123833,#98296,#98297) ;
#76462 = AXIS2_PLACEMENT_3D('',#123834,#98298,#98299) ;
#76463 = AXIS2_PLACEMENT_3D('',#123835,#98300,#98301) ;
#76464 = AXIS2_PLACEMENT_3D('',#123836,#98302,#98303) ;
#76465 = AXIS2_PLACEMENT_3D('',#123837,#98304,#98305) ;
#76466 = AXIS2_PLACEMENT_3D('',#123838,#98306,#98307) ;
#76467 = AXIS2_PLACEMENT_3D('',#123839,#98308,#98309) ;
#76468 = AXIS2_PLACEMENT_3D('',#123840,#98310,#98311) ;
#76469 = AXIS2_PLACEMENT_3D('',#123841,#98312,#98313) ;
#76470 = AXIS2_PLACEMENT_3D('',#123842,#98314,#98315) ;
#76471 = AXIS2_PLACEMENT_3D('',#123843,#98316,#98317) ;
#76472 = AXIS2_PLACEMENT_3D('',#123844,#98318,#98319) ;
#76473 = AXIS2_PLACEMENT_3D('',#123845,#98320,#98321) ;
#76474 = AXIS2_PLACEMENT_3D('',#123846,#98322,#98323) ;
#76475 = AXIS2_PLACEMENT_3D('',#123847,#98324,#98325) ;
#76476 = AXIS2_PLACEMENT_3D('',#123848,#98326,#98327) ;
#76477 = AXIS2_PLACEMENT_3D('',#123849,#98328,#98329) ;
#76478 = AXIS2_PLACEMENT_3D('',#123850,#98330,#98331) ;
#76479 = AXIS2_PLACEMENT_3D('',#123851,#98332,#98333) ;
#76480 = AXIS2_PLACEMENT_3D('',#123852,#98334,#98335) ;
#76481 = AXIS2_PLACEMENT_3D('',#123853,#98336,#98337) ;
#76482 = AXIS2_PLACEMENT_3D('',#123854,#98338,#98339) ;
#76483 = AXIS2_PLACEMENT_3D('',#123855,#98340,#98341) ;
#76484 = AXIS2_PLACEMENT_3D('',#123856,#98342,#98343) ;
#76485 = AXIS2_PLACEMENT_3D('',#123857,#98344,#98345) ;
#76486 = AXIS2_PLACEMENT_3D('',#123858,#98346,#98347) ;
#76487 = AXIS2_PLACEMENT_3D('',#123859,#98348,#98349) ;
#76488 = AXIS2_PLACEMENT_3D('',#123860,#98350,#98351) ;
#76489 = AXIS2_PLACEMENT_3D('',#123861,#98352,#98353) ;
#76490 = AXIS2_PLACEMENT_3D('',#123862,#98354,#98355) ;
#76491 = AXIS2_PLACEMENT_3D('',#123863,#98356,#98357) ;
#76492 = AXIS2_PLACEMENT_3D('',#123864,#98358,#98359) ;
#76493 = AXIS2_PLACEMENT_3D('',#123865,#98360,#98361) ;
#76494 = AXIS2_PLACEMENT_3D('',#123866,#98362,#98363) ;
#76495 = AXIS2_PLACEMENT_3D('',#123867,#98364,#98365) ;
#76496 = AXIS2_PLACEMENT_3D('',#123868,#98366,#98367) ;
#76497 = AXIS2_PLACEMENT_3D('',#123869,#98368,#98369) ;
#76498 = AXIS2_PLACEMENT_3D('',#123870,#98370,#98371) ;
#76499 = AXIS2_PLACEMENT_3D('',#123871,#98372,#98373) ;
#76500 = AXIS2_PLACEMENT_3D('',#123872,#98374,#98375) ;
#76501 = AXIS2_PLACEMENT_3D('',#123873,#98376,#98377) ;
#76502 = AXIS2_PLACEMENT_3D('',#123874,#98378,#98379) ;
#76503 = AXIS2_PLACEMENT_3D('',#123875,#98380,#98381) ;
#76504 = AXIS2_PLACEMENT_3D('',#123876,#98382,#98383) ;
#76505 = AXIS2_PLACEMENT_3D('',#123877,#98384,#98385) ;
#76506 = AXIS2_PLACEMENT_3D('',#123878,#98386,#98387) ;
#76507 = AXIS2_PLACEMENT_3D('',#123879,#98388,#98389) ;
#76508 = AXIS2_PLACEMENT_3D('',#123880,#98390,#98391) ;
#76509 = AXIS2_PLACEMENT_3D('',#123881,#98392,#98393) ;
#76510 = AXIS2_PLACEMENT_3D('',#123882,#98394,#98395) ;
#76511 = AXIS2_PLACEMENT_3D('',#123883,#98396,#98397) ;
#76512 = AXIS2_PLACEMENT_3D('',#123884,#98398,#98399) ;
#76513 = AXIS2_PLACEMENT_3D('',#123885,#98400,#98401) ;
#76514 = AXIS2_PLACEMENT_3D('',#123886,#98402,#98403) ;
#76515 = AXIS2_PLACEMENT_3D('',#123887,#98404,#98405) ;
#76516 = AXIS2_PLACEMENT_3D('',#123888,#98406,#98407) ;
#76517 = AXIS2_PLACEMENT_3D('',#123889,#98408,#98409) ;
#76518 = AXIS2_PLACEMENT_3D('',#123890,#98410,#98411) ;
#76519 = AXIS2_PLACEMENT_3D('',#123891,#98412,#98413) ;
#76520 = AXIS2_PLACEMENT_3D('',#123892,#98414,#98415) ;
#76521 = AXIS2_PLACEMENT_3D('',#123893,#98416,#98417) ;
#76522 = AXIS2_PLACEMENT_3D('',#123894,#98418,#98419) ;
#76523 = AXIS2_PLACEMENT_3D('',#123895,#98420,#98421) ;
#76524 = AXIS2_PLACEMENT_3D('',#123896,#98422,#98423) ;
#76525 = AXIS2_PLACEMENT_3D('',#123897,#98424,#98425) ;
#76526 = AXIS2_PLACEMENT_3D('',#123898,#98426,#98427) ;
#76527 = AXIS2_PLACEMENT_3D('',#123899,#98428,#98429) ;
#76528 = AXIS2_PLACEMENT_3D('',#123900,#98430,#98431) ;
#76529 = AXIS2_PLACEMENT_3D('',#123901,#98432,#98433) ;
#76530 = AXIS2_PLACEMENT_3D('',#123902,#98434,#98435) ;
#76531 = AXIS2_PLACEMENT_3D('',#123903,#98436,#98437) ;
#76532 = AXIS2_PLACEMENT_3D('',#123904,#98438,#98439) ;
#76533 = AXIS2_PLACEMENT_3D('',#123905,#98440,#98441) ;
#76534 = AXIS2_PLACEMENT_3D('',#123906,#98442,#98443) ;
#76535 = AXIS2_PLACEMENT_3D('',#123907,#98444,#98445) ;
#76536 = AXIS2_PLACEMENT_3D('',#123908,#98446,#98447) ;
#76537 = AXIS2_PLACEMENT_3D('',#123909,#98448,#98449) ;
#76538 = AXIS2_PLACEMENT_3D('',#123910,#98450,#98451) ;
#76539 = AXIS2_PLACEMENT_3D('',#123911,#98452,#98453) ;
#76540 = AXIS2_PLACEMENT_3D('',#123912,#98454,#98455) ;
#76541 = AXIS2_PLACEMENT_3D('',#123913,#98456,#98457) ;
#76542 = AXIS2_PLACEMENT_3D('',#123914,#98458,#98459) ;
#76543 = AXIS2_PLACEMENT_3D('',#123915,#98460,#98461) ;
#76544 = AXIS2_PLACEMENT_3D('',#123916,#98462,#98463) ;
#76545 = AXIS2_PLACEMENT_3D('',#123917,#98464,#98465) ;
#76546 = AXIS2_PLACEMENT_3D('',#123918,#98466,#98467) ;
#76547 = AXIS2_PLACEMENT_3D('',#123919,#98468,#98469) ;
#76548 = AXIS2_PLACEMENT_3D('',#123920,#98470,#98471) ;
#76549 = AXIS2_PLACEMENT_3D('',#123921,#98472,#98473) ;
#76550 = AXIS2_PLACEMENT_3D('',#123922,#98474,#98475) ;
#76551 = AXIS2_PLACEMENT_3D('',#123923,#98476,#98477) ;
#76552 = AXIS2_PLACEMENT_3D('',#123924,#98478,#98479) ;
#76553 = AXIS2_PLACEMENT_3D('',#123925,#98480,#98481) ;
#76554 = AXIS2_PLACEMENT_3D('',#123926,#98482,#98483) ;
#76555 = AXIS2_PLACEMENT_3D('',#123927,#98484,#98485) ;
#76556 = AXIS2_PLACEMENT_3D('',#123928,#98486,#98487) ;
#76557 = AXIS2_PLACEMENT_3D('',#123929,#98488,#98489) ;
#76558 = AXIS2_PLACEMENT_3D('',#123930,#98490,#98491) ;
#76559 = AXIS2_PLACEMENT_3D('',#123931,#98492,#98493) ;
#76560 = AXIS2_PLACEMENT_3D('',#123932,#98494,#98495) ;
#76561 = AXIS2_PLACEMENT_3D('',#123933,#98496,#98497) ;
#76562 = AXIS2_PLACEMENT_3D('',#123934,#98498,#98499) ;
#76563 = AXIS2_PLACEMENT_3D('',#123935,#98500,#98501) ;
#76564 = AXIS2_PLACEMENT_3D('',#123936,#98502,#98503) ;
#76565 = AXIS2_PLACEMENT_3D('',#123937,#98504,#98505) ;
#76566 = AXIS2_PLACEMENT_3D('',#123938,#98506,#98507) ;
#76567 = AXIS2_PLACEMENT_3D('',#123939,#98508,#98509) ;
#76568 = AXIS2_PLACEMENT_3D('',#123940,#98510,#98511) ;
#76569 = AXIS2_PLACEMENT_3D('',#123941,#98512,#98513) ;
#76570 = AXIS2_PLACEMENT_3D('',#123942,#98514,#98515) ;
#76571 = AXIS2_PLACEMENT_3D('',#123943,#98516,#98517) ;
#76572 = AXIS2_PLACEMENT_3D('',#123944,#98518,#98519) ;
#76573 = AXIS2_PLACEMENT_3D('',#123945,#98520,#98521) ;
#76574 = AXIS2_PLACEMENT_3D('',#123946,#98522,#98523) ;
#76575 = AXIS2_PLACEMENT_3D('',#123947,#98524,#98525) ;
#76576 = AXIS2_PLACEMENT_3D('',#123948,#98526,#98527) ;
#76577 = AXIS2_PLACEMENT_3D('',#123949,#98528,#98529) ;
#76578 = AXIS2_PLACEMENT_3D('',#123950,#98530,#98531) ;
#76579 = AXIS2_PLACEMENT_3D('',#123951,#98532,#98533) ;
#76580 = AXIS2_PLACEMENT_3D('',#123952,#98534,#98535) ;
#76581 = AXIS2_PLACEMENT_3D('',#123953,#98536,#98537) ;
#76582 = AXIS2_PLACEMENT_3D('',#123954,#98538,#98539) ;
#76583 = AXIS2_PLACEMENT_3D('',#123955,#98540,#98541) ;
#76584 = AXIS2_PLACEMENT_3D('',#123956,#98542,#98543) ;
#76585 = AXIS2_PLACEMENT_3D('',#123957,#98544,#98545) ;
#76586 = AXIS2_PLACEMENT_3D('',#123958,#98546,#98547) ;
#76587 = AXIS2_PLACEMENT_3D('',#123959,#98548,#98549) ;
#76588 = AXIS2_PLACEMENT_3D('',#123960,#98550,#98551) ;
#76589 = AXIS2_PLACEMENT_3D('',#123961,#98552,#98553) ;
#76590 = AXIS2_PLACEMENT_3D('',#123962,#98554,#98555) ;
#76591 = AXIS2_PLACEMENT_3D('',#123963,#98556,#98557) ;
#76592 = AXIS2_PLACEMENT_3D('',#123964,#98558,#98559) ;
#76593 = AXIS2_PLACEMENT_3D('',#123965,#98560,#98561) ;
#76594 = AXIS2_PLACEMENT_3D('',#123966,#98562,#98563) ;
#76595 = AXIS2_PLACEMENT_3D('',#123967,#98564,#98565) ;
#76596 = AXIS2_PLACEMENT_3D('',#123968,#98566,#98567) ;
#76597 = AXIS2_PLACEMENT_3D('',#123969,#98568,#98569) ;
#76598 = AXIS2_PLACEMENT_3D('',#123970,#98570,#98571) ;
#76599 = AXIS2_PLACEMENT_3D('',#123971,#98572,#98573) ;
#76600 = AXIS2_PLACEMENT_3D('',#123972,#98574,#98575) ;
#76601 = AXIS2_PLACEMENT_3D('',#123973,#98576,#98577) ;
#76602 = AXIS2_PLACEMENT_3D('',#123974,#98578,#98579) ;
#76603 = AXIS2_PLACEMENT_3D('',#123975,#98580,#98581) ;
#76604 = AXIS2_PLACEMENT_3D('',#123976,#98582,#98583) ;
#76605 = AXIS2_PLACEMENT_3D('',#123977,#98584,#98585) ;
#76606 = AXIS2_PLACEMENT_3D('',#123978,#98586,#98587) ;
#76607 = AXIS2_PLACEMENT_3D('',#123979,#98588,#98589) ;
#76608 = AXIS2_PLACEMENT_3D('',#123980,#98590,#98591) ;
#76609 = AXIS2_PLACEMENT_3D('',#123981,#98592,#98593) ;
#76610 = AXIS2_PLACEMENT_3D('',#123982,#98594,#98595) ;
#76611 = AXIS2_PLACEMENT_3D('',#123983,#98596,#98597) ;
#76612 = AXIS2_PLACEMENT_3D('',#123984,#98598,#98599) ;
#76613 = AXIS2_PLACEMENT_3D('',#123985,#98600,#98601) ;
#76614 = AXIS2_PLACEMENT_3D('',#123986,#98602,#98603) ;
#76615 = AXIS2_PLACEMENT_3D('',#123987,#98604,#98605) ;
#76616 = AXIS2_PLACEMENT_3D('',#123988,#98606,#98607) ;
#76617 = AXIS2_PLACEMENT_3D('',#123989,#98608,#98609) ;
#76618 = AXIS2_PLACEMENT_3D('',#123990,#98610,#98611) ;
#76619 = AXIS2_PLACEMENT_3D('',#123991,#98612,#98613) ;
#76620 = AXIS2_PLACEMENT_3D('',#123992,#98614,#98615) ;
#76621 = AXIS2_PLACEMENT_3D('',#123993,#98616,#98617) ;
#76622 = AXIS2_PLACEMENT_3D('',#123994,#98618,#98619) ;
#76623 = AXIS2_PLACEMENT_3D('',#123995,#98620,#98621) ;
#76624 = AXIS2_PLACEMENT_3D('',#123996,#98622,#98623) ;
#76625 = AXIS2_PLACEMENT_3D('',#123997,#98624,#98625) ;
#76626 = AXIS2_PLACEMENT_3D('',#123998,#98626,#98627) ;
#76627 = AXIS2_PLACEMENT_3D('',#123999,#98628,#98629) ;
#76628 = AXIS2_PLACEMENT_3D('',#124000,#98630,#98631) ;
#76629 = AXIS2_PLACEMENT_3D('',#124001,#98632,#98633) ;
#76630 = AXIS2_PLACEMENT_3D('',#124002,#98634,#98635) ;
#76631 = AXIS2_PLACEMENT_3D('',#124003,#98636,#98637) ;
#76632 = AXIS2_PLACEMENT_3D('',#124004,#98638,#98639) ;
#76633 = AXIS2_PLACEMENT_3D('',#124005,#98640,#98641) ;
#76634 = AXIS2_PLACEMENT_3D('',#124006,#98642,#98643) ;
#76635 = AXIS2_PLACEMENT_3D('',#124007,#98644,#98645) ;
#76636 = AXIS2_PLACEMENT_3D('',#124008,#98646,#98647) ;
#76637 = AXIS2_PLACEMENT_3D('',#124009,#98648,#98649) ;
#76638 = AXIS2_PLACEMENT_3D('',#124010,#98650,#98651) ;
#76639 = AXIS2_PLACEMENT_3D('',#124011,#98652,#98653) ;
#76640 = AXIS2_PLACEMENT_3D('',#124012,#98654,#98655) ;
#76641 = AXIS2_PLACEMENT_3D('',#124013,#98656,#98657) ;
#76642 = AXIS2_PLACEMENT_3D('',#124014,#98658,#98659) ;
#76643 = AXIS2_PLACEMENT_3D('',#124015,#98660,#98661) ;
#76644 = AXIS2_PLACEMENT_3D('',#124016,#98662,#98663) ;
#76645 = AXIS2_PLACEMENT_3D('',#124017,#98664,#98665) ;
#76646 = AXIS2_PLACEMENT_3D('',#124018,#98666,#98667) ;
#76647 = AXIS2_PLACEMENT_3D('',#124019,#98668,#98669) ;
#76648 = AXIS2_PLACEMENT_3D('',#124020,#98670,#98671) ;
#76649 = AXIS2_PLACEMENT_3D('',#124021,#98672,#98673) ;
#76650 = AXIS2_PLACEMENT_3D('',#124022,#98674,#98675) ;
#76651 = AXIS2_PLACEMENT_3D('',#124023,#98676,#98677) ;
#76652 = AXIS2_PLACEMENT_3D('',#124024,#98678,#98679) ;
#76653 = AXIS2_PLACEMENT_3D('',#124025,#98680,#98681) ;
#76654 = AXIS2_PLACEMENT_3D('',#124026,#98682,#98683) ;
#76655 = AXIS2_PLACEMENT_3D('',#124027,#98684,#98685) ;
#76656 = AXIS2_PLACEMENT_3D('',#124028,#98686,#98687) ;
#76657 = AXIS2_PLACEMENT_3D('',#124029,#98688,#98689) ;
#76658 = AXIS2_PLACEMENT_3D('',#124030,#98690,#98691) ;
#76659 = AXIS2_PLACEMENT_3D('',#124031,#98692,#98693) ;
#76660 = AXIS2_PLACEMENT_3D('',#124032,#98694,#98695) ;
#76661 = AXIS2_PLACEMENT_3D('',#124033,#98696,#98697) ;
#76662 = AXIS2_PLACEMENT_3D('',#124034,#98698,#98699) ;
#76663 = AXIS2_PLACEMENT_3D('',#124035,#98700,#98701) ;
#76664 = AXIS2_PLACEMENT_3D('',#124036,#98702,#98703) ;
#76665 = AXIS2_PLACEMENT_3D('',#124037,#98704,#98705) ;
#76666 = AXIS2_PLACEMENT_3D('',#124038,#98706,#98707) ;
#76667 = AXIS2_PLACEMENT_3D('',#124039,#98708,#98709) ;
#76668 = AXIS2_PLACEMENT_3D('',#124040,#98710,#98711) ;
#76669 = AXIS2_PLACEMENT_3D('',#124041,#98712,#98713) ;
#76670 = AXIS2_PLACEMENT_3D('',#124042,#98714,#98715) ;
#76671 = AXIS2_PLACEMENT_3D('',#124089,#98718,#98719) ;
#76672 = AXIS2_PLACEMENT_3D('',#124169,#98721,#98722) ;
#76673 = AXIS2_PLACEMENT_3D('',#124245,#98724,#98725) ;
#76674 = AXIS2_PLACEMENT_3D('',#124321,#98727,#98728) ;
#76675 = AXIS2_PLACEMENT_3D('',#124397,#98730,#98731) ;
#76676 = AXIS2_PLACEMENT_3D('',#124473,#98733,#98734) ;
#76677 = AXIS2_PLACEMENT_3D('',#124549,#98736,#98737) ;
#76678 = AXIS2_PLACEMENT_3D('',#124625,#98739,#98740) ;
#76679 = AXIS2_PLACEMENT_3D('',#124705,#98742,#98743) ;
#76680 = AXIS2_PLACEMENT_3D('',#124781,#98745,#98746) ;
#76681 = AXIS2_PLACEMENT_3D('',#124799,#98748,#98749) ;
#76682 = AXIS2_PLACEMENT_3D('',#124808,#98750,#98751) ;
#76683 = AXIS2_PLACEMENT_3D('',#124884,#98753,#98754) ;
#76684 = AXIS2_PLACEMENT_3D('',#124960,#98756,#98757) ;
#76685 = AXIS2_PLACEMENT_3D('',#125036,#98759,#98760) ;
#76686 = AXIS2_PLACEMENT_3D('',#125112,#98762,#98763) ;
#76687 = AXIS2_PLACEMENT_3D('',#125188,#98765,#98766) ;
#76688 = AXIS2_PLACEMENT_3D('',#125266,#98768,#98769) ;
#76689 = AXIS2_PLACEMENT_3D('',#125344,#98771,#98772) ;
#76690 = AXIS2_PLACEMENT_3D('',#125346,#98773,#98774) ;
#76691 = AXIS2_PLACEMENT_3D('',#125379,#98776,#98777) ;
#76692 = AXIS2_PLACEMENT_3D('',#125383,#98779,#98780) ;
#76693 = AXIS2_PLACEMENT_3D('',#125453,#98782,#98783) ;
#76694 = AXIS2_PLACEMENT_3D('',#125526,#98784,#98785) ;
#76695 = AXIS2_PLACEMENT_3D('',#125551,#98786,#98787) ;
#76696 = AXIS2_PLACEMENT_3D('',#125566,#98788,#98789) ;
#76697 = AXIS2_PLACEMENT_3D('',#125568,#98790,#98791) ;
#76698 = AXIS2_PLACEMENT_3D('',#125571,#98793,#98794) ;
#76699 = AXIS2_PLACEMENT_3D('',#125572,#98795,#98796) ;
#76700 = AXIS2_PLACEMENT_3D('',#125574,#98797,#98798) ;
#76701 = AXIS2_PLACEMENT_3D('',#125576,#98800,#98801) ;
#76702 = AXIS2_PLACEMENT_3D('',#125579,#98803,#98804) ;
#76703 = AXIS2_PLACEMENT_3D('',#125581,#98805,#98806) ;
#76704 = AXIS2_PLACEMENT_3D('',#125582,#98807,#98808) ;
#76705 = AXIS2_PLACEMENT_3D('',#125583,#98809,#98810) ;
#76706 = AXIS2_PLACEMENT_3D('',#125617,#98812,#98813) ;
#76707 = AXIS2_PLACEMENT_3D('',#125638,#98814,#98815) ;
#76708 = AXIS2_PLACEMENT_3D('',#125643,#98817,#98818) ;
#76709 = AXIS2_PLACEMENT_3D('',#125646,#98820,#98821) ;
#76710 = AXIS2_PLACEMENT_3D('',#125647,#98822,#98823) ;
#76711 = AXIS2_PLACEMENT_3D('',#125652,#98825,#98826) ;
#76712 = AXIS2_PLACEMENT_3D('',#125655,#98828,#98829) ;
#76713 = AXIS2_PLACEMENT_3D('',#125656,#98830,#98831) ;
#76714 = AXIS2_PLACEMENT_3D('',#125661,#98833,#98834) ;
#76715 = AXIS2_PLACEMENT_3D('',#125664,#98836,#98837) ;
#76716 = AXIS2_PLACEMENT_3D('',#125665,#98838,#98839) ;
#76717 = AXIS2_PLACEMENT_3D('',#125670,#98841,#98842) ;
#76718 = AXIS2_PLACEMENT_3D('',#125673,#98844,#98845) ;
#76719 = AXIS2_PLACEMENT_3D('',#125674,#98846,#98847) ;
#76720 = AXIS2_PLACEMENT_3D('',#125679,#98849,#98850) ;
#76721 = AXIS2_PLACEMENT_3D('',#125682,#98852,#98853) ;
#76722 = AXIS2_PLACEMENT_3D('',#125683,#98854,#98855) ;
#76723 = AXIS2_PLACEMENT_3D('',#125688,#98857,#98858) ;
#76724 = AXIS2_PLACEMENT_3D('',#125691,#98860,#98861) ;
#76725 = AXIS2_PLACEMENT_3D('',#125692,#98862,#98863) ;
#76726 = AXIS2_PLACEMENT_3D('',#125698,#98864,#98865) ;
#76727 = AXIS2_PLACEMENT_3D('',#125702,#98866,#98867) ;
#76728 = AXIS2_PLACEMENT_3D('',#125704,#98868,#98869) ;
#76729 = AXIS2_PLACEMENT_3D('',#125711,#98870,#98871) ;
#76730 = AXIS2_PLACEMENT_3D('',#125713,#98872,#98873) ;
#76731 = AXIS2_PLACEMENT_3D('',#125720,#98874,#98875) ;
#76732 = AXIS2_PLACEMENT_3D('',#125722,#98876,#98877) ;
#76733 = AXIS2_PLACEMENT_3D('',#125729,#98878,#98879) ;
#76734 = AXIS2_PLACEMENT_3D('',#125731,#98880,#98881) ;
#76735 = AXIS2_PLACEMENT_3D('',#125738,#98882,#98883) ;
#76736 = AXIS2_PLACEMENT_3D('',#125739,#98884,#98885) ;
#76737 = AXIS2_PLACEMENT_3D('',#125746,#98886,#98887) ;
#76738 = AXIS2_PLACEMENT_3D('',#125752,#98888,#98889) ;
#76739 = AXIS2_PLACEMENT_3D('',#125756,#98890,#98891) ;
#76740 = AXIS2_PLACEMENT_3D('',#125758,#98892,#98893) ;
#76741 = AXIS2_PLACEMENT_3D('',#125765,#98894,#98895) ;
#76742 = AXIS2_PLACEMENT_3D('',#125770,#98896,#98897) ;
#76743 = AXIS2_PLACEMENT_3D('',#125774,#98898,#98899) ;
#76744 = AXIS2_PLACEMENT_3D('',#125779,#98900,#98901) ;
#76745 = AXIS2_PLACEMENT_3D('',#125783,#98902,#98903) ;
#76746 = AXIS2_PLACEMENT_3D('',#125788,#98904,#98905) ;
#76747 = AXIS2_PLACEMENT_3D('',#125792,#98906,#98907) ;
#76748 = AXIS2_PLACEMENT_3D('',#125796,#98908,#98909) ;
#76749 = AXIS2_PLACEMENT_3D('',#125800,#98910,#98911) ;
#76750 = AXIS2_PLACEMENT_3D('',#125801,#98912,#98913) ;
#76751 = AXIS2_PLACEMENT_3D('',#125802,#98914,#98915) ;
#76752 = AXIS2_PLACEMENT_3D('',#125803,#98916,#98917) ;
#76753 = AXIS2_PLACEMENT_3D('',#125804,#98918,#98919) ;
#76754 = AXIS2_PLACEMENT_3D('',#125805,#98920,#98921) ;
#76755 = AXIS2_PLACEMENT_3D('',#125806,#98922,#98923) ;
#76756 = AXIS2_PLACEMENT_3D('',#125807,#98924,#98925) ;
#76757 = AXIS2_PLACEMENT_3D('',#125808,#98926,#98927) ;
#76758 = AXIS2_PLACEMENT_3D('',#126351,#98929,#98930) ;
#76759 = AXIS2_PLACEMENT_3D('',#126362,#98931,#98932) ;
#76760 = AXIS2_PLACEMENT_3D('',#126364,#98934,#98935) ;
#76761 = AXIS2_PLACEMENT_3D('',#126366,#98937,#98938) ;
#76762 = AXIS2_PLACEMENT_3D('',#126367,#98939,#98940) ;
#76763 = AXIS2_PLACEMENT_3D('',#126368,#98941,#98942) ;
#76764 = AXIS2_PLACEMENT_3D('',#126373,#98944,#98945) ;
#76765 = AXIS2_PLACEMENT_3D('',#126375,#98946,#98947) ;
#76766 = AXIS2_PLACEMENT_3D('',#126377,#98948,#98949) ;
#76767 = AXIS2_PLACEMENT_3D('',#126379,#98950,#98951) ;
#76768 = AXIS2_PLACEMENT_3D('',#126381,#98952,#98953) ;
#76769 = AXIS2_PLACEMENT_3D('',#126383,#98954,#98955) ;
#76770 = AXIS2_PLACEMENT_3D('',#126385,#98956,#98957) ;
#76771 = AXIS2_PLACEMENT_3D('',#126387,#98958,#98959) ;
#76772 = AXIS2_PLACEMENT_3D('',#126389,#98960,#98961) ;
#76773 = AXIS2_PLACEMENT_3D('',#126391,#98962,#98963) ;
#76774 = AXIS2_PLACEMENT_3D('',#126393,#98964,#98965) ;
#76775 = AXIS2_PLACEMENT_3D('',#126395,#98966,#98967) ;
#76776 = AXIS2_PLACEMENT_3D('',#126397,#98968,#98969) ;
#76777 = AXIS2_PLACEMENT_3D('',#126399,#98970,#98971) ;
#76778 = AXIS2_PLACEMENT_3D('',#126401,#98972,#98973) ;
#76779 = AXIS2_PLACEMENT_3D('',#126403,#98974,#98975) ;
#76780 = AXIS2_PLACEMENT_3D('',#126404,#98976,#98977) ;
#76781 = AXIS2_PLACEMENT_3D('',#126405,#98978,#98979) ;
#76782 = AXIS2_PLACEMENT_3D('',#126406,#98980,#98981) ;
#76783 = AXIS2_PLACEMENT_3D('',#126407,#98982,#98983) ;
#76784 = AXIS2_PLACEMENT_3D('',#126409,#98984,#98985) ;
#76785 = AXIS2_PLACEMENT_3D('',#126411,#98986,#98987) ;
#76786 = AXIS2_PLACEMENT_3D('',#126412,#98988,#98989) ;
#76787 = AXIS2_PLACEMENT_3D('',#126413,#98990,#98991) ;
#76788 = AXIS2_PLACEMENT_3D('',#126415,#98992,#98993) ;
#76789 = AXIS2_PLACEMENT_3D('',#126417,#98994,#98995) ;
#76790 = AXIS2_PLACEMENT_3D('',#126418,#98996,#98997) ;
#76791 = AXIS2_PLACEMENT_3D('',#126419,#98998,#98999) ;
#76792 = AXIS2_PLACEMENT_3D('',#126422,#99001,#99002) ;
#76793 = AXIS2_PLACEMENT_3D('',#126423,#99003,#99004) ;
#76794 = AXIS2_PLACEMENT_3D('',#126426,#99006,#99007) ;
#76795 = AXIS2_PLACEMENT_3D('',#126427,#99008,#99009) ;
#76796 = AXIS2_PLACEMENT_3D('',#126430,#99010,#99011) ;
#76797 = AXIS2_PLACEMENT_3D('',#126432,#99012,#99013) ;
#76798 = AXIS2_PLACEMENT_3D('',#126434,#99014,#99015) ;
#76799 = AXIS2_PLACEMENT_3D('',#126436,#99016,#99017) ;
#76800 = AXIS2_PLACEMENT_3D('',#126438,#99018,#99019) ;
#76801 = AXIS2_PLACEMENT_3D('',#126440,#99020,#99021) ;
#76802 = AXIS2_PLACEMENT_3D('',#126442,#99022,#99023) ;
#76803 = AXIS2_PLACEMENT_3D('',#126444,#99024,#99025) ;
#76804 = AXIS2_PLACEMENT_3D('',#126446,#99026,#99027) ;
#76805 = AXIS2_PLACEMENT_3D('',#126448,#99028,#99029) ;
#76806 = AXIS2_PLACEMENT_3D('',#126450,#99030,#99031) ;
#76807 = AXIS2_PLACEMENT_3D('',#126452,#99032,#99033) ;
#76808 = AXIS2_PLACEMENT_3D('',#126454,#99034,#99035) ;
#76809 = AXIS2_PLACEMENT_3D('',#126456,#99036,#99037) ;
#76810 = AXIS2_PLACEMENT_3D('',#126458,#99038,#99039) ;
#76811 = AXIS2_PLACEMENT_3D('',#126459,#99040,#99041) ;
#76812 = AXIS2_PLACEMENT_3D('',#126460,#99042,#99043) ;
#76813 = AXIS2_PLACEMENT_3D('',#126467,#99046,#99047) ;
#76814 = AXIS2_PLACEMENT_3D('',#126474,#99050,#99051) ;
#76815 = AXIS2_PLACEMENT_3D('',#126481,#99054,#99055) ;
#76816 = AXIS2_PLACEMENT_3D('',#126488,#99058,#99059) ;
#76817 = AXIS2_PLACEMENT_3D('',#126489,#99060,#99061) ;
#76818 = AXIS2_PLACEMENT_3D('',#126492,#99064,#99065) ;
#76819 = AXIS2_PLACEMENT_3D('',#126493,#99066,#99067) ;
#76820 = AXIS2_PLACEMENT_3D('',#126496,#99070,#99071) ;
#76821 = AXIS2_PLACEMENT_3D('',#126500,#99074,#99075) ;
#76822 = AXIS2_PLACEMENT_3D('',#126501,#99076,#99077) ;
#76823 = AXIS2_PLACEMENT_3D('',#126502,#99078,#99079) ;
#76824 = AXIS2_PLACEMENT_3D('',#126506,#99082,#99083) ;
#76825 = AXIS2_PLACEMENT_3D('',#126510,#99086,#99087) ;
#76826 = AXIS2_PLACEMENT_3D('',#126511,#99088,#99089) ;
#76827 = AXIS2_PLACEMENT_3D('',#126512,#99090,#99091) ;
#76828 = AXIS2_PLACEMENT_3D('',#126519,#99094,#99095) ;
#76829 = AXIS2_PLACEMENT_3D('',#126524,#99097,#99098) ;
#76830 = AXIS2_PLACEMENT_3D('',#126526,#99100,#99101) ;
#76831 = AXIS2_PLACEMENT_3D('',#126527,#99102,#99103) ;
#76832 = AXIS2_PLACEMENT_3D('',#126530,#99106,#99107) ;
#76833 = AXIS2_PLACEMENT_3D('',#126534,#99108,#99109) ;
#76834 = AXIS2_PLACEMENT_3D('',#126538,#99110,#99111) ;
#76835 = AXIS2_PLACEMENT_3D('',#126539,#99112,#99113) ;
#76836 = AXIS2_PLACEMENT_3D('',#126540,#99114,#99115) ;
#76837 = AXIS2_PLACEMENT_3D('',#126541,#99116,#99117) ;
#76838 = AXIS2_PLACEMENT_3D('',#126542,#99118,#99119) ;
#76839 = AXIS2_PLACEMENT_3D('',#126543,#99120,#99121) ;
#76840 = AXIS2_PLACEMENT_3D('',#126544,#99122,#99123) ;
#76841 = AXIS2_PLACEMENT_3D('',#126545,#99124,#99125) ;
#76842 = AXIS2_PLACEMENT_3D('',#126546,#99126,#99127) ;
#76843 = AXIS2_PLACEMENT_3D('',#126547,#99128,#99129) ;
#76844 = AXIS2_PLACEMENT_3D('',#126548,#99130,#99131) ;
#76845 = AXIS2_PLACEMENT_3D('',#126549,#99132,#99133) ;
#76846 = AXIS2_PLACEMENT_3D('',#126550,#99134,#99135) ;
#76847 = AXIS2_PLACEMENT_3D('',#126551,#99136,#99137) ;
#76848 = AXIS2_PLACEMENT_3D('',#126552,#99138,#99139) ;
#76849 = AXIS2_PLACEMENT_3D('',#126553,#99140,#99141) ;
#76850 = AXIS2_PLACEMENT_3D('',#126554,#99142,#99143) ;
#76851 = AXIS2_PLACEMENT_3D('',#126555,#99144,#99145) ;
#76852 = DIRECTION('axis',(0.,0.,1.)) ;
#76853 = DIRECTION('refdir',(1.,0.,0.)) ;
#76854 = DIRECTION('axis',(0.,0.,1.)) ;
#76855 = DIRECTION('refdir',(1.,0.,0.)) ;
#76856 = DIRECTION('center_axis',(-1.,-3.65204942310907E-15,-6.7286639138916E-31)) ;
#76857 = DIRECTION('ref_axis',(3.73969860926368E-15,-1.,0.)) ;
#76858 = DIRECTION('center_axis',(-1.,-3.65204942310907E-15,-6.7286639138916E-31)) ;
#76859 = DIRECTION('ref_axis',(3.65204942310907E-15,-1.,-4.60751496844179E-46)) ;
#76860 = DIRECTION('center_axis',(-1.,-3.65204942310907E-15,-6.7286639138916E-31)) ;
#76861 = DIRECTION('ref_axis',(3.65204942310907E-15,-1.,-4.60751496844179E-46)) ;
#76862 = DIRECTION('center_axis',(6.7286639138916E-31,3.1453968851229E-45,
-1.)) ;
#76863 = DIRECTION('ref_axis',(-4.67462326157961E-15,1.,0.)) ;
#76864 = DIRECTION('center_axis',(1.,3.65204942310907E-15,6.7286639138916E-31)) ;
#76865 = DIRECTION('ref_axis',(3.65204942310907E-15,-1.,-2.10629255700197E-46)) ;
#76866 = DIRECTION('center_axis',(-1.,-3.65204942310907E-15,-6.7286639138916E-31)) ;
#76867 = DIRECTION('ref_axis',(3.73969860926368E-15,-1.,0.)) ;
#76868 = DIRECTION('center_axis',(-1.,-3.65204942310907E-15,-6.7286639138916E-31)) ;
#76869 = DIRECTION('ref_axis',(3.65204942310907E-15,-1.,-2.10629255700197E-46)) ;
#76870 = DIRECTION('center_axis',(6.7286639138916E-31,3.1453968851229E-45,
-1.)) ;
#76871 = DIRECTION('ref_axis',(-4.67462326157961E-15,1.,0.)) ;
#76872 = DIRECTION('center_axis',(1.,3.65204942310907E-15,6.7286639138916E-31)) ;
#76873 = DIRECTION('ref_axis',(3.65204942310907E-15,-1.,-4.60751496844179E-46)) ;
#76874 = DIRECTION('center_axis',(1.,3.65204942310907E-15,6.7286639138916E-31)) ;
#76875 = DIRECTION('ref_axis',(3.65204942310907E-15,-1.,-4.60751496844179E-46)) ;
#76876 = DIRECTION('center_axis',(0.,-1.,-1.83697019872103E-16)) ;
#76877 = DIRECTION('ref_axis',(0.,1.8503717077086E-16,-1.)) ;
#76878 = DIRECTION('center_axis',(0.,-1.,-1.83697019872103E-16)) ;
#76879 = DIRECTION('ref_axis',(0.,1.83697019872103E-16,-1.)) ;
#76880 = DIRECTION('center_axis',(0.,-1.,-1.83697019872103E-16)) ;
#76881 = DIRECTION('ref_axis',(0.,1.83697019872103E-16,-1.)) ;
#76882 = DIRECTION('center_axis',(-1.,0.,0.)) ;
#76883 = DIRECTION('ref_axis',(0.,-1.92747052886313E-16,1.)) ;
#76884 = DIRECTION('center_axis',(0.,1.,1.83697019872103E-16)) ;
#76885 = DIRECTION('ref_axis',(0.,1.83697019872103E-16,-1.)) ;
#76886 = DIRECTION('center_axis',(0.,1.,1.83697019872103E-16)) ;
#76887 = DIRECTION('ref_axis',(0.,1.83697019872103E-16,-1.)) ;
#76888 = DIRECTION('center_axis',(-4.15069017696469E-34,1.,1.83697019872103E-16)) ;
#76889 = DIRECTION('ref_axis',(0.,-1.8503717077086E-16,1.)) ;
#76890 = DIRECTION('center_axis',(-4.15069017696469E-34,1.,1.83697019872103E-16)) ;
#76891 = DIRECTION('ref_axis',(-5.57464581117898E-51,-1.83697019872103E-16,
1.)) ;
#76892 = DIRECTION('center_axis',(-1.,-4.15069017696469E-34,-8.00033299054114E-50)) ;
#76893 = DIRECTION('ref_axis',(0.,1.92747052886313E-16,-1.)) ;
#76894 = DIRECTION('center_axis',(4.15069017696469E-34,-1.,-1.83697019872103E-16)) ;
#76895 = DIRECTION('ref_axis',(-1.3756804551505E-50,-1.83697019872103E-16,
1.)) ;
#76896 = DIRECTION('center_axis',(0.,-1.,-1.83697019872103E-16)) ;
#76897 = DIRECTION('ref_axis',(0.,1.8503717077086E-16,-1.)) ;
#76898 = DIRECTION('center_axis',(0.,-1.,-1.83697019872103E-16)) ;
#76899 = DIRECTION('ref_axis',(0.,1.83697019872103E-16,-1.)) ;
#76900 = DIRECTION('center_axis',(0.,-1.,-1.83697019872103E-16)) ;
#76901 = DIRECTION('ref_axis',(0.,1.83697019872103E-16,-1.)) ;
#76902 = DIRECTION('center_axis',(-1.,0.,0.)) ;
#76903 = DIRECTION('ref_axis',(0.,-1.92747052886313E-16,1.)) ;
#76904 = DIRECTION('center_axis',(0.,1.,1.83697019872103E-16)) ;
#76905 = DIRECTION('ref_axis',(0.,1.83697019872103E-16,-1.)) ;
#76906 = DIRECTION('center_axis',(0.,1.,1.83697019872103E-16)) ;
#76907 = DIRECTION('ref_axis',(0.,1.83697019872103E-16,-1.)) ;
#76908 = DIRECTION('center_axis',(-4.15069017696469E-34,1.,1.83697019872103E-16)) ;
#76909 = DIRECTION('ref_axis',(0.,-1.8503717077086E-16,1.)) ;
#76910 = DIRECTION('center_axis',(-4.15069017696469E-34,1.,1.83697019872103E-16)) ;
#76911 = DIRECTION('ref_axis',(-5.57464581117898E-51,-1.83697019872103E-16,
1.)) ;
#76912 = DIRECTION('center_axis',(-1.,-4.15069017696469E-34,-8.00033299054114E-50)) ;
#76913 = DIRECTION('ref_axis',(0.,1.92747052886313E-16,-1.)) ;
#76914 = DIRECTION('center_axis',(4.15069017696469E-34,-1.,-1.83697019872103E-16)) ;
#76915 = DIRECTION('ref_axis',(-1.3756804551505E-50,-1.83697019872103E-16,
1.)) ;
#76916 = DIRECTION('center_axis',(0.,1.,1.83697019872103E-16)) ;
#76917 = DIRECTION('ref_axis',(0.,-1.83697019872103E-16,1.)) ;
#76918 = DIRECTION('',(-8.65956056235478E-17,0.70710678118656,-0.707106781186535)) ;
#76919 = DIRECTION('center_axis',(0.,1.,1.83697019872103E-16)) ;
#76920 = DIRECTION('ref_axis',(0.,-1.83697019872103E-16,1.)) ;
#76921 = DIRECTION('center_axis',(0.,1.,1.83697019872103E-16)) ;
#76922 = DIRECTION('ref_axis',(0.,-1.83697019872103E-16,1.)) ;
#76923 = DIRECTION('',(0.,1.,1.83697019872103E-16)) ;
#76924 = DIRECTION('center_axis',(0.,1.,1.83697019872103E-16)) ;
#76925 = DIRECTION('ref_axis',(0.,-1.83697019872103E-16,1.)) ;
#76926 = DIRECTION('',(-8.65956056235478E-17,0.70710678118656,-0.707106781186535)) ;
#76927 = DIRECTION('center_axis',(0.,1.,1.83697019872103E-16)) ;
#76928 = DIRECTION('ref_axis',(0.,-1.83697019872103E-16,1.)) ;
#76929 = DIRECTION('center_axis',(0.,1.,1.83697019872103E-16)) ;
#76930 = DIRECTION('ref_axis',(0.,-1.83697019872103E-16,1.)) ;
#76931 = DIRECTION('',(0.,1.,1.83697019872103E-16)) ;
#76932 = DIRECTION('center_axis',(1.,3.65204942310907E-15,6.7286639138916E-31)) ;
#76933 = DIRECTION('ref_axis',(-3.65204942310907E-15,1.,-8.63909056582784E-47)) ;
#76934 = DIRECTION('',(1.,3.65204942310907E-15,6.7286639138916E-31)) ;
#76935 = DIRECTION('center_axis',(-1.,-3.65204942310907E-15,-6.7286639138916E-31)) ;
#76936 = DIRECTION('ref_axis',(3.65204942310907E-15,-1.,-1.30970071666515E-61)) ;
#76937 = DIRECTION('',(0.,-2.47817639425257E-16,1.)) ;
#76938 = DIRECTION('',(3.65204942310907E-15,-1.,1.22867065825113E-46)) ;
#76939 = DIRECTION('',(1.03517906367563E-32,1.81408990951823E-16,-1.)) ;
#76940 = DIRECTION('',(-3.65204942310907E-15,1.,7.70988211545247E-16)) ;
#76941 = DIRECTION('',(0.,2.47817639425258E-16,-1.)) ;
#76942 = DIRECTION('',(1.03517906367563E-32,1.81408990951823E-16,-1.)) ;
#76943 = DIRECTION('center_axis',(1.,3.65204942310907E-15,6.7286639138916E-31)) ;
#76944 = DIRECTION('ref_axis',(3.65204942310907E-15,-1.,2.45734131650226E-45)) ;
#76945 = DIRECTION('',(3.65204942310907E-15,-1.,-3.44027784310316E-46)) ;
#76946 = DIRECTION('center_axis',(1.,3.65204942310907E-15,6.7286639138916E-31)) ;
#76947 = DIRECTION('ref_axis',(3.65204942310907E-15,-1.,2.45734131650226E-45)) ;
#76948 = DIRECTION('',(-6.7286639138916E-31,-2.45734131650226E-45,1.)) ;
#76949 = DIRECTION('center_axis',(1.,3.65204942310907E-15,6.7286639138916E-31)) ;
#76950 = DIRECTION('ref_axis',(3.65204942310907E-15,-1.,2.45734131650226E-45)) ;
#76951 = DIRECTION('',(-3.65204942310907E-15,1.,3.44027784310316E-46)) ;
#76952 = DIRECTION('center_axis',(1.,3.65204942310907E-15,6.7286639138916E-31)) ;
#76953 = DIRECTION('ref_axis',(3.65204942310907E-15,-1.,2.45734131650226E-45)) ;
#76954 = DIRECTION('',(6.7286639138916E-31,2.45734131650226E-45,-1.)) ;
#76955 = DIRECTION('center_axis',(-1.,-3.65204942310907E-15,-6.7286639138916E-31)) ;
#76956 = DIRECTION('ref_axis',(3.65204942310907E-15,-1.,-1.30970071666515E-61)) ;
#76957 = DIRECTION('',(-1.03517906367563E-32,-1.81408990951823E-16,1.)) ;
#76958 = DIRECTION('',(-3.65204942310907E-15,1.,-1.22867065825113E-46)) ;
#76959 = DIRECTION('',(0.,-2.47817639425257E-16,1.)) ;
#76960 = DIRECTION('',(0.,-1.81408990951823E-16,1.)) ;
#76961 = DIRECTION('',(0.,2.47817639425258E-16,-1.)) ;
#76962 = DIRECTION('',(3.65204942310907E-15,-1.,-7.70988211545247E-16)) ;
#76963 = DIRECTION('center_axis',(-1.,-3.65204942310907E-15,-6.7286639138916E-31)) ;
#76964 = DIRECTION('ref_axis',(3.65204942310907E-15,-1.,2.45734131650226E-45)) ;
#76965 = DIRECTION('',(-3.65204942310907E-15,1.,3.44027784310316E-46)) ;
#76966 = DIRECTION('center_axis',(-1.,-3.65204942310907E-15,-6.7286639138916E-31)) ;
#76967 = DIRECTION('ref_axis',(3.65204942310907E-15,-1.,2.45734131650226E-45)) ;
#76968 = DIRECTION('',(-6.7286639138916E-31,-2.45734131650226E-45,1.)) ;
#76969 = DIRECTION('center_axis',(-1.,-3.65204942310907E-15,-6.7286639138916E-31)) ;
#76970 = DIRECTION('ref_axis',(3.65204942310907E-15,-1.,2.45734131650226E-45)) ;
#76971 = DIRECTION('',(3.65204942310907E-15,-1.,-3.44027784310316E-46)) ;
#76972 = DIRECTION('center_axis',(-1.,-3.65204942310907E-15,-6.7286639138916E-31)) ;
#76973 = DIRECTION('ref_axis',(3.65204942310907E-15,-1.,2.45734131650226E-45)) ;
#76974 = DIRECTION('',(6.7286639138916E-31,2.45734131650226E-45,-1.)) ;
#76975 = DIRECTION('center_axis',(4.72515227845561E-31,7.02672800395669E-16,
-1.)) ;
#76976 = DIRECTION('ref_axis',(2.70755867152026E-31,1.,7.02672800395669E-16)) ;
#76977 = DIRECTION('center_axis',(4.72515227845561E-31,7.02672800395669E-16,
-1.)) ;
#76978 = DIRECTION('ref_axis',(-3.32023598379838E-46,1.,7.02672800395669E-16)) ;
#76979 = DIRECTION('',(-7.43707788821665E-32,1.,7.02672800395669E-16)) ;
#76980 = DIRECTION('',(-1.,-7.43707788821671E-32,8.21355058201474E-31)) ;
#76981 = DIRECTION('',(-1.,-7.43707788821671E-32,8.21355058201474E-31)) ;
#76982 = DIRECTION('',(3.49501116159781E-15,-1.,-7.02672800395669E-16)) ;
#76983 = DIRECTION('',(-1.,4.18667286880966E-31,-4.7251522784556E-31)) ;
#76984 = DIRECTION('',(-7.43707788821665E-32,1.,7.02672800395669E-16)) ;
#76985 = DIRECTION('center_axis',(4.72515227845561E-31,7.02672800395669E-16,
-1.)) ;
#76986 = DIRECTION('ref_axis',(-3.32023598379838E-46,1.,7.02672800395669E-16)) ;
#76987 = DIRECTION('',(-1.,4.18667286880966E-31,-4.7251522784556E-31)) ;
#76988 = DIRECTION('',(-2.16840434497101E-16,1.,7.02672800395669E-16)) ;
#76989 = DIRECTION('',(1.,-4.18667286880966E-31,4.7251522784556E-31)) ;
#76990 = DIRECTION('center_axis',(4.72515227845561E-31,7.02672800395669E-16,
-1.)) ;
#76991 = DIRECTION('ref_axis',(-3.32023598379838E-46,1.,7.02672800395669E-16)) ;
#76992 = DIRECTION('',(1.97633094273713E-47,-1.,-7.02672800395669E-16)) ;
#76993 = DIRECTION('center_axis',(4.72515227845561E-31,7.02672800395669E-16,
-1.)) ;
#76994 = DIRECTION('ref_axis',(-3.32023598379838E-46,1.,7.02672800395669E-16)) ;
#76995 = DIRECTION('',(1.,-3.32023598379838E-46,4.72515227845561E-31)) ;
#76996 = DIRECTION('center_axis',(4.72515227845561E-31,7.02672800395669E-16,
-1.)) ;
#76997 = DIRECTION('ref_axis',(-3.32023598379838E-46,1.,7.02672800395669E-16)) ;
#76998 = DIRECTION('',(-1.97633094273713E-47,1.,7.02672800395669E-16)) ;
#76999 = DIRECTION('center_axis',(4.72515227845561E-31,7.02672800395669E-16,
-1.)) ;
#77000 = DIRECTION('ref_axis',(-3.32023598379838E-46,1.,7.02672800395669E-16)) ;
#77001 = DIRECTION('',(-1.,3.32023598379838E-46,-4.72515227845561E-31)) ;
#77002 = DIRECTION('center_axis',(4.72515227845561E-31,7.02672800395669E-16,
-1.)) ;
#77003 = DIRECTION('ref_axis',(-3.32023598379838E-46,1.,7.02672800395669E-16)) ;
#77004 = DIRECTION('',(-8.67361737988404E-17,-1.,-7.02672800395669E-16)) ;
#77005 = DIRECTION('center_axis',(4.72515227845561E-31,7.02672800395669E-16,
-1.)) ;
#77006 = DIRECTION('ref_axis',(-3.32023598379838E-46,1.,7.02672800395669E-16)) ;
#77007 = DIRECTION('',(1.,-3.32023598379838E-46,4.72515227845561E-31)) ;
#77008 = DIRECTION('center_axis',(4.72515227845561E-31,7.02672800395669E-16,
-1.)) ;
#77009 = DIRECTION('ref_axis',(-3.32023598379838E-46,1.,7.02672800395669E-16)) ;
#77010 = DIRECTION('',(1.73472347597681E-16,1.,7.02672800395669E-16)) ;
#77011 = DIRECTION('center_axis',(4.72515227845561E-31,7.02672800395669E-16,
-1.)) ;
#77012 = DIRECTION('ref_axis',(-3.32023598379838E-46,1.,7.02672800395669E-16)) ;
#77013 = DIRECTION('',(-1.,3.32023598379838E-46,-4.72515227845561E-31)) ;
#77014 = DIRECTION('center_axis',(4.72515227845561E-31,7.02672800395669E-16,
-1.)) ;
#77015 = DIRECTION('ref_axis',(-3.32023598379838E-46,1.,7.02672800395669E-16)) ;
#77016 = DIRECTION('',(3.46944695195361E-16,1.,7.02672800395669E-16)) ;
#77017 = DIRECTION('center_axis',(4.72515227845561E-31,7.02672800395669E-16,
-1.)) ;
#77018 = DIRECTION('ref_axis',(-3.32023598379838E-46,1.,7.02672800395669E-16)) ;
#77019 = DIRECTION('',(-1.,3.32023598379838E-46,-4.72515227845561E-31)) ;
#77020 = DIRECTION('center_axis',(4.72515227845561E-31,7.02672800395669E-16,
-1.)) ;
#77021 = DIRECTION('ref_axis',(-3.32023598379838E-46,1.,7.02672800395669E-16)) ;
#77022 = DIRECTION('',(-1.73472347597681E-16,-1.,-7.02672800395669E-16)) ;
#77023 = DIRECTION('center_axis',(4.72515227845561E-31,7.02672800395669E-16,
-1.)) ;
#77024 = DIRECTION('ref_axis',(-3.32023598379838E-46,1.,7.02672800395669E-16)) ;
#77025 = DIRECTION('',(1.,-3.32023598379838E-46,4.72515227845561E-31)) ;
#77026 = DIRECTION('center_axis',(4.72515227845561E-31,7.02672800395669E-16,
-1.)) ;
#77027 = DIRECTION('ref_axis',(-3.32023598379838E-46,1.,7.02672800395669E-16)) ;
#77028 = DIRECTION('',(6.93889390390723E-16,1.,7.02672800395669E-16)) ;
#77029 = DIRECTION('center_axis',(4.72515227845561E-31,7.02672800395669E-16,
-1.)) ;
#77030 = DIRECTION('ref_axis',(-3.32023598379838E-46,1.,7.02672800395669E-16)) ;
#77031 = DIRECTION('',(-1.,3.32023598379838E-46,-4.72515227845561E-31)) ;
#77032 = DIRECTION('center_axis',(4.72515227845561E-31,7.02672800395669E-16,
-1.)) ;
#77033 = DIRECTION('ref_axis',(-3.32023598379838E-46,1.,7.02672800395669E-16)) ;
#77034 = DIRECTION('',(4.15029497974802E-48,-1.,-7.02672800395669E-16)) ;
#77035 = DIRECTION('center_axis',(4.72515227845561E-31,7.02672800395669E-16,
-1.)) ;
#77036 = DIRECTION('ref_axis',(-3.32023598379838E-46,1.,7.02672800395669E-16)) ;
#77037 = DIRECTION('',(1.,-3.32023598379838E-46,4.72515227845561E-31)) ;
#77038 = DIRECTION('center_axis',(4.72515227845561E-31,7.02672800395669E-16,
-1.)) ;
#77039 = DIRECTION('ref_axis',(2.70755867152026E-31,1.,7.02672800395669E-16)) ;
#77040 = DIRECTION('',(-1.,-7.43707788821671E-32,8.21355058201474E-31)) ;
#77041 = DIRECTION('',(7.43707788821665E-32,-1.,-7.02672800395669E-16)) ;
#77042 = DIRECTION('center_axis',(-4.72515227845561E-31,-7.02672800395669E-16,
1.)) ;
#77043 = DIRECTION('ref_axis',(-3.32023598379838E-46,1.,7.02672800395669E-16)) ;
#77044 = DIRECTION('',(-1.,4.18667286880966E-31,-4.7251522784556E-31)) ;
#77045 = DIRECTION('',(2.16840434497101E-16,-1.,-7.02672800395669E-16)) ;
#77046 = DIRECTION('',(1.,-4.18667286880966E-31,4.7251522784556E-31)) ;
#77047 = DIRECTION('center_axis',(-4.72515227845561E-31,-7.02672800395669E-16,
1.)) ;
#77048 = DIRECTION('ref_axis',(-3.32023598379838E-46,1.,7.02672800395669E-16)) ;
#77049 = DIRECTION('',(7.43707788821665E-32,-1.,-7.02672800395669E-16)) ;
#77050 = DIRECTION('',(1.,-4.18667286880966E-31,4.7251522784556E-31)) ;
#77051 = DIRECTION('',(-3.49501116159781E-15,1.,7.02672800395669E-16)) ;
#77052 = DIRECTION('',(-1.,-7.43707788821671E-32,8.21355058201474E-31)) ;
#77053 = DIRECTION('center_axis',(-4.72515227845561E-31,-7.02672800395669E-16,
1.)) ;
#77054 = DIRECTION('ref_axis',(-3.32023598379838E-46,1.,7.02672800395669E-16)) ;
#77055 = DIRECTION('',(-1.97633094273713E-47,1.,7.02672800395669E-16)) ;
#77056 = DIRECTION('center_axis',(-4.72515227845561E-31,-7.02672800395669E-16,
1.)) ;
#77057 = DIRECTION('ref_axis',(-3.32023598379838E-46,1.,7.02672800395669E-16)) ;
#77058 = DIRECTION('',(1.,-3.32023598379838E-46,4.72515227845561E-31)) ;
#77059 = DIRECTION('center_axis',(-4.72515227845561E-31,-7.02672800395669E-16,
1.)) ;
#77060 = DIRECTION('ref_axis',(-3.32023598379838E-46,1.,7.02672800395669E-16)) ;
#77061 = DIRECTION('',(1.97633094273713E-47,-1.,-7.02672800395669E-16)) ;
#77062 = DIRECTION('center_axis',(-4.72515227845561E-31,-7.02672800395669E-16,
1.)) ;
#77063 = DIRECTION('ref_axis',(-3.32023598379838E-46,1.,7.02672800395669E-16)) ;
#77064 = DIRECTION('',(-1.,3.32023598379838E-46,-4.72515227845561E-31)) ;
#77065 = DIRECTION('center_axis',(-4.72515227845561E-31,-7.02672800395669E-16,
1.)) ;
#77066 = DIRECTION('ref_axis',(-3.32023598379838E-46,1.,7.02672800395669E-16)) ;
#77067 = DIRECTION('',(8.67361737988404E-17,1.,7.02672800395669E-16)) ;
#77068 = DIRECTION('center_axis',(-4.72515227845561E-31,-7.02672800395669E-16,
1.)) ;
#77069 = DIRECTION('ref_axis',(-3.32023598379838E-46,1.,7.02672800395669E-16)) ;
#77070 = DIRECTION('',(1.,-3.32023598379838E-46,4.72515227845561E-31)) ;
#77071 = DIRECTION('center_axis',(-4.72515227845561E-31,-7.02672800395669E-16,
1.)) ;
#77072 = DIRECTION('ref_axis',(-3.32023598379838E-46,1.,7.02672800395669E-16)) ;
#77073 = DIRECTION('',(-1.73472347597681E-16,-1.,-7.02672800395669E-16)) ;
#77074 = DIRECTION('center_axis',(-4.72515227845561E-31,-7.02672800395669E-16,
1.)) ;
#77075 = DIRECTION('ref_axis',(-3.32023598379838E-46,1.,7.02672800395669E-16)) ;
#77076 = DIRECTION('',(-1.,3.32023598379838E-46,-4.72515227845561E-31)) ;
#77077 = DIRECTION('center_axis',(-4.72515227845561E-31,-7.02672800395669E-16,
1.)) ;
#77078 = DIRECTION('ref_axis',(-3.32023598379838E-46,1.,7.02672800395669E-16)) ;
#77079 = DIRECTION('',(-3.46944695195361E-16,-1.,-7.02672800395669E-16)) ;
#77080 = DIRECTION('center_axis',(-4.72515227845561E-31,-7.02672800395669E-16,
1.)) ;
#77081 = DIRECTION('ref_axis',(-3.32023598379838E-46,1.,7.02672800395669E-16)) ;
#77082 = DIRECTION('',(-1.,3.32023598379838E-46,-4.72515227845561E-31)) ;
#77083 = DIRECTION('center_axis',(-4.72515227845561E-31,-7.02672800395669E-16,
1.)) ;
#77084 = DIRECTION('ref_axis',(-3.32023598379838E-46,1.,7.02672800395669E-16)) ;
#77085 = DIRECTION('',(1.73472347597681E-16,1.,7.02672800395669E-16)) ;
#77086 = DIRECTION('center_axis',(-4.72515227845561E-31,-7.02672800395669E-16,
1.)) ;
#77087 = DIRECTION('ref_axis',(-3.32023598379838E-46,1.,7.02672800395669E-16)) ;
#77088 = DIRECTION('',(1.,-3.32023598379838E-46,4.72515227845561E-31)) ;
#77089 = DIRECTION('center_axis',(-4.72515227845561E-31,-7.02672800395669E-16,
1.)) ;
#77090 = DIRECTION('ref_axis',(-3.32023598379838E-46,1.,7.02672800395669E-16)) ;
#77091 = DIRECTION('',(-6.93889390390723E-16,-1.,-7.02672800395669E-16)) ;
#77092 = DIRECTION('center_axis',(-4.72515227845561E-31,-7.02672800395669E-16,
1.)) ;
#77093 = DIRECTION('ref_axis',(-3.32023598379838E-46,1.,7.02672800395669E-16)) ;
#77094 = DIRECTION('',(-1.,3.32023598379838E-46,-4.72515227845561E-31)) ;
#77095 = DIRECTION('center_axis',(-4.72515227845561E-31,-7.02672800395669E-16,
1.)) ;
#77096 = DIRECTION('ref_axis',(-3.32023598379838E-46,1.,7.02672800395669E-16)) ;
#77097 = DIRECTION('',(-4.15029497974802E-48,1.,7.02672800395669E-16)) ;
#77098 = DIRECTION('center_axis',(-4.72515227845561E-31,-7.02672800395669E-16,
1.)) ;
#77099 = DIRECTION('ref_axis',(-3.32023598379838E-46,1.,7.02672800395669E-16)) ;
#77100 = DIRECTION('',(1.,-3.32023598379838E-46,4.72515227845561E-31)) ;
#77101 = DIRECTION('center_axis',(-8.13512808509168E-31,-3.26576826218999E-61,
1.)) ;
#77102 = DIRECTION('ref_axis',(1.,4.27339674608664E-31,8.13512808509168E-31)) ;
#77103 = DIRECTION('',(-1.,-4.27339674608664E-31,-8.13512808509168E-31)) ;
#77104 = DIRECTION('',(4.27339674608664E-31,-1.,2.10694726592902E-62)) ;
#77105 = DIRECTION('center_axis',(-4.93038065763132E-32,0.,1.)) ;
#77106 = DIRECTION('ref_axis',(1.,0.,4.93038065763132E-32)) ;
#77107 = DIRECTION('',(-1.,4.27339674608665E-31,-4.93038065763132E-32)) ;
#77108 = DIRECTION('',(2.16840434497101E-16,-1.,1.06910588403688E-47)) ;
#77109 = DIRECTION('',(1.,-4.27339674608665E-31,4.93038065763132E-32)) ;
#77110 = DIRECTION('center_axis',(-4.93038065763132E-32,0.,1.)) ;
#77111 = DIRECTION('ref_axis',(1.,0.,4.93038065763132E-32)) ;
#77112 = DIRECTION('',(4.27339674608664E-31,-1.,2.10694726592902E-62)) ;
#77113 = DIRECTION('',(1.,-4.27339674608665E-31,4.93038065763132E-32)) ;
#77114 = DIRECTION('',(-3.49247269410375E-15,1.,-1.72192198183147E-46)) ;
#77115 = DIRECTION('',(-1.,-4.27339674608664E-31,-8.13512808509168E-31)) ;
#77116 = DIRECTION('center_axis',(-4.93038065763132E-32,0.,1.)) ;
#77117 = DIRECTION('ref_axis',(1.,0.,4.93038065763132E-32)) ;
#77118 = DIRECTION('',(1.73472347597681E-16,-1.,8.55284707229503E-48)) ;
#77119 = DIRECTION('center_axis',(-4.93038065763132E-32,0.,1.)) ;
#77120 = DIRECTION('ref_axis',(1.,0.,4.93038065763132E-32)) ;
#77121 = DIRECTION('',(-1.,0.,-4.93038065763132E-32)) ;
#77122 = DIRECTION('center_axis',(-4.93038065763132E-32,0.,1.)) ;
#77123 = DIRECTION('ref_axis',(1.,0.,4.93038065763132E-32)) ;
#77124 = DIRECTION('',(-2.60208521396521E-16,1.,-1.28292706084425E-47)) ;
#77125 = DIRECTION('center_axis',(-4.93038065763132E-32,0.,1.)) ;
#77126 = DIRECTION('ref_axis',(1.,0.,4.93038065763132E-32)) ;
#77127 = DIRECTION('',(1.,0.,4.93038065763132E-32)) ;
#77128 = DIRECTION('center_axis',(-4.93038065763132E-32,0.,1.)) ;
#77129 = DIRECTION('ref_axis',(1.,0.,4.93038065763132E-32)) ;
#77130 = DIRECTION('',(0.,-1.,0.)) ;
#77131 = DIRECTION('center_axis',(-4.93038065763132E-32,0.,1.)) ;
#77132 = DIRECTION('ref_axis',(1.,0.,4.93038065763132E-32)) ;
#77133 = DIRECTION('',(-1.,0.,-4.93038065763132E-32)) ;
#77134 = DIRECTION('center_axis',(-4.93038065763132E-32,0.,1.)) ;
#77135 = DIRECTION('ref_axis',(1.,0.,4.93038065763132E-32)) ;
#77136 = DIRECTION('',(-3.46944695195361E-16,1.,-1.71056941445901E-47)) ;
#77137 = DIRECTION('center_axis',(-4.93038065763132E-32,0.,1.)) ;
#77138 = DIRECTION('ref_axis',(1.,0.,4.93038065763132E-32)) ;
#77139 = DIRECTION('',(1.,0.,4.93038065763132E-32)) ;
#77140 = DIRECTION('center_axis',(-4.93038065763132E-32,0.,1.)) ;
#77141 = DIRECTION('ref_axis',(1.,0.,4.93038065763132E-32)) ;
#77142 = DIRECTION('',(6.93889390390723E-16,-1.,3.42113882891801E-47)) ;
#77143 = DIRECTION('center_axis',(-4.93038065763132E-32,0.,1.)) ;
#77144 = DIRECTION('ref_axis',(1.,0.,4.93038065763132E-32)) ;
#77145 = DIRECTION('',(-1.,0.,-4.93038065763132E-32)) ;
#77146 = DIRECTION('center_axis',(-4.93038065763132E-32,0.,1.)) ;
#77147 = DIRECTION('ref_axis',(1.,0.,4.93038065763132E-32)) ;
#77148 = DIRECTION('',(0.,1.,0.)) ;
#77149 = DIRECTION('center_axis',(-4.93038065763132E-32,0.,1.)) ;
#77150 = DIRECTION('ref_axis',(1.,0.,4.93038065763132E-32)) ;
#77151 = DIRECTION('',(1.,0.,4.93038065763132E-32)) ;
#77152 = DIRECTION('center_axis',(-4.93038065763132E-32,0.,1.)) ;
#77153 = DIRECTION('ref_axis',(1.,0.,4.93038065763132E-32)) ;
#77154 = DIRECTION('',(0.,-1.,0.)) ;
#77155 = DIRECTION('center_axis',(-4.93038065763132E-32,0.,1.)) ;
#77156 = DIRECTION('ref_axis',(1.,0.,4.93038065763132E-32)) ;
#77157 = DIRECTION('',(-1.,0.,-4.93038065763132E-32)) ;
#77158 = DIRECTION('center_axis',(-4.93038065763132E-32,0.,1.)) ;
#77159 = DIRECTION('ref_axis',(1.,0.,4.93038065763132E-32)) ;
#77160 = DIRECTION('',(0.,1.,0.)) ;
#77161 = DIRECTION('center_axis',(-4.93038065763132E-32,0.,1.)) ;
#77162 = DIRECTION('ref_axis',(1.,0.,4.93038065763132E-32)) ;
#77163 = DIRECTION('',(1.,0.,4.93038065763132E-32)) ;
#77164 = DIRECTION('center_axis',(-4.93038065763132E-32,0.,1.)) ;
#77165 = DIRECTION('ref_axis',(1.,0.,4.93038065763132E-32)) ;
#77166 = DIRECTION('',(0.,-1.,0.)) ;
#77167 = DIRECTION('center_axis',(-4.93038065763132E-32,0.,1.)) ;
#77168 = DIRECTION('ref_axis',(1.,0.,4.93038065763132E-32)) ;
#77169 = DIRECTION('',(-1.,0.,-4.93038065763132E-32)) ;
#77170 = DIRECTION('center_axis',(-4.93038065763132E-32,0.,1.)) ;
#77171 = DIRECTION('ref_axis',(1.,0.,4.93038065763132E-32)) ;
#77172 = DIRECTION('',(0.,1.,0.)) ;
#77173 = DIRECTION('center_axis',(-4.93038065763132E-32,0.,1.)) ;
#77174 = DIRECTION('ref_axis',(1.,0.,4.93038065763132E-32)) ;
#77175 = DIRECTION('',(1.,0.,4.93038065763132E-32)) ;
#77176 = DIRECTION('center_axis',(-4.93038065763132E-32,0.,1.)) ;
#77177 = DIRECTION('ref_axis',(1.,0.,4.93038065763132E-32)) ;
#77178 = DIRECTION('',(3.46944695195361E-16,-1.,1.71056941445901E-47)) ;
#77179 = DIRECTION('center_axis',(-4.93038065763132E-32,0.,1.)) ;
#77180 = DIRECTION('ref_axis',(1.,0.,4.93038065763132E-32)) ;
#77181 = DIRECTION('',(-1.,0.,-4.93038065763132E-32)) ;
#77182 = DIRECTION('center_axis',(-4.93038065763132E-32,0.,1.)) ;
#77183 = DIRECTION('ref_axis',(1.,0.,4.93038065763132E-32)) ;
#77184 = DIRECTION('',(0.,1.,0.)) ;
#77185 = DIRECTION('center_axis',(-4.93038065763132E-32,0.,1.)) ;
#77186 = DIRECTION('ref_axis',(1.,0.,4.93038065763132E-32)) ;
#77187 = DIRECTION('',(1.,0.,4.93038065763132E-32)) ;
#77188 = DIRECTION('center_axis',(-4.93038065763132E-32,0.,1.)) ;
#77189 = DIRECTION('ref_axis',(1.,0.,4.93038065763132E-32)) ;
#77190 = DIRECTION('',(-3.46944695195361E-16,1.,-1.71056941445901E-47)) ;
#77191 = DIRECTION('center_axis',(-4.93038065763132E-32,0.,1.)) ;
#77192 = DIRECTION('ref_axis',(1.,0.,4.93038065763132E-32)) ;
#77193 = DIRECTION('',(1.,0.,4.93038065763132E-32)) ;
#77194 = DIRECTION('center_axis',(-4.93038065763132E-32,0.,1.)) ;
#77195 = DIRECTION('ref_axis',(1.,0.,4.93038065763132E-32)) ;
#77196 = DIRECTION('',(0.,-1.,0.)) ;
#77197 = DIRECTION('center_axis',(-4.93038065763132E-32,0.,1.)) ;
#77198 = DIRECTION('ref_axis',(1.,0.,4.93038065763132E-32)) ;
#77199 = DIRECTION('',(-1.,0.,-4.93038065763132E-32)) ;
#77200 = DIRECTION('center_axis',(-8.13512808509168E-31,-3.26576826218999E-61,
1.)) ;
#77201 = DIRECTION('ref_axis',(1.,4.27339674608664E-31,8.13512808509168E-31)) ;
#77202 = DIRECTION('center_axis',(4.93038065763132E-32,0.,-1.)) ;
#77203 = DIRECTION('ref_axis',(1.,0.,4.93038065763132E-32)) ;
#77204 = DIRECTION('',(-4.27339674608664E-31,1.,-2.10694726592902E-62)) ;
#77205 = DIRECTION('',(-1.,-4.27339674608664E-31,-8.13512808509168E-31)) ;
#77206 = DIRECTION('',(-1.,-4.27339674608664E-31,-8.13512808509168E-31)) ;
#77207 = DIRECTION('',(3.49247269410375E-15,-1.,1.72192198183147E-46)) ;
#77208 = DIRECTION('',(-1.,4.27339674608665E-31,-4.93038065763132E-32)) ;
#77209 = DIRECTION('',(-4.27339674608664E-31,1.,-2.10694726592902E-62)) ;
#77210 = DIRECTION('center_axis',(4.93038065763132E-32,0.,-1.)) ;
#77211 = DIRECTION('ref_axis',(1.,0.,4.93038065763132E-32)) ;
#77212 = DIRECTION('',(-1.,4.27339674608665E-31,-4.93038065763132E-32)) ;
#77213 = DIRECTION('',(-2.16840434497101E-16,1.,-1.06910588403688E-47)) ;
#77214 = DIRECTION('',(1.,-4.27339674608665E-31,4.93038065763132E-32)) ;
#77215 = DIRECTION('center_axis',(4.93038065763132E-32,0.,-1.)) ;
#77216 = DIRECTION('ref_axis',(1.,0.,4.93038065763132E-32)) ;
#77217 = DIRECTION('',(-1.73472347597681E-16,1.,-8.55284707229503E-48)) ;
#77218 = DIRECTION('center_axis',(4.93038065763132E-32,0.,-1.)) ;
#77219 = DIRECTION('ref_axis',(1.,0.,4.93038065763132E-32)) ;
#77220 = DIRECTION('',(-1.,0.,-4.93038065763132E-32)) ;
#77221 = DIRECTION('center_axis',(4.93038065763132E-32,0.,-1.)) ;
#77222 = DIRECTION('ref_axis',(1.,0.,4.93038065763132E-32)) ;
#77223 = DIRECTION('',(2.60208521396521E-16,-1.,1.28292706084425E-47)) ;
#77224 = DIRECTION('center_axis',(4.93038065763132E-32,0.,-1.)) ;
#77225 = DIRECTION('ref_axis',(1.,0.,4.93038065763132E-32)) ;
#77226 = DIRECTION('',(1.,0.,4.93038065763132E-32)) ;
#77227 = DIRECTION('center_axis',(4.93038065763132E-32,0.,-1.)) ;
#77228 = DIRECTION('ref_axis',(1.,0.,4.93038065763132E-32)) ;
#77229 = DIRECTION('',(0.,1.,0.)) ;
#77230 = DIRECTION('center_axis',(4.93038065763132E-32,0.,-1.)) ;
#77231 = DIRECTION('ref_axis',(1.,0.,4.93038065763132E-32)) ;
#77232 = DIRECTION('',(-1.,0.,-4.93038065763132E-32)) ;
#77233 = DIRECTION('center_axis',(4.93038065763132E-32,0.,-1.)) ;
#77234 = DIRECTION('ref_axis',(1.,0.,4.93038065763132E-32)) ;
#77235 = DIRECTION('',(3.46944695195361E-16,-1.,1.71056941445901E-47)) ;
#77236 = DIRECTION('center_axis',(4.93038065763132E-32,0.,-1.)) ;
#77237 = DIRECTION('ref_axis',(1.,0.,4.93038065763132E-32)) ;
#77238 = DIRECTION('',(1.,0.,4.93038065763132E-32)) ;
#77239 = DIRECTION('center_axis',(4.93038065763132E-32,0.,-1.)) ;
#77240 = DIRECTION('ref_axis',(1.,0.,4.93038065763132E-32)) ;
#77241 = DIRECTION('',(-6.93889390390723E-16,1.,-3.42113882891801E-47)) ;
#77242 = DIRECTION('center_axis',(4.93038065763132E-32,0.,-1.)) ;
#77243 = DIRECTION('ref_axis',(1.,0.,4.93038065763132E-32)) ;
#77244 = DIRECTION('',(-1.,0.,-4.93038065763132E-32)) ;
#77245 = DIRECTION('center_axis',(4.93038065763132E-32,0.,-1.)) ;
#77246 = DIRECTION('ref_axis',(1.,0.,4.93038065763132E-32)) ;
#77247 = DIRECTION('',(0.,-1.,0.)) ;
#77248 = DIRECTION('center_axis',(4.93038065763132E-32,0.,-1.)) ;
#77249 = DIRECTION('ref_axis',(1.,0.,4.93038065763132E-32)) ;
#77250 = DIRECTION('',(1.,0.,4.93038065763132E-32)) ;
#77251 = DIRECTION('center_axis',(4.93038065763132E-32,0.,-1.)) ;
#77252 = DIRECTION('ref_axis',(1.,0.,4.93038065763132E-32)) ;
#77253 = DIRECTION('',(0.,1.,0.)) ;
#77254 = DIRECTION('center_axis',(4.93038065763132E-32,0.,-1.)) ;
#77255 = DIRECTION('ref_axis',(1.,0.,4.93038065763132E-32)) ;
#77256 = DIRECTION('',(-1.,0.,-4.93038065763132E-32)) ;
#77257 = DIRECTION('center_axis',(4.93038065763132E-32,0.,-1.)) ;
#77258 = DIRECTION('ref_axis',(1.,0.,4.93038065763132E-32)) ;
#77259 = DIRECTION('',(0.,-1.,0.)) ;
#77260 = DIRECTION('center_axis',(4.93038065763132E-32,0.,-1.)) ;
#77261 = DIRECTION('ref_axis',(1.,0.,4.93038065763132E-32)) ;
#77262 = DIRECTION('',(1.,0.,4.93038065763132E-32)) ;
#77263 = DIRECTION('center_axis',(4.93038065763132E-32,0.,-1.)) ;
#77264 = DIRECTION('ref_axis',(1.,0.,4.93038065763132E-32)) ;
#77265 = DIRECTION('',(0.,1.,0.)) ;
#77266 = DIRECTION('center_axis',(4.93038065763132E-32,0.,-1.)) ;
#77267 = DIRECTION('ref_axis',(1.,0.,4.93038065763132E-32)) ;
#77268 = DIRECTION('',(-1.,0.,-4.93038065763132E-32)) ;
#77269 = DIRECTION('center_axis',(4.93038065763132E-32,0.,-1.)) ;
#77270 = DIRECTION('ref_axis',(1.,0.,4.93038065763132E-32)) ;
#77271 = DIRECTION('',(0.,-1.,0.)) ;
#77272 = DIRECTION('center_axis',(4.93038065763132E-32,0.,-1.)) ;
#77273 = DIRECTION('ref_axis',(1.,0.,4.93038065763132E-32)) ;
#77274 = DIRECTION('',(1.,0.,4.93038065763132E-32)) ;
#77275 = DIRECTION('center_axis',(4.93038065763132E-32,0.,-1.)) ;
#77276 = DIRECTION('ref_axis',(1.,0.,4.93038065763132E-32)) ;
#77277 = DIRECTION('',(-3.46944695195361E-16,1.,-1.71056941445901E-47)) ;
#77278 = DIRECTION('center_axis',(4.93038065763132E-32,0.,-1.)) ;
#77279 = DIRECTION('ref_axis',(1.,0.,4.93038065763132E-32)) ;
#77280 = DIRECTION('',(-1.,0.,-4.93038065763132E-32)) ;
#77281 = DIRECTION('center_axis',(4.93038065763132E-32,0.,-1.)) ;
#77282 = DIRECTION('ref_axis',(1.,0.,4.93038065763132E-32)) ;
#77283 = DIRECTION('',(0.,-1.,0.)) ;
#77284 = DIRECTION('center_axis',(4.93038065763132E-32,0.,-1.)) ;
#77285 = DIRECTION('ref_axis',(1.,0.,4.93038065763132E-32)) ;
#77286 = DIRECTION('',(1.,0.,4.93038065763132E-32)) ;
#77287 = DIRECTION('center_axis',(4.93038065763132E-32,0.,-1.)) ;
#77288 = DIRECTION('ref_axis',(1.,0.,4.93038065763132E-32)) ;
#77289 = DIRECTION('',(3.46944695195361E-16,-1.,1.71056941445901E-47)) ;
#77290 = DIRECTION('center_axis',(4.93038065763132E-32,0.,-1.)) ;
#77291 = DIRECTION('ref_axis',(1.,0.,4.93038065763132E-32)) ;
#77292 = DIRECTION('',(1.,0.,4.93038065763132E-32)) ;
#77293 = DIRECTION('center_axis',(4.93038065763132E-32,0.,-1.)) ;
#77294 = DIRECTION('ref_axis',(1.,0.,4.93038065763132E-32)) ;
#77295 = DIRECTION('',(0.,1.,0.)) ;
#77296 = DIRECTION('center_axis',(4.93038065763132E-32,0.,-1.)) ;
#77297 = DIRECTION('ref_axis',(1.,0.,4.93038065763132E-32)) ;
#77298 = DIRECTION('',(-1.,0.,-4.93038065763132E-32)) ;
#77299 = DIRECTION('center_axis',(-4.15069017696469E-34,1.,1.83697019872103E-16)) ;
#77300 = DIRECTION('ref_axis',(4.60199940496102E-66,-1.83697019872103E-16,
1.)) ;
#77301 = DIRECTION('center_axis',(-4.15069017696469E-34,1.,1.83697019872103E-16)) ;
#77302 = DIRECTION('ref_axis',(1.85623770982812E-63,-1.83697019872103E-16,
1.)) ;
#77303 = DIRECTION('',(6.04532600737121E-48,-1.83697019872103E-16,1.)) ;
#77304 = DIRECTION('',(-1.,-3.29092219981587E-32,0.)) ;
#77305 = DIRECTION('',(0.,2.16840434497101E-16,-1.)) ;
#77306 = DIRECTION('',(-1.,-3.29092219981587E-32,0.)) ;
#77307 = DIRECTION('',(6.04532600737121E-48,-1.83697019872103E-16,1.)) ;
#77308 = DIRECTION('center_axis',(-4.15069017696469E-34,1.,1.83697019872103E-16)) ;
#77309 = DIRECTION('ref_axis',(1.85623770982812E-63,-1.83697019872103E-16,
1.)) ;
#77310 = DIRECTION('',(-1.,-4.15069017696469E-34,-7.62469415920825E-50)) ;
#77311 = DIRECTION('',(6.04532600737121E-48,-1.83697019872103E-16,1.)) ;
#77312 = DIRECTION('',(1.,4.15069017696469E-34,7.62469415920825E-50)) ;
#77313 = DIRECTION('center_axis',(-4.15069017696469E-34,1.,1.83697019872103E-16)) ;
#77314 = DIRECTION('ref_axis',(4.60199940496102E-66,-1.83697019872103E-16,
1.)) ;
#77315 = DIRECTION('',(-1.,-3.29092219981587E-32,0.)) ;
#77316 = DIRECTION('',(-6.04532600737121E-48,1.83697019872103E-16,-1.)) ;
#77317 = DIRECTION('center_axis',(4.15069017696469E-34,-1.,-1.83697019872103E-16)) ;
#77318 = DIRECTION('ref_axis',(-7.37593019805628E-50,-1.83697019872103E-16,
1.)) ;
#77319 = DIRECTION('',(-1.,-4.15069017696469E-34,-7.62469415920825E-50)) ;
#77320 = DIRECTION('',(-6.04532600737121E-48,1.83697019872103E-16,-1.)) ;
#77321 = DIRECTION('',(1.,4.15069017696469E-34,7.62469415920825E-50)) ;
#77322 = DIRECTION('center_axis',(4.15069017696469E-34,-1.,-1.83697019872103E-16)) ;
#77323 = DIRECTION('ref_axis',(-7.37593019805628E-50,-1.83697019872103E-16,
1.)) ;
#77324 = DIRECTION('',(-6.04532600737121E-48,1.83697019872103E-16,-1.)) ;
#77325 = DIRECTION('',(-1.,-3.29092219981587E-32,0.)) ;
#77326 = DIRECTION('',(0.,2.16840434497101E-16,-1.)) ;
#77327 = DIRECTION('center_axis',(-1.,-3.29092219981587E-32,0.)) ;
#77328 = DIRECTION('ref_axis',(0.,0.,1.)) ;
#77329 = DIRECTION('',(-3.29092219981587E-32,-1.,0.)) ;
#77330 = DIRECTION('',(6.04532600737121E-48,-1.83697019872103E-16,1.)) ;
#77331 = DIRECTION('',(-3.29092219981587E-32,1.,1.83697019872103E-16)) ;
#77332 = DIRECTION('',(-6.04532600737121E-48,1.83697019872103E-16,-1.)) ;
#77333 = DIRECTION('center_axis',(-1.,-3.29092219981587E-32,0.)) ;
#77334 = DIRECTION('ref_axis',(0.,0.,1.)) ;
#77335 = DIRECTION('',(3.29092219981587E-32,-1.,-1.83697019872103E-16)) ;
#77336 = DIRECTION('',(6.04532600737121E-48,-1.83697019872103E-16,1.)) ;
#77337 = DIRECTION('',(3.29092219981587E-32,1.,0.)) ;
#77338 = DIRECTION('',(-6.04532600737121E-48,1.83697019872103E-16,-1.)) ;
#77339 = DIRECTION('center_axis',(-1.,-3.29092219981587E-32,0.)) ;
#77340 = DIRECTION('ref_axis',(0.,0.,1.)) ;
#77341 = DIRECTION('',(6.04532600737121E-48,-1.83697019872103E-16,1.)) ;
#77342 = DIRECTION('',(-3.29092219981587E-32,1.,1.83697019872103E-16)) ;
#77343 = DIRECTION('',(-6.04532600737121E-48,1.83697019872103E-16,-1.)) ;
#77344 = DIRECTION('',(3.29092219981587E-32,-1.,-1.83697019872103E-16)) ;
#77345 = DIRECTION('center_axis',(0.,1.83697019872103E-16,-1.)) ;
#77346 = DIRECTION('ref_axis',(-4.15069017696464E-34,1.,1.83697019872103E-16)) ;
#77347 = DIRECTION('',(-1.,-4.15069017696469E-34,-7.62469415920825E-50)) ;
#77348 = DIRECTION('',(-3.29092219981587E-32,1.,1.83697019872103E-16)) ;
#77349 = DIRECTION('',(1.,4.15069017696469E-34,7.62469415920825E-50)) ;
#77350 = DIRECTION('',(3.29092219981587E-32,-1.,-1.83697019872103E-16)) ;
#77351 = DIRECTION('center_axis',(0.,-1.83697019872103E-16,1.)) ;
#77352 = DIRECTION('ref_axis',(4.15069017696464E-34,-1.,-1.83697019872103E-16)) ;
#77353 = DIRECTION('',(1.,4.15069017696469E-34,7.62469415920825E-50)) ;
#77354 = DIRECTION('',(-3.29092219981587E-32,1.,1.83697019872103E-16)) ;
#77355 = DIRECTION('',(-1.,-4.15069017696469E-34,-7.62469415920825E-50)) ;
#77356 = DIRECTION('',(3.29092219981587E-32,-1.,-1.83697019872103E-16)) ;
#77357 = DIRECTION('center_axis',(-1.,-3.29092219981587E-32,0.)) ;
#77358 = DIRECTION('ref_axis',(0.,0.,1.)) ;
#77359 = DIRECTION('center_axis',(1.,3.29092219981587E-32,0.)) ;
#77360 = DIRECTION('ref_axis',(3.29092219981587E-32,-1.,0.)) ;
#77361 = DIRECTION('',(3.94430452610506E-31,-2.89120579329467E-16,-1.)) ;
#77362 = DIRECTION('center_axis',(-1.,-3.29092219981587E-32,0.)) ;
#77363 = DIRECTION('ref_axis',(3.29092219981587E-32,-1.,0.)) ;
#77364 = DIRECTION('center_axis',(1.,3.29092219981587E-32,0.)) ;
#77365 = DIRECTION('ref_axis',(0.,0.,-1.)) ;
#77366 = DIRECTION('center_axis',(-1.,-3.29092219981587E-32,0.)) ;
#77367 = DIRECTION('ref_axis',(-3.29092219981587E-32,1.,-6.24500451351651E-14)) ;
#77368 = DIRECTION('',(-6.4275824215152E-33,1.,2.16840434497101E-16)) ;
#77369 = DIRECTION('center_axis',(-1.,-3.29092219981587E-32,0.)) ;
#77370 = DIRECTION('ref_axis',(0.,0.,1.)) ;
#77371 = DIRECTION('',(3.94430452610506E-31,-2.89120579329467E-16,-1.)) ;
#77372 = DIRECTION('center_axis',(1.,3.29092219981587E-32,0.)) ;
#77373 = DIRECTION('ref_axis',(-3.29092219981587E-32,1.,0.)) ;
#77374 = DIRECTION('center_axis',(1.,3.29092219981587E-32,0.)) ;
#77375 = DIRECTION('ref_axis',(3.29092219981587E-32,-1.,0.)) ;
#77376 = DIRECTION('center_axis',(1.,3.29092219981587E-32,0.)) ;
#77377 = DIRECTION('ref_axis',(-3.29092219981587E-32,1.,0.)) ;
#77378 = DIRECTION('center_axis',(-1.,-3.29092219981587E-32,0.)) ;
#77379 = DIRECTION('ref_axis',(3.29092219981587E-32,-1.,0.)) ;
#77380 = DIRECTION('center_axis',(-4.27339674608665E-31,-1.,-2.10694726592902E-62)) ;
#77381 = DIRECTION('ref_axis',(4.93038065763132E-32,-3.97608260439759E-77,
-1.)) ;
#77382 = DIRECTION('',(8.13512808509168E-31,9.86076131526265E-32,-1.)) ;
#77383 = DIRECTION('',(1.,-4.27339674608665E-31,4.93038065763132E-32)) ;
#77384 = DIRECTION('',(-7.39557098644695E-32,-9.86076131526265E-32,1.)) ;
#77385 = DIRECTION('',(-1.,4.27339674608665E-31,-4.93038065763132E-32)) ;
#77386 = DIRECTION('center_axis',(-1.,-4.27339674608664E-31,-4.93038065763132E-32)) ;
#77387 = DIRECTION('ref_axis',(-4.93038065763132E-32,0.,1.)) ;
#77388 = DIRECTION('',(4.27339674608664E-31,-1.,2.10694726592902E-62)) ;
#77389 = DIRECTION('',(-8.13512808509168E-31,-9.86076131526265E-32,1.)) ;
#77390 = DIRECTION('',(-4.27339674608664E-31,1.,-2.10694726592902E-62)) ;
#77391 = DIRECTION('',(8.13512808509168E-31,9.86076131526265E-32,-1.)) ;
#77392 = DIRECTION('center_axis',(-4.27339674608665E-31,-1.,-2.10694726592902E-62)) ;
#77393 = DIRECTION('ref_axis',(4.93038065763132E-32,-3.97608260439759E-77,
-1.)) ;
#77394 = DIRECTION('',(1.,-4.27339674608665E-31,4.93038065763132E-32)) ;
#77395 = DIRECTION('',(-8.13512808509168E-31,-9.86076131526265E-32,1.)) ;
#77396 = DIRECTION('',(-1.,4.27339674608665E-31,-4.93038065763132E-32)) ;
#77397 = DIRECTION('',(7.39557098644699E-31,9.86076131526265E-32,-1.)) ;
#77398 = DIRECTION('center_axis',(-1.,-2.168404344971E-16,-7.39557098644699E-31)) ;
#77399 = DIRECTION('ref_axis',(2.168404344971E-16,-1.,-9.86076131526265E-32)) ;
#77400 = DIRECTION('',(2.16840434497101E-16,-1.,1.06910588403688E-47)) ;
#77401 = DIRECTION('',(-7.39557098644699E-31,-9.86076131526265E-32,1.)) ;
#77402 = DIRECTION('',(-2.16840434497101E-16,1.,-1.06910588403688E-47)) ;
#77403 = DIRECTION('',(7.39557098644699E-31,9.86076131526265E-32,-1.)) ;
#77404 = DIRECTION('center_axis',(4.27339674608665E-31,1.,2.10694726592902E-62)) ;
#77405 = DIRECTION('ref_axis',(-4.93038065763132E-32,3.97608260439759E-77,
1.)) ;
#77406 = DIRECTION('',(-1.,4.27339674608665E-31,-4.93038065763132E-32)) ;
#77407 = DIRECTION('',(-7.39557098644699E-31,-9.86076131526265E-32,1.)) ;
#77408 = DIRECTION('',(1.,-4.27339674608665E-31,4.93038065763132E-32)) ;
#77409 = DIRECTION('',(8.13512808509168E-31,9.86076131526265E-32,-1.)) ;
#77410 = DIRECTION('center_axis',(-1.,-3.49247269410375E-15,-7.39557098644699E-32)) ;
#77411 = DIRECTION('ref_axis',(3.49247269410375E-15,-1.,3.2391255885562E-16)) ;
#77412 = DIRECTION('',(3.49247269410375E-15,-1.,1.72192198183147E-46)) ;
#77413 = DIRECTION('',(7.39557098644695E-32,9.86076131526265E-32,-1.)) ;
#77414 = DIRECTION('',(-3.49247269410375E-15,1.,-1.72192198183147E-46)) ;
#77415 = DIRECTION('',(-1.08370143847609E-30,2.89120579329467E-16,1.)) ;
#77416 = DIRECTION('center_axis',(-1.,-4.27339674608664E-31,-4.93038065763132E-32)) ;
#77417 = DIRECTION('ref_axis',(-4.93038065763132E-32,0.,1.)) ;
#77418 = DIRECTION('',(4.27339674608664E-31,-1.,2.10694726592902E-62)) ;
#77419 = DIRECTION('',(-8.13512808509168E-31,-9.86076131526265E-32,1.)) ;
#77420 = DIRECTION('',(-4.27339674608664E-31,1.,-2.10694726592902E-62)) ;
#77421 = DIRECTION('center_axis',(4.7978874716823E-31,1.,-2.89120579329467E-16)) ;
#77422 = DIRECTION('ref_axis',(-3.94430452610506E-31,2.89120579329467E-16,
1.)) ;
#77423 = DIRECTION('',(1.08370143847609E-30,-2.89120579329467E-16,-1.)) ;
#77424 = DIRECTION('center_axis',(-2.14282066180855E-30,7.70988211545247E-16,
-1.)) ;
#77425 = DIRECTION('ref_axis',(0.,1.,7.70988211545247E-16)) ;
#77426 = DIRECTION('',(3.65204942310907E-15,-1.,-7.70988211545247E-16)) ;
#77427 = DIRECTION('',(-1.,-3.49148133884313E-15,-5.4907029126972E-31)) ;
#77428 = DIRECTION('',(-3.65204942310907E-15,1.,7.70988211545247E-16)) ;
#77429 = DIRECTION('',(1.,3.65204942310907E-15,6.72866391389159E-31)) ;
#77430 = DIRECTION('center_axis',(-3.49148133884313E-15,1.,1.81408990951823E-16)) ;
#77431 = DIRECTION('ref_axis',(-1.,-3.49148133884313E-15,0.)) ;
#77432 = DIRECTION('',(-1.03517906367563E-32,-1.81408990951823E-16,1.)) ;
#77433 = DIRECTION('',(-1.,-3.49148133884313E-15,-6.7286639138916E-31)) ;
#77434 = DIRECTION('',(1.03517906367563E-32,1.81408990951823E-16,-1.)) ;
#77435 = DIRECTION('',(1.,3.49148133884313E-15,5.4907029126972E-31)) ;
#77436 = DIRECTION('center_axis',(6.7286639138916E-31,2.33447425067715E-45,
-1.)) ;
#77437 = DIRECTION('ref_axis',(-1.,-8.92425379131539E-92,-6.7286639138916E-31)) ;
#77438 = DIRECTION('',(-3.65204942310907E-15,1.,-1.22867065825113E-46)) ;
#77439 = DIRECTION('',(-1.,-3.65204942310907E-15,-6.7286639138916E-31)) ;
#77440 = DIRECTION('',(3.65204942310907E-15,-1.,1.22867065825113E-46)) ;
#77441 = DIRECTION('',(1.,3.49148133884313E-15,6.7286639138916E-31)) ;
#77442 = DIRECTION('center_axis',(3.65204942310907E-15,-1.,-2.47817639425257E-16)) ;
#77443 = DIRECTION('ref_axis',(1.,3.65204942310907E-15,0.)) ;
#77444 = DIRECTION('',(1.,3.65204942310907E-15,6.7286639138916E-31)) ;
#77445 = DIRECTION('',(1.,3.65204942310907E-15,6.12323399573677E-17)) ;
#77446 = DIRECTION('center_axis',(-3.65204942310907E-15,1.,2.47817639425258E-16)) ;
#77447 = DIRECTION('ref_axis',(-1.,-3.65204942310907E-15,0.)) ;
#77448 = DIRECTION('',(-1.,-3.65204942310907E-15,-6.72866391389159E-31)) ;
#77449 = DIRECTION('',(1.,3.65204942310907E-15,6.12323399573677E-17)) ;
#77450 = DIRECTION('center_axis',(0.,0.,-1.)) ;
#77451 = DIRECTION('ref_axis',(-1.,0.,0.)) ;
#77452 = DIRECTION('center_axis',(-1.03517906367563E-32,-1.81408990951823E-16,
1.)) ;
#77453 = DIRECTION('ref_axis',(1.87790789395849E-48,-1.,-1.81408990951823E-16)) ;
#77454 = DIRECTION('',(3.29092219981587E-32,1.,0.)) ;
#77455 = DIRECTION('center_axis',(0.,0.,1.)) ;
#77456 = DIRECTION('ref_axis',(1.,0.,0.)) ;
#77457 = DIRECTION('center_axis',(0.,0.,1.)) ;
#77458 = DIRECTION('ref_axis',(1.,0.,0.)) ;
#77459 = DIRECTION('center_axis',(1.03517906367563E-32,1.81408990951823E-16,
-1.)) ;
#77460 = DIRECTION('ref_axis',(1.87790789395849E-48,-1.,-1.81408990951823E-16)) ;
#77461 = DIRECTION('center_axis',(0.,0.,-1.)) ;
#77462 = DIRECTION('ref_axis',(-1.,0.,0.)) ;
#77463 = DIRECTION('center_axis',(-1.03517906367563E-32,-1.81408990951823E-16,
1.)) ;
#77464 = DIRECTION('ref_axis',(1.87790789395849E-48,-1.,-1.81408990951823E-16)) ;
#77465 = DIRECTION('center_axis',(-1.03517906367563E-32,-1.81408990951823E-16,
1.)) ;
#77466 = DIRECTION('ref_axis',(1.87790789395849E-48,-1.,-1.81408990951823E-16)) ;
#77467 = DIRECTION('center_axis',(-1.,5.06932053596301E-14,2.51253409742467E-28)) ;
#77468 = DIRECTION('ref_axis',(-5.06932053596301E-14,-1.,-9.19700082708845E-58)) ;
#77469 = DIRECTION('',(4.42639173855935E-31,8.67361737988403E-16,-1.)) ;
#77470 = DIRECTION('center_axis',(1.,-5.06932053596301E-14,-2.51253409742467E-28)) ;
#77471 = DIRECTION('ref_axis',(-5.06932053596301E-14,-1.,-9.19700082708845E-58)) ;
#77472 = DIRECTION('center_axis',(-1.,5.06932053596301E-14,2.51253409742467E-28)) ;
#77473 = DIRECTION('ref_axis',(-5.06932053596301E-14,-1.,1.62924697510308E-57)) ;
#77474 = DIRECTION('center_axis',(1.,0.,0.)) ;
#77475 = DIRECTION('ref_axis',(0.,0.,-1.)) ;
#77476 = DIRECTION('center_axis',(-1.,-3.29092219981587E-32,0.)) ;
#77477 = DIRECTION('ref_axis',(3.29092219981587E-32,-1.,0.)) ;
#77478 = DIRECTION('',(4.42639173855935E-31,8.67361737988403E-16,-1.)) ;
#77479 = DIRECTION('center_axis',(-1.,0.,0.)) ;
#77480 = DIRECTION('ref_axis',(0.,0.,1.)) ;
#77481 = DIRECTION('center_axis',(-1.,-3.29092219981587E-32,0.)) ;
#77482 = DIRECTION('ref_axis',(3.29092219981587E-32,-1.,0.)) ;
#77483 = DIRECTION('center_axis',(1.,-5.06932053596301E-14,-2.51253409742467E-28)) ;
#77484 = DIRECTION('ref_axis',(-5.06932053596301E-14,-1.,-2.48867833802847E-46)) ;
#77485 = DIRECTION('center_axis',(-1.,-3.29092219981587E-32,0.)) ;
#77486 = DIRECTION('ref_axis',(3.29092219981587E-32,-1.,0.)) ;
#77487 = DIRECTION('center_axis',(-1.,5.06932053596301E-14,2.51253409742467E-28)) ;
#77488 = DIRECTION('ref_axis',(-5.06932053596301E-14,-1.,1.69691425681666E-45)) ;
#77489 = DIRECTION('center_axis',(-4.18667286880966E-31,-1.,-8.60595472516328E-62)) ;
#77490 = DIRECTION('ref_axis',(2.05555938924125E-31,-1.72481183944414E-76,
-1.)) ;
#77491 = DIRECTION('',(1.,-4.18667286880966E-31,4.7251522784556E-31)) ;
#77492 = DIRECTION('',(-8.21355058201474E-31,3.43874493783169E-61,-1.)) ;
#77493 = DIRECTION('',(-1.,4.18667286880966E-31,-4.7251522784556E-31)) ;
#77494 = DIRECTION('',(5.76147612141447E-31,-2.41214157618207E-61,1.)) ;
#77495 = DIRECTION('center_axis',(1.,2.168404344971E-16,-5.76147612141446E-31)) ;
#77496 = DIRECTION('ref_axis',(-2.168404344971E-16,1.,-2.50236562288566E-63)) ;
#77497 = DIRECTION('',(-2.16840434497101E-16,1.,7.02672800395669E-16)) ;
#77498 = DIRECTION('',(-5.76147612141447E-31,2.33363072919793E-61,-1.)) ;
#77499 = DIRECTION('',(2.16840434497101E-16,-1.,-7.02672800395669E-16)) ;
#77500 = DIRECTION('',(5.76147612141447E-31,-2.33363072919793E-61,1.)) ;
#77501 = DIRECTION('center_axis',(4.18667286880966E-31,1.,8.60595472516328E-62)) ;
#77502 = DIRECTION('ref_axis',(-2.05555938924125E-31,1.72481183944414E-76,
1.)) ;
#77503 = DIRECTION('',(-1.,4.18667286880966E-31,-4.7251522784556E-31)) ;
#77504 = DIRECTION('',(-5.76147612141447E-31,2.41214157618207E-61,-1.)) ;
#77505 = DIRECTION('',(1.,-4.18667286880966E-31,4.7251522784556E-31)) ;
#77506 = DIRECTION('',(8.21355058201474E-31,-3.43874493783169E-61,1.)) ;
#77507 = DIRECTION('center_axis',(1.,7.43707788821671E-32,2.05555938924125E-31)) ;
#77508 = DIRECTION('ref_axis',(2.05555938924125E-31,0.,-1.)) ;
#77509 = DIRECTION('',(-7.43707788821665E-32,1.,7.02672800395669E-16)) ;
#77510 = DIRECTION('',(-8.21355058201474E-31,3.43874493783169E-61,-1.)) ;
#77511 = DIRECTION('',(7.43707788821665E-32,-1.,-7.02672800395669E-16)) ;
#77512 = DIRECTION('',(8.21355058201474E-31,-3.43874493783169E-61,1.)) ;
#77513 = DIRECTION('center_axis',(-4.18667286880966E-31,-1.,-8.60595472516328E-62)) ;
#77514 = DIRECTION('ref_axis',(2.05555938924125E-31,-1.72481183944414E-76,
-1.)) ;
#77515 = DIRECTION('',(-1.,4.18667286880966E-31,-4.7251522784556E-31)) ;
#77516 = DIRECTION('',(-8.21355058201474E-31,3.43874493783169E-61,-1.)) ;
#77517 = DIRECTION('',(1.,-4.18667286880966E-31,4.7251522784556E-31)) ;
#77518 = DIRECTION('',(-2.73644213932283E-30,1.14565880617704E-60,1.)) ;
#77519 = DIRECTION('center_axis',(1.,3.49501116159781E-15,2.76935136132099E-30)) ;
#77520 = DIRECTION('ref_axis',(-1.18287628881384E-30,1.13081975060932E-15,
-1.)) ;
#77521 = DIRECTION('',(2.73644213932283E-30,-1.24460305557223E-60,-1.)) ;
#77522 = DIRECTION('',(-3.49501116159781E-15,1.,7.02672800395669E-16)) ;
#77523 = DIRECTION('',(2.94996816089511E-31,-8.67361737988403E-16,1.)) ;
#77524 = DIRECTION('',(3.49501116159781E-15,-1.,-7.02672800395669E-16)) ;
#77525 = DIRECTION('center_axis',(2.70755867152026E-31,1.,8.67361737988403E-16)) ;
#77526 = DIRECTION('ref_axis',(-4.42639173855935E-31,-8.67361737988403E-16,
1.)) ;
#77527 = DIRECTION('',(-2.94996816089511E-31,8.67361737988403E-16,-1.)) ;
#77528 = DIRECTION('center_axis',(1.,7.43707788821671E-32,2.05555938924125E-31)) ;
#77529 = DIRECTION('ref_axis',(2.05555938924125E-31,0.,-1.)) ;
#77530 = DIRECTION('',(8.21355058201474E-31,-3.43874493783169E-61,1.)) ;
#77531 = DIRECTION('',(-7.43707788821665E-32,1.,7.02672800395669E-16)) ;
#77532 = DIRECTION('',(7.43707788821665E-32,-1.,-7.02672800395669E-16)) ;
#77533 = DIRECTION('center_axis',(0.,-1.,0.)) ;
#77534 = DIRECTION('ref_axis',(0.,0.,-1.)) ;
#77535 = DIRECTION('',(1.,0.,4.93038065763132E-32)) ;
#77536 = DIRECTION('',(0.,0.,-1.)) ;
#77537 = DIRECTION('',(-1.,0.,-4.93038065763132E-32)) ;
#77538 = DIRECTION('',(0.,0.,1.)) ;
#77539 = DIRECTION('center_axis',(-1.,0.,0.)) ;
#77540 = DIRECTION('ref_axis',(0.,0.,1.)) ;
#77541 = DIRECTION('',(0.,-1.,0.)) ;
#77542 = DIRECTION('',(0.,0.,-1.)) ;
#77543 = DIRECTION('',(0.,1.,0.)) ;
#77544 = DIRECTION('',(0.,0.,1.)) ;
#77545 = DIRECTION('center_axis',(0.,1.,0.)) ;
#77546 = DIRECTION('ref_axis',(0.,0.,1.)) ;
#77547 = DIRECTION('',(1.,0.,4.93038065763132E-32)) ;
#77548 = DIRECTION('',(0.,0.,1.)) ;
#77549 = DIRECTION('',(-1.,0.,-4.93038065763132E-32)) ;
#77550 = DIRECTION('',(0.,0.,-1.)) ;
#77551 = DIRECTION('center_axis',(1.,0.,0.)) ;
#77552 = DIRECTION('ref_axis',(0.,0.,-1.)) ;
#77553 = DIRECTION('',(0.,1.,0.)) ;
#77554 = DIRECTION('',(0.,0.,-1.)) ;
#77555 = DIRECTION('',(0.,-1.,0.)) ;
#77556 = DIRECTION('',(0.,0.,1.)) ;
#77557 = DIRECTION('center_axis',(0.,-1.,0.)) ;
#77558 = DIRECTION('ref_axis',(0.,0.,-1.)) ;
#77559 = DIRECTION('',(1.,0.,4.93038065763132E-32)) ;
#77560 = DIRECTION('',(0.,0.,-1.)) ;
#77561 = DIRECTION('',(-1.,0.,-4.93038065763132E-32)) ;
#77562 = DIRECTION('',(0.,0.,1.)) ;
#77563 = DIRECTION('center_axis',(-1.,0.,0.)) ;
#77564 = DIRECTION('ref_axis',(0.,0.,1.)) ;
#77565 = DIRECTION('',(0.,-1.,0.)) ;
#77566 = DIRECTION('',(0.,0.,-1.)) ;
#77567 = DIRECTION('',(0.,1.,0.)) ;
#77568 = DIRECTION('',(0.,0.,1.)) ;
#77569 = DIRECTION('center_axis',(0.,1.,0.)) ;
#77570 = DIRECTION('ref_axis',(0.,0.,1.)) ;
#77571 = DIRECTION('',(1.,0.,4.93038065763132E-32)) ;
#77572 = DIRECTION('',(0.,0.,1.)) ;
#77573 = DIRECTION('',(-1.,0.,-4.93038065763132E-32)) ;
#77574 = DIRECTION('',(0.,0.,-1.)) ;
#77575 = DIRECTION('center_axis',(1.,0.,0.)) ;
#77576 = DIRECTION('ref_axis',(0.,0.,-1.)) ;
#77577 = DIRECTION('',(0.,1.,0.)) ;
#77578 = DIRECTION('',(0.,0.,-1.)) ;
#77579 = DIRECTION('',(0.,-1.,0.)) ;
#77580 = DIRECTION('',(0.,0.,1.)) ;
#77581 = DIRECTION('center_axis',(0.,-1.,0.)) ;
#77582 = DIRECTION('ref_axis',(0.,0.,-1.)) ;
#77583 = DIRECTION('',(1.,0.,4.93038065763132E-32)) ;
#77584 = DIRECTION('',(0.,0.,-1.)) ;
#77585 = DIRECTION('',(-1.,0.,-4.93038065763132E-32)) ;
#77586 = DIRECTION('',(0.,0.,1.)) ;
#77587 = DIRECTION('center_axis',(-1.,0.,0.)) ;
#77588 = DIRECTION('ref_axis',(0.,0.,1.)) ;
#77589 = DIRECTION('',(0.,-1.,0.)) ;
#77590 = DIRECTION('',(0.,0.,-1.)) ;
#77591 = DIRECTION('',(0.,1.,0.)) ;
#77592 = DIRECTION('',(0.,0.,1.)) ;
#77593 = DIRECTION('center_axis',(0.,1.,0.)) ;
#77594 = DIRECTION('ref_axis',(0.,0.,1.)) ;
#77595 = DIRECTION('',(1.,0.,4.93038065763132E-32)) ;
#77596 = DIRECTION('',(0.,0.,1.)) ;
#77597 = DIRECTION('',(-1.,0.,-4.93038065763132E-32)) ;
#77598 = DIRECTION('',(0.,0.,-1.)) ;
#77599 = DIRECTION('center_axis',(1.,6.93889390390723E-16,0.)) ;
#77600 = DIRECTION('ref_axis',(-6.93889390390723E-16,1.,0.)) ;
#77601 = DIRECTION('',(-6.93889390390723E-16,1.,-3.42113882891801E-47)) ;
#77602 = DIRECTION('',(0.,0.,-1.)) ;
#77603 = DIRECTION('',(6.93889390390723E-16,-1.,3.42113882891801E-47)) ;
#77604 = DIRECTION('',(0.,0.,1.)) ;
#77605 = DIRECTION('center_axis',(0.,-1.,0.)) ;
#77606 = DIRECTION('ref_axis',(0.,0.,-1.)) ;
#77607 = DIRECTION('',(1.,0.,4.93038065763132E-32)) ;
#77608 = DIRECTION('',(0.,0.,-1.)) ;
#77609 = DIRECTION('',(-1.,0.,-4.93038065763132E-32)) ;
#77610 = DIRECTION('',(0.,0.,1.)) ;
#77611 = DIRECTION('center_axis',(-1.,0.,0.)) ;
#77612 = DIRECTION('ref_axis',(0.,0.,1.)) ;
#77613 = DIRECTION('',(0.,-1.,0.)) ;
#77614 = DIRECTION('',(0.,0.,-1.)) ;
#77615 = DIRECTION('',(0.,1.,0.)) ;
#77616 = DIRECTION('',(0.,0.,1.)) ;
#77617 = DIRECTION('center_axis',(0.,1.,0.)) ;
#77618 = DIRECTION('ref_axis',(0.,0.,1.)) ;
#77619 = DIRECTION('',(1.,0.,4.93038065763132E-32)) ;
#77620 = DIRECTION('',(0.,0.,1.)) ;
#77621 = DIRECTION('',(-1.,0.,-4.93038065763132E-32)) ;
#77622 = DIRECTION('',(0.,0.,-1.)) ;
#77623 = DIRECTION('center_axis',(1.,3.46944695195361E-16,0.)) ;
#77624 = DIRECTION('ref_axis',(-3.46944695195361E-16,1.,0.)) ;
#77625 = DIRECTION('',(-3.46944695195361E-16,1.,-1.71056941445901E-47)) ;
#77626 = DIRECTION('',(0.,0.,-1.)) ;
#77627 = DIRECTION('',(3.46944695195361E-16,-1.,1.71056941445901E-47)) ;
#77628 = DIRECTION('',(0.,0.,1.)) ;
#77629 = DIRECTION('center_axis',(0.,-1.,0.)) ;
#77630 = DIRECTION('ref_axis',(0.,0.,-1.)) ;
#77631 = DIRECTION('',(1.,0.,4.93038065763132E-32)) ;
#77632 = DIRECTION('',(0.,0.,-1.)) ;
#77633 = DIRECTION('',(-1.,0.,-4.93038065763132E-32)) ;
#77634 = DIRECTION('',(0.,0.,1.)) ;
#77635 = DIRECTION('center_axis',(-1.,-3.46944695195361E-16,0.)) ;
#77636 = DIRECTION('ref_axis',(3.46944695195361E-16,-1.,0.)) ;
#77637 = DIRECTION('',(3.46944695195361E-16,-1.,1.71056941445901E-47)) ;
#77638 = DIRECTION('',(0.,0.,-1.)) ;
#77639 = DIRECTION('',(-3.46944695195361E-16,1.,-1.71056941445901E-47)) ;
#77640 = DIRECTION('',(0.,0.,1.)) ;
#77641 = DIRECTION('center_axis',(0.,1.,0.)) ;
#77642 = DIRECTION('ref_axis',(0.,0.,1.)) ;
#77643 = DIRECTION('',(1.,0.,4.93038065763132E-32)) ;
#77644 = DIRECTION('',(0.,0.,1.)) ;
#77645 = DIRECTION('',(-1.,0.,-4.93038065763132E-32)) ;
#77646 = DIRECTION('',(0.,0.,-1.)) ;
#77647 = DIRECTION('center_axis',(1.,0.,0.)) ;
#77648 = DIRECTION('ref_axis',(0.,0.,-1.)) ;
#77649 = DIRECTION('',(0.,1.,0.)) ;
#77650 = DIRECTION('',(0.,0.,-1.)) ;
#77651 = DIRECTION('',(0.,-1.,0.)) ;
#77652 = DIRECTION('',(0.,0.,1.)) ;
#77653 = DIRECTION('center_axis',(0.,-1.,0.)) ;
#77654 = DIRECTION('ref_axis',(0.,0.,-1.)) ;
#77655 = DIRECTION('',(-1.,0.,-4.93038065763132E-32)) ;
#77656 = DIRECTION('',(0.,0.,1.)) ;
#77657 = DIRECTION('',(1.,0.,4.93038065763132E-32)) ;
#77658 = DIRECTION('',(0.,0.,-1.)) ;
#77659 = DIRECTION('center_axis',(-1.,-3.46944695195361E-16,0.)) ;
#77660 = DIRECTION('ref_axis',(3.46944695195361E-16,-1.,0.)) ;
#77661 = DIRECTION('',(3.46944695195361E-16,-1.,1.71056941445901E-47)) ;
#77662 = DIRECTION('',(0.,0.,-1.)) ;
#77663 = DIRECTION('',(-3.46944695195361E-16,1.,-1.71056941445901E-47)) ;
#77664 = DIRECTION('',(0.,0.,1.)) ;
#77665 = DIRECTION('center_axis',(0.,1.,0.)) ;
#77666 = DIRECTION('ref_axis',(0.,0.,1.)) ;
#77667 = DIRECTION('',(-1.,0.,-4.93038065763132E-32)) ;
#77668 = DIRECTION('',(0.,0.,-1.)) ;
#77669 = DIRECTION('',(1.,0.,4.93038065763132E-32)) ;
#77670 = DIRECTION('',(0.,0.,1.)) ;
#77671 = DIRECTION('center_axis',(1.,0.,0.)) ;
#77672 = DIRECTION('ref_axis',(0.,0.,-1.)) ;
#77673 = DIRECTION('',(0.,1.,0.)) ;
#77674 = DIRECTION('',(0.,0.,-1.)) ;
#77675 = DIRECTION('',(0.,-1.,0.)) ;
#77676 = DIRECTION('',(0.,0.,1.)) ;
#77677 = DIRECTION('center_axis',(1.,1.73472347597681E-16,0.)) ;
#77678 = DIRECTION('ref_axis',(-1.73472347597681E-16,1.,0.)) ;
#77679 = DIRECTION('',(-1.73472347597681E-16,1.,-8.55284707229503E-48)) ;
#77680 = DIRECTION('',(0.,0.,-1.)) ;
#77681 = DIRECTION('',(1.73472347597681E-16,-1.,8.55284707229503E-48)) ;
#77682 = DIRECTION('',(0.,0.,1.)) ;
#77683 = DIRECTION('center_axis',(0.,-1.,0.)) ;
#77684 = DIRECTION('ref_axis',(0.,0.,-1.)) ;
#77685 = DIRECTION('',(1.,0.,4.93038065763132E-32)) ;
#77686 = DIRECTION('',(0.,0.,-1.)) ;
#77687 = DIRECTION('',(-1.,0.,-4.93038065763132E-32)) ;
#77688 = DIRECTION('',(0.,0.,1.)) ;
#77689 = DIRECTION('center_axis',(-1.,-2.60208521396521E-16,0.)) ;
#77690 = DIRECTION('ref_axis',(2.60208521396521E-16,-1.,0.)) ;
#77691 = DIRECTION('',(2.60208521396521E-16,-1.,1.28292706084425E-47)) ;
#77692 = DIRECTION('',(0.,0.,-1.)) ;
#77693 = DIRECTION('',(-2.60208521396521E-16,1.,-1.28292706084425E-47)) ;
#77694 = DIRECTION('',(0.,0.,1.)) ;
#77695 = DIRECTION('center_axis',(0.,1.,0.)) ;
#77696 = DIRECTION('ref_axis',(0.,0.,1.)) ;
#77697 = DIRECTION('',(1.,0.,4.93038065763132E-32)) ;
#77698 = DIRECTION('',(0.,0.,1.)) ;
#77699 = DIRECTION('',(-1.,0.,-4.93038065763132E-32)) ;
#77700 = DIRECTION('',(0.,0.,-1.)) ;
#77701 = DIRECTION('center_axis',(0.,-1.,-7.02672800395669E-16)) ;
#77702 = DIRECTION('ref_axis',(0.,7.02672800395669E-16,-1.)) ;
#77703 = DIRECTION('',(1.,-3.32023598379838E-46,4.72515227845561E-31)) ;
#77704 = DIRECTION('',(4.72515227845561E-31,7.02672800395669E-16,-1.)) ;
#77705 = DIRECTION('',(-1.,3.32023598379838E-46,-4.72515227845561E-31)) ;
#77706 = DIRECTION('',(-4.72515227845561E-31,-7.02672800395669E-16,1.)) ;
#77707 = DIRECTION('center_axis',(1.,-6.93889390390723E-16,-1.50619732651321E-32)) ;
#77708 = DIRECTION('ref_axis',(6.93889390390723E-16,1.,-3.11691497273953E-64)) ;
#77709 = DIRECTION('',(-6.93889390390723E-16,-1.,-7.02672800395669E-16)) ;
#77710 = DIRECTION('',(-4.72515227845561E-31,-7.02672800395669E-16,1.)) ;
#77711 = DIRECTION('',(6.93889390390723E-16,1.,7.02672800395669E-16)) ;
#77712 = DIRECTION('',(4.72515227845561E-31,7.02672800395669E-16,-1.)) ;
#77713 = DIRECTION('center_axis',(0.,1.,7.02672800395669E-16)) ;
#77714 = DIRECTION('ref_axis',(0.,-7.02672800395669E-16,1.)) ;
#77715 = DIRECTION('',(1.,-3.32023598379838E-46,4.72515227845561E-31)) ;
#77716 = DIRECTION('',(-4.72515227845561E-31,-7.02672800395669E-16,1.)) ;
#77717 = DIRECTION('',(-1.,3.32023598379838E-46,-4.72515227845561E-31)) ;
#77718 = DIRECTION('',(4.72515227845561E-31,7.02672800395669E-16,-1.)) ;
#77719 = DIRECTION('center_axis',(-1.,3.2787330340009E-46,-4.72515227845561E-31)) ;
#77720 = DIRECTION('ref_axis',(-4.72515227845561E-31,0.,1.)) ;
#77721 = DIRECTION('',(-4.15029497974802E-48,1.,7.02672800395669E-16)) ;
#77722 = DIRECTION('',(-4.72515227845561E-31,-7.02672800395669E-16,1.)) ;
#77723 = DIRECTION('',(4.15029497974802E-48,-1.,-7.02672800395669E-16)) ;
#77724 = DIRECTION('',(4.72515227845561E-31,7.02672800395669E-16,-1.)) ;
#77725 = DIRECTION('center_axis',(0.,1.,7.02672800395669E-16)) ;
#77726 = DIRECTION('ref_axis',(0.,-7.02672800395669E-16,1.)) ;
#77727 = DIRECTION('',(-1.,3.32023598379838E-46,-4.72515227845561E-31)) ;
#77728 = DIRECTION('',(4.72515227845561E-31,7.02672800395669E-16,-1.)) ;
#77729 = DIRECTION('',(1.,-3.32023598379838E-46,4.72515227845561E-31)) ;
#77730 = DIRECTION('',(-4.72515227845561E-31,-7.02672800395669E-16,1.)) ;
#77731 = DIRECTION('center_axis',(1.,-3.12260288952466E-46,4.72515227845561E-31)) ;
#77732 = DIRECTION('ref_axis',(4.72515227845561E-31,0.,-1.)) ;
#77733 = DIRECTION('',(1.97633094273713E-47,-1.,-7.02672800395669E-16)) ;
#77734 = DIRECTION('',(-4.72515227845561E-31,-7.02672800395669E-16,1.)) ;
#77735 = DIRECTION('',(-1.97633094273713E-47,1.,7.02672800395669E-16)) ;
#77736 = DIRECTION('',(4.72515227845561E-31,7.02672800395669E-16,-1.)) ;
#77737 = DIRECTION('center_axis',(0.,-1.,-7.02672800395669E-16)) ;
#77738 = DIRECTION('ref_axis',(0.,7.02672800395669E-16,-1.)) ;
#77739 = DIRECTION('',(-1.,3.32023598379838E-46,-4.72515227845561E-31)) ;
#77740 = DIRECTION('',(-4.72515227845561E-31,-7.02672800395669E-16,1.)) ;
#77741 = DIRECTION('',(1.,-3.32023598379838E-46,4.72515227845561E-31)) ;
#77742 = DIRECTION('',(4.72515227845561E-31,7.02672800395669E-16,-1.)) ;
#77743 = DIRECTION('center_axis',(-1.,3.12260288952466E-46,-4.72515227845561E-31)) ;
#77744 = DIRECTION('ref_axis',(-4.72515227845561E-31,0.,1.)) ;
#77745 = DIRECTION('',(-1.97633094273713E-47,1.,7.02672800395669E-16)) ;
#77746 = DIRECTION('',(-4.72515227845561E-31,-7.02672800395669E-16,1.)) ;
#77747 = DIRECTION('',(1.97633094273713E-47,-1.,-7.02672800395669E-16)) ;
#77748 = DIRECTION('',(4.72515227845561E-31,7.02672800395669E-16,-1.)) ;
#77749 = DIRECTION('center_axis',(0.,-1.,-7.02672800395669E-16)) ;
#77750 = DIRECTION('ref_axis',(0.,7.02672800395669E-16,-1.)) ;
#77751 = DIRECTION('',(1.,-3.32023598379838E-46,4.72515227845561E-31)) ;
#77752 = DIRECTION('',(4.72515227845561E-31,7.02672800395669E-16,-1.)) ;
#77753 = DIRECTION('',(-1.,3.32023598379838E-46,-4.72515227845561E-31)) ;
#77754 = DIRECTION('',(-4.72515227845561E-31,-7.02672800395669E-16,1.)) ;
#77755 = DIRECTION('center_axis',(1.,-3.46944695195361E-16,2.28726627290214E-31)) ;
#77756 = DIRECTION('ref_axis',(3.46944695195361E-16,1.,1.5484195688691E-63)) ;
#77757 = DIRECTION('',(-3.46944695195361E-16,-1.,-7.02672800395669E-16)) ;
#77758 = DIRECTION('',(-4.72515227845561E-31,-7.02672800395669E-16,1.)) ;
#77759 = DIRECTION('',(3.46944695195361E-16,1.,7.02672800395669E-16)) ;
#77760 = DIRECTION('',(4.72515227845561E-31,7.02672800395669E-16,-1.)) ;
#77761 = DIRECTION('center_axis',(0.,1.,7.02672800395669E-16)) ;
#77762 = DIRECTION('ref_axis',(0.,-7.02672800395669E-16,1.)) ;
#77763 = DIRECTION('',(1.,-3.32023598379838E-46,4.72515227845561E-31)) ;
#77764 = DIRECTION('',(-4.72515227845561E-31,-7.02672800395669E-16,1.)) ;
#77765 = DIRECTION('',(-1.,3.32023598379838E-46,-4.72515227845561E-31)) ;
#77766 = DIRECTION('',(4.72515227845561E-31,7.02672800395669E-16,-1.)) ;
#77767 = DIRECTION('center_axis',(-1.,1.73472347597681E-16,-3.50620927567887E-31)) ;
#77768 = DIRECTION('ref_axis',(-1.73472347597681E-16,-1.,-1.0604312475688E-64)) ;
#77769 = DIRECTION('',(1.73472347597681E-16,1.,7.02672800395669E-16)) ;
#77770 = DIRECTION('',(-4.72515227845561E-31,-7.02672800395669E-16,1.)) ;
#77771 = DIRECTION('',(-1.73472347597681E-16,-1.,-7.02672800395669E-16)) ;
#77772 = DIRECTION('',(4.72515227845561E-31,7.02672800395669E-16,-1.)) ;
#77773 = DIRECTION('center_axis',(-1.,8.67361737988404E-17,-4.11568077706724E-31)) ;
#77774 = DIRECTION('ref_axis',(-8.67361737988404E-17,-1.,1.5859151899932E-63)) ;
#77775 = DIRECTION('',(8.67361737988404E-17,1.,7.02672800395669E-16)) ;
#77776 = DIRECTION('',(-4.72515227845561E-31,-7.02672800395669E-16,1.)) ;
#77777 = DIRECTION('',(-8.67361737988404E-17,-1.,-7.02672800395669E-16)) ;
#77778 = DIRECTION('',(4.72515227845561E-31,7.02672800395669E-16,-1.)) ;
#77779 = DIRECTION('center_axis',(0.,-1.,-7.02672800395669E-16)) ;
#77780 = DIRECTION('ref_axis',(0.,7.02672800395669E-16,-1.)) ;
#77781 = DIRECTION('',(-1.,3.32023598379838E-46,-4.72515227845561E-31)) ;
#77782 = DIRECTION('',(-4.72515227845561E-31,-7.02672800395669E-16,1.)) ;
#77783 = DIRECTION('',(1.,-3.32023598379838E-46,4.72515227845561E-31)) ;
#77784 = DIRECTION('',(4.72515227845561E-31,7.02672800395669E-16,-1.)) ;
#77785 = DIRECTION('center_axis',(1.,-1.73472347597681E-16,3.50620927567887E-31)) ;
#77786 = DIRECTION('ref_axis',(1.73472347597681E-16,1.,1.0604312475688E-64)) ;
#77787 = DIRECTION('',(-1.73472347597681E-16,-1.,-7.02672800395669E-16)) ;
#77788 = DIRECTION('',(-4.72515227845561E-31,-7.02672800395669E-16,1.)) ;
#77789 = DIRECTION('',(1.73472347597681E-16,1.,7.02672800395669E-16)) ;
#77790 = DIRECTION('',(4.72515227845561E-31,7.02672800395669E-16,-1.)) ;
#77791 = DIRECTION('center_axis',(0.,1.,7.02672800395669E-16)) ;
#77792 = DIRECTION('ref_axis',(0.,-7.02672800395669E-16,1.)) ;
#77793 = DIRECTION('',(-1.,3.32023598379838E-46,-4.72515227845561E-31)) ;
#77794 = DIRECTION('',(4.72515227845561E-31,7.02672800395669E-16,-1.)) ;
#77795 = DIRECTION('',(1.,-3.32023598379838E-46,4.72515227845561E-31)) ;
#77796 = DIRECTION('',(-4.72515227845561E-31,-7.02672800395669E-16,1.)) ;
#77797 = DIRECTION('center_axis',(6.7286639138916E-31,2.80136910081258E-45,
-1.)) ;
#77798 = DIRECTION('ref_axis',(-1.,1.16708558817391E-91,-6.7286639138916E-31)) ;
#77799 = DIRECTION('',(-1.,-3.65204942310907E-15,-6.7286639138916E-31)) ;
#77800 = DIRECTION('',(3.65204942310907E-15,-1.,-3.44027784310316E-46)) ;
#77801 = DIRECTION('',(1.,3.65204942310907E-15,6.7286639138916E-31)) ;
#77802 = DIRECTION('',(-3.65204942310907E-15,1.,3.44027784310316E-46)) ;
#77803 = DIRECTION('center_axis',(3.65204942310907E-15,-1.,0.)) ;
#77804 = DIRECTION('ref_axis',(1.,3.65204942310907E-15,0.)) ;
#77805 = DIRECTION('',(6.7286639138916E-31,2.45734131650226E-45,-1.)) ;
#77806 = DIRECTION('',(-1.,-3.65204942310907E-15,-6.7286639138916E-31)) ;
#77807 = DIRECTION('',(-6.7286639138916E-31,-2.45734131650226E-45,1.)) ;
#77808 = DIRECTION('',(1.,3.65204942310907E-15,6.7286639138916E-31)) ;
#77809 = DIRECTION('center_axis',(-6.7286639138916E-31,-2.80136910081258E-45,
1.)) ;
#77810 = DIRECTION('ref_axis',(1.,-1.16708558817391E-91,6.7286639138916E-31)) ;
#77811 = DIRECTION('',(-1.,-3.65204942310907E-15,-6.7286639138916E-31)) ;
#77812 = DIRECTION('',(-3.65204942310907E-15,1.,3.44027784310316E-46)) ;
#77813 = DIRECTION('',(1.,3.65204942310907E-15,6.7286639138916E-31)) ;
#77814 = DIRECTION('',(3.65204942310907E-15,-1.,-3.44027784310316E-46)) ;
#77815 = DIRECTION('center_axis',(-3.65204942310907E-15,1.,0.)) ;
#77816 = DIRECTION('ref_axis',(-1.,-3.65204942310907E-15,0.)) ;
#77817 = DIRECTION('',(6.7286639138916E-31,2.45734131650226E-45,-1.)) ;
#77818 = DIRECTION('',(1.,3.65204942310907E-15,6.7286639138916E-31)) ;
#77819 = DIRECTION('',(-6.7286639138916E-31,-2.45734131650226E-45,1.)) ;
#77820 = DIRECTION('',(-1.,-3.65204942310907E-15,-6.7286639138916E-31)) ;
#77821 = DIRECTION('center_axis',(3.49501116159781E-15,-1.,-7.02672800395669E-16)) ;
#77822 = DIRECTION('ref_axis',(1.,3.49501116159781E-15,-4.6242849322719E-44)) ;
#77823 = DIRECTION('center_axis',(0.,-1.,0.)) ;
#77824 = DIRECTION('ref_axis',(0.,0.,-1.)) ;
#77825 = DIRECTION('center_axis',(-2.42270293935615E-13,0.707106781186481,
0.707106781186614)) ;
#77826 = DIRECTION('ref_axis',(5.46329954747089E-13,-0.707106781186614,0.707106781186481)) ;
#77827 = DIRECTION('center_axis',(2.94996816089511E-31,-8.67361737988403E-16,
1.)) ;
#77828 = DIRECTION('ref_axis',(-2.55868951104443E-46,-1.,-8.67361737988403E-16)) ;
#77829 = DIRECTION('center_axis',(-1.88071505525119E-14,-0.707106781186579,
0.707106781186516)) ;
#77830 = DIRECTION('ref_axis',(-5.62922653036698E-12,-0.707106781186516,-0.707106781186579)) ;
#77831 = DIRECTION('center_axis',(0.,1.,0.)) ;
#77832 = DIRECTION('ref_axis',(1.,0.,0.)) ;
#77833 = DIRECTION('center_axis',(-1.,0.,0.)) ;
#77834 = DIRECTION('ref_axis',(0.,0.,-1.)) ;
#77835 = DIRECTION('center_axis',(0.,0.,1.)) ;
#77836 = DIRECTION('ref_axis',(-1.,0.,0.)) ;
#77837 = DIRECTION('center_axis',(-3.49501116159781E-15,1.,7.02672800395669E-16)) ;
#77838 = DIRECTION('ref_axis',(-1.,-3.49501116159781E-15,-2.45584928033405E-30)) ;
#77839 = DIRECTION('center_axis',(0.,-1.,0.)) ;
#77840 = DIRECTION('ref_axis',(0.,0.,-1.)) ;
#77841 = DIRECTION('center_axis',(-2.73644213932283E-30,1.14565880617704E-60,
1.)) ;
#77842 = DIRECTION('ref_axis',(1.,3.13502903450913E-90,2.73644213932283E-30)) ;
#77843 = DIRECTION('center_axis',(0.,0.,1.)) ;
#77844 = DIRECTION('ref_axis',(1.,0.,0.)) ;
#77845 = DIRECTION('center_axis',(-1.,4.18667286880966E-31,-4.7251522784556E-31)) ;
#77846 = DIRECTION('ref_axis',(-4.7251522784556E-31,1.97826668452042E-61,
1.)) ;
#77847 = DIRECTION('center_axis',(-1.,0.,0.)) ;
#77848 = DIRECTION('ref_axis',(0.,0.,1.)) ;
#77849 = DIRECTION('center_axis',(0.,1.,0.)) ;
#77850 = DIRECTION('ref_axis',(1.,0.,0.)) ;
#77851 = DIRECTION('center_axis',(-1.,0.,0.)) ;
#77852 = DIRECTION('ref_axis',(0.,0.,-1.)) ;
#77853 = DIRECTION('center_axis',(0.,1.,0.)) ;
#77854 = DIRECTION('ref_axis',(1.,0.,0.)) ;
#77855 = DIRECTION('center_axis',(0.,1.,0.)) ;
#77856 = DIRECTION('ref_axis',(0.,0.,-1.)) ;
#77857 = DIRECTION('center_axis',(0.,0.,1.)) ;
#77858 = DIRECTION('ref_axis',(-1.,0.,0.)) ;
#77859 = DIRECTION('center_axis',(1.,-4.18667286880966E-31,4.7251522784556E-31)) ;
#77860 = DIRECTION('ref_axis',(4.7251522784556E-31,-1.97826668452042E-61,
-1.)) ;
#77861 = DIRECTION('center_axis',(-1.,0.,-1.75279351218493E-14)) ;
#77862 = DIRECTION('ref_axis',(-1.75279351218493E-14,0.,1.)) ;
#77863 = DIRECTION('center_axis',(-8.21355058201474E-31,3.43874493783169E-61,
-1.)) ;
#77864 = DIRECTION('ref_axis',(-1.,-2.82443054855277E-91,8.21355058201474E-31)) ;
#77865 = DIRECTION('center_axis',(0.,0.,1.)) ;
#77866 = DIRECTION('ref_axis',(1.,0.,0.)) ;
#77867 = DIRECTION('center_axis',(-7.43707788821665E-32,1.,7.02672800395669E-16)) ;
#77868 = DIRECTION('ref_axis',(5.2258323464739E-47,-7.02672800395669E-16,
1.)) ;
#77869 = DIRECTION('center_axis',(0.,1.,0.)) ;
#77870 = DIRECTION('ref_axis',(0.,0.,1.)) ;
#77871 = DIRECTION('center_axis',(0.,1.,0.)) ;
#77872 = DIRECTION('ref_axis',(1.,0.,0.)) ;
#77873 = DIRECTION('center_axis',(0.,1.,0.)) ;
#77874 = DIRECTION('ref_axis',(0.,0.,-1.)) ;
#77875 = DIRECTION('center_axis',(4.72515227845561E-31,7.02672800395669E-16,
-1.)) ;
#77876 = DIRECTION('ref_axis',(0.,1.,0.)) ;
#77877 = DIRECTION('center_axis',(4.72515227845561E-31,7.02672800395669E-16,
-1.)) ;
#77878 = DIRECTION('ref_axis',(-3.32023598379838E-46,1.,7.02672800395669E-16)) ;
#77879 = DIRECTION('center_axis',(-1.,0.,0.)) ;
#77880 = DIRECTION('ref_axis',(0.,0.,-1.)) ;
#77881 = DIRECTION('center_axis',(7.43707788821665E-32,-1.,-7.02672800395669E-16)) ;
#77882 = DIRECTION('ref_axis',(8.2037222863304E-61,7.02672800395669E-16,-1.)) ;
#77883 = DIRECTION('center_axis',(0.,1.,0.)) ;
#77884 = DIRECTION('ref_axis',(0.,0.,1.)) ;
#77885 = DIRECTION('center_axis',(8.21355058201474E-31,-3.43874493783169E-61,
1.)) ;
#77886 = DIRECTION('ref_axis',(1.,2.82443054855277E-91,-8.21355058201474E-31)) ;
#77887 = DIRECTION('center_axis',(4.72515227845561E-31,7.02672800395669E-16,
-1.)) ;
#77888 = DIRECTION('ref_axis',(-3.32023598379838E-46,1.,7.02672800395669E-16)) ;
#77889 = DIRECTION('center_axis',(-1.,4.18667286880966E-31,-4.7251522784556E-31)) ;
#77890 = DIRECTION('ref_axis',(-4.7251522784556E-31,1.97826668452042E-61,
1.)) ;
#77891 = DIRECTION('center_axis',(-1.,0.,0.)) ;
#77892 = DIRECTION('ref_axis',(0.,0.,1.)) ;
#77893 = DIRECTION('center_axis',(4.72515227845561E-31,7.02672800395669E-16,
-1.)) ;
#77894 = DIRECTION('ref_axis',(0.,1.,0.)) ;
#77895 = DIRECTION('center_axis',(-1.,0.,0.)) ;
#77896 = DIRECTION('ref_axis',(0.,0.,-1.)) ;
#77897 = DIRECTION('center_axis',(0.,1.,0.)) ;
#77898 = DIRECTION('ref_axis',(1.,0.,0.)) ;
#77899 = DIRECTION('center_axis',(0.,1.,0.)) ;
#77900 = DIRECTION('ref_axis',(0.,0.,-1.)) ;
#77901 = DIRECTION('center_axis',(4.62592926927149E-14,0.,1.)) ;
#77902 = DIRECTION('ref_axis',(-1.,0.,4.62592926927149E-14)) ;
#77903 = DIRECTION('center_axis',(1.,-4.18667286880966E-31,4.7251522784556E-31)) ;
#77904 = DIRECTION('ref_axis',(4.7251522784556E-31,-1.97826668452042E-61,
-1.)) ;
#77905 = DIRECTION('center_axis',(-1.,0.,-1.01192202765316E-14)) ;
#77906 = DIRECTION('ref_axis',(-1.01192202765316E-14,0.,1.)) ;
#77907 = DIRECTION('center_axis',(-5.76147612141446E-31,2.41214157618207E-61,
-1.)) ;
#77908 = DIRECTION('ref_axis',(-1.,-1.3897496092644E-91,5.76147612141446E-31)) ;
#77909 = DIRECTION('center_axis',(0.,-4.62592926927149E-14,1.)) ;
#77910 = DIRECTION('ref_axis',(0.,-1.,-4.62592926927149E-14)) ;
#77911 = DIRECTION('center_axis',(-2.16840434497101E-16,1.,7.02672800395669E-16)) ;
#77912 = DIRECTION('ref_axis',(1.52367875347092E-31,-7.02672800395669E-16,
1.)) ;
#77913 = DIRECTION('center_axis',(0.,1.,0.)) ;
#77914 = DIRECTION('ref_axis',(0.,0.,1.)) ;
#77915 = DIRECTION('center_axis',(0.,1.,0.)) ;
#77916 = DIRECTION('ref_axis',(1.,0.,0.)) ;
#77917 = DIRECTION('center_axis',(0.,1.,0.)) ;
#77918 = DIRECTION('ref_axis',(0.,0.,-1.)) ;
#77919 = DIRECTION('center_axis',(0.,1.,0.)) ;
#77920 = DIRECTION('ref_axis',(1.,0.,0.)) ;
#77921 = DIRECTION('center_axis',(1.,0.,0.)) ;
#77922 = DIRECTION('ref_axis',(0.,0.,1.)) ;
#77923 = DIRECTION('center_axis',(0.,4.62592926927149E-14,1.)) ;
#77924 = DIRECTION('ref_axis',(0.,1.,-4.62592926927149E-14)) ;
#77925 = DIRECTION('center_axis',(2.16840434497101E-16,-1.,-7.02672800395669E-16)) ;
#77926 = DIRECTION('ref_axis',(3.47941294872983E-45,7.02672800395669E-16,
-1.)) ;
#77927 = DIRECTION('center_axis',(0.,1.,0.)) ;
#77928 = DIRECTION('ref_axis',(0.,0.,1.)) ;
#77929 = DIRECTION('center_axis',(-5.76147612141446E-31,2.41214157618207E-61,
-1.)) ;
#77930 = DIRECTION('ref_axis',(-1.,-1.3897496092644E-91,5.76147612141446E-31)) ;
#77931 = DIRECTION('center_axis',(0.,0.,1.)) ;
#77932 = DIRECTION('ref_axis',(1.,0.,0.)) ;
#77933 = DIRECTION('center_axis',(1.,-4.18667286880966E-31,4.7251522784556E-31)) ;
#77934 = DIRECTION('ref_axis',(4.7251522784556E-31,-1.97826668452042E-61,
-1.)) ;
#77935 = DIRECTION('center_axis',(1.,0.,0.)) ;
#77936 = DIRECTION('ref_axis',(0.,0.,-1.)) ;
#77937 = DIRECTION('center_axis',(-3.49247269410375E-15,1.,-1.72192198183147E-46)) ;
#77938 = DIRECTION('ref_axis',(-1.,-3.49247269410375E-15,6.01376550292341E-61)) ;
#77939 = DIRECTION('center_axis',(-2.16795153641756E-13,0.707106781186498,
-0.707106781186597)) ;
#77940 = DIRECTION('ref_axis',(8.90474808132134E-13,0.707106781186597,0.707106781186498)) ;
#77941 = DIRECTION('center_axis',(0.,-1.,0.)) ;
#77942 = DIRECTION('ref_axis',(0.,0.,-1.)) ;
#77943 = DIRECTION('center_axis',(0.,1.,0.)) ;
#77944 = DIRECTION('ref_axis',(1.,0.,0.)) ;
#77945 = DIRECTION('center_axis',(1.,-1.01192202765314E-14,0.)) ;
#77946 = DIRECTION('ref_axis',(-1.01192202765314E-14,-1.,0.)) ;
#77947 = DIRECTION('center_axis',(4.72515227845561E-31,7.02672800395669E-16,
-1.)) ;
#77948 = DIRECTION('ref_axis',(0.,1.,0.)) ;
#77949 = DIRECTION('center_axis',(4.72515227845561E-31,7.02672800395669E-16,
-1.)) ;
#77950 = DIRECTION('ref_axis',(-3.32023598379838E-46,1.,7.02672800395669E-16)) ;
#77951 = DIRECTION('center_axis',(0.,1.,0.)) ;
#77952 = DIRECTION('ref_axis',(0.,0.,-1.)) ;
#77953 = DIRECTION('center_axis',(0.,1.,0.)) ;
#77954 = DIRECTION('ref_axis',(1.,0.,0.)) ;
#77955 = DIRECTION('center_axis',(0.,0.,-1.)) ;
#77956 = DIRECTION('ref_axis',(1.,0.,0.)) ;
#77957 = DIRECTION('center_axis',(-1.,0.,0.)) ;
#77958 = DIRECTION('ref_axis',(0.,0.,-1.)) ;
#77959 = DIRECTION('center_axis',(1.08370143847609E-30,-2.89120579329467E-16,
-1.)) ;
#77960 = DIRECTION('ref_axis',(3.13320387712385E-46,1.,-2.89120579329467E-16)) ;
#77961 = DIRECTION('center_axis',(-5.66779128014443E-14,-0.707106781186571,
-0.707106781186524)) ;
#77962 = DIRECTION('ref_axis',(2.75100792174159E-12,0.707106781186524,-0.707106781186571)) ;
#77963 = DIRECTION('center_axis',(-1.,4.18667286880966E-31,-4.7251522784556E-31)) ;
#77964 = DIRECTION('ref_axis',(-4.7251522784556E-31,1.97826668452042E-61,
1.)) ;
#77965 = DIRECTION('center_axis',(1.,0.,0.)) ;
#77966 = DIRECTION('ref_axis',(0.,0.,-1.)) ;
#77967 = DIRECTION('center_axis',(8.21355058201474E-31,-3.43874493783169E-61,
1.)) ;
#77968 = DIRECTION('ref_axis',(1.,2.82443054855277E-91,-8.21355058201474E-31)) ;
#77969 = DIRECTION('center_axis',(4.72515227845561E-31,7.02672800395669E-16,
-1.)) ;
#77970 = DIRECTION('ref_axis',(-3.32023598379838E-46,1.,7.02672800395669E-16)) ;
#77971 = DIRECTION('center_axis',(-7.43707788821665E-32,1.,7.02672800395669E-16)) ;
#77972 = DIRECTION('ref_axis',(5.2258323464739E-47,-7.02672800395669E-16,
1.)) ;
#77973 = DIRECTION('center_axis',(4.91504984860095E-14,1.,0.)) ;
#77974 = DIRECTION('ref_axis',(-1.,4.91504984860095E-14,0.)) ;
#77975 = DIRECTION('center_axis',(-1.,4.27339674608665E-31,-4.93038065763132E-32)) ;
#77976 = DIRECTION('ref_axis',(-4.27339674608665E-31,-1.,-2.10694726592902E-62)) ;
#77977 = DIRECTION('center_axis',(-1.,0.,0.)) ;
#77978 = DIRECTION('ref_axis',(0.,0.,1.)) ;
#77979 = DIRECTION('center_axis',(7.39557098644695E-32,9.86076131526265E-32,
-1.)) ;
#77980 = DIRECTION('ref_axis',(-7.29259602874349E-63,1.,9.86076131526265E-32)) ;
#77981 = DIRECTION('center_axis',(0.,0.,-1.)) ;
#77982 = DIRECTION('ref_axis',(-1.,0.,0.)) ;
#77983 = DIRECTION('center_axis',(3.49247269410375E-15,-1.,1.72192198183147E-46)) ;
#77984 = DIRECTION('ref_axis',(1.,3.49247269410375E-15,-6.01376550292341E-61)) ;
#77985 = DIRECTION('center_axis',(0.,-1.,0.)) ;
#77986 = DIRECTION('ref_axis',(0.,0.,-1.)) ;
#77987 = DIRECTION('center_axis',(4.72515227845561E-31,7.02672800395669E-16,
-1.)) ;
#77988 = DIRECTION('ref_axis',(0.,1.,0.)) ;
#77989 = DIRECTION('center_axis',(0.,1.,0.)) ;
#77990 = DIRECTION('ref_axis',(0.,0.,-1.)) ;
#77991 = DIRECTION('center_axis',(-1.,5.06932053596301E-14,2.51253409742467E-28)) ;
#77992 = DIRECTION('ref_axis',(-5.06896112386E-14,-1.,0.)) ;
#77993 = DIRECTION('center_axis',(0.,0.,1.)) ;
#77994 = DIRECTION('ref_axis',(1.,0.,0.)) ;
#77995 = DIRECTION('center_axis',(0.,1.,0.)) ;
#77996 = DIRECTION('ref_axis',(1.,0.,0.)) ;
#77997 = DIRECTION('center_axis',(0.,0.,-1.)) ;
#77998 = DIRECTION('ref_axis',(1.,0.,0.)) ;
#77999 = DIRECTION('center_axis',(0.,1.,0.)) ;
#78000 = DIRECTION('ref_axis',(0.,0.,-1.)) ;
#78001 = DIRECTION('center_axis',(0.,1.,0.)) ;
#78002 = DIRECTION('ref_axis',(1.,0.,0.)) ;
#78003 = DIRECTION('center_axis',(-1.,0.,0.)) ;
#78004 = DIRECTION('ref_axis',(0.,0.,-1.)) ;
#78005 = DIRECTION('center_axis',(7.43707788821665E-32,-1.,-7.02672800395669E-16)) ;
#78006 = DIRECTION('ref_axis',(8.2037222863304E-61,7.02672800395669E-16,-1.)) ;
#78007 = DIRECTION('center_axis',(0.,1.,4.7704895589363E-14)) ;
#78008 = DIRECTION('ref_axis',(0.,-4.7704895589363E-14,1.)) ;
#78009 = DIRECTION('center_axis',(-6.04532600737121E-48,1.83697019872103E-16,
-1.)) ;
#78010 = DIRECTION('ref_axis',(1.11050837170941E-63,1.,1.83697019872103E-16)) ;
#78011 = DIRECTION('center_axis',(0.,0.,1.)) ;
#78012 = DIRECTION('ref_axis',(1.,0.,0.)) ;
#78013 = DIRECTION('center_axis',(-4.27339674608664E-31,1.,-2.10694726592902E-62)) ;
#78014 = DIRECTION('ref_axis',(-1.,-4.27339674608664E-31,9.00382159039722E-93)) ;
#78015 = DIRECTION('center_axis',(0.,1.,0.)) ;
#78016 = DIRECTION('ref_axis',(0.,0.,1.)) ;
#78017 = DIRECTION('center_axis',(-8.13512808509168E-31,-9.86076131526265E-32,
1.)) ;
#78018 = DIRECTION('ref_axis',(1.,-8.02185563161788E-62,8.13512808509168E-31)) ;
#78019 = DIRECTION('center_axis',(0.,0.,-1.)) ;
#78020 = DIRECTION('ref_axis',(-1.,0.,0.)) ;
#78021 = DIRECTION('center_axis',(1.,-4.27339674608665E-31,4.93038065763132E-32)) ;
#78022 = DIRECTION('ref_axis',(4.27339674608665E-31,1.,2.10694726592902E-62)) ;
#78023 = DIRECTION('center_axis',(-1.,-1.75279351218489E-14,0.)) ;
#78024 = DIRECTION('ref_axis',(1.75279351218489E-14,-1.,0.)) ;
#78025 = DIRECTION('center_axis',(-1.,5.06932053596301E-14,2.51253409742467E-28)) ;
#78026 = DIRECTION('ref_axis',(-5.06859511626947E-14,-1.,0.)) ;
#78027 = DIRECTION('center_axis',(0.,0.,1.)) ;
#78028 = DIRECTION('ref_axis',(1.,0.,0.)) ;
#78029 = DIRECTION('center_axis',(-4.15069017696469E-34,1.,1.83697019872103E-16)) ;
#78030 = DIRECTION('ref_axis',(0.,-1.85037170770859E-16,1.)) ;
#78031 = DIRECTION('center_axis',(-4.15069017696469E-34,1.,1.83697019872103E-16)) ;
#78032 = DIRECTION('ref_axis',(1.24381980576027E-51,-1.83697019872103E-16,
1.)) ;
#78033 = DIRECTION('center_axis',(-1.,0.,0.)) ;
#78034 = DIRECTION('ref_axis',(0.,-9.03501810404582E-16,-1.)) ;
#78035 = DIRECTION('center_axis',(-4.93038065763132E-32,0.,1.)) ;
#78036 = DIRECTION('ref_axis',(1.,0.,0.)) ;
#78037 = DIRECTION('center_axis',(-1.,0.,0.)) ;
#78038 = DIRECTION('ref_axis',(0.,0.,-1.)) ;
#78039 = DIRECTION('center_axis',(-4.93038065763132E-32,0.,1.)) ;
#78040 = DIRECTION('ref_axis',(1.,0.,4.93038065763132E-32)) ;
#78041 = DIRECTION('center_axis',(0.,1.,0.)) ;
#78042 = DIRECTION('ref_axis',(1.,0.,0.)) ;
#78043 = DIRECTION('center_axis',(0.,1.,0.)) ;
#78044 = DIRECTION('ref_axis',(-1.77086354839302E-14,0.,-1.)) ;
#78045 = DIRECTION('center_axis',(6.04532600737121E-48,-1.83697019872103E-16,
1.)) ;
#78046 = DIRECTION('ref_axis',(-1.11050837170941E-63,-1.,-1.83697019872103E-16)) ;
#78047 = DIRECTION('center_axis',(0.,0.,1.)) ;
#78048 = DIRECTION('ref_axis',(1.,0.,0.)) ;
#78049 = DIRECTION('center_axis',(3.29092219981587E-32,-1.,-1.83697019872103E-16)) ;
#78050 = DIRECTION('ref_axis',(-6.04532600737121E-48,1.83697019872103E-16,
-1.)) ;
#78051 = DIRECTION('center_axis',(-4.15069017696469E-34,1.,1.83697019872103E-16)) ;
#78052 = DIRECTION('ref_axis',(7.62469415920825E-50,-1.83697019872103E-16,
1.)) ;
#78053 = DIRECTION('center_axis',(-1.,-4.15069017696469E-34,-7.62469415920825E-50)) ;
#78054 = DIRECTION('ref_axis',(4.15069017696469E-34,-1.,3.16477431489857E-83)) ;
#78055 = DIRECTION('center_axis',(-1.,0.,-1.73472347597682E-14)) ;
#78056 = DIRECTION('ref_axis',(-1.73472347597682E-14,0.,1.)) ;
#78057 = DIRECTION('center_axis',(1.,-4.27339674608665E-31,4.93038065763132E-32)) ;
#78058 = DIRECTION('ref_axis',(4.27339674608665E-31,1.,2.10694726592902E-62)) ;
#78059 = DIRECTION('center_axis',(-1.,0.,-3.90312782094789E-14)) ;
#78060 = DIRECTION('ref_axis',(-3.90312782094789E-14,0.,1.)) ;
#78061 = DIRECTION('center_axis',(8.13512808509168E-31,9.86076131526265E-32,
-1.)) ;
#78062 = DIRECTION('ref_axis',(-1.,8.02185563161788E-62,-8.13512808509168E-31)) ;
#78063 = DIRECTION('center_axis',(-4.93038065763132E-32,0.,1.)) ;
#78064 = DIRECTION('ref_axis',(1.,0.,4.93038065763132E-32)) ;
#78065 = DIRECTION('center_axis',(4.27339674608664E-31,-1.,2.10694726592902E-62)) ;
#78066 = DIRECTION('ref_axis',(1.,4.27339674608664E-31,-9.00382159039724E-93)) ;
#78067 = DIRECTION('center_axis',(0.,1.,0.)) ;
#78068 = DIRECTION('ref_axis',(0.,0.,1.)) ;
#78069 = DIRECTION('center_axis',(-4.15069017696469E-34,1.,1.83697019872103E-16)) ;
#78070 = DIRECTION('ref_axis',(0.,0.,1.)) ;
#78071 = DIRECTION('center_axis',(-1.,0.,0.)) ;
#78072 = DIRECTION('ref_axis',(0.,0.,-1.)) ;
#78073 = DIRECTION('center_axis',(0.,1.,0.)) ;
#78074 = DIRECTION('ref_axis',(1.,0.,0.)) ;
#78075 = DIRECTION('center_axis',(0.,1.15648231731787E-14,1.)) ;
#78076 = DIRECTION('ref_axis',(-1.73472347597681E-14,1.,-1.15648231731787E-14)) ;
#78077 = DIRECTION('center_axis',(0.,-1.,-1.80700362080916E-16)) ;
#78078 = DIRECTION('ref_axis',(0.,-1.80700362080916E-16,1.)) ;
#78079 = DIRECTION('center_axis',(0.,1.,0.)) ;
#78080 = DIRECTION('ref_axis',(1.,0.,0.)) ;
#78081 = DIRECTION('center_axis',(0.,0.,-1.)) ;
#78082 = DIRECTION('ref_axis',(1.,0.,0.)) ;
#78083 = DIRECTION('center_axis',(-5.78241158658958E-15,1.,0.)) ;
#78084 = DIRECTION('ref_axis',(1.,5.78241158658958E-15,0.)) ;
#78085 = DIRECTION('center_axis',(-4.93038065763132E-32,0.,1.)) ;
#78086 = DIRECTION('ref_axis',(1.,0.,0.)) ;
#78087 = DIRECTION('center_axis',(-1.,0.,0.)) ;
#78088 = DIRECTION('ref_axis',(0.,0.,-1.)) ;
#78089 = DIRECTION('center_axis',(1.,4.15069017696469E-34,7.62469415920825E-50)) ;
#78090 = DIRECTION('ref_axis',(-4.15069017696469E-34,1.,-3.16477431489857E-83)) ;
#78091 = DIRECTION('center_axis',(-1.,0.,0.)) ;
#78092 = DIRECTION('ref_axis',(0.,0.,1.)) ;
#78093 = DIRECTION('center_axis',(-3.29092219981587E-32,1.,1.83697019872103E-16)) ;
#78094 = DIRECTION('ref_axis',(6.04532600737121E-48,-1.83697019872103E-16,
1.)) ;
#78095 = DIRECTION('center_axis',(0.,-1.,0.)) ;
#78096 = DIRECTION('ref_axis',(0.,0.,-1.)) ;
#78097 = DIRECTION('center_axis',(6.04532600737121E-48,-1.83697019872103E-16,
1.)) ;
#78098 = DIRECTION('ref_axis',(-1.11050837170941E-63,-1.,-1.83697019872103E-16)) ;
#78099 = DIRECTION('center_axis',(-1.15648231731789E-14,0.,1.)) ;
#78100 = DIRECTION('ref_axis',(1.,0.,1.15648231731789E-14)) ;
#78101 = DIRECTION('center_axis',(2.16840434497101E-16,-1.,1.06910588403688E-47)) ;
#78102 = DIRECTION('ref_axis',(1.,2.16840434497101E-16,-2.31825384417965E-63)) ;
#78103 = DIRECTION('center_axis',(0.,1.,5.78241158658946E-15)) ;
#78104 = DIRECTION('ref_axis',(0.,-5.78241158658946E-15,1.)) ;
#78105 = DIRECTION('center_axis',(-7.39557098644699E-31,-9.86076131526265E-32,
1.)) ;
#78106 = DIRECTION('ref_axis',(1.,-7.29259602874353E-62,7.39557098644699E-31)) ;
#78107 = DIRECTION('center_axis',(0.,0.,-1.)) ;
#78108 = DIRECTION('ref_axis',(-1.,0.,0.)) ;
#78109 = DIRECTION('center_axis',(-1.,4.27339674608665E-31,-4.93038065763132E-32)) ;
#78110 = DIRECTION('ref_axis',(-4.27339674608665E-31,-1.,-2.10694726592902E-62)) ;
#78111 = DIRECTION('center_axis',(-1.,0.,0.)) ;
#78112 = DIRECTION('ref_axis',(0.,0.,1.)) ;
#78113 = DIRECTION('center_axis',(0.,1.,0.)) ;
#78114 = DIRECTION('ref_axis',(1.,0.,0.)) ;
#78115 = DIRECTION('center_axis',(0.,0.,1.)) ;
#78116 = DIRECTION('ref_axis',(-1.,0.,0.)) ;
#78117 = DIRECTION('center_axis',(0.,1.,0.)) ;
#78118 = DIRECTION('ref_axis',(1.,0.,0.)) ;
#78119 = DIRECTION('center_axis',(1.,1.73472347597681E-14,3.13465160219275E-30)) ;
#78120 = DIRECTION('ref_axis',(1.73472347597681E-14,-1.,-6.13284536654788E-60)) ;
#78121 = DIRECTION('center_axis',(0.,-1.,-1.80700362080916E-16)) ;
#78122 = DIRECTION('ref_axis',(0.,-1.80700362080916E-16,1.)) ;
#78123 = DIRECTION('center_axis',(-1.,-3.29092219981587E-32,0.)) ;
#78124 = DIRECTION('ref_axis',(0.,-1.,0.)) ;
#78125 = DIRECTION('center_axis',(-5.34873071759516E-14,-1.,7.22801448323682E-15)) ;
#78126 = DIRECTION('ref_axis',(1.,-5.34873071759516E-14,2.24207754291971E-43)) ;
#78127 = DIRECTION('center_axis',(0.,0.,-1.)) ;
#78128 = DIRECTION('ref_axis',(-1.,0.,0.)) ;
#78129 = DIRECTION('center_axis',(0.,1.,0.)) ;
#78130 = DIRECTION('ref_axis',(1.,0.,0.)) ;
#78131 = DIRECTION('center_axis',(0.,0.,-1.)) ;
#78132 = DIRECTION('ref_axis',(1.,0.,0.)) ;
#78133 = DIRECTION('center_axis',(1.,-3.90312782094779E-14,0.)) ;
#78134 = DIRECTION('ref_axis',(-3.90312782094779E-14,-1.,0.)) ;
#78135 = DIRECTION('center_axis',(0.,1.,0.)) ;
#78136 = DIRECTION('ref_axis',(1.,0.,0.)) ;
#78137 = DIRECTION('center_axis',(0.,1.,0.)) ;
#78138 = DIRECTION('ref_axis',(0.,0.,-1.)) ;
#78139 = DIRECTION('center_axis',(-6.04532600737121E-48,1.83697019872103E-16,
-1.)) ;
#78140 = DIRECTION('ref_axis',(1.11050837170941E-63,1.,1.83697019872103E-16)) ;
#78141 = DIRECTION('center_axis',(0.,0.,1.)) ;
#78142 = DIRECTION('ref_axis',(1.,0.,0.)) ;
#78143 = DIRECTION('center_axis',(-3.29092219981587E-32,1.,1.83697019872103E-16)) ;
#78144 = DIRECTION('ref_axis',(6.04532600737121E-48,-1.83697019872103E-16,
1.)) ;
#78145 = DIRECTION('center_axis',(0.,-1.,0.)) ;
#78146 = DIRECTION('ref_axis',(0.,0.,-1.)) ;
#78147 = DIRECTION('center_axis',(1.,4.15069017696469E-34,7.62469415920825E-50)) ;
#78148 = DIRECTION('ref_axis',(-4.15069017696469E-34,1.,-3.16477431489857E-83)) ;
#78149 = DIRECTION('center_axis',(1.,0.,0.)) ;
#78150 = DIRECTION('ref_axis',(0.,0.,-1.)) ;
#78151 = DIRECTION('center_axis',(-6.04532600737121E-48,1.83697019872103E-16,
-1.)) ;
#78152 = DIRECTION('ref_axis',(1.11050837170941E-63,1.,1.83697019872103E-16)) ;
#78153 = DIRECTION('center_axis',(0.,0.,-1.)) ;
#78154 = DIRECTION('ref_axis',(-1.,0.,0.)) ;
#78155 = DIRECTION('center_axis',(-4.27339674608664E-31,1.,-2.10694726592902E-62)) ;
#78156 = DIRECTION('ref_axis',(-1.,-4.27339674608664E-31,9.00382159039722E-93)) ;
#78157 = DIRECTION('center_axis',(0.,-1.,0.)) ;
#78158 = DIRECTION('ref_axis',(0.,0.,-1.)) ;
#78159 = DIRECTION('center_axis',(-1.,4.27339674608665E-31,-4.93038065763132E-32)) ;
#78160 = DIRECTION('ref_axis',(-4.27339674608665E-31,-1.,-2.10694726592902E-62)) ;
#78161 = DIRECTION('center_axis',(1.,0.,0.)) ;
#78162 = DIRECTION('ref_axis',(0.,0.,-1.)) ;
#78163 = DIRECTION('center_axis',(-7.39557098644699E-31,-9.86076131526265E-32,
1.)) ;
#78164 = DIRECTION('ref_axis',(1.,-7.29259602874353E-62,7.39557098644699E-31)) ;
#78165 = DIRECTION('center_axis',(0.,0.,-1.)) ;
#78166 = DIRECTION('ref_axis',(-1.,0.,0.)) ;
#78167 = DIRECTION('center_axis',(-2.16840434497101E-16,1.,-1.06910588403688E-47)) ;
#78168 = DIRECTION('ref_axis',(-1.,-2.16840434497101E-16,2.31825384417965E-63)) ;
#78169 = DIRECTION('center_axis',(0.,1.,0.)) ;
#78170 = DIRECTION('ref_axis',(0.,0.,1.)) ;
#78171 = DIRECTION('center_axis',(0.,1.,0.)) ;
#78172 = DIRECTION('ref_axis',(1.,0.,0.)) ;
#78173 = DIRECTION('center_axis',(1.,0.,0.)) ;
#78174 = DIRECTION('ref_axis',(0.,0.,1.)) ;
#78175 = DIRECTION('center_axis',(-4.15069017696469E-34,1.,1.83697019872103E-16)) ;
#78176 = DIRECTION('ref_axis',(0.,-1.85037170770859E-16,1.)) ;
#78177 = DIRECTION('center_axis',(-4.15069017696469E-34,1.,1.83697019872103E-16)) ;
#78178 = DIRECTION('ref_axis',(1.24381980576027E-51,-1.83697019872103E-16,
1.)) ;
#78179 = DIRECTION('center_axis',(-4.93038065763132E-32,0.,1.)) ;
#78180 = DIRECTION('ref_axis',(1.,0.,0.)) ;
#78181 = DIRECTION('center_axis',(-4.93038065763132E-32,0.,1.)) ;
#78182 = DIRECTION('ref_axis',(1.,0.,4.93038065763132E-32)) ;
#78183 = DIRECTION('center_axis',(0.,1.,0.)) ;
#78184 = DIRECTION('ref_axis',(1.,0.,0.)) ;
#78185 = DIRECTION('center_axis',(1.,0.,0.)) ;
#78186 = DIRECTION('ref_axis',(0.,0.,1.)) ;
#78187 = DIRECTION('center_axis',(-1.,-4.15069017696469E-34,-7.62469415920825E-50)) ;
#78188 = DIRECTION('ref_axis',(4.15069017696469E-34,-1.,3.16477431489857E-83)) ;
#78189 = DIRECTION('center_axis',(1.,0.,0.)) ;
#78190 = DIRECTION('ref_axis',(0.,0.,-1.)) ;
#78191 = DIRECTION('center_axis',(3.29092219981587E-32,-1.,-1.83697019872103E-16)) ;
#78192 = DIRECTION('ref_axis',(-6.04532600737121E-48,1.83697019872103E-16,
-1.)) ;
#78193 = DIRECTION('center_axis',(-4.15069017696469E-34,1.,1.83697019872103E-16)) ;
#78194 = DIRECTION('ref_axis',(7.62469415920825E-50,-1.83697019872103E-16,
1.)) ;
#78195 = DIRECTION('center_axis',(8.13512808509168E-31,9.86076131526265E-32,
-1.)) ;
#78196 = DIRECTION('ref_axis',(-1.,8.02185563161788E-62,-8.13512808509168E-31)) ;
#78197 = DIRECTION('center_axis',(-4.93038065763132E-32,0.,1.)) ;
#78198 = DIRECTION('ref_axis',(1.,0.,4.93038065763132E-32)) ;
#78199 = DIRECTION('center_axis',(1.,-4.27339674608665E-31,4.93038065763132E-32)) ;
#78200 = DIRECTION('ref_axis',(4.27339674608665E-31,1.,2.10694726592902E-62)) ;
#78201 = DIRECTION('center_axis',(1.,0.,0.)) ;
#78202 = DIRECTION('ref_axis',(0.,0.,-1.)) ;
#78203 = DIRECTION('center_axis',(-4.15069017696469E-34,1.,1.83697019872103E-16)) ;
#78204 = DIRECTION('ref_axis',(0.,0.,1.)) ;
#78205 = DIRECTION('center_axis',(0.,0.,1.)) ;
#78206 = DIRECTION('ref_axis',(-1.,0.,0.)) ;
#78207 = DIRECTION('center_axis',(-4.93038065763132E-32,0.,1.)) ;
#78208 = DIRECTION('ref_axis',(1.,0.,0.)) ;
#78209 = DIRECTION('center_axis',(0.,1.,0.)) ;
#78210 = DIRECTION('ref_axis',(-1.77086354839302E-14,0.,-1.)) ;
#78211 = DIRECTION('center_axis',(6.04532600737121E-48,-1.83697019872103E-16,
1.)) ;
#78212 = DIRECTION('ref_axis',(-1.11050837170941E-63,-1.,-1.83697019872103E-16)) ;
#78213 = DIRECTION('center_axis',(0.,0.,1.)) ;
#78214 = DIRECTION('ref_axis',(1.,0.,0.)) ;
#78215 = DIRECTION('center_axis',(4.27339674608664E-31,-1.,2.10694726592902E-62)) ;
#78216 = DIRECTION('ref_axis',(1.,4.27339674608664E-31,-9.00382159039724E-93)) ;
#78217 = DIRECTION('center_axis',(4.48136897960683E-14,1.,0.)) ;
#78218 = DIRECTION('ref_axis',(-1.,4.48136897960683E-14,0.)) ;
#78219 = DIRECTION('center_axis',(-1.,-3.29092219981587E-32,0.)) ;
#78220 = DIRECTION('ref_axis',(0.,-1.,0.)) ;
#78221 = DIRECTION('center_axis',(-1.,3.32023598379838E-46,-4.72515227845561E-31)) ;
#78222 = DIRECTION('ref_axis',(-4.72515227845561E-31,1.56886206238552E-76,
1.)) ;
#78223 = DIRECTION('center_axis',(-1.,0.,0.)) ;
#78224 = DIRECTION('ref_axis',(0.,0.,1.)) ;
#78225 = DIRECTION('center_axis',(1.,0.,0.)) ;
#78226 = DIRECTION('ref_axis',(0.,0.,-1.)) ;
#78227 = DIRECTION('center_axis',(4.72515227845561E-31,7.02672800395669E-16,
-1.)) ;
#78228 = DIRECTION('ref_axis',(0.,1.,0.)) ;
#78229 = DIRECTION('center_axis',(4.72515227845561E-31,7.02672800395669E-16,
-1.)) ;
#78230 = DIRECTION('ref_axis',(-3.32023598379838E-46,1.,7.02672800395669E-16)) ;
#78231 = DIRECTION('center_axis',(0.,-1.,0.)) ;
#78232 = DIRECTION('ref_axis',(0.,0.,1.)) ;
#78233 = DIRECTION('center_axis',(4.72515227845561E-31,7.02672800395669E-16,
-1.)) ;
#78234 = DIRECTION('ref_axis',(0.,1.,0.)) ;
#78235 = DIRECTION('center_axis',(0.,-1.,0.)) ;
#78236 = DIRECTION('ref_axis',(0.,0.,1.)) ;
#78237 = DIRECTION('center_axis',(4.72515227845561E-31,7.02672800395669E-16,
-1.)) ;
#78238 = DIRECTION('ref_axis',(-3.32023598379838E-46,1.,7.02672800395669E-16)) ;
#78239 = DIRECTION('center_axis',(-4.72515227845561E-31,-7.02672800395669E-16,
1.)) ;
#78240 = DIRECTION('ref_axis',(3.32023598379838E-46,-1.,-7.02672800395669E-16)) ;
#78241 = DIRECTION('center_axis',(4.72515227845561E-31,7.02672800395669E-16,
-1.)) ;
#78242 = DIRECTION('ref_axis',(-3.32023598379838E-46,1.,7.02672800395669E-16)) ;
#78243 = DIRECTION('center_axis',(-8.67361737988404E-17,-1.,-7.02672800395669E-16)) ;
#78244 = DIRECTION('ref_axis',(6.09471501388366E-32,7.02672800395669E-16,
-1.)) ;
#78245 = DIRECTION('center_axis',(0.,-1.,0.)) ;
#78246 = DIRECTION('ref_axis',(0.,0.,-1.)) ;
#78247 = DIRECTION('center_axis',(1.,-3.32023598379838E-46,4.72515227845561E-31)) ;
#78248 = DIRECTION('ref_axis',(4.72515227845561E-31,-1.56886206238552E-76,
-1.)) ;
#78249 = DIRECTION('center_axis',(1.,0.,0.)) ;
#78250 = DIRECTION('ref_axis',(0.,0.,-1.)) ;
#78251 = DIRECTION('center_axis',(-1.,0.,0.)) ;
#78252 = DIRECTION('ref_axis',(0.,0.,1.)) ;
#78253 = DIRECTION('center_axis',(1.73472347597681E-16,1.,7.02672800395669E-16)) ;
#78254 = DIRECTION('ref_axis',(-1.21894300277673E-31,-7.02672800395669E-16,
1.)) ;
#78255 = DIRECTION('center_axis',(0.,-1.,0.)) ;
#78256 = DIRECTION('ref_axis',(0.,0.,-1.)) ;
#78257 = DIRECTION('center_axis',(-4.72515227845561E-31,-7.02672800395669E-16,
1.)) ;
#78258 = DIRECTION('ref_axis',(3.32023598379838E-46,-1.,-7.02672800395669E-16)) ;
#78259 = DIRECTION('center_axis',(4.72515227845561E-31,7.02672800395669E-16,
-1.)) ;
#78260 = DIRECTION('ref_axis',(-3.32023598379838E-46,1.,7.02672800395669E-16)) ;
#78261 = DIRECTION('center_axis',(-1.,3.32023598379838E-46,-4.72515227845561E-31)) ;
#78262 = DIRECTION('ref_axis',(-4.72515227845561E-31,1.56886206238552E-76,
1.)) ;
#78263 = DIRECTION('center_axis',(1.,0.,0.)) ;
#78264 = DIRECTION('ref_axis',(0.,0.,-1.)) ;
#78265 = DIRECTION('center_axis',(-1.,0.,0.)) ;
#78266 = DIRECTION('ref_axis',(0.,0.,1.)) ;
#78267 = DIRECTION('center_axis',(4.72515227845561E-31,7.02672800395669E-16,
-1.)) ;
#78268 = DIRECTION('ref_axis',(0.,1.,0.)) ;
#78269 = DIRECTION('center_axis',(0.,-1.,0.)) ;
#78270 = DIRECTION('ref_axis',(0.,0.,1.)) ;
#78271 = DIRECTION('center_axis',(4.72515227845561E-31,7.02672800395669E-16,
-1.)) ;
#78272 = DIRECTION('ref_axis',(0.,1.,0.)) ;
#78273 = DIRECTION('center_axis',(4.72515227845561E-31,7.02672800395669E-16,
-1.)) ;
#78274 = DIRECTION('ref_axis',(-3.32023598379837E-46,1.,7.02672800395669E-16)) ;
#78275 = DIRECTION('center_axis',(4.72515227845561E-31,7.02672800395669E-16,
-1.)) ;
#78276 = DIRECTION('ref_axis',(0.,1.,0.)) ;
#78277 = DIRECTION('center_axis',(4.72515227845561E-31,7.02672800395669E-16,
-1.)) ;
#78278 = DIRECTION('ref_axis',(-3.32023598379837E-46,1.,7.02672800395669E-16)) ;
#78279 = DIRECTION('center_axis',(4.72515227845561E-31,7.02672800395669E-16,
-1.)) ;
#78280 = DIRECTION('ref_axis',(0.,1.,0.)) ;
#78281 = DIRECTION('center_axis',(0.,-1.,0.)) ;
#78282 = DIRECTION('ref_axis',(0.,0.,1.)) ;
#78283 = DIRECTION('center_axis',(-8.67361737988404E-17,-1.,-7.02672800395669E-16)) ;
#78284 = DIRECTION('ref_axis',(6.09471501388366E-32,7.02672800395669E-16,
-1.)) ;
#78285 = DIRECTION('center_axis',(0.,-1.,0.)) ;
#78286 = DIRECTION('ref_axis',(0.,0.,-1.)) ;
#78287 = DIRECTION('center_axis',(-4.72515227845561E-31,-7.02672800395669E-16,
1.)) ;
#78288 = DIRECTION('ref_axis',(3.32023598379837E-46,-1.,-7.02672800395669E-16)) ;
#78289 = DIRECTION('center_axis',(4.72515227845561E-31,7.02672800395669E-16,
-1.)) ;
#78290 = DIRECTION('ref_axis',(-3.32023598379837E-46,1.,7.02672800395669E-16)) ;
#78291 = DIRECTION('center_axis',(-4.72515227845561E-31,-7.02672800395669E-16,
1.)) ;
#78292 = DIRECTION('ref_axis',(3.32023598379837E-46,-1.,-7.02672800395669E-16)) ;
#78293 = DIRECTION('center_axis',(4.72515227845561E-31,7.02672800395669E-16,
-1.)) ;
#78294 = DIRECTION('ref_axis',(-3.32023598379837E-46,1.,7.02672800395669E-16)) ;
#78295 = DIRECTION('center_axis',(1.73472347597681E-16,1.,7.02672800395669E-16)) ;
#78296 = DIRECTION('ref_axis',(-1.21894300277673E-31,-7.02672800395669E-16,
1.)) ;
#78297 = DIRECTION('center_axis',(0.,-1.,0.)) ;
#78298 = DIRECTION('ref_axis',(0.,0.,-1.)) ;
#78299 = DIRECTION('center_axis',(4.72515227845561E-31,7.02672800395669E-16,
-1.)) ;
#78300 = DIRECTION('ref_axis',(0.,1.,0.)) ;
#78301 = DIRECTION('center_axis',(1.,0.,0.)) ;
#78302 = DIRECTION('ref_axis',(0.,0.,1.)) ;
#78303 = DIRECTION('center_axis',(4.72515227845561E-31,7.02672800395669E-16,
-1.)) ;
#78304 = DIRECTION('ref_axis',(0.,1.,0.)) ;
#78305 = DIRECTION('center_axis',(-1.,0.,0.)) ;
#78306 = DIRECTION('ref_axis',(0.,0.,-1.)) ;
#78307 = DIRECTION('center_axis',(1.,-3.32023598379838E-46,4.72515227845561E-31)) ;
#78308 = DIRECTION('ref_axis',(4.72515227845561E-31,-1.56886206238552E-76,
-1.)) ;
#78309 = DIRECTION('center_axis',(1.,-3.32023598379838E-46,4.72515227845561E-31)) ;
#78310 = DIRECTION('ref_axis',(4.72515227845561E-31,-1.56886206238552E-76,
-1.)) ;
#78311 = DIRECTION('center_axis',(1.,0.,0.)) ;
#78312 = DIRECTION('ref_axis',(0.,0.,-1.)) ;
#78313 = DIRECTION('center_axis',(-1.,0.,0.)) ;
#78314 = DIRECTION('ref_axis',(0.,0.,1.)) ;
#78315 = DIRECTION('center_axis',(4.72515227845561E-31,7.02672800395669E-16,
-1.)) ;
#78316 = DIRECTION('ref_axis',(0.,1.,0.)) ;
#78317 = DIRECTION('center_axis',(4.72515227845561E-31,7.02672800395669E-16,
-1.)) ;
#78318 = DIRECTION('ref_axis',(-3.32023598379837E-46,1.,7.02672800395669E-16)) ;
#78319 = DIRECTION('center_axis',(0.,1.,0.)) ;
#78320 = DIRECTION('ref_axis',(0.,0.,-1.)) ;
#78321 = DIRECTION('center_axis',(4.72515227845561E-31,7.02672800395669E-16,
-1.)) ;
#78322 = DIRECTION('ref_axis',(0.,1.,0.)) ;
#78323 = DIRECTION('center_axis',(0.,1.,0.)) ;
#78324 = DIRECTION('ref_axis',(0.,0.,-1.)) ;
#78325 = DIRECTION('center_axis',(4.72515227845561E-31,7.02672800395669E-16,
-1.)) ;
#78326 = DIRECTION('ref_axis',(-3.32023598379837E-46,1.,7.02672800395669E-16)) ;
#78327 = DIRECTION('center_axis',(-4.72515227845561E-31,-7.02672800395669E-16,
1.)) ;
#78328 = DIRECTION('ref_axis',(3.32023598379837E-46,-1.,-7.02672800395669E-16)) ;
#78329 = DIRECTION('center_axis',(4.72515227845561E-31,7.02672800395669E-16,
-1.)) ;
#78330 = DIRECTION('ref_axis',(-3.32023598379837E-46,1.,7.02672800395669E-16)) ;
#78331 = DIRECTION('center_axis',(3.46944695195361E-16,1.,7.02672800395669E-16)) ;
#78332 = DIRECTION('ref_axis',(-2.43788600555346E-31,-7.02672800395669E-16,
1.)) ;
#78333 = DIRECTION('center_axis',(0.,1.,0.)) ;
#78334 = DIRECTION('ref_axis',(0.,0.,1.)) ;
#78335 = DIRECTION('center_axis',(-1.,3.32023598379838E-46,-4.72515227845561E-31)) ;
#78336 = DIRECTION('ref_axis',(-4.72515227845561E-31,1.56886206238552E-76,
1.)) ;
#78337 = DIRECTION('center_axis',(-1.,0.,0.)) ;
#78338 = DIRECTION('ref_axis',(0.,0.,1.)) ;
#78339 = DIRECTION('center_axis',(1.,0.,0.)) ;
#78340 = DIRECTION('ref_axis',(0.,0.,-1.)) ;
#78341 = DIRECTION('center_axis',(-1.73472347597681E-16,-1.,-7.02672800395669E-16)) ;
#78342 = DIRECTION('ref_axis',(1.21894300277673E-31,7.02672800395669E-16,
-1.)) ;
#78343 = DIRECTION('center_axis',(0.,1.,0.)) ;
#78344 = DIRECTION('ref_axis',(0.,0.,1.)) ;
#78345 = DIRECTION('center_axis',(-4.72515227845561E-31,-7.02672800395669E-16,
1.)) ;
#78346 = DIRECTION('ref_axis',(3.32023598379837E-46,-1.,-7.02672800395669E-16)) ;
#78347 = DIRECTION('center_axis',(4.72515227845561E-31,7.02672800395669E-16,
-1.)) ;
#78348 = DIRECTION('ref_axis',(-3.32023598379837E-46,1.,7.02672800395669E-16)) ;
#78349 = DIRECTION('center_axis',(1.,-3.32023598379838E-46,4.72515227845561E-31)) ;
#78350 = DIRECTION('ref_axis',(4.72515227845561E-31,-1.56886206238552E-76,
-1.)) ;
#78351 = DIRECTION('center_axis',(-1.,0.,0.)) ;
#78352 = DIRECTION('ref_axis',(0.,0.,1.)) ;
#78353 = DIRECTION('center_axis',(1.,0.,0.)) ;
#78354 = DIRECTION('ref_axis',(0.,0.,-1.)) ;
#78355 = DIRECTION('center_axis',(4.72515227845561E-31,7.02672800395669E-16,
-1.)) ;
#78356 = DIRECTION('ref_axis',(0.,1.,0.)) ;
#78357 = DIRECTION('center_axis',(0.,1.,0.)) ;
#78358 = DIRECTION('ref_axis',(0.,0.,-1.)) ;
#78359 = DIRECTION('center_axis',(4.72515227845561E-31,7.02672800395669E-16,
-1.)) ;
#78360 = DIRECTION('ref_axis',(0.,1.,0.)) ;
#78361 = DIRECTION('center_axis',(4.72515227845561E-31,7.02672800395669E-16,
-1.)) ;
#78362 = DIRECTION('ref_axis',(-3.32023598379838E-46,1.,7.02672800395669E-16)) ;
#78363 = DIRECTION('center_axis',(4.72515227845561E-31,7.02672800395669E-16,
-1.)) ;
#78364 = DIRECTION('ref_axis',(0.,1.,0.)) ;
#78365 = DIRECTION('center_axis',(4.72515227845561E-31,7.02672800395669E-16,
-1.)) ;
#78366 = DIRECTION('ref_axis',(-3.32023598379838E-46,1.,7.02672800395669E-16)) ;
#78367 = DIRECTION('center_axis',(4.72515227845561E-31,7.02672800395669E-16,
-1.)) ;
#78368 = DIRECTION('ref_axis',(0.,1.,0.)) ;
#78369 = DIRECTION('center_axis',(0.,1.,0.)) ;
#78370 = DIRECTION('ref_axis',(0.,0.,-1.)) ;
#78371 = DIRECTION('center_axis',(3.46944695195361E-16,1.,7.02672800395669E-16)) ;
#78372 = DIRECTION('ref_axis',(-2.43788600555346E-31,-7.02672800395669E-16,
1.)) ;
#78373 = DIRECTION('center_axis',(0.,1.,0.)) ;
#78374 = DIRECTION('ref_axis',(0.,0.,1.)) ;
#78375 = DIRECTION('center_axis',(-4.72515227845561E-31,-7.02672800395669E-16,
1.)) ;
#78376 = DIRECTION('ref_axis',(3.32023598379838E-46,-1.,-7.02672800395669E-16)) ;
#78377 = DIRECTION('center_axis',(4.72515227845561E-31,7.02672800395669E-16,
-1.)) ;
#78378 = DIRECTION('ref_axis',(-3.32023598379838E-46,1.,7.02672800395669E-16)) ;
#78379 = DIRECTION('center_axis',(-4.72515227845561E-31,-7.02672800395669E-16,
1.)) ;
#78380 = DIRECTION('ref_axis',(3.32023598379838E-46,-1.,-7.02672800395669E-16)) ;
#78381 = DIRECTION('center_axis',(4.72515227845561E-31,7.02672800395669E-16,
-1.)) ;
#78382 = DIRECTION('ref_axis',(-3.32023598379838E-46,1.,7.02672800395669E-16)) ;
#78383 = DIRECTION('center_axis',(-1.73472347597681E-16,-1.,-7.02672800395669E-16)) ;
#78384 = DIRECTION('ref_axis',(1.21894300277673E-31,7.02672800395669E-16,
-1.)) ;
#78385 = DIRECTION('center_axis',(0.,1.,0.)) ;
#78386 = DIRECTION('ref_axis',(0.,0.,1.)) ;
#78387 = DIRECTION('center_axis',(4.72515227845561E-31,7.02672800395669E-16,
-1.)) ;
#78388 = DIRECTION('ref_axis',(0.,1.,0.)) ;
#78389 = DIRECTION('center_axis',(-1.,0.,0.)) ;
#78390 = DIRECTION('ref_axis',(0.,0.,-1.)) ;
#78391 = DIRECTION('center_axis',(4.72515227845561E-31,7.02672800395669E-16,
-1.)) ;
#78392 = DIRECTION('ref_axis',(0.,1.,0.)) ;
#78393 = DIRECTION('center_axis',(1.,0.,0.)) ;
#78394 = DIRECTION('ref_axis',(0.,0.,1.)) ;
#78395 = DIRECTION('center_axis',(-1.,3.32023598379838E-46,-4.72515227845561E-31)) ;
#78396 = DIRECTION('ref_axis',(-4.72515227845561E-31,1.56886206238552E-76,
1.)) ;
#78397 = DIRECTION('center_axis',(-1.,3.32023598379838E-46,-4.72515227845561E-31)) ;
#78398 = DIRECTION('ref_axis',(-4.72515227845561E-31,1.56886206238552E-76,
1.)) ;
#78399 = DIRECTION('center_axis',(-1.,0.,0.)) ;
#78400 = DIRECTION('ref_axis',(0.,0.,1.)) ;
#78401 = DIRECTION('center_axis',(1.,0.,0.)) ;
#78402 = DIRECTION('ref_axis',(0.,0.,-1.)) ;
#78403 = DIRECTION('center_axis',(4.72515227845561E-31,7.02672800395669E-16,
-1.)) ;
#78404 = DIRECTION('ref_axis',(0.,1.,0.)) ;
#78405 = DIRECTION('center_axis',(4.72515227845561E-31,7.02672800395669E-16,
-1.)) ;
#78406 = DIRECTION('ref_axis',(-3.32023598379838E-46,1.,7.02672800395669E-16)) ;
#78407 = DIRECTION('center_axis',(0.,-1.,0.)) ;
#78408 = DIRECTION('ref_axis',(0.,0.,1.)) ;
#78409 = DIRECTION('center_axis',(4.72515227845561E-31,7.02672800395669E-16,
-1.)) ;
#78410 = DIRECTION('ref_axis',(0.,1.,0.)) ;
#78411 = DIRECTION('center_axis',(0.,-1.,0.)) ;
#78412 = DIRECTION('ref_axis',(0.,0.,1.)) ;
#78413 = DIRECTION('center_axis',(4.72515227845561E-31,7.02672800395669E-16,
-1.)) ;
#78414 = DIRECTION('ref_axis',(-3.32023598379838E-46,1.,7.02672800395669E-16)) ;
#78415 = DIRECTION('center_axis',(-4.72515227845561E-31,-7.02672800395669E-16,
1.)) ;
#78416 = DIRECTION('ref_axis',(3.32023598379838E-46,-1.,-7.02672800395669E-16)) ;
#78417 = DIRECTION('center_axis',(4.72515227845561E-31,7.02672800395669E-16,
-1.)) ;
#78418 = DIRECTION('ref_axis',(-3.32023598379838E-46,1.,7.02672800395669E-16)) ;
#78419 = DIRECTION('center_axis',(1.97633094273713E-47,-1.,-7.02672800395669E-16)) ;
#78420 = DIRECTION('ref_axis',(-1.38871399804171E-62,7.02672800395669E-16,
-1.)) ;
#78421 = DIRECTION('center_axis',(0.,-1.,0.)) ;
#78422 = DIRECTION('ref_axis',(0.,0.,-1.)) ;
#78423 = DIRECTION('center_axis',(1.,-3.32023598379838E-46,4.72515227845561E-31)) ;
#78424 = DIRECTION('ref_axis',(4.72515227845561E-31,-1.56886206238552E-76,
-1.)) ;
#78425 = DIRECTION('center_axis',(1.,0.,0.)) ;
#78426 = DIRECTION('ref_axis',(0.,0.,-1.)) ;
#78427 = DIRECTION('center_axis',(-1.,0.,0.)) ;
#78428 = DIRECTION('ref_axis',(0.,0.,1.)) ;
#78429 = DIRECTION('center_axis',(-1.97633094273713E-47,1.,7.02672800395669E-16)) ;
#78430 = DIRECTION('ref_axis',(1.38871399804171E-62,-7.02672800395669E-16,
1.)) ;
#78431 = DIRECTION('center_axis',(0.,-1.,0.)) ;
#78432 = DIRECTION('ref_axis',(0.,0.,-1.)) ;
#78433 = DIRECTION('center_axis',(-4.72515227845561E-31,-7.02672800395669E-16,
1.)) ;
#78434 = DIRECTION('ref_axis',(3.32023598379838E-46,-1.,-7.02672800395669E-16)) ;
#78435 = DIRECTION('center_axis',(4.72515227845561E-31,7.02672800395669E-16,
-1.)) ;
#78436 = DIRECTION('ref_axis',(-3.32023598379838E-46,1.,7.02672800395669E-16)) ;
#78437 = DIRECTION('center_axis',(-1.,3.32023598379838E-46,-4.72515227845561E-31)) ;
#78438 = DIRECTION('ref_axis',(-4.72515227845561E-31,1.56886206238552E-76,
1.)) ;
#78439 = DIRECTION('center_axis',(1.,0.,0.)) ;
#78440 = DIRECTION('ref_axis',(0.,0.,-1.)) ;
#78441 = DIRECTION('center_axis',(-1.,0.,0.)) ;
#78442 = DIRECTION('ref_axis',(0.,0.,1.)) ;
#78443 = DIRECTION('center_axis',(4.72515227845561E-31,7.02672800395669E-16,
-1.)) ;
#78444 = DIRECTION('ref_axis',(0.,1.,0.)) ;
#78445 = DIRECTION('center_axis',(0.,-1.,0.)) ;
#78446 = DIRECTION('ref_axis',(0.,0.,1.)) ;
#78447 = DIRECTION('center_axis',(4.72515227845561E-31,7.02672800395669E-16,
-1.)) ;
#78448 = DIRECTION('ref_axis',(0.,1.,0.)) ;
#78449 = DIRECTION('center_axis',(4.72515227845561E-31,7.02672800395669E-16,
-1.)) ;
#78450 = DIRECTION('ref_axis',(-3.32023598379837E-46,1.,7.02672800395669E-16)) ;
#78451 = DIRECTION('center_axis',(4.72515227845561E-31,7.02672800395669E-16,
-1.)) ;
#78452 = DIRECTION('ref_axis',(0.,1.,0.)) ;
#78453 = DIRECTION('center_axis',(4.72515227845561E-31,7.02672800395669E-16,
-1.)) ;
#78454 = DIRECTION('ref_axis',(-3.32023598379837E-46,1.,7.02672800395669E-16)) ;
#78455 = DIRECTION('center_axis',(4.72515227845561E-31,7.02672800395669E-16,
-1.)) ;
#78456 = DIRECTION('ref_axis',(0.,1.,0.)) ;
#78457 = DIRECTION('center_axis',(0.,-1.,0.)) ;
#78458 = DIRECTION('ref_axis',(0.,0.,1.)) ;
#78459 = DIRECTION('center_axis',(1.97633094273713E-47,-1.,-7.02672800395669E-16)) ;
#78460 = DIRECTION('ref_axis',(-1.38871399804171E-62,7.02672800395669E-16,
-1.)) ;
#78461 = DIRECTION('center_axis',(0.,-1.,0.)) ;
#78462 = DIRECTION('ref_axis',(0.,0.,-1.)) ;
#78463 = DIRECTION('center_axis',(-4.72515227845561E-31,-7.02672800395669E-16,
1.)) ;
#78464 = DIRECTION('ref_axis',(3.32023598379837E-46,-1.,-7.02672800395669E-16)) ;
#78465 = DIRECTION('center_axis',(4.72515227845561E-31,7.02672800395669E-16,
-1.)) ;
#78466 = DIRECTION('ref_axis',(-3.32023598379837E-46,1.,7.02672800395669E-16)) ;
#78467 = DIRECTION('center_axis',(-4.72515227845561E-31,-7.02672800395669E-16,
1.)) ;
#78468 = DIRECTION('ref_axis',(3.32023598379837E-46,-1.,-7.02672800395669E-16)) ;
#78469 = DIRECTION('center_axis',(4.72515227845561E-31,7.02672800395669E-16,
-1.)) ;
#78470 = DIRECTION('ref_axis',(-3.32023598379837E-46,1.,7.02672800395669E-16)) ;
#78471 = DIRECTION('center_axis',(-1.97633094273713E-47,1.,7.02672800395669E-16)) ;
#78472 = DIRECTION('ref_axis',(1.38871399804171E-62,-7.02672800395669E-16,
1.)) ;
#78473 = DIRECTION('center_axis',(0.,-1.,0.)) ;
#78474 = DIRECTION('ref_axis',(0.,0.,-1.)) ;
#78475 = DIRECTION('center_axis',(4.72515227845561E-31,7.02672800395669E-16,
-1.)) ;
#78476 = DIRECTION('ref_axis',(0.,1.,0.)) ;
#78477 = DIRECTION('center_axis',(1.,0.,0.)) ;
#78478 = DIRECTION('ref_axis',(0.,0.,1.)) ;
#78479 = DIRECTION('center_axis',(4.72515227845561E-31,7.02672800395669E-16,
-1.)) ;
#78480 = DIRECTION('ref_axis',(0.,1.,0.)) ;
#78481 = DIRECTION('center_axis',(-1.,0.,0.)) ;
#78482 = DIRECTION('ref_axis',(0.,0.,-1.)) ;
#78483 = DIRECTION('center_axis',(1.,-3.32023598379838E-46,4.72515227845561E-31)) ;
#78484 = DIRECTION('ref_axis',(4.72515227845561E-31,-1.56886206238552E-76,
-1.)) ;
#78485 = DIRECTION('center_axis',(1.,-3.32023598379838E-46,4.72515227845561E-31)) ;
#78486 = DIRECTION('ref_axis',(4.72515227845561E-31,-1.56886206238552E-76,
-1.)) ;
#78487 = DIRECTION('center_axis',(1.,0.,0.)) ;
#78488 = DIRECTION('ref_axis',(0.,0.,-1.)) ;
#78489 = DIRECTION('center_axis',(-1.,0.,0.)) ;
#78490 = DIRECTION('ref_axis',(0.,0.,1.)) ;
#78491 = DIRECTION('center_axis',(4.72515227845561E-31,7.02672800395669E-16,
-1.)) ;
#78492 = DIRECTION('ref_axis',(0.,1.,0.)) ;
#78493 = DIRECTION('center_axis',(4.72515227845561E-31,7.02672800395669E-16,
-1.)) ;
#78494 = DIRECTION('ref_axis',(-3.32023598379837E-46,1.,7.02672800395669E-16)) ;
#78495 = DIRECTION('center_axis',(0.,1.,0.)) ;
#78496 = DIRECTION('ref_axis',(0.,0.,-1.)) ;
#78497 = DIRECTION('center_axis',(4.72515227845561E-31,7.02672800395669E-16,
-1.)) ;
#78498 = DIRECTION('ref_axis',(0.,1.,0.)) ;
#78499 = DIRECTION('center_axis',(0.,1.,0.)) ;
#78500 = DIRECTION('ref_axis',(0.,0.,-1.)) ;
#78501 = DIRECTION('center_axis',(4.72515227845561E-31,7.02672800395669E-16,
-1.)) ;
#78502 = DIRECTION('ref_axis',(-3.32023598379837E-46,1.,7.02672800395669E-16)) ;
#78503 = DIRECTION('center_axis',(-4.72515227845561E-31,-7.02672800395669E-16,
1.)) ;
#78504 = DIRECTION('ref_axis',(3.32023598379837E-46,-1.,-7.02672800395669E-16)) ;
#78505 = DIRECTION('center_axis',(4.72515227845561E-31,7.02672800395669E-16,
-1.)) ;
#78506 = DIRECTION('ref_axis',(-3.32023598379837E-46,1.,7.02672800395669E-16)) ;
#78507 = DIRECTION('center_axis',(6.93889390390723E-16,1.,7.02672800395669E-16)) ;
#78508 = DIRECTION('ref_axis',(-4.87577201110693E-31,-7.02672800395669E-16,
1.)) ;
#78509 = DIRECTION('center_axis',(0.,1.,0.)) ;
#78510 = DIRECTION('ref_axis',(0.,0.,1.)) ;
#78511 = DIRECTION('center_axis',(-1.,3.32023598379838E-46,-4.72515227845561E-31)) ;
#78512 = DIRECTION('ref_axis',(-4.72515227845561E-31,1.56886206238552E-76,
1.)) ;
#78513 = DIRECTION('center_axis',(-1.,0.,0.)) ;
#78514 = DIRECTION('ref_axis',(0.,0.,1.)) ;
#78515 = DIRECTION('center_axis',(1.,0.,0.)) ;
#78516 = DIRECTION('ref_axis',(0.,0.,-1.)) ;
#78517 = DIRECTION('center_axis',(4.15029497974802E-48,-1.,-7.02672800395669E-16)) ;
#78518 = DIRECTION('ref_axis',(-2.91629939588763E-63,7.02672800395669E-16,
-1.)) ;
#78519 = DIRECTION('center_axis',(0.,1.,0.)) ;
#78520 = DIRECTION('ref_axis',(0.,0.,1.)) ;
#78521 = DIRECTION('center_axis',(-4.72515227845561E-31,-7.02672800395669E-16,
1.)) ;
#78522 = DIRECTION('ref_axis',(3.32023598379837E-46,-1.,-7.02672800395669E-16)) ;
#78523 = DIRECTION('center_axis',(4.72515227845561E-31,7.02672800395669E-16,
-1.)) ;
#78524 = DIRECTION('ref_axis',(-3.32023598379837E-46,1.,7.02672800395669E-16)) ;
#78525 = DIRECTION('center_axis',(1.,-3.32023598379838E-46,4.72515227845561E-31)) ;
#78526 = DIRECTION('ref_axis',(4.72515227845561E-31,-1.56886206238552E-76,
-1.)) ;
#78527 = DIRECTION('center_axis',(-1.,0.,0.)) ;
#78528 = DIRECTION('ref_axis',(0.,0.,1.)) ;
#78529 = DIRECTION('center_axis',(1.,0.,0.)) ;
#78530 = DIRECTION('ref_axis',(0.,0.,-1.)) ;
#78531 = DIRECTION('center_axis',(4.72515227845561E-31,7.02672800395669E-16,
-1.)) ;
#78532 = DIRECTION('ref_axis',(0.,1.,0.)) ;
#78533 = DIRECTION('center_axis',(0.,1.,0.)) ;
#78534 = DIRECTION('ref_axis',(0.,0.,-1.)) ;
#78535 = DIRECTION('center_axis',(4.72515227845561E-31,7.02672800395669E-16,
-1.)) ;
#78536 = DIRECTION('ref_axis',(0.,1.,0.)) ;
#78537 = DIRECTION('center_axis',(4.72515227845561E-31,7.02672800395669E-16,
-1.)) ;
#78538 = DIRECTION('ref_axis',(-3.32023598379838E-46,1.,7.02672800395669E-16)) ;
#78539 = DIRECTION('center_axis',(4.72515227845561E-31,7.02672800395669E-16,
-1.)) ;
#78540 = DIRECTION('ref_axis',(0.,1.,0.)) ;
#78541 = DIRECTION('center_axis',(4.72515227845561E-31,7.02672800395669E-16,
-1.)) ;
#78542 = DIRECTION('ref_axis',(-3.32023598379838E-46,1.,7.02672800395669E-16)) ;
#78543 = DIRECTION('center_axis',(4.72515227845561E-31,7.02672800395669E-16,
-1.)) ;
#78544 = DIRECTION('ref_axis',(0.,1.,0.)) ;
#78545 = DIRECTION('center_axis',(0.,1.,0.)) ;
#78546 = DIRECTION('ref_axis',(0.,0.,-1.)) ;
#78547 = DIRECTION('center_axis',(6.93889390390723E-16,1.,7.02672800395669E-16)) ;
#78548 = DIRECTION('ref_axis',(-4.87577201110693E-31,-7.02672800395669E-16,
1.)) ;
#78549 = DIRECTION('center_axis',(0.,1.,0.)) ;
#78550 = DIRECTION('ref_axis',(0.,0.,1.)) ;
#78551 = DIRECTION('center_axis',(-4.72515227845561E-31,-7.02672800395669E-16,
1.)) ;
#78552 = DIRECTION('ref_axis',(3.32023598379838E-46,-1.,-7.02672800395669E-16)) ;
#78553 = DIRECTION('center_axis',(4.72515227845561E-31,7.02672800395669E-16,
-1.)) ;
#78554 = DIRECTION('ref_axis',(-3.32023598379838E-46,1.,7.02672800395669E-16)) ;
#78555 = DIRECTION('center_axis',(-4.72515227845561E-31,-7.02672800395669E-16,
1.)) ;
#78556 = DIRECTION('ref_axis',(3.32023598379838E-46,-1.,-7.02672800395669E-16)) ;
#78557 = DIRECTION('center_axis',(4.72515227845561E-31,7.02672800395669E-16,
-1.)) ;
#78558 = DIRECTION('ref_axis',(-3.32023598379838E-46,1.,7.02672800395669E-16)) ;
#78559 = DIRECTION('center_axis',(4.15029497974802E-48,-1.,-7.02672800395669E-16)) ;
#78560 = DIRECTION('ref_axis',(-2.91629939588763E-63,7.02672800395669E-16,
-1.)) ;
#78561 = DIRECTION('center_axis',(0.,1.,0.)) ;
#78562 = DIRECTION('ref_axis',(0.,0.,1.)) ;
#78563 = DIRECTION('center_axis',(4.72515227845561E-31,7.02672800395669E-16,
-1.)) ;
#78564 = DIRECTION('ref_axis',(0.,1.,0.)) ;
#78565 = DIRECTION('center_axis',(-1.,0.,0.)) ;
#78566 = DIRECTION('ref_axis',(0.,0.,-1.)) ;
#78567 = DIRECTION('center_axis',(4.72515227845561E-31,7.02672800395669E-16,
-1.)) ;
#78568 = DIRECTION('ref_axis',(0.,1.,0.)) ;
#78569 = DIRECTION('center_axis',(1.,0.,0.)) ;
#78570 = DIRECTION('ref_axis',(0.,0.,1.)) ;
#78571 = DIRECTION('center_axis',(-1.,3.32023598379838E-46,-4.72515227845561E-31)) ;
#78572 = DIRECTION('ref_axis',(-4.72515227845561E-31,1.56886206238552E-76,
1.)) ;
#78573 = DIRECTION('center_axis',(6.7286639138916E-31,2.45734131650226E-45,
-1.)) ;
#78574 = DIRECTION('ref_axis',(-1.,1.65346238404636E-75,-6.7286639138916E-31)) ;
#78575 = DIRECTION('center_axis',(0.,0.,1.)) ;
#78576 = DIRECTION('ref_axis',(1.,0.,0.)) ;
#78577 = DIRECTION('center_axis',(0.,0.,-1.)) ;
#78578 = DIRECTION('ref_axis',(-1.,0.,0.)) ;
#78579 = DIRECTION('center_axis',(-1.,-3.65204942310907E-15,-6.7286639138916E-31)) ;
#78580 = DIRECTION('ref_axis',(0.,-1.,0.)) ;
#78581 = DIRECTION('center_axis',(0.,1.,0.)) ;
#78582 = DIRECTION('ref_axis',(0.,0.,-1.)) ;
#78583 = DIRECTION('center_axis',(1.,3.65204942310907E-15,6.7286639138916E-31)) ;
#78584 = DIRECTION('ref_axis',(3.65204942310907E-15,-1.,2.45734131650226E-45)) ;
#78585 = DIRECTION('center_axis',(-1.,-3.65204942310907E-15,-6.7286639138916E-31)) ;
#78586 = DIRECTION('ref_axis',(0.,-1.,0.)) ;
#78587 = DIRECTION('center_axis',(1.,3.65204942310907E-15,6.7286639138916E-31)) ;
#78588 = DIRECTION('ref_axis',(3.65204942310907E-15,-1.,2.45734131650226E-45)) ;
#78589 = DIRECTION('center_axis',(0.,1.,0.)) ;
#78590 = DIRECTION('ref_axis',(0.,0.,-1.)) ;
#78591 = DIRECTION('center_axis',(-3.65204942310907E-15,1.,3.44027784310316E-46)) ;
#78592 = DIRECTION('ref_axis',(-1.,-3.65204942310907E-15,7.32903774880691E-61)) ;
#78593 = DIRECTION('center_axis',(-5.78241158658946E-15,1.,0.)) ;
#78594 = DIRECTION('ref_axis',(-1.,-5.78241158658946E-15,0.)) ;
#78595 = DIRECTION('center_axis',(-1.,-3.65204942310907E-15,-6.7286639138916E-31)) ;
#78596 = DIRECTION('ref_axis',(3.65204942310907E-15,-1.,5.11946107604649E-46)) ;
#78597 = DIRECTION('center_axis',(1.,3.65204942310907E-15,6.7286639138916E-31)) ;
#78598 = DIRECTION('ref_axis',(3.65204942310907E-15,-1.,2.45734131650226E-45)) ;
#78599 = DIRECTION('center_axis',(-6.7286639138916E-31,-2.45734131650226E-45,
1.)) ;
#78600 = DIRECTION('ref_axis',(1.,6.11909198179539E-89,6.7286639138916E-31)) ;
#78601 = DIRECTION('center_axis',(0.,0.,1.)) ;
#78602 = DIRECTION('ref_axis',(1.,0.,0.)) ;
#78603 = DIRECTION('center_axis',(0.,0.,-1.)) ;
#78604 = DIRECTION('ref_axis',(-1.,0.,0.)) ;
#78605 = DIRECTION('center_axis',(-1.,-3.65204942310907E-15,-6.7286639138916E-31)) ;
#78606 = DIRECTION('ref_axis',(3.65204942310907E-15,-1.,5.11946107604649E-46)) ;
#78607 = DIRECTION('center_axis',(1.,3.65204942310907E-15,6.7286639138916E-31)) ;
#78608 = DIRECTION('ref_axis',(3.65204942310907E-15,-1.,2.45734131650226E-45)) ;
#78609 = DIRECTION('center_axis',(3.65204942310907E-15,-1.,-3.44027784310316E-46)) ;
#78610 = DIRECTION('ref_axis',(1.,3.65204942310907E-15,-7.32903774880691E-61)) ;
#78611 = DIRECTION('center_axis',(-5.78241158658946E-15,1.,0.)) ;
#78612 = DIRECTION('ref_axis',(-1.,-5.78241158658946E-15,0.)) ;
#78613 = DIRECTION('center_axis',(-6.7286639138916E-31,-2.45734131650226E-45,
1.)) ;
#78614 = DIRECTION('ref_axis',(1.,-1.65346238404636E-75,6.7286639138916E-31)) ;
#78615 = DIRECTION('center_axis',(0.,0.,-1.)) ;
#78616 = DIRECTION('ref_axis',(-1.,0.,0.)) ;
#78617 = DIRECTION('center_axis',(0.,0.,1.)) ;
#78618 = DIRECTION('ref_axis',(1.,0.,0.)) ;
#78619 = DIRECTION('center_axis',(-1.,-3.65204942310907E-15,-6.7286639138916E-31)) ;
#78620 = DIRECTION('ref_axis',(0.,-1.,0.)) ;
#78621 = DIRECTION('center_axis',(1.,3.65204942310907E-15,6.7286639138916E-31)) ;
#78622 = DIRECTION('ref_axis',(3.65204942310907E-15,-1.,2.45734131650226E-45)) ;
#78623 = DIRECTION('center_axis',(-1.,-3.65204942310907E-15,-6.7286639138916E-31)) ;
#78624 = DIRECTION('ref_axis',(0.,-1.,0.)) ;
#78625 = DIRECTION('center_axis',(0.,1.,0.)) ;
#78626 = DIRECTION('ref_axis',(0.,0.,-1.)) ;
#78627 = DIRECTION('center_axis',(-1.,-3.65204942310907E-15,-6.7286639138916E-31)) ;
#78628 = DIRECTION('ref_axis',(0.,-1.,0.)) ;
#78629 = DIRECTION('center_axis',(0.,1.,0.)) ;
#78630 = DIRECTION('ref_axis',(0.,0.,-1.)) ;
#78631 = DIRECTION('center_axis',(-1.,-3.65204942310907E-15,-6.7286639138916E-31)) ;
#78632 = DIRECTION('ref_axis',(0.,-1.,0.)) ;
#78633 = DIRECTION('center_axis',(1.,3.65204942310907E-15,6.7286639138916E-31)) ;
#78634 = DIRECTION('ref_axis',(3.65204942310907E-15,-1.,2.45734131650226E-45)) ;
#78635 = DIRECTION('center_axis',(-1.,-3.65204942310907E-15,-6.7286639138916E-31)) ;
#78636 = DIRECTION('ref_axis',(3.65204942310907E-15,-1.,5.11946107604637E-46)) ;
#78637 = DIRECTION('center_axis',(1.,3.65204942310907E-15,6.7286639138916E-31)) ;
#78638 = DIRECTION('ref_axis',(3.65204942310907E-15,-1.,2.45734131650226E-45)) ;
#78639 = DIRECTION('center_axis',(3.65204942310907E-15,-1.,-3.44027784310316E-46)) ;
#78640 = DIRECTION('ref_axis',(1.,3.65204942310907E-15,-1.10542957505209E-75)) ;
#78641 = DIRECTION('center_axis',(-5.78241158658946E-15,1.,2.67490270053792E-28)) ;
#78642 = DIRECTION('ref_axis',(-1.,-5.78241158658946E-15,3.1861838222649E-58)) ;
#78643 = DIRECTION('center_axis',(-3.65204942310907E-15,1.,3.44027784310316E-46)) ;
#78644 = DIRECTION('ref_axis',(-1.,-3.65204942310907E-15,1.10542957505209E-75)) ;
#78645 = DIRECTION('center_axis',(-5.78241158658946E-15,1.,0.)) ;
#78646 = DIRECTION('ref_axis',(-1.,-5.78241158658946E-15,0.)) ;
#78647 = DIRECTION('center_axis',(-1.,-3.65204942310907E-15,-6.7286639138916E-31)) ;
#78648 = DIRECTION('ref_axis',(3.65204942310907E-15,-1.,5.11946107604637E-46)) ;
#78649 = DIRECTION('center_axis',(1.,3.65204942310907E-15,6.7286639138916E-31)) ;
#78650 = DIRECTION('ref_axis',(3.65204942310907E-15,-1.,2.45734131650226E-45)) ;
#78651 = DIRECTION('center_axis',(-1.,-3.65204942310907E-15,-6.7286639138916E-31)) ;
#78652 = DIRECTION('ref_axis',(0.,-1.,0.)) ;
#78653 = DIRECTION('center_axis',(0.,0.,1.)) ;
#78654 = DIRECTION('ref_axis',(-1.,-5.78241158658946E-15,0.)) ;
#78655 = DIRECTION('center_axis',(-1.,-3.65204942310907E-15,-6.7286639138916E-31)) ;
#78656 = DIRECTION('ref_axis',(0.,-1.,0.)) ;
#78657 = DIRECTION('center_axis',(0.,0.,-1.)) ;
#78658 = DIRECTION('ref_axis',(1.,0.,0.)) ;
#78659 = DIRECTION('center_axis',(6.7286639138916E-31,2.45734131650226E-45,
-1.)) ;
#78660 = DIRECTION('ref_axis',(-1.,-6.11909198179539E-89,-6.7286639138916E-31)) ;
#78661 = DIRECTION('center_axis',(1.,0.,4.93038065763132E-32)) ;
#78662 = DIRECTION('ref_axis',(4.93038065763132E-32,0.,-1.)) ;
#78663 = DIRECTION('center_axis',(1.,0.,0.)) ;
#78664 = DIRECTION('ref_axis',(0.,0.,-1.)) ;
#78665 = DIRECTION('center_axis',(-1.,0.,0.)) ;
#78666 = DIRECTION('ref_axis',(0.,0.,1.)) ;
#78667 = DIRECTION('center_axis',(-4.93038065763132E-32,0.,1.)) ;
#78668 = DIRECTION('ref_axis',(1.,0.,0.)) ;
#78669 = DIRECTION('center_axis',(-4.93038065763132E-32,0.,1.)) ;
#78670 = DIRECTION('ref_axis',(1.,0.,4.93038065763132E-32)) ;
#78671 = DIRECTION('center_axis',(0.,-1.,0.)) ;
#78672 = DIRECTION('ref_axis',(0.,0.,1.)) ;
#78673 = DIRECTION('center_axis',(-4.93038065763132E-32,0.,1.)) ;
#78674 = DIRECTION('ref_axis',(1.,0.,0.)) ;
#78675 = DIRECTION('center_axis',(0.,-1.,0.)) ;
#78676 = DIRECTION('ref_axis',(0.,0.,1.)) ;
#78677 = DIRECTION('center_axis',(-4.93038065763132E-32,0.,1.)) ;
#78678 = DIRECTION('ref_axis',(1.,0.,4.93038065763132E-32)) ;
#78679 = DIRECTION('center_axis',(0.,0.,-1.)) ;
#78680 = DIRECTION('ref_axis',(-1.,0.,0.)) ;
#78681 = DIRECTION('center_axis',(-4.93038065763132E-32,0.,1.)) ;
#78682 = DIRECTION('ref_axis',(1.,0.,4.93038065763132E-32)) ;
#78683 = DIRECTION('center_axis',(0.,-1.,0.)) ;
#78684 = DIRECTION('ref_axis',(0.,0.,-1.)) ;
#78685 = DIRECTION('center_axis',(0.,-1.,0.)) ;
#78686 = DIRECTION('ref_axis',(0.,0.,-1.)) ;
#78687 = DIRECTION('center_axis',(-1.,0.,-4.93038065763132E-32)) ;
#78688 = DIRECTION('ref_axis',(-4.93038065763132E-32,0.,1.)) ;
#78689 = DIRECTION('center_axis',(-1.,0.,0.)) ;
#78690 = DIRECTION('ref_axis',(0.,0.,1.)) ;
#78691 = DIRECTION('center_axis',(1.,0.,0.)) ;
#78692 = DIRECTION('ref_axis',(0.,0.,-1.)) ;
#78693 = DIRECTION('center_axis',(0.,1.,0.)) ;
#78694 = DIRECTION('ref_axis',(0.,0.,1.)) ;
#78695 = DIRECTION('center_axis',(0.,-1.,0.)) ;
#78696 = DIRECTION('ref_axis',(0.,0.,-1.)) ;
#78697 = DIRECTION('center_axis',(0.,0.,-1.)) ;
#78698 = DIRECTION('ref_axis',(-1.,0.,0.)) ;
#78699 = DIRECTION('center_axis',(-4.93038065763132E-32,0.,1.)) ;
#78700 = DIRECTION('ref_axis',(1.,0.,4.93038065763132E-32)) ;
#78701 = DIRECTION('center_axis',(1.,0.,4.93038065763132E-32)) ;
#78702 = DIRECTION('ref_axis',(4.93038065763132E-32,0.,-1.)) ;
#78703 = DIRECTION('center_axis',(-1.,0.,0.)) ;
#78704 = DIRECTION('ref_axis',(0.,0.,1.)) ;
#78705 = DIRECTION('center_axis',(1.,0.,0.)) ;
#78706 = DIRECTION('ref_axis',(0.,0.,-1.)) ;
#78707 = DIRECTION('center_axis',(-4.93038065763132E-32,0.,1.)) ;
#78708 = DIRECTION('ref_axis',(1.,0.,0.)) ;
#78709 = DIRECTION('center_axis',(0.,-1.,0.)) ;
#78710 = DIRECTION('ref_axis',(0.,0.,1.)) ;
#78711 = DIRECTION('center_axis',(-4.93038065763132E-32,0.,1.)) ;
#78712 = DIRECTION('ref_axis',(1.,0.,0.)) ;
#78713 = DIRECTION('center_axis',(-4.93038065763132E-32,0.,1.)) ;
#78714 = DIRECTION('ref_axis',(1.,0.,4.93038065763132E-32)) ;
#78715 = DIRECTION('center_axis',(-4.93038065763132E-32,0.,1.)) ;
#78716 = DIRECTION('ref_axis',(1.,0.,0.)) ;
#78717 = DIRECTION('center_axis',(-4.93038065763132E-32,0.,1.)) ;
#78718 = DIRECTION('ref_axis',(1.,0.,4.93038065763132E-32)) ;
#78719 = DIRECTION('center_axis',(-4.93038065763132E-32,0.,1.)) ;
#78720 = DIRECTION('ref_axis',(1.,0.,0.)) ;
#78721 = DIRECTION('center_axis',(0.,-1.,0.)) ;
#78722 = DIRECTION('ref_axis',(0.,0.,1.)) ;
#78723 = DIRECTION('center_axis',(0.,-1.,0.)) ;
#78724 = DIRECTION('ref_axis',(0.,0.,-1.)) ;
#78725 = DIRECTION('center_axis',(0.,-1.,0.)) ;
#78726 = DIRECTION('ref_axis',(0.,0.,-1.)) ;
#78727 = DIRECTION('center_axis',(0.,0.,-1.)) ;
#78728 = DIRECTION('ref_axis',(-1.,0.,0.)) ;
#78729 = DIRECTION('center_axis',(-4.93038065763132E-32,0.,1.)) ;
#78730 = DIRECTION('ref_axis',(1.,0.,4.93038065763132E-32)) ;
#78731 = DIRECTION('center_axis',(0.,0.,-1.)) ;
#78732 = DIRECTION('ref_axis',(-1.,0.,0.)) ;
#78733 = DIRECTION('center_axis',(-4.93038065763132E-32,0.,1.)) ;
#78734 = DIRECTION('ref_axis',(1.,0.,4.93038065763132E-32)) ;
#78735 = DIRECTION('center_axis',(0.,1.,0.)) ;
#78736 = DIRECTION('ref_axis',(0.,0.,1.)) ;
#78737 = DIRECTION('center_axis',(0.,-1.,0.)) ;
#78738 = DIRECTION('ref_axis',(0.,0.,-1.)) ;
#78739 = DIRECTION('center_axis',(-4.93038065763132E-32,0.,1.)) ;
#78740 = DIRECTION('ref_axis',(1.,0.,0.)) ;
#78741 = DIRECTION('center_axis',(-1.,0.,0.)) ;
#78742 = DIRECTION('ref_axis',(0.,0.,-1.)) ;
#78743 = DIRECTION('center_axis',(-4.93038065763132E-32,0.,1.)) ;
#78744 = DIRECTION('ref_axis',(1.,0.,0.)) ;
#78745 = DIRECTION('center_axis',(1.,0.,0.)) ;
#78746 = DIRECTION('ref_axis',(0.,0.,1.)) ;
#78747 = DIRECTION('center_axis',(-1.,0.,-4.93038065763132E-32)) ;
#78748 = DIRECTION('ref_axis',(-4.93038065763132E-32,0.,1.)) ;
#78749 = DIRECTION('center_axis',(1.,0.,4.93038065763132E-32)) ;
#78750 = DIRECTION('ref_axis',(4.93038065763132E-32,0.,-1.)) ;
#78751 = DIRECTION('center_axis',(1.,0.,0.)) ;
#78752 = DIRECTION('ref_axis',(0.,0.,-1.)) ;
#78753 = DIRECTION('center_axis',(-1.,0.,0.)) ;
#78754 = DIRECTION('ref_axis',(0.,0.,1.)) ;
#78755 = DIRECTION('center_axis',(-4.93038065763132E-32,0.,1.)) ;
#78756 = DIRECTION('ref_axis',(1.,0.,0.)) ;
#78757 = DIRECTION('center_axis',(-4.93038065763132E-32,0.,1.)) ;
#78758 = DIRECTION('ref_axis',(1.,0.,4.93038065763132E-32)) ;
#78759 = DIRECTION('center_axis',(0.,-1.,0.)) ;
#78760 = DIRECTION('ref_axis',(0.,0.,1.)) ;
#78761 = DIRECTION('center_axis',(-4.93038065763132E-32,0.,1.)) ;
#78762 = DIRECTION('ref_axis',(1.,0.,0.)) ;
#78763 = DIRECTION('center_axis',(0.,-1.,0.)) ;
#78764 = DIRECTION('ref_axis',(0.,0.,1.)) ;
#78765 = DIRECTION('center_axis',(-4.93038065763132E-32,0.,1.)) ;
#78766 = DIRECTION('ref_axis',(1.,0.,4.93038065763132E-32)) ;
#78767 = DIRECTION('center_axis',(0.,0.,-1.)) ;
#78768 = DIRECTION('ref_axis',(-1.,0.,0.)) ;
#78769 = DIRECTION('center_axis',(-4.93038065763132E-32,0.,1.)) ;
#78770 = DIRECTION('ref_axis',(1.,0.,4.93038065763132E-32)) ;
#78771 = DIRECTION('center_axis',(0.,-1.,0.)) ;
#78772 = DIRECTION('ref_axis',(0.,0.,-1.)) ;
#78773 = DIRECTION('center_axis',(0.,-1.,0.)) ;
#78774 = DIRECTION('ref_axis',(0.,0.,-1.)) ;
#78775 = DIRECTION('center_axis',(-1.,0.,-4.93038065763132E-32)) ;
#78776 = DIRECTION('ref_axis',(-4.93038065763132E-32,0.,1.)) ;
#78777 = DIRECTION('center_axis',(-1.,0.,0.)) ;
#78778 = DIRECTION('ref_axis',(0.,0.,1.)) ;
#78779 = DIRECTION('center_axis',(1.,0.,0.)) ;
#78780 = DIRECTION('ref_axis',(0.,0.,-1.)) ;
#78781 = DIRECTION('center_axis',(0.,1.,0.)) ;
#78782 = DIRECTION('ref_axis',(0.,0.,1.)) ;
#78783 = DIRECTION('center_axis',(0.,-1.,0.)) ;
#78784 = DIRECTION('ref_axis',(0.,0.,-1.)) ;
#78785 = DIRECTION('center_axis',(0.,0.,-1.)) ;
#78786 = DIRECTION('ref_axis',(-1.,0.,0.)) ;
#78787 = DIRECTION('center_axis',(-4.93038065763132E-32,0.,1.)) ;
#78788 = DIRECTION('ref_axis',(1.,0.,4.93038065763132E-32)) ;
#78789 = DIRECTION('center_axis',(1.,0.,4.93038065763132E-32)) ;
#78790 = DIRECTION('ref_axis',(4.93038065763132E-32,0.,-1.)) ;
#78791 = DIRECTION('center_axis',(-1.,0.,0.)) ;
#78792 = DIRECTION('ref_axis',(0.,0.,1.)) ;
#78793 = DIRECTION('center_axis',(1.,0.,0.)) ;
#78794 = DIRECTION('ref_axis',(0.,0.,-1.)) ;
#78795 = DIRECTION('center_axis',(-4.93038065763132E-32,0.,1.)) ;
#78796 = DIRECTION('ref_axis',(1.,0.,0.)) ;
#78797 = DIRECTION('center_axis',(0.,-1.,0.)) ;
#78798 = DIRECTION('ref_axis',(0.,0.,1.)) ;
#78799 = DIRECTION('center_axis',(-4.93038065763132E-32,0.,1.)) ;
#78800 = DIRECTION('ref_axis',(1.,0.,0.)) ;
#78801 = DIRECTION('center_axis',(-4.93038065763132E-32,0.,1.)) ;
#78802 = DIRECTION('ref_axis',(1.,0.,4.93038065763132E-32)) ;
#78803 = DIRECTION('center_axis',(-4.93038065763132E-32,0.,1.)) ;
#78804 = DIRECTION('ref_axis',(1.,0.,0.)) ;
#78805 = DIRECTION('center_axis',(-4.93038065763132E-32,0.,1.)) ;
#78806 = DIRECTION('ref_axis',(1.,0.,4.93038065763132E-32)) ;
#78807 = DIRECTION('center_axis',(-4.93038065763132E-32,0.,1.)) ;
#78808 = DIRECTION('ref_axis',(1.,0.,0.)) ;
#78809 = DIRECTION('center_axis',(0.,-1.,0.)) ;
#78810 = DIRECTION('ref_axis',(0.,0.,1.)) ;
#78811 = DIRECTION('center_axis',(0.,-1.,0.)) ;
#78812 = DIRECTION('ref_axis',(0.,0.,-1.)) ;
#78813 = DIRECTION('center_axis',(0.,-1.,0.)) ;
#78814 = DIRECTION('ref_axis',(0.,0.,-1.)) ;
#78815 = DIRECTION('center_axis',(0.,0.,-1.)) ;
#78816 = DIRECTION('ref_axis',(-1.,0.,0.)) ;
#78817 = DIRECTION('center_axis',(-4.93038065763132E-32,0.,1.)) ;
#78818 = DIRECTION('ref_axis',(1.,0.,4.93038065763132E-32)) ;
#78819 = DIRECTION('center_axis',(0.,0.,-1.)) ;
#78820 = DIRECTION('ref_axis',(-1.,0.,0.)) ;
#78821 = DIRECTION('center_axis',(-4.93038065763132E-32,0.,1.)) ;
#78822 = DIRECTION('ref_axis',(1.,0.,4.93038065763132E-32)) ;
#78823 = DIRECTION('center_axis',(0.,1.,0.)) ;
#78824 = DIRECTION('ref_axis',(0.,0.,1.)) ;
#78825 = DIRECTION('center_axis',(0.,-1.,0.)) ;
#78826 = DIRECTION('ref_axis',(0.,0.,-1.)) ;
#78827 = DIRECTION('center_axis',(-4.93038065763132E-32,0.,1.)) ;
#78828 = DIRECTION('ref_axis',(1.,0.,0.)) ;
#78829 = DIRECTION('center_axis',(-1.,0.,0.)) ;
#78830 = DIRECTION('ref_axis',(0.,0.,-1.)) ;
#78831 = DIRECTION('center_axis',(-4.93038065763132E-32,0.,1.)) ;
#78832 = DIRECTION('ref_axis',(1.,0.,0.)) ;
#78833 = DIRECTION('center_axis',(1.,0.,0.)) ;
#78834 = DIRECTION('ref_axis',(0.,0.,1.)) ;
#78835 = DIRECTION('center_axis',(-1.,0.,-4.93038065763132E-32)) ;
#78836 = DIRECTION('ref_axis',(-4.93038065763132E-32,0.,1.)) ;
#78837 = DIRECTION('center_axis',(1.,0.,4.93038065763132E-32)) ;
#78838 = DIRECTION('ref_axis',(4.93038065763132E-32,0.,-1.)) ;
#78839 = DIRECTION('center_axis',(1.,0.,0.)) ;
#78840 = DIRECTION('ref_axis',(0.,0.,-1.)) ;
#78841 = DIRECTION('center_axis',(-1.,0.,0.)) ;
#78842 = DIRECTION('ref_axis',(0.,0.,1.)) ;
#78843 = DIRECTION('center_axis',(-4.93038065763132E-32,0.,1.)) ;
#78844 = DIRECTION('ref_axis',(1.,0.,0.)) ;
#78845 = DIRECTION('center_axis',(-4.93038065763132E-32,0.,1.)) ;
#78846 = DIRECTION('ref_axis',(1.,0.,4.93038065763132E-32)) ;
#78847 = DIRECTION('center_axis',(0.,-1.,0.)) ;
#78848 = DIRECTION('ref_axis',(0.,0.,1.)) ;
#78849 = DIRECTION('center_axis',(-4.93038065763132E-32,0.,1.)) ;
#78850 = DIRECTION('ref_axis',(1.,0.,0.)) ;
#78851 = DIRECTION('center_axis',(0.,-1.,0.)) ;
#78852 = DIRECTION('ref_axis',(0.,0.,1.)) ;
#78853 = DIRECTION('center_axis',(-4.93038065763132E-32,0.,1.)) ;
#78854 = DIRECTION('ref_axis',(1.,0.,4.93038065763132E-32)) ;
#78855 = DIRECTION('center_axis',(0.,0.,-1.)) ;
#78856 = DIRECTION('ref_axis',(-1.,0.,0.)) ;
#78857 = DIRECTION('center_axis',(-4.93038065763132E-32,0.,1.)) ;
#78858 = DIRECTION('ref_axis',(1.,0.,4.93038065763132E-32)) ;
#78859 = DIRECTION('center_axis',(6.93889390390723E-16,-1.,3.42113882891801E-47)) ;
#78860 = DIRECTION('ref_axis',(1.,6.93889390390723E-16,-2.37389193643995E-62)) ;
#78861 = DIRECTION('center_axis',(0.,-1.,0.)) ;
#78862 = DIRECTION('ref_axis',(0.,0.,-1.)) ;
#78863 = DIRECTION('center_axis',(-1.,0.,-4.93038065763132E-32)) ;
#78864 = DIRECTION('ref_axis',(-4.93038065763132E-32,0.,1.)) ;
#78865 = DIRECTION('center_axis',(-1.,0.,0.)) ;
#78866 = DIRECTION('ref_axis',(0.,0.,1.)) ;
#78867 = DIRECTION('center_axis',(1.,0.,0.)) ;
#78868 = DIRECTION('ref_axis',(0.,0.,-1.)) ;
#78869 = DIRECTION('center_axis',(0.,1.,0.)) ;
#78870 = DIRECTION('ref_axis',(0.,0.,1.)) ;
#78871 = DIRECTION('center_axis',(0.,-1.,0.)) ;
#78872 = DIRECTION('ref_axis',(0.,0.,-1.)) ;
#78873 = DIRECTION('center_axis',(0.,0.,-1.)) ;
#78874 = DIRECTION('ref_axis',(-1.,0.,0.)) ;
#78875 = DIRECTION('center_axis',(-4.93038065763132E-32,0.,1.)) ;
#78876 = DIRECTION('ref_axis',(1.,0.,4.93038065763132E-32)) ;
#78877 = DIRECTION('center_axis',(1.,0.,4.93038065763132E-32)) ;
#78878 = DIRECTION('ref_axis',(4.93038065763132E-32,0.,-1.)) ;
#78879 = DIRECTION('center_axis',(-1.,0.,0.)) ;
#78880 = DIRECTION('ref_axis',(0.,0.,1.)) ;
#78881 = DIRECTION('center_axis',(1.,0.,0.)) ;
#78882 = DIRECTION('ref_axis',(0.,0.,-1.)) ;
#78883 = DIRECTION('center_axis',(-4.93038065763132E-32,0.,1.)) ;
#78884 = DIRECTION('ref_axis',(1.,0.,0.)) ;
#78885 = DIRECTION('center_axis',(0.,-1.,0.)) ;
#78886 = DIRECTION('ref_axis',(0.,0.,1.)) ;
#78887 = DIRECTION('center_axis',(-4.93038065763132E-32,0.,1.)) ;
#78888 = DIRECTION('ref_axis',(1.,0.,0.)) ;
#78889 = DIRECTION('center_axis',(-4.93038065763132E-32,0.,1.)) ;
#78890 = DIRECTION('ref_axis',(1.,0.,4.93038065763132E-32)) ;
#78891 = DIRECTION('center_axis',(-4.93038065763132E-32,0.,1.)) ;
#78892 = DIRECTION('ref_axis',(1.,0.,0.)) ;
#78893 = DIRECTION('center_axis',(-4.93038065763132E-32,0.,1.)) ;
#78894 = DIRECTION('ref_axis',(1.,0.,4.93038065763132E-32)) ;
#78895 = DIRECTION('center_axis',(-4.93038065763132E-32,0.,1.)) ;
#78896 = DIRECTION('ref_axis',(1.,0.,0.)) ;
#78897 = DIRECTION('center_axis',(0.,-1.,0.)) ;
#78898 = DIRECTION('ref_axis',(0.,0.,1.)) ;
#78899 = DIRECTION('center_axis',(6.93889390390723E-16,-1.,3.42113882891801E-47)) ;
#78900 = DIRECTION('ref_axis',(1.,6.93889390390723E-16,-2.37389193643995E-62)) ;
#78901 = DIRECTION('center_axis',(0.,-1.,0.)) ;
#78902 = DIRECTION('ref_axis',(0.,0.,-1.)) ;
#78903 = DIRECTION('center_axis',(0.,0.,-1.)) ;
#78904 = DIRECTION('ref_axis',(-1.,0.,0.)) ;
#78905 = DIRECTION('center_axis',(-4.93038065763132E-32,0.,1.)) ;
#78906 = DIRECTION('ref_axis',(1.,0.,4.93038065763132E-32)) ;
#78907 = DIRECTION('center_axis',(0.,0.,-1.)) ;
#78908 = DIRECTION('ref_axis',(-1.,0.,0.)) ;
#78909 = DIRECTION('center_axis',(-4.93038065763132E-32,0.,1.)) ;
#78910 = DIRECTION('ref_axis',(1.,0.,4.93038065763132E-32)) ;
#78911 = DIRECTION('center_axis',(0.,1.,0.)) ;
#78912 = DIRECTION('ref_axis',(0.,0.,1.)) ;
#78913 = DIRECTION('center_axis',(0.,-1.,0.)) ;
#78914 = DIRECTION('ref_axis',(0.,0.,-1.)) ;
#78915 = DIRECTION('center_axis',(-4.93038065763132E-32,0.,1.)) ;
#78916 = DIRECTION('ref_axis',(1.,0.,0.)) ;
#78917 = DIRECTION('center_axis',(-1.,0.,0.)) ;
#78918 = DIRECTION('ref_axis',(0.,0.,-1.)) ;
#78919 = DIRECTION('center_axis',(-4.93038065763132E-32,0.,1.)) ;
#78920 = DIRECTION('ref_axis',(1.,0.,0.)) ;
#78921 = DIRECTION('center_axis',(1.,0.,0.)) ;
#78922 = DIRECTION('ref_axis',(0.,0.,1.)) ;
#78923 = DIRECTION('center_axis',(-1.,0.,-4.93038065763132E-32)) ;
#78924 = DIRECTION('ref_axis',(-4.93038065763132E-32,0.,1.)) ;
#78925 = DIRECTION('center_axis',(1.,0.,4.93038065763132E-32)) ;
#78926 = DIRECTION('ref_axis',(4.93038065763132E-32,0.,-1.)) ;
#78927 = DIRECTION('center_axis',(1.,0.,0.)) ;
#78928 = DIRECTION('ref_axis',(0.,0.,-1.)) ;
#78929 = DIRECTION('center_axis',(-1.,0.,0.)) ;
#78930 = DIRECTION('ref_axis',(0.,0.,1.)) ;
#78931 = DIRECTION('center_axis',(-4.93038065763132E-32,0.,1.)) ;
#78932 = DIRECTION('ref_axis',(1.,0.,0.)) ;
#78933 = DIRECTION('center_axis',(-4.93038065763132E-32,0.,1.)) ;
#78934 = DIRECTION('ref_axis',(1.,0.,4.93038065763132E-32)) ;
#78935 = DIRECTION('center_axis',(0.,-1.,0.)) ;
#78936 = DIRECTION('ref_axis',(0.,0.,1.)) ;
#78937 = DIRECTION('center_axis',(-4.93038065763132E-32,0.,1.)) ;
#78938 = DIRECTION('ref_axis',(1.,0.,0.)) ;
#78939 = DIRECTION('center_axis',(0.,-1.,0.)) ;
#78940 = DIRECTION('ref_axis',(0.,0.,1.)) ;
#78941 = DIRECTION('center_axis',(-4.93038065763132E-32,0.,1.)) ;
#78942 = DIRECTION('ref_axis',(1.,0.,4.93038065763132E-32)) ;
#78943 = DIRECTION('center_axis',(0.,0.,-1.)) ;
#78944 = DIRECTION('ref_axis',(-1.,0.,0.)) ;
#78945 = DIRECTION('center_axis',(-4.93038065763132E-32,0.,1.)) ;
#78946 = DIRECTION('ref_axis',(1.,0.,4.93038065763132E-32)) ;
#78947 = DIRECTION('center_axis',(3.46944695195361E-16,-1.,1.71056941445901E-47)) ;
#78948 = DIRECTION('ref_axis',(1.,3.46944695195361E-16,-5.93472984109987E-63)) ;
#78949 = DIRECTION('center_axis',(0.,-1.,0.)) ;
#78950 = DIRECTION('ref_axis',(0.,0.,-1.)) ;
#78951 = DIRECTION('center_axis',(-1.,0.,-4.93038065763132E-32)) ;
#78952 = DIRECTION('ref_axis',(-4.93038065763132E-32,0.,1.)) ;
#78953 = DIRECTION('center_axis',(-1.,0.,0.)) ;
#78954 = DIRECTION('ref_axis',(0.,0.,1.)) ;
#78955 = DIRECTION('center_axis',(1.,0.,0.)) ;
#78956 = DIRECTION('ref_axis',(0.,0.,-1.)) ;
#78957 = DIRECTION('center_axis',(0.,1.,0.)) ;
#78958 = DIRECTION('ref_axis',(0.,0.,1.)) ;
#78959 = DIRECTION('center_axis',(0.,-1.,0.)) ;
#78960 = DIRECTION('ref_axis',(0.,0.,-1.)) ;
#78961 = DIRECTION('center_axis',(0.,0.,-1.)) ;
#78962 = DIRECTION('ref_axis',(-1.,0.,0.)) ;
#78963 = DIRECTION('center_axis',(-4.93038065763132E-32,0.,1.)) ;
#78964 = DIRECTION('ref_axis',(1.,0.,4.93038065763132E-32)) ;
#78965 = DIRECTION('center_axis',(1.,0.,4.93038065763132E-32)) ;
#78966 = DIRECTION('ref_axis',(4.93038065763132E-32,0.,-1.)) ;
#78967 = DIRECTION('center_axis',(-1.,0.,0.)) ;
#78968 = DIRECTION('ref_axis',(0.,0.,1.)) ;
#78969 = DIRECTION('center_axis',(1.,0.,0.)) ;
#78970 = DIRECTION('ref_axis',(0.,0.,-1.)) ;
#78971 = DIRECTION('center_axis',(-4.93038065763132E-32,0.,1.)) ;
#78972 = DIRECTION('ref_axis',(1.,0.,0.)) ;
#78973 = DIRECTION('center_axis',(0.,-1.,0.)) ;
#78974 = DIRECTION('ref_axis',(0.,0.,1.)) ;
#78975 = DIRECTION('center_axis',(-4.93038065763132E-32,0.,1.)) ;
#78976 = DIRECTION('ref_axis',(1.,0.,0.)) ;
#78977 = DIRECTION('center_axis',(-4.93038065763132E-32,0.,1.)) ;
#78978 = DIRECTION('ref_axis',(1.,0.,4.93038065763132E-32)) ;
#78979 = DIRECTION('center_axis',(-4.93038065763132E-32,0.,1.)) ;
#78980 = DIRECTION('ref_axis',(1.,0.,0.)) ;
#78981 = DIRECTION('center_axis',(-4.93038065763132E-32,0.,1.)) ;
#78982 = DIRECTION('ref_axis',(1.,0.,4.93038065763132E-32)) ;
#78983 = DIRECTION('center_axis',(-4.93038065763132E-32,0.,1.)) ;
#78984 = DIRECTION('ref_axis',(1.,0.,0.)) ;
#78985 = DIRECTION('center_axis',(0.,-1.,0.)) ;
#78986 = DIRECTION('ref_axis',(0.,0.,1.)) ;
#78987 = DIRECTION('center_axis',(3.46944695195361E-16,-1.,1.71056941445901E-47)) ;
#78988 = DIRECTION('ref_axis',(1.,3.46944695195361E-16,-5.93472984109987E-63)) ;
#78989 = DIRECTION('center_axis',(0.,-1.,0.)) ;
#78990 = DIRECTION('ref_axis',(0.,0.,-1.)) ;
#78991 = DIRECTION('center_axis',(0.,0.,-1.)) ;
#78992 = DIRECTION('ref_axis',(-1.,0.,0.)) ;
#78993 = DIRECTION('center_axis',(-4.93038065763132E-32,0.,1.)) ;
#78994 = DIRECTION('ref_axis',(1.,0.,4.93038065763132E-32)) ;
#78995 = DIRECTION('center_axis',(0.,0.,-1.)) ;
#78996 = DIRECTION('ref_axis',(-1.,0.,0.)) ;
#78997 = DIRECTION('center_axis',(-4.93038065763132E-32,0.,1.)) ;
#78998 = DIRECTION('ref_axis',(1.,0.,4.93038065763132E-32)) ;
#78999 = DIRECTION('center_axis',(0.,1.,0.)) ;
#79000 = DIRECTION('ref_axis',(0.,0.,1.)) ;
#79001 = DIRECTION('center_axis',(0.,-1.,0.)) ;
#79002 = DIRECTION('ref_axis',(0.,0.,-1.)) ;
#79003 = DIRECTION('center_axis',(-4.93038065763132E-32,0.,1.)) ;
#79004 = DIRECTION('ref_axis',(1.,0.,0.)) ;
#79005 = DIRECTION('center_axis',(-1.,0.,0.)) ;
#79006 = DIRECTION('ref_axis',(0.,0.,-1.)) ;
#79007 = DIRECTION('center_axis',(-4.93038065763132E-32,0.,1.)) ;
#79008 = DIRECTION('ref_axis',(1.,0.,0.)) ;
#79009 = DIRECTION('center_axis',(1.,0.,0.)) ;
#79010 = DIRECTION('ref_axis',(0.,0.,1.)) ;
#79011 = DIRECTION('center_axis',(-1.,0.,-4.93038065763132E-32)) ;
#79012 = DIRECTION('ref_axis',(-4.93038065763132E-32,0.,1.)) ;
#79013 = DIRECTION('center_axis',(1.,0.,4.93038065763132E-32)) ;
#79014 = DIRECTION('ref_axis',(4.93038065763132E-32,0.,-1.)) ;
#79015 = DIRECTION('center_axis',(1.,0.,0.)) ;
#79016 = DIRECTION('ref_axis',(0.,0.,-1.)) ;
#79017 = DIRECTION('center_axis',(-1.,0.,0.)) ;
#79018 = DIRECTION('ref_axis',(0.,0.,1.)) ;
#79019 = DIRECTION('center_axis',(-4.93038065763132E-32,0.,1.)) ;
#79020 = DIRECTION('ref_axis',(1.,0.,0.)) ;
#79021 = DIRECTION('center_axis',(-4.93038065763132E-32,0.,1.)) ;
#79022 = DIRECTION('ref_axis',(1.,0.,4.93038065763132E-32)) ;
#79023 = DIRECTION('center_axis',(0.,-1.,0.)) ;
#79024 = DIRECTION('ref_axis',(0.,0.,1.)) ;
#79025 = DIRECTION('center_axis',(-4.93038065763132E-32,0.,1.)) ;
#79026 = DIRECTION('ref_axis',(1.,0.,0.)) ;
#79027 = DIRECTION('center_axis',(0.,-1.,0.)) ;
#79028 = DIRECTION('ref_axis',(0.,0.,1.)) ;
#79029 = DIRECTION('center_axis',(-4.93038065763132E-32,0.,1.)) ;
#79030 = DIRECTION('ref_axis',(1.,0.,4.93038065763132E-32)) ;
#79031 = DIRECTION('center_axis',(0.,0.,-1.)) ;
#79032 = DIRECTION('ref_axis',(-1.,0.,0.)) ;
#79033 = DIRECTION('center_axis',(-4.93038065763132E-32,0.,1.)) ;
#79034 = DIRECTION('ref_axis',(1.,0.,4.93038065763132E-32)) ;
#79035 = DIRECTION('center_axis',(0.,-1.,0.)) ;
#79036 = DIRECTION('ref_axis',(0.,0.,-1.)) ;
#79037 = DIRECTION('center_axis',(0.,-1.,0.)) ;
#79038 = DIRECTION('ref_axis',(0.,0.,-1.)) ;
#79039 = DIRECTION('center_axis',(-1.,0.,-4.93038065763132E-32)) ;
#79040 = DIRECTION('ref_axis',(-4.93038065763132E-32,0.,1.)) ;
#79041 = DIRECTION('center_axis',(-1.,0.,0.)) ;
#79042 = DIRECTION('ref_axis',(0.,0.,1.)) ;
#79043 = DIRECTION('center_axis',(1.,0.,0.)) ;
#79044 = DIRECTION('ref_axis',(0.,0.,-1.)) ;
#79045 = DIRECTION('center_axis',(-3.46944695195361E-16,1.,-1.71056941445901E-47)) ;
#79046 = DIRECTION('ref_axis',(-1.,-3.46944695195361E-16,5.93472984109987E-63)) ;
#79047 = DIRECTION('center_axis',(0.,-1.,0.)) ;
#79048 = DIRECTION('ref_axis',(0.,0.,-1.)) ;
#79049 = DIRECTION('center_axis',(0.,0.,-1.)) ;
#79050 = DIRECTION('ref_axis',(-1.,0.,0.)) ;
#79051 = DIRECTION('center_axis',(-4.93038065763132E-32,0.,1.)) ;
#79052 = DIRECTION('ref_axis',(1.,0.,4.93038065763132E-32)) ;
#79053 = DIRECTION('center_axis',(1.,0.,4.93038065763132E-32)) ;
#79054 = DIRECTION('ref_axis',(4.93038065763132E-32,0.,-1.)) ;
#79055 = DIRECTION('center_axis',(-1.,0.,0.)) ;
#79056 = DIRECTION('ref_axis',(0.,0.,1.)) ;
#79057 = DIRECTION('center_axis',(1.,0.,0.)) ;
#79058 = DIRECTION('ref_axis',(0.,0.,-1.)) ;
#79059 = DIRECTION('center_axis',(-4.93038065763132E-32,0.,1.)) ;
#79060 = DIRECTION('ref_axis',(1.,0.,0.)) ;
#79061 = DIRECTION('center_axis',(0.,-1.,0.)) ;
#79062 = DIRECTION('ref_axis',(0.,0.,1.)) ;
#79063 = DIRECTION('center_axis',(-4.93038065763132E-32,0.,1.)) ;
#79064 = DIRECTION('ref_axis',(1.,0.,0.)) ;
#79065 = DIRECTION('center_axis',(-4.93038065763132E-32,0.,1.)) ;
#79066 = DIRECTION('ref_axis',(1.,0.,4.93038065763132E-32)) ;
#79067 = DIRECTION('center_axis',(-4.93038065763132E-32,0.,1.)) ;
#79068 = DIRECTION('ref_axis',(1.,0.,0.)) ;
#79069 = DIRECTION('center_axis',(-4.93038065763132E-32,0.,1.)) ;
#79070 = DIRECTION('ref_axis',(1.,0.,4.93038065763132E-32)) ;
#79071 = DIRECTION('center_axis',(-4.93038065763132E-32,0.,1.)) ;
#79072 = DIRECTION('ref_axis',(1.,0.,0.)) ;
#79073 = DIRECTION('center_axis',(0.,-1.,0.)) ;
#79074 = DIRECTION('ref_axis',(0.,0.,1.)) ;
#79075 = DIRECTION('center_axis',(0.,-1.,0.)) ;
#79076 = DIRECTION('ref_axis',(0.,0.,-1.)) ;
#79077 = DIRECTION('center_axis',(0.,-1.,0.)) ;
#79078 = DIRECTION('ref_axis',(0.,0.,-1.)) ;
#79079 = DIRECTION('center_axis',(0.,0.,-1.)) ;
#79080 = DIRECTION('ref_axis',(-1.,0.,0.)) ;
#79081 = DIRECTION('center_axis',(-4.93038065763132E-32,0.,1.)) ;
#79082 = DIRECTION('ref_axis',(1.,0.,4.93038065763132E-32)) ;
#79083 = DIRECTION('center_axis',(0.,0.,-1.)) ;
#79084 = DIRECTION('ref_axis',(-1.,0.,0.)) ;
#79085 = DIRECTION('center_axis',(-4.93038065763132E-32,0.,1.)) ;
#79086 = DIRECTION('ref_axis',(1.,0.,4.93038065763132E-32)) ;
#79087 = DIRECTION('center_axis',(-3.46944695195361E-16,1.,-1.71056941445901E-47)) ;
#79088 = DIRECTION('ref_axis',(-1.,-3.46944695195361E-16,5.93472984109987E-63)) ;
#79089 = DIRECTION('center_axis',(0.,-1.,0.)) ;
#79090 = DIRECTION('ref_axis',(0.,0.,-1.)) ;
#79091 = DIRECTION('center_axis',(-4.93038065763132E-32,0.,1.)) ;
#79092 = DIRECTION('ref_axis',(1.,0.,0.)) ;
#79093 = DIRECTION('center_axis',(-1.,0.,0.)) ;
#79094 = DIRECTION('ref_axis',(0.,0.,-1.)) ;
#79095 = DIRECTION('center_axis',(-4.93038065763132E-32,0.,1.)) ;
#79096 = DIRECTION('ref_axis',(1.,0.,0.)) ;
#79097 = DIRECTION('center_axis',(1.,0.,0.)) ;
#79098 = DIRECTION('ref_axis',(0.,0.,1.)) ;
#79099 = DIRECTION('center_axis',(-1.,0.,-4.93038065763132E-32)) ;
#79100 = DIRECTION('ref_axis',(-4.93038065763132E-32,0.,1.)) ;
#79101 = DIRECTION('center_axis',(-1.,0.,-4.93038065763132E-32)) ;
#79102 = DIRECTION('ref_axis',(-4.93038065763132E-32,0.,1.)) ;
#79103 = DIRECTION('center_axis',(-1.,0.,0.)) ;
#79104 = DIRECTION('ref_axis',(0.,0.,1.)) ;
#79105 = DIRECTION('center_axis',(1.,0.,0.)) ;
#79106 = DIRECTION('ref_axis',(0.,0.,-1.)) ;
#79107 = DIRECTION('center_axis',(-4.93038065763132E-32,0.,1.)) ;
#79108 = DIRECTION('ref_axis',(1.,0.,0.)) ;
#79109 = DIRECTION('center_axis',(-4.93038065763132E-32,0.,1.)) ;
#79110 = DIRECTION('ref_axis',(1.,0.,4.93038065763132E-32)) ;
#79111 = DIRECTION('center_axis',(0.,1.,0.)) ;
#79112 = DIRECTION('ref_axis',(0.,0.,-1.)) ;
#79113 = DIRECTION('center_axis',(-4.93038065763132E-32,0.,1.)) ;
#79114 = DIRECTION('ref_axis',(1.,0.,0.)) ;
#79115 = DIRECTION('center_axis',(0.,1.,0.)) ;
#79116 = DIRECTION('ref_axis',(0.,0.,-1.)) ;
#79117 = DIRECTION('center_axis',(-4.93038065763132E-32,0.,1.)) ;
#79118 = DIRECTION('ref_axis',(1.,0.,4.93038065763132E-32)) ;
#79119 = DIRECTION('center_axis',(0.,0.,-1.)) ;
#79120 = DIRECTION('ref_axis',(-1.,0.,0.)) ;
#79121 = DIRECTION('center_axis',(-4.93038065763132E-32,0.,1.)) ;
#79122 = DIRECTION('ref_axis',(1.,0.,4.93038065763132E-32)) ;
#79123 = DIRECTION('center_axis',(-3.46944695195361E-16,1.,-1.71056941445901E-47)) ;
#79124 = DIRECTION('ref_axis',(-1.,-3.46944695195361E-16,5.93472984109987E-63)) ;
#79125 = DIRECTION('center_axis',(0.,1.,0.)) ;
#79126 = DIRECTION('ref_axis',(0.,0.,1.)) ;
#79127 = DIRECTION('center_axis',(1.,0.,4.93038065763132E-32)) ;
#79128 = DIRECTION('ref_axis',(4.93038065763132E-32,0.,-1.)) ;
#79129 = DIRECTION('center_axis',(1.,0.,0.)) ;
#79130 = DIRECTION('ref_axis',(0.,0.,-1.)) ;
#79131 = DIRECTION('center_axis',(-1.,0.,0.)) ;
#79132 = DIRECTION('ref_axis',(0.,0.,1.)) ;
#79133 = DIRECTION('center_axis',(0.,-1.,0.)) ;
#79134 = DIRECTION('ref_axis',(0.,0.,-1.)) ;
#79135 = DIRECTION('center_axis',(0.,1.,0.)) ;
#79136 = DIRECTION('ref_axis',(0.,0.,1.)) ;
#79137 = DIRECTION('center_axis',(0.,0.,-1.)) ;
#79138 = DIRECTION('ref_axis',(-1.,0.,0.)) ;
#79139 = DIRECTION('center_axis',(-4.93038065763132E-32,0.,1.)) ;
#79140 = DIRECTION('ref_axis',(1.,0.,4.93038065763132E-32)) ;
#79141 = DIRECTION('center_axis',(-1.,0.,-4.93038065763132E-32)) ;
#79142 = DIRECTION('ref_axis',(-4.93038065763132E-32,0.,1.)) ;
#79143 = DIRECTION('center_axis',(1.,0.,0.)) ;
#79144 = DIRECTION('ref_axis',(0.,0.,-1.)) ;
#79145 = DIRECTION('center_axis',(-1.,0.,0.)) ;
#79146 = DIRECTION('ref_axis',(0.,0.,1.)) ;
#79147 = DIRECTION('center_axis',(-4.93038065763132E-32,0.,1.)) ;
#79148 = DIRECTION('ref_axis',(1.,0.,0.)) ;
#79149 = DIRECTION('center_axis',(0.,1.,0.)) ;
#79150 = DIRECTION('ref_axis',(0.,0.,-1.)) ;
#79151 = DIRECTION('center_axis',(-4.93038065763132E-32,0.,1.)) ;
#79152 = DIRECTION('ref_axis',(1.,0.,0.)) ;
#79153 = DIRECTION('center_axis',(-4.93038065763132E-32,0.,1.)) ;
#79154 = DIRECTION('ref_axis',(1.,0.,4.93038065763132E-32)) ;
#79155 = DIRECTION('center_axis',(-4.93038065763132E-32,0.,1.)) ;
#79156 = DIRECTION('ref_axis',(1.,0.,0.)) ;
#79157 = DIRECTION('center_axis',(-4.93038065763132E-32,0.,1.)) ;
#79158 = DIRECTION('ref_axis',(1.,0.,4.93038065763132E-32)) ;
#79159 = DIRECTION('center_axis',(-4.93038065763132E-32,0.,1.)) ;
#79160 = DIRECTION('ref_axis',(1.,0.,0.)) ;
#79161 = DIRECTION('center_axis',(0.,1.,0.)) ;
#79162 = DIRECTION('ref_axis',(0.,0.,-1.)) ;
#79163 = DIRECTION('center_axis',(-3.46944695195361E-16,1.,-1.71056941445901E-47)) ;
#79164 = DIRECTION('ref_axis',(-1.,-3.46944695195361E-16,5.93472984109987E-63)) ;
#79165 = DIRECTION('center_axis',(0.,1.,0.)) ;
#79166 = DIRECTION('ref_axis',(0.,0.,1.)) ;
#79167 = DIRECTION('center_axis',(0.,0.,-1.)) ;
#79168 = DIRECTION('ref_axis',(-1.,0.,0.)) ;
#79169 = DIRECTION('center_axis',(-4.93038065763132E-32,0.,1.)) ;
#79170 = DIRECTION('ref_axis',(1.,0.,4.93038065763132E-32)) ;
#79171 = DIRECTION('center_axis',(0.,0.,-1.)) ;
#79172 = DIRECTION('ref_axis',(-1.,0.,0.)) ;
#79173 = DIRECTION('center_axis',(-4.93038065763132E-32,0.,1.)) ;
#79174 = DIRECTION('ref_axis',(1.,0.,4.93038065763132E-32)) ;
#79175 = DIRECTION('center_axis',(0.,-1.,0.)) ;
#79176 = DIRECTION('ref_axis',(0.,0.,-1.)) ;
#79177 = DIRECTION('center_axis',(0.,1.,0.)) ;
#79178 = DIRECTION('ref_axis',(0.,0.,1.)) ;
#79179 = DIRECTION('center_axis',(-4.93038065763132E-32,0.,1.)) ;
#79180 = DIRECTION('ref_axis',(1.,0.,0.)) ;
#79181 = DIRECTION('center_axis',(1.,0.,0.)) ;
#79182 = DIRECTION('ref_axis',(0.,0.,1.)) ;
#79183 = DIRECTION('center_axis',(-4.93038065763132E-32,0.,1.)) ;
#79184 = DIRECTION('ref_axis',(1.,0.,0.)) ;
#79185 = DIRECTION('center_axis',(-1.,0.,0.)) ;
#79186 = DIRECTION('ref_axis',(0.,0.,-1.)) ;
#79187 = DIRECTION('center_axis',(1.,0.,4.93038065763132E-32)) ;
#79188 = DIRECTION('ref_axis',(4.93038065763132E-32,0.,-1.)) ;
#79189 = DIRECTION('center_axis',(1.,0.,4.93038065763132E-32)) ;
#79190 = DIRECTION('ref_axis',(4.93038065763132E-32,0.,-1.)) ;
#79191 = DIRECTION('center_axis',(1.,0.,0.)) ;
#79192 = DIRECTION('ref_axis',(0.,0.,-1.)) ;
#79193 = DIRECTION('center_axis',(-1.,0.,0.)) ;
#79194 = DIRECTION('ref_axis',(0.,0.,1.)) ;
#79195 = DIRECTION('center_axis',(-4.93038065763132E-32,0.,1.)) ;
#79196 = DIRECTION('ref_axis',(1.,0.,0.)) ;
#79197 = DIRECTION('center_axis',(-4.93038065763132E-32,0.,1.)) ;
#79198 = DIRECTION('ref_axis',(1.,0.,4.93038065763132E-32)) ;
#79199 = DIRECTION('center_axis',(0.,-1.,0.)) ;
#79200 = DIRECTION('ref_axis',(0.,0.,1.)) ;
#79201 = DIRECTION('center_axis',(-4.93038065763132E-32,0.,1.)) ;
#79202 = DIRECTION('ref_axis',(1.,0.,0.)) ;
#79203 = DIRECTION('center_axis',(0.,-1.,0.)) ;
#79204 = DIRECTION('ref_axis',(0.,0.,1.)) ;
#79205 = DIRECTION('center_axis',(-4.93038065763132E-32,0.,1.)) ;
#79206 = DIRECTION('ref_axis',(1.,0.,4.93038065763132E-32)) ;
#79207 = DIRECTION('center_axis',(0.,0.,-1.)) ;
#79208 = DIRECTION('ref_axis',(-1.,0.,0.)) ;
#79209 = DIRECTION('center_axis',(-4.93038065763132E-32,0.,1.)) ;
#79210 = DIRECTION('ref_axis',(1.,0.,4.93038065763132E-32)) ;
#79211 = DIRECTION('center_axis',(1.73472347597681E-16,-1.,8.55284707229503E-48)) ;
#79212 = DIRECTION('ref_axis',(1.,1.73472347597681E-16,-1.48368246027497E-63)) ;
#79213 = DIRECTION('center_axis',(0.,-1.,0.)) ;
#79214 = DIRECTION('ref_axis',(0.,0.,-1.)) ;
#79215 = DIRECTION('center_axis',(-1.,0.,-4.93038065763132E-32)) ;
#79216 = DIRECTION('ref_axis',(-4.93038065763132E-32,0.,1.)) ;
#79217 = DIRECTION('center_axis',(-1.,0.,0.)) ;
#79218 = DIRECTION('ref_axis',(0.,0.,1.)) ;
#79219 = DIRECTION('center_axis',(1.,0.,0.)) ;
#79220 = DIRECTION('ref_axis',(0.,0.,-1.)) ;
#79221 = DIRECTION('center_axis',(-2.60208521396521E-16,1.,-1.28292706084425E-47)) ;
#79222 = DIRECTION('ref_axis',(-1.,-2.60208521396521E-16,3.33828553561868E-63)) ;
#79223 = DIRECTION('center_axis',(0.,-1.,0.)) ;
#79224 = DIRECTION('ref_axis',(0.,0.,-1.)) ;
#79225 = DIRECTION('center_axis',(0.,0.,-1.)) ;
#79226 = DIRECTION('ref_axis',(-1.,0.,0.)) ;
#79227 = DIRECTION('center_axis',(-4.93038065763132E-32,0.,1.)) ;
#79228 = DIRECTION('ref_axis',(1.,0.,4.93038065763132E-32)) ;
#79229 = DIRECTION('center_axis',(1.,0.,4.93038065763132E-32)) ;
#79230 = DIRECTION('ref_axis',(4.93038065763132E-32,0.,-1.)) ;
#79231 = DIRECTION('center_axis',(-1.,0.,0.)) ;
#79232 = DIRECTION('ref_axis',(0.,0.,1.)) ;
#79233 = DIRECTION('center_axis',(1.,0.,0.)) ;
#79234 = DIRECTION('ref_axis',(0.,0.,-1.)) ;
#79235 = DIRECTION('center_axis',(-4.93038065763132E-32,0.,1.)) ;
#79236 = DIRECTION('ref_axis',(1.,0.,0.)) ;
#79237 = DIRECTION('center_axis',(0.,-1.,0.)) ;
#79238 = DIRECTION('ref_axis',(0.,0.,1.)) ;
#79239 = DIRECTION('center_axis',(-4.93038065763132E-32,0.,1.)) ;
#79240 = DIRECTION('ref_axis',(1.,0.,0.)) ;
#79241 = DIRECTION('center_axis',(-4.93038065763132E-32,0.,1.)) ;
#79242 = DIRECTION('ref_axis',(1.,0.,4.93038065763132E-32)) ;
#79243 = DIRECTION('center_axis',(-4.93038065763132E-32,0.,1.)) ;
#79244 = DIRECTION('ref_axis',(1.,0.,0.)) ;
#79245 = DIRECTION('center_axis',(-4.93038065763132E-32,0.,1.)) ;
#79246 = DIRECTION('ref_axis',(1.,0.,4.93038065763132E-32)) ;
#79247 = DIRECTION('center_axis',(-4.93038065763132E-32,0.,1.)) ;
#79248 = DIRECTION('ref_axis',(1.,0.,0.)) ;
#79249 = DIRECTION('center_axis',(0.,-1.,0.)) ;
#79250 = DIRECTION('ref_axis',(0.,0.,1.)) ;
#79251 = DIRECTION('center_axis',(1.73472347597681E-16,-1.,8.55284707229503E-48)) ;
#79252 = DIRECTION('ref_axis',(1.,1.73472347597681E-16,-1.48368246027497E-63)) ;
#79253 = DIRECTION('center_axis',(0.,-1.,0.)) ;
#79254 = DIRECTION('ref_axis',(0.,0.,-1.)) ;
#79255 = DIRECTION('center_axis',(0.,0.,-1.)) ;
#79256 = DIRECTION('ref_axis',(-1.,0.,0.)) ;
#79257 = DIRECTION('center_axis',(-4.93038065763132E-32,0.,1.)) ;
#79258 = DIRECTION('ref_axis',(1.,0.,4.93038065763132E-32)) ;
#79259 = DIRECTION('center_axis',(0.,0.,-1.)) ;
#79260 = DIRECTION('ref_axis',(-1.,0.,0.)) ;
#79261 = DIRECTION('center_axis',(-4.93038065763132E-32,0.,1.)) ;
#79262 = DIRECTION('ref_axis',(1.,0.,4.93038065763132E-32)) ;
#79263 = DIRECTION('center_axis',(-2.60208521396521E-16,1.,-1.28292706084425E-47)) ;
#79264 = DIRECTION('ref_axis',(-1.,-2.60208521396521E-16,3.33828553561868E-63)) ;
#79265 = DIRECTION('center_axis',(0.,-1.,0.)) ;
#79266 = DIRECTION('ref_axis',(0.,0.,-1.)) ;
#79267 = DIRECTION('center_axis',(-4.93038065763132E-32,0.,1.)) ;
#79268 = DIRECTION('ref_axis',(1.,0.,0.)) ;
#79269 = DIRECTION('center_axis',(-1.,0.,0.)) ;
#79270 = DIRECTION('ref_axis',(0.,0.,-1.)) ;
#79271 = DIRECTION('center_axis',(-4.93038065763132E-32,0.,1.)) ;
#79272 = DIRECTION('ref_axis',(1.,0.,0.)) ;
#79273 = DIRECTION('center_axis',(1.,0.,0.)) ;
#79274 = DIRECTION('ref_axis',(0.,0.,1.)) ;
#79275 = DIRECTION('center_axis',(-1.,0.,-4.93038065763132E-32)) ;
#79276 = DIRECTION('ref_axis',(-4.93038065763132E-32,0.,1.)) ;
#79277 = DIRECTION('center_axis',(-3.65204942310907E-15,1.,-1.22867065825113E-46)) ;
#79278 = DIRECTION('ref_axis',(-1.,-3.65204942310907E-15,-8.41343619123299E-62)) ;
#79279 = DIRECTION('center_axis',(0.707106781186535,0.70710678118656,3.59045601457188E-14)) ;
#79280 = DIRECTION('ref_axis',(0.70710678118656,-0.707106781186535,-1.32030231652671E-12)) ;
#79281 = DIRECTION('center_axis',(0.,-1.,0.)) ;
#79282 = DIRECTION('ref_axis',(0.,0.,-1.)) ;
#79283 = DIRECTION('center_axis',(3.65204942310907E-15,-1.,-7.70988211545247E-16)) ;
#79284 = DIRECTION('ref_axis',(1.,3.65204942310907E-15,-1.29620107950046E-43)) ;
#79285 = DIRECTION('center_axis',(0.,-1.,0.)) ;
#79286 = DIRECTION('ref_axis',(0.,0.,-1.)) ;
#79287 = DIRECTION('center_axis',(0.707106781186586,0.707106781186509,6.51411305500852E-14)) ;
#79288 = DIRECTION('ref_axis',(0.707106781186509,-0.707106781186586,-4.14202338982266E-13)) ;
#79289 = DIRECTION('center_axis',(-1.03517906367563E-32,-1.81408990951823E-16,
1.)) ;
#79290 = DIRECTION('ref_axis',(1.87790789395849E-48,-1.,-1.81408990951823E-16)) ;
#79291 = DIRECTION('center_axis',(0.,-4.62592926927146E-14,1.)) ;
#79292 = DIRECTION('ref_axis',(0.,-1.,-4.62592926927146E-14)) ;
#79293 = DIRECTION('center_axis',(0.,0.,-1.)) ;
#79294 = DIRECTION('ref_axis',(-1.,0.,0.)) ;
#79295 = DIRECTION('center_axis',(0.,1.,0.)) ;
#79296 = DIRECTION('ref_axis',(1.,0.,0.)) ;
#79297 = DIRECTION('center_axis',(1.,0.,0.)) ;
#79298 = DIRECTION('ref_axis',(0.,0.,1.)) ;
#79299 = DIRECTION('center_axis',(-1.,-3.65204942310907E-15,-6.7286639138916E-31)) ;
#79300 = DIRECTION('ref_axis',(3.65204942310907E-15,-1.,2.45734131650226E-45)) ;
#79301 = DIRECTION('center_axis',(0.707106781186584,-0.707106781186511,5.62504775616304E-14)) ;
#79302 = DIRECTION('ref_axis',(0.707106781186511,0.707106781186584,-5.62770983609062E-12)) ;
#79303 = DIRECTION('center_axis',(-1.,-3.65204942310907E-15,-6.72866391389159E-31)) ;
#79304 = DIRECTION('ref_axis',(3.65204942310907E-15,-1.,2.45734131650226E-45)) ;
#79305 = DIRECTION('center_axis',(0.707106781186529,-0.707106781186566,5.43697625063671E-14)) ;
#79306 = DIRECTION('ref_axis',(0.707106781186566,0.707106781186529,-3.4443471035871E-13)) ;
#79307 = DIRECTION('center_axis',(0.,1.,0.)) ;
#79308 = DIRECTION('ref_axis',(1.,0.,0.)) ;
#79309 = DIRECTION('center_axis',(1.,0.,0.)) ;
#79310 = DIRECTION('ref_axis',(0.,0.,1.)) ;
#79311 = DIRECTION('center_axis',(-1.,-3.49148133884313E-15,-6.7286639138916E-31)) ;
#79312 = DIRECTION('ref_axis',(3.49148133884313E-15,-1.,2.34930044906997E-45)) ;
#79313 = DIRECTION('center_axis',(1.,0.,0.)) ;
#79314 = DIRECTION('ref_axis',(0.,0.,-1.)) ;
#79315 = DIRECTION('center_axis',(3.65204942310907E-15,-1.,1.22867065825113E-46)) ;
#79316 = DIRECTION('ref_axis',(1.,3.65204942310907E-15,3.45446742203778E-76)) ;
#79317 = DIRECTION('center_axis',(0.,-1.,0.)) ;
#79318 = DIRECTION('ref_axis',(0.,0.,-1.)) ;
#79319 = DIRECTION('center_axis',(-3.65204942310907E-15,1.,7.70988211545247E-16)) ;
#79320 = DIRECTION('ref_axis',(-1.,-3.65204942310907E-15,5.2794132247463E-31)) ;
#79321 = DIRECTION('center_axis',(0.,-1.,0.)) ;
#79322 = DIRECTION('ref_axis',(0.,0.,-1.)) ;
#79323 = DIRECTION('center_axis',(1.,3.49148133884313E-15,5.4907029126972E-31)) ;
#79324 = DIRECTION('ref_axis',(-3.49148133884313E-15,1.,-1.91706867568139E-45)) ;
#79325 = DIRECTION('center_axis',(1.,0.,0.)) ;
#79326 = DIRECTION('ref_axis',(0.,0.,-1.)) ;
#79327 = DIRECTION('center_axis',(0.,1.,0.)) ;
#79328 = DIRECTION('ref_axis',(1.,0.,0.)) ;
#79329 = DIRECTION('center_axis',(4.62592926927157E-14,0.,-1.)) ;
#79330 = DIRECTION('ref_axis',(1.,0.,4.62592926927157E-14)) ;
#79331 = DIRECTION('center_axis',(0.,1.,0.)) ;
#79332 = DIRECTION('ref_axis',(1.,0.,0.)) ;
#79333 = DIRECTION('center_axis',(0.,0.,1.)) ;
#79334 = DIRECTION('ref_axis',(-1.,0.,0.)) ;
#79335 = DIRECTION('center_axis',(1.03517906367563E-32,1.81408990951823E-16,
-1.)) ;
#79336 = DIRECTION('ref_axis',(-1.73199155682659E-62,1.,1.81408990951823E-16)) ;
#79337 = DIRECTION('axis',(0.,0.,1.)) ;
#79338 = DIRECTION('refdir',(1.,0.,0.)) ;
#79339 = DIRECTION('center_axis',(0.967224433265373,0.251696850907845,0.0335498276829)) ;
#79340 = DIRECTION('ref_axis',(0.148186156389733,-0.666803895723232,0.730351578147647)) ;
#79341 = DIRECTION('center_axis',(0.,0.707106781186549,-0.707106781186547)) ;
#79342 = DIRECTION('ref_axis',(0.,0.707106781186546,0.707106781186549)) ;
#79343 = DIRECTION('center_axis',(0.978007532938554,-0.147978541149823,-0.146981688909242)) ;
#79344 = DIRECTION('ref_axis',(0.193734423938406,0.383507624685863,0.902988856403589)) ;
#79345 = DIRECTION('center_axis',(0.,0.447213595499958,0.894427190999916)) ;
#79346 = DIRECTION('ref_axis',(0.,-0.894427190999916,0.447213595499958)) ;
#79347 = DIRECTION('center_axis',(0.960001452008132,0.250435160947733,-0.125217579849484)) ;
#79348 = DIRECTION('ref_axis',(0.276742394167923,-0.916645079799563,0.288401534235619)) ;
#79349 = DIRECTION('center_axis',(0.,1.,0.)) ;
#79350 = DIRECTION('ref_axis',(0.,0.,1.)) ;
#79351 = DIRECTION('center_axis',(-1.,0.,0.)) ;
#79352 = DIRECTION('ref_axis',(0.,0.413905171642071,-0.910320003563553)) ;
#79353 = DIRECTION('center_axis',(1.,1.44560289664734E-16,0.)) ;
#79354 = DIRECTION('ref_axis',(0.,1.,0.)) ;
#79355 = DIRECTION('center_axis',(1.,1.44560289664734E-16,0.)) ;
#79356 = DIRECTION('ref_axis',(-1.44560289664734E-16,1.,0.)) ;
#79357 = DIRECTION('center_axis',(-1.77035296021731E-32,1.22464679914735E-16,
-1.)) ;
#79358 = DIRECTION('ref_axis',(0.,-1.,-1.22464679914735E-16)) ;
#79359 = DIRECTION('center_axis',(-1.,-1.44560289664734E-16,0.)) ;
#79360 = DIRECTION('ref_axis',(-1.44560289664734E-16,1.,0.)) ;
#79361 = DIRECTION('center_axis',(1.,-3.46944695195361E-16,0.)) ;
#79362 = DIRECTION('ref_axis',(2.61228946970625E-16,1.,0.)) ;
#79363 = DIRECTION('center_axis',(1.,-3.46944695195361E-16,0.)) ;
#79364 = DIRECTION('ref_axis',(3.46944695195361E-16,1.,0.)) ;
#79365 = DIRECTION('center_axis',(-4.24884710452153E-32,-1.22464679914735E-16,
1.)) ;
#79366 = DIRECTION('ref_axis',(-3.26536183713281E-16,-1.,-1.22464679914735E-16)) ;
#79367 = DIRECTION('center_axis',(-1.,3.46944695195361E-16,0.)) ;
#79368 = DIRECTION('ref_axis',(3.46944695195361E-16,1.,0.)) ;
#79369 = DIRECTION('center_axis',(-1.,3.46944695195361E-16,0.)) ;
#79370 = DIRECTION('ref_axis',(-3.46944695195361E-16,-1.,0.)) ;
#79371 = DIRECTION('center_axis',(-1.,0.,0.)) ;
#79372 = DIRECTION('ref_axis',(0.,0.,1.)) ;
#79373 = DIRECTION('',(1.,-3.46944695195361E-16,0.)) ;
#79374 = DIRECTION('center_axis',(-1.,8.01625584951926E-16,-1.08420217248551E-15)) ;
#79375 = DIRECTION('ref_axis',(1.08420217248551E-15,-1.92678538844662E-45,
-1.)) ;
#79376 = DIRECTION('center_axis',(-1.,8.01625584951926E-16,-1.08420217248551E-15)) ;
#79377 = DIRECTION('ref_axis',(1.08420217248551E-15,-1.92678538844662E-45,
-1.)) ;
#79378 = DIRECTION('',(-1.,3.46944695195361E-16,0.)) ;
#79379 = DIRECTION('center_axis',(-1.,3.46944695195361E-16,0.)) ;
#79380 = DIRECTION('ref_axis',(-3.46944695195361E-16,-1.,0.)) ;
#79381 = DIRECTION('center_axis',(-1.,0.,0.)) ;
#79382 = DIRECTION('ref_axis',(0.,0.,1.)) ;
#79383 = DIRECTION('',(1.,-3.46944695195361E-16,0.)) ;
#79384 = DIRECTION('center_axis',(-1.,2.2680138501079E-15,0.)) ;
#79385 = DIRECTION('ref_axis',(2.2680138501079E-15,1.,0.)) ;
#79386 = DIRECTION('',(-1.,3.46944695195361E-16,0.)) ;
#79387 = DIRECTION('center_axis',(-1.,3.18032637262401E-16,0.)) ;
#79388 = DIRECTION('ref_axis',(-5.55111512312578E-16,-1.,0.)) ;
#79389 = DIRECTION('center_axis',(1.,-3.18032637262401E-16,0.)) ;
#79390 = DIRECTION('ref_axis',(-3.18032637262401E-16,-1.,0.)) ;
#79391 = DIRECTION('center_axis',(-2.01298417874256E-16,-0.632948931301568,
-0.774193548387096)) ;
#79392 = DIRECTION('ref_axis',(1.73472347597681E-14,-0.774193548387096,0.632948931301568)) ;
#79393 = DIRECTION('center_axis',(-1.,3.18032637262401E-16,0.)) ;
#79394 = DIRECTION('ref_axis',(-3.18032637262401E-16,-1.,0.)) ;
#79395 = DIRECTION('center_axis',(-2.01298417874256E-16,-0.632948931301568,
0.774193548387096)) ;
#79396 = DIRECTION('ref_axis',(9.63584817660562E-32,-0.774193548387096,-0.632948931301568)) ;
#79397 = DIRECTION('center_axis',(1.,1.44560289664734E-16,0.)) ;
#79398 = DIRECTION('ref_axis',(-1.44560289664734E-16,1.,0.)) ;
#79399 = DIRECTION('',(-1.,-1.44560289664734E-16,0.)) ;
#79400 = DIRECTION('center_axis',(-1.,3.46944695195361E-16,0.)) ;
#79401 = DIRECTION('ref_axis',(-3.46944695195361E-16,-1.,0.)) ;
#79402 = DIRECTION('',(-1.,3.46944695195361E-16,0.)) ;
#79403 = DIRECTION('center_axis',(-1.,3.46944695195361E-16,0.)) ;
#79404 = DIRECTION('ref_axis',(3.46944695195361E-16,1.,3.5527136788005E-15)) ;
#79405 = DIRECTION('center_axis',(-1.,3.46944695195361E-16,0.)) ;
#79406 = DIRECTION('ref_axis',(3.46944695195361E-16,1.,0.)) ;
#79407 = DIRECTION('center_axis',(-1.,3.46944695195361E-16,0.)) ;
#79408 = DIRECTION('ref_axis',(-3.46944695195361E-16,-1.,0.)) ;
#79409 = DIRECTION('',(1.,-3.46944695195361E-16,0.)) ;
#79410 = DIRECTION('center_axis',(-1.,-1.44560289664734E-16,-2.65552944032596E-32)) ;
#79411 = DIRECTION('ref_axis',(1.44560289664734E-16,-1.,-2.80018320648271E-64)) ;
#79412 = DIRECTION('',(2.65552944032596E-32,3.29043518662928E-48,-1.)) ;
#79413 = DIRECTION('',(1.44560289664734E-16,-1.,-2.4093381610789E-16)) ;
#79414 = DIRECTION('',(0.,0.,1.)) ;
#79415 = DIRECTION('center_axis',(0.999999956301289,0.000282786981229719,
8.61913163152323E-5)) ;
#79416 = DIRECTION('ref_axis',(0.000288266391063448,-0.997396273403499,-0.0721151211834231)) ;
#79417 = DIRECTION('',(-1.44560289664734E-16,1.,-7.2280144832367E-17)) ;
#79418 = DIRECTION('center_axis',(0.316227766016838,0.948683298050514,0.)) ;
#79419 = DIRECTION('ref_axis',(-0.948683298050514,0.316227766016838,0.)) ;
#79420 = DIRECTION('',(-0.948683298050514,0.316227766016838,0.)) ;
#79421 = DIRECTION('',(0.,0.,1.)) ;
#79422 = DIRECTION('',(0.937042571331636,-0.312347523777212,-0.156173761888606)) ;
#79423 = DIRECTION('',(0.,0.,-1.)) ;
#79424 = DIRECTION('center_axis',(1.,1.73472347597681E-15,0.)) ;
#79425 = DIRECTION('ref_axis',(-1.73472347597681E-15,1.,0.)) ;
#79426 = DIRECTION('',(-1.73472347597681E-15,1.,0.)) ;
#79427 = DIRECTION('',(0.,0.,1.)) ;
#79428 = DIRECTION('',(1.73472347597681E-15,-1.,-2.89120579329468E-16)) ;
#79429 = DIRECTION('',(0.,0.,-1.)) ;
#79430 = DIRECTION('center_axis',(0.164398987305357,-0.986393923832144,0.)) ;
#79431 = DIRECTION('ref_axis',(0.986393923832144,0.164398987305357,0.)) ;
#79432 = DIRECTION('',(-0.973328526784575,-0.162221421130762,0.162221421130763)) ;
#79433 = DIRECTION('',(0.,0.,-1.)) ;
#79434 = DIRECTION('',(0.986393923832144,0.164398987305357,0.)) ;
#79435 = DIRECTION('',(0.,0.,1.)) ;
#79436 = DIRECTION('center_axis',(-9.91270557701033E-17,1.,0.)) ;
#79437 = DIRECTION('ref_axis',(-1.,-9.91270557701033E-17,0.)) ;
#79438 = DIRECTION('',(1.,9.91270557701033E-17,0.)) ;
#79439 = DIRECTION('',(0.,0.,-1.)) ;
#79440 = DIRECTION('',(-1.,-9.91270557701033E-17,0.)) ;
#79441 = DIRECTION('',(0.,0.,1.)) ;
#79442 = DIRECTION('center_axis',(-9.91270557701033E-17,1.,0.)) ;
#79443 = DIRECTION('ref_axis',(-1.,-9.91270557701033E-17,0.)) ;
#79444 = DIRECTION('',(-1.,-9.91270557701033E-17,0.)) ;
#79445 = DIRECTION('',(0.,0.,-1.)) ;
#79446 = DIRECTION('',(-1.,-9.91270557701033E-17,0.)) ;
#79447 = DIRECTION('',(0.,0.,1.)) ;
#79448 = DIRECTION('center_axis',(1.,1.15648231731787E-15,0.)) ;
#79449 = DIRECTION('ref_axis',(-1.15648231731787E-15,1.,0.)) ;
#79450 = DIRECTION('',(-1.15648231731787E-15,1.,0.)) ;
#79451 = DIRECTION('',(0.,0.,-1.)) ;
#79452 = DIRECTION('',(-1.15648231731787E-15,1.,0.)) ;
#79453 = DIRECTION('',(0.,0.,1.)) ;
#79454 = DIRECTION('center_axis',(-1.,-1.15648231731787E-15,0.)) ;
#79455 = DIRECTION('ref_axis',(-1.15648231731787E-15,1.,1.77635683940025E-15)) ;
#79456 = DIRECTION('',(0.,0.,1.)) ;
#79457 = DIRECTION('center_axis',(0.,0.,1.)) ;
#79458 = DIRECTION('ref_axis',(1.,0.,0.)) ;
#79459 = DIRECTION('',(-1.,0.,0.)) ;
#79460 = DIRECTION('center_axis',(0.,0.,-1.)) ;
#79461 = DIRECTION('ref_axis',(1.,0.,0.)) ;
#79462 = DIRECTION('center_axis',(0.,0.,-1.)) ;
#79463 = DIRECTION('ref_axis',(1.,0.,0.)) ;
#79464 = DIRECTION('center_axis',(0.,0.,-1.)) ;
#79465 = DIRECTION('ref_axis',(1.,0.,0.)) ;
#79466 = DIRECTION('center_axis',(0.,0.,-1.)) ;
#79467 = DIRECTION('ref_axis',(1.,0.,0.)) ;
#79468 = DIRECTION('',(1.,0.,0.)) ;
#79469 = DIRECTION('center_axis',(0.,0.,1.)) ;
#79470 = DIRECTION('ref_axis',(1.,0.,0.)) ;
#79471 = DIRECTION('',(3.46944695195361E-16,1.,0.)) ;
#79472 = DIRECTION('center_axis',(0.,0.,1.)) ;
#79473 = DIRECTION('ref_axis',(1.,0.,0.)) ;
#79474 = DIRECTION('',(1.,-3.46944695195361E-16,0.)) ;
#79475 = DIRECTION('center_axis',(0.,0.,-1.)) ;
#79476 = DIRECTION('ref_axis',(1.,0.,0.)) ;
#79477 = DIRECTION('',(2.71050543121376E-16,1.,0.)) ;
#79478 = DIRECTION('center_axis',(0.,0.,-1.)) ;
#79479 = DIRECTION('ref_axis',(1.,0.,0.)) ;
#79480 = DIRECTION('',(-1.,3.46944695195361E-16,0.)) ;
#79481 = DIRECTION('center_axis',(0.,0.,1.)) ;
#79482 = DIRECTION('ref_axis',(1.,0.,0.)) ;
#79483 = DIRECTION('',(3.46944695195361E-16,1.,0.)) ;
#79484 = DIRECTION('center_axis',(0.,0.,1.)) ;
#79485 = DIRECTION('ref_axis',(1.,0.,0.)) ;
#79486 = DIRECTION('center_axis',(0.,0.,-1.)) ;
#79487 = DIRECTION('ref_axis',(1.,0.,0.)) ;
#79488 = DIRECTION('',(0.986393923832144,-0.164398987305354,0.)) ;
#79489 = DIRECTION('center_axis',(0.,0.,-1.)) ;
#79490 = DIRECTION('ref_axis',(1.,-6.50521303491307E-15,0.)) ;
#79491 = DIRECTION('center_axis',(0.,0.,-1.)) ;
#79492 = DIRECTION('ref_axis',(1.,0.,0.)) ;
#79493 = DIRECTION('',(1.,0.,0.)) ;
#79494 = DIRECTION('',(1.13380619344889E-16,-1.,0.)) ;
#79495 = DIRECTION('center_axis',(0.,0.,-1.)) ;
#79496 = DIRECTION('ref_axis',(1.,0.,0.)) ;
#79497 = DIRECTION('',(-1.,-1.92747052886312E-16,0.)) ;
#79498 = DIRECTION('center_axis',(0.,0.,1.)) ;
#79499 = DIRECTION('ref_axis',(1.,0.,0.)) ;
#79500 = DIRECTION('',(0.,-1.,0.)) ;
#79501 = DIRECTION('center_axis',(0.,0.,-1.)) ;
#79502 = DIRECTION('ref_axis',(1.,0.,0.)) ;
#79503 = DIRECTION('center_axis',(0.,0.,1.)) ;
#79504 = DIRECTION('ref_axis',(1.,0.,0.)) ;
#79505 = DIRECTION('',(-0.948683298050514,0.316227766016838,0.)) ;
#79506 = DIRECTION('center_axis',(0.,0.,1.)) ;
#79507 = DIRECTION('ref_axis',(1.,0.,0.)) ;
#79508 = DIRECTION('',(-1.,0.,0.)) ;
#79509 = DIRECTION('center_axis',(0.,0.,1.)) ;
#79510 = DIRECTION('ref_axis',(1.,0.,0.)) ;
#79511 = DIRECTION('',(0.,-1.,0.)) ;
#79512 = DIRECTION('center_axis',(0.,0.,-1.)) ;
#79513 = DIRECTION('ref_axis',(1.,0.,0.)) ;
#79514 = DIRECTION('',(-1.,-1.92747052886312E-16,0.)) ;
#79515 = DIRECTION('center_axis',(0.,0.,1.)) ;
#79516 = DIRECTION('ref_axis',(1.,0.,0.)) ;
#79517 = DIRECTION('',(1.13380619344889E-16,-1.,0.)) ;
#79518 = DIRECTION('',(1.,0.,0.)) ;
#79519 = DIRECTION('center_axis',(0.,0.,1.)) ;
#79520 = DIRECTION('ref_axis',(1.,0.,0.)) ;
#79521 = DIRECTION('center_axis',(0.,0.,1.)) ;
#79522 = DIRECTION('ref_axis',(1.,0.,0.)) ;
#79523 = DIRECTION('',(-0.986393923832144,0.164398987305354,0.)) ;
#79524 = DIRECTION('center_axis',(0.,0.,1.)) ;
#79525 = DIRECTION('ref_axis',(1.,0.,0.)) ;
#79526 = DIRECTION('center_axis',(0.,0.,-1.)) ;
#79527 = DIRECTION('ref_axis',(1.,0.,0.)) ;
#79528 = DIRECTION('',(-3.46944695195361E-16,-1.,0.)) ;
#79529 = DIRECTION('center_axis',(0.,0.,-1.)) ;
#79530 = DIRECTION('ref_axis',(1.,0.,0.)) ;
#79531 = DIRECTION('',(-1.,3.46944695195361E-16,0.)) ;
#79532 = DIRECTION('center_axis',(0.,0.,1.)) ;
#79533 = DIRECTION('ref_axis',(1.,0.,0.)) ;
#79534 = DIRECTION('',(3.46944695195361E-16,1.,0.)) ;
#79535 = DIRECTION('center_axis',(0.,0.,1.)) ;
#79536 = DIRECTION('ref_axis',(1.,0.,0.)) ;
#79537 = DIRECTION('',(1.,-3.46944695195361E-16,0.)) ;
#79538 = DIRECTION('center_axis',(0.,0.,-1.)) ;
#79539 = DIRECTION('ref_axis',(1.,0.,0.)) ;
#79540 = DIRECTION('',(-3.46944695195361E-16,-1.,0.)) ;
#79541 = DIRECTION('center_axis',(0.,0.,-1.)) ;
#79542 = DIRECTION('ref_axis',(1.,0.,0.)) ;
#79543 = DIRECTION('',(1.,0.,0.)) ;
#79544 = DIRECTION('center_axis',(0.,0.,1.)) ;
#79545 = DIRECTION('ref_axis',(1.,0.,0.)) ;
#79546 = DIRECTION('',(0.986393923832144,0.164398987305357,0.)) ;
#79547 = DIRECTION('center_axis',(0.,0.,1.)) ;
#79548 = DIRECTION('ref_axis',(1.,0.,0.)) ;
#79549 = DIRECTION('',(-1.73472347597681E-15,1.,0.)) ;
#79550 = DIRECTION('center_axis',(0.,0.,1.)) ;
#79551 = DIRECTION('ref_axis',(1.,0.,0.)) ;
#79552 = DIRECTION('center_axis',(-1.92747052886312E-16,1.,0.)) ;
#79553 = DIRECTION('ref_axis',(-1.,-1.92747052886312E-16,0.)) ;
#79554 = DIRECTION('',(0.,0.,1.)) ;
#79555 = DIRECTION('',(0.,0.,-1.)) ;
#79556 = DIRECTION('center_axis',(-1.,0.,0.)) ;
#79557 = DIRECTION('ref_axis',(0.,0.,1.)) ;
#79558 = DIRECTION('',(0.,0.,1.)) ;
#79559 = DIRECTION('',(0.,0.,-1.)) ;
#79560 = DIRECTION('center_axis',(0.,1.,0.)) ;
#79561 = DIRECTION('ref_axis',(0.,0.,1.)) ;
#79562 = DIRECTION('',(0.,0.,-1.)) ;
#79563 = DIRECTION('',(0.,0.,1.)) ;
#79564 = DIRECTION('',(0.,0.,-1.)) ;
#79565 = DIRECTION('',(0.,0.,-1.)) ;
#79566 = DIRECTION('center_axis',(0.316227766016838,0.948683298050514,0.)) ;
#79567 = DIRECTION('ref_axis',(-0.948683298050514,0.316227766016838,0.)) ;
#79568 = DIRECTION('center_axis',(-0.316227766016857,-0.948683298050507,-2.6817125824357E-14)) ;
#79569 = DIRECTION('ref_axis',(0.831595960762403,-0.277198653587473,-0.481257794215271)) ;
#79570 = DIRECTION('',(0.,0.,1.)) ;
#79571 = DIRECTION('',(0.,0.,-1.)) ;
#79572 = DIRECTION('',(-0.937042571331636,0.312347523777212,-0.156173761888606)) ;
#79573 = DIRECTION('center_axis',(1.,1.73472347597681E-15,0.)) ;
#79574 = DIRECTION('ref_axis',(-1.73472347597681E-15,1.,0.)) ;
#79575 = DIRECTION('',(-1.73472347597681E-15,1.,-2.89120579329468E-16)) ;
#79576 = DIRECTION('',(0.,0.,1.)) ;
#79577 = DIRECTION('',(0.,0.,-1.)) ;
#79578 = DIRECTION('center_axis',(0.164398987305357,-0.986393923832144,0.)) ;
#79579 = DIRECTION('ref_axis',(0.986393923832144,0.164398987305357,0.)) ;
#79580 = DIRECTION('',(0.973328526784575,0.162221421130762,0.162221421130763)) ;
#79581 = DIRECTION('',(0.,0.,1.)) ;
#79582 = DIRECTION('',(0.,0.,-1.)) ;
#79583 = DIRECTION('center_axis',(0.,-1.,0.)) ;
#79584 = DIRECTION('ref_axis',(0.,0.,-1.)) ;
#79585 = DIRECTION('',(0.,0.,1.)) ;
#79586 = DIRECTION('',(0.,0.,1.)) ;
#79587 = DIRECTION('',(0.,0.,1.)) ;
#79588 = DIRECTION('',(0.,0.,-1.)) ;
#79589 = DIRECTION('',(1.,0.,2.25271179641597E-31)) ;
#79590 = DIRECTION('center_axis',(0.,-1.,0.)) ;
#79591 = DIRECTION('ref_axis',(0.,0.,-1.)) ;
#79592 = DIRECTION('',(0.,0.,-1.)) ;
#79593 = DIRECTION('center_axis',(0.,-1.,0.)) ;
#79594 = DIRECTION('ref_axis',(0.,0.,-1.)) ;
#79595 = DIRECTION('',(-1.,0.,-3.21815970916568E-32)) ;
#79596 = DIRECTION('',(0.,0.,-1.)) ;
#79597 = DIRECTION('center_axis',(1.,-3.46944695195361E-16,0.)) ;
#79598 = DIRECTION('ref_axis',(3.46944695195361E-16,1.,0.)) ;
#79599 = DIRECTION('center_axis',(1.,-3.46944695195361E-16,0.)) ;
#79600 = DIRECTION('ref_axis',(3.46944695195361E-16,1.,0.)) ;
#79601 = DIRECTION('',(1.5529910948782E-31,4.47619207437002E-16,-1.)) ;
#79602 = DIRECTION('',(0.,0.,1.)) ;
#79603 = DIRECTION('center_axis',(1.,-3.46944695195361E-16,0.)) ;
#79604 = DIRECTION('ref_axis',(3.46944695195361E-16,1.,0.)) ;
#79605 = DIRECTION('center_axis',(1.,-3.46944695195361E-16,0.)) ;
#79606 = DIRECTION('ref_axis',(3.46944695195361E-16,1.,0.)) ;
#79607 = DIRECTION('center_axis',(1.,-3.46944695195361E-16,0.)) ;
#79608 = DIRECTION('ref_axis',(3.46944695195361E-16,1.,0.)) ;
#79609 = DIRECTION('',(3.46944695195361E-16,1.,9.27571383489107E-17)) ;
#79610 = DIRECTION('',(0.,0.,1.)) ;
#79611 = DIRECTION('',(-3.46944695195361E-16,-1.,-6.49299968442375E-16)) ;
#79612 = DIRECTION('center_axis',(1.,-3.46944695195361E-16,0.)) ;
#79613 = DIRECTION('ref_axis',(3.46944695195361E-16,1.,0.)) ;
#79614 = DIRECTION('center_axis',(1.,-3.46944695195361E-16,0.)) ;
#79615 = DIRECTION('ref_axis',(3.46944695195361E-16,1.,0.)) ;
#79616 = DIRECTION('center_axis',(1.,-3.46944695195361E-16,0.)) ;
#79617 = DIRECTION('ref_axis',(3.46944695195361E-16,1.,0.)) ;
#79618 = DIRECTION('',(0.,0.,1.)) ;
#79619 = DIRECTION('',(-1.5529910948782E-31,-4.47619207437002E-16,-1.)) ;
#79620 = DIRECTION('center_axis',(1.,-3.46944695195361E-16,0.)) ;
#79621 = DIRECTION('ref_axis',(3.46944695195361E-16,1.,0.)) ;
#79622 = DIRECTION('center_axis',(1.,-3.46944695195361E-16,0.)) ;
#79623 = DIRECTION('ref_axis',(3.46944695195361E-16,1.,0.)) ;
#79624 = DIRECTION('center_axis',(1.,-3.46944695195361E-16,0.)) ;
#79625 = DIRECTION('ref_axis',(3.46944695195361E-16,1.,0.)) ;
#79626 = DIRECTION('',(-3.46944695195361E-16,-1.,-1.06487173641454E-15)) ;
#79627 = DIRECTION('center_axis',(1.,-3.46944695195361E-16,0.)) ;
#79628 = DIRECTION('ref_axis',(3.46944695195361E-16,1.,0.)) ;
#79629 = DIRECTION('',(3.46944695195361E-16,1.,2.45739631480277E-16)) ;
#79630 = DIRECTION('center_axis',(1.,-3.46944695195361E-16,0.)) ;
#79631 = DIRECTION('ref_axis',(3.46944695195361E-16,1.,0.)) ;
#79632 = DIRECTION('center_axis',(1.,-3.46944695195361E-16,0.)) ;
#79633 = DIRECTION('ref_axis',(3.46944695195361E-16,1.,0.)) ;
#79634 = DIRECTION('center_axis',(0.,-1.,0.)) ;
#79635 = DIRECTION('ref_axis',(0.,0.,-1.)) ;
#79636 = DIRECTION('center_axis',(0.,-1.,0.)) ;
#79637 = DIRECTION('ref_axis',(0.,0.,-1.)) ;
#79638 = DIRECTION('',(-1.,0.,-1.40488587213121E-32)) ;
#79639 = DIRECTION('',(0.,0.,1.)) ;
#79640 = DIRECTION('',(0.,0.,1.)) ;
#79641 = DIRECTION('',(0.,0.,1.)) ;
#79642 = DIRECTION('',(1.,0.,1.40488587213121E-32)) ;
#79643 = DIRECTION('center_axis',(0.,-1.,0.)) ;
#79644 = DIRECTION('ref_axis',(0.,0.,-1.)) ;
#79645 = DIRECTION('',(7.2280144832367E-17,0.,-1.)) ;
#79646 = DIRECTION('center_axis',(-1.,-1.13380619344889E-16,0.)) ;
#79647 = DIRECTION('ref_axis',(1.13380619344889E-16,-1.,0.)) ;
#79648 = DIRECTION('center_axis',(-1.,-1.13380619344889E-16,0.)) ;
#79649 = DIRECTION('ref_axis',(1.13380619344889E-16,-1.,0.)) ;
#79650 = DIRECTION('',(1.13380619344889E-16,-1.,1.23908819712629E-16)) ;
#79651 = DIRECTION('',(0.,0.,-1.)) ;
#79652 = DIRECTION('',(-1.13380619344889E-16,1.,-1.23908819712629E-16)) ;
#79653 = DIRECTION('center_axis',(-1.,-1.13380619344889E-16,0.)) ;
#79654 = DIRECTION('ref_axis',(1.13380619344889E-16,-1.,0.)) ;
#79655 = DIRECTION('',(0.,0.,1.)) ;
#79656 = DIRECTION('center_axis',(-1.40488587213121E-32,1.23908819712629E-16,
1.)) ;
#79657 = DIRECTION('ref_axis',(0.,-1.,1.23908819712629E-16)) ;
#79658 = DIRECTION('',(-1.,0.,-1.40488587213121E-32)) ;
#79659 = DIRECTION('',(-1.13380619344889E-16,1.,-1.23908819712629E-16)) ;
#79660 = DIRECTION('center_axis',(1.40488587213121E-32,-1.23908819712629E-16,
-1.)) ;
#79661 = DIRECTION('ref_axis',(-1.74077750246726E-48,-1.,1.23908819712629E-16)) ;
#79662 = DIRECTION('center_axis',(1.40488587213121E-32,-1.23908819712629E-16,
-1.)) ;
#79663 = DIRECTION('ref_axis',(0.,1.,-1.23908819712629E-16)) ;
#79664 = DIRECTION('center_axis',(-1.40488587213121E-32,1.23908819712629E-16,
1.)) ;
#79665 = DIRECTION('ref_axis',(1.74077750246726E-48,1.,-1.23908819712629E-16)) ;
#79666 = DIRECTION('',(1.13380619344889E-16,-1.,1.23908819712629E-16)) ;
#79667 = DIRECTION('',(1.,0.,1.40488587213121E-32)) ;
#79668 = DIRECTION('center_axis',(-1.,-1.23908819712629E-16,-8.95614743483648E-33)) ;
#79669 = DIRECTION('ref_axis',(1.23908819712629E-16,-1.,5.38566640001825E-66)) ;
#79670 = DIRECTION('',(-8.95614743483648E-33,-1.10974565782288E-48,1.)) ;
#79671 = DIRECTION('',(1.23908819712629E-16,-1.,7.2280144832367E-17)) ;
#79672 = DIRECTION('',(-8.95614743483648E-33,0.,1.)) ;
#79673 = DIRECTION('',(-1.23908819712629E-16,1.,-1.23908819712629E-16)) ;
#79674 = DIRECTION('',(8.95614743483648E-33,1.0154535431059E-48,-1.)) ;
#79675 = DIRECTION('',(1.23908819712629E-16,-1.,1.23908819712629E-16)) ;
#79676 = DIRECTION('',(-8.95614743483648E-33,0.,1.)) ;
#79677 = DIRECTION('',(-1.23908819712629E-16,1.,2.4093381610789E-16)) ;
#79678 = DIRECTION('center_axis',(-1.7912294869673E-32,7.2280144832367E-17,
1.)) ;
#79679 = DIRECTION('ref_axis',(0.,-1.,7.2280144832367E-17)) ;
#79680 = DIRECTION('',(-1.23908819712629E-16,1.,-7.2280144832367E-17)) ;
#79681 = DIRECTION('',(1.,1.23908819712629E-16,8.95614743483648E-33)) ;
#79682 = DIRECTION('',(1.44560289664734E-16,-1.,7.2280144832367E-17)) ;
#79683 = DIRECTION('',(-1.,0.,-1.7912294869673E-32)) ;
#79684 = DIRECTION('center_axis',(-2.08976773479518E-32,2.4093381610789E-16,
-1.)) ;
#79685 = DIRECTION('ref_axis',(0.,1.,2.4093381610789E-16)) ;
#79686 = DIRECTION('',(-1.44560289664734E-16,1.,2.4093381610789E-16)) ;
#79687 = DIRECTION('',(-1.,-1.23908819712629E-16,-8.95614743483648E-33)) ;
#79688 = DIRECTION('',(1.23908819712629E-16,-1.,-2.4093381610789E-16)) ;
#79689 = DIRECTION('',(1.,0.,-2.08976773479518E-32)) ;
#79690 = DIRECTION('center_axis',(-1.23908819712629E-16,1.,0.)) ;
#79691 = DIRECTION('ref_axis',(-1.,-1.23908819712629E-16,0.)) ;
#79692 = DIRECTION('',(8.95614743483648E-33,1.10974565782288E-48,-1.)) ;
#79693 = DIRECTION('',(1.,1.23908819712629E-16,8.95614743483648E-33)) ;
#79694 = DIRECTION('',(-2.65552944032596E-32,-3.29043518662928E-48,1.)) ;
#79695 = DIRECTION('',(-1.,-1.23908819712629E-16,-8.95614743483648E-33)) ;
#79696 = DIRECTION('center_axis',(-1.,-1.44560289664734E-16,-2.65552944032596E-32)) ;
#79697 = DIRECTION('ref_axis',(1.44560289664734E-16,-1.,-2.80018320648271E-64)) ;
#79698 = DIRECTION('',(1.44560289664734E-16,-1.,-2.4093381610789E-16)) ;
#79699 = DIRECTION('',(-2.65552944032596E-32,0.,1.)) ;
#79700 = DIRECTION('',(-1.44560289664734E-16,1.,-7.2280144832367E-17)) ;
#79701 = DIRECTION('',(0.,0.,-1.)) ;
#79702 = DIRECTION('center_axis',(0.,1.,0.)) ;
#79703 = DIRECTION('ref_axis',(0.,0.,1.)) ;
#79704 = DIRECTION('',(8.95614743483648E-33,0.,-1.)) ;
#79705 = DIRECTION('',(1.,0.,1.40488587213121E-32)) ;
#79706 = DIRECTION('',(-7.2280144832367E-17,0.,1.)) ;
#79707 = DIRECTION('',(-1.,0.,-1.40488587213121E-32)) ;
#79708 = DIRECTION('',(8.95614743483648E-33,0.,-1.)) ;
#79709 = DIRECTION('',(1.,0.,1.7912294869673E-32)) ;
#79710 = DIRECTION('',(2.65552944032596E-32,0.,-1.)) ;
#79711 = DIRECTION('',(-1.,0.,2.08976773479518E-32)) ;
#79712 = DIRECTION('center_axis',(1.,1.44560289664734E-16,0.)) ;
#79713 = DIRECTION('ref_axis',(-1.44560289664734E-16,1.,0.)) ;
#79714 = DIRECTION('',(1.44560289664734E-16,-1.,0.)) ;
#79715 = DIRECTION('center_axis',(-1.,-1.44560289664734E-16,0.)) ;
#79716 = DIRECTION('ref_axis',(-1.44560289664734E-16,1.,-4.33680868994201E-15)) ;
#79717 = DIRECTION('',(0.,0.,-1.)) ;
#79718 = DIRECTION('center_axis',(-1.,-1.44560289664734E-16,0.)) ;
#79719 = DIRECTION('ref_axis',(-1.44560289664734E-16,1.,0.)) ;
#79720 = DIRECTION('',(1.44560289664734E-16,-1.,0.)) ;
#79721 = DIRECTION('center_axis',(-1.,-1.44560289664734E-16,0.)) ;
#79722 = DIRECTION('ref_axis',(-1.44560289664734E-16,1.,0.)) ;
#79723 = DIRECTION('',(0.,0.,1.)) ;
#79724 = DIRECTION('center_axis',(-1.,-1.44560289664734E-16,0.)) ;
#79725 = DIRECTION('ref_axis',(-1.44560289664734E-16,1.,0.)) ;
#79726 = DIRECTION('center_axis',(1.,-3.46944695195361E-16,0.)) ;
#79727 = DIRECTION('ref_axis',(3.46944695195361E-16,1.,0.)) ;
#79728 = DIRECTION('center_axis',(1.,-3.46944695195361E-16,0.)) ;
#79729 = DIRECTION('ref_axis',(3.46944695195361E-16,1.,0.)) ;
#79730 = DIRECTION('',(0.,0.,-1.)) ;
#79731 = DIRECTION('',(-1.5529910948782E-31,-4.47619207437002E-16,1.)) ;
#79732 = DIRECTION('center_axis',(-1.,3.46944695195361E-16,0.)) ;
#79733 = DIRECTION('ref_axis',(3.46944695195361E-16,1.,-1.77635683940025E-15)) ;
#79734 = DIRECTION('',(-3.46944695195361E-16,-1.,-2.45739631480277E-16)) ;
#79735 = DIRECTION('center_axis',(1.,-3.46944695195361E-16,0.)) ;
#79736 = DIRECTION('ref_axis',(3.46944695195361E-16,1.,0.)) ;
#79737 = DIRECTION('center_axis',(3.46944695195361E-16,1.,4.47619207437002E-16)) ;
#79738 = DIRECTION('ref_axis',(-8.18685017503995E-48,-4.47619207437002E-16,
1.)) ;
#79739 = DIRECTION('',(-1.5529910948782E-31,-4.47619207437002E-16,1.)) ;
#79740 = DIRECTION('',(-1.,3.46944695195361E-16,0.)) ;
#79741 = DIRECTION('',(1.5529910948782E-31,4.47619207437002E-16,-1.)) ;
#79742 = DIRECTION('center_axis',(-8.52580615413453E-32,-2.45739631480277E-16,
1.)) ;
#79743 = DIRECTION('ref_axis',(0.,-1.,-2.45739631480277E-16)) ;
#79744 = DIRECTION('',(1.,-3.46944695195361E-16,0.)) ;
#79745 = DIRECTION('',(-3.46944695195361E-16,-1.,-2.45739631480277E-16)) ;
#79746 = DIRECTION('',(3.46944695195361E-16,1.,2.45739631480277E-16)) ;
#79747 = DIRECTION('center_axis',(1.,-3.46944695195361E-16,0.)) ;
#79748 = DIRECTION('ref_axis',(3.46944695195361E-16,1.,0.)) ;
#79749 = DIRECTION('center_axis',(1.,-3.46944695195361E-16,0.)) ;
#79750 = DIRECTION('ref_axis',(3.46944695195361E-16,1.,0.)) ;
#79751 = DIRECTION('',(1.,-3.46944695195361E-16,0.)) ;
#79752 = DIRECTION('center_axis',(-1.,3.46944695195361E-16,0.)) ;
#79753 = DIRECTION('ref_axis',(3.46944695195361E-16,1.,0.)) ;
#79754 = DIRECTION('',(-1.,3.46944695195361E-16,0.)) ;
#79755 = DIRECTION('center_axis',(1.,-3.46944695195361E-16,0.)) ;
#79756 = DIRECTION('ref_axis',(3.46944695195361E-16,1.,0.)) ;
#79757 = DIRECTION('center_axis',(1.,-3.46944695195361E-16,0.)) ;
#79758 = DIRECTION('ref_axis',(-3.46944695195361E-16,-1.,-1.77635683940025E-15)) ;
#79759 = DIRECTION('',(1.,-3.46944695195361E-16,0.)) ;
#79760 = DIRECTION('center_axis',(-1.,3.46944695195361E-16,0.)) ;
#79761 = DIRECTION('ref_axis',(3.46944695195361E-16,1.,-1.77635683940025E-15)) ;
#79762 = DIRECTION('',(-1.,3.46944695195361E-16,0.)) ;
#79763 = DIRECTION('center_axis',(3.69451600012496E-31,1.06487173641454E-15,
-1.)) ;
#79764 = DIRECTION('ref_axis',(0.,1.,1.06487173641454E-15)) ;
#79765 = DIRECTION('',(3.46944695195361E-16,1.,1.06487173641454E-15)) ;
#79766 = DIRECTION('',(-1.,3.46944695195361E-16,0.)) ;
#79767 = DIRECTION('',(-3.46944695195361E-16,-1.,-1.06487173641454E-15)) ;
#79768 = DIRECTION('center_axis',(3.46944695195361E-16,1.,-4.47619207437002E-16)) ;
#79769 = DIRECTION('ref_axis',(8.18685017503995E-48,4.47619207437002E-16,
1.)) ;
#79770 = DIRECTION('',(1.,-3.46944695195361E-16,0.)) ;
#79771 = DIRECTION('',(1.5529910948782E-31,4.47619207437002E-16,1.)) ;
#79772 = DIRECTION('',(-1.5529910948782E-31,-4.47619207437002E-16,-1.)) ;
#79773 = DIRECTION('center_axis',(-1.,3.46944695195361E-16,0.)) ;
#79774 = DIRECTION('ref_axis',(-3.46944695195361E-16,-1.,0.)) ;
#79775 = DIRECTION('center_axis',(-1.,3.46944695195361E-16,0.)) ;
#79776 = DIRECTION('ref_axis',(-3.46944695195361E-16,-1.,0.)) ;
#79777 = DIRECTION('',(1.5529910948782E-31,4.47619207437002E-16,1.)) ;
#79778 = DIRECTION('',(0.,0.,-1.)) ;
#79779 = DIRECTION('center_axis',(1.,-3.46944695195361E-16,0.)) ;
#79780 = DIRECTION('ref_axis',(-3.46944695195361E-16,-1.,2.16840434497101E-15)) ;
#79781 = DIRECTION('center_axis',(1.,-3.46944695195361E-16,0.)) ;
#79782 = DIRECTION('ref_axis',(-3.46944695195361E-16,-1.,-5.32907051820075E-15)) ;
#79783 = DIRECTION('',(3.46944695195361E-16,1.,1.06487173641454E-15)) ;
#79784 = DIRECTION('center_axis',(1.,-3.46944695195361E-16,0.)) ;
#79785 = DIRECTION('ref_axis',(3.46944695195361E-16,1.,0.)) ;
#79786 = DIRECTION('center_axis',(-1.,3.46944695195361E-16,0.)) ;
#79787 = DIRECTION('ref_axis',(3.46944695195361E-16,1.,0.)) ;
#79788 = DIRECTION('',(0.,0.,-1.)) ;
#79789 = DIRECTION('',(0.,0.,1.)) ;
#79790 = DIRECTION('',(-3.46944695195361E-16,-1.,-9.27571383489107E-17)) ;
#79791 = DIRECTION('center_axis',(-3.46944695195361E-16,-1.,0.)) ;
#79792 = DIRECTION('ref_axis',(1.,-3.46944695195361E-16,0.)) ;
#79793 = DIRECTION('',(1.,-3.46944695195361E-16,0.)) ;
#79794 = DIRECTION('',(0.,0.,-1.)) ;
#79795 = DIRECTION('',(0.,0.,1.)) ;
#79796 = DIRECTION('center_axis',(1.,-3.46944695195361E-16,0.)) ;
#79797 = DIRECTION('ref_axis',(3.46944695195361E-16,1.,0.)) ;
#79798 = DIRECTION('center_axis',(1.,-3.46944695195361E-16,0.)) ;
#79799 = DIRECTION('ref_axis',(3.46944695195361E-16,1.,0.)) ;
#79800 = DIRECTION('',(1.,-3.46944695195361E-16,0.)) ;
#79801 = DIRECTION('center_axis',(-1.,3.46944695195361E-16,0.)) ;
#79802 = DIRECTION('ref_axis',(3.46944695195361E-16,1.,0.)) ;
#79803 = DIRECTION('',(-1.,3.46944695195361E-16,0.)) ;
#79804 = DIRECTION('center_axis',(-3.21815970916568E-32,-9.27571383489107E-17,
1.)) ;
#79805 = DIRECTION('ref_axis',(0.,-1.,-9.27571383489107E-17)) ;
#79806 = DIRECTION('',(3.46944695195361E-16,1.,9.27571383489107E-17)) ;
#79807 = DIRECTION('',(1.,0.,3.21815970916568E-32)) ;
#79808 = DIRECTION('',(-3.46944695195361E-16,-1.,-9.27571383489107E-17)) ;
#79809 = DIRECTION('',(-1.,3.46944695195361E-16,0.)) ;
#79810 = DIRECTION('center_axis',(1.,-3.46944695195361E-16,0.)) ;
#79811 = DIRECTION('ref_axis',(3.46944695195361E-16,1.,0.)) ;
#79812 = DIRECTION('center_axis',(1.,-3.46944695195361E-16,0.)) ;
#79813 = DIRECTION('ref_axis',(-3.46944695195361E-16,-1.,-2.66453525910038E-15)) ;
#79814 = DIRECTION('',(1.,-3.46944695195361E-16,0.)) ;
#79815 = DIRECTION('center_axis',(-1.,3.46944695195361E-16,0.)) ;
#79816 = DIRECTION('ref_axis',(3.46944695195361E-16,1.,-3.5527136788005E-15)) ;
#79817 = DIRECTION('',(-1.,3.46944695195361E-16,0.)) ;
#79818 = DIRECTION('center_axis',(-3.46944695195361E-16,-1.,0.)) ;
#79819 = DIRECTION('ref_axis',(1.,-3.46944695195361E-16,0.)) ;
#79820 = DIRECTION('',(0.,0.,-1.)) ;
#79821 = DIRECTION('',(-1.,3.46944695195361E-16,0.)) ;
#79822 = DIRECTION('',(0.,0.,1.)) ;
#79823 = DIRECTION('center_axis',(2.25271179641597E-31,6.49299968442375E-16,
-1.)) ;
#79824 = DIRECTION('ref_axis',(0.,1.,6.49299968442375E-16)) ;
#79825 = DIRECTION('',(3.46944695195361E-16,1.,6.49299968442375E-16)) ;
#79826 = DIRECTION('',(-1.,0.,-2.25271179641597E-31)) ;
#79827 = DIRECTION('',(-3.46944695195361E-16,-1.,-6.49299968442375E-16)) ;
#79828 = DIRECTION('',(1.,-3.46944695195361E-16,0.)) ;
#79829 = DIRECTION('center_axis',(-1.,3.46944695195361E-16,0.)) ;
#79830 = DIRECTION('ref_axis',(-3.46944695195361E-16,-1.,0.)) ;
#79831 = DIRECTION('',(3.46944695195361E-16,1.,6.49299968442375E-16)) ;
#79832 = DIRECTION('',(0.,0.,1.)) ;
#79833 = DIRECTION('',(0.,0.,-1.)) ;
#79834 = DIRECTION('center_axis',(-1.,3.46944695195361E-16,0.)) ;
#79835 = DIRECTION('ref_axis',(-3.46944695195361E-16,-1.,0.)) ;
#79836 = DIRECTION('center_axis',(-0.164398987305357,0.,-0.986393923832144)) ;
#79837 = DIRECTION('ref_axis',(-0.986393923832144,0.,0.164398987305357)) ;
#79838 = DIRECTION('',(-0.937042571331636,0.312347523777212,0.156173761888606)) ;
#79839 = DIRECTION('',(0.,-1.,0.)) ;
#79840 = DIRECTION('',(0.973328526784575,0.162221421130762,-0.162221421130763)) ;
#79841 = DIRECTION('',(-1.73472347597681E-15,1.,2.89120579329468E-16)) ;
#79842 = DIRECTION('center_axis',(-1.,0.,0.)) ;
#79843 = DIRECTION('ref_axis',(0.,0.,1.)) ;
#79844 = DIRECTION('center_axis',(-1.,0.,0.)) ;
#79845 = DIRECTION('ref_axis',(0.,0.958782004973288,-0.284142687640211)) ;
#79846 = DIRECTION('',(0.,0.,1.)) ;
#79847 = DIRECTION('',(0.,-1.,0.)) ;
#79848 = DIRECTION('center_axis',(-1.,0.,0.)) ;
#79849 = DIRECTION('ref_axis',(0.,0.758705435142026,-0.651433851350964)) ;
#79850 = DIRECTION('',(0.,0.,-1.)) ;
#79851 = DIRECTION('center_axis',(-1.,0.,0.)) ;
#79852 = DIRECTION('ref_axis',(0.,-0.654778578355217,-0.755820754760757)) ;
#79853 = DIRECTION('',(0.,1.,0.)) ;
#79854 = DIRECTION('center_axis',(-0.164398987305357,0.,0.986393923832144)) ;
#79855 = DIRECTION('ref_axis',(0.986393923832144,0.,0.164398987305357)) ;
#79856 = DIRECTION('',(-0.973328526784575,-0.162221421130762,-0.162221421130763)) ;
#79857 = DIRECTION('',(0.,1.,0.)) ;
#79858 = DIRECTION('',(0.937042571331636,-0.312347523777212,0.156173761888606)) ;
#79859 = DIRECTION('',(1.73472347597681E-15,-1.,2.89120579329468E-16)) ;
#79860 = DIRECTION('center_axis',(-0.573462344363329,0.81923192051904,0.)) ;
#79861 = DIRECTION('ref_axis',(-0.81923192051904,-0.573462344363329,0.)) ;
#79862 = DIRECTION('',(-0.710669054518702,-0.497468338163091,0.49746833816309)) ;
#79863 = DIRECTION('',(0.,0.,-1.)) ;
#79864 = DIRECTION('',(0.710669054518702,0.497468338163091,0.49746833816309)) ;
#79865 = DIRECTION('',(0.,0.,1.)) ;
#79866 = DIRECTION('center_axis',(-1.,0.,0.)) ;
#79867 = DIRECTION('ref_axis',(0.,0.,1.)) ;
#79868 = DIRECTION('',(0.,0.,1.)) ;
#79869 = DIRECTION('',(0.,-1.,-9.34081871679819E-17)) ;
#79870 = DIRECTION('',(0.,0.,-1.)) ;
#79871 = DIRECTION('',(0.,1.,-9.34081871679819E-17)) ;
#79872 = DIRECTION('center_axis',(-0.573462344363329,-0.81923192051904,0.)) ;
#79873 = DIRECTION('ref_axis',(0.81923192051904,-0.573462344363329,0.)) ;
#79874 = DIRECTION('',(-0.710669054518701,0.497468338163091,-0.497468338163091)) ;
#79875 = DIRECTION('',(0.,0.,1.)) ;
#79876 = DIRECTION('',(0.710669054518701,-0.497468338163091,-0.497468338163091)) ;
#79877 = DIRECTION('',(0.,0.,-1.)) ;
#79878 = DIRECTION('center_axis',(0.,0.,1.)) ;
#79879 = DIRECTION('ref_axis',(1.,0.,0.)) ;
#79880 = DIRECTION('',(1.,6.67201336914158E-17,0.)) ;
#79881 = DIRECTION('',(1.33440267382831E-16,1.,0.)) ;
#79882 = DIRECTION('',(-1.,1.33440267382831E-16,0.)) ;
#79883 = DIRECTION('center_axis',(0.,0.,1.)) ;
#79884 = DIRECTION('ref_axis',(1.,0.,0.)) ;
#79885 = DIRECTION('',(1.,-1.33440267382831E-16,0.)) ;
#79886 = DIRECTION('',(-1.33440267382831E-16,-1.,0.)) ;
#79887 = DIRECTION('',(-1.,-6.67201336914158E-17,0.)) ;
#79888 = DIRECTION('center_axis',(-6.67201336914158E-17,1.,0.)) ;
#79889 = DIRECTION('ref_axis',(-1.,-6.67201336914158E-17,0.)) ;
#79890 = DIRECTION('',(1.,6.67201336914158E-17,0.)) ;
#79891 = DIRECTION('',(0.,0.,1.)) ;
#79892 = DIRECTION('',(-1.,-6.67201336914158E-17,0.)) ;
#79893 = DIRECTION('center_axis',(-1.33440267382831E-16,-1.,0.)) ;
#79894 = DIRECTION('ref_axis',(1.,-1.33440267382831E-16,0.)) ;
#79895 = DIRECTION('',(1.,-1.33440267382831E-16,0.)) ;
#79896 = DIRECTION('',(0.,0.,-1.)) ;
#79897 = DIRECTION('',(-1.,1.33440267382831E-16,0.)) ;
#79898 = DIRECTION('center_axis',(0.,0.,1.)) ;
#79899 = DIRECTION('ref_axis',(1.,0.,0.)) ;
#79900 = DIRECTION('',(0.,-1.,0.)) ;
#79901 = DIRECTION('',(1.,0.,0.)) ;
#79902 = DIRECTION('',(0.,1.,0.)) ;
#79903 = DIRECTION('center_axis',(0.,0.,-1.)) ;
#79904 = DIRECTION('ref_axis',(1.,0.,0.)) ;
#79905 = DIRECTION('',(-1.44560289664734E-16,1.,-7.2280144832367E-17)) ;
#79906 = DIRECTION('center_axis',(0.,0.,1.)) ;
#79907 = DIRECTION('ref_axis',(1.,0.,0.)) ;
#79908 = DIRECTION('center_axis',(0.,0.,1.)) ;
#79909 = DIRECTION('ref_axis',(1.,0.,0.)) ;
#79910 = DIRECTION('',(0.,-1.,0.)) ;
#79911 = DIRECTION('',(-1.,0.,0.)) ;
#79912 = DIRECTION('',(0.,1.,0.)) ;
#79913 = DIRECTION('center_axis',(0.,0.,-1.)) ;
#79914 = DIRECTION('ref_axis',(1.,-1.82602471155453E-15,0.)) ;
#79915 = DIRECTION('',(1.44560289664734E-16,-1.,-2.4093381610789E-16)) ;
#79916 = DIRECTION('center_axis',(0.,0.,1.)) ;
#79917 = DIRECTION('ref_axis',(1.,0.,0.)) ;
#79918 = DIRECTION('center_axis',(0.,0.,-1.)) ;
#79919 = DIRECTION('ref_axis',(-1.,0.,0.)) ;
#79920 = DIRECTION('',(0.,0.,-1.)) ;
#79921 = DIRECTION('center_axis',(0.,0.,-1.)) ;
#79922 = DIRECTION('ref_axis',(1.,0.,0.)) ;
#79923 = DIRECTION('center_axis',(0.,0.,1.)) ;
#79924 = DIRECTION('ref_axis',(1.,0.,0.)) ;
#79925 = DIRECTION('center_axis',(1.,0.,0.)) ;
#79926 = DIRECTION('ref_axis',(0.,0.,-1.)) ;
#79927 = DIRECTION('',(0.,-1.,0.)) ;
#79928 = DIRECTION('',(0.,0.,1.)) ;
#79929 = DIRECTION('',(0.,1.,0.)) ;
#79930 = DIRECTION('center_axis',(0.81923192051904,0.573462344363329,0.)) ;
#79931 = DIRECTION('ref_axis',(-0.573462344363329,0.81923192051904,0.)) ;
#79932 = DIRECTION('',(-0.497468338163091,0.710669054518701,0.497468338163091)) ;
#79933 = DIRECTION('',(0.,0.,-1.)) ;
#79934 = DIRECTION('',(0.497468338163091,-0.710669054518701,0.497468338163091)) ;
#79935 = DIRECTION('',(0.,0.,1.)) ;
#79936 = DIRECTION('center_axis',(0.,1.,0.)) ;
#79937 = DIRECTION('ref_axis',(0.,0.,1.)) ;
#79938 = DIRECTION('',(0.,0.,1.)) ;
#79939 = DIRECTION('',(-1.,0.,0.)) ;
#79940 = DIRECTION('',(0.,0.,-1.)) ;
#79941 = DIRECTION('',(1.,0.,0.)) ;
#79942 = DIRECTION('center_axis',(-0.81923192051904,0.573462344363329,0.)) ;
#79943 = DIRECTION('ref_axis',(-0.573462344363329,-0.81923192051904,0.)) ;
#79944 = DIRECTION('',(0.497468338163091,0.710669054518701,-0.497468338163091)) ;
#79945 = DIRECTION('',(0.,0.,1.)) ;
#79946 = DIRECTION('',(-0.497468338163091,-0.710669054518701,-0.497468338163091)) ;
#79947 = DIRECTION('',(0.,0.,-1.)) ;
#79948 = DIRECTION('center_axis',(-1.,0.,0.)) ;
#79949 = DIRECTION('ref_axis',(0.,0.,1.)) ;
#79950 = DIRECTION('',(0.,-1.,0.)) ;
#79951 = DIRECTION('',(0.,0.,-1.)) ;
#79952 = DIRECTION('',(0.,1.,0.)) ;
#79953 = DIRECTION('',(0.,0.,-1.)) ;
#79954 = DIRECTION('center_axis',(0.,0.,-1.)) ;
#79955 = DIRECTION('ref_axis',(-1.,0.,0.)) ;
#79956 = DIRECTION('center_axis',(0.,0.,1.)) ;
#79957 = DIRECTION('ref_axis',(1.,0.,0.)) ;
#79958 = DIRECTION('center_axis',(0.,0.,-1.)) ;
#79959 = DIRECTION('ref_axis',(1.,5.20417042793042E-15,0.)) ;
#79960 = DIRECTION('center_axis',(-0.573462344363328,7.65229685658278E-17,
0.819231920519041)) ;
#79961 = DIRECTION('ref_axis',(0.819231920519041,1.22423955297878E-32,0.573462344363328)) ;
#79962 = DIRECTION('',(-0.710669054518702,-0.497468338163091,-0.497468338163091)) ;
#79963 = DIRECTION('',(1.33440267382831E-16,1.,-2.91413396387194E-34)) ;
#79964 = DIRECTION('',(0.710669054518701,-0.497468338163091,0.497468338163091)) ;
#79965 = DIRECTION('',(5.04890651880155E-33,-1.,9.34081871679819E-17)) ;
#79966 = DIRECTION('center_axis',(-0.573462344363328,7.65229685658278E-17,
-0.819231920519041)) ;
#79967 = DIRECTION('ref_axis',(-0.819231920519041,-1.22423955297878E-32,0.573462344363328)) ;
#79968 = DIRECTION('',(-0.710669054518701,0.497468338163091,0.497468338163091)) ;
#79969 = DIRECTION('',(-1.33440267382831E-16,-1.,7.77328292223541E-33)) ;
#79970 = DIRECTION('',(0.710669054518702,0.497468338163091,-0.497468338163091)) ;
#79971 = DIRECTION('',(-5.04890651880155E-33,1.,9.34081871679819E-17)) ;
#79972 = DIRECTION('center_axis',(0.,0.573462344363328,-0.819231920519041)) ;
#79973 = DIRECTION('ref_axis',(0.,0.819231920519041,0.573462344363328)) ;
#79974 = DIRECTION('',(0.497468338163091,0.710669054518701,0.497468338163091)) ;
#79975 = DIRECTION('',(-1.,0.,0.)) ;
#79976 = DIRECTION('',(0.497468338163091,-0.710669054518701,-0.497468338163091)) ;
#79977 = DIRECTION('',(1.,0.,0.)) ;
#79978 = DIRECTION('center_axis',(0.,0.573462344363328,0.819231920519041)) ;
#79979 = DIRECTION('ref_axis',(0.,-0.819231920519041,0.573462344363328)) ;
#79980 = DIRECTION('',(-0.497468338163091,0.710669054518701,-0.497468338163091)) ;
#79981 = DIRECTION('',(1.,0.,0.)) ;
#79982 = DIRECTION('',(-0.497468338163091,-0.710669054518701,0.497468338163091)) ;
#79983 = DIRECTION('',(-1.,0.,0.)) ;
#79984 = DIRECTION('center_axis',(-0.164398987305354,-0.986393923832144,0.)) ;
#79985 = DIRECTION('ref_axis',(0.,0.,1.)) ;
#79986 = DIRECTION('',(0.,0.,-1.)) ;
#79987 = DIRECTION('center_axis',(-0.164398987305423,-0.986393923832133,1.19343312735544E-12)) ;
#79988 = DIRECTION('ref_axis',(-0.057729035739095,0.0096215059577276,0.998285923498744)) ;
#79989 = DIRECTION('',(0.,0.,1.)) ;
#79990 = DIRECTION('center_axis',(1.,-2.89120579329441E-16,0.)) ;
#79991 = DIRECTION('ref_axis',(-2.89120579329441E-16,-1.,-3.43024899888577E-15)) ;
#79992 = DIRECTION('center_axis',(1.,1.15648231731787E-15,0.)) ;
#79993 = DIRECTION('ref_axis',(1.15648231731787E-15,-1.,0.)) ;
#79994 = DIRECTION('center_axis',(0.166689823575762,0.983956802822934,0.0635886223687179)) ;
#79995 = DIRECTION('ref_axis',(-0.0486480010045635,0.0726194157819113,-0.996172571620878)) ;
#79996 = DIRECTION('center_axis',(0.166689823572632,0.983956802827715,-0.0635886223029427)) ;
#79997 = DIRECTION('ref_axis',(-0.0462047034091838,0.072214919352298,0.996318287900915)) ;
#79998 = DIRECTION('center_axis',(-0.164398987305354,-0.986393923832144,0.)) ;
#79999 = DIRECTION('ref_axis',(0.,0.,1.)) ;
#80000 = DIRECTION('',(0.,0.,1.)) ;
#80001 = DIRECTION('center_axis',(-0.164398987305404,-0.986393923832136,-8.67951365333722E-13)) ;
#80002 = DIRECTION('ref_axis',(-0.0554192327871164,0.00923653879873397,-0.99842045000506)) ;
#80003 = DIRECTION('',(0.,0.,-1.)) ;
#80004 = DIRECTION('center_axis',(0.,0.,1.)) ;
#80005 = DIRECTION('ref_axis',(1.,0.,0.)) ;
#80006 = DIRECTION('center_axis',(0.,0.,1.)) ;
#80007 = DIRECTION('ref_axis',(1.,0.,0.)) ;
#80008 = DIRECTION('center_axis',(0.,1.,0.)) ;
#80009 = DIRECTION('ref_axis',(1.,0.,0.)) ;
#80010 = DIRECTION('center_axis',(0.,-0.888198741900269,0.45945945945946)) ;
#80011 = DIRECTION('ref_axis',(0.,0.45945945945946,0.888198741900269)) ;
#80012 = DIRECTION('center_axis',(-1.,0.,1.22067519501986E-15)) ;
#80013 = DIRECTION('ref_axis',(-1.22067519501986E-15,0.,-1.)) ;
#80014 = DIRECTION('center_axis',(0.,0.,1.)) ;
#80015 = DIRECTION('ref_axis',(1.,0.,0.)) ;
#80016 = DIRECTION('center_axis',(0.,0.,-1.)) ;
#80017 = DIRECTION('ref_axis',(-1.,0.,0.)) ;
#80018 = DIRECTION('center_axis',(1.,-3.46944695195361E-16,0.)) ;
#80019 = DIRECTION('ref_axis',(3.46944695195361E-16,1.,0.)) ;
#80020 = DIRECTION('center_axis',(-1.,3.46944695195361E-16,0.)) ;
#80021 = DIRECTION('ref_axis',(3.46944695195361E-16,1.,2.168404344971E-15)) ;
#80022 = DIRECTION('center_axis',(-1.,3.46944695195361E-16,0.)) ;
#80023 = DIRECTION('ref_axis',(-3.41607084500048E-16,-1.,0.)) ;
#80024 = DIRECTION('center_axis',(0.,-0.459459459459457,0.888198741900271)) ;
#80025 = DIRECTION('ref_axis',(0.,-0.888198741900271,-0.459459459459457)) ;
#80026 = DIRECTION('center_axis',(1.,-3.46944695195361E-16,0.)) ;
#80027 = DIRECTION('ref_axis',(0.,1.,0.)) ;
#80028 = DIRECTION('center_axis',(0.,0.888198741900269,-0.45945945945946)) ;
#80029 = DIRECTION('ref_axis',(0.,-0.45945945945946,-0.888198741900269)) ;
#80030 = DIRECTION('center_axis',(0.,1.,0.)) ;
#80031 = DIRECTION('ref_axis',(1.,0.,0.)) ;
#80032 = DIRECTION('center_axis',(0.,-1.,0.)) ;
#80033 = DIRECTION('ref_axis',(0.,0.,1.)) ;
#80034 = DIRECTION('center_axis',(-1.,0.,0.)) ;
#80035 = DIRECTION('ref_axis',(0.,0.,-1.)) ;
#80036 = DIRECTION('center_axis',(0.,0.,-1.)) ;
#80037 = DIRECTION('ref_axis',(-1.,0.,0.)) ;
#80038 = DIRECTION('center_axis',(0.,0.,-1.)) ;
#80039 = DIRECTION('ref_axis',(-1.,0.,0.)) ;
#80040 = DIRECTION('center_axis',(1.,-3.46944695195361E-16,0.)) ;
#80041 = DIRECTION('ref_axis',(3.46944695195361E-16,1.,0.)) ;
#80042 = DIRECTION('center_axis',(-1.,3.46944695195361E-16,0.)) ;
#80043 = DIRECTION('ref_axis',(3.46944695195361E-16,1.,0.)) ;
#80044 = DIRECTION('center_axis',(1.,0.,0.)) ;
#80045 = DIRECTION('ref_axis',(0.,0.,-1.)) ;
#80046 = DIRECTION('center_axis',(0.,0.,1.)) ;
#80047 = DIRECTION('ref_axis',(1.,0.,0.)) ;
#80048 = DIRECTION('center_axis',(0.,0.,1.)) ;
#80049 = DIRECTION('ref_axis',(1.,0.,0.)) ;
#80050 = DIRECTION('center_axis',(1.,-3.46944695195361E-16,0.)) ;
#80051 = DIRECTION('ref_axis',(3.80647894157197E-16,1.,0.)) ;
#80052 = DIRECTION('center_axis',(0.,0.459459459459459,-0.888198741900269)) ;
#80053 = DIRECTION('ref_axis',(0.,0.88819874190027,0.459459459459459)) ;
#80054 = DIRECTION('center_axis',(1.,-3.46944695195361E-16,0.)) ;
#80055 = DIRECTION('ref_axis',(3.46944695195361E-16,1.,0.)) ;
#80056 = DIRECTION('center_axis',(-1.,3.46944695195361E-16,0.)) ;
#80057 = DIRECTION('ref_axis',(3.46944695195361E-16,1.,-3.25260651745651E-15)) ;
#80058 = DIRECTION('center_axis',(-3.46944695195361E-16,-1.,-6.49299968442375E-16)) ;
#80059 = DIRECTION('ref_axis',(2.25271179641597E-31,6.49299968442375E-16,
-1.)) ;
#80060 = DIRECTION('center_axis',(0.,-1.,0.)) ;
#80061 = DIRECTION('ref_axis',(0.,0.,-1.)) ;
#80062 = DIRECTION('center_axis',(0.,0.,1.)) ;
#80063 = DIRECTION('ref_axis',(1.,0.,0.)) ;
#80064 = DIRECTION('center_axis',(-3.25260651745651E-15,0.,1.)) ;
#80065 = DIRECTION('ref_axis',(1.,0.,3.25260651745651E-15)) ;
#80066 = DIRECTION('center_axis',(0.,1.,0.)) ;
#80067 = DIRECTION('ref_axis',(1.,0.,0.)) ;
#80068 = DIRECTION('center_axis',(0.,-0.888198741900269,-0.45945945945946)) ;
#80069 = DIRECTION('ref_axis',(0.,-0.45945945945946,0.888198741900269)) ;
#80070 = DIRECTION('center_axis',(1.,-3.46944695195361E-16,0.)) ;
#80071 = DIRECTION('ref_axis',(0.,1.,0.)) ;
#80072 = DIRECTION('center_axis',(0.,0.888198741900269,0.45945945945946)) ;
#80073 = DIRECTION('ref_axis',(0.,0.45945945945946,-0.888198741900269)) ;
#80074 = DIRECTION('center_axis',(1.,-3.46944695195361E-16,0.)) ;
#80075 = DIRECTION('ref_axis',(0.,1.,0.)) ;
#80076 = DIRECTION('center_axis',(0.,1.,0.)) ;
#80077 = DIRECTION('ref_axis',(0.,0.,-1.)) ;
#80078 = DIRECTION('center_axis',(0.,1.,0.)) ;
#80079 = DIRECTION('ref_axis',(1.,0.,0.)) ;
#80080 = DIRECTION('center_axis',(-1.,0.,0.)) ;
#80081 = DIRECTION('ref_axis',(0.,0.,-1.)) ;
#80082 = DIRECTION('center_axis',(1.,-3.46944695195361E-16,0.)) ;
#80083 = DIRECTION('ref_axis',(3.41607084500048E-16,1.,0.)) ;
#80084 = DIRECTION('center_axis',(-9.62987005567165E-16,-0.459459459459459,
-0.88819874190027)) ;
#80085 = DIRECTION('ref_axis',(-9.03304156918849E-31,0.88819874190027,-0.459459459459459)) ;
#80086 = DIRECTION('center_axis',(1.,-3.46944695195361E-16,0.)) ;
#80087 = DIRECTION('ref_axis',(3.46944695195361E-16,1.,0.)) ;
#80088 = DIRECTION('center_axis',(-1.,3.46944695195361E-16,0.)) ;
#80089 = DIRECTION('ref_axis',(3.46944695195361E-16,1.,-5.42101086242751E-15)) ;
#80090 = DIRECTION('center_axis',(1.,0.,0.)) ;
#80091 = DIRECTION('ref_axis',(0.,0.,-1.)) ;
#80092 = DIRECTION('center_axis',(1.,-3.46944695195361E-16,0.)) ;
#80093 = DIRECTION('ref_axis',(3.80647894157197E-16,1.,0.)) ;
#80094 = DIRECTION('center_axis',(0.,0.459459459459459,0.888198741900269)) ;
#80095 = DIRECTION('ref_axis',(0.,-0.88819874190027,0.459459459459459)) ;
#80096 = DIRECTION('center_axis',(-3.46944695195361E-16,-1.,-6.49299968442375E-16)) ;
#80097 = DIRECTION('ref_axis',(2.25271179641597E-31,6.49299968442375E-16,
-1.)) ;
#80098 = DIRECTION('center_axis',(0.,1.,0.)) ;
#80099 = DIRECTION('ref_axis',(0.,0.,-1.)) ;
#80100 = DIRECTION('center_axis',(1.,0.,2.25271179641597E-31)) ;
#80101 = DIRECTION('ref_axis',(2.25271179641597E-31,0.,-1.)) ;
#80102 = DIRECTION('center_axis',(-1.,0.,0.)) ;
#80103 = DIRECTION('ref_axis',(0.,0.,1.)) ;
#80104 = DIRECTION('center_axis',(0.,1.,0.)) ;
#80105 = DIRECTION('ref_axis',(1.,0.,0.)) ;
#80106 = DIRECTION('center_axis',(0.,-1.,0.)) ;
#80107 = DIRECTION('ref_axis',(-1.0842021724855E-15,0.,1.)) ;
#80108 = DIRECTION('center_axis',(1.,-3.46944695195361E-16,0.)) ;
#80109 = DIRECTION('ref_axis',(0.,1.,0.)) ;
#80110 = DIRECTION('center_axis',(0.,1.,0.)) ;
#80111 = DIRECTION('ref_axis',(0.,0.,-1.)) ;
#80112 = DIRECTION('center_axis',(0.,-1.,0.)) ;
#80113 = DIRECTION('ref_axis',(0.,0.,-1.)) ;
#80114 = DIRECTION('center_axis',(0.,0.,1.)) ;
#80115 = DIRECTION('ref_axis',(-1.,0.,0.)) ;
#80116 = DIRECTION('center_axis',(0.,0.,-1.)) ;
#80117 = DIRECTION('ref_axis',(-1.,0.,0.)) ;
#80118 = DIRECTION('center_axis',(0.,0.,-1.)) ;
#80119 = DIRECTION('ref_axis',(-1.,0.,0.)) ;
#80120 = DIRECTION('center_axis',(-3.46944695195361E-16,-1.,-9.27571383489107E-17)) ;
#80121 = DIRECTION('ref_axis',(1.,-3.46944695195361E-16,-3.21815970916568E-32)) ;
#80122 = DIRECTION('center_axis',(0.,-1.,0.)) ;
#80123 = DIRECTION('ref_axis',(0.,0.,-1.)) ;
#80124 = DIRECTION('center_axis',(3.46944695195361E-16,1.,9.27571383489107E-17)) ;
#80125 = DIRECTION('ref_axis',(-1.,3.46944695195361E-16,3.21815970916568E-32)) ;
#80126 = DIRECTION('center_axis',(0.,1.,0.)) ;
#80127 = DIRECTION('ref_axis',(0.,0.,-1.)) ;
#80128 = DIRECTION('center_axis',(0.,0.,-1.)) ;
#80129 = DIRECTION('ref_axis',(-1.,0.,0.)) ;
#80130 = DIRECTION('center_axis',(0.,0.,1.)) ;
#80131 = DIRECTION('ref_axis',(1.,0.,0.)) ;
#80132 = DIRECTION('center_axis',(0.,1.,0.)) ;
#80133 = DIRECTION('ref_axis',(1.,0.,0.)) ;
#80134 = DIRECTION('center_axis',(-1.,0.,1.0842021724855E-15)) ;
#80135 = DIRECTION('ref_axis',(-1.0842021724855E-15,0.,-1.)) ;
#80136 = DIRECTION('center_axis',(0.,-1.,0.)) ;
#80137 = DIRECTION('ref_axis',(0.,0.,-1.)) ;
#80138 = DIRECTION('center_axis',(1.,0.,0.)) ;
#80139 = DIRECTION('ref_axis',(0.,0.,1.)) ;
#80140 = DIRECTION('center_axis',(1.,0.,3.21815970916568E-32)) ;
#80141 = DIRECTION('ref_axis',(3.21815970916568E-32,0.,-1.)) ;
#80142 = DIRECTION('center_axis',(0.,1.,0.)) ;
#80143 = DIRECTION('ref_axis',(1.,0.,0.)) ;
#80144 = DIRECTION('center_axis',(0.,0.,-1.)) ;
#80145 = DIRECTION('ref_axis',(1.,0.,0.)) ;
#80146 = DIRECTION('center_axis',(1.,0.,0.)) ;
#80147 = DIRECTION('ref_axis',(0.,-1.0842021724855E-15,1.)) ;
#80148 = DIRECTION('center_axis',(1.0842021724855E-15,1.,0.)) ;
#80149 = DIRECTION('ref_axis',(1.,-1.0842021724855E-15,0.)) ;
#80150 = DIRECTION('center_axis',(1.,0.,-2.08976773479518E-32)) ;
#80151 = DIRECTION('ref_axis',(-2.08976773479518E-32,0.,-1.)) ;
#80152 = DIRECTION('center_axis',(-0.447220452189876,-7.10036016473618E-6,
-0.894423762593922)) ;
#80153 = DIRECTION('ref_axis',(0.894325663269753,0.0148067719390998,-0.447171519130926)) ;
#80154 = DIRECTION('center_axis',(-1.23908819712629E-16,1.,2.4093381610789E-16)) ;
#80155 = DIRECTION('ref_axis',(2.98538247827883E-32,-2.4093381610789E-16,
1.)) ;
#80156 = DIRECTION('center_axis',(-5.60223391439791E-6,-0.447219005480428,
-0.894424485971684)) ;
#80157 = DIRECTION('ref_axis',(0.0146917039380788,0.894327914919915,-0.447170811245985)) ;
#80158 = DIRECTION('center_axis',(-8.95614743483648E-33,0.,1.)) ;
#80159 = DIRECTION('ref_axis',(1.,0.,8.95614743483648E-33)) ;
#80160 = DIRECTION('center_axis',(1.40488587213121E-32,-1.23908819712629E-16,
-1.)) ;
#80161 = DIRECTION('ref_axis',(1.74077750246726E-48,1.,-1.23908819712629E-16)) ;
#80162 = DIRECTION('center_axis',(-2.65552944032596E-32,0.,1.)) ;
#80163 = DIRECTION('ref_axis',(1.,0.,2.65552944032596E-32)) ;
#80164 = DIRECTION('center_axis',(0.8944244859717,-5.60223399946766E-6,0.447219005480397)) ;
#80165 = DIRECTION('ref_axis',(0.447170811245932,0.0146917039416789,-0.894327914919883)) ;
#80166 = DIRECTION('center_axis',(0.894423762593955,-7.10036019092399E-6,
-0.447220452189809)) ;
#80167 = DIRECTION('ref_axis',(0.44717151913086,0.0148067719390903,0.894325663269786)) ;
#80168 = DIRECTION('center_axis',(-8.95614743483648E-33,-1.10974565782288E-48,
1.)) ;
#80169 = DIRECTION('ref_axis',(1.,-9.9390457266313E-81,8.95614743483648E-33)) ;
#80170 = DIRECTION('center_axis',(-7.10036022482307E-6,0.894423762593866,
0.447220452189987)) ;
#80171 = DIRECTION('ref_axis',(-0.014806771937735,-0.447171519131047,0.894325663269715)) ;
#80172 = DIRECTION('center_axis',(-5.60223398444571E-6,0.894424485971634,
-0.447219005480529)) ;
#80173 = DIRECTION('ref_axis',(0.0146917039434335,0.447170811246052,0.894327914919794)) ;
#80174 = DIRECTION('center_axis',(1.40488587213121E-32,-1.23908819712629E-16,
-1.)) ;
#80175 = DIRECTION('ref_axis',(0.,1.,0.)) ;
#80176 = DIRECTION('center_axis',(-1.,0.,0.)) ;
#80177 = DIRECTION('ref_axis',(0.,0.,-1.)) ;
#80178 = DIRECTION('center_axis',(0.,-1.,0.)) ;
#80179 = DIRECTION('ref_axis',(0.,0.,1.)) ;
#80180 = DIRECTION('center_axis',(-1.,0.,-1.40488587213121E-32)) ;
#80181 = DIRECTION('ref_axis',(-1.40488587213121E-32,0.,1.)) ;
#80182 = DIRECTION('',(-1.,0.,-1.40488587213121E-32)) ;
#80183 = DIRECTION('center_axis',(-1.,0.,0.)) ;
#80184 = DIRECTION('ref_axis',(0.,0.,1.)) ;
#80185 = DIRECTION('center_axis',(0.,1.,0.)) ;
#80186 = DIRECTION('ref_axis',(1.,0.,0.)) ;
#80187 = DIRECTION('center_axis',(0.,1.,0.)) ;
#80188 = DIRECTION('ref_axis',(0.,0.,-1.)) ;
#80189 = DIRECTION('center_axis',(0.,0.,-1.)) ;
#80190 = DIRECTION('ref_axis',(1.,0.,0.)) ;
#80191 = DIRECTION('center_axis',(-1.,0.,-1.7912294869673E-32)) ;
#80192 = DIRECTION('ref_axis',(-1.7912294869673E-32,0.,1.)) ;
#80193 = DIRECTION('center_axis',(-0.447219005480468,-5.60223398368281E-6,
0.894424485971665)) ;
#80194 = DIRECTION('ref_axis',(0.894327914919842,0.0146917039421028,0.447170811245999)) ;
#80195 = DIRECTION('center_axis',(-1.,0.,0.)) ;
#80196 = DIRECTION('ref_axis',(0.,0.,1.)) ;
#80197 = DIRECTION('center_axis',(1.23908819712629E-16,-1.,7.2280144832367E-17)) ;
#80198 = DIRECTION('ref_axis',(1.,1.23908819712629E-16,-8.95614743483648E-33)) ;
#80199 = DIRECTION('center_axis',(-7.10036017276901E-6,-0.447220452189912,
0.894423762593904)) ;
#80200 = DIRECTION('ref_axis',(-0.0148067719326949,-0.894325663269819,-0.447171519131005)) ;
#80201 = DIRECTION('center_axis',(0.,-1.,1.0842021724855E-15)) ;
#80202 = DIRECTION('ref_axis',(0.,-1.0842021724855E-15,-1.)) ;
#80203 = DIRECTION('center_axis',(1.23908819712629E-16,-1.,1.23908819712629E-16)) ;
#80204 = DIRECTION('ref_axis',(3.09997069395837E-48,-1.23908819712629E-16,
-1.)) ;
#80205 = DIRECTION('center_axis',(0.,-1.,0.)) ;
#80206 = DIRECTION('ref_axis',(0.,0.,-1.)) ;
#80207 = DIRECTION('',(-1.23908819712629E-16,1.,-1.23908819712629E-16)) ;
#80208 = DIRECTION('center_axis',(1.,0.,1.40488587213121E-32)) ;
#80209 = DIRECTION('ref_axis',(1.40488587213121E-32,0.,-1.)) ;
#80210 = DIRECTION('center_axis',(-0.707106781186547,0.707106781186548,-7.05268145719433E-16)) ;
#80211 = DIRECTION('ref_axis',(0.707106781186548,0.707106781186547,-6.32735679406601E-14)) ;
#80212 = DIRECTION('center_axis',(1.,0.,0.)) ;
#80213 = DIRECTION('ref_axis',(0.,0.,-1.)) ;
#80214 = DIRECTION('center_axis',(0.,-1.,0.)) ;
#80215 = DIRECTION('ref_axis',(0.,0.,-1.)) ;
#80216 = DIRECTION('center_axis',(0.,0.,1.)) ;
#80217 = DIRECTION('ref_axis',(-1.,0.,0.)) ;
#80218 = DIRECTION('center_axis',(7.2280144832367E-17,0.,-1.)) ;
#80219 = DIRECTION('ref_axis',(-1.,0.,-7.2280144832367E-17)) ;
#80220 = DIRECTION('',(7.2280144832367E-17,0.,-1.)) ;
#80221 = DIRECTION('center_axis',(0.,0.,-1.)) ;
#80222 = DIRECTION('ref_axis',(-1.,0.,0.)) ;
#80223 = DIRECTION('center_axis',(0.,1.,0.)) ;
#80224 = DIRECTION('ref_axis',(1.,0.,0.)) ;
#80225 = DIRECTION('center_axis',(0.,0.,1.)) ;
#80226 = DIRECTION('ref_axis',(-1.,0.,0.)) ;
#80227 = DIRECTION('center_axis',(0.,1.,0.)) ;
#80228 = DIRECTION('ref_axis',(1.,0.,0.)) ;
#80229 = DIRECTION('center_axis',(1.,0.,0.)) ;
#80230 = DIRECTION('ref_axis',(0.,0.,1.)) ;
#80231 = DIRECTION('center_axis',(0.,0.,-1.)) ;
#80232 = DIRECTION('ref_axis',(1.,0.,0.)) ;
#80233 = DIRECTION('center_axis',(-1.13380619344889E-16,1.,-1.23908819712629E-16)) ;
#80234 = DIRECTION('ref_axis',(-1.40488587213121E-32,1.23908819712629E-16,
1.)) ;
#80235 = DIRECTION('center_axis',(0.,1.,0.)) ;
#80236 = DIRECTION('ref_axis',(0.,0.,1.)) ;
#80237 = DIRECTION('center_axis',(7.2280144832367E-17,0.,-1.)) ;
#80238 = DIRECTION('ref_axis',(-1.,0.,-7.2280144832367E-17)) ;
#80239 = DIRECTION('center_axis',(0.,0.,1.)) ;
#80240 = DIRECTION('ref_axis',(1.,0.,0.)) ;
#80241 = DIRECTION('center_axis',(0.,1.,0.)) ;
#80242 = DIRECTION('ref_axis',(1.,0.,0.)) ;
#80243 = DIRECTION('center_axis',(0.,1.,0.)) ;
#80244 = DIRECTION('ref_axis',(0.,0.,-1.)) ;
#80245 = DIRECTION('center_axis',(1.,2.16840434497101E-15,-2.93873587705572E-31)) ;
#80246 = DIRECTION('ref_axis',(2.16840434497101E-15,-1.,-1.03035812136257E-62)) ;
#80247 = DIRECTION('center_axis',(-8.95614743483648E-33,0.,1.)) ;
#80248 = DIRECTION('ref_axis',(1.,0.,8.95614743483648E-33)) ;
#80249 = DIRECTION('center_axis',(-1.40488587213121E-32,1.23908819712629E-16,
1.)) ;
#80250 = DIRECTION('ref_axis',(-1.74077750246726E-48,-1.,1.23908819712629E-16)) ;
#80251 = DIRECTION('center_axis',(8.95614743483648E-33,1.0154535431059E-48,
-1.)) ;
#80252 = DIRECTION('ref_axis',(-1.,1.76545184268265E-95,-8.95614743483648E-33)) ;
#80253 = DIRECTION('center_axis',(2.16840434497101E-15,0.,-1.)) ;
#80254 = DIRECTION('ref_axis',(-1.,0.,-2.16840434497101E-15)) ;
#80255 = DIRECTION('',(-8.95614743483648E-33,-1.0154535431059E-48,1.)) ;
#80256 = DIRECTION('center_axis',(-1.,-1.13380619344889E-16,0.)) ;
#80257 = DIRECTION('ref_axis',(0.,-1.,0.)) ;
#80258 = DIRECTION('center_axis',(0.,0.,1.)) ;
#80259 = DIRECTION('ref_axis',(-1.,0.,0.)) ;
#80260 = DIRECTION('center_axis',(0.,-1.,0.)) ;
#80261 = DIRECTION('ref_axis',(0.,0.,-1.)) ;
#80262 = DIRECTION('center_axis',(-1.,0.,0.)) ;
#80263 = DIRECTION('ref_axis',(0.,0.,-1.)) ;
#80264 = DIRECTION('center_axis',(1.,0.,1.40488587213121E-32)) ;
#80265 = DIRECTION('ref_axis',(1.40488587213121E-32,0.,-1.)) ;
#80266 = DIRECTION('',(1.,0.,1.40488587213121E-32)) ;
#80267 = DIRECTION('center_axis',(1.,0.,0.)) ;
#80268 = DIRECTION('ref_axis',(0.,0.,-1.)) ;
#80269 = DIRECTION('center_axis',(-1.40488587213121E-32,1.23908819712629E-16,
1.)) ;
#80270 = DIRECTION('ref_axis',(0.,-1.,0.)) ;
#80271 = DIRECTION('center_axis',(0.,-1.,0.)) ;
#80272 = DIRECTION('ref_axis',(0.,0.,1.)) ;
#80273 = DIRECTION('center_axis',(0.,1.,0.)) ;
#80274 = DIRECTION('ref_axis',(1.,0.,0.)) ;
#80275 = DIRECTION('center_axis',(1.,0.,0.)) ;
#80276 = DIRECTION('ref_axis',(0.,0.,1.)) ;
#80277 = DIRECTION('center_axis',(0.,1.,0.)) ;
#80278 = DIRECTION('ref_axis',(0.,0.,-1.)) ;
#80279 = DIRECTION('center_axis',(0.,0.,1.)) ;
#80280 = DIRECTION('ref_axis',(1.,0.,0.)) ;
#80281 = DIRECTION('center_axis',(0.,0.,1.)) ;
#80282 = DIRECTION('ref_axis',(1.,0.,0.)) ;
#80283 = DIRECTION('center_axis',(1.,0.,1.40488587213121E-32)) ;
#80284 = DIRECTION('ref_axis',(1.40488587213121E-32,0.,-1.)) ;
#80285 = DIRECTION('center_axis',(-0.707106781186543,0.707106781186552,9.74552346812296E-15)) ;
#80286 = DIRECTION('ref_axis',(0.707106781186552,0.707106781186543,-2.44769167512091E-14)) ;
#80287 = DIRECTION('center_axis',(-1.23908819712629E-16,1.,-1.23908819712629E-16)) ;
#80288 = DIRECTION('ref_axis',(-3.09997069395837E-48,1.23908819712629E-16,
1.)) ;
#80289 = DIRECTION('',(1.23908819712629E-16,-1.,1.23908819712629E-16)) ;
#80290 = DIRECTION('center_axis',(-1.,-1.13380619344889E-16,0.)) ;
#80291 = DIRECTION('ref_axis',(0.,-1.,0.)) ;
#80292 = DIRECTION('center_axis',(0.,-1.,0.)) ;
#80293 = DIRECTION('ref_axis',(0.,0.,1.)) ;
#80294 = DIRECTION('center_axis',(1.13380619344889E-16,-1.,1.23908819712629E-16)) ;
#80295 = DIRECTION('ref_axis',(1.40488587213121E-32,-1.23908819712629E-16,
-1.)) ;
#80296 = DIRECTION('center_axis',(-1.5529910948782E-31,-4.47619207437002E-16,
1.)) ;
#80297 = DIRECTION('ref_axis',(-1.26404997831554E-61,-1.,-4.47619207437002E-16)) ;
#80298 = DIRECTION('center_axis',(0.,2.16840434497101E-15,-1.)) ;
#80299 = DIRECTION('ref_axis',(0.,1.,2.16840434497101E-15)) ;
#80300 = DIRECTION('center_axis',(0.,1.,0.)) ;
#80301 = DIRECTION('ref_axis',(1.,0.,0.)) ;
#80302 = DIRECTION('center_axis',(3.85194802226865E-15,0.888198741900269,
-0.45945945945946)) ;
#80303 = DIRECTION('ref_axis',(1.56255765105114E-31,-0.45945945945946,-0.888198741900269)) ;
#80304 = DIRECTION('center_axis',(-1.,0.,1.22067519501986E-15)) ;
#80305 = DIRECTION('ref_axis',(-1.22067519501986E-15,-4.33680868994202E-15,
-1.)) ;
#80306 = DIRECTION('center_axis',(1.5529910948782E-31,4.47619207437002E-16,
-1.)) ;
#80307 = DIRECTION('ref_axis',(-6.951486430461E-47,1.,4.47619207437002E-16)) ;
#80308 = DIRECTION('center_axis',(0.,0.,1.)) ;
#80309 = DIRECTION('ref_axis',(1.,0.,0.)) ;
#80310 = DIRECTION('center_axis',(1.,-3.46944695195361E-16,0.)) ;
#80311 = DIRECTION('ref_axis',(3.46944695195361E-16,1.,0.)) ;
#80312 = DIRECTION('center_axis',(-1.,3.46944695195361E-16,0.)) ;
#80313 = DIRECTION('ref_axis',(3.46944695195361E-16,1.,0.)) ;
#80314 = DIRECTION('center_axis',(1.,-3.46944695195361E-16,0.)) ;
#80315 = DIRECTION('ref_axis',(3.41607084500048E-16,1.,0.)) ;
#80316 = DIRECTION('center_axis',(0.,0.459459459459457,-0.888198741900271)) ;
#80317 = DIRECTION('ref_axis',(0.,0.888198741900271,0.459459459459457)) ;
#80318 = DIRECTION('center_axis',(0.,0.,1.)) ;
#80319 = DIRECTION('ref_axis',(1.,0.,0.)) ;
#80320 = DIRECTION('center_axis',(0.,0.,-1.)) ;
#80321 = DIRECTION('ref_axis',(-1.,0.,0.)) ;
#80322 = DIRECTION('center_axis',(-1.,3.46944695195361E-16,0.)) ;
#80323 = DIRECTION('ref_axis',(-3.46944695195361E-16,-1.,0.)) ;
#80324 = DIRECTION('center_axis',(-1.,3.46944695195361E-16,0.)) ;
#80325 = DIRECTION('ref_axis',(-3.46944695195361E-16,-1.,0.)) ;
#80326 = DIRECTION('center_axis',(-1.,3.46944695195361E-16,0.)) ;
#80327 = DIRECTION('ref_axis',(3.46944695195361E-16,1.,0.)) ;
#80328 = DIRECTION('center_axis',(1.,-3.46944695195361E-16,0.)) ;
#80329 = DIRECTION('ref_axis',(0.,1.,0.)) ;
#80330 = DIRECTION('center_axis',(0.,-0.888198741900269,0.459459459459461)) ;
#80331 = DIRECTION('ref_axis',(0.,0.459459459459461,0.888198741900269)) ;
#80332 = DIRECTION('center_axis',(0.,1.,0.)) ;
#80333 = DIRECTION('ref_axis',(1.,0.,0.)) ;
#80334 = DIRECTION('center_axis',(0.,1.,0.)) ;
#80335 = DIRECTION('ref_axis',(1.0842021724855E-15,0.,-1.)) ;
#80336 = DIRECTION('center_axis',(-1.,0.,0.)) ;
#80337 = DIRECTION('ref_axis',(0.,0.,-1.)) ;
#80338 = DIRECTION('center_axis',(1.,-3.46944695195361E-16,0.)) ;
#80339 = DIRECTION('ref_axis',(3.70074341541719E-16,1.,0.)) ;
#80340 = DIRECTION('center_axis',(0.,0.63294893130157,-0.774193548387094)) ;
#80341 = DIRECTION('ref_axis',(-1.0842021724855E-15,-0.774193548387094,-0.63294893130157)) ;
#80342 = DIRECTION('center_axis',(1.,-3.46944695195361E-16,0.)) ;
#80343 = DIRECTION('ref_axis',(3.80647894157197E-16,1.,0.)) ;
#80344 = DIRECTION('center_axis',(0.,-0.45945945945946,0.888198741900269)) ;
#80345 = DIRECTION('ref_axis',(0.,-0.888198741900269,-0.45945945945946)) ;
#80346 = DIRECTION('center_axis',(1.,-3.46944695195361E-16,0.)) ;
#80347 = DIRECTION('ref_axis',(3.46944695195361E-16,1.,0.)) ;
#80348 = DIRECTION('center_axis',(-1.,3.46944695195361E-16,0.)) ;
#80349 = DIRECTION('ref_axis',(3.46944695195361E-16,1.,-7.58941520739854E-15)) ;
#80350 = DIRECTION('center_axis',(-3.46944695195361E-16,-1.,-2.45739631480277E-16)) ;
#80351 = DIRECTION('ref_axis',(1.,-3.46944695195361E-16,-8.52580615413453E-32)) ;
#80352 = DIRECTION('center_axis',(0.,1.,0.)) ;
#80353 = DIRECTION('ref_axis',(0.,0.,1.)) ;
#80354 = DIRECTION('center_axis',(1.,-3.46944695195361E-16,0.)) ;
#80355 = DIRECTION('ref_axis',(3.33066907387547E-16,1.,0.)) ;
#80356 = DIRECTION('center_axis',(8.02036034720251E-16,0.293103448275862,
-0.956080733311157)) ;
#80357 = DIRECTION('ref_axis',(-2.28610793645795E-31,0.956080733311157,0.293103448275862)) ;
#80358 = DIRECTION('center_axis',(-1.,3.46944695195361E-16,0.)) ;
#80359 = DIRECTION('ref_axis',(-3.46944695195361E-16,-1.,0.)) ;
#80360 = DIRECTION('center_axis',(-1.,3.46944695195361E-16,0.)) ;
#80361 = DIRECTION('ref_axis',(-3.46944695195361E-16,-1.,0.)) ;
#80362 = DIRECTION('center_axis',(-1.,3.46944695195361E-16,0.)) ;
#80363 = DIRECTION('ref_axis',(-3.46944695195361E-16,-1.,0.)) ;
#80364 = DIRECTION('center_axis',(0.,0.,-1.)) ;
#80365 = DIRECTION('ref_axis',(-1.,0.,0.)) ;
#80366 = DIRECTION('center_axis',(0.,0.,1.)) ;
#80367 = DIRECTION('ref_axis',(1.,0.,0.)) ;
#80368 = DIRECTION('center_axis',(-1.5529910948782E-31,-4.47619207437002E-16,
-1.)) ;
#80369 = DIRECTION('ref_axis',(1.06958075088238E-61,1.,-4.47619207437002E-16)) ;
#80370 = DIRECTION('center_axis',(2.16840434497101E-15,0.,1.)) ;
#80371 = DIRECTION('ref_axis',(1.,0.,-2.16840434497101E-15)) ;
#80372 = DIRECTION('center_axis',(1.,-3.46944695195361E-16,0.)) ;
#80373 = DIRECTION('ref_axis',(0.,1.,0.)) ;
#80374 = DIRECTION('center_axis',(0.,-1.,0.)) ;
#80375 = DIRECTION('ref_axis',(0.,0.,1.)) ;
#80376 = DIRECTION('center_axis',(0.577350269189625,0.577350269189627,0.577350269189625)) ;
#80377 = DIRECTION('ref_axis',(-0.707106781186548,0.,0.707106781186548)) ;
#80378 = DIRECTION('center_axis',(-1.,3.46944695195361E-16,0.)) ;
#80379 = DIRECTION('ref_axis',(-3.70074341541719E-16,-1.,0.)) ;
#80380 = DIRECTION('center_axis',(0.,0.63294893130157,0.774193548387094)) ;
#80381 = DIRECTION('ref_axis',(0.,0.774193548387094,-0.63294893130157)) ;
#80382 = DIRECTION('center_axis',(0.,1.,0.)) ;
#80383 = DIRECTION('ref_axis',(1.,0.,0.)) ;
#80384 = DIRECTION('center_axis',(-1.,0.,0.)) ;
#80385 = DIRECTION('ref_axis',(0.,-4.33680868994202E-15,-1.)) ;
#80386 = DIRECTION('center_axis',(0.,0.888198741900271,0.459459459459457)) ;
#80387 = DIRECTION('ref_axis',(-1.0842021724855E-15,0.459459459459457,-0.888198741900271)) ;
#80388 = DIRECTION('center_axis',(3.46944695195361E-16,1.,2.45739631480277E-16)) ;
#80389 = DIRECTION('ref_axis',(-1.,3.46944695195361E-16,8.52580615413453E-32)) ;
#80390 = DIRECTION('center_axis',(-1.,3.46944695195361E-16,0.)) ;
#80391 = DIRECTION('ref_axis',(-3.33066907387547E-16,-1.,0.)) ;
#80392 = DIRECTION('center_axis',(0.,0.293103448275864,0.956080733311156)) ;
#80393 = DIRECTION('ref_axis',(0.,-0.956080733311156,0.293103448275864)) ;
#80394 = DIRECTION('center_axis',(-3.46944695195361E-16,-1.,-1.06487173641454E-15)) ;
#80395 = DIRECTION('ref_axis',(3.69451600012496E-31,1.06487173641454E-15,
-1.)) ;
#80396 = DIRECTION('center_axis',(0.,-1.,0.)) ;
#80397 = DIRECTION('ref_axis',(0.,0.,-1.)) ;
#80398 = DIRECTION('center_axis',(0.,1.,0.)) ;
#80399 = DIRECTION('ref_axis',(0.,0.,1.)) ;
#80400 = DIRECTION('center_axis',(-1.,3.46944695195361E-16,0.)) ;
#80401 = DIRECTION('ref_axis',(-3.41607084500048E-16,-1.,0.)) ;
#80402 = DIRECTION('center_axis',(-4.88154879316133E-15,0.45945945945946,
0.888198741900269)) ;
#80403 = DIRECTION('ref_axis',(5.19745563204766E-30,-0.888198741900269,0.45945945945946)) ;
#80404 = DIRECTION('center_axis',(1.,-3.46944695195361E-16,0.)) ;
#80405 = DIRECTION('ref_axis',(3.46944695195361E-16,1.,0.)) ;
#80406 = DIRECTION('center_axis',(-1.,3.46944695195361E-16,0.)) ;
#80407 = DIRECTION('ref_axis',(3.46944695195361E-16,1.,0.)) ;
#80408 = DIRECTION('center_axis',(-1.5529910948782E-31,-4.47619207437002E-16,
-1.)) ;
#80409 = DIRECTION('ref_axis',(-6.95148643046101E-47,1.,-4.47619207437002E-16)) ;
#80410 = DIRECTION('center_axis',(0.,0.,-1.)) ;
#80411 = DIRECTION('ref_axis',(-1.,0.,0.)) ;
#80412 = DIRECTION('center_axis',(0.,0.224137931034483,-0.974557431797419)) ;
#80413 = DIRECTION('ref_axis',(0.,-0.974557431797419,-0.224137931034483)) ;
#80414 = DIRECTION('center_axis',(0.577350269189626,0.577350269189625,0.577350269189626)) ;
#80415 = DIRECTION('ref_axis',(-0.707106781186548,0.,0.707106781186548)) ;
#80416 = DIRECTION('center_axis',(0.408248290463863,-0.816496580927726,0.408248290463863)) ;
#80417 = DIRECTION('ref_axis',(0.707106781186548,0.,-0.707106781186548)) ;
#80418 = DIRECTION('center_axis',(0.,1.,0.)) ;
#80419 = DIRECTION('ref_axis',(1.,0.,0.)) ;
#80420 = DIRECTION('center_axis',(-1.,0.,0.)) ;
#80421 = DIRECTION('ref_axis',(0.,-8.67361737988403E-15,-1.)) ;
#80422 = DIRECTION('center_axis',(1.,-3.46944695195361E-16,0.)) ;
#80423 = DIRECTION('ref_axis',(0.,1.,0.)) ;
#80424 = DIRECTION('center_axis',(9.96293888229924E-16,-0.888198741900269,
-0.45945945945946)) ;
#80425 = DIRECTION('ref_axis',(-5.65334012505894E-32,-0.45945945945946,0.888198741900269)) ;
#80426 = DIRECTION('center_axis',(1.,-3.46944695195361E-16,0.)) ;
#80427 = DIRECTION('ref_axis',(-3.70074341541719E-16,-1.,-1.22464679914735E-16)) ;
#80428 = DIRECTION('center_axis',(1.58436874053304E-16,-0.224137931034483,
-0.974557431797419)) ;
#80429 = DIRECTION('ref_axis',(6.2575771930786E-32,0.974557431797419,-0.224137931034483)) ;
#80430 = DIRECTION('center_axis',(1.,-3.46944695195361E-16,0.)) ;
#80431 = DIRECTION('ref_axis',(3.46944695195361E-16,1.,0.)) ;
#80432 = DIRECTION('center_axis',(-1.,3.46944695195361E-16,0.)) ;
#80433 = DIRECTION('ref_axis',(3.46944695195361E-16,1.,3.25260651745652E-15)) ;
#80434 = DIRECTION('center_axis',(1.,-3.46944695195361E-16,0.)) ;
#80435 = DIRECTION('ref_axis',(3.80647894157197E-16,1.,0.)) ;
#80436 = DIRECTION('center_axis',(0.,-0.45945945945946,-0.888198741900269)) ;
#80437 = DIRECTION('ref_axis',(0.,0.888198741900269,-0.45945945945946)) ;
#80438 = DIRECTION('center_axis',(1.,-3.46944695195361E-16,0.)) ;
#80439 = DIRECTION('ref_axis',(0.,1.,0.)) ;
#80440 = DIRECTION('center_axis',(0.,-1.,0.)) ;
#80441 = DIRECTION('ref_axis',(0.,0.,1.)) ;
#80442 = DIRECTION('center_axis',(-3.46944695195361E-16,-1.,-1.06487173641454E-15)) ;
#80443 = DIRECTION('ref_axis',(3.69451600012496E-31,1.06487173641454E-15,
-1.)) ;
#80444 = DIRECTION('center_axis',(0.,0.,1.)) ;
#80445 = DIRECTION('ref_axis',(1.,0.,0.)) ;
#80446 = DIRECTION('center_axis',(0.,-1.,0.)) ;
#80447 = DIRECTION('ref_axis',(0.,0.,-1.)) ;
#80448 = DIRECTION('center_axis',(0.,-1.,0.)) ;
#80449 = DIRECTION('ref_axis',(0.,0.,-1.)) ;
#80450 = DIRECTION('center_axis',(0.,1.,0.)) ;
#80451 = DIRECTION('ref_axis',(0.,0.,-1.)) ;
#80452 = DIRECTION('center_axis',(0.,0.,1.)) ;
#80453 = DIRECTION('ref_axis',(1.,0.,0.)) ;
#80454 = DIRECTION('center_axis',(8.67361737988404E-15,-1.,0.)) ;
#80455 = DIRECTION('ref_axis',(1.,8.67361737988404E-15,0.)) ;
#80456 = DIRECTION('center_axis',(0.497468338163091,-0.710669054518702,0.497468338163091)) ;
#80457 = DIRECTION('ref_axis',(0.81923192051904,0.573462344363328,8.04804396179112E-16)) ;
#80458 = DIRECTION('center_axis',(0.497468338163091,-0.710669054518702,0.497468338163091)) ;
#80459 = DIRECTION('ref_axis',(0.81923192051904,0.573462344363328,7.6535433881835E-16)) ;
#80460 = DIRECTION('center_axis',(0.497468338163092,-0.7106690545187,0.497468338163092)) ;
#80461 = DIRECTION('ref_axis',(-2.51524304138174E-16,-0.57346234436333,-0.819231920519039)) ;
#80462 = DIRECTION('center_axis',(0.,0.,1.)) ;
#80463 = DIRECTION('ref_axis',(1.,0.,0.)) ;
#80464 = DIRECTION('center_axis',(0.,-1.,0.)) ;
#80465 = DIRECTION('ref_axis',(0.,0.,-1.)) ;
#80466 = DIRECTION('center_axis',(0.,1.,0.)) ;
#80467 = DIRECTION('ref_axis',(0.,0.,1.)) ;
#80468 = DIRECTION('center_axis',(0.,1.,0.)) ;
#80469 = DIRECTION('ref_axis',(0.,0.,1.)) ;
#80470 = DIRECTION('center_axis',(0.,1.,0.)) ;
#80471 = DIRECTION('ref_axis',(1.,0.,0.)) ;
#80472 = DIRECTION('center_axis',(-1.98515611757154E-15,0.,1.)) ;
#80473 = DIRECTION('ref_axis',(-1.,0.,-1.98515611757154E-15)) ;
#80474 = DIRECTION('center_axis',(1.,-4.06575814682065E-16,2.84603070277446E-16)) ;
#80475 = DIRECTION('ref_axis',(-4.06575814682065E-16,-1.,6.48893816316174E-47)) ;
#80476 = DIRECTION('center_axis',(0.,1.,0.)) ;
#80477 = DIRECTION('ref_axis',(0.,0.,1.)) ;
#80478 = DIRECTION('center_axis',(0.,1.,0.)) ;
#80479 = DIRECTION('ref_axis',(0.,0.,1.)) ;
#80480 = DIRECTION('center_axis',(0.497468338163091,0.710669054518702,-0.497468338163091)) ;
#80481 = DIRECTION('ref_axis',(-0.81923192051904,0.573462344363328,7.6535433881835E-16)) ;
#80482 = DIRECTION('center_axis',(-0.497468338163091,-0.710669054518702,0.497468338163091)) ;
#80483 = DIRECTION('ref_axis',(-0.81923192051904,0.57346234436333,3.73565257438817E-15)) ;
#80484 = DIRECTION('center_axis',(-0.497468338163093,-0.7106690545187,0.497468338163091)) ;
#80485 = DIRECTION('ref_axis',(0.819231920519039,-0.573462344363331,1.48853464230757E-16)) ;
#80486 = DIRECTION('center_axis',(1.,0.,0.)) ;
#80487 = DIRECTION('ref_axis',(0.,0.,-1.)) ;
#80488 = DIRECTION('center_axis',(1.,0.,-9.9257805878577E-16)) ;
#80489 = DIRECTION('ref_axis',(-9.9257805878577E-16,0.,-1.)) ;
#80490 = DIRECTION('center_axis',(0.,0.,-1.)) ;
#80491 = DIRECTION('ref_axis',(-1.,0.,0.)) ;
#80492 = DIRECTION('center_axis',(-1.23327997120227E-15,1.76182853028895E-15,
1.)) ;
#80493 = DIRECTION('ref_axis',(7.00649232162409E-46,-1.,1.76182853028895E-15)) ;
#80494 = DIRECTION('center_axis',(-0.497468338163091,0.710669054518702,0.497468338163091)) ;
#80495 = DIRECTION('ref_axis',(-0.81923192051904,-0.573462344363328,7.6535433881835E-16)) ;
#80496 = DIRECTION('center_axis',(0.497468338163091,-0.710669054518702,-0.497468338163091)) ;
#80497 = DIRECTION('ref_axis',(-0.819231920519043,-0.573462344363324,-7.46600562027492E-15)) ;
#80498 = DIRECTION('center_axis',(0.497468338163093,-0.7106690545187,-0.497468338163091)) ;
#80499 = DIRECTION('ref_axis',(0.819231920519039,0.573462344363331,2.16059097207149E-16)) ;
#80500 = DIRECTION('center_axis',(0.,1.,0.)) ;
#80501 = DIRECTION('ref_axis',(1.,0.,0.)) ;
#80502 = DIRECTION('center_axis',(-1.13841228110978E-15,-1.62630325872826E-15,
1.)) ;
#80503 = DIRECTION('ref_axis',(3.5236570605779E-15,1.,1.62630325872826E-15)) ;
#80504 = DIRECTION('center_axis',(0.,1.,0.)) ;
#80505 = DIRECTION('ref_axis',(1.,0.,0.)) ;
#80506 = DIRECTION('center_axis',(1.,0.,-1.65429676464295E-16)) ;
#80507 = DIRECTION('ref_axis',(1.65429676464295E-16,0.,1.)) ;
#80508 = DIRECTION('center_axis',(0.,0.,-1.)) ;
#80509 = DIRECTION('ref_axis',(-1.,0.,0.)) ;
#80510 = DIRECTION('center_axis',(3.3085935292859E-16,0.,1.)) ;
#80511 = DIRECTION('ref_axis',(1.,0.,-3.3085935292859E-16)) ;
#80512 = DIRECTION('center_axis',(1.,0.,0.)) ;
#80513 = DIRECTION('ref_axis',(0.,0.,-1.)) ;
#80514 = DIRECTION('center_axis',(1.,1.21972744404619E-15,8.53809210832338E-16)) ;
#80515 = DIRECTION('ref_axis',(-1.21972744404619E-15,1.,-2.84382165153726E-47)) ;
#80516 = DIRECTION('center_axis',(0.,1.,0.)) ;
#80517 = DIRECTION('ref_axis',(1.,0.,0.)) ;
#80518 = DIRECTION('center_axis',(0.497468338163092,0.710669054518701,0.497468338163092)) ;
#80519 = DIRECTION('ref_axis',(2.72143460710088E-15,0.573462344363328,-0.819231920519041)) ;
#80520 = DIRECTION('center_axis',(-0.497468338163091,-0.710669054518702,-0.497468338163091)) ;
#80521 = DIRECTION('ref_axis',(0.81923192051904,-0.573462344363328,7.6535433881835E-16)) ;
#80522 = DIRECTION('center_axis',(-0.497468338163091,-0.710669054518702,-0.497468338163091)) ;
#80523 = DIRECTION('ref_axis',(0.81923192051904,-0.573462344363328,7.6535433881835E-16)) ;
#80524 = DIRECTION('center_axis',(0.,-1.,0.)) ;
#80525 = DIRECTION('ref_axis',(0.,0.,-1.)) ;
#80526 = DIRECTION('center_axis',(0.,1.,0.)) ;
#80527 = DIRECTION('ref_axis',(0.,0.,-1.)) ;
#80528 = DIRECTION('center_axis',(-8.67361737988403E-15,1.,0.)) ;
#80529 = DIRECTION('ref_axis',(-1.,-8.67361737988403E-15,0.)) ;
#80530 = DIRECTION('center_axis',(0.,0.,1.)) ;
#80531 = DIRECTION('ref_axis',(1.,0.,0.)) ;
#80532 = DIRECTION('center_axis',(1.,6.67201336914158E-17,0.)) ;
#80533 = DIRECTION('ref_axis',(-6.67201336914158E-17,1.,0.)) ;
#80534 = DIRECTION('center_axis',(-1.,-6.67201336914158E-17,0.)) ;
#80535 = DIRECTION('ref_axis',(-6.67201336914158E-17,1.,0.)) ;
#80536 = DIRECTION('center_axis',(-1.,1.33440267382831E-16,0.)) ;
#80537 = DIRECTION('ref_axis',(-1.33440267382831E-16,-1.,0.)) ;
#80538 = DIRECTION('center_axis',(-1.,1.33440267382831E-16,0.)) ;
#80539 = DIRECTION('ref_axis',(-1.33440267382831E-16,-1.,0.)) ;
#80540 = DIRECTION('center_axis',(0.710669054518702,0.497468338163091,0.497468338163091)) ;
#80541 = DIRECTION('ref_axis',(-0.573462344363328,0.819231920519041,3.92980824865032E-16)) ;
#80542 = DIRECTION('center_axis',(0.710669054518702,0.497468338163091,0.497468338163091)) ;
#80543 = DIRECTION('ref_axis',(-0.573462344363328,0.819231920519041,3.92980824865032E-16)) ;
#80544 = DIRECTION('center_axis',(0.710669054518701,0.497468338163091,0.497468338163092)) ;
#80545 = DIRECTION('ref_axis',(0.573462344363329,2.49119655197717E-16,-0.81923192051904)) ;
#80546 = DIRECTION('center_axis',(-0.710669054518702,0.497468338163091,-0.497468338163091)) ;
#80547 = DIRECTION('ref_axis',(-0.573462344363328,-0.819231920519041,6.69271761853466E-16)) ;
#80548 = DIRECTION('center_axis',(0.710669054518702,-0.497468338163091,0.497468338163091)) ;
#80549 = DIRECTION('ref_axis',(-0.573462344363329,-0.81923192051904,1.7228593515426E-15)) ;
#80550 = DIRECTION('center_axis',(0.7106690545187,-0.497468338163094,0.497468338163091)) ;
#80551 = DIRECTION('ref_axis',(0.573462344363331,0.819231920519038,2.86772422505918E-16)) ;
#80552 = DIRECTION('center_axis',(0.,1.,-9.34081871679819E-17)) ;
#80553 = DIRECTION('ref_axis',(0.,9.34081871679819E-17,1.)) ;
#80554 = DIRECTION('center_axis',(-4.33680868994205E-15,-1.,-3.03576608295944E-15)) ;
#80555 = DIRECTION('ref_axis',(1.,-4.33680868994205E-15,-1.12103877145985E-44)) ;
#80556 = DIRECTION('center_axis',(0.,1.,5.29374964685745E-15)) ;
#80557 = DIRECTION('ref_axis',(0.,-5.29374964685745E-15,1.)) ;
#80558 = DIRECTION('center_axis',(0.,1.,0.)) ;
#80559 = DIRECTION('ref_axis',(1.,0.,0.)) ;
#80560 = DIRECTION('center_axis',(0.,6.45175738210751E-15,1.)) ;
#80561 = DIRECTION('ref_axis',(0.,1.,-6.45175738210751E-15)) ;
#80562 = DIRECTION('center_axis',(-1.,-6.67201336914158E-17,0.)) ;
#80563 = DIRECTION('ref_axis',(6.67201336914158E-17,-1.,0.)) ;
#80564 = DIRECTION('center_axis',(-1.,-6.67201336914158E-17,0.)) ;
#80565 = DIRECTION('ref_axis',(6.67201336914158E-17,-1.,0.)) ;
#80566 = DIRECTION('center_axis',(1.,-1.33440267382831E-16,0.)) ;
#80567 = DIRECTION('ref_axis',(1.33440267382831E-16,1.,0.)) ;
#80568 = DIRECTION('center_axis',(-1.,1.33440267382831E-16,0.)) ;
#80569 = DIRECTION('ref_axis',(1.33440267382831E-16,1.,0.)) ;
#80570 = DIRECTION('center_axis',(0.,1.,0.)) ;
#80571 = DIRECTION('ref_axis',(1.,0.,0.)) ;
#80572 = DIRECTION('center_axis',(1.76182853028896E-15,-1.23327997120227E-15,
1.)) ;
#80573 = DIRECTION('ref_axis',(-1.,7.2314321996121E-47,1.76182853028896E-15)) ;
#80574 = DIRECTION('center_axis',(0.,0.,-1.)) ;
#80575 = DIRECTION('ref_axis',(-1.,0.,0.)) ;
#80576 = DIRECTION('center_axis',(-2.71050543121378E-16,-1.89735380184965E-16,
1.)) ;
#80577 = DIRECTION('ref_axis',(1.,-2.13821176807699E-48,2.71050543121378E-16)) ;
#80578 = DIRECTION('center_axis',(-0.710669054518702,-0.497468338163091,0.497468338163091)) ;
#80579 = DIRECTION('ref_axis',(0.573462344363328,-0.819231920519041,3.92980824865032E-16)) ;
#80580 = DIRECTION('center_axis',(0.710669054518702,0.497468338163091,-0.497468338163091)) ;
#80581 = DIRECTION('ref_axis',(0.573462344363328,-0.819231920519041,3.92980824865032E-16)) ;
#80582 = DIRECTION('center_axis',(0.710669054518701,0.497468338163091,-0.497468338163092)) ;
#80583 = DIRECTION('ref_axis',(-0.573462344363329,-1.81914022221326E-16,-0.81923192051904)) ;
#80584 = DIRECTION('center_axis',(0.710669054518702,-0.497468338163091,-0.497468338163091)) ;
#80585 = DIRECTION('ref_axis',(0.573462344363328,0.819231920519041,6.69271761853466E-16)) ;
#80586 = DIRECTION('center_axis',(0.710669054518702,-0.497468338163091,-0.497468338163091)) ;
#80587 = DIRECTION('ref_axis',(0.573462344363328,0.819231920519041,6.69271761853466E-16)) ;
#80588 = DIRECTION('center_axis',(0.7106690545187,-0.497468338163091,-0.497468338163093)) ;
#80589 = DIRECTION('ref_axis',(-0.573462344363331,2.8326473018354E-16,-0.819231920519039)) ;
#80590 = DIRECTION('center_axis',(0.,0.,-1.)) ;
#80591 = DIRECTION('ref_axis',(-1.,0.,0.)) ;
#80592 = DIRECTION('center_axis',(0.,1.15800773525007E-15,1.)) ;
#80593 = DIRECTION('ref_axis',(0.,-1.,1.15800773525007E-15)) ;
#80594 = DIRECTION('center_axis',(0.,1.,0.)) ;
#80595 = DIRECTION('ref_axis',(1.,0.,0.)) ;
#80596 = DIRECTION('center_axis',(0.,1.,0.)) ;
#80597 = DIRECTION('ref_axis',(0.,0.,-1.)) ;
#80598 = DIRECTION('center_axis',(0.,1.,0.)) ;
#80599 = DIRECTION('ref_axis',(1.,0.,0.)) ;
#80600 = DIRECTION('center_axis',(4.33680868994204E-15,-1.,-3.03576608295944E-15)) ;
#80601 = DIRECTION('ref_axis',(-1.,-4.33680868994205E-15,4.47233396150273E-15)) ;
#80602 = DIRECTION('center_axis',(0.,1.,9.34081871679819E-17)) ;
#80603 = DIRECTION('ref_axis',(0.,-9.34081871679819E-17,1.)) ;
#80604 = DIRECTION('center_axis',(0.,0.,1.)) ;
#80605 = DIRECTION('ref_axis',(1.,0.,0.)) ;
#80606 = DIRECTION('center_axis',(-2.16840434497102E-15,-3.61400724161847E-16,
1.)) ;
#80607 = DIRECTION('ref_axis',(1.,1.51670488080685E-47,2.16840434497102E-15)) ;
#80608 = DIRECTION('center_axis',(0.973328526784575,0.162221421130762,-0.162221421130763)) ;
#80609 = DIRECTION('ref_axis',(-0.164398987305358,5.99282649549846E-16,-0.986393923832144)) ;
#80610 = DIRECTION('center_axis',(0.973328526784574,0.162221421130765,-0.162221421130767)) ;
#80611 = DIRECTION('ref_axis',(-0.164398987305362,8.41797083535674E-17,-0.986393923832143)) ;
#80612 = DIRECTION('center_axis',(0.,1.,0.)) ;
#80613 = DIRECTION('ref_axis',(1.,0.,0.)) ;
#80614 = DIRECTION('center_axis',(0.,1.,-8.79325913341701E-15)) ;
#80615 = DIRECTION('ref_axis',(0.,-8.79325913341701E-15,-1.)) ;
#80616 = DIRECTION('center_axis',(0.,0.,1.)) ;
#80617 = DIRECTION('ref_axis',(1.,0.,0.)) ;
#80618 = DIRECTION('center_axis',(0.,-2.28569887277128E-15,1.)) ;
#80619 = DIRECTION('ref_axis',(0.,-1.,-2.28569887277128E-15)) ;
#80620 = DIRECTION('center_axis',(1.73472347597681E-15,-1.,-2.89120579329468E-16)) ;
#80621 = DIRECTION('ref_axis',(1.,1.73472347597681E-15,5.01544256350843E-31)) ;
#80622 = DIRECTION('center_axis',(8.67361737988409E-15,1.,-1.44560289664739E-15)) ;
#80623 = DIRECTION('ref_axis',(-1.,8.67361737988409E-15,-1.40129846432482E-45)) ;
#80624 = DIRECTION('center_axis',(0.,1.,0.)) ;
#80625 = DIRECTION('ref_axis',(1.,0.,0.)) ;
#80626 = DIRECTION('center_axis',(-0.937042571331634,0.312347523777217,0.156173761888611)) ;
#80627 = DIRECTION('ref_axis',(0.316227766016843,0.948683298050512,6.71158276827649E-18)) ;
#80628 = DIRECTION('center_axis',(0.937042571331636,-0.312347523777212,-0.156173761888606)) ;
#80629 = DIRECTION('ref_axis',(0.316227766016838,0.948683298050514,8.61595672567599E-16)) ;
#80630 = DIRECTION('center_axis',(-0.973328526784575,-0.162221421130762,-0.162221421130763)) ;
#80631 = DIRECTION('ref_axis',(-0.164398987305358,5.99282649549846E-16,0.986393923832144)) ;
#80632 = DIRECTION('center_axis',(0.978231976292118,-0.146734796047265,-0.146734795425574)) ;
#80633 = DIRECTION('ref_axis',(0.182318633552554,0.945435290892317,0.270022270553542)) ;
#80634 = DIRECTION('center_axis',(0.973328526784574,0.162221421130767,0.162221421130768)) ;
#80635 = DIRECTION('ref_axis',(0.164398987305363,1.28476843531205E-16,-0.986393923832143)) ;
#80636 = DIRECTION('center_axis',(0.,0.,1.)) ;
#80637 = DIRECTION('ref_axis',(1.,0.,0.)) ;
#80638 = DIRECTION('center_axis',(0.,2.19831478335425E-15,-1.)) ;
#80639 = DIRECTION('ref_axis',(0.,1.,2.19831478335425E-15)) ;
#80640 = DIRECTION('center_axis',(0.,1.,0.)) ;
#80641 = DIRECTION('ref_axis',(1.,0.,0.)) ;
#80642 = DIRECTION('center_axis',(8.67361737988408E-15,1.,1.44560289664739E-15)) ;
#80643 = DIRECTION('ref_axis',(1.,-8.67361737988408E-15,5.60519385729927E-45)) ;
#80644 = DIRECTION('center_axis',(1.73472347597681E-15,-1.,2.89120579329468E-16)) ;
#80645 = DIRECTION('ref_axis',(1.,1.73472347597681E-15,-5.01544256350843E-31)) ;
#80646 = DIRECTION('center_axis',(0.,1.,0.)) ;
#80647 = DIRECTION('ref_axis',(0.,0.,1.)) ;
#80648 = DIRECTION('center_axis',(0.,0.,1.)) ;
#80649 = DIRECTION('ref_axis',(1.,0.,0.)) ;
#80650 = DIRECTION('center_axis',(3.25260651745652E-15,-1.08420217248553E-15,
-1.)) ;
#80651 = DIRECTION('ref_axis',(-1.,9.53266123289697E-45,-3.25260651745652E-15)) ;
#80652 = DIRECTION('center_axis',(0.,1.,0.)) ;
#80653 = DIRECTION('ref_axis',(1.,0.,0.)) ;
#80654 = DIRECTION('center_axis',(-0.937042571331635,0.312347523777215,-0.15617376188861)) ;
#80655 = DIRECTION('ref_axis',(0.316227766016841,0.948683298050513,6.5590042956861E-18)) ;
#80656 = DIRECTION('center_axis',(-0.937042571331636,0.312347523777212,-0.156173761888606)) ;
#80657 = DIRECTION('ref_axis',(0.331350514299571,0.654034959159569,-0.680033167478286)) ;
#80658 = DIRECTION('center_axis',(0.961519724091138,0.245047216428683,-0.124224320904791)) ;
#80659 = DIRECTION('ref_axis',(0.262092069891023,-0.682554728199521,0.682221950623634)) ;
#80660 = DIRECTION('center_axis',(2.65552944032596E-32,3.29043518662928E-48,
-1.)) ;
#80661 = DIRECTION('ref_axis',(-1.,1.31155984465371E-95,-2.65552944032596E-32)) ;
#80662 = DIRECTION('center_axis',(2.65552944032596E-32,3.29043518662928E-48,
-1.)) ;
#80663 = DIRECTION('ref_axis',(-1.,8.7378475095785E-80,-2.65552944032596E-32)) ;
#80664 = DIRECTION('center_axis',(-2.65552944032596E-32,-3.29043518662928E-48,
1.)) ;
#80665 = DIRECTION('ref_axis',(-1.,8.7378475095785E-80,-2.65552944032596E-32)) ;
#80666 = DIRECTION('center_axis',(0.,0.,1.)) ;
#80667 = DIRECTION('ref_axis',(1.,0.,0.)) ;
#80668 = DIRECTION('center_axis',(0.,0.,-1.)) ;
#80669 = DIRECTION('ref_axis',(-1.,0.,0.)) ;
#80670 = DIRECTION('center_axis',(0.,0.,1.)) ;
#80671 = DIRECTION('ref_axis',(1.,0.,0.)) ;
#80672 = DIRECTION('center_axis',(0.,0.,1.)) ;
#80673 = DIRECTION('ref_axis',(1.,0.,0.)) ;
#80674 = DIRECTION('center_axis',(0.,0.,-1.)) ;
#80675 = DIRECTION('ref_axis',(-1.,0.,0.)) ;
#80676 = DIRECTION('center_axis',(0.,0.,-1.)) ;
#80677 = DIRECTION('ref_axis',(-1.,0.,0.)) ;
#80678 = DIRECTION('center_axis',(1.,1.15648231731787E-15,0.)) ;
#80679 = DIRECTION('ref_axis',(1.03435541192675E-15,-1.,7.6571373978539E-16)) ;
#80680 = DIRECTION('center_axis',(7.089177613099E-16,-0.612994899008946,-0.790086864711098)) ;
#80681 = DIRECTION('ref_axis',(-4.46849810277083E-31,-0.790086864711098,0.612994899008946)) ;
#80682 = DIRECTION('center_axis',(7.08917761309899E-16,-0.612994899008945,
0.790086864711098)) ;
#80683 = DIRECTION('ref_axis',(-1.73472347597681E-14,0.790086864711098,0.612994899008945)) ;
#80684 = DIRECTION('center_axis',(0.,0.,-1.)) ;
#80685 = DIRECTION('ref_axis',(-1.,0.,0.)) ;
#80686 = DIRECTION('center_axis',(0.,0.,1.)) ;
#80687 = DIRECTION('ref_axis',(-1.,2.16840434497102E-15,0.)) ;
#80688 = DIRECTION('center_axis',(1.08420217248551E-15,-1.,0.)) ;
#80689 = DIRECTION('ref_axis',(1.,1.08420217248551E-15,0.)) ;
#80690 = DIRECTION('center_axis',(1.44560289664734E-16,-1.,-2.4093381610789E-16)) ;
#80691 = DIRECTION('ref_axis',(2.05395038580596E-47,2.4093381610789E-16,-1.)) ;
#80692 = DIRECTION('center_axis',(0.,-1.,0.)) ;
#80693 = DIRECTION('ref_axis',(0.,0.,-1.)) ;
#80694 = DIRECTION('center_axis',(1.,0.,0.)) ;
#80695 = DIRECTION('ref_axis',(0.,1.,0.)) ;
#80696 = DIRECTION('center_axis',(1.,0.,0.)) ;
#80697 = DIRECTION('ref_axis',(0.,0.,-1.)) ;
#80698 = DIRECTION('center_axis',(1.,1.23908819712629E-16,8.95614743483648E-33)) ;
#80699 = DIRECTION('ref_axis',(-1.23908819712629E-16,1.,-1.10974565782288E-48)) ;
#80700 = DIRECTION('center_axis',(1.,0.,0.)) ;
#80701 = DIRECTION('ref_axis',(0.,0.,-1.)) ;
#80702 = DIRECTION('center_axis',(-1.,0.,0.)) ;
#80703 = DIRECTION('ref_axis',(0.,0.,1.)) ;
#80704 = DIRECTION('center_axis',(1.,1.23908819712629E-16,8.95614743483648E-33)) ;
#80705 = DIRECTION('ref_axis',(-1.23908819712629E-16,1.,-1.10974565782288E-48)) ;
#80706 = DIRECTION('center_axis',(-1.,0.,0.)) ;
#80707 = DIRECTION('ref_axis',(0.,0.,1.)) ;
#80708 = DIRECTION('center_axis',(1.,0.,0.)) ;
#80709 = DIRECTION('ref_axis',(0.,-1.,0.)) ;
#80710 = DIRECTION('center_axis',(0.,1.,0.)) ;
#80711 = DIRECTION('ref_axis',(0.,0.,1.)) ;
#80712 = DIRECTION('center_axis',(-1.44560289664734E-16,1.,-7.2280144832367E-17)) ;
#80713 = DIRECTION('ref_axis',(0.707106781238322,1.5332934167208E-16,0.707106781134773)) ;
#80714 = DIRECTION('center_axis',(-1.0842021724855E-15,1.,0.)) ;
#80715 = DIRECTION('ref_axis',(-1.,-1.0842021724855E-15,0.)) ;
#80716 = DIRECTION('center_axis',(0.,1.,0.)) ;
#80717 = DIRECTION('ref_axis',(0.,0.,1.)) ;
#80718 = DIRECTION('center_axis',(0.,-1.,0.)) ;
#80719 = DIRECTION('ref_axis',(0.,0.,-1.)) ;
#80720 = DIRECTION('center_axis',(0.,1.,0.)) ;
#80721 = DIRECTION('ref_axis',(0.,0.,1.)) ;
#80722 = DIRECTION('center_axis',(0.,0.,1.)) ;
#80723 = DIRECTION('ref_axis',(1.,0.,0.)) ;
#80724 = DIRECTION('center_axis',(0.431191646767813,0.0335421424156054,0.901636672080186)) ;
#80725 = DIRECTION('ref_axis',(0.899826811311216,0.0573593277252533,-0.432459960190994)) ;
#80726 = DIRECTION('center_axis',(0.,0.,1.)) ;
#80727 = DIRECTION('ref_axis',(-1.,0.,0.)) ;
#80728 = DIRECTION('center_axis',(0.,0.,-1.)) ;
#80729 = DIRECTION('ref_axis',(0.707109343403322,-0.707104218960488,0.)) ;
#80730 = DIRECTION('center_axis',(-3.25260651745653E-15,0.,1.)) ;
#80731 = DIRECTION('ref_axis',(1.,0.,3.25260651745653E-15)) ;
#80732 = DIRECTION('center_axis',(0.,0.,1.)) ;
#80733 = DIRECTION('ref_axis',(1.,0.,0.)) ;
#80734 = DIRECTION('center_axis',(0.431188264323706,0.0335835000991875,-0.901636750155293)) ;
#80735 = DIRECTION('ref_axis',(0.899831768190665,0.0572892318879771,0.432458937778544)) ;
#80736 = DIRECTION('center_axis',(0.,-1.,0.)) ;
#80737 = DIRECTION('ref_axis',(0.,0.,-1.)) ;
#80738 = DIRECTION('center_axis',(0.,1.,0.)) ;
#80739 = DIRECTION('ref_axis',(0.,0.,1.)) ;
#80740 = DIRECTION('center_axis',(0.,0.,1.)) ;
#80741 = DIRECTION('ref_axis',(1.,0.,0.)) ;
#80742 = DIRECTION('center_axis',(0.,0.,-1.)) ;
#80743 = DIRECTION('ref_axis',(-1.,0.,0.)) ;
#80744 = DIRECTION('center_axis',(0.,0.,1.)) ;
#80745 = DIRECTION('ref_axis',(-0.986393923832144,0.164398987305354,0.)) ;
#80746 = DIRECTION('center_axis',(0.98470178743927,-0.164116964573216,0.0585492250433781)) ;
#80747 = DIRECTION('ref_axis',(0.164398987305362,0.986393923832143,-7.60669428566932E-17)) ;
#80748 = DIRECTION('center_axis',(0.984834538781277,-0.164139089796902,0.0562075655416074)) ;
#80749 = DIRECTION('ref_axis',(0.164398987305379,0.98639392383214,1.87706412796466E-17)) ;
#80750 = DIRECTION('center_axis',(0.986393923832144,-0.129889480441767,0.100775740620418)) ;
#80751 = DIRECTION('ref_axis',(0.,0.612994899008947,0.790086864711097)) ;
#80752 = DIRECTION('center_axis',(0.,1.,0.)) ;
#80753 = DIRECTION('ref_axis',(1.,0.,0.)) ;
#80754 = DIRECTION('center_axis',(0.,0.,-1.)) ;
#80755 = DIRECTION('ref_axis',(-1.,0.,0.)) ;
#80756 = DIRECTION('center_axis',(1.,2.8359373108165E-15,0.)) ;
#80757 = DIRECTION('ref_axis',(-2.8359373108165E-15,1.,0.)) ;
#80758 = DIRECTION('center_axis',(0.,0.,-1.)) ;
#80759 = DIRECTION('ref_axis',(-1.,0.,0.)) ;
#80760 = DIRECTION('center_axis',(0.,0.,1.)) ;
#80761 = DIRECTION('ref_axis',(1.,0.,0.)) ;
#80762 = DIRECTION('center_axis',(1.,0.,0.)) ;
#80763 = DIRECTION('ref_axis',(0.,0.,-1.)) ;
#80764 = DIRECTION('center_axis',(1.,0.,0.)) ;
#80765 = DIRECTION('ref_axis',(0.,0.,-1.)) ;
#80766 = DIRECTION('center_axis',(0.,1.,0.)) ;
#80767 = DIRECTION('ref_axis',(1.,0.,0.)) ;
#80768 = DIRECTION('center_axis',(1.,-8.50781193244945E-15,0.)) ;
#80769 = DIRECTION('ref_axis',(8.50781193244945E-15,1.,0.)) ;
#80770 = DIRECTION('center_axis',(0.,1.,0.)) ;
#80771 = DIRECTION('ref_axis',(1.,0.,0.)) ;
#80772 = DIRECTION('center_axis',(-5.42101086242753E-16,1.70882313734897E-16,
1.)) ;
#80773 = DIRECTION('ref_axis',(1.,9.53096053428495E-47,5.42101086242753E-16)) ;
#80774 = DIRECTION('center_axis',(-1.,0.,0.)) ;
#80775 = DIRECTION('ref_axis',(0.,0.,1.)) ;
#80776 = DIRECTION('center_axis',(1.,0.,0.)) ;
#80777 = DIRECTION('ref_axis',(0.,0.,-1.)) ;
#80778 = DIRECTION('center_axis',(0.,0.,-1.)) ;
#80779 = DIRECTION('ref_axis',(-1.,0.,0.)) ;
#80780 = DIRECTION('center_axis',(0.,0.,1.)) ;
#80781 = DIRECTION('ref_axis',(1.,0.,0.)) ;
#80782 = DIRECTION('center_axis',(0.,1.,0.)) ;
#80783 = DIRECTION('ref_axis',(1.,0.,0.)) ;
#80784 = DIRECTION('center_axis',(0.,1.,0.)) ;
#80785 = DIRECTION('ref_axis',(1.,0.,0.)) ;
#80786 = DIRECTION('center_axis',(0.,0.,-1.)) ;
#80787 = DIRECTION('ref_axis',(-1.,0.,0.)) ;
#80788 = DIRECTION('center_axis',(0.,1.,0.)) ;
#80789 = DIRECTION('ref_axis',(0.,0.,1.)) ;
#80790 = DIRECTION('center_axis',(0.,0.,-1.)) ;
#80791 = DIRECTION('ref_axis',(-1.,0.,0.)) ;
#80792 = DIRECTION('center_axis',(0.,0.,1.)) ;
#80793 = DIRECTION('ref_axis',(1.,0.,0.)) ;
#80794 = DIRECTION('center_axis',(1.33440267382831E-16,1.,0.)) ;
#80795 = DIRECTION('ref_axis',(-1.,1.33440267382831E-16,0.)) ;
#80796 = DIRECTION('center_axis',(0.,1.,0.)) ;
#80797 = DIRECTION('ref_axis',(0.,0.,1.)) ;
#80798 = DIRECTION('center_axis',(0.,1.,0.)) ;
#80799 = DIRECTION('ref_axis',(1.,0.,0.)) ;
#80800 = DIRECTION('center_axis',(0.,1.,0.)) ;
#80801 = DIRECTION('ref_axis',(0.,0.,1.)) ;
#80802 = DIRECTION('center_axis',(0.,1.,0.)) ;
#80803 = DIRECTION('ref_axis',(1.,0.,0.)) ;
#80804 = DIRECTION('center_axis',(1.37797793267296E-15,-1.62630325872825E-15,
1.)) ;
#80805 = DIRECTION('ref_axis',(0.,-1.,-1.62630325872825E-15)) ;
#80806 = DIRECTION('center_axis',(-1.33440267382831E-16,-1.,0.)) ;
#80807 = DIRECTION('ref_axis',(1.,-1.33440267382831E-16,0.)) ;
#80808 = DIRECTION('center_axis',(0.,1.,0.)) ;
#80809 = DIRECTION('ref_axis',(0.,0.,1.)) ;
#80810 = DIRECTION('center_axis',(0.,0.,-1.)) ;
#80811 = DIRECTION('ref_axis',(-1.,0.,0.)) ;
#80812 = DIRECTION('center_axis',(0.,0.,1.)) ;
#80813 = DIRECTION('ref_axis',(1.,0.,0.)) ;
#80814 = DIRECTION('center_axis',(0.,1.,0.)) ;
#80815 = DIRECTION('ref_axis',(1.,0.,0.)) ;
#80816 = DIRECTION('center_axis',(0.,0.,1.)) ;
#80817 = DIRECTION('ref_axis',(1.,0.,0.)) ;
#80818 = DIRECTION('center_axis',(0.,0.,1.)) ;
#80819 = DIRECTION('ref_axis',(1.,0.,0.)) ;
#80820 = DIRECTION('center_axis',(0.,0.,1.)) ;
#80821 = DIRECTION('ref_axis',(-0.986393923832144,0.164398987305354,0.)) ;
#80822 = DIRECTION('center_axis',(0.984701787439272,-0.164116964573205,-0.0585492250433871)) ;
#80823 = DIRECTION('ref_axis',(0.16439898730535,0.986393923832145,-3.2807868055655E-16)) ;
#80824 = DIRECTION('center_axis',(0.984834538781259,-0.164139089796881,-0.0562075655419907)) ;
#80825 = DIRECTION('ref_axis',(0.164398987305362,0.986393923832143,6.03508511856301E-17)) ;
#80826 = DIRECTION('center_axis',(0.,0.,1.)) ;
#80827 = DIRECTION('ref_axis',(-0.986393923832144,0.164398987305354,0.)) ;
#80828 = DIRECTION('center_axis',(0.,0.,1.)) ;
#80829 = DIRECTION('ref_axis',(1.,0.,0.)) ;
#80830 = DIRECTION('center_axis',(0.342346838791424,0.100237737316009,-0.934211452502744)) ;
#80831 = DIRECTION('ref_axis',(0.878411850255022,0.318727802445567,0.356097190777698)) ;
#80832 = DIRECTION('center_axis',(0.,0.,-1.)) ;
#80833 = DIRECTION('ref_axis',(-1.,0.,0.)) ;
#80834 = DIRECTION('center_axis',(0.,0.,-1.)) ;
#80835 = DIRECTION('ref_axis',(-1.,0.,0.)) ;
#80836 = DIRECTION('center_axis',(0.,0.,-1.)) ;
#80837 = DIRECTION('ref_axis',(-1.,0.,0.)) ;
#80838 = DIRECTION('center_axis',(-0.342346838792776,-0.10023773732969,-0.93421145250078)) ;
#80839 = DIRECTION('ref_axis',(0.87841177851845,0.318728005207571,-0.35609718625181)) ;
#80840 = DIRECTION('center_axis',(0.,0.,1.)) ;
#80841 = DIRECTION('ref_axis',(1.,0.,0.)) ;
#80842 = DIRECTION('center_axis',(0.967224433277961,0.251696850864675,0.0335498276438615)) ;
#80843 = DIRECTION('ref_axis',(0.148186136307302,-0.666803827414714,0.730351644587319)) ;
#80844 = DIRECTION('center_axis',(0.,0.707106781186549,-0.707106781186547)) ;
#80845 = DIRECTION('ref_axis',(0.,0.707106781186546,0.707106781186549)) ;
#80846 = DIRECTION('center_axis',(0.978007532938632,-0.147978541149458,-0.146981688909092)) ;
#80847 = DIRECTION('ref_axis',(0.193734423934244,0.383507624640146,0.902988856423898)) ;
#80848 = DIRECTION('center_axis',(0.,0.447213595499958,0.894427190999916)) ;
#80849 = DIRECTION('ref_axis',(0.,-0.894427190999916,0.447213595499958)) ;
#80850 = DIRECTION('center_axis',(0.960001452008144,0.250435160947709,-0.125217579849438)) ;
#80851 = DIRECTION('ref_axis',(0.276742394168032,-0.916645079798508,0.288401534238868)) ;
#80852 = DIRECTION('center_axis',(0.,1.,0.)) ;
#80853 = DIRECTION('ref_axis',(0.,0.,1.)) ;
#80854 = DIRECTION('center_axis',(-1.,-1.19199144472199E-13,1.20231350744192E-12)) ;
#80855 = DIRECTION('ref_axis',(-1.14382718901782E-12,0.413905147578545,-0.91032001450478)) ;
#80856 = DIRECTION('center_axis',(1.,1.44560289664734E-16,0.)) ;
#80857 = DIRECTION('ref_axis',(0.,1.,0.)) ;
#80858 = DIRECTION('center_axis',(1.,1.44560289664734E-16,0.)) ;
#80859 = DIRECTION('ref_axis',(-1.44560289664734E-16,1.,0.)) ;
#80860 = DIRECTION('center_axis',(0.,0.,-1.)) ;
#80861 = DIRECTION('ref_axis',(0.,-1.,0.)) ;
#80862 = DIRECTION('center_axis',(-1.,-1.44560289664734E-16,0.)) ;
#80863 = DIRECTION('ref_axis',(-1.44560289664734E-16,1.,0.)) ;
#80864 = DIRECTION('center_axis',(1.,-3.46944695195361E-16,0.)) ;
#80865 = DIRECTION('ref_axis',(2.61228946970625E-16,1.,0.)) ;
#80866 = DIRECTION('center_axis',(1.,-3.46944695195361E-16,0.)) ;
#80867 = DIRECTION('ref_axis',(3.46944695195361E-16,1.,0.)) ;
#80868 = DIRECTION('center_axis',(0.,0.,1.)) ;
#80869 = DIRECTION('ref_axis',(-3.26536183713281E-16,-1.,0.)) ;
#80870 = DIRECTION('center_axis',(-1.,3.46944695195361E-16,0.)) ;
#80871 = DIRECTION('ref_axis',(3.46944695195361E-16,1.,0.)) ;
#80872 = DIRECTION('center_axis',(-1.,3.46944695195361E-16,0.)) ;
#80873 = DIRECTION('ref_axis',(-3.46944695195361E-16,-1.,0.)) ;
#80874 = DIRECTION('center_axis',(-1.,0.,0.)) ;
#80875 = DIRECTION('ref_axis',(0.,0.,1.)) ;
#80876 = DIRECTION('',(1.,-3.46944695195361E-16,0.)) ;
#80877 = DIRECTION('center_axis',(-1.,8.01625584951926E-16,-1.08420217248551E-15)) ;
#80878 = DIRECTION('ref_axis',(1.08420217248551E-15,2.168404344971E-15,-1.)) ;
#80879 = DIRECTION('center_axis',(-1.,8.01625584951926E-16,-1.08420217248551E-15)) ;
#80880 = DIRECTION('ref_axis',(1.08420217248551E-15,2.168404344971E-15,-1.)) ;
#80881 = DIRECTION('',(-1.,3.46944695195361E-16,0.)) ;
#80882 = DIRECTION('center_axis',(-1.,3.46944695195361E-16,0.)) ;
#80883 = DIRECTION('ref_axis',(-3.46944695195361E-16,-1.,0.)) ;
#80884 = DIRECTION('center_axis',(-1.,0.,0.)) ;
#80885 = DIRECTION('ref_axis',(0.,0.,1.)) ;
#80886 = DIRECTION('',(1.,-3.46944695195361E-16,0.)) ;
#80887 = DIRECTION('center_axis',(-1.,2.2680138501079E-15,0.)) ;
#80888 = DIRECTION('ref_axis',(2.2680138501079E-15,1.,0.)) ;
#80889 = DIRECTION('',(-1.,3.46944695195361E-16,0.)) ;
#80890 = DIRECTION('center_axis',(-1.,3.18032637262401E-16,0.)) ;
#80891 = DIRECTION('ref_axis',(-5.55111512312578E-16,-1.,0.)) ;
#80892 = DIRECTION('center_axis',(1.,-3.18032637262401E-16,0.)) ;
#80893 = DIRECTION('ref_axis',(-3.18032637262401E-16,-1.,0.)) ;
#80894 = DIRECTION('center_axis',(-2.01298417874256E-16,-0.632948931301568,
-0.774193548387096)) ;
#80895 = DIRECTION('ref_axis',(1.73472347597681E-14,-0.774193548387096,0.632948931301568)) ;
#80896 = DIRECTION('center_axis',(-1.,3.18032637262401E-16,0.)) ;
#80897 = DIRECTION('ref_axis',(-3.18032637262401E-16,-1.,0.)) ;
#80898 = DIRECTION('center_axis',(-2.01298417874256E-16,-0.632948931301568,
0.774193548387096)) ;
#80899 = DIRECTION('ref_axis',(9.63584817660562E-32,-0.774193548387096,-0.632948931301568)) ;
#80900 = DIRECTION('center_axis',(1.,1.44560289664734E-16,0.)) ;
#80901 = DIRECTION('ref_axis',(-1.44560289664734E-16,1.,0.)) ;
#80902 = DIRECTION('',(-1.,-1.44560289664734E-16,0.)) ;
#80903 = DIRECTION('center_axis',(-1.,3.46944695195361E-16,0.)) ;
#80904 = DIRECTION('ref_axis',(-3.46944695195361E-16,-1.,0.)) ;
#80905 = DIRECTION('',(-1.,3.46944695195361E-16,0.)) ;
#80906 = DIRECTION('center_axis',(-1.,3.46944695195361E-16,0.)) ;
#80907 = DIRECTION('ref_axis',(3.46944695195361E-16,1.,3.46944695195361E-15)) ;
#80908 = DIRECTION('center_axis',(-1.,3.46944695195361E-16,0.)) ;
#80909 = DIRECTION('ref_axis',(3.46944695195361E-16,1.,0.)) ;
#80910 = DIRECTION('center_axis',(-1.,3.46944695195361E-16,0.)) ;
#80911 = DIRECTION('ref_axis',(-3.46944695195361E-16,-1.,0.)) ;
#80912 = DIRECTION('',(1.,-3.46944695195361E-16,0.)) ;
#80913 = DIRECTION('center_axis',(-1.,-1.44560289664734E-16,-2.65552944032596E-32)) ;
#80914 = DIRECTION('ref_axis',(1.44560289664734E-16,-1.,-2.80018320648271E-64)) ;
#80915 = DIRECTION('',(2.65552944032596E-32,3.29043518662928E-48,-1.)) ;
#80916 = DIRECTION('',(1.44560289664734E-16,-1.,-2.4093381610789E-16)) ;
#80917 = DIRECTION('',(0.,0.,1.)) ;
#80918 = DIRECTION('center_axis',(0.999999956301289,0.000282786981237219,
8.61913163216796E-5)) ;
#80919 = DIRECTION('ref_axis',(0.000288266391068138,-0.99739627340708,-0.0721151211339053)) ;
#80920 = DIRECTION('',(-1.44560289664734E-16,1.,-7.2280144832367E-17)) ;
#80921 = DIRECTION('center_axis',(0.316227766016838,0.948683298050514,0.)) ;
#80922 = DIRECTION('ref_axis',(-0.948683298050514,0.316227766016838,0.)) ;
#80923 = DIRECTION('',(-0.948683298050514,0.316227766016838,0.)) ;
#80924 = DIRECTION('',(0.,0.,1.)) ;
#80925 = DIRECTION('',(0.937042571331636,-0.312347523777212,-0.156173761888606)) ;
#80926 = DIRECTION('',(0.,0.,-1.)) ;
#80927 = DIRECTION('center_axis',(1.,1.73472347597681E-15,0.)) ;
#80928 = DIRECTION('ref_axis',(-1.73472347597681E-15,1.,0.)) ;
#80929 = DIRECTION('',(-1.73472347597681E-15,1.,0.)) ;
#80930 = DIRECTION('',(0.,0.,1.)) ;
#80931 = DIRECTION('',(1.73472347597681E-15,-1.,-2.89120579329468E-16)) ;
#80932 = DIRECTION('',(0.,0.,-1.)) ;
#80933 = DIRECTION('center_axis',(0.164398987305357,-0.986393923832144,0.)) ;
#80934 = DIRECTION('ref_axis',(0.986393923832144,0.164398987305357,0.)) ;
#80935 = DIRECTION('',(-0.973328526784575,-0.162221421130762,0.162221421130763)) ;
#80936 = DIRECTION('',(0.,0.,-1.)) ;
#80937 = DIRECTION('',(0.986393923832144,0.164398987305357,0.)) ;
#80938 = DIRECTION('',(0.,0.,1.)) ;
#80939 = DIRECTION('center_axis',(-9.91270557701033E-17,1.,0.)) ;
#80940 = DIRECTION('ref_axis',(-1.,-9.91270557701033E-17,0.)) ;
#80941 = DIRECTION('',(1.,9.91270557701033E-17,0.)) ;
#80942 = DIRECTION('',(0.,0.,-1.)) ;
#80943 = DIRECTION('',(-1.,-9.91270557701033E-17,0.)) ;
#80944 = DIRECTION('',(0.,0.,1.)) ;
#80945 = DIRECTION('center_axis',(-9.91270557701033E-17,1.,0.)) ;
#80946 = DIRECTION('ref_axis',(-1.,-9.91270557701033E-17,0.)) ;
#80947 = DIRECTION('',(-1.,-9.91270557701033E-17,0.)) ;
#80948 = DIRECTION('',(0.,0.,-1.)) ;
#80949 = DIRECTION('',(-1.,-9.91270557701033E-17,0.)) ;
#80950 = DIRECTION('',(0.,0.,1.)) ;
#80951 = DIRECTION('center_axis',(1.,1.15648231731787E-15,0.)) ;
#80952 = DIRECTION('ref_axis',(-1.15648231731787E-15,1.,0.)) ;
#80953 = DIRECTION('',(-1.15648231731787E-15,1.,0.)) ;
#80954 = DIRECTION('',(0.,0.,-1.)) ;
#80955 = DIRECTION('',(-1.15648231731787E-15,1.,0.)) ;
#80956 = DIRECTION('',(0.,0.,1.)) ;
#80957 = DIRECTION('center_axis',(-1.,-1.15648231731787E-15,0.)) ;
#80958 = DIRECTION('ref_axis',(-1.15648231731787E-15,1.,1.82070621850777E-15)) ;
#80959 = DIRECTION('',(0.,0.,1.)) ;
#80960 = DIRECTION('center_axis',(0.,0.,1.)) ;
#80961 = DIRECTION('ref_axis',(1.,0.,0.)) ;
#80962 = DIRECTION('',(-1.,0.,0.)) ;
#80963 = DIRECTION('center_axis',(0.,0.,-1.)) ;
#80964 = DIRECTION('ref_axis',(1.,0.,0.)) ;
#80965 = DIRECTION('center_axis',(0.,0.,-1.)) ;
#80966 = DIRECTION('ref_axis',(1.,0.,0.)) ;
#80967 = DIRECTION('center_axis',(0.,0.,-1.)) ;
#80968 = DIRECTION('ref_axis',(1.,0.,0.)) ;
#80969 = DIRECTION('center_axis',(0.,0.,-1.)) ;
#80970 = DIRECTION('ref_axis',(1.,0.,0.)) ;
#80971 = DIRECTION('',(1.,0.,0.)) ;
#80972 = DIRECTION('center_axis',(0.,0.,1.)) ;
#80973 = DIRECTION('ref_axis',(1.,0.,0.)) ;
#80974 = DIRECTION('',(3.46944695195361E-16,1.,0.)) ;
#80975 = DIRECTION('center_axis',(0.,0.,1.)) ;
#80976 = DIRECTION('ref_axis',(1.,0.,0.)) ;
#80977 = DIRECTION('',(1.,-3.46944695195361E-16,0.)) ;
#80978 = DIRECTION('center_axis',(0.,0.,-1.)) ;
#80979 = DIRECTION('ref_axis',(1.,0.,0.)) ;
#80980 = DIRECTION('',(2.71050543121376E-16,1.,0.)) ;
#80981 = DIRECTION('center_axis',(0.,0.,-1.)) ;
#80982 = DIRECTION('ref_axis',(1.,0.,0.)) ;
#80983 = DIRECTION('',(-1.,3.46944695195361E-16,0.)) ;
#80984 = DIRECTION('center_axis',(0.,0.,1.)) ;
#80985 = DIRECTION('ref_axis',(1.,0.,0.)) ;
#80986 = DIRECTION('',(3.46944695195361E-16,1.,0.)) ;
#80987 = DIRECTION('center_axis',(0.,0.,1.)) ;
#80988 = DIRECTION('ref_axis',(1.,0.,0.)) ;
#80989 = DIRECTION('center_axis',(0.,0.,-1.)) ;
#80990 = DIRECTION('ref_axis',(1.,0.,0.)) ;
#80991 = DIRECTION('',(0.986393923832144,-0.164398987305354,0.)) ;
#80992 = DIRECTION('center_axis',(0.,0.,-1.)) ;
#80993 = DIRECTION('ref_axis',(1.,-6.50521303491307E-15,0.)) ;
#80994 = DIRECTION('center_axis',(0.,0.,-1.)) ;
#80995 = DIRECTION('ref_axis',(1.,0.,0.)) ;
#80996 = DIRECTION('',(1.,0.,0.)) ;
#80997 = DIRECTION('',(1.13380619344889E-16,-1.,0.)) ;
#80998 = DIRECTION('center_axis',(0.,0.,-1.)) ;
#80999 = DIRECTION('ref_axis',(1.,0.,0.)) ;
#81000 = DIRECTION('',(-1.,-1.92747052886312E-16,0.)) ;
#81001 = DIRECTION('center_axis',(0.,0.,1.)) ;
#81002 = DIRECTION('ref_axis',(1.,0.,0.)) ;
#81003 = DIRECTION('',(0.,-1.,0.)) ;
#81004 = DIRECTION('center_axis',(0.,0.,-1.)) ;
#81005 = DIRECTION('ref_axis',(1.,0.,0.)) ;
#81006 = DIRECTION('center_axis',(0.,0.,1.)) ;
#81007 = DIRECTION('ref_axis',(1.,0.,0.)) ;
#81008 = DIRECTION('',(-0.948683298050514,0.316227766016838,0.)) ;
#81009 = DIRECTION('center_axis',(0.,0.,1.)) ;
#81010 = DIRECTION('ref_axis',(1.,0.,0.)) ;
#81011 = DIRECTION('',(-1.,0.,0.)) ;
#81012 = DIRECTION('center_axis',(0.,0.,1.)) ;
#81013 = DIRECTION('ref_axis',(1.,0.,0.)) ;
#81014 = DIRECTION('',(0.,-1.,0.)) ;
#81015 = DIRECTION('center_axis',(0.,0.,-1.)) ;
#81016 = DIRECTION('ref_axis',(1.,0.,0.)) ;
#81017 = DIRECTION('',(-1.,-1.92747052886312E-16,0.)) ;
#81018 = DIRECTION('center_axis',(0.,0.,1.)) ;
#81019 = DIRECTION('ref_axis',(1.,0.,0.)) ;
#81020 = DIRECTION('',(1.13380619344889E-16,-1.,0.)) ;
#81021 = DIRECTION('',(1.,0.,0.)) ;
#81022 = DIRECTION('center_axis',(0.,0.,1.)) ;
#81023 = DIRECTION('ref_axis',(1.,0.,0.)) ;
#81024 = DIRECTION('center_axis',(0.,0.,1.)) ;
#81025 = DIRECTION('ref_axis',(1.,0.,0.)) ;
#81026 = DIRECTION('',(-0.986393923832144,0.164398987305354,0.)) ;
#81027 = DIRECTION('center_axis',(0.,0.,1.)) ;
#81028 = DIRECTION('ref_axis',(1.,0.,0.)) ;
#81029 = DIRECTION('center_axis',(0.,0.,-1.)) ;
#81030 = DIRECTION('ref_axis',(1.,0.,0.)) ;
#81031 = DIRECTION('',(-3.46944695195361E-16,-1.,0.)) ;
#81032 = DIRECTION('center_axis',(0.,0.,-1.)) ;
#81033 = DIRECTION('ref_axis',(1.,0.,0.)) ;
#81034 = DIRECTION('',(-1.,3.46944695195361E-16,0.)) ;
#81035 = DIRECTION('center_axis',(0.,0.,1.)) ;
#81036 = DIRECTION('ref_axis',(1.,0.,0.)) ;
#81037 = DIRECTION('',(3.46944695195361E-16,1.,0.)) ;
#81038 = DIRECTION('center_axis',(0.,0.,1.)) ;
#81039 = DIRECTION('ref_axis',(1.,0.,0.)) ;
#81040 = DIRECTION('',(1.,-3.46944695195361E-16,0.)) ;
#81041 = DIRECTION('center_axis',(0.,0.,-1.)) ;
#81042 = DIRECTION('ref_axis',(1.,0.,0.)) ;
#81043 = DIRECTION('',(-3.46944695195361E-16,-1.,0.)) ;
#81044 = DIRECTION('center_axis',(0.,0.,-1.)) ;
#81045 = DIRECTION('ref_axis',(1.,0.,0.)) ;
#81046 = DIRECTION('',(1.,0.,0.)) ;
#81047 = DIRECTION('center_axis',(0.,0.,1.)) ;
#81048 = DIRECTION('ref_axis',(1.,0.,0.)) ;
#81049 = DIRECTION('',(0.986393923832144,0.164398987305357,0.)) ;
#81050 = DIRECTION('center_axis',(0.,0.,1.)) ;
#81051 = DIRECTION('ref_axis',(1.,0.,0.)) ;
#81052 = DIRECTION('',(-1.73472347597681E-15,1.,0.)) ;
#81053 = DIRECTION('center_axis',(0.,0.,1.)) ;
#81054 = DIRECTION('ref_axis',(1.,0.,0.)) ;
#81055 = DIRECTION('center_axis',(-1.92747052886312E-16,1.,0.)) ;
#81056 = DIRECTION('ref_axis',(-1.,-1.92747052886312E-16,0.)) ;
#81057 = DIRECTION('',(0.,0.,1.)) ;
#81058 = DIRECTION('',(0.,0.,-1.)) ;
#81059 = DIRECTION('center_axis',(-1.,0.,0.)) ;
#81060 = DIRECTION('ref_axis',(0.,0.,1.)) ;
#81061 = DIRECTION('',(0.,0.,1.)) ;
#81062 = DIRECTION('',(0.,0.,-1.)) ;
#81063 = DIRECTION('center_axis',(0.,1.,0.)) ;
#81064 = DIRECTION('ref_axis',(0.,0.,1.)) ;
#81065 = DIRECTION('',(0.,0.,-1.)) ;
#81066 = DIRECTION('',(0.,0.,1.)) ;
#81067 = DIRECTION('',(0.,0.,-1.)) ;
#81068 = DIRECTION('',(0.,0.,-1.)) ;
#81069 = DIRECTION('center_axis',(0.316227766016838,0.948683298050514,0.)) ;
#81070 = DIRECTION('ref_axis',(-0.948683298050514,0.316227766016838,0.)) ;
#81071 = DIRECTION('center_axis',(-0.316227766016878,-0.9486832980505,-8.70066748967434E-14)) ;
#81072 = DIRECTION('ref_axis',(0.831595960760918,-0.277198653586968,-0.481257794218128)) ;
#81073 = DIRECTION('',(0.,0.,1.)) ;
#81074 = DIRECTION('',(0.,0.,-1.)) ;
#81075 = DIRECTION('',(-0.937042571331636,0.312347523777212,-0.156173761888606)) ;
#81076 = DIRECTION('center_axis',(1.,1.73472347597681E-15,0.)) ;
#81077 = DIRECTION('ref_axis',(-1.73472347597681E-15,1.,0.)) ;
#81078 = DIRECTION('',(-1.73472347597681E-15,1.,-2.89120579329468E-16)) ;
#81079 = DIRECTION('',(0.,0.,1.)) ;
#81080 = DIRECTION('',(0.,0.,-1.)) ;
#81081 = DIRECTION('center_axis',(0.164398987305357,-0.986393923832144,0.)) ;
#81082 = DIRECTION('ref_axis',(0.986393923832144,0.164398987305357,0.)) ;
#81083 = DIRECTION('',(0.973328526784575,0.162221421130762,0.162221421130763)) ;
#81084 = DIRECTION('',(0.,0.,1.)) ;
#81085 = DIRECTION('',(0.,0.,-1.)) ;
#81086 = DIRECTION('center_axis',(0.,-1.,0.)) ;
#81087 = DIRECTION('ref_axis',(0.,0.,-1.)) ;
#81088 = DIRECTION('',(0.,0.,1.)) ;
#81089 = DIRECTION('',(0.,0.,1.)) ;
#81090 = DIRECTION('',(0.,0.,1.)) ;
#81091 = DIRECTION('',(0.,0.,-1.)) ;
#81092 = DIRECTION('',(1.,0.,2.25271179641597E-31)) ;
#81093 = DIRECTION('center_axis',(0.,-1.,0.)) ;
#81094 = DIRECTION('ref_axis',(0.,0.,-1.)) ;
#81095 = DIRECTION('',(0.,0.,-1.)) ;
#81096 = DIRECTION('center_axis',(0.,-1.,0.)) ;
#81097 = DIRECTION('ref_axis',(0.,0.,-1.)) ;
#81098 = DIRECTION('',(-1.,0.,-3.21815970916568E-32)) ;
#81099 = DIRECTION('',(0.,0.,-1.)) ;
#81100 = DIRECTION('center_axis',(1.,-3.46944695195361E-16,0.)) ;
#81101 = DIRECTION('ref_axis',(3.46944695195361E-16,1.,0.)) ;
#81102 = DIRECTION('center_axis',(1.,-3.46944695195361E-16,0.)) ;
#81103 = DIRECTION('ref_axis',(3.46944695195361E-16,1.,0.)) ;
#81104 = DIRECTION('',(1.5529910948782E-31,4.47619207437002E-16,-1.)) ;
#81105 = DIRECTION('',(0.,0.,1.)) ;
#81106 = DIRECTION('center_axis',(1.,-3.46944695195361E-16,0.)) ;
#81107 = DIRECTION('ref_axis',(3.46944695195361E-16,1.,0.)) ;
#81108 = DIRECTION('center_axis',(1.,-3.46944695195361E-16,0.)) ;
#81109 = DIRECTION('ref_axis',(3.46944695195361E-16,1.,0.)) ;
#81110 = DIRECTION('center_axis',(1.,-3.46944695195361E-16,0.)) ;
#81111 = DIRECTION('ref_axis',(3.46944695195361E-16,1.,0.)) ;
#81112 = DIRECTION('',(3.46944695195361E-16,1.,9.27571383489107E-17)) ;
#81113 = DIRECTION('',(0.,0.,1.)) ;
#81114 = DIRECTION('',(-3.46944695195361E-16,-1.,-6.49299968442375E-16)) ;
#81115 = DIRECTION('center_axis',(1.,-3.46944695195361E-16,0.)) ;
#81116 = DIRECTION('ref_axis',(3.46944695195361E-16,1.,0.)) ;
#81117 = DIRECTION('center_axis',(1.,-3.46944695195361E-16,0.)) ;
#81118 = DIRECTION('ref_axis',(3.46944695195361E-16,1.,0.)) ;
#81119 = DIRECTION('center_axis',(1.,-3.46944695195361E-16,0.)) ;
#81120 = DIRECTION('ref_axis',(3.46944695195361E-16,1.,0.)) ;
#81121 = DIRECTION('',(0.,0.,1.)) ;
#81122 = DIRECTION('',(-1.5529910948782E-31,-4.47619207437002E-16,-1.)) ;
#81123 = DIRECTION('center_axis',(1.,-3.46944695195361E-16,0.)) ;
#81124 = DIRECTION('ref_axis',(3.46944695195361E-16,1.,0.)) ;
#81125 = DIRECTION('center_axis',(1.,-3.46944695195361E-16,0.)) ;
#81126 = DIRECTION('ref_axis',(3.46944695195361E-16,1.,0.)) ;
#81127 = DIRECTION('center_axis',(1.,-3.46944695195361E-16,0.)) ;
#81128 = DIRECTION('ref_axis',(3.46944695195361E-16,1.,0.)) ;
#81129 = DIRECTION('',(-3.46944695195361E-16,-1.,-1.06487173641454E-15)) ;
#81130 = DIRECTION('center_axis',(1.,-3.46944695195361E-16,0.)) ;
#81131 = DIRECTION('ref_axis',(3.46944695195361E-16,1.,0.)) ;
#81132 = DIRECTION('',(3.46944695195361E-16,1.,2.45739631480277E-16)) ;
#81133 = DIRECTION('center_axis',(1.,-3.46944695195361E-16,0.)) ;
#81134 = DIRECTION('ref_axis',(3.46944695195361E-16,1.,0.)) ;
#81135 = DIRECTION('center_axis',(1.,-3.46944695195361E-16,0.)) ;
#81136 = DIRECTION('ref_axis',(3.46944695195361E-16,1.,0.)) ;
#81137 = DIRECTION('center_axis',(0.,-1.,0.)) ;
#81138 = DIRECTION('ref_axis',(0.,0.,-1.)) ;
#81139 = DIRECTION('center_axis',(0.,-1.,0.)) ;
#81140 = DIRECTION('ref_axis',(0.,0.,-1.)) ;
#81141 = DIRECTION('',(-1.,0.,-1.40488587213121E-32)) ;
#81142 = DIRECTION('',(0.,0.,1.)) ;
#81143 = DIRECTION('',(0.,0.,1.)) ;
#81144 = DIRECTION('',(0.,0.,1.)) ;
#81145 = DIRECTION('',(1.,0.,1.40488587213121E-32)) ;
#81146 = DIRECTION('center_axis',(0.,-1.,0.)) ;
#81147 = DIRECTION('ref_axis',(0.,0.,-1.)) ;
#81148 = DIRECTION('',(7.2280144832367E-17,0.,-1.)) ;
#81149 = DIRECTION('center_axis',(-1.,-1.13380619344889E-16,0.)) ;
#81150 = DIRECTION('ref_axis',(1.13380619344889E-16,-1.,0.)) ;
#81151 = DIRECTION('center_axis',(-1.,-1.13380619344889E-16,0.)) ;
#81152 = DIRECTION('ref_axis',(1.13380619344889E-16,-1.,0.)) ;
#81153 = DIRECTION('',(1.13380619344889E-16,-1.,1.23908819712629E-16)) ;
#81154 = DIRECTION('',(0.,0.,-1.)) ;
#81155 = DIRECTION('',(-1.13380619344889E-16,1.,-1.23908819712629E-16)) ;
#81156 = DIRECTION('center_axis',(-1.,-1.13380619344889E-16,0.)) ;
#81157 = DIRECTION('ref_axis',(1.13380619344889E-16,-1.,0.)) ;
#81158 = DIRECTION('',(0.,0.,1.)) ;
#81159 = DIRECTION('center_axis',(-1.40488587213121E-32,1.23908819712629E-16,
1.)) ;
#81160 = DIRECTION('ref_axis',(0.,-1.,1.23908819712629E-16)) ;
#81161 = DIRECTION('',(-1.,0.,-1.40488587213121E-32)) ;
#81162 = DIRECTION('',(-1.13380619344889E-16,1.,-1.23908819712629E-16)) ;
#81163 = DIRECTION('center_axis',(1.40488587213121E-32,-1.23908819712629E-16,
-1.)) ;
#81164 = DIRECTION('ref_axis',(-1.74077750246726E-48,-1.,1.23908819712629E-16)) ;
#81165 = DIRECTION('center_axis',(1.40488587213121E-32,-1.23908819712629E-16,
-1.)) ;
#81166 = DIRECTION('ref_axis',(0.,1.,-1.23908819712629E-16)) ;
#81167 = DIRECTION('center_axis',(-1.40488587213121E-32,1.23908819712629E-16,
1.)) ;
#81168 = DIRECTION('ref_axis',(1.74077750246726E-48,1.,-1.23908819712629E-16)) ;
#81169 = DIRECTION('',(1.13380619344889E-16,-1.,1.23908819712629E-16)) ;
#81170 = DIRECTION('',(1.,0.,1.40488587213121E-32)) ;
#81171 = DIRECTION('center_axis',(-1.,-1.23908819712629E-16,-8.95614743483648E-33)) ;
#81172 = DIRECTION('ref_axis',(1.23908819712629E-16,-1.,5.38566640001825E-66)) ;
#81173 = DIRECTION('',(-8.95614743483648E-33,-1.10974565782288E-48,1.)) ;
#81174 = DIRECTION('',(1.23908819712629E-16,-1.,7.2280144832367E-17)) ;
#81175 = DIRECTION('',(-8.95614743483648E-33,0.,1.)) ;
#81176 = DIRECTION('',(-1.23908819712629E-16,1.,-1.23908819712629E-16)) ;
#81177 = DIRECTION('',(8.95614743483648E-33,1.0154535431059E-48,-1.)) ;
#81178 = DIRECTION('',(1.23908819712629E-16,-1.,1.23908819712629E-16)) ;
#81179 = DIRECTION('',(-8.95614743483648E-33,0.,1.)) ;
#81180 = DIRECTION('',(-1.23908819712629E-16,1.,2.4093381610789E-16)) ;
#81181 = DIRECTION('center_axis',(-1.7912294869673E-32,7.2280144832367E-17,
1.)) ;
#81182 = DIRECTION('ref_axis',(0.,-1.,7.2280144832367E-17)) ;
#81183 = DIRECTION('',(-1.23908819712629E-16,1.,-7.2280144832367E-17)) ;
#81184 = DIRECTION('',(1.,1.23908819712629E-16,8.95614743483648E-33)) ;
#81185 = DIRECTION('',(1.44560289664734E-16,-1.,7.2280144832367E-17)) ;
#81186 = DIRECTION('',(-1.,0.,-1.7912294869673E-32)) ;
#81187 = DIRECTION('center_axis',(-2.08976773479518E-32,2.4093381610789E-16,
-1.)) ;
#81188 = DIRECTION('ref_axis',(0.,1.,2.4093381610789E-16)) ;
#81189 = DIRECTION('',(-1.44560289664734E-16,1.,2.4093381610789E-16)) ;
#81190 = DIRECTION('',(-1.,-1.23908819712629E-16,-8.95614743483648E-33)) ;
#81191 = DIRECTION('',(1.23908819712629E-16,-1.,-2.4093381610789E-16)) ;
#81192 = DIRECTION('',(1.,0.,-2.08976773479518E-32)) ;
#81193 = DIRECTION('center_axis',(-1.23908819712629E-16,1.,0.)) ;
#81194 = DIRECTION('ref_axis',(-1.,-1.23908819712629E-16,0.)) ;
#81195 = DIRECTION('',(8.95614743483648E-33,1.10974565782288E-48,-1.)) ;
#81196 = DIRECTION('',(1.,1.23908819712629E-16,8.95614743483648E-33)) ;
#81197 = DIRECTION('',(-2.65552944032596E-32,-3.29043518662928E-48,1.)) ;
#81198 = DIRECTION('',(-1.,-1.23908819712629E-16,-8.95614743483648E-33)) ;
#81199 = DIRECTION('center_axis',(-1.,-1.44560289664734E-16,-2.65552944032596E-32)) ;
#81200 = DIRECTION('ref_axis',(1.44560289664734E-16,-1.,-2.80018320648271E-64)) ;
#81201 = DIRECTION('',(1.44560289664734E-16,-1.,-2.4093381610789E-16)) ;
#81202 = DIRECTION('',(-2.65552944032596E-32,0.,1.)) ;
#81203 = DIRECTION('',(-1.44560289664734E-16,1.,-7.2280144832367E-17)) ;
#81204 = DIRECTION('',(0.,0.,-1.)) ;
#81205 = DIRECTION('center_axis',(0.,1.,0.)) ;
#81206 = DIRECTION('ref_axis',(0.,0.,1.)) ;
#81207 = DIRECTION('',(8.95614743483648E-33,0.,-1.)) ;
#81208 = DIRECTION('',(1.,0.,1.40488587213121E-32)) ;
#81209 = DIRECTION('',(-7.2280144832367E-17,0.,1.)) ;
#81210 = DIRECTION('',(-1.,0.,-1.40488587213121E-32)) ;
#81211 = DIRECTION('',(8.95614743483648E-33,0.,-1.)) ;
#81212 = DIRECTION('',(1.,0.,1.7912294869673E-32)) ;
#81213 = DIRECTION('',(2.65552944032596E-32,0.,-1.)) ;
#81214 = DIRECTION('',(-1.,0.,2.08976773479518E-32)) ;
#81215 = DIRECTION('center_axis',(1.,1.44560289664734E-16,0.)) ;
#81216 = DIRECTION('ref_axis',(-1.44560289664734E-16,1.,0.)) ;
#81217 = DIRECTION('',(1.44560289664734E-16,-1.,0.)) ;
#81218 = DIRECTION('center_axis',(-1.,-1.44560289664734E-16,0.)) ;
#81219 = DIRECTION('ref_axis',(-1.44560289664734E-16,1.,0.)) ;
#81220 = DIRECTION('',(0.,0.,-1.)) ;
#81221 = DIRECTION('center_axis',(-1.,-1.44560289664734E-16,0.)) ;
#81222 = DIRECTION('ref_axis',(-1.44560289664734E-16,1.,0.)) ;
#81223 = DIRECTION('',(1.44560289664734E-16,-1.,0.)) ;
#81224 = DIRECTION('center_axis',(-1.,-1.44560289664734E-16,0.)) ;
#81225 = DIRECTION('ref_axis',(-1.44560289664734E-16,1.,0.)) ;
#81226 = DIRECTION('',(0.,0.,1.)) ;
#81227 = DIRECTION('center_axis',(-1.,-1.44560289664734E-16,0.)) ;
#81228 = DIRECTION('ref_axis',(-1.44560289664734E-16,1.,0.)) ;
#81229 = DIRECTION('center_axis',(1.,-3.46944695195361E-16,0.)) ;
#81230 = DIRECTION('ref_axis',(3.46944695195361E-16,1.,0.)) ;
#81231 = DIRECTION('center_axis',(1.,-3.46944695195361E-16,0.)) ;
#81232 = DIRECTION('ref_axis',(3.46944695195361E-16,1.,0.)) ;
#81233 = DIRECTION('',(0.,0.,-1.)) ;
#81234 = DIRECTION('',(-1.5529910948782E-31,-4.47619207437002E-16,1.)) ;
#81235 = DIRECTION('center_axis',(-1.,3.46944695195361E-16,0.)) ;
#81236 = DIRECTION('ref_axis',(3.46944695195361E-16,1.,1.87537673078574E-15)) ;
#81237 = DIRECTION('',(-3.46944695195361E-16,-1.,-2.45739631480277E-16)) ;
#81238 = DIRECTION('center_axis',(1.,-3.46944695195361E-16,0.)) ;
#81239 = DIRECTION('ref_axis',(3.46944695195361E-16,1.,0.)) ;
#81240 = DIRECTION('center_axis',(3.46944695195361E-16,1.,4.47619207437002E-16)) ;
#81241 = DIRECTION('ref_axis',(-8.18685017503995E-48,-4.47619207437002E-16,
1.)) ;
#81242 = DIRECTION('',(-1.5529910948782E-31,-4.47619207437002E-16,1.)) ;
#81243 = DIRECTION('',(-1.,3.46944695195361E-16,0.)) ;
#81244 = DIRECTION('',(1.5529910948782E-31,4.47619207437002E-16,-1.)) ;
#81245 = DIRECTION('center_axis',(-8.52580615413453E-32,-2.45739631480277E-16,
1.)) ;
#81246 = DIRECTION('ref_axis',(0.,-1.,-2.45739631480277E-16)) ;
#81247 = DIRECTION('',(1.,-3.46944695195361E-16,0.)) ;
#81248 = DIRECTION('',(-3.46944695195361E-16,-1.,-2.45739631480277E-16)) ;
#81249 = DIRECTION('',(3.46944695195361E-16,1.,2.45739631480277E-16)) ;
#81250 = DIRECTION('center_axis',(1.,-3.46944695195361E-16,0.)) ;
#81251 = DIRECTION('ref_axis',(3.46944695195361E-16,1.,0.)) ;
#81252 = DIRECTION('center_axis',(1.,-3.46944695195361E-16,0.)) ;
#81253 = DIRECTION('ref_axis',(3.46944695195361E-16,1.,0.)) ;
#81254 = DIRECTION('',(1.,-3.46944695195361E-16,0.)) ;
#81255 = DIRECTION('center_axis',(-1.,3.46944695195361E-16,0.)) ;
#81256 = DIRECTION('ref_axis',(3.46944695195361E-16,1.,0.)) ;
#81257 = DIRECTION('',(-1.,3.46944695195361E-16,0.)) ;
#81258 = DIRECTION('center_axis',(1.,-3.46944695195361E-16,0.)) ;
#81259 = DIRECTION('ref_axis',(3.46944695195361E-16,1.,0.)) ;
#81260 = DIRECTION('center_axis',(1.,-3.46944695195361E-16,0.)) ;
#81261 = DIRECTION('ref_axis',(-3.46944695195361E-16,-1.,-5.45198806735568E-15)) ;
#81262 = DIRECTION('',(1.,-3.46944695195361E-16,0.)) ;
#81263 = DIRECTION('center_axis',(-1.,3.46944695195361E-16,0.)) ;
#81264 = DIRECTION('ref_axis',(3.46944695195361E-16,1.,-2.47817639425258E-15)) ;
#81265 = DIRECTION('',(-1.,3.46944695195361E-16,0.)) ;
#81266 = DIRECTION('center_axis',(3.69451600012496E-31,1.06487173641454E-15,
-1.)) ;
#81267 = DIRECTION('ref_axis',(0.,1.,1.06487173641454E-15)) ;
#81268 = DIRECTION('',(3.46944695195361E-16,1.,1.06487173641454E-15)) ;
#81269 = DIRECTION('',(-1.,3.46944695195361E-16,0.)) ;
#81270 = DIRECTION('',(-3.46944695195361E-16,-1.,-1.06487173641454E-15)) ;
#81271 = DIRECTION('center_axis',(3.46944695195361E-16,1.,-4.47619207437002E-16)) ;
#81272 = DIRECTION('ref_axis',(8.18685017503995E-48,4.47619207437002E-16,
1.)) ;
#81273 = DIRECTION('',(1.,-3.46944695195361E-16,0.)) ;
#81274 = DIRECTION('',(1.5529910948782E-31,4.47619207437002E-16,1.)) ;
#81275 = DIRECTION('',(-1.5529910948782E-31,-4.47619207437002E-16,-1.)) ;
#81276 = DIRECTION('center_axis',(-1.,3.46944695195361E-16,0.)) ;
#81277 = DIRECTION('ref_axis',(-3.46944695195361E-16,-1.,0.)) ;
#81278 = DIRECTION('center_axis',(-1.,3.46944695195361E-16,0.)) ;
#81279 = DIRECTION('ref_axis',(-3.46944695195361E-16,-1.,0.)) ;
#81280 = DIRECTION('',(1.5529910948782E-31,4.47619207437002E-16,1.)) ;
#81281 = DIRECTION('',(0.,0.,-1.)) ;
#81282 = DIRECTION('center_axis',(1.,-3.46944695195361E-16,0.)) ;
#81283 = DIRECTION('ref_axis',(-3.46944695195361E-16,-1.,2.16840434497101E-15)) ;
#81284 = DIRECTION('center_axis',(1.,-3.46944695195361E-16,0.)) ;
#81285 = DIRECTION('ref_axis',(-3.46944695195361E-16,-1.,-6.28089534405396E-15)) ;
#81286 = DIRECTION('',(3.46944695195361E-16,1.,1.06487173641454E-15)) ;
#81287 = DIRECTION('center_axis',(1.,-3.46944695195361E-16,0.)) ;
#81288 = DIRECTION('ref_axis',(3.46944695195361E-16,1.,0.)) ;
#81289 = DIRECTION('center_axis',(-1.,3.46944695195361E-16,0.)) ;
#81290 = DIRECTION('ref_axis',(3.46944695195361E-16,1.,0.)) ;
#81291 = DIRECTION('',(0.,0.,-1.)) ;
#81292 = DIRECTION('',(0.,0.,1.)) ;
#81293 = DIRECTION('',(-3.46944695195361E-16,-1.,-9.27571383489107E-17)) ;
#81294 = DIRECTION('center_axis',(-3.46944695195361E-16,-1.,0.)) ;
#81295 = DIRECTION('ref_axis',(1.,-3.46944695195361E-16,0.)) ;
#81296 = DIRECTION('',(1.,-3.46944695195361E-16,0.)) ;
#81297 = DIRECTION('',(0.,0.,-1.)) ;
#81298 = DIRECTION('',(0.,0.,1.)) ;
#81299 = DIRECTION('center_axis',(1.,-3.46944695195361E-16,0.)) ;
#81300 = DIRECTION('ref_axis',(3.46944695195361E-16,1.,0.)) ;
#81301 = DIRECTION('center_axis',(1.,-3.46944695195361E-16,0.)) ;
#81302 = DIRECTION('ref_axis',(3.46944695195361E-16,1.,0.)) ;
#81303 = DIRECTION('',(1.,-3.46944695195361E-16,0.)) ;
#81304 = DIRECTION('center_axis',(-1.,3.46944695195361E-16,0.)) ;
#81305 = DIRECTION('ref_axis',(3.46944695195361E-16,1.,0.)) ;
#81306 = DIRECTION('',(-1.,3.46944695195361E-16,0.)) ;
#81307 = DIRECTION('center_axis',(-3.21815970916568E-32,-9.27571383489107E-17,
1.)) ;
#81308 = DIRECTION('ref_axis',(0.,-1.,-9.27571383489107E-17)) ;
#81309 = DIRECTION('',(3.46944695195361E-16,1.,9.27571383489107E-17)) ;
#81310 = DIRECTION('',(1.,0.,3.21815970916568E-32)) ;
#81311 = DIRECTION('',(-3.46944695195361E-16,-1.,-9.27571383489107E-17)) ;
#81312 = DIRECTION('',(-1.,3.46944695195361E-16,0.)) ;
#81313 = DIRECTION('center_axis',(1.,-3.46944695195361E-16,0.)) ;
#81314 = DIRECTION('ref_axis',(3.46944695195361E-16,1.,0.)) ;
#81315 = DIRECTION('center_axis',(1.,-3.46944695195361E-16,0.)) ;
#81316 = DIRECTION('ref_axis',(-3.46944695195361E-16,-1.,-2.47817639425258E-15)) ;
#81317 = DIRECTION('',(1.,-3.46944695195361E-16,0.)) ;
#81318 = DIRECTION('center_axis',(-1.,3.46944695195361E-16,0.)) ;
#81319 = DIRECTION('ref_axis',(3.46944695195361E-16,1.,-3.46944695195361E-15)) ;
#81320 = DIRECTION('',(-1.,3.46944695195361E-16,0.)) ;
#81321 = DIRECTION('center_axis',(-3.46944695195361E-16,-1.,0.)) ;
#81322 = DIRECTION('ref_axis',(1.,-3.46944695195361E-16,0.)) ;
#81323 = DIRECTION('',(0.,0.,-1.)) ;
#81324 = DIRECTION('',(-1.,3.46944695195361E-16,0.)) ;
#81325 = DIRECTION('',(0.,0.,1.)) ;
#81326 = DIRECTION('center_axis',(2.25271179641597E-31,6.49299968442375E-16,
-1.)) ;
#81327 = DIRECTION('ref_axis',(0.,1.,6.49299968442375E-16)) ;
#81328 = DIRECTION('',(3.46944695195361E-16,1.,6.49299968442375E-16)) ;
#81329 = DIRECTION('',(-1.,0.,-2.25271179641597E-31)) ;
#81330 = DIRECTION('',(-3.46944695195361E-16,-1.,-6.49299968442375E-16)) ;
#81331 = DIRECTION('',(1.,-3.46944695195361E-16,0.)) ;
#81332 = DIRECTION('center_axis',(-1.,3.46944695195361E-16,0.)) ;
#81333 = DIRECTION('ref_axis',(-3.46944695195361E-16,-1.,0.)) ;
#81334 = DIRECTION('',(3.46944695195361E-16,1.,6.49299968442375E-16)) ;
#81335 = DIRECTION('',(0.,0.,1.)) ;
#81336 = DIRECTION('',(0.,0.,-1.)) ;
#81337 = DIRECTION('center_axis',(-1.,3.46944695195361E-16,0.)) ;
#81338 = DIRECTION('ref_axis',(-3.46944695195361E-16,-1.,0.)) ;
#81339 = DIRECTION('center_axis',(-0.164398987305357,0.,-0.986393923832144)) ;
#81340 = DIRECTION('ref_axis',(-0.986393923832144,0.,0.164398987305357)) ;
#81341 = DIRECTION('',(-0.937042571331636,0.312347523777212,0.156173761888606)) ;
#81342 = DIRECTION('',(0.,-1.,0.)) ;
#81343 = DIRECTION('',(0.973328526784575,0.162221421130762,-0.162221421130763)) ;
#81344 = DIRECTION('',(-1.73472347597681E-15,1.,2.89120579329468E-16)) ;
#81345 = DIRECTION('center_axis',(-1.,0.,0.)) ;
#81346 = DIRECTION('ref_axis',(0.,0.,1.)) ;
#81347 = DIRECTION('center_axis',(-1.,0.,0.)) ;
#81348 = DIRECTION('ref_axis',(0.,0.958782004879663,-0.284142687956128)) ;
#81349 = DIRECTION('',(0.,0.,1.)) ;
#81350 = DIRECTION('',(0.,-1.,0.)) ;
#81351 = DIRECTION('center_axis',(-1.,0.,0.)) ;
#81352 = DIRECTION('ref_axis',(0.,0.758705346999943,-0.651433954007385)) ;
#81353 = DIRECTION('',(0.,0.,-1.)) ;
#81354 = DIRECTION('center_axis',(-1.,0.,0.)) ;
#81355 = DIRECTION('ref_axis',(0.,-0.654778494946305,-0.75582082701911)) ;
#81356 = DIRECTION('',(0.,1.,0.)) ;
#81357 = DIRECTION('center_axis',(-0.164398987305357,0.,0.986393923832144)) ;
#81358 = DIRECTION('ref_axis',(0.986393923832144,0.,0.164398987305357)) ;
#81359 = DIRECTION('',(-0.973328526784575,-0.162221421130762,-0.162221421130763)) ;
#81360 = DIRECTION('',(0.,1.,0.)) ;
#81361 = DIRECTION('',(0.937042571331636,-0.312347523777212,0.156173761888606)) ;
#81362 = DIRECTION('',(1.73472347597681E-15,-1.,2.89120579329468E-16)) ;
#81363 = DIRECTION('center_axis',(-0.573462344363329,0.81923192051904,0.)) ;
#81364 = DIRECTION('ref_axis',(-0.81923192051904,-0.573462344363329,0.)) ;
#81365 = DIRECTION('',(-0.710669054518702,-0.497468338163091,0.49746833816309)) ;
#81366 = DIRECTION('',(0.,0.,-1.)) ;
#81367 = DIRECTION('',(0.710669054518702,0.497468338163091,0.49746833816309)) ;
#81368 = DIRECTION('',(0.,0.,1.)) ;
#81369 = DIRECTION('center_axis',(-1.,0.,0.)) ;
#81370 = DIRECTION('ref_axis',(0.,0.,1.)) ;
#81371 = DIRECTION('',(0.,0.,1.)) ;
#81372 = DIRECTION('',(0.,-1.,-9.34081871679819E-17)) ;
#81373 = DIRECTION('',(0.,0.,-1.)) ;
#81374 = DIRECTION('',(0.,1.,-9.34081871679819E-17)) ;
#81375 = DIRECTION('center_axis',(-0.573462344363329,-0.81923192051904,0.)) ;
#81376 = DIRECTION('ref_axis',(0.81923192051904,-0.573462344363329,0.)) ;
#81377 = DIRECTION('',(-0.710669054518701,0.497468338163091,-0.497468338163091)) ;
#81378 = DIRECTION('',(0.,0.,1.)) ;
#81379 = DIRECTION('',(0.710669054518701,-0.497468338163091,-0.497468338163091)) ;
#81380 = DIRECTION('',(0.,0.,-1.)) ;
#81381 = DIRECTION('center_axis',(0.,0.,1.)) ;
#81382 = DIRECTION('ref_axis',(1.,0.,0.)) ;
#81383 = DIRECTION('',(1.,6.67201336914158E-17,0.)) ;
#81384 = DIRECTION('',(1.33440267382831E-16,1.,0.)) ;
#81385 = DIRECTION('',(-1.,1.33440267382831E-16,0.)) ;
#81386 = DIRECTION('center_axis',(0.,0.,1.)) ;
#81387 = DIRECTION('ref_axis',(1.,0.,0.)) ;
#81388 = DIRECTION('',(1.,-1.33440267382831E-16,0.)) ;
#81389 = DIRECTION('',(-1.33440267382831E-16,-1.,0.)) ;
#81390 = DIRECTION('',(-1.,-6.67201336914158E-17,0.)) ;
#81391 = DIRECTION('center_axis',(-6.67201336914158E-17,1.,0.)) ;
#81392 = DIRECTION('ref_axis',(-1.,-6.67201336914158E-17,0.)) ;
#81393 = DIRECTION('',(1.,6.67201336914158E-17,0.)) ;
#81394 = DIRECTION('',(0.,0.,1.)) ;
#81395 = DIRECTION('',(-1.,-6.67201336914158E-17,0.)) ;
#81396 = DIRECTION('center_axis',(-1.33440267382831E-16,-1.,0.)) ;
#81397 = DIRECTION('ref_axis',(1.,-1.33440267382831E-16,0.)) ;
#81398 = DIRECTION('',(1.,-1.33440267382831E-16,0.)) ;
#81399 = DIRECTION('',(0.,0.,-1.)) ;
#81400 = DIRECTION('',(-1.,1.33440267382831E-16,0.)) ;
#81401 = DIRECTION('center_axis',(0.,0.,1.)) ;
#81402 = DIRECTION('ref_axis',(1.,0.,0.)) ;
#81403 = DIRECTION('',(0.,-1.,0.)) ;
#81404 = DIRECTION('',(1.,0.,0.)) ;
#81405 = DIRECTION('',(0.,1.,0.)) ;
#81406 = DIRECTION('center_axis',(0.,0.,-1.)) ;
#81407 = DIRECTION('ref_axis',(1.,0.,0.)) ;
#81408 = DIRECTION('',(-1.44560289664734E-16,1.,-7.2280144832367E-17)) ;
#81409 = DIRECTION('center_axis',(0.,0.,1.)) ;
#81410 = DIRECTION('ref_axis',(1.,0.,0.)) ;
#81411 = DIRECTION('center_axis',(0.,0.,1.)) ;
#81412 = DIRECTION('ref_axis',(1.,0.,0.)) ;
#81413 = DIRECTION('',(0.,-1.,0.)) ;
#81414 = DIRECTION('',(-1.,0.,0.)) ;
#81415 = DIRECTION('',(0.,1.,0.)) ;
#81416 = DIRECTION('center_axis',(0.,0.,-1.)) ;
#81417 = DIRECTION('ref_axis',(1.,-1.82602471155453E-15,0.)) ;
#81418 = DIRECTION('',(1.44560289664734E-16,-1.,-2.4093381610789E-16)) ;
#81419 = DIRECTION('center_axis',(0.,0.,1.)) ;
#81420 = DIRECTION('ref_axis',(1.,0.,0.)) ;
#81421 = DIRECTION('center_axis',(0.,0.,-1.)) ;
#81422 = DIRECTION('ref_axis',(-1.,0.,0.)) ;
#81423 = DIRECTION('',(0.,0.,-1.)) ;
#81424 = DIRECTION('center_axis',(0.,0.,-1.)) ;
#81425 = DIRECTION('ref_axis',(1.,0.,0.)) ;
#81426 = DIRECTION('center_axis',(0.,0.,1.)) ;
#81427 = DIRECTION('ref_axis',(1.,0.,0.)) ;
#81428 = DIRECTION('center_axis',(1.,0.,0.)) ;
#81429 = DIRECTION('ref_axis',(0.,0.,-1.)) ;
#81430 = DIRECTION('',(0.,-1.,0.)) ;
#81431 = DIRECTION('',(0.,0.,1.)) ;
#81432 = DIRECTION('',(0.,1.,0.)) ;
#81433 = DIRECTION('center_axis',(0.81923192051904,0.573462344363329,0.)) ;
#81434 = DIRECTION('ref_axis',(-0.573462344363329,0.81923192051904,0.)) ;
#81435 = DIRECTION('',(-0.497468338163091,0.710669054518701,0.497468338163091)) ;
#81436 = DIRECTION('',(0.,0.,-1.)) ;
#81437 = DIRECTION('',(0.497468338163091,-0.710669054518701,0.497468338163091)) ;
#81438 = DIRECTION('',(0.,0.,1.)) ;
#81439 = DIRECTION('center_axis',(0.,1.,0.)) ;
#81440 = DIRECTION('ref_axis',(0.,0.,1.)) ;
#81441 = DIRECTION('',(0.,0.,1.)) ;
#81442 = DIRECTION('',(-1.,0.,0.)) ;
#81443 = DIRECTION('',(0.,0.,-1.)) ;
#81444 = DIRECTION('',(1.,0.,0.)) ;
#81445 = DIRECTION('center_axis',(-0.81923192051904,0.573462344363329,0.)) ;
#81446 = DIRECTION('ref_axis',(-0.573462344363329,-0.81923192051904,0.)) ;
#81447 = DIRECTION('',(0.497468338163091,0.710669054518701,-0.497468338163091)) ;
#81448 = DIRECTION('',(0.,0.,1.)) ;
#81449 = DIRECTION('',(-0.497468338163091,-0.710669054518701,-0.497468338163091)) ;
#81450 = DIRECTION('',(0.,0.,-1.)) ;
#81451 = DIRECTION('center_axis',(-1.,0.,0.)) ;
#81452 = DIRECTION('ref_axis',(0.,0.,1.)) ;
#81453 = DIRECTION('',(0.,-1.,0.)) ;
#81454 = DIRECTION('',(0.,0.,-1.)) ;
#81455 = DIRECTION('',(0.,1.,0.)) ;
#81456 = DIRECTION('',(0.,0.,-1.)) ;
#81457 = DIRECTION('center_axis',(0.,0.,-1.)) ;
#81458 = DIRECTION('ref_axis',(-1.,0.,0.)) ;
#81459 = DIRECTION('center_axis',(0.,0.,1.)) ;
#81460 = DIRECTION('ref_axis',(1.,0.,0.)) ;
#81461 = DIRECTION('center_axis',(0.,0.,-1.)) ;
#81462 = DIRECTION('ref_axis',(1.,5.20417042793042E-15,0.)) ;
#81463 = DIRECTION('center_axis',(-0.573462344363328,7.65229685658278E-17,
0.819231920519041)) ;
#81464 = DIRECTION('ref_axis',(0.819231920519041,1.22423955297878E-32,0.573462344363328)) ;
#81465 = DIRECTION('',(-0.710669054518702,-0.497468338163091,-0.497468338163091)) ;
#81466 = DIRECTION('',(1.33440267382831E-16,1.,-2.91413396387194E-34)) ;
#81467 = DIRECTION('',(0.710669054518701,-0.497468338163091,0.497468338163091)) ;
#81468 = DIRECTION('',(5.04890651880155E-33,-1.,9.34081871679819E-17)) ;
#81469 = DIRECTION('center_axis',(-0.573462344363328,7.65229685658278E-17,
-0.819231920519041)) ;
#81470 = DIRECTION('ref_axis',(-0.819231920519041,-1.22423955297878E-32,0.573462344363328)) ;
#81471 = DIRECTION('',(-0.710669054518701,0.497468338163091,0.497468338163091)) ;
#81472 = DIRECTION('',(-1.33440267382831E-16,-1.,7.77328292223541E-33)) ;
#81473 = DIRECTION('',(0.710669054518702,0.497468338163091,-0.497468338163091)) ;
#81474 = DIRECTION('',(-5.04890651880155E-33,1.,9.34081871679819E-17)) ;
#81475 = DIRECTION('center_axis',(0.,0.573462344363328,-0.819231920519041)) ;
#81476 = DIRECTION('ref_axis',(0.,0.819231920519041,0.573462344363328)) ;
#81477 = DIRECTION('',(0.497468338163091,0.710669054518701,0.497468338163091)) ;
#81478 = DIRECTION('',(-1.,0.,0.)) ;
#81479 = DIRECTION('',(0.497468338163091,-0.710669054518701,-0.497468338163091)) ;
#81480 = DIRECTION('',(1.,0.,0.)) ;
#81481 = DIRECTION('center_axis',(0.,0.573462344363328,0.819231920519041)) ;
#81482 = DIRECTION('ref_axis',(0.,-0.819231920519041,0.573462344363328)) ;
#81483 = DIRECTION('',(-0.497468338163091,0.710669054518701,-0.497468338163091)) ;
#81484 = DIRECTION('',(1.,0.,0.)) ;
#81485 = DIRECTION('',(-0.497468338163091,-0.710669054518701,0.497468338163091)) ;
#81486 = DIRECTION('',(-1.,0.,0.)) ;
#81487 = DIRECTION('center_axis',(-0.164398987305354,-0.986393923832144,0.)) ;
#81488 = DIRECTION('ref_axis',(0.,0.,1.)) ;
#81489 = DIRECTION('',(0.,0.,-1.)) ;
#81490 = DIRECTION('center_axis',(-0.164398987305441,-0.98639392383213,1.51891488936633E-12)) ;
#81491 = DIRECTION('ref_axis',(-0.0577290357396497,0.00962150595815054,0.998285923498708)) ;
#81492 = DIRECTION('',(0.,0.,1.)) ;
#81493 = DIRECTION('center_axis',(1.,-2.89120579329441E-16,0.)) ;
#81494 = DIRECTION('ref_axis',(-2.89120579329441E-16,-1.,4.23109396156707E-14)) ;
#81495 = DIRECTION('center_axis',(1.,1.15648231731787E-15,0.)) ;
#81496 = DIRECTION('ref_axis',(1.15648231731787E-15,-1.,0.)) ;
#81497 = DIRECTION('center_axis',(0.166689823568342,0.983956802834268,0.0635886222127804)) ;
#81498 = DIRECTION('ref_axis',(-0.0486480010311504,0.0726194156279799,-0.996172571630801)) ;
#81499 = DIRECTION('center_axis',(0.166689823568934,0.983956802833365,-0.0635886222252155)) ;
#81500 = DIRECTION('ref_axis',(-0.0462047034218524,0.0722149192754741,0.996318287905896)) ;
#81501 = DIRECTION('center_axis',(-0.164398987305354,-0.986393923832144,0.)) ;
#81502 = DIRECTION('ref_axis',(0.,0.,1.)) ;
#81503 = DIRECTION('',(0.,0.,1.)) ;
#81504 = DIRECTION('center_axis',(-0.164398987305435,-0.986393923832131,-1.41042096917786E-12)) ;
#81505 = DIRECTION('ref_axis',(-0.055419232787587,0.00923653879936327,-0.998420450005028)) ;
#81506 = DIRECTION('',(0.,0.,-1.)) ;
#81507 = DIRECTION('center_axis',(0.,0.,1.)) ;
#81508 = DIRECTION('ref_axis',(1.,0.,0.)) ;
#81509 = DIRECTION('center_axis',(0.,0.,1.)) ;
#81510 = DIRECTION('ref_axis',(1.,0.,0.)) ;
#81511 = DIRECTION('center_axis',(0.,1.,0.)) ;
#81512 = DIRECTION('ref_axis',(1.,0.,0.)) ;
#81513 = DIRECTION('center_axis',(0.,-0.888198741900269,0.45945945945946)) ;
#81514 = DIRECTION('ref_axis',(0.,0.45945945945946,0.888198741900269)) ;
#81515 = DIRECTION('center_axis',(-1.,0.,1.22067519501986E-15)) ;
#81516 = DIRECTION('ref_axis',(-1.22067519501986E-15,0.,-1.)) ;
#81517 = DIRECTION('center_axis',(0.,0.,1.)) ;
#81518 = DIRECTION('ref_axis',(1.,0.,0.)) ;
#81519 = DIRECTION('center_axis',(0.,0.,-1.)) ;
#81520 = DIRECTION('ref_axis',(-1.,0.,0.)) ;
#81521 = DIRECTION('center_axis',(1.,-3.46944695195361E-16,0.)) ;
#81522 = DIRECTION('ref_axis',(3.46944695195361E-16,1.,0.)) ;
#81523 = DIRECTION('center_axis',(-1.,3.46944695195361E-16,0.)) ;
#81524 = DIRECTION('ref_axis',(3.46944695195361E-16,1.,4.33680868994201E-15)) ;
#81525 = DIRECTION('center_axis',(-1.,3.46944695195361E-16,0.)) ;
#81526 = DIRECTION('ref_axis',(-3.41607084500048E-16,-1.,0.)) ;
#81527 = DIRECTION('center_axis',(0.,-0.459459459459457,0.888198741900271)) ;
#81528 = DIRECTION('ref_axis',(0.,-0.888198741900271,-0.459459459459457)) ;
#81529 = DIRECTION('center_axis',(1.,-3.46944695195361E-16,0.)) ;
#81530 = DIRECTION('ref_axis',(0.,1.,0.)) ;
#81531 = DIRECTION('center_axis',(0.,0.888198741900269,-0.45945945945946)) ;
#81532 = DIRECTION('ref_axis',(0.,-0.45945945945946,-0.888198741900269)) ;
#81533 = DIRECTION('center_axis',(0.,1.,0.)) ;
#81534 = DIRECTION('ref_axis',(1.,0.,0.)) ;
#81535 = DIRECTION('center_axis',(0.,-1.,0.)) ;
#81536 = DIRECTION('ref_axis',(0.,0.,1.)) ;
#81537 = DIRECTION('center_axis',(-1.,0.,0.)) ;
#81538 = DIRECTION('ref_axis',(0.,0.,-1.)) ;
#81539 = DIRECTION('center_axis',(0.,0.,-1.)) ;
#81540 = DIRECTION('ref_axis',(-1.,0.,0.)) ;
#81541 = DIRECTION('center_axis',(0.,0.,-1.)) ;
#81542 = DIRECTION('ref_axis',(-1.,0.,0.)) ;
#81543 = DIRECTION('center_axis',(1.,-3.46944695195361E-16,0.)) ;
#81544 = DIRECTION('ref_axis',(3.46944695195361E-16,1.,0.)) ;
#81545 = DIRECTION('center_axis',(-1.,3.46944695195361E-16,0.)) ;
#81546 = DIRECTION('ref_axis',(3.46944695195361E-16,1.,0.)) ;
#81547 = DIRECTION('center_axis',(1.,0.,0.)) ;
#81548 = DIRECTION('ref_axis',(0.,0.,-1.)) ;
#81549 = DIRECTION('center_axis',(0.,0.,1.)) ;
#81550 = DIRECTION('ref_axis',(1.,0.,0.)) ;
#81551 = DIRECTION('center_axis',(0.,0.,1.)) ;
#81552 = DIRECTION('ref_axis',(1.,0.,0.)) ;
#81553 = DIRECTION('center_axis',(1.,-3.46944695195361E-16,0.)) ;
#81554 = DIRECTION('ref_axis',(3.80647894157197E-16,1.,0.)) ;
#81555 = DIRECTION('center_axis',(0.,0.459459459459459,-0.888198741900269)) ;
#81556 = DIRECTION('ref_axis',(0.,0.88819874190027,0.459459459459459)) ;
#81557 = DIRECTION('center_axis',(1.,-3.46944695195361E-16,0.)) ;
#81558 = DIRECTION('ref_axis',(3.46944695195361E-16,1.,0.)) ;
#81559 = DIRECTION('center_axis',(-1.,3.46944695195361E-16,0.)) ;
#81560 = DIRECTION('ref_axis',(3.46944695195361E-16,1.,0.)) ;
#81561 = DIRECTION('center_axis',(-3.46944695195361E-16,-1.,-6.49299968442375E-16)) ;
#81562 = DIRECTION('ref_axis',(2.25271179641597E-31,6.49299968442375E-16,
-1.)) ;
#81563 = DIRECTION('center_axis',(0.,-1.,0.)) ;
#81564 = DIRECTION('ref_axis',(0.,0.,-1.)) ;
#81565 = DIRECTION('center_axis',(0.,0.,1.)) ;
#81566 = DIRECTION('ref_axis',(1.,0.,0.)) ;
#81567 = DIRECTION('center_axis',(-3.25260651745651E-15,0.,1.)) ;
#81568 = DIRECTION('ref_axis',(1.,0.,3.25260651745651E-15)) ;
#81569 = DIRECTION('center_axis',(0.,1.,0.)) ;
#81570 = DIRECTION('ref_axis',(1.,0.,0.)) ;
#81571 = DIRECTION('center_axis',(0.,-0.888198741900269,-0.45945945945946)) ;
#81572 = DIRECTION('ref_axis',(0.,-0.45945945945946,0.888198741900269)) ;
#81573 = DIRECTION('center_axis',(1.,-3.46944695195361E-16,0.)) ;
#81574 = DIRECTION('ref_axis',(0.,1.,0.)) ;
#81575 = DIRECTION('center_axis',(0.,0.888198741900269,0.45945945945946)) ;
#81576 = DIRECTION('ref_axis',(0.,0.45945945945946,-0.888198741900269)) ;
#81577 = DIRECTION('center_axis',(1.,-3.46944695195361E-16,0.)) ;
#81578 = DIRECTION('ref_axis',(0.,1.,0.)) ;
#81579 = DIRECTION('center_axis',(0.,1.,0.)) ;
#81580 = DIRECTION('ref_axis',(0.,0.,-1.)) ;
#81581 = DIRECTION('center_axis',(0.,1.,0.)) ;
#81582 = DIRECTION('ref_axis',(1.,0.,0.)) ;
#81583 = DIRECTION('center_axis',(-1.,0.,0.)) ;
#81584 = DIRECTION('ref_axis',(0.,0.,-1.)) ;
#81585 = DIRECTION('center_axis',(1.,-3.46944695195361E-16,0.)) ;
#81586 = DIRECTION('ref_axis',(3.41607084500048E-16,1.,0.)) ;
#81587 = DIRECTION('center_axis',(-9.62987005567165E-16,-0.459459459459459,
-0.88819874190027)) ;
#81588 = DIRECTION('ref_axis',(1.2595106985394E-31,0.88819874190027,-0.459459459459459)) ;
#81589 = DIRECTION('center_axis',(1.,-3.46944695195361E-16,0.)) ;
#81590 = DIRECTION('ref_axis',(3.46944695195361E-16,1.,0.)) ;
#81591 = DIRECTION('center_axis',(-1.,3.46944695195361E-16,0.)) ;
#81592 = DIRECTION('ref_axis',(3.46944695195361E-16,1.,0.)) ;
#81593 = DIRECTION('center_axis',(1.,0.,0.)) ;
#81594 = DIRECTION('ref_axis',(0.,0.,-1.)) ;
#81595 = DIRECTION('center_axis',(1.,-3.46944695195361E-16,0.)) ;
#81596 = DIRECTION('ref_axis',(3.80647894157197E-16,1.,0.)) ;
#81597 = DIRECTION('center_axis',(0.,0.459459459459459,0.888198741900269)) ;
#81598 = DIRECTION('ref_axis',(0.,-0.88819874190027,0.459459459459459)) ;
#81599 = DIRECTION('center_axis',(-3.46944695195361E-16,-1.,-6.49299968442375E-16)) ;
#81600 = DIRECTION('ref_axis',(2.25271179641597E-31,6.49299968442375E-16,
-1.)) ;
#81601 = DIRECTION('center_axis',(0.,1.,0.)) ;
#81602 = DIRECTION('ref_axis',(0.,0.,-1.)) ;
#81603 = DIRECTION('center_axis',(1.,0.,2.25271179641597E-31)) ;
#81604 = DIRECTION('ref_axis',(2.25271179641597E-31,0.,-1.)) ;
#81605 = DIRECTION('center_axis',(-1.,0.,0.)) ;
#81606 = DIRECTION('ref_axis',(0.,0.,1.)) ;
#81607 = DIRECTION('center_axis',(0.,1.,0.)) ;
#81608 = DIRECTION('ref_axis',(1.,0.,0.)) ;
#81609 = DIRECTION('center_axis',(0.,-1.,0.)) ;
#81610 = DIRECTION('ref_axis',(-1.0842021724855E-15,0.,1.)) ;
#81611 = DIRECTION('center_axis',(1.,-3.46944695195361E-16,0.)) ;
#81612 = DIRECTION('ref_axis',(0.,1.,0.)) ;
#81613 = DIRECTION('center_axis',(0.,1.,0.)) ;
#81614 = DIRECTION('ref_axis',(0.,0.,-1.)) ;
#81615 = DIRECTION('center_axis',(0.,-1.,0.)) ;
#81616 = DIRECTION('ref_axis',(0.,0.,-1.)) ;
#81617 = DIRECTION('center_axis',(0.,0.,1.)) ;
#81618 = DIRECTION('ref_axis',(-1.,0.,0.)) ;
#81619 = DIRECTION('center_axis',(0.,0.,-1.)) ;
#81620 = DIRECTION('ref_axis',(-1.,0.,0.)) ;
#81621 = DIRECTION('center_axis',(0.,0.,-1.)) ;
#81622 = DIRECTION('ref_axis',(-1.,0.,0.)) ;
#81623 = DIRECTION('center_axis',(-3.46944695195361E-16,-1.,-9.27571383489107E-17)) ;
#81624 = DIRECTION('ref_axis',(1.,-3.46944695195361E-16,-3.21815970916568E-32)) ;
#81625 = DIRECTION('center_axis',(0.,-1.,0.)) ;
#81626 = DIRECTION('ref_axis',(0.,0.,-1.)) ;
#81627 = DIRECTION('center_axis',(3.46944695195361E-16,1.,9.27571383489107E-17)) ;
#81628 = DIRECTION('ref_axis',(-1.,3.46944695195361E-16,3.21815970916568E-32)) ;
#81629 = DIRECTION('center_axis',(0.,1.,0.)) ;
#81630 = DIRECTION('ref_axis',(0.,0.,-1.)) ;
#81631 = DIRECTION('center_axis',(0.,0.,-1.)) ;
#81632 = DIRECTION('ref_axis',(-1.,0.,0.)) ;
#81633 = DIRECTION('center_axis',(0.,0.,1.)) ;
#81634 = DIRECTION('ref_axis',(1.,0.,0.)) ;
#81635 = DIRECTION('center_axis',(0.,1.,0.)) ;
#81636 = DIRECTION('ref_axis',(1.,0.,0.)) ;
#81637 = DIRECTION('center_axis',(-1.,0.,1.0842021724855E-15)) ;
#81638 = DIRECTION('ref_axis',(-1.0842021724855E-15,0.,-1.)) ;
#81639 = DIRECTION('center_axis',(0.,-1.,0.)) ;
#81640 = DIRECTION('ref_axis',(0.,0.,-1.)) ;
#81641 = DIRECTION('center_axis',(1.,0.,0.)) ;
#81642 = DIRECTION('ref_axis',(0.,0.,1.)) ;
#81643 = DIRECTION('center_axis',(1.,0.,3.21815970916568E-32)) ;
#81644 = DIRECTION('ref_axis',(3.21815970916568E-32,0.,-1.)) ;
#81645 = DIRECTION('center_axis',(0.,1.,0.)) ;
#81646 = DIRECTION('ref_axis',(1.,0.,0.)) ;
#81647 = DIRECTION('center_axis',(0.,0.,-1.)) ;
#81648 = DIRECTION('ref_axis',(1.,0.,0.)) ;
#81649 = DIRECTION('center_axis',(1.,0.,0.)) ;
#81650 = DIRECTION('ref_axis',(0.,-1.0842021724855E-15,1.)) ;
#81651 = DIRECTION('center_axis',(1.0842021724855E-15,1.,0.)) ;
#81652 = DIRECTION('ref_axis',(1.,-1.0842021724855E-15,0.)) ;
#81653 = DIRECTION('center_axis',(1.,0.,-2.08976773479518E-32)) ;
#81654 = DIRECTION('ref_axis',(-2.08976773479518E-32,0.,-1.)) ;
#81655 = DIRECTION('center_axis',(-0.447220452189904,-7.10036017517955E-6,
-0.894423762593907)) ;
#81656 = DIRECTION('ref_axis',(0.894325663269773,0.0148067719364733,-0.447171519130972)) ;
#81657 = DIRECTION('center_axis',(-1.23908819712629E-16,1.,2.4093381610789E-16)) ;
#81658 = DIRECTION('ref_axis',(2.98538247827883E-32,-2.4093381610789E-16,
1.)) ;
#81659 = DIRECTION('center_axis',(-5.60223420161783E-6,-0.447219005480058,
-0.89442448597187)) ;
#81660 = DIRECTION('ref_axis',(0.0146917039338177,0.894327914920155,-0.447170811245647)) ;
#81661 = DIRECTION('center_axis',(-8.95614743483648E-33,0.,1.)) ;
#81662 = DIRECTION('ref_axis',(1.,0.,8.95614743483648E-33)) ;
#81663 = DIRECTION('center_axis',(1.40488587213121E-32,-1.23908819712629E-16,
-1.)) ;
#81664 = DIRECTION('ref_axis',(1.74077750246726E-48,1.,-1.23908819712629E-16)) ;
#81665 = DIRECTION('center_axis',(-2.65552944032596E-32,0.,1.)) ;
#81666 = DIRECTION('ref_axis',(1.,0.,2.65552944032596E-32)) ;
#81667 = DIRECTION('center_axis',(0.894424485971804,-5.60223417044988E-6,
0.44721900548019)) ;
#81668 = DIRECTION('ref_axis',(0.447170811245807,0.0146917039294042,-0.894327914920147)) ;
#81669 = DIRECTION('center_axis',(0.894423762594036,-7.10036034885401E-6,
-0.447220452189647)) ;
#81670 = DIRECTION('ref_axis',(0.447171519130767,0.0148067719290092,0.89432566327)) ;
#81671 = DIRECTION('center_axis',(-8.95614743483648E-33,-1.10974565782288E-48,
1.)) ;
#81672 = DIRECTION('ref_axis',(1.,-9.9390457266313E-81,8.95614743483648E-33)) ;
#81673 = DIRECTION('center_axis',(-7.10036015927338E-6,0.894423762593895,
0.447220452189929)) ;
#81674 = DIRECTION('ref_axis',(-0.014806771929487,-0.447171519131043,0.894325663269853)) ;
#81675 = DIRECTION('center_axis',(-5.60223394757394E-6,0.89442448597165,-0.447219005480498)) ;
#81676 = DIRECTION('ref_axis',(0.0146917039348304,0.447170811246077,0.894327914919923)) ;
#81677 = DIRECTION('center_axis',(1.40488587213121E-32,-1.23908819712629E-16,
-1.)) ;
#81678 = DIRECTION('ref_axis',(0.,1.,0.)) ;
#81679 = DIRECTION('center_axis',(-1.,0.,0.)) ;
#81680 = DIRECTION('ref_axis',(0.,0.,-1.)) ;
#81681 = DIRECTION('center_axis',(0.,-1.,0.)) ;
#81682 = DIRECTION('ref_axis',(0.,0.,1.)) ;
#81683 = DIRECTION('center_axis',(-1.,0.,-1.40488587213121E-32)) ;
#81684 = DIRECTION('ref_axis',(-1.40488587213121E-32,0.,1.)) ;
#81685 = DIRECTION('',(-1.,0.,-1.40488587213121E-32)) ;
#81686 = DIRECTION('center_axis',(-1.,0.,0.)) ;
#81687 = DIRECTION('ref_axis',(0.,0.,1.)) ;
#81688 = DIRECTION('center_axis',(0.,1.,0.)) ;
#81689 = DIRECTION('ref_axis',(1.,0.,0.)) ;
#81690 = DIRECTION('center_axis',(0.,1.,0.)) ;
#81691 = DIRECTION('ref_axis',(0.,0.,-1.)) ;
#81692 = DIRECTION('center_axis',(0.,0.,-1.)) ;
#81693 = DIRECTION('ref_axis',(1.,0.,0.)) ;
#81694 = DIRECTION('center_axis',(-1.,0.,-1.7912294869673E-32)) ;
#81695 = DIRECTION('ref_axis',(-1.7912294869673E-32,0.,1.)) ;
#81696 = DIRECTION('center_axis',(-0.447219005480384,-5.6022339276529E-6,
0.894424485971707)) ;
#81697 = DIRECTION('ref_axis',(0.8943279149199,0.014691703940891,0.447170811245923)) ;
#81698 = DIRECTION('center_axis',(-1.,0.,0.)) ;
#81699 = DIRECTION('ref_axis',(0.,0.,1.)) ;
#81700 = DIRECTION('center_axis',(1.23908819712629E-16,-1.,7.2280144832367E-17)) ;
#81701 = DIRECTION('ref_axis',(1.,1.23908819712629E-16,-8.95614743483648E-33)) ;
#81702 = DIRECTION('center_axis',(-7.10036038195002E-6,-0.447220452189466,
0.894423762594126)) ;
#81703 = DIRECTION('ref_axis',(-0.0148067719344191,-0.894325663270018,-0.447171519130551)) ;
#81704 = DIRECTION('center_axis',(0.,-1.,1.0842021724855E-15)) ;
#81705 = DIRECTION('ref_axis',(0.,-1.0842021724855E-15,-1.)) ;
#81706 = DIRECTION('center_axis',(1.23908819712629E-16,-1.,1.23908819712629E-16)) ;
#81707 = DIRECTION('ref_axis',(3.32059923884369E-47,-1.23908819712629E-16,
-1.)) ;
#81708 = DIRECTION('center_axis',(0.,-1.,0.)) ;
#81709 = DIRECTION('ref_axis',(0.,0.,-1.)) ;
#81710 = DIRECTION('',(-1.23908819712629E-16,1.,-1.23908819712629E-16)) ;
#81711 = DIRECTION('center_axis',(1.,0.,1.40488587213121E-32)) ;
#81712 = DIRECTION('ref_axis',(1.40488587213121E-32,0.,-1.)) ;
#81713 = DIRECTION('center_axis',(-0.707106781186547,0.707106781186548,-7.05268145719399E-16)) ;
#81714 = DIRECTION('ref_axis',(0.707106781186548,0.707106781186547,-6.41252558311899E-13)) ;
#81715 = DIRECTION('center_axis',(1.,0.,0.)) ;
#81716 = DIRECTION('ref_axis',(0.,0.,-1.)) ;
#81717 = DIRECTION('center_axis',(0.,-1.,0.)) ;
#81718 = DIRECTION('ref_axis',(0.,0.,-1.)) ;
#81719 = DIRECTION('center_axis',(0.,0.,1.)) ;
#81720 = DIRECTION('ref_axis',(-1.,0.,0.)) ;
#81721 = DIRECTION('center_axis',(7.2280144832367E-17,0.,-1.)) ;
#81722 = DIRECTION('ref_axis',(-1.,0.,-7.2280144832367E-17)) ;
#81723 = DIRECTION('',(7.2280144832367E-17,0.,-1.)) ;
#81724 = DIRECTION('center_axis',(0.,0.,-1.)) ;
#81725 = DIRECTION('ref_axis',(-1.,0.,0.)) ;
#81726 = DIRECTION('center_axis',(0.,1.,0.)) ;
#81727 = DIRECTION('ref_axis',(1.,0.,0.)) ;
#81728 = DIRECTION('center_axis',(0.,0.,1.)) ;
#81729 = DIRECTION('ref_axis',(-1.,0.,0.)) ;
#81730 = DIRECTION('center_axis',(0.,1.,0.)) ;
#81731 = DIRECTION('ref_axis',(1.,0.,0.)) ;
#81732 = DIRECTION('center_axis',(1.,0.,0.)) ;
#81733 = DIRECTION('ref_axis',(0.,0.,1.)) ;
#81734 = DIRECTION('center_axis',(0.,0.,-1.)) ;
#81735 = DIRECTION('ref_axis',(1.,0.,0.)) ;
#81736 = DIRECTION('center_axis',(-1.13380619344889E-16,1.,-1.23908819712629E-16)) ;
#81737 = DIRECTION('ref_axis',(-1.40488587213121E-32,1.23908819712629E-16,
1.)) ;
#81738 = DIRECTION('center_axis',(0.,1.,0.)) ;
#81739 = DIRECTION('ref_axis',(0.,0.,1.)) ;
#81740 = DIRECTION('center_axis',(7.2280144832367E-17,0.,-1.)) ;
#81741 = DIRECTION('ref_axis',(-1.,0.,-7.2280144832367E-17)) ;
#81742 = DIRECTION('center_axis',(0.,0.,1.)) ;
#81743 = DIRECTION('ref_axis',(1.,0.,0.)) ;
#81744 = DIRECTION('center_axis',(0.,1.,0.)) ;
#81745 = DIRECTION('ref_axis',(1.,0.,0.)) ;
#81746 = DIRECTION('center_axis',(0.,1.,0.)) ;
#81747 = DIRECTION('ref_axis',(0.,0.,-1.)) ;
#81748 = DIRECTION('center_axis',(1.,2.16840434497101E-15,-2.93873587705572E-31)) ;
#81749 = DIRECTION('ref_axis',(2.16840434497101E-15,-1.,-1.03035812136257E-62)) ;
#81750 = DIRECTION('center_axis',(-8.95614743483648E-33,0.,1.)) ;
#81751 = DIRECTION('ref_axis',(1.,0.,8.95614743483648E-33)) ;
#81752 = DIRECTION('center_axis',(-1.40488587213121E-32,1.23908819712629E-16,
1.)) ;
#81753 = DIRECTION('ref_axis',(-1.74077750246726E-48,-1.,1.23908819712629E-16)) ;
#81754 = DIRECTION('center_axis',(8.95614743483648E-33,1.0154535431059E-48,
-1.)) ;
#81755 = DIRECTION('ref_axis',(-1.,9.09455164528354E-81,-8.95614743483648E-33)) ;
#81756 = DIRECTION('center_axis',(2.16840434497101E-15,0.,-1.)) ;
#81757 = DIRECTION('ref_axis',(-1.,0.,-2.16840434497101E-15)) ;
#81758 = DIRECTION('',(-8.95614743483648E-33,-1.0154535431059E-48,1.)) ;
#81759 = DIRECTION('center_axis',(-1.,-1.13380619344889E-16,0.)) ;
#81760 = DIRECTION('ref_axis',(0.,-1.,0.)) ;
#81761 = DIRECTION('center_axis',(0.,0.,1.)) ;
#81762 = DIRECTION('ref_axis',(-1.,0.,0.)) ;
#81763 = DIRECTION('center_axis',(0.,-1.,0.)) ;
#81764 = DIRECTION('ref_axis',(0.,0.,-1.)) ;
#81765 = DIRECTION('center_axis',(-1.,0.,0.)) ;
#81766 = DIRECTION('ref_axis',(0.,0.,-1.)) ;
#81767 = DIRECTION('center_axis',(1.,0.,1.40488587213121E-32)) ;
#81768 = DIRECTION('ref_axis',(1.40488587213121E-32,0.,-1.)) ;
#81769 = DIRECTION('',(1.,0.,1.40488587213121E-32)) ;
#81770 = DIRECTION('center_axis',(1.,0.,0.)) ;
#81771 = DIRECTION('ref_axis',(0.,0.,-1.)) ;
#81772 = DIRECTION('center_axis',(-1.40488587213121E-32,1.23908819712629E-16,
1.)) ;
#81773 = DIRECTION('ref_axis',(0.,-1.,0.)) ;
#81774 = DIRECTION('center_axis',(0.,-1.,0.)) ;
#81775 = DIRECTION('ref_axis',(0.,0.,1.)) ;
#81776 = DIRECTION('center_axis',(0.,1.,0.)) ;
#81777 = DIRECTION('ref_axis',(1.,0.,0.)) ;
#81778 = DIRECTION('center_axis',(1.,0.,0.)) ;
#81779 = DIRECTION('ref_axis',(0.,0.,1.)) ;
#81780 = DIRECTION('center_axis',(0.,1.,0.)) ;
#81781 = DIRECTION('ref_axis',(0.,0.,-1.)) ;
#81782 = DIRECTION('center_axis',(0.,0.,1.)) ;
#81783 = DIRECTION('ref_axis',(1.,0.,0.)) ;
#81784 = DIRECTION('center_axis',(0.,0.,1.)) ;
#81785 = DIRECTION('ref_axis',(1.,0.,0.)) ;
#81786 = DIRECTION('center_axis',(1.,0.,1.40488587213121E-32)) ;
#81787 = DIRECTION('ref_axis',(1.40488587213121E-32,0.,-1.)) ;
#81788 = DIRECTION('center_axis',(-0.707106781186546,0.707106781186549,4.10337830236758E-15)) ;
#81789 = DIRECTION('ref_axis',(0.707106781186549,0.707106781186546,2.73734725485009E-13)) ;
#81790 = DIRECTION('center_axis',(-1.23908819712629E-16,1.,-1.23908819712629E-16)) ;
#81791 = DIRECTION('ref_axis',(2.97429620636545E-47,1.23908819712629E-16,
1.)) ;
#81792 = DIRECTION('',(1.23908819712629E-16,-1.,1.23908819712629E-16)) ;
#81793 = DIRECTION('center_axis',(-1.,-1.13380619344889E-16,0.)) ;
#81794 = DIRECTION('ref_axis',(0.,-1.,0.)) ;
#81795 = DIRECTION('center_axis',(0.,-1.,0.)) ;
#81796 = DIRECTION('ref_axis',(0.,0.,1.)) ;
#81797 = DIRECTION('center_axis',(1.13380619344889E-16,-1.,1.23908819712629E-16)) ;
#81798 = DIRECTION('ref_axis',(1.40488587213121E-32,-1.23908819712629E-16,
-1.)) ;
#81799 = DIRECTION('center_axis',(-1.5529910948782E-31,-4.47619207437002E-16,
1.)) ;
#81800 = DIRECTION('ref_axis',(6.951486430461E-47,-1.,-4.47619207437002E-16)) ;
#81801 = DIRECTION('center_axis',(0.,2.16840434497101E-15,-1.)) ;
#81802 = DIRECTION('ref_axis',(0.,1.,2.16840434497101E-15)) ;
#81803 = DIRECTION('center_axis',(0.,1.,0.)) ;
#81804 = DIRECTION('ref_axis',(1.,0.,0.)) ;
#81805 = DIRECTION('center_axis',(3.85194802226865E-15,0.888198741900269,
-0.45945945945946)) ;
#81806 = DIRECTION('ref_axis',(3.2526065174565E-15,-0.45945945945946,-0.888198741900269)) ;
#81807 = DIRECTION('center_axis',(-1.,0.,1.22067519501986E-15)) ;
#81808 = DIRECTION('ref_axis',(-1.22067519501986E-15,-1.7347234759768E-14,
-1.)) ;
#81809 = DIRECTION('center_axis',(1.5529910948782E-31,4.47619207437002E-16,
-1.)) ;
#81810 = DIRECTION('ref_axis',(-6.951486430461E-47,1.,4.47619207437002E-16)) ;
#81811 = DIRECTION('center_axis',(0.,0.,1.)) ;
#81812 = DIRECTION('ref_axis',(1.,0.,0.)) ;
#81813 = DIRECTION('center_axis',(1.,-3.46944695195361E-16,0.)) ;
#81814 = DIRECTION('ref_axis',(3.46944695195361E-16,1.,0.)) ;
#81815 = DIRECTION('center_axis',(-1.,3.46944695195361E-16,0.)) ;
#81816 = DIRECTION('ref_axis',(3.46944695195361E-16,1.,0.)) ;
#81817 = DIRECTION('center_axis',(1.,-3.46944695195361E-16,0.)) ;
#81818 = DIRECTION('ref_axis',(3.41607084500048E-16,1.,0.)) ;
#81819 = DIRECTION('center_axis',(0.,0.459459459459457,-0.888198741900271)) ;
#81820 = DIRECTION('ref_axis',(0.,0.888198741900271,0.459459459459457)) ;
#81821 = DIRECTION('center_axis',(0.,0.,1.)) ;
#81822 = DIRECTION('ref_axis',(1.,0.,0.)) ;
#81823 = DIRECTION('center_axis',(0.,0.,-1.)) ;
#81824 = DIRECTION('ref_axis',(-1.,0.,0.)) ;
#81825 = DIRECTION('center_axis',(-1.,3.46944695195361E-16,0.)) ;
#81826 = DIRECTION('ref_axis',(-3.46944695195361E-16,-1.,0.)) ;
#81827 = DIRECTION('center_axis',(-1.,3.46944695195361E-16,0.)) ;
#81828 = DIRECTION('ref_axis',(-3.46944695195361E-16,-1.,0.)) ;
#81829 = DIRECTION('center_axis',(-1.,3.46944695195361E-16,0.)) ;
#81830 = DIRECTION('ref_axis',(3.46944695195361E-16,1.,-5.20417042793042E-14)) ;
#81831 = DIRECTION('center_axis',(1.,-3.46944695195361E-16,0.)) ;
#81832 = DIRECTION('ref_axis',(0.,1.,0.)) ;
#81833 = DIRECTION('center_axis',(0.,-0.888198741900269,0.459459459459461)) ;
#81834 = DIRECTION('ref_axis',(0.,0.459459459459461,0.888198741900269)) ;
#81835 = DIRECTION('center_axis',(0.,1.,0.)) ;
#81836 = DIRECTION('ref_axis',(1.,0.,0.)) ;
#81837 = DIRECTION('center_axis',(0.,1.,0.)) ;
#81838 = DIRECTION('ref_axis',(0.,0.,-1.)) ;
#81839 = DIRECTION('center_axis',(-1.,0.,0.)) ;
#81840 = DIRECTION('ref_axis',(0.,0.,-1.)) ;
#81841 = DIRECTION('center_axis',(1.,-3.46944695195361E-16,0.)) ;
#81842 = DIRECTION('ref_axis',(3.70074341541719E-16,1.,0.)) ;
#81843 = DIRECTION('center_axis',(0.,0.63294893130157,-0.774193548387094)) ;
#81844 = DIRECTION('ref_axis',(-1.08420217248551E-15,-0.774193548387094,-0.63294893130157)) ;
#81845 = DIRECTION('center_axis',(1.,-3.46944695195361E-16,0.)) ;
#81846 = DIRECTION('ref_axis',(3.80647894157197E-16,1.,0.)) ;
#81847 = DIRECTION('center_axis',(0.,-0.45945945945946,0.888198741900269)) ;
#81848 = DIRECTION('ref_axis',(0.,-0.888198741900269,-0.45945945945946)) ;
#81849 = DIRECTION('center_axis',(1.,-3.46944695195361E-16,0.)) ;
#81850 = DIRECTION('ref_axis',(3.46944695195361E-16,1.,0.)) ;
#81851 = DIRECTION('center_axis',(-1.,3.46944695195361E-16,0.)) ;
#81852 = DIRECTION('ref_axis',(3.46944695195361E-16,1.,8.67361737988405E-15)) ;
#81853 = DIRECTION('center_axis',(-3.46944695195361E-16,-1.,-2.45739631480277E-16)) ;
#81854 = DIRECTION('ref_axis',(1.,-3.46944695195361E-16,-8.52580615413453E-32)) ;
#81855 = DIRECTION('center_axis',(0.,1.,0.)) ;
#81856 = DIRECTION('ref_axis',(0.,0.,1.)) ;
#81857 = DIRECTION('center_axis',(1.,-3.46944695195361E-16,0.)) ;
#81858 = DIRECTION('ref_axis',(3.33066907387547E-16,1.,0.)) ;
#81859 = DIRECTION('center_axis',(8.02036034720251E-16,0.293103448275862,
-0.956080733311157)) ;
#81860 = DIRECTION('ref_axis',(-1.93209005840966E-30,0.956080733311157,0.293103448275862)) ;
#81861 = DIRECTION('center_axis',(-1.,3.46944695195361E-16,0.)) ;
#81862 = DIRECTION('ref_axis',(-3.46944695195361E-16,-1.,0.)) ;
#81863 = DIRECTION('center_axis',(-1.,3.46944695195361E-16,0.)) ;
#81864 = DIRECTION('ref_axis',(-3.46944695195361E-16,-1.,0.)) ;
#81865 = DIRECTION('center_axis',(-1.,3.46944695195361E-16,0.)) ;
#81866 = DIRECTION('ref_axis',(-3.46944695195361E-16,-1.,0.)) ;
#81867 = DIRECTION('center_axis',(0.,0.,-1.)) ;
#81868 = DIRECTION('ref_axis',(-1.,0.,0.)) ;
#81869 = DIRECTION('center_axis',(0.,0.,1.)) ;
#81870 = DIRECTION('ref_axis',(1.,0.,0.)) ;
#81871 = DIRECTION('center_axis',(-1.5529910948782E-31,-4.47619207437002E-16,
-1.)) ;
#81872 = DIRECTION('ref_axis',(-6.95148643046101E-47,1.,-4.47619207437002E-16)) ;
#81873 = DIRECTION('center_axis',(2.16840434497101E-15,0.,1.)) ;
#81874 = DIRECTION('ref_axis',(1.,0.,-2.16840434497101E-15)) ;
#81875 = DIRECTION('center_axis',(1.,-3.46944695195361E-16,0.)) ;
#81876 = DIRECTION('ref_axis',(0.,1.,0.)) ;
#81877 = DIRECTION('center_axis',(0.,-1.,0.)) ;
#81878 = DIRECTION('ref_axis',(0.,0.,1.)) ;
#81879 = DIRECTION('center_axis',(0.577350269189627,0.577350269189627,0.577350269189623)) ;
#81880 = DIRECTION('ref_axis',(-0.707106781186548,2.22044604925032E-15,0.707106781186547)) ;
#81881 = DIRECTION('center_axis',(-1.,3.46944695195361E-16,0.)) ;
#81882 = DIRECTION('ref_axis',(-3.70074341541719E-16,-1.,0.)) ;
#81883 = DIRECTION('center_axis',(0.,0.63294893130157,0.774193548387094)) ;
#81884 = DIRECTION('ref_axis',(0.,0.774193548387094,-0.63294893130157)) ;
#81885 = DIRECTION('center_axis',(0.,1.,0.)) ;
#81886 = DIRECTION('ref_axis',(1.,0.,0.)) ;
#81887 = DIRECTION('center_axis',(-1.,0.,0.)) ;
#81888 = DIRECTION('ref_axis',(0.,8.67361737988405E-15,-1.)) ;
#81889 = DIRECTION('center_axis',(0.,0.888198741900271,0.459459459459457)) ;
#81890 = DIRECTION('ref_axis',(-1.0842021724855E-15,0.459459459459457,-0.888198741900271)) ;
#81891 = DIRECTION('center_axis',(3.46944695195361E-16,1.,2.45739631480277E-16)) ;
#81892 = DIRECTION('ref_axis',(-1.,3.46944695195361E-16,8.52580615413453E-32)) ;
#81893 = DIRECTION('center_axis',(-1.,3.46944695195361E-16,0.)) ;
#81894 = DIRECTION('ref_axis',(-3.33066907387547E-16,-1.,0.)) ;
#81895 = DIRECTION('center_axis',(0.,0.293103448275864,0.956080733311156)) ;
#81896 = DIRECTION('ref_axis',(0.,-0.956080733311156,0.293103448275864)) ;
#81897 = DIRECTION('center_axis',(-3.46944695195361E-16,-1.,-1.06487173641454E-15)) ;
#81898 = DIRECTION('ref_axis',(3.69451600012496E-31,1.06487173641454E-15,
-1.)) ;
#81899 = DIRECTION('center_axis',(0.,-1.,0.)) ;
#81900 = DIRECTION('ref_axis',(0.,0.,-1.)) ;
#81901 = DIRECTION('center_axis',(0.,1.,0.)) ;
#81902 = DIRECTION('ref_axis',(0.,0.,1.)) ;
#81903 = DIRECTION('center_axis',(-1.,3.46944695195361E-16,0.)) ;
#81904 = DIRECTION('ref_axis',(-3.41607084500048E-16,-1.,0.)) ;
#81905 = DIRECTION('center_axis',(-4.88154879316133E-15,0.45945945945946,
0.888198741900269)) ;
#81906 = DIRECTION('ref_axis',(5.19745563204766E-30,-0.888198741900269,0.45945945945946)) ;
#81907 = DIRECTION('center_axis',(1.,-3.46944695195361E-16,0.)) ;
#81908 = DIRECTION('ref_axis',(3.46944695195361E-16,1.,0.)) ;
#81909 = DIRECTION('center_axis',(-1.,3.46944695195361E-16,0.)) ;
#81910 = DIRECTION('ref_axis',(3.46944695195361E-16,1.,0.)) ;
#81911 = DIRECTION('center_axis',(-1.5529910948782E-31,-4.47619207437002E-16,
-1.)) ;
#81912 = DIRECTION('ref_axis',(-6.95148643046101E-47,1.,-4.47619207437002E-16)) ;
#81913 = DIRECTION('center_axis',(0.,0.,-1.)) ;
#81914 = DIRECTION('ref_axis',(-1.,0.,0.)) ;
#81915 = DIRECTION('center_axis',(0.,0.224137931034483,-0.974557431797419)) ;
#81916 = DIRECTION('ref_axis',(0.,-0.974557431797419,-0.224137931034483)) ;
#81917 = DIRECTION('center_axis',(0.577350269189627,0.577350269189627,0.577350269189623)) ;
#81918 = DIRECTION('ref_axis',(-0.707106781186548,2.22044604925032E-15,0.707106781186547)) ;
#81919 = DIRECTION('center_axis',(0.408248290463864,-0.816496580927725,0.408248290463864)) ;
#81920 = DIRECTION('ref_axis',(0.707106781186545,-2.77555756156289E-15,-0.70710678118655)) ;
#81921 = DIRECTION('center_axis',(0.,1.,0.)) ;
#81922 = DIRECTION('ref_axis',(1.,0.,0.)) ;
#81923 = DIRECTION('center_axis',(-1.,0.,0.)) ;
#81924 = DIRECTION('ref_axis',(0.,8.67361737988401E-15,-1.)) ;
#81925 = DIRECTION('center_axis',(1.,-3.46944695195361E-16,0.)) ;
#81926 = DIRECTION('ref_axis',(0.,1.,0.)) ;
#81927 = DIRECTION('center_axis',(9.96293888229924E-16,-0.888198741900269,
-0.45945945945946)) ;
#81928 = DIRECTION('ref_axis',(-1.07192530966007E-30,-0.45945945945946,0.888198741900269)) ;
#81929 = DIRECTION('center_axis',(1.,-3.46944695195361E-16,0.)) ;
#81930 = DIRECTION('ref_axis',(-3.70074341541719E-16,-1.,0.)) ;
#81931 = DIRECTION('center_axis',(1.58436874053304E-16,-0.224137931034483,
-0.974557431797419)) ;
#81932 = DIRECTION('ref_axis',(2.18893094986727E-31,0.974557431797419,-0.224137931034483)) ;
#81933 = DIRECTION('center_axis',(1.,-3.46944695195361E-16,0.)) ;
#81934 = DIRECTION('ref_axis',(3.46944695195361E-16,1.,0.)) ;
#81935 = DIRECTION('center_axis',(-1.,3.46944695195361E-16,0.)) ;
#81936 = DIRECTION('ref_axis',(3.46944695195361E-16,1.,0.)) ;
#81937 = DIRECTION('center_axis',(1.,-3.46944695195361E-16,0.)) ;
#81938 = DIRECTION('ref_axis',(3.80647894157197E-16,1.,0.)) ;
#81939 = DIRECTION('center_axis',(0.,-0.45945945945946,-0.888198741900269)) ;
#81940 = DIRECTION('ref_axis',(0.,0.888198741900269,-0.45945945945946)) ;
#81941 = DIRECTION('center_axis',(1.,-3.46944695195361E-16,0.)) ;
#81942 = DIRECTION('ref_axis',(0.,1.,0.)) ;
#81943 = DIRECTION('center_axis',(0.,-1.,0.)) ;
#81944 = DIRECTION('ref_axis',(0.,0.,1.)) ;
#81945 = DIRECTION('center_axis',(-3.46944695195361E-16,-1.,-1.06487173641454E-15)) ;
#81946 = DIRECTION('ref_axis',(3.69451600012496E-31,1.06487173641454E-15,
-1.)) ;
#81947 = DIRECTION('center_axis',(0.,0.,1.)) ;
#81948 = DIRECTION('ref_axis',(1.,0.,0.)) ;
#81949 = DIRECTION('center_axis',(0.,-1.,0.)) ;
#81950 = DIRECTION('ref_axis',(0.,0.,-1.)) ;
#81951 = DIRECTION('center_axis',(0.,-1.,0.)) ;
#81952 = DIRECTION('ref_axis',(0.,0.,-1.)) ;
#81953 = DIRECTION('center_axis',(0.,1.,0.)) ;
#81954 = DIRECTION('ref_axis',(0.,0.,-1.)) ;
#81955 = DIRECTION('center_axis',(0.,0.,1.)) ;
#81956 = DIRECTION('ref_axis',(1.,0.,0.)) ;
#81957 = DIRECTION('center_axis',(8.67361737988404E-15,-1.,0.)) ;
#81958 = DIRECTION('ref_axis',(1.,8.67361737988404E-15,0.)) ;
#81959 = DIRECTION('center_axis',(0.497468338163091,-0.710669054518702,0.497468338163091)) ;
#81960 = DIRECTION('ref_axis',(0.81923192051904,0.573462344363328,8.04804396179112E-16)) ;
#81961 = DIRECTION('center_axis',(0.497468338163091,-0.710669054518702,0.497468338163091)) ;
#81962 = DIRECTION('ref_axis',(0.81923192051904,0.573462344363328,7.6535433881835E-16)) ;
#81963 = DIRECTION('center_axis',(0.497468338163092,-0.7106690545187,0.497468338163092)) ;
#81964 = DIRECTION('ref_axis',(3.85026974001056E-16,-0.57346234436333,-0.81923192051904)) ;
#81965 = DIRECTION('center_axis',(0.,0.,1.)) ;
#81966 = DIRECTION('ref_axis',(1.,0.,0.)) ;
#81967 = DIRECTION('center_axis',(0.,-1.,0.)) ;
#81968 = DIRECTION('ref_axis',(0.,0.,-1.)) ;
#81969 = DIRECTION('center_axis',(0.,1.,0.)) ;
#81970 = DIRECTION('ref_axis',(0.,0.,1.)) ;
#81971 = DIRECTION('center_axis',(0.,1.,0.)) ;
#81972 = DIRECTION('ref_axis',(0.,0.,1.)) ;
#81973 = DIRECTION('center_axis',(0.,1.,0.)) ;
#81974 = DIRECTION('ref_axis',(1.,0.,0.)) ;
#81975 = DIRECTION('center_axis',(-1.98515611757154E-15,0.,1.)) ;
#81976 = DIRECTION('ref_axis',(-1.,0.,-1.98515611757154E-15)) ;
#81977 = DIRECTION('center_axis',(1.,-4.06575814682065E-16,2.84603070277446E-16)) ;
#81978 = DIRECTION('ref_axis',(-4.06575814682065E-16,-1.,6.48893816316174E-47)) ;
#81979 = DIRECTION('center_axis',(0.,1.,0.)) ;
#81980 = DIRECTION('ref_axis',(0.,0.,1.)) ;
#81981 = DIRECTION('center_axis',(0.,1.,0.)) ;
#81982 = DIRECTION('ref_axis',(0.,0.,1.)) ;
#81983 = DIRECTION('center_axis',(0.497468338163091,0.710669054518702,-0.497468338163091)) ;
#81984 = DIRECTION('ref_axis',(-0.81923192051904,0.573462344363328,7.6535433881835E-16)) ;
#81985 = DIRECTION('center_axis',(-0.497468338163091,-0.710669054518702,0.497468338163091)) ;
#81986 = DIRECTION('ref_axis',(-0.819231920519043,0.573462344363324,-7.81372826690202E-15)) ;
#81987 = DIRECTION('center_axis',(-0.497468338163093,-0.7106690545187,0.497468338163091)) ;
#81988 = DIRECTION('ref_axis',(0.819231920519039,-0.573462344363331,1.48853464230757E-16)) ;
#81989 = DIRECTION('center_axis',(1.,0.,0.)) ;
#81990 = DIRECTION('ref_axis',(0.,0.,-1.)) ;
#81991 = DIRECTION('center_axis',(1.,0.,-9.9257805878577E-16)) ;
#81992 = DIRECTION('ref_axis',(-9.9257805878577E-16,0.,-1.)) ;
#81993 = DIRECTION('center_axis',(0.,0.,-1.)) ;
#81994 = DIRECTION('ref_axis',(-1.,0.,0.)) ;
#81995 = DIRECTION('center_axis',(-1.23327997120227E-15,1.76182853028895E-15,
1.)) ;
#81996 = DIRECTION('ref_axis',(-2.17282783909808E-30,-1.,1.76182853028895E-15)) ;
#81997 = DIRECTION('center_axis',(-0.497468338163091,0.710669054518702,0.497468338163091)) ;
#81998 = DIRECTION('ref_axis',(-0.81923192051904,-0.573462344363328,7.6535433881835E-16)) ;
#81999 = DIRECTION('center_axis',(0.497468338163091,-0.710669054518702,-0.497468338163091)) ;
#82000 = DIRECTION('ref_axis',(-0.819231920519046,-0.57346234436332,-1.68077391522259E-14)) ;
#82001 = DIRECTION('center_axis',(0.497468338163093,-0.7106690545187,-0.497468338163091)) ;
#82002 = DIRECTION('ref_axis',(0.819231920519039,0.573462344363331,2.16059097207149E-16)) ;
#82003 = DIRECTION('center_axis',(0.,1.,0.)) ;
#82004 = DIRECTION('ref_axis',(1.,0.,0.)) ;
#82005 = DIRECTION('center_axis',(-1.13841228110978E-15,-1.62630325872826E-15,
1.)) ;
#82006 = DIRECTION('ref_axis',(3.52365706057789E-15,1.,1.62630325872826E-15)) ;
#82007 = DIRECTION('center_axis',(0.,1.,0.)) ;
#82008 = DIRECTION('ref_axis',(1.,0.,0.)) ;
#82009 = DIRECTION('center_axis',(1.,0.,-1.65429676464295E-16)) ;
#82010 = DIRECTION('ref_axis',(1.65429676464295E-16,0.,1.)) ;
#82011 = DIRECTION('center_axis',(0.,0.,-1.)) ;
#82012 = DIRECTION('ref_axis',(-1.,0.,0.)) ;
#82013 = DIRECTION('center_axis',(3.3085935292859E-16,0.,1.)) ;
#82014 = DIRECTION('ref_axis',(1.,0.,-3.3085935292859E-16)) ;
#82015 = DIRECTION('center_axis',(1.,0.,0.)) ;
#82016 = DIRECTION('ref_axis',(0.,0.,-1.)) ;
#82017 = DIRECTION('center_axis',(1.,1.21972744404619E-15,8.53809210832338E-16)) ;
#82018 = DIRECTION('ref_axis',(-1.21972744404619E-15,1.,-2.84382165153726E-47)) ;
#82019 = DIRECTION('center_axis',(0.,1.,0.)) ;
#82020 = DIRECTION('ref_axis',(1.,0.,0.)) ;
#82021 = DIRECTION('center_axis',(0.497468338163092,0.710669054518701,0.497468338163092)) ;
#82022 = DIRECTION('ref_axis',(7.543021249686E-16,0.573462344363329,-0.81923192051904)) ;
#82023 = DIRECTION('center_axis',(-0.497468338163091,-0.710669054518702,-0.497468338163091)) ;
#82024 = DIRECTION('ref_axis',(0.81923192051904,-0.573462344363328,7.6535433881835E-16)) ;
#82025 = DIRECTION('center_axis',(-0.497468338163091,-0.710669054518702,-0.497468338163091)) ;
#82026 = DIRECTION('ref_axis',(0.81923192051904,-0.573462344363328,7.6535433881835E-16)) ;
#82027 = DIRECTION('center_axis',(0.,-1.,0.)) ;
#82028 = DIRECTION('ref_axis',(0.,0.,-1.)) ;
#82029 = DIRECTION('center_axis',(0.,1.,0.)) ;
#82030 = DIRECTION('ref_axis',(0.,0.,-1.)) ;
#82031 = DIRECTION('center_axis',(-8.67361737988403E-15,1.,0.)) ;
#82032 = DIRECTION('ref_axis',(-1.,-8.67361737988403E-15,0.)) ;
#82033 = DIRECTION('center_axis',(0.,0.,1.)) ;
#82034 = DIRECTION('ref_axis',(1.,0.,0.)) ;
#82035 = DIRECTION('center_axis',(1.,6.67201336914158E-17,0.)) ;
#82036 = DIRECTION('ref_axis',(-6.67201336914158E-17,1.,0.)) ;
#82037 = DIRECTION('center_axis',(-1.,-6.67201336914158E-17,0.)) ;
#82038 = DIRECTION('ref_axis',(-6.67201336914158E-17,1.,0.)) ;
#82039 = DIRECTION('center_axis',(-1.,1.33440267382831E-16,0.)) ;
#82040 = DIRECTION('ref_axis',(-1.33440267382831E-16,-1.,0.)) ;
#82041 = DIRECTION('center_axis',(-1.,1.33440267382831E-16,0.)) ;
#82042 = DIRECTION('ref_axis',(-1.33440267382831E-16,-1.,0.)) ;
#82043 = DIRECTION('center_axis',(0.710669054518702,0.497468338163091,0.497468338163091)) ;
#82044 = DIRECTION('ref_axis',(-0.573462344363328,0.819231920519041,3.92980824865032E-16)) ;
#82045 = DIRECTION('center_axis',(0.710669054518702,0.497468338163091,0.497468338163091)) ;
#82046 = DIRECTION('ref_axis',(-0.573462344363328,0.819231920519041,3.92980824865032E-16)) ;
#82047 = DIRECTION('center_axis',(0.710669054518701,0.497468338163091,0.497468338163092)) ;
#82048 = DIRECTION('ref_axis',(0.573462344363329,4.22980978511263E-16,-0.81923192051904)) ;
#82049 = DIRECTION('center_axis',(-0.710669054518702,0.497468338163091,-0.497468338163091)) ;
#82050 = DIRECTION('ref_axis',(-0.573462344363328,-0.819231920519041,6.69271761853466E-16)) ;
#82051 = DIRECTION('center_axis',(0.710669054518702,-0.497468338163091,0.497468338163091)) ;
#82052 = DIRECTION('ref_axis',(-0.573462344363328,-0.819231920519041,6.69271761853466E-16)) ;
#82053 = DIRECTION('center_axis',(0.7106690545187,-0.497468338163094,0.497468338163091)) ;
#82054 = DIRECTION('ref_axis',(0.573462344363331,0.819231920519038,2.86772422505918E-16)) ;
#82055 = DIRECTION('center_axis',(0.,1.,-9.34081871679819E-17)) ;
#82056 = DIRECTION('ref_axis',(0.,9.34081871679819E-17,1.)) ;
#82057 = DIRECTION('center_axis',(-4.33680868994205E-15,-1.,-3.03576608295944E-15)) ;
#82058 = DIRECTION('ref_axis',(1.,-4.33680868994205E-15,-1.12103877145985E-44)) ;
#82059 = DIRECTION('center_axis',(0.,1.,5.29374964685745E-15)) ;
#82060 = DIRECTION('ref_axis',(0.,-5.29374964685745E-15,1.)) ;
#82061 = DIRECTION('center_axis',(0.,1.,0.)) ;
#82062 = DIRECTION('ref_axis',(1.,0.,0.)) ;
#82063 = DIRECTION('center_axis',(0.,6.45175738210751E-15,1.)) ;
#82064 = DIRECTION('ref_axis',(0.,1.,-6.45175738210751E-15)) ;
#82065 = DIRECTION('center_axis',(-1.,-6.67201336914158E-17,0.)) ;
#82066 = DIRECTION('ref_axis',(6.67201336914158E-17,-1.,0.)) ;
#82067 = DIRECTION('center_axis',(-1.,-6.67201336914158E-17,0.)) ;
#82068 = DIRECTION('ref_axis',(6.67201336914158E-17,-1.,0.)) ;
#82069 = DIRECTION('center_axis',(1.,-1.33440267382831E-16,0.)) ;
#82070 = DIRECTION('ref_axis',(1.33440267382831E-16,1.,0.)) ;
#82071 = DIRECTION('center_axis',(-1.,1.33440267382831E-16,0.)) ;
#82072 = DIRECTION('ref_axis',(1.33440267382831E-16,1.,0.)) ;
#82073 = DIRECTION('center_axis',(0.,1.,0.)) ;
#82074 = DIRECTION('ref_axis',(1.,0.,0.)) ;
#82075 = DIRECTION('center_axis',(1.76182853028896E-15,-1.23327997120227E-15,
1.)) ;
#82076 = DIRECTION('ref_axis',(-1.,-2.1728278390981E-30,1.76182853028896E-15)) ;
#82077 = DIRECTION('center_axis',(0.,0.,-1.)) ;
#82078 = DIRECTION('ref_axis',(-1.,0.,0.)) ;
#82079 = DIRECTION('center_axis',(-2.71050543121378E-16,-1.89735380184965E-16,
1.)) ;
#82080 = DIRECTION('ref_axis',(1.,-5.14278778484758E-32,2.71050543121378E-16)) ;
#82081 = DIRECTION('center_axis',(-0.710669054518702,-0.497468338163091,0.497468338163091)) ;
#82082 = DIRECTION('ref_axis',(0.573462344363328,-0.819231920519041,3.92980824865032E-16)) ;
#82083 = DIRECTION('center_axis',(0.710669054518702,0.497468338163091,-0.497468338163091)) ;
#82084 = DIRECTION('ref_axis',(0.573462344363328,-0.819231920519041,3.92980824865032E-16)) ;
#82085 = DIRECTION('center_axis',(0.710669054518701,0.497468338163091,-0.497468338163092)) ;
#82086 = DIRECTION('ref_axis',(-0.573462344363329,-3.835309211505E-16,-0.81923192051904)) ;
#82087 = DIRECTION('center_axis',(0.710669054518702,-0.497468338163091,-0.497468338163091)) ;
#82088 = DIRECTION('ref_axis',(0.573462344363328,0.819231920519041,6.69271761853466E-16)) ;
#82089 = DIRECTION('center_axis',(0.710669054518702,-0.497468338163091,-0.497468338163091)) ;
#82090 = DIRECTION('ref_axis',(0.573462344363328,0.819231920519041,6.69271761853466E-16)) ;
#82091 = DIRECTION('center_axis',(0.7106690545187,-0.497468338163091,-0.497468338163093)) ;
#82092 = DIRECTION('ref_axis',(-0.57346234436333,9.18832260081103E-16,-0.819231920519039)) ;
#82093 = DIRECTION('center_axis',(0.,0.,-1.)) ;
#82094 = DIRECTION('ref_axis',(-1.,0.,0.)) ;
#82095 = DIRECTION('center_axis',(0.,1.15800773525007E-15,1.)) ;
#82096 = DIRECTION('ref_axis',(0.,-1.,1.15800773525007E-15)) ;
#82097 = DIRECTION('center_axis',(0.,1.,0.)) ;
#82098 = DIRECTION('ref_axis',(1.,0.,0.)) ;
#82099 = DIRECTION('center_axis',(0.,1.,0.)) ;
#82100 = DIRECTION('ref_axis',(0.,0.,-1.)) ;
#82101 = DIRECTION('center_axis',(0.,1.,0.)) ;
#82102 = DIRECTION('ref_axis',(1.,0.,0.)) ;
#82103 = DIRECTION('center_axis',(4.33680868994204E-15,-1.,-3.03576608295944E-15)) ;
#82104 = DIRECTION('ref_axis',(-1.,-4.33680868994204E-15,5.60519385729927E-45)) ;
#82105 = DIRECTION('center_axis',(0.,1.,9.34081871679819E-17)) ;
#82106 = DIRECTION('ref_axis',(0.,-9.34081871679819E-17,1.)) ;
#82107 = DIRECTION('center_axis',(0.,0.,1.)) ;
#82108 = DIRECTION('ref_axis',(1.,0.,0.)) ;
#82109 = DIRECTION('center_axis',(-2.16840434497102E-15,-3.61400724161847E-16,
1.)) ;
#82110 = DIRECTION('ref_axis',(1.,-7.83662900548222E-31,2.16840434497102E-15)) ;
#82111 = DIRECTION('center_axis',(0.973328526784575,0.162221421130762,-0.162221421130763)) ;
#82112 = DIRECTION('ref_axis',(-0.164398987305358,5.55382797573317E-16,-0.986393923832144)) ;
#82113 = DIRECTION('center_axis',(0.973328526784574,0.162221421130765,-0.162221421130767)) ;
#82114 = DIRECTION('ref_axis',(-0.164398987305362,-2.05045540520021E-17,-0.986393923832143)) ;
#82115 = DIRECTION('center_axis',(0.,1.,0.)) ;
#82116 = DIRECTION('ref_axis',(1.,0.,0.)) ;
#82117 = DIRECTION('center_axis',(0.,1.,-8.79325913341701E-15)) ;
#82118 = DIRECTION('ref_axis',(0.,-8.79325913341701E-15,-1.)) ;
#82119 = DIRECTION('center_axis',(0.,0.,1.)) ;
#82120 = DIRECTION('ref_axis',(1.,0.,0.)) ;
#82121 = DIRECTION('center_axis',(0.,-2.28569887277128E-15,1.)) ;
#82122 = DIRECTION('ref_axis',(0.,-1.,-2.28569887277128E-15)) ;
#82123 = DIRECTION('center_axis',(1.73472347597681E-15,-1.,-2.89120579329468E-16)) ;
#82124 = DIRECTION('ref_axis',(1.,1.73472347597681E-15,5.01544256350843E-31)) ;
#82125 = DIRECTION('center_axis',(8.67361737988409E-15,1.,-1.44560289664739E-15)) ;
#82126 = DIRECTION('ref_axis',(-1.,8.67361737988409E-15,-1.40129846432482E-45)) ;
#82127 = DIRECTION('center_axis',(0.,1.,0.)) ;
#82128 = DIRECTION('ref_axis',(1.,0.,0.)) ;
#82129 = DIRECTION('center_axis',(-0.937042571331634,0.312347523777217,0.156173761888611)) ;
#82130 = DIRECTION('ref_axis',(0.316227766016843,0.948683298050512,6.71158276827649E-18)) ;
#82131 = DIRECTION('center_axis',(0.937042571331636,-0.312347523777212,-0.156173761888606)) ;
#82132 = DIRECTION('ref_axis',(0.316227766016838,0.948683298050514,8.61595672567599E-16)) ;
#82133 = DIRECTION('center_axis',(-0.973328526784575,-0.162221421130762,-0.162221421130763)) ;
#82134 = DIRECTION('ref_axis',(-0.164398987305358,5.55382797573317E-16,0.986393923832144)) ;
#82135 = DIRECTION('center_axis',(0.97823197629215,-0.146734796047206,-0.146734795425419)) ;
#82136 = DIRECTION('ref_axis',(0.182318633555366,0.945435290883781,0.270022270581529)) ;
#82137 = DIRECTION('center_axis',(0.973328526784574,0.162221421130767,0.162221421130768)) ;
#82138 = DIRECTION('ref_axis',(0.164398987305363,2.02768900722254E-16,-0.986393923832143)) ;
#82139 = DIRECTION('center_axis',(0.,0.,1.)) ;
#82140 = DIRECTION('ref_axis',(1.,0.,0.)) ;
#82141 = DIRECTION('center_axis',(0.,2.19831478335425E-15,-1.)) ;
#82142 = DIRECTION('ref_axis',(0.,1.,2.19831478335425E-15)) ;
#82143 = DIRECTION('center_axis',(0.,1.,0.)) ;
#82144 = DIRECTION('ref_axis',(1.,0.,0.)) ;
#82145 = DIRECTION('center_axis',(8.67361737988408E-15,1.,1.44560289664739E-15)) ;
#82146 = DIRECTION('ref_axis',(1.,-8.67361737988408E-15,5.60519385729927E-45)) ;
#82147 = DIRECTION('center_axis',(1.73472347597681E-15,-1.,2.89120579329468E-16)) ;
#82148 = DIRECTION('ref_axis',(1.,1.73472347597681E-15,-5.01544256350843E-31)) ;
#82149 = DIRECTION('center_axis',(0.,1.,0.)) ;
#82150 = DIRECTION('ref_axis',(0.,0.,1.)) ;
#82151 = DIRECTION('center_axis',(0.,0.,1.)) ;
#82152 = DIRECTION('ref_axis',(1.,0.,0.)) ;
#82153 = DIRECTION('center_axis',(3.25260651745652E-15,-1.08420217248553E-15,
-1.)) ;
#82154 = DIRECTION('ref_axis',(-1.,-3.52648305246695E-30,-3.25260651745652E-15)) ;
#82155 = DIRECTION('center_axis',(0.,1.,0.)) ;
#82156 = DIRECTION('ref_axis',(1.,0.,0.)) ;
#82157 = DIRECTION('center_axis',(-0.937042571331635,0.312347523777215,-0.15617376188861)) ;
#82158 = DIRECTION('ref_axis',(0.316227766016841,0.948683298050513,6.5590042956861E-18)) ;
#82159 = DIRECTION('center_axis',(-0.937042571331636,0.312347523777212,-0.156173761888606)) ;
#82160 = DIRECTION('ref_axis',(0.331350514299575,0.654034959159593,-0.680033167478261)) ;
#82161 = DIRECTION('center_axis',(0.961519724091326,0.245047216427987,-0.124224320904711)) ;
#82162 = DIRECTION('ref_axis',(0.262092069890881,-0.682554728203127,0.682221950620082)) ;
#82163 = DIRECTION('center_axis',(2.65552944032596E-32,3.29043518662928E-48,
-1.)) ;
#82164 = DIRECTION('ref_axis',(-1.,8.7378475095785E-80,-2.65552944032596E-32)) ;
#82165 = DIRECTION('center_axis',(2.65552944032596E-32,3.29043518662928E-48,
-1.)) ;
#82166 = DIRECTION('ref_axis',(-1.,8.7378475095785E-80,-2.65552944032596E-32)) ;
#82167 = DIRECTION('center_axis',(-2.65552944032596E-32,-3.29043518662928E-48,
1.)) ;
#82168 = DIRECTION('ref_axis',(-1.,8.7378475095785E-80,-2.65552944032596E-32)) ;
#82169 = DIRECTION('center_axis',(0.,0.,1.)) ;
#82170 = DIRECTION('ref_axis',(1.,0.,0.)) ;
#82171 = DIRECTION('center_axis',(0.,0.,-1.)) ;
#82172 = DIRECTION('ref_axis',(-1.,0.,0.)) ;
#82173 = DIRECTION('center_axis',(0.,0.,1.)) ;
#82174 = DIRECTION('ref_axis',(1.,0.,0.)) ;
#82175 = DIRECTION('center_axis',(0.,0.,1.)) ;
#82176 = DIRECTION('ref_axis',(1.,0.,0.)) ;
#82177 = DIRECTION('center_axis',(0.,0.,-1.)) ;
#82178 = DIRECTION('ref_axis',(-1.,0.,0.)) ;
#82179 = DIRECTION('center_axis',(0.,0.,-1.)) ;
#82180 = DIRECTION('ref_axis',(-1.,0.,0.)) ;
#82181 = DIRECTION('center_axis',(1.,1.15648231731787E-15,0.)) ;
#82182 = DIRECTION('ref_axis',(1.03435541192675E-15,-1.,7.75766558945062E-16)) ;
#82183 = DIRECTION('center_axis',(7.089177613099E-16,-0.612994899008946,-0.790086864711098)) ;
#82184 = DIRECTION('ref_axis',(-4.46849810277083E-31,-0.790086864711098,0.612994899008946)) ;
#82185 = DIRECTION('center_axis',(7.08917761309899E-16,-0.612994899008945,
0.790086864711098)) ;
#82186 = DIRECTION('ref_axis',(-1.73472347597681E-14,0.790086864711098,0.612994899008945)) ;
#82187 = DIRECTION('center_axis',(0.,0.,-1.)) ;
#82188 = DIRECTION('ref_axis',(-1.,0.,0.)) ;
#82189 = DIRECTION('center_axis',(0.,0.,1.)) ;
#82190 = DIRECTION('ref_axis',(-1.,2.16840434497102E-15,0.)) ;
#82191 = DIRECTION('center_axis',(1.08420217248551E-15,-1.,0.)) ;
#82192 = DIRECTION('ref_axis',(1.,1.08420217248551E-15,0.)) ;
#82193 = DIRECTION('center_axis',(1.44560289664734E-16,-1.,-2.4093381610789E-16)) ;
#82194 = DIRECTION('ref_axis',(-7.25154722885103E-47,2.4093381610789E-16,
-1.)) ;
#82195 = DIRECTION('center_axis',(0.,-1.,0.)) ;
#82196 = DIRECTION('ref_axis',(0.,0.,-1.)) ;
#82197 = DIRECTION('center_axis',(1.,0.,0.)) ;
#82198 = DIRECTION('ref_axis',(0.,1.,0.)) ;
#82199 = DIRECTION('center_axis',(1.,0.,0.)) ;
#82200 = DIRECTION('ref_axis',(0.,0.,-1.)) ;
#82201 = DIRECTION('center_axis',(1.,1.23908819712629E-16,8.95614743483648E-33)) ;
#82202 = DIRECTION('ref_axis',(-1.23908819712629E-16,1.,-1.10974565782288E-48)) ;
#82203 = DIRECTION('center_axis',(1.,0.,0.)) ;
#82204 = DIRECTION('ref_axis',(0.,0.,-1.)) ;
#82205 = DIRECTION('center_axis',(-1.,0.,0.)) ;
#82206 = DIRECTION('ref_axis',(0.,0.,1.)) ;
#82207 = DIRECTION('center_axis',(1.,1.23908819712629E-16,8.95614743483648E-33)) ;
#82208 = DIRECTION('ref_axis',(-1.23908819712629E-16,1.,-1.10974565782288E-48)) ;
#82209 = DIRECTION('center_axis',(-1.,0.,0.)) ;
#82210 = DIRECTION('ref_axis',(0.,0.,1.)) ;
#82211 = DIRECTION('center_axis',(1.,0.,0.)) ;
#82212 = DIRECTION('ref_axis',(0.,-1.,0.)) ;
#82213 = DIRECTION('center_axis',(0.,1.,0.)) ;
#82214 = DIRECTION('ref_axis',(0.,0.,1.)) ;
#82215 = DIRECTION('center_axis',(-1.44560289664734E-16,1.,-7.2280144832367E-17)) ;
#82216 = DIRECTION('ref_axis',(0.707106781238324,1.5332934167208E-16,0.707106781134771)) ;
#82217 = DIRECTION('center_axis',(-1.0842021724855E-15,1.,0.)) ;
#82218 = DIRECTION('ref_axis',(-1.,-1.0842021724855E-15,0.)) ;
#82219 = DIRECTION('center_axis',(0.,1.,0.)) ;
#82220 = DIRECTION('ref_axis',(0.,0.,1.)) ;
#82221 = DIRECTION('center_axis',(0.,-1.,0.)) ;
#82222 = DIRECTION('ref_axis',(0.,0.,-1.)) ;
#82223 = DIRECTION('center_axis',(0.,1.,0.)) ;
#82224 = DIRECTION('ref_axis',(0.,0.,1.)) ;
#82225 = DIRECTION('center_axis',(0.,0.,1.)) ;
#82226 = DIRECTION('ref_axis',(1.,0.,0.)) ;
#82227 = DIRECTION('center_axis',(0.431191646767808,0.0335421424157979,0.901636672080181)) ;
#82228 = DIRECTION('ref_axis',(0.899826811333414,0.057359327390736,-0.432459960189175)) ;
#82229 = DIRECTION('center_axis',(0.,0.,1.)) ;
#82230 = DIRECTION('ref_axis',(-1.,0.,0.)) ;
#82231 = DIRECTION('center_axis',(0.,0.,-1.)) ;
#82232 = DIRECTION('ref_axis',(0.707109343403326,-0.707104218960485,0.)) ;
#82233 = DIRECTION('center_axis',(-3.25260651745653E-15,0.,1.)) ;
#82234 = DIRECTION('ref_axis',(1.,0.,3.25260651745653E-15)) ;
#82235 = DIRECTION('center_axis',(0.,0.,1.)) ;
#82236 = DIRECTION('ref_axis',(1.,0.,0.)) ;
#82237 = DIRECTION('center_axis',(0.431188264323626,0.0335835000995436,-0.901636750155318)) ;
#82238 = DIRECTION('ref_axis',(0.899831768136793,0.0572892327006458,0.432458937782981)) ;
#82239 = DIRECTION('center_axis',(0.,-1.,0.)) ;
#82240 = DIRECTION('ref_axis',(0.,0.,-1.)) ;
#82241 = DIRECTION('center_axis',(0.,1.,0.)) ;
#82242 = DIRECTION('ref_axis',(0.,0.,1.)) ;
#82243 = DIRECTION('center_axis',(0.,0.,1.)) ;
#82244 = DIRECTION('ref_axis',(1.,0.,0.)) ;
#82245 = DIRECTION('center_axis',(0.,0.,-1.)) ;
#82246 = DIRECTION('ref_axis',(-1.,0.,0.)) ;
#82247 = DIRECTION('center_axis',(0.,0.,1.)) ;
#82248 = DIRECTION('ref_axis',(-0.986393923832144,0.164398987305354,0.)) ;
#82249 = DIRECTION('center_axis',(0.98470178743927,-0.164116964573216,0.0585492250433781)) ;
#82250 = DIRECTION('ref_axis',(0.164398987305362,0.986393923832143,-7.60669428566932E-17)) ;
#82251 = DIRECTION('center_axis',(0.984834538781277,-0.164139089796902,0.0562075655416074)) ;
#82252 = DIRECTION('ref_axis',(0.164398987305379,0.98639392383214,1.87706412796466E-17)) ;
#82253 = DIRECTION('center_axis',(0.986393923832144,-0.129889480441767,0.100775740620418)) ;
#82254 = DIRECTION('ref_axis',(0.,0.612994899008947,0.790086864711097)) ;
#82255 = DIRECTION('center_axis',(0.,1.,0.)) ;
#82256 = DIRECTION('ref_axis',(1.,0.,0.)) ;
#82257 = DIRECTION('center_axis',(0.,0.,-1.)) ;
#82258 = DIRECTION('ref_axis',(-1.,0.,0.)) ;
#82259 = DIRECTION('center_axis',(1.,2.8359373108165E-15,0.)) ;
#82260 = DIRECTION('ref_axis',(-2.8359373108165E-15,1.,0.)) ;
#82261 = DIRECTION('center_axis',(0.,0.,-1.)) ;
#82262 = DIRECTION('ref_axis',(-1.,0.,0.)) ;
#82263 = DIRECTION('center_axis',(0.,0.,1.)) ;
#82264 = DIRECTION('ref_axis',(1.,0.,0.)) ;
#82265 = DIRECTION('center_axis',(1.,0.,0.)) ;
#82266 = DIRECTION('ref_axis',(0.,0.,-1.)) ;
#82267 = DIRECTION('center_axis',(1.,0.,0.)) ;
#82268 = DIRECTION('ref_axis',(0.,0.,-1.)) ;
#82269 = DIRECTION('center_axis',(0.,1.,0.)) ;
#82270 = DIRECTION('ref_axis',(1.,0.,0.)) ;
#82271 = DIRECTION('center_axis',(1.,-8.50781193244945E-15,0.)) ;
#82272 = DIRECTION('ref_axis',(8.50781193244945E-15,1.,0.)) ;
#82273 = DIRECTION('center_axis',(0.,1.,0.)) ;
#82274 = DIRECTION('ref_axis',(1.,0.,0.)) ;
#82275 = DIRECTION('center_axis',(-5.42101086242753E-16,1.70882313734897E-16,
1.)) ;
#82276 = DIRECTION('ref_axis',(1.,9.26354878953623E-32,5.42101086242753E-16)) ;
#82277 = DIRECTION('center_axis',(-1.,0.,0.)) ;
#82278 = DIRECTION('ref_axis',(0.,0.,1.)) ;
#82279 = DIRECTION('center_axis',(1.,0.,0.)) ;
#82280 = DIRECTION('ref_axis',(0.,0.,-1.)) ;
#82281 = DIRECTION('center_axis',(0.,0.,-1.)) ;
#82282 = DIRECTION('ref_axis',(-1.,0.,0.)) ;
#82283 = DIRECTION('center_axis',(0.,0.,1.)) ;
#82284 = DIRECTION('ref_axis',(1.,0.,0.)) ;
#82285 = DIRECTION('center_axis',(0.,1.,0.)) ;
#82286 = DIRECTION('ref_axis',(1.,0.,0.)) ;
#82287 = DIRECTION('center_axis',(0.,1.,0.)) ;
#82288 = DIRECTION('ref_axis',(1.,0.,0.)) ;
#82289 = DIRECTION('center_axis',(0.,0.,-1.)) ;
#82290 = DIRECTION('ref_axis',(-1.,0.,0.)) ;
#82291 = DIRECTION('center_axis',(0.,1.,0.)) ;
#82292 = DIRECTION('ref_axis',(0.,0.,1.)) ;
#82293 = DIRECTION('center_axis',(0.,0.,-1.)) ;
#82294 = DIRECTION('ref_axis',(-1.,0.,0.)) ;
#82295 = DIRECTION('center_axis',(0.,0.,1.)) ;
#82296 = DIRECTION('ref_axis',(1.,0.,0.)) ;
#82297 = DIRECTION('center_axis',(1.33440267382831E-16,1.,0.)) ;
#82298 = DIRECTION('ref_axis',(-1.,1.33440267382831E-16,0.)) ;
#82299 = DIRECTION('center_axis',(0.,1.,0.)) ;
#82300 = DIRECTION('ref_axis',(0.,0.,1.)) ;
#82301 = DIRECTION('center_axis',(0.,1.,0.)) ;
#82302 = DIRECTION('ref_axis',(1.,0.,0.)) ;
#82303 = DIRECTION('center_axis',(0.,1.,0.)) ;
#82304 = DIRECTION('ref_axis',(0.,0.,1.)) ;
#82305 = DIRECTION('center_axis',(0.,1.,0.)) ;
#82306 = DIRECTION('ref_axis',(1.,0.,0.)) ;
#82307 = DIRECTION('center_axis',(1.37797793267296E-15,-1.62630325872825E-15,
1.)) ;
#82308 = DIRECTION('ref_axis',(-2.24101000236165E-30,-1.,-1.62630325872825E-15)) ;
#82309 = DIRECTION('center_axis',(-1.33440267382831E-16,-1.,0.)) ;
#82310 = DIRECTION('ref_axis',(1.,-1.33440267382831E-16,0.)) ;
#82311 = DIRECTION('center_axis',(0.,1.,0.)) ;
#82312 = DIRECTION('ref_axis',(0.,0.,1.)) ;
#82313 = DIRECTION('center_axis',(0.,0.,-1.)) ;
#82314 = DIRECTION('ref_axis',(-1.,0.,0.)) ;
#82315 = DIRECTION('center_axis',(0.,0.,1.)) ;
#82316 = DIRECTION('ref_axis',(1.,0.,0.)) ;
#82317 = DIRECTION('center_axis',(0.,1.,0.)) ;
#82318 = DIRECTION('ref_axis',(1.,0.,0.)) ;
#82319 = DIRECTION('center_axis',(0.,0.,1.)) ;
#82320 = DIRECTION('ref_axis',(1.,0.,0.)) ;
#82321 = DIRECTION('center_axis',(0.,0.,1.)) ;
#82322 = DIRECTION('ref_axis',(1.,0.,0.)) ;
#82323 = DIRECTION('center_axis',(0.,0.,1.)) ;
#82324 = DIRECTION('ref_axis',(-0.986393923832144,0.164398987305354,0.)) ;
#82325 = DIRECTION('center_axis',(0.984701787439272,-0.164116964573205,-0.0585492250433871)) ;
#82326 = DIRECTION('ref_axis',(0.16439898730535,0.986393923832145,-3.2807868055655E-16)) ;
#82327 = DIRECTION('center_axis',(0.984834538781259,-0.164139089796881,-0.0562075655419907)) ;
#82328 = DIRECTION('ref_axis',(0.164398987305362,0.986393923832143,6.03508511856301E-17)) ;
#82329 = DIRECTION('center_axis',(0.,0.,1.)) ;
#82330 = DIRECTION('ref_axis',(-0.986393923832144,0.164398987305354,0.)) ;
#82331 = DIRECTION('center_axis',(0.,0.,1.)) ;
#82332 = DIRECTION('ref_axis',(1.,0.,0.)) ;
#82333 = DIRECTION('center_axis',(0.342346838791228,0.100237737313318,-0.934211452503104)) ;
#82334 = DIRECTION('ref_axis',(0.878411849450466,0.318727804720941,0.356097190725765)) ;
#82335 = DIRECTION('center_axis',(0.,0.,-1.)) ;
#82336 = DIRECTION('ref_axis',(-1.,0.,0.)) ;
#82337 = DIRECTION('center_axis',(0.,0.,-1.)) ;
#82338 = DIRECTION('ref_axis',(-1.,0.,0.)) ;
#82339 = DIRECTION('center_axis',(0.,0.,-1.)) ;
#82340 = DIRECTION('ref_axis',(-1.,0.,0.)) ;
#82341 = DIRECTION('center_axis',(-0.34234683879479,-0.100237737344036,-0.934211452498503)) ;
#82342 = DIRECTION('ref_axis',(0.878411778138233,0.318728006274644,-0.356097186234627)) ;
#82343 = DIRECTION('center_axis',(0.,0.,1.)) ;
#82344 = DIRECTION('ref_axis',(1.,0.,0.)) ;
#82345 = DIRECTION('center_axis',(0.967224433243486,0.251696850982797,0.0335498277515765)) ;
#82346 = DIRECTION('ref_axis',(0.148186128295972,-0.666803800143469,0.73035167111117)) ;
#82347 = DIRECTION('center_axis',(0.,0.707106781186549,-0.707106781186547)) ;
#82348 = DIRECTION('ref_axis',(0.,0.707106781186546,0.707106781186549)) ;
#82349 = DIRECTION('center_axis',(0.978007532938557,-0.147978541149799,-0.146981688909249)) ;
#82350 = DIRECTION('ref_axis',(0.193734423935374,0.383507624650126,0.902988856419417)) ;
#82351 = DIRECTION('center_axis',(0.,0.447213595499958,0.894427190999916)) ;
#82352 = DIRECTION('ref_axis',(0.,-0.894427190999916,0.447213595499958)) ;
#82353 = DIRECTION('center_axis',(0.960001452008117,0.250435160947751,-0.125217579849561)) ;
#82354 = DIRECTION('ref_axis',(0.276742394168104,-0.916645079798534,0.288401534238716)) ;
#82355 = DIRECTION('center_axis',(0.,1.,0.)) ;
#82356 = DIRECTION('ref_axis',(0.,0.,1.)) ;
#82357 = DIRECTION('center_axis',(-1.,0.,0.)) ;
#82358 = DIRECTION('ref_axis',(0.,0.413905208611621,-0.910319986754202)) ;
#82359 = DIRECTION('center_axis',(1.,1.44560289664734E-16,0.)) ;
#82360 = DIRECTION('ref_axis',(0.,1.,0.)) ;
#82361 = DIRECTION('center_axis',(1.,1.44560289664734E-16,0.)) ;
#82362 = DIRECTION('ref_axis',(-1.44560289664734E-16,1.,0.)) ;
#82363 = DIRECTION('center_axis',(0.,0.,-1.)) ;
#82364 = DIRECTION('ref_axis',(0.,-1.,0.)) ;
#82365 = DIRECTION('center_axis',(-1.,-1.44560289664734E-16,0.)) ;
#82366 = DIRECTION('ref_axis',(-1.44560289664734E-16,1.,0.)) ;
#82367 = DIRECTION('center_axis',(1.,-3.46944695195361E-16,0.)) ;
#82368 = DIRECTION('ref_axis',(2.61228946970625E-16,1.,0.)) ;
#82369 = DIRECTION('center_axis',(1.,-3.46944695195361E-16,0.)) ;
#82370 = DIRECTION('ref_axis',(3.46944695195361E-16,1.,0.)) ;
#82371 = DIRECTION('center_axis',(0.,0.,1.)) ;
#82372 = DIRECTION('ref_axis',(-3.26536183713281E-16,-1.,0.)) ;
#82373 = DIRECTION('center_axis',(-1.,3.46944695195361E-16,0.)) ;
#82374 = DIRECTION('ref_axis',(3.46944695195361E-16,1.,0.)) ;
#82375 = DIRECTION('center_axis',(-1.,3.46944695195361E-16,0.)) ;
#82376 = DIRECTION('ref_axis',(-3.46944695195361E-16,-1.,0.)) ;
#82377 = DIRECTION('center_axis',(-1.,0.,0.)) ;
#82378 = DIRECTION('ref_axis',(0.,0.,1.)) ;
#82379 = DIRECTION('',(1.,-3.46944695195361E-16,0.)) ;
#82380 = DIRECTION('center_axis',(-1.,8.01625584951926E-16,-1.08420217248551E-15)) ;
#82381 = DIRECTION('ref_axis',(1.08420217248551E-15,-4.33680868994204E-15,
-1.)) ;
#82382 = DIRECTION('center_axis',(-1.,8.01625584951926E-16,-1.08420217248551E-15)) ;
#82383 = DIRECTION('ref_axis',(1.08420217248551E-15,-4.33680868994204E-15,
-1.)) ;
#82384 = DIRECTION('',(-1.,3.46944695195361E-16,0.)) ;
#82385 = DIRECTION('center_axis',(-1.,3.46944695195361E-16,0.)) ;
#82386 = DIRECTION('ref_axis',(-3.46944695195361E-16,-1.,0.)) ;
#82387 = DIRECTION('center_axis',(-1.,0.,0.)) ;
#82388 = DIRECTION('ref_axis',(0.,0.,1.)) ;
#82389 = DIRECTION('',(1.,-3.46944695195361E-16,0.)) ;
#82390 = DIRECTION('center_axis',(-1.,2.2680138501079E-15,0.)) ;
#82391 = DIRECTION('ref_axis',(2.2680138501079E-15,1.,0.)) ;
#82392 = DIRECTION('',(-1.,3.46944695195361E-16,0.)) ;
#82393 = DIRECTION('center_axis',(-1.,3.18032637262401E-16,0.)) ;
#82394 = DIRECTION('ref_axis',(-5.55111512312578E-16,-1.,0.)) ;
#82395 = DIRECTION('center_axis',(1.,-3.18032637262401E-16,0.)) ;
#82396 = DIRECTION('ref_axis',(-3.18032637262401E-16,-1.,0.)) ;
#82397 = DIRECTION('center_axis',(-2.01298417874256E-16,-0.632948931301568,
-0.774193548387096)) ;
#82398 = DIRECTION('ref_axis',(1.73472347597681E-14,-0.774193548387096,0.632948931301568)) ;
#82399 = DIRECTION('center_axis',(-1.,3.18032637262401E-16,0.)) ;
#82400 = DIRECTION('ref_axis',(-3.18032637262401E-16,-1.,0.)) ;
#82401 = DIRECTION('center_axis',(-2.01298417874256E-16,-0.632948931301568,
0.774193548387096)) ;
#82402 = DIRECTION('ref_axis',(9.63584817660562E-32,-0.774193548387096,-0.632948931301568)) ;
#82403 = DIRECTION('center_axis',(1.,1.44560289664734E-16,0.)) ;
#82404 = DIRECTION('ref_axis',(-1.44560289664734E-16,1.,0.)) ;
#82405 = DIRECTION('',(-1.,-1.44560289664734E-16,0.)) ;
#82406 = DIRECTION('center_axis',(-1.,3.46944695195361E-16,0.)) ;
#82407 = DIRECTION('ref_axis',(-3.46944695195361E-16,-1.,0.)) ;
#82408 = DIRECTION('',(-1.,3.46944695195361E-16,0.)) ;
#82409 = DIRECTION('center_axis',(-1.,3.46944695195361E-16,0.)) ;
#82410 = DIRECTION('ref_axis',(3.46944695195361E-16,1.,-3.46944695195361E-15)) ;
#82411 = DIRECTION('center_axis',(-1.,3.46944695195361E-16,0.)) ;
#82412 = DIRECTION('ref_axis',(3.46944695195361E-16,1.,0.)) ;
#82413 = DIRECTION('center_axis',(-1.,3.46944695195361E-16,0.)) ;
#82414 = DIRECTION('ref_axis',(-3.46944695195361E-16,-1.,0.)) ;
#82415 = DIRECTION('',(1.,-3.46944695195361E-16,0.)) ;
#82416 = DIRECTION('center_axis',(-1.,-1.44560289664734E-16,-2.65552944032596E-32)) ;
#82417 = DIRECTION('ref_axis',(1.44560289664734E-16,-1.,-2.80018320648271E-64)) ;
#82418 = DIRECTION('',(2.65552944032596E-32,3.29043518662928E-48,-1.)) ;
#82419 = DIRECTION('',(1.44560289664734E-16,-1.,-2.4093381610789E-16)) ;
#82420 = DIRECTION('',(0.,0.,1.)) ;
#82421 = DIRECTION('center_axis',(0.999999956301289,0.000282786981403369,
8.61913163653833E-5)) ;
#82422 = DIRECTION('ref_axis',(0.000288266391240805,-0.997396273402903,-0.0721151211916738)) ;
#82423 = DIRECTION('',(-1.44560289664734E-16,1.,-7.2280144832367E-17)) ;
#82424 = DIRECTION('center_axis',(0.316227766016838,0.948683298050514,0.)) ;
#82425 = DIRECTION('ref_axis',(-0.948683298050514,0.316227766016838,0.)) ;
#82426 = DIRECTION('',(-0.948683298050514,0.316227766016838,0.)) ;
#82427 = DIRECTION('',(0.,0.,1.)) ;
#82428 = DIRECTION('',(0.937042571331636,-0.312347523777212,-0.156173761888606)) ;
#82429 = DIRECTION('',(0.,0.,-1.)) ;
#82430 = DIRECTION('center_axis',(1.,1.73472347597681E-15,0.)) ;
#82431 = DIRECTION('ref_axis',(-1.73472347597681E-15,1.,0.)) ;
#82432 = DIRECTION('',(-1.73472347597681E-15,1.,0.)) ;
#82433 = DIRECTION('',(0.,0.,1.)) ;
#82434 = DIRECTION('',(1.73472347597681E-15,-1.,-2.89120579329468E-16)) ;
#82435 = DIRECTION('',(0.,0.,-1.)) ;
#82436 = DIRECTION('center_axis',(0.164398987305357,-0.986393923832144,0.)) ;
#82437 = DIRECTION('ref_axis',(0.986393923832144,0.164398987305357,0.)) ;
#82438 = DIRECTION('',(-0.973328526784575,-0.162221421130762,0.162221421130763)) ;
#82439 = DIRECTION('',(0.,0.,-1.)) ;
#82440 = DIRECTION('',(0.986393923832144,0.164398987305357,0.)) ;
#82441 = DIRECTION('',(0.,0.,1.)) ;
#82442 = DIRECTION('center_axis',(-9.91270557701033E-17,1.,0.)) ;
#82443 = DIRECTION('ref_axis',(-1.,-9.91270557701033E-17,0.)) ;
#82444 = DIRECTION('',(1.,9.91270557701033E-17,0.)) ;
#82445 = DIRECTION('',(0.,0.,-1.)) ;
#82446 = DIRECTION('',(-1.,-9.91270557701033E-17,0.)) ;
#82447 = DIRECTION('',(0.,0.,1.)) ;
#82448 = DIRECTION('center_axis',(-9.91270557701033E-17,1.,0.)) ;
#82449 = DIRECTION('ref_axis',(-1.,-9.91270557701033E-17,0.)) ;
#82450 = DIRECTION('',(-1.,-9.91270557701033E-17,0.)) ;
#82451 = DIRECTION('',(0.,0.,-1.)) ;
#82452 = DIRECTION('',(-1.,-9.91270557701033E-17,0.)) ;
#82453 = DIRECTION('',(0.,0.,1.)) ;
#82454 = DIRECTION('center_axis',(1.,1.15648231731787E-15,0.)) ;
#82455 = DIRECTION('ref_axis',(-1.15648231731787E-15,1.,0.)) ;
#82456 = DIRECTION('',(-1.15648231731787E-15,1.,0.)) ;
#82457 = DIRECTION('',(0.,0.,-1.)) ;
#82458 = DIRECTION('',(-1.15648231731787E-15,1.,0.)) ;
#82459 = DIRECTION('',(0.,0.,1.)) ;
#82460 = DIRECTION('center_axis',(-1.,-1.15648231731787E-15,0.)) ;
#82461 = DIRECTION('ref_axis',(-1.15648231731787E-15,1.,1.56060533014952E-15)) ;
#82462 = DIRECTION('',(0.,0.,1.)) ;
#82463 = DIRECTION('center_axis',(0.,0.,1.)) ;
#82464 = DIRECTION('ref_axis',(1.,0.,0.)) ;
#82465 = DIRECTION('',(-1.,0.,0.)) ;
#82466 = DIRECTION('center_axis',(0.,0.,-1.)) ;
#82467 = DIRECTION('ref_axis',(1.,0.,0.)) ;
#82468 = DIRECTION('center_axis',(0.,0.,-1.)) ;
#82469 = DIRECTION('ref_axis',(1.,0.,0.)) ;
#82470 = DIRECTION('center_axis',(0.,0.,-1.)) ;
#82471 = DIRECTION('ref_axis',(1.,0.,0.)) ;
#82472 = DIRECTION('center_axis',(0.,0.,-1.)) ;
#82473 = DIRECTION('ref_axis',(1.,0.,0.)) ;
#82474 = DIRECTION('',(1.,0.,0.)) ;
#82475 = DIRECTION('center_axis',(0.,0.,1.)) ;
#82476 = DIRECTION('ref_axis',(1.,0.,0.)) ;
#82477 = DIRECTION('',(3.46944695195361E-16,1.,0.)) ;
#82478 = DIRECTION('center_axis',(0.,0.,1.)) ;
#82479 = DIRECTION('ref_axis',(1.,0.,0.)) ;
#82480 = DIRECTION('',(1.,-3.46944695195361E-16,0.)) ;
#82481 = DIRECTION('center_axis',(0.,0.,-1.)) ;
#82482 = DIRECTION('ref_axis',(1.,0.,0.)) ;
#82483 = DIRECTION('',(2.71050543121376E-16,1.,0.)) ;
#82484 = DIRECTION('center_axis',(0.,0.,-1.)) ;
#82485 = DIRECTION('ref_axis',(1.,0.,0.)) ;
#82486 = DIRECTION('',(-1.,3.46944695195361E-16,0.)) ;
#82487 = DIRECTION('center_axis',(0.,0.,1.)) ;
#82488 = DIRECTION('ref_axis',(1.,0.,0.)) ;
#82489 = DIRECTION('',(3.46944695195361E-16,1.,0.)) ;
#82490 = DIRECTION('center_axis',(0.,0.,1.)) ;
#82491 = DIRECTION('ref_axis',(1.,0.,0.)) ;
#82492 = DIRECTION('center_axis',(0.,0.,-1.)) ;
#82493 = DIRECTION('ref_axis',(1.,0.,0.)) ;
#82494 = DIRECTION('',(0.986393923832144,-0.164398987305354,0.)) ;
#82495 = DIRECTION('center_axis',(0.,0.,-1.)) ;
#82496 = DIRECTION('ref_axis',(1.,-6.50521303491307E-15,0.)) ;
#82497 = DIRECTION('center_axis',(0.,0.,-1.)) ;
#82498 = DIRECTION('ref_axis',(1.,0.,0.)) ;
#82499 = DIRECTION('',(1.,0.,0.)) ;
#82500 = DIRECTION('',(1.13380619344889E-16,-1.,0.)) ;
#82501 = DIRECTION('center_axis',(0.,0.,-1.)) ;
#82502 = DIRECTION('ref_axis',(1.,0.,0.)) ;
#82503 = DIRECTION('',(-1.,-1.92747052886312E-16,0.)) ;
#82504 = DIRECTION('center_axis',(0.,0.,1.)) ;
#82505 = DIRECTION('ref_axis',(1.,0.,0.)) ;
#82506 = DIRECTION('',(0.,-1.,0.)) ;
#82507 = DIRECTION('center_axis',(0.,0.,-1.)) ;
#82508 = DIRECTION('ref_axis',(1.,0.,0.)) ;
#82509 = DIRECTION('center_axis',(0.,0.,1.)) ;
#82510 = DIRECTION('ref_axis',(1.,0.,0.)) ;
#82511 = DIRECTION('',(-0.948683298050514,0.316227766016838,0.)) ;
#82512 = DIRECTION('center_axis',(0.,0.,1.)) ;
#82513 = DIRECTION('ref_axis',(1.,0.,0.)) ;
#82514 = DIRECTION('',(-1.,0.,0.)) ;
#82515 = DIRECTION('center_axis',(0.,0.,1.)) ;
#82516 = DIRECTION('ref_axis',(1.,0.,0.)) ;
#82517 = DIRECTION('',(0.,-1.,0.)) ;
#82518 = DIRECTION('center_axis',(0.,0.,-1.)) ;
#82519 = DIRECTION('ref_axis',(1.,0.,0.)) ;
#82520 = DIRECTION('',(-1.,-1.92747052886312E-16,0.)) ;
#82521 = DIRECTION('center_axis',(0.,0.,1.)) ;
#82522 = DIRECTION('ref_axis',(1.,0.,0.)) ;
#82523 = DIRECTION('',(1.13380619344889E-16,-1.,0.)) ;
#82524 = DIRECTION('',(1.,0.,0.)) ;
#82525 = DIRECTION('center_axis',(0.,0.,1.)) ;
#82526 = DIRECTION('ref_axis',(1.,0.,0.)) ;
#82527 = DIRECTION('center_axis',(0.,0.,1.)) ;
#82528 = DIRECTION('ref_axis',(1.,0.,0.)) ;
#82529 = DIRECTION('',(-0.986393923832144,0.164398987305354,0.)) ;
#82530 = DIRECTION('center_axis',(0.,0.,1.)) ;
#82531 = DIRECTION('ref_axis',(1.,0.,0.)) ;
#82532 = DIRECTION('center_axis',(0.,0.,-1.)) ;
#82533 = DIRECTION('ref_axis',(1.,0.,0.)) ;
#82534 = DIRECTION('',(-3.46944695195361E-16,-1.,0.)) ;
#82535 = DIRECTION('center_axis',(0.,0.,-1.)) ;
#82536 = DIRECTION('ref_axis',(1.,0.,0.)) ;
#82537 = DIRECTION('',(-1.,3.46944695195361E-16,0.)) ;
#82538 = DIRECTION('center_axis',(0.,0.,1.)) ;
#82539 = DIRECTION('ref_axis',(1.,0.,0.)) ;
#82540 = DIRECTION('',(3.46944695195361E-16,1.,0.)) ;
#82541 = DIRECTION('center_axis',(0.,0.,1.)) ;
#82542 = DIRECTION('ref_axis',(1.,0.,0.)) ;
#82543 = DIRECTION('',(1.,-3.46944695195361E-16,0.)) ;
#82544 = DIRECTION('center_axis',(0.,0.,-1.)) ;
#82545 = DIRECTION('ref_axis',(1.,0.,0.)) ;
#82546 = DIRECTION('',(-3.46944695195361E-16,-1.,0.)) ;
#82547 = DIRECTION('center_axis',(0.,0.,-1.)) ;
#82548 = DIRECTION('ref_axis',(1.,0.,0.)) ;
#82549 = DIRECTION('',(1.,0.,0.)) ;
#82550 = DIRECTION('center_axis',(0.,0.,1.)) ;
#82551 = DIRECTION('ref_axis',(1.,0.,0.)) ;
#82552 = DIRECTION('',(0.986393923832144,0.164398987305357,0.)) ;
#82553 = DIRECTION('center_axis',(0.,0.,1.)) ;
#82554 = DIRECTION('ref_axis',(1.,0.,0.)) ;
#82555 = DIRECTION('',(-1.73472347597681E-15,1.,0.)) ;
#82556 = DIRECTION('center_axis',(0.,0.,1.)) ;
#82557 = DIRECTION('ref_axis',(1.,0.,0.)) ;
#82558 = DIRECTION('center_axis',(-1.92747052886312E-16,1.,0.)) ;
#82559 = DIRECTION('ref_axis',(-1.,-1.92747052886312E-16,0.)) ;
#82560 = DIRECTION('',(0.,0.,1.)) ;
#82561 = DIRECTION('',(0.,0.,-1.)) ;
#82562 = DIRECTION('center_axis',(-1.,0.,0.)) ;
#82563 = DIRECTION('ref_axis',(0.,0.,1.)) ;
#82564 = DIRECTION('',(0.,0.,1.)) ;
#82565 = DIRECTION('',(0.,0.,-1.)) ;
#82566 = DIRECTION('center_axis',(0.,1.,0.)) ;
#82567 = DIRECTION('ref_axis',(0.,0.,1.)) ;
#82568 = DIRECTION('',(0.,0.,-1.)) ;
#82569 = DIRECTION('',(0.,0.,1.)) ;
#82570 = DIRECTION('',(0.,0.,-1.)) ;
#82571 = DIRECTION('',(0.,0.,-1.)) ;
#82572 = DIRECTION('center_axis',(0.316227766016838,0.948683298050514,0.)) ;
#82573 = DIRECTION('ref_axis',(-0.948683298050514,0.316227766016838,0.)) ;
#82574 = DIRECTION('center_axis',(-0.316227766016835,-0.948683298050515,3.34717459363351E-14)) ;
#82575 = DIRECTION('ref_axis',(0.831595960764329,-0.277198653588124,-0.481257794211568)) ;
#82576 = DIRECTION('',(0.,0.,1.)) ;
#82577 = DIRECTION('',(0.,0.,-1.)) ;
#82578 = DIRECTION('',(-0.937042571331636,0.312347523777212,-0.156173761888606)) ;
#82579 = DIRECTION('center_axis',(1.,1.73472347597681E-15,0.)) ;
#82580 = DIRECTION('ref_axis',(-1.73472347597681E-15,1.,0.)) ;
#82581 = DIRECTION('',(-1.73472347597681E-15,1.,-2.89120579329468E-16)) ;
#82582 = DIRECTION('',(0.,0.,1.)) ;
#82583 = DIRECTION('',(0.,0.,-1.)) ;
#82584 = DIRECTION('center_axis',(0.164398987305357,-0.986393923832144,0.)) ;
#82585 = DIRECTION('ref_axis',(0.986393923832144,0.164398987305357,0.)) ;
#82586 = DIRECTION('',(0.973328526784575,0.162221421130762,0.162221421130763)) ;
#82587 = DIRECTION('',(0.,0.,1.)) ;
#82588 = DIRECTION('',(0.,0.,-1.)) ;
#82589 = DIRECTION('center_axis',(0.,-1.,0.)) ;
#82590 = DIRECTION('ref_axis',(0.,0.,-1.)) ;
#82591 = DIRECTION('',(0.,0.,1.)) ;
#82592 = DIRECTION('',(0.,0.,1.)) ;
#82593 = DIRECTION('',(0.,0.,1.)) ;
#82594 = DIRECTION('',(0.,0.,-1.)) ;
#82595 = DIRECTION('',(1.,0.,2.25271179641597E-31)) ;
#82596 = DIRECTION('center_axis',(0.,-1.,0.)) ;
#82597 = DIRECTION('ref_axis',(0.,0.,-1.)) ;
#82598 = DIRECTION('',(0.,0.,-1.)) ;
#82599 = DIRECTION('center_axis',(0.,-1.,0.)) ;
#82600 = DIRECTION('ref_axis',(0.,0.,-1.)) ;
#82601 = DIRECTION('',(-1.,0.,-3.21815970916568E-32)) ;
#82602 = DIRECTION('',(0.,0.,-1.)) ;
#82603 = DIRECTION('center_axis',(1.,-3.46944695195361E-16,0.)) ;
#82604 = DIRECTION('ref_axis',(3.46944695195361E-16,1.,0.)) ;
#82605 = DIRECTION('center_axis',(1.,-3.46944695195361E-16,0.)) ;
#82606 = DIRECTION('ref_axis',(3.46944695195361E-16,1.,0.)) ;
#82607 = DIRECTION('',(1.5529910948782E-31,4.47619207437002E-16,-1.)) ;
#82608 = DIRECTION('',(0.,0.,1.)) ;
#82609 = DIRECTION('center_axis',(1.,-3.46944695195361E-16,0.)) ;
#82610 = DIRECTION('ref_axis',(3.46944695195361E-16,1.,0.)) ;
#82611 = DIRECTION('center_axis',(1.,-3.46944695195361E-16,0.)) ;
#82612 = DIRECTION('ref_axis',(3.46944695195361E-16,1.,0.)) ;
#82613 = DIRECTION('center_axis',(1.,-3.46944695195361E-16,0.)) ;
#82614 = DIRECTION('ref_axis',(3.46944695195361E-16,1.,0.)) ;
#82615 = DIRECTION('',(3.46944695195361E-16,1.,9.27571383489107E-17)) ;
#82616 = DIRECTION('',(0.,0.,1.)) ;
#82617 = DIRECTION('',(-3.46944695195361E-16,-1.,-6.49299968442375E-16)) ;
#82618 = DIRECTION('center_axis',(1.,-3.46944695195361E-16,0.)) ;
#82619 = DIRECTION('ref_axis',(3.46944695195361E-16,1.,0.)) ;
#82620 = DIRECTION('center_axis',(1.,-3.46944695195361E-16,0.)) ;
#82621 = DIRECTION('ref_axis',(3.46944695195361E-16,1.,0.)) ;
#82622 = DIRECTION('center_axis',(1.,-3.46944695195361E-16,0.)) ;
#82623 = DIRECTION('ref_axis',(3.46944695195361E-16,1.,0.)) ;
#82624 = DIRECTION('',(0.,0.,1.)) ;
#82625 = DIRECTION('',(-1.5529910948782E-31,-4.47619207437002E-16,-1.)) ;
#82626 = DIRECTION('center_axis',(1.,-3.46944695195361E-16,0.)) ;
#82627 = DIRECTION('ref_axis',(3.46944695195361E-16,1.,0.)) ;
#82628 = DIRECTION('center_axis',(1.,-3.46944695195361E-16,0.)) ;
#82629 = DIRECTION('ref_axis',(3.46944695195361E-16,1.,0.)) ;
#82630 = DIRECTION('center_axis',(1.,-3.46944695195361E-16,0.)) ;
#82631 = DIRECTION('ref_axis',(3.46944695195361E-16,1.,0.)) ;
#82632 = DIRECTION('',(-3.46944695195361E-16,-1.,-1.06487173641454E-15)) ;
#82633 = DIRECTION('center_axis',(1.,-3.46944695195361E-16,0.)) ;
#82634 = DIRECTION('ref_axis',(3.46944695195361E-16,1.,0.)) ;
#82635 = DIRECTION('',(3.46944695195361E-16,1.,2.45739631480277E-16)) ;
#82636 = DIRECTION('center_axis',(1.,-3.46944695195361E-16,0.)) ;
#82637 = DIRECTION('ref_axis',(3.46944695195361E-16,1.,0.)) ;
#82638 = DIRECTION('center_axis',(1.,-3.46944695195361E-16,0.)) ;
#82639 = DIRECTION('ref_axis',(3.46944695195361E-16,1.,0.)) ;
#82640 = DIRECTION('center_axis',(0.,-1.,0.)) ;
#82641 = DIRECTION('ref_axis',(0.,0.,-1.)) ;
#82642 = DIRECTION('center_axis',(0.,-1.,0.)) ;
#82643 = DIRECTION('ref_axis',(0.,0.,-1.)) ;
#82644 = DIRECTION('',(-1.,0.,-1.40488587213121E-32)) ;
#82645 = DIRECTION('',(0.,0.,1.)) ;
#82646 = DIRECTION('',(0.,0.,1.)) ;
#82647 = DIRECTION('',(0.,0.,1.)) ;
#82648 = DIRECTION('',(1.,0.,1.40488587213121E-32)) ;
#82649 = DIRECTION('center_axis',(0.,-1.,0.)) ;
#82650 = DIRECTION('ref_axis',(0.,0.,-1.)) ;
#82651 = DIRECTION('',(7.2280144832367E-17,0.,-1.)) ;
#82652 = DIRECTION('center_axis',(-1.,-1.13380619344889E-16,0.)) ;
#82653 = DIRECTION('ref_axis',(1.13380619344889E-16,-1.,0.)) ;
#82654 = DIRECTION('center_axis',(-1.,-1.13380619344889E-16,0.)) ;
#82655 = DIRECTION('ref_axis',(1.13380619344889E-16,-1.,0.)) ;
#82656 = DIRECTION('',(1.13380619344889E-16,-1.,1.23908819712629E-16)) ;
#82657 = DIRECTION('',(0.,0.,-1.)) ;
#82658 = DIRECTION('',(-1.13380619344889E-16,1.,-1.23908819712629E-16)) ;
#82659 = DIRECTION('center_axis',(-1.,-1.13380619344889E-16,0.)) ;
#82660 = DIRECTION('ref_axis',(1.13380619344889E-16,-1.,0.)) ;
#82661 = DIRECTION('',(0.,0.,1.)) ;
#82662 = DIRECTION('center_axis',(-1.40488587213121E-32,1.23908819712629E-16,
1.)) ;
#82663 = DIRECTION('ref_axis',(0.,-1.,1.23908819712629E-16)) ;
#82664 = DIRECTION('',(-1.,0.,-1.40488587213121E-32)) ;
#82665 = DIRECTION('',(-1.13380619344889E-16,1.,-1.23908819712629E-16)) ;
#82666 = DIRECTION('center_axis',(1.40488587213121E-32,-1.23908819712629E-16,
-1.)) ;
#82667 = DIRECTION('ref_axis',(-1.74077750246726E-48,-1.,1.23908819712629E-16)) ;
#82668 = DIRECTION('center_axis',(1.40488587213121E-32,-1.23908819712629E-16,
-1.)) ;
#82669 = DIRECTION('ref_axis',(0.,1.,-1.23908819712629E-16)) ;
#82670 = DIRECTION('center_axis',(-1.40488587213121E-32,1.23908819712629E-16,
1.)) ;
#82671 = DIRECTION('ref_axis',(1.74077750246726E-48,1.,-1.23908819712629E-16)) ;
#82672 = DIRECTION('',(1.13380619344889E-16,-1.,1.23908819712629E-16)) ;
#82673 = DIRECTION('',(1.,0.,1.40488587213121E-32)) ;
#82674 = DIRECTION('center_axis',(-1.,-1.23908819712629E-16,-8.95614743483648E-33)) ;
#82675 = DIRECTION('ref_axis',(1.23908819712629E-16,-1.,5.38566640001825E-66)) ;
#82676 = DIRECTION('',(-8.95614743483648E-33,-1.10974565782288E-48,1.)) ;
#82677 = DIRECTION('',(1.23908819712629E-16,-1.,7.2280144832367E-17)) ;
#82678 = DIRECTION('',(-8.95614743483648E-33,0.,1.)) ;
#82679 = DIRECTION('',(-1.23908819712629E-16,1.,-1.23908819712629E-16)) ;
#82680 = DIRECTION('',(8.95614743483648E-33,1.0154535431059E-48,-1.)) ;
#82681 = DIRECTION('',(1.23908819712629E-16,-1.,1.23908819712629E-16)) ;
#82682 = DIRECTION('',(-8.95614743483648E-33,0.,1.)) ;
#82683 = DIRECTION('',(-1.23908819712629E-16,1.,2.4093381610789E-16)) ;
#82684 = DIRECTION('center_axis',(-1.7912294869673E-32,7.2280144832367E-17,
1.)) ;
#82685 = DIRECTION('ref_axis',(0.,-1.,7.2280144832367E-17)) ;
#82686 = DIRECTION('',(-1.23908819712629E-16,1.,-7.2280144832367E-17)) ;
#82687 = DIRECTION('',(1.,1.23908819712629E-16,8.95614743483648E-33)) ;
#82688 = DIRECTION('',(1.44560289664734E-16,-1.,7.2280144832367E-17)) ;
#82689 = DIRECTION('',(-1.,0.,-1.7912294869673E-32)) ;
#82690 = DIRECTION('center_axis',(-2.08976773479518E-32,2.4093381610789E-16,
-1.)) ;
#82691 = DIRECTION('ref_axis',(0.,1.,2.4093381610789E-16)) ;
#82692 = DIRECTION('',(-1.44560289664734E-16,1.,2.4093381610789E-16)) ;
#82693 = DIRECTION('',(-1.,-1.23908819712629E-16,-8.95614743483648E-33)) ;
#82694 = DIRECTION('',(1.23908819712629E-16,-1.,-2.4093381610789E-16)) ;
#82695 = DIRECTION('',(1.,0.,-2.08976773479518E-32)) ;
#82696 = DIRECTION('center_axis',(-1.23908819712629E-16,1.,0.)) ;
#82697 = DIRECTION('ref_axis',(-1.,-1.23908819712629E-16,0.)) ;
#82698 = DIRECTION('',(8.95614743483648E-33,1.10974565782288E-48,-1.)) ;
#82699 = DIRECTION('',(1.,1.23908819712629E-16,8.95614743483648E-33)) ;
#82700 = DIRECTION('',(-2.65552944032596E-32,-3.29043518662928E-48,1.)) ;
#82701 = DIRECTION('',(-1.,-1.23908819712629E-16,-8.95614743483648E-33)) ;
#82702 = DIRECTION('center_axis',(-1.,-1.44560289664734E-16,-2.65552944032596E-32)) ;
#82703 = DIRECTION('ref_axis',(1.44560289664734E-16,-1.,-2.80018320648271E-64)) ;
#82704 = DIRECTION('',(1.44560289664734E-16,-1.,-2.4093381610789E-16)) ;
#82705 = DIRECTION('',(-2.65552944032596E-32,0.,1.)) ;
#82706 = DIRECTION('',(-1.44560289664734E-16,1.,-7.2280144832367E-17)) ;
#82707 = DIRECTION('',(0.,0.,-1.)) ;
#82708 = DIRECTION('center_axis',(0.,1.,0.)) ;
#82709 = DIRECTION('ref_axis',(0.,0.,1.)) ;
#82710 = DIRECTION('',(8.95614743483648E-33,0.,-1.)) ;
#82711 = DIRECTION('',(1.,0.,1.40488587213121E-32)) ;
#82712 = DIRECTION('',(-7.2280144832367E-17,0.,1.)) ;
#82713 = DIRECTION('',(-1.,0.,-1.40488587213121E-32)) ;
#82714 = DIRECTION('',(8.95614743483648E-33,0.,-1.)) ;
#82715 = DIRECTION('',(1.,0.,1.7912294869673E-32)) ;
#82716 = DIRECTION('',(2.65552944032596E-32,0.,-1.)) ;
#82717 = DIRECTION('',(-1.,0.,2.08976773479518E-32)) ;
#82718 = DIRECTION('center_axis',(1.,1.44560289664734E-16,0.)) ;
#82719 = DIRECTION('ref_axis',(-1.44560289664734E-16,1.,0.)) ;
#82720 = DIRECTION('',(1.44560289664734E-16,-1.,0.)) ;
#82721 = DIRECTION('center_axis',(-1.,-1.44560289664734E-16,0.)) ;
#82722 = DIRECTION('ref_axis',(-1.44560289664734E-16,1.,0.)) ;
#82723 = DIRECTION('',(0.,0.,-1.)) ;
#82724 = DIRECTION('center_axis',(-1.,-1.44560289664734E-16,0.)) ;
#82725 = DIRECTION('ref_axis',(-1.44560289664734E-16,1.,0.)) ;
#82726 = DIRECTION('',(1.44560289664734E-16,-1.,0.)) ;
#82727 = DIRECTION('center_axis',(-1.,-1.44560289664734E-16,0.)) ;
#82728 = DIRECTION('ref_axis',(-1.44560289664734E-16,1.,0.)) ;
#82729 = DIRECTION('',(0.,0.,1.)) ;
#82730 = DIRECTION('center_axis',(-1.,-1.44560289664734E-16,0.)) ;
#82731 = DIRECTION('ref_axis',(-1.44560289664734E-16,1.,0.)) ;
#82732 = DIRECTION('center_axis',(1.,-3.46944695195361E-16,0.)) ;
#82733 = DIRECTION('ref_axis',(3.46944695195361E-16,1.,0.)) ;
#82734 = DIRECTION('center_axis',(1.,-3.46944695195361E-16,0.)) ;
#82735 = DIRECTION('ref_axis',(3.46944695195361E-16,1.,0.)) ;
#82736 = DIRECTION('',(0.,0.,-1.)) ;
#82737 = DIRECTION('',(-1.5529910948782E-31,-4.47619207437002E-16,1.)) ;
#82738 = DIRECTION('center_axis',(-1.,3.46944695195361E-16,0.)) ;
#82739 = DIRECTION('ref_axis',(3.46944695195361E-16,1.,0.)) ;
#82740 = DIRECTION('',(-3.46944695195361E-16,-1.,-2.45739631480277E-16)) ;
#82741 = DIRECTION('center_axis',(1.,-3.46944695195361E-16,0.)) ;
#82742 = DIRECTION('ref_axis',(3.46944695195361E-16,1.,0.)) ;
#82743 = DIRECTION('center_axis',(3.46944695195361E-16,1.,4.47619207437002E-16)) ;
#82744 = DIRECTION('ref_axis',(-8.18685017503995E-48,-4.47619207437002E-16,
1.)) ;
#82745 = DIRECTION('',(-1.5529910948782E-31,-4.47619207437002E-16,1.)) ;
#82746 = DIRECTION('',(-1.,3.46944695195361E-16,0.)) ;
#82747 = DIRECTION('',(1.5529910948782E-31,4.47619207437002E-16,-1.)) ;
#82748 = DIRECTION('center_axis',(-8.52580615413453E-32,-2.45739631480277E-16,
1.)) ;
#82749 = DIRECTION('ref_axis',(0.,-1.,-2.45739631480277E-16)) ;
#82750 = DIRECTION('',(1.,-3.46944695195361E-16,0.)) ;
#82751 = DIRECTION('',(-3.46944695195361E-16,-1.,-2.45739631480277E-16)) ;
#82752 = DIRECTION('',(3.46944695195361E-16,1.,2.45739631480277E-16)) ;
#82753 = DIRECTION('center_axis',(1.,-3.46944695195361E-16,0.)) ;
#82754 = DIRECTION('ref_axis',(3.46944695195361E-16,1.,0.)) ;
#82755 = DIRECTION('center_axis',(1.,-3.46944695195361E-16,0.)) ;
#82756 = DIRECTION('ref_axis',(3.46944695195361E-16,1.,0.)) ;
#82757 = DIRECTION('',(1.,-3.46944695195361E-16,0.)) ;
#82758 = DIRECTION('center_axis',(-1.,3.46944695195361E-16,0.)) ;
#82759 = DIRECTION('ref_axis',(3.46944695195361E-16,1.,0.)) ;
#82760 = DIRECTION('',(-1.,3.46944695195361E-16,0.)) ;
#82761 = DIRECTION('center_axis',(1.,-3.46944695195361E-16,0.)) ;
#82762 = DIRECTION('ref_axis',(3.46944695195361E-16,1.,0.)) ;
#82763 = DIRECTION('center_axis',(1.,-3.46944695195361E-16,0.)) ;
#82764 = DIRECTION('ref_axis',(-3.46944695195361E-16,-1.,-9.91270557701033E-16)) ;
#82765 = DIRECTION('',(1.,-3.46944695195361E-16,0.)) ;
#82766 = DIRECTION('center_axis',(-1.,3.46944695195361E-16,0.)) ;
#82767 = DIRECTION('ref_axis',(3.46944695195361E-16,1.,-1.98254111540207E-15)) ;
#82768 = DIRECTION('',(-1.,3.46944695195361E-16,0.)) ;
#82769 = DIRECTION('center_axis',(3.69451600012496E-31,1.06487173641454E-15,
-1.)) ;
#82770 = DIRECTION('ref_axis',(0.,1.,1.06487173641454E-15)) ;
#82771 = DIRECTION('',(3.46944695195361E-16,1.,1.06487173641454E-15)) ;
#82772 = DIRECTION('',(-1.,3.46944695195361E-16,0.)) ;
#82773 = DIRECTION('',(-3.46944695195361E-16,-1.,-1.06487173641454E-15)) ;
#82774 = DIRECTION('center_axis',(3.46944695195361E-16,1.,-4.47619207437002E-16)) ;
#82775 = DIRECTION('ref_axis',(8.18685017503995E-48,4.47619207437002E-16,
1.)) ;
#82776 = DIRECTION('',(1.,-3.46944695195361E-16,0.)) ;
#82777 = DIRECTION('',(1.5529910948782E-31,4.47619207437002E-16,1.)) ;
#82778 = DIRECTION('',(-1.5529910948782E-31,-4.47619207437002E-16,-1.)) ;
#82779 = DIRECTION('center_axis',(-1.,3.46944695195361E-16,0.)) ;
#82780 = DIRECTION('ref_axis',(-3.46944695195361E-16,-1.,0.)) ;
#82781 = DIRECTION('center_axis',(-1.,3.46944695195361E-16,0.)) ;
#82782 = DIRECTION('ref_axis',(-3.46944695195361E-16,-1.,0.)) ;
#82783 = DIRECTION('',(1.5529910948782E-31,4.47619207437002E-16,1.)) ;
#82784 = DIRECTION('',(0.,0.,-1.)) ;
#82785 = DIRECTION('center_axis',(1.,-3.46944695195361E-16,0.)) ;
#82786 = DIRECTION('ref_axis',(-3.46944695195361E-16,-1.,0.)) ;
#82787 = DIRECTION('center_axis',(1.,-3.46944695195361E-16,0.)) ;
#82788 = DIRECTION('ref_axis',(-3.46944695195361E-16,-1.,0.)) ;
#82789 = DIRECTION('',(3.46944695195361E-16,1.,1.06487173641454E-15)) ;
#82790 = DIRECTION('center_axis',(1.,-3.46944695195361E-16,0.)) ;
#82791 = DIRECTION('ref_axis',(3.46944695195361E-16,1.,0.)) ;
#82792 = DIRECTION('center_axis',(-1.,3.46944695195361E-16,0.)) ;
#82793 = DIRECTION('ref_axis',(3.46944695195361E-16,1.,0.)) ;
#82794 = DIRECTION('',(0.,0.,-1.)) ;
#82795 = DIRECTION('',(0.,0.,1.)) ;
#82796 = DIRECTION('',(-3.46944695195361E-16,-1.,-9.27571383489107E-17)) ;
#82797 = DIRECTION('center_axis',(-3.46944695195361E-16,-1.,0.)) ;
#82798 = DIRECTION('ref_axis',(1.,-3.46944695195361E-16,0.)) ;
#82799 = DIRECTION('',(1.,-3.46944695195361E-16,0.)) ;
#82800 = DIRECTION('',(0.,0.,-1.)) ;
#82801 = DIRECTION('',(0.,0.,1.)) ;
#82802 = DIRECTION('center_axis',(1.,-3.46944695195361E-16,0.)) ;
#82803 = DIRECTION('ref_axis',(3.46944695195361E-16,1.,0.)) ;
#82804 = DIRECTION('center_axis',(1.,-3.46944695195361E-16,0.)) ;
#82805 = DIRECTION('ref_axis',(3.46944695195361E-16,1.,0.)) ;
#82806 = DIRECTION('',(1.,-3.46944695195361E-16,0.)) ;
#82807 = DIRECTION('center_axis',(-1.,3.46944695195361E-16,0.)) ;
#82808 = DIRECTION('ref_axis',(3.46944695195361E-16,1.,-9.91270557701033E-16)) ;
#82809 = DIRECTION('',(-1.,3.46944695195361E-16,0.)) ;
#82810 = DIRECTION('center_axis',(-3.21815970916568E-32,-9.27571383489107E-17,
1.)) ;
#82811 = DIRECTION('ref_axis',(0.,-1.,-9.27571383489107E-17)) ;
#82812 = DIRECTION('',(3.46944695195361E-16,1.,9.27571383489107E-17)) ;
#82813 = DIRECTION('',(1.,0.,3.21815970916568E-32)) ;
#82814 = DIRECTION('',(-3.46944695195361E-16,-1.,-9.27571383489107E-17)) ;
#82815 = DIRECTION('',(-1.,3.46944695195361E-16,0.)) ;
#82816 = DIRECTION('center_axis',(1.,-3.46944695195361E-16,0.)) ;
#82817 = DIRECTION('ref_axis',(3.46944695195361E-16,1.,0.)) ;
#82818 = DIRECTION('center_axis',(1.,-3.46944695195361E-16,0.)) ;
#82819 = DIRECTION('ref_axis',(-3.46944695195361E-16,-1.,4.95635278850516E-15)) ;
#82820 = DIRECTION('',(1.,-3.46944695195361E-16,0.)) ;
#82821 = DIRECTION('center_axis',(-1.,3.46944695195361E-16,0.)) ;
#82822 = DIRECTION('ref_axis',(3.46944695195361E-16,1.,2.9738116731031E-15)) ;
#82823 = DIRECTION('',(-1.,3.46944695195361E-16,0.)) ;
#82824 = DIRECTION('center_axis',(-3.46944695195361E-16,-1.,0.)) ;
#82825 = DIRECTION('ref_axis',(1.,-3.46944695195361E-16,0.)) ;
#82826 = DIRECTION('',(0.,0.,-1.)) ;
#82827 = DIRECTION('',(-1.,3.46944695195361E-16,0.)) ;
#82828 = DIRECTION('',(0.,0.,1.)) ;
#82829 = DIRECTION('center_axis',(2.25271179641597E-31,6.49299968442375E-16,
-1.)) ;
#82830 = DIRECTION('ref_axis',(0.,1.,6.49299968442375E-16)) ;
#82831 = DIRECTION('',(3.46944695195361E-16,1.,6.49299968442375E-16)) ;
#82832 = DIRECTION('',(-1.,0.,-2.25271179641597E-31)) ;
#82833 = DIRECTION('',(-3.46944695195361E-16,-1.,-6.49299968442375E-16)) ;
#82834 = DIRECTION('',(1.,-3.46944695195361E-16,0.)) ;
#82835 = DIRECTION('center_axis',(-1.,3.46944695195361E-16,0.)) ;
#82836 = DIRECTION('ref_axis',(-3.46944695195361E-16,-1.,0.)) ;
#82837 = DIRECTION('',(3.46944695195361E-16,1.,6.49299968442375E-16)) ;
#82838 = DIRECTION('',(0.,0.,1.)) ;
#82839 = DIRECTION('',(0.,0.,-1.)) ;
#82840 = DIRECTION('center_axis',(-1.,3.46944695195361E-16,0.)) ;
#82841 = DIRECTION('ref_axis',(-3.46944695195361E-16,-1.,0.)) ;
#82842 = DIRECTION('center_axis',(-0.164398987305357,0.,-0.986393923832144)) ;
#82843 = DIRECTION('ref_axis',(-0.986393923832144,0.,0.164398987305357)) ;
#82844 = DIRECTION('',(-0.937042571331636,0.312347523777212,0.156173761888606)) ;
#82845 = DIRECTION('',(0.,-1.,0.)) ;
#82846 = DIRECTION('',(0.973328526784575,0.162221421130762,-0.162221421130763)) ;
#82847 = DIRECTION('',(-1.73472347597681E-15,1.,2.89120579329468E-16)) ;
#82848 = DIRECTION('center_axis',(-1.,0.,0.)) ;
#82849 = DIRECTION('ref_axis',(0.,0.,1.)) ;
#82850 = DIRECTION('center_axis',(-1.,0.,0.)) ;
#82851 = DIRECTION('ref_axis',(0.,0.958782008217047,-0.284142676694803)) ;
#82852 = DIRECTION('',(0.,0.,1.)) ;
#82853 = DIRECTION('',(0.,-1.,0.)) ;
#82854 = DIRECTION('center_axis',(-1.,0.,0.)) ;
#82855 = DIRECTION('ref_axis',(0.,0.75870512941688,-0.651434207419687)) ;
#82856 = DIRECTION('',(0.,0.,-1.)) ;
#82857 = DIRECTION('center_axis',(-1.,0.,0.)) ;
#82858 = DIRECTION('ref_axis',(0.,-0.65477883641065,-0.755820531203483)) ;
#82859 = DIRECTION('',(0.,1.,0.)) ;
#82860 = DIRECTION('center_axis',(-0.164398987305357,0.,0.986393923832144)) ;
#82861 = DIRECTION('ref_axis',(0.986393923832144,0.,0.164398987305357)) ;
#82862 = DIRECTION('',(-0.973328526784575,-0.162221421130762,-0.162221421130763)) ;
#82863 = DIRECTION('',(0.,1.,0.)) ;
#82864 = DIRECTION('',(0.937042571331636,-0.312347523777212,0.156173761888606)) ;
#82865 = DIRECTION('',(1.73472347597681E-15,-1.,2.89120579329468E-16)) ;
#82866 = DIRECTION('center_axis',(-0.573462344363329,0.81923192051904,0.)) ;
#82867 = DIRECTION('ref_axis',(-0.81923192051904,-0.573462344363329,0.)) ;
#82868 = DIRECTION('',(-0.710669054518702,-0.497468338163091,0.49746833816309)) ;
#82869 = DIRECTION('',(0.,0.,-1.)) ;
#82870 = DIRECTION('',(0.710669054518702,0.497468338163091,0.49746833816309)) ;
#82871 = DIRECTION('',(0.,0.,1.)) ;
#82872 = DIRECTION('center_axis',(-1.,0.,0.)) ;
#82873 = DIRECTION('ref_axis',(0.,0.,1.)) ;
#82874 = DIRECTION('',(0.,0.,1.)) ;
#82875 = DIRECTION('',(0.,-1.,-9.34081871679819E-17)) ;
#82876 = DIRECTION('',(0.,0.,-1.)) ;
#82877 = DIRECTION('',(0.,1.,-9.34081871679819E-17)) ;
#82878 = DIRECTION('center_axis',(-0.573462344363329,-0.81923192051904,0.)) ;
#82879 = DIRECTION('ref_axis',(0.81923192051904,-0.573462344363329,0.)) ;
#82880 = DIRECTION('',(-0.710669054518701,0.497468338163091,-0.497468338163091)) ;
#82881 = DIRECTION('',(0.,0.,1.)) ;
#82882 = DIRECTION('',(0.710669054518701,-0.497468338163091,-0.497468338163091)) ;
#82883 = DIRECTION('',(0.,0.,-1.)) ;
#82884 = DIRECTION('center_axis',(0.,0.,1.)) ;
#82885 = DIRECTION('ref_axis',(1.,0.,0.)) ;
#82886 = DIRECTION('',(1.,6.67201336914158E-17,0.)) ;
#82887 = DIRECTION('',(1.33440267382831E-16,1.,0.)) ;
#82888 = DIRECTION('',(-1.,1.33440267382831E-16,0.)) ;
#82889 = DIRECTION('center_axis',(0.,0.,1.)) ;
#82890 = DIRECTION('ref_axis',(1.,0.,0.)) ;
#82891 = DIRECTION('',(1.,-1.33440267382831E-16,0.)) ;
#82892 = DIRECTION('',(-1.33440267382831E-16,-1.,0.)) ;
#82893 = DIRECTION('',(-1.,-6.67201336914158E-17,0.)) ;
#82894 = DIRECTION('center_axis',(-6.67201336914158E-17,1.,0.)) ;
#82895 = DIRECTION('ref_axis',(-1.,-6.67201336914158E-17,0.)) ;
#82896 = DIRECTION('',(1.,6.67201336914158E-17,0.)) ;
#82897 = DIRECTION('',(0.,0.,1.)) ;
#82898 = DIRECTION('',(-1.,-6.67201336914158E-17,0.)) ;
#82899 = DIRECTION('center_axis',(-1.33440267382831E-16,-1.,0.)) ;
#82900 = DIRECTION('ref_axis',(1.,-1.33440267382831E-16,0.)) ;
#82901 = DIRECTION('',(1.,-1.33440267382831E-16,0.)) ;
#82902 = DIRECTION('',(0.,0.,-1.)) ;
#82903 = DIRECTION('',(-1.,1.33440267382831E-16,0.)) ;
#82904 = DIRECTION('center_axis',(0.,0.,1.)) ;
#82905 = DIRECTION('ref_axis',(1.,0.,0.)) ;
#82906 = DIRECTION('',(0.,-1.,0.)) ;
#82907 = DIRECTION('',(1.,0.,0.)) ;
#82908 = DIRECTION('',(0.,1.,0.)) ;
#82909 = DIRECTION('center_axis',(0.,0.,-1.)) ;
#82910 = DIRECTION('ref_axis',(1.,0.,0.)) ;
#82911 = DIRECTION('',(-1.44560289664734E-16,1.,-7.2280144832367E-17)) ;
#82912 = DIRECTION('center_axis',(0.,0.,1.)) ;
#82913 = DIRECTION('ref_axis',(1.,0.,0.)) ;
#82914 = DIRECTION('center_axis',(0.,0.,1.)) ;
#82915 = DIRECTION('ref_axis',(1.,0.,0.)) ;
#82916 = DIRECTION('',(0.,-1.,0.)) ;
#82917 = DIRECTION('',(-1.,0.,0.)) ;
#82918 = DIRECTION('',(0.,1.,0.)) ;
#82919 = DIRECTION('center_axis',(0.,0.,-1.)) ;
#82920 = DIRECTION('ref_axis',(1.,-1.82602471155453E-15,0.)) ;
#82921 = DIRECTION('',(1.44560289664734E-16,-1.,-2.4093381610789E-16)) ;
#82922 = DIRECTION('center_axis',(0.,0.,1.)) ;
#82923 = DIRECTION('ref_axis',(1.,0.,0.)) ;
#82924 = DIRECTION('center_axis',(0.,0.,-1.)) ;
#82925 = DIRECTION('ref_axis',(-1.,0.,0.)) ;
#82926 = DIRECTION('',(0.,0.,-1.)) ;
#82927 = DIRECTION('center_axis',(0.,0.,-1.)) ;
#82928 = DIRECTION('ref_axis',(1.,0.,0.)) ;
#82929 = DIRECTION('center_axis',(0.,0.,1.)) ;
#82930 = DIRECTION('ref_axis',(1.,0.,0.)) ;
#82931 = DIRECTION('center_axis',(1.,0.,0.)) ;
#82932 = DIRECTION('ref_axis',(0.,0.,-1.)) ;
#82933 = DIRECTION('',(0.,-1.,0.)) ;
#82934 = DIRECTION('',(0.,0.,1.)) ;
#82935 = DIRECTION('',(0.,1.,0.)) ;
#82936 = DIRECTION('center_axis',(0.81923192051904,0.573462344363329,0.)) ;
#82937 = DIRECTION('ref_axis',(-0.573462344363329,0.81923192051904,0.)) ;
#82938 = DIRECTION('',(-0.497468338163091,0.710669054518701,0.497468338163091)) ;
#82939 = DIRECTION('',(0.,0.,-1.)) ;
#82940 = DIRECTION('',(0.497468338163091,-0.710669054518701,0.497468338163091)) ;
#82941 = DIRECTION('',(0.,0.,1.)) ;
#82942 = DIRECTION('center_axis',(0.,1.,0.)) ;
#82943 = DIRECTION('ref_axis',(0.,0.,1.)) ;
#82944 = DIRECTION('',(0.,0.,1.)) ;
#82945 = DIRECTION('',(-1.,0.,0.)) ;
#82946 = DIRECTION('',(0.,0.,-1.)) ;
#82947 = DIRECTION('',(1.,0.,0.)) ;
#82948 = DIRECTION('center_axis',(-0.81923192051904,0.573462344363329,0.)) ;
#82949 = DIRECTION('ref_axis',(-0.573462344363329,-0.81923192051904,0.)) ;
#82950 = DIRECTION('',(0.497468338163091,0.710669054518701,-0.497468338163091)) ;
#82951 = DIRECTION('',(0.,0.,1.)) ;
#82952 = DIRECTION('',(-0.497468338163091,-0.710669054518701,-0.497468338163091)) ;
#82953 = DIRECTION('',(0.,0.,-1.)) ;
#82954 = DIRECTION('center_axis',(-1.,0.,0.)) ;
#82955 = DIRECTION('ref_axis',(0.,0.,1.)) ;
#82956 = DIRECTION('',(0.,-1.,0.)) ;
#82957 = DIRECTION('',(0.,0.,-1.)) ;
#82958 = DIRECTION('',(0.,1.,0.)) ;
#82959 = DIRECTION('',(0.,0.,-1.)) ;
#82960 = DIRECTION('center_axis',(0.,0.,-1.)) ;
#82961 = DIRECTION('ref_axis',(-1.,0.,0.)) ;
#82962 = DIRECTION('center_axis',(0.,0.,1.)) ;
#82963 = DIRECTION('ref_axis',(1.,0.,0.)) ;
#82964 = DIRECTION('center_axis',(0.,0.,-1.)) ;
#82965 = DIRECTION('ref_axis',(1.,5.20417042793042E-15,0.)) ;
#82966 = DIRECTION('center_axis',(-0.573462344363328,7.65229685658278E-17,
0.819231920519041)) ;
#82967 = DIRECTION('ref_axis',(0.819231920519041,1.22423955297878E-32,0.573462344363328)) ;
#82968 = DIRECTION('',(-0.710669054518702,-0.497468338163091,-0.497468338163091)) ;
#82969 = DIRECTION('',(1.33440267382831E-16,1.,-2.91413396387194E-34)) ;
#82970 = DIRECTION('',(0.710669054518701,-0.497468338163091,0.497468338163091)) ;
#82971 = DIRECTION('',(5.04890651880155E-33,-1.,9.34081871679819E-17)) ;
#82972 = DIRECTION('center_axis',(-0.573462344363328,7.65229685658278E-17,
-0.819231920519041)) ;
#82973 = DIRECTION('ref_axis',(-0.819231920519041,-1.22423955297878E-32,0.573462344363328)) ;
#82974 = DIRECTION('',(-0.710669054518701,0.497468338163091,0.497468338163091)) ;
#82975 = DIRECTION('',(-1.33440267382831E-16,-1.,7.77328292223541E-33)) ;
#82976 = DIRECTION('',(0.710669054518702,0.497468338163091,-0.497468338163091)) ;
#82977 = DIRECTION('',(-5.04890651880155E-33,1.,9.34081871679819E-17)) ;
#82978 = DIRECTION('center_axis',(0.,0.573462344363328,-0.819231920519041)) ;
#82979 = DIRECTION('ref_axis',(0.,0.819231920519041,0.573462344363328)) ;
#82980 = DIRECTION('',(0.497468338163091,0.710669054518701,0.497468338163091)) ;
#82981 = DIRECTION('',(-1.,0.,0.)) ;
#82982 = DIRECTION('',(0.497468338163091,-0.710669054518701,-0.497468338163091)) ;
#82983 = DIRECTION('',(1.,0.,0.)) ;
#82984 = DIRECTION('center_axis',(0.,0.573462344363328,0.819231920519041)) ;
#82985 = DIRECTION('ref_axis',(0.,-0.819231920519041,0.573462344363328)) ;
#82986 = DIRECTION('',(-0.497468338163091,0.710669054518701,-0.497468338163091)) ;
#82987 = DIRECTION('',(1.,0.,0.)) ;
#82988 = DIRECTION('',(-0.497468338163091,-0.710669054518701,0.497468338163091)) ;
#82989 = DIRECTION('',(-1.,0.,0.)) ;
#82990 = DIRECTION('center_axis',(-0.164398987305354,-0.986393923832144,0.)) ;
#82991 = DIRECTION('ref_axis',(0.,0.,1.)) ;
#82992 = DIRECTION('',(0.,0.,-1.)) ;
#82993 = DIRECTION('center_axis',(-0.164398987305377,-0.98639392383214,4.33975683157178E-13)) ;
#82994 = DIRECTION('ref_axis',(-0.0577290357386321,0.00962150595687908,0.998285923498779)) ;
#82995 = DIRECTION('',(0.,0.,1.)) ;
#82996 = DIRECTION('center_axis',(1.,-2.89120579329441E-16,0.)) ;
#82997 = DIRECTION('ref_axis',(-2.89120579329441E-16,-1.,-1.20980294963545E-15)) ;
#82998 = DIRECTION('center_axis',(1.,1.15648231731787E-15,0.)) ;
#82999 = DIRECTION('ref_axis',(1.15648231731787E-15,-1.,0.)) ;
#83000 = DIRECTION('center_axis',(0.166689823582857,0.983956802812107,0.0635886225176511)) ;
#83001 = DIRECTION('ref_axis',(-0.0486480009802627,0.0726194159291099,-0.996172571611334)) ;
#83002 = DIRECTION('center_axis',(0.166689823544614,0.983956802870497,-0.0635886217143894)) ;
#83003 = DIRECTION('ref_axis',(-0.0462047035092779,0.0722149187712735,0.996318287938387)) ;
#83004 = DIRECTION('center_axis',(-0.164398987305354,-0.986393923832144,0.)) ;
#83005 = DIRECTION('ref_axis',(0.,0.,1.)) ;
#83006 = DIRECTION('',(0.,0.,1.)) ;
#83007 = DIRECTION('center_axis',(-0.164398987305428,-0.986393923832132,-1.30192704752217E-12)) ;
#83008 = DIRECTION('ref_axis',(-0.0554192327865001,0.0092365387990719,-0.998420450005091)) ;
#83009 = DIRECTION('',(0.,0.,-1.)) ;
#83010 = DIRECTION('center_axis',(0.,0.,1.)) ;
#83011 = DIRECTION('ref_axis',(1.,0.,0.)) ;
#83012 = DIRECTION('center_axis',(0.,0.,1.)) ;
#83013 = DIRECTION('ref_axis',(1.,0.,0.)) ;
#83014 = DIRECTION('center_axis',(0.,1.,0.)) ;
#83015 = DIRECTION('ref_axis',(1.,0.,0.)) ;
#83016 = DIRECTION('center_axis',(0.,-0.888198741900269,0.45945945945946)) ;
#83017 = DIRECTION('ref_axis',(0.,0.45945945945946,0.888198741900269)) ;
#83018 = DIRECTION('center_axis',(-1.,0.,1.22067519501986E-15)) ;
#83019 = DIRECTION('ref_axis',(-1.22067519501986E-15,0.,-1.)) ;
#83020 = DIRECTION('center_axis',(0.,0.,1.)) ;
#83021 = DIRECTION('ref_axis',(1.,0.,0.)) ;
#83022 = DIRECTION('center_axis',(0.,0.,-1.)) ;
#83023 = DIRECTION('ref_axis',(-1.,0.,0.)) ;
#83024 = DIRECTION('center_axis',(1.,-3.46944695195361E-16,0.)) ;
#83025 = DIRECTION('ref_axis',(3.46944695195361E-16,1.,0.)) ;
#83026 = DIRECTION('center_axis',(-1.,3.46944695195361E-16,0.)) ;
#83027 = DIRECTION('ref_axis',(3.46944695195361E-16,1.,0.)) ;
#83028 = DIRECTION('center_axis',(-1.,3.46944695195361E-16,0.)) ;
#83029 = DIRECTION('ref_axis',(-3.41607084500048E-16,-1.,0.)) ;
#83030 = DIRECTION('center_axis',(0.,-0.459459459459457,0.888198741900271)) ;
#83031 = DIRECTION('ref_axis',(0.,-0.888198741900271,-0.459459459459457)) ;
#83032 = DIRECTION('center_axis',(1.,-3.46944695195361E-16,0.)) ;
#83033 = DIRECTION('ref_axis',(0.,1.,0.)) ;
#83034 = DIRECTION('center_axis',(0.,0.888198741900269,-0.45945945945946)) ;
#83035 = DIRECTION('ref_axis',(0.,-0.45945945945946,-0.888198741900269)) ;
#83036 = DIRECTION('center_axis',(0.,1.,0.)) ;
#83037 = DIRECTION('ref_axis',(1.,0.,0.)) ;
#83038 = DIRECTION('center_axis',(0.,-1.,0.)) ;
#83039 = DIRECTION('ref_axis',(0.,0.,1.)) ;
#83040 = DIRECTION('center_axis',(-1.,0.,0.)) ;
#83041 = DIRECTION('ref_axis',(0.,0.,-1.)) ;
#83042 = DIRECTION('center_axis',(0.,0.,-1.)) ;
#83043 = DIRECTION('ref_axis',(-1.,0.,0.)) ;
#83044 = DIRECTION('center_axis',(0.,0.,-1.)) ;
#83045 = DIRECTION('ref_axis',(-1.,0.,0.)) ;
#83046 = DIRECTION('center_axis',(1.,-3.46944695195361E-16,0.)) ;
#83047 = DIRECTION('ref_axis',(3.46944695195361E-16,1.,0.)) ;
#83048 = DIRECTION('center_axis',(-1.,3.46944695195361E-16,0.)) ;
#83049 = DIRECTION('ref_axis',(3.46944695195361E-16,1.,0.)) ;
#83050 = DIRECTION('center_axis',(1.,0.,0.)) ;
#83051 = DIRECTION('ref_axis',(0.,0.,-1.)) ;
#83052 = DIRECTION('center_axis',(0.,0.,1.)) ;
#83053 = DIRECTION('ref_axis',(1.,0.,0.)) ;
#83054 = DIRECTION('center_axis',(0.,0.,1.)) ;
#83055 = DIRECTION('ref_axis',(1.,0.,0.)) ;
#83056 = DIRECTION('center_axis',(1.,-3.46944695195361E-16,0.)) ;
#83057 = DIRECTION('ref_axis',(3.80647894157197E-16,1.,0.)) ;
#83058 = DIRECTION('center_axis',(0.,0.459459459459459,-0.888198741900269)) ;
#83059 = DIRECTION('ref_axis',(0.,0.888198741900269,0.459459459459459)) ;
#83060 = DIRECTION('center_axis',(1.,-3.46944695195361E-16,0.)) ;
#83061 = DIRECTION('ref_axis',(3.46944695195361E-16,1.,0.)) ;
#83062 = DIRECTION('center_axis',(-1.,3.46944695195361E-16,0.)) ;
#83063 = DIRECTION('ref_axis',(3.46944695195361E-16,1.,0.)) ;
#83064 = DIRECTION('center_axis',(-3.46944695195361E-16,-1.,-6.49299968442375E-16)) ;
#83065 = DIRECTION('ref_axis',(2.25271179641597E-31,6.49299968442375E-16,
-1.)) ;
#83066 = DIRECTION('center_axis',(0.,-1.,0.)) ;
#83067 = DIRECTION('ref_axis',(0.,0.,-1.)) ;
#83068 = DIRECTION('center_axis',(0.,0.,1.)) ;
#83069 = DIRECTION('ref_axis',(1.,0.,0.)) ;
#83070 = DIRECTION('center_axis',(-3.25260651745651E-15,0.,1.)) ;
#83071 = DIRECTION('ref_axis',(1.,0.,3.25260651745651E-15)) ;
#83072 = DIRECTION('center_axis',(0.,1.,0.)) ;
#83073 = DIRECTION('ref_axis',(1.,0.,0.)) ;
#83074 = DIRECTION('center_axis',(0.,-0.888198741900269,-0.45945945945946)) ;
#83075 = DIRECTION('ref_axis',(0.,-0.45945945945946,0.888198741900269)) ;
#83076 = DIRECTION('center_axis',(1.,-3.46944695195361E-16,0.)) ;
#83077 = DIRECTION('ref_axis',(0.,1.,0.)) ;
#83078 = DIRECTION('center_axis',(0.,0.888198741900269,0.45945945945946)) ;
#83079 = DIRECTION('ref_axis',(0.,0.45945945945946,-0.888198741900269)) ;
#83080 = DIRECTION('center_axis',(1.,-3.46944695195361E-16,0.)) ;
#83081 = DIRECTION('ref_axis',(0.,1.,0.)) ;
#83082 = DIRECTION('center_axis',(0.,1.,0.)) ;
#83083 = DIRECTION('ref_axis',(0.,0.,-1.)) ;
#83084 = DIRECTION('center_axis',(0.,1.,0.)) ;
#83085 = DIRECTION('ref_axis',(1.,0.,0.)) ;
#83086 = DIRECTION('center_axis',(-1.,0.,0.)) ;
#83087 = DIRECTION('ref_axis',(0.,0.,-1.)) ;
#83088 = DIRECTION('center_axis',(1.,-3.46944695195361E-16,0.)) ;
#83089 = DIRECTION('ref_axis',(3.41607084500048E-16,1.,0.)) ;
#83090 = DIRECTION('center_axis',(-9.62987005567165E-16,-0.459459459459459,
-0.88819874190027)) ;
#83091 = DIRECTION('ref_axis',(-7.31984232283282E-30,0.88819874190027,-0.459459459459459)) ;
#83092 = DIRECTION('center_axis',(1.,-3.46944695195361E-16,0.)) ;
#83093 = DIRECTION('ref_axis',(3.46944695195361E-16,1.,0.)) ;
#83094 = DIRECTION('center_axis',(-1.,3.46944695195361E-16,0.)) ;
#83095 = DIRECTION('ref_axis',(3.46944695195361E-16,1.,0.)) ;
#83096 = DIRECTION('center_axis',(1.,0.,0.)) ;
#83097 = DIRECTION('ref_axis',(0.,0.,-1.)) ;
#83098 = DIRECTION('center_axis',(1.,-3.46944695195361E-16,0.)) ;
#83099 = DIRECTION('ref_axis',(3.80647894157197E-16,1.,0.)) ;
#83100 = DIRECTION('center_axis',(0.,0.459459459459459,0.888198741900269)) ;
#83101 = DIRECTION('ref_axis',(0.,-0.888198741900269,0.459459459459459)) ;
#83102 = DIRECTION('center_axis',(-3.46944695195361E-16,-1.,-6.49299968442375E-16)) ;
#83103 = DIRECTION('ref_axis',(2.25271179641597E-31,6.49299968442375E-16,
-1.)) ;
#83104 = DIRECTION('center_axis',(0.,1.,0.)) ;
#83105 = DIRECTION('ref_axis',(0.,0.,-1.)) ;
#83106 = DIRECTION('center_axis',(1.,0.,2.25271179641597E-31)) ;
#83107 = DIRECTION('ref_axis',(2.25271179641597E-31,0.,-1.)) ;
#83108 = DIRECTION('center_axis',(-1.,0.,0.)) ;
#83109 = DIRECTION('ref_axis',(0.,0.,1.)) ;
#83110 = DIRECTION('center_axis',(0.,1.,0.)) ;
#83111 = DIRECTION('ref_axis',(1.,0.,0.)) ;
#83112 = DIRECTION('center_axis',(0.,-1.,0.)) ;
#83113 = DIRECTION('ref_axis',(-1.08420217248551E-15,0.,1.)) ;
#83114 = DIRECTION('center_axis',(1.,-3.46944695195361E-16,0.)) ;
#83115 = DIRECTION('ref_axis',(0.,1.,0.)) ;
#83116 = DIRECTION('center_axis',(0.,1.,0.)) ;
#83117 = DIRECTION('ref_axis',(0.,0.,-1.)) ;
#83118 = DIRECTION('center_axis',(0.,-1.,0.)) ;
#83119 = DIRECTION('ref_axis',(0.,0.,-1.)) ;
#83120 = DIRECTION('center_axis',(0.,0.,1.)) ;
#83121 = DIRECTION('ref_axis',(-1.,0.,0.)) ;
#83122 = DIRECTION('center_axis',(0.,0.,-1.)) ;
#83123 = DIRECTION('ref_axis',(-1.,0.,0.)) ;
#83124 = DIRECTION('center_axis',(0.,0.,-1.)) ;
#83125 = DIRECTION('ref_axis',(-1.,0.,0.)) ;
#83126 = DIRECTION('center_axis',(-3.46944695195361E-16,-1.,-9.27571383489107E-17)) ;
#83127 = DIRECTION('ref_axis',(1.,-3.46944695195361E-16,-3.21815970916568E-32)) ;
#83128 = DIRECTION('center_axis',(0.,-1.,0.)) ;
#83129 = DIRECTION('ref_axis',(0.,0.,-1.)) ;
#83130 = DIRECTION('center_axis',(3.46944695195361E-16,1.,9.27571383489107E-17)) ;
#83131 = DIRECTION('ref_axis',(-1.,3.46944695195361E-16,3.21815970916568E-32)) ;
#83132 = DIRECTION('center_axis',(0.,1.,0.)) ;
#83133 = DIRECTION('ref_axis',(0.,0.,-1.)) ;
#83134 = DIRECTION('center_axis',(0.,0.,-1.)) ;
#83135 = DIRECTION('ref_axis',(-1.,0.,0.)) ;
#83136 = DIRECTION('center_axis',(0.,0.,1.)) ;
#83137 = DIRECTION('ref_axis',(1.,0.,0.)) ;
#83138 = DIRECTION('center_axis',(0.,1.,0.)) ;
#83139 = DIRECTION('ref_axis',(1.,0.,0.)) ;
#83140 = DIRECTION('center_axis',(-1.,0.,1.0842021724855E-15)) ;
#83141 = DIRECTION('ref_axis',(-1.0842021724855E-15,0.,-1.)) ;
#83142 = DIRECTION('center_axis',(0.,-1.,0.)) ;
#83143 = DIRECTION('ref_axis',(0.,0.,-1.)) ;
#83144 = DIRECTION('center_axis',(1.,0.,0.)) ;
#83145 = DIRECTION('ref_axis',(0.,0.,1.)) ;
#83146 = DIRECTION('center_axis',(1.,0.,3.21815970916568E-32)) ;
#83147 = DIRECTION('ref_axis',(3.21815970916568E-32,0.,-1.)) ;
#83148 = DIRECTION('center_axis',(0.,1.,0.)) ;
#83149 = DIRECTION('ref_axis',(1.,0.,0.)) ;
#83150 = DIRECTION('center_axis',(0.,0.,-1.)) ;
#83151 = DIRECTION('ref_axis',(1.,0.,0.)) ;
#83152 = DIRECTION('center_axis',(1.,0.,0.)) ;
#83153 = DIRECTION('ref_axis',(0.,-1.08420217248551E-15,1.)) ;
#83154 = DIRECTION('center_axis',(1.0842021724855E-15,1.,0.)) ;
#83155 = DIRECTION('ref_axis',(1.,-1.0842021724855E-15,0.)) ;
#83156 = DIRECTION('center_axis',(1.,0.,-2.08976773479518E-32)) ;
#83157 = DIRECTION('ref_axis',(-2.08976773479518E-32,0.,-1.)) ;
#83158 = DIRECTION('center_axis',(-0.447220452189278,-7.10035983522275E-6,
-0.894423762594221)) ;
#83159 = DIRECTION('ref_axis',(0.894325663270205,0.0148067719276498,-0.4471715191304)) ;
#83160 = DIRECTION('center_axis',(-1.23908819712629E-16,1.,2.4093381610789E-16)) ;
#83161 = DIRECTION('ref_axis',(2.98538247827883E-32,-2.4093381610789E-16,
1.)) ;
#83162 = DIRECTION('center_axis',(-5.60223412787738E-6,-0.447219005480045,
-0.894424485971876)) ;
#83163 = DIRECTION('ref_axis',(0.0146917039260204,0.894327914920264,-0.447170811245684)) ;
#83164 = DIRECTION('center_axis',(-8.95614743483648E-33,0.,1.)) ;
#83165 = DIRECTION('ref_axis',(1.,0.,8.95614743483648E-33)) ;
#83166 = DIRECTION('center_axis',(1.40488587213121E-32,-1.23908819712629E-16,
-1.)) ;
#83167 = DIRECTION('ref_axis',(1.74077750246726E-48,1.,-1.23908819712629E-16)) ;
#83168 = DIRECTION('center_axis',(-2.65552944032596E-32,0.,1.)) ;
#83169 = DIRECTION('ref_axis',(1.,0.,2.65552944032596E-32)) ;
#83170 = DIRECTION('center_axis',(0.894424485971418,-5.60223478642178E-6,
0.447219005480961)) ;
#83171 = DIRECTION('ref_axis',(0.447170811246659,0.0146917039183822,-0.894327914919902)) ;
#83172 = DIRECTION('center_axis',(0.89442376259406,-7.10036036684763E-6,-0.4472204521896)) ;
#83173 = DIRECTION('ref_axis',(0.447171519130562,0.0148067719529079,0.894325663269706)) ;
#83174 = DIRECTION('center_axis',(-8.95614743483648E-33,-1.10974565782288E-48,
1.)) ;
#83175 = DIRECTION('ref_axis',(1.,-9.9390457266313E-81,8.95614743483648E-33)) ;
#83176 = DIRECTION('center_axis',(-7.10035964917347E-6,0.894423762594175,
0.447220452189369)) ;
#83177 = DIRECTION('ref_axis',(-0.0148067720024296,-0.447171519129994,0.89432566326917)) ;
#83178 = DIRECTION('center_axis',(-5.60223406011642E-6,0.894424485971595,
-0.447219005480606)) ;
#83179 = DIRECTION('ref_axis',(0.0146917039587169,0.44717081124603,0.894327914919554)) ;
#83180 = DIRECTION('center_axis',(1.40488587213121E-32,-1.23908819712629E-16,
-1.)) ;
#83181 = DIRECTION('ref_axis',(0.,1.,0.)) ;
#83182 = DIRECTION('center_axis',(-1.,0.,0.)) ;
#83183 = DIRECTION('ref_axis',(0.,0.,-1.)) ;
#83184 = DIRECTION('center_axis',(0.,-1.,0.)) ;
#83185 = DIRECTION('ref_axis',(0.,0.,1.)) ;
#83186 = DIRECTION('center_axis',(-1.,0.,-1.40488587213121E-32)) ;
#83187 = DIRECTION('ref_axis',(-1.40488587213121E-32,0.,1.)) ;
#83188 = DIRECTION('',(-1.,0.,-1.40488587213121E-32)) ;
#83189 = DIRECTION('center_axis',(-1.,0.,0.)) ;
#83190 = DIRECTION('ref_axis',(0.,0.,1.)) ;
#83191 = DIRECTION('center_axis',(0.,1.,0.)) ;
#83192 = DIRECTION('ref_axis',(1.,0.,0.)) ;
#83193 = DIRECTION('center_axis',(0.,1.,0.)) ;
#83194 = DIRECTION('ref_axis',(0.,0.,-1.)) ;
#83195 = DIRECTION('center_axis',(0.,0.,-1.)) ;
#83196 = DIRECTION('ref_axis',(1.,0.,0.)) ;
#83197 = DIRECTION('center_axis',(-1.,0.,-1.7912294869673E-32)) ;
#83198 = DIRECTION('ref_axis',(-1.7912294869673E-32,0.,1.)) ;
#83199 = DIRECTION('center_axis',(-0.447219005480393,-5.60223393701113E-6,
0.894424485971702)) ;
#83200 = DIRECTION('ref_axis',(0.894327914919925,0.0146917039386571,0.447170811245947)) ;
#83201 = DIRECTION('center_axis',(-1.,0.,0.)) ;
#83202 = DIRECTION('ref_axis',(0.,0.,1.)) ;
#83203 = DIRECTION('center_axis',(1.23908819712629E-16,-1.,7.2280144832367E-17)) ;
#83204 = DIRECTION('ref_axis',(1.,1.23908819712629E-16,-8.95614743483648E-33)) ;
#83205 = DIRECTION('center_axis',(-7.10036022080745E-6,-0.447220452189551,
0.894423762594084)) ;
#83206 = DIRECTION('ref_axis',(-0.0148067719367088,-0.894325663269946,-0.447171519130618)) ;
#83207 = DIRECTION('center_axis',(0.,-1.,1.0842021724855E-15)) ;
#83208 = DIRECTION('ref_axis',(0.,-1.0842021724855E-15,-1.)) ;
#83209 = DIRECTION('center_axis',(1.23908819712629E-16,-1.,1.23908819712629E-16)) ;
#83210 = DIRECTION('ref_axis',(-9.81657386420148E-47,-1.23908819712629E-16,
-1.)) ;
#83211 = DIRECTION('center_axis',(0.,-1.,0.)) ;
#83212 = DIRECTION('ref_axis',(0.,0.,-1.)) ;
#83213 = DIRECTION('',(-1.23908819712629E-16,1.,-1.23908819712629E-16)) ;
#83214 = DIRECTION('center_axis',(1.,0.,1.40488587213121E-32)) ;
#83215 = DIRECTION('ref_axis',(1.40488587213121E-32,0.,-1.)) ;
#83216 = DIRECTION('center_axis',(-0.707106781186547,0.707106781186548,-6.4115285974492E-16)) ;
#83217 = DIRECTION('ref_axis',(0.707106781186548,0.707106781186547,-1.7981834674121E-12)) ;
#83218 = DIRECTION('center_axis',(1.,0.,0.)) ;
#83219 = DIRECTION('ref_axis',(0.,0.,-1.)) ;
#83220 = DIRECTION('center_axis',(0.,-1.,0.)) ;
#83221 = DIRECTION('ref_axis',(0.,0.,-1.)) ;
#83222 = DIRECTION('center_axis',(0.,0.,1.)) ;
#83223 = DIRECTION('ref_axis',(-1.,0.,0.)) ;
#83224 = DIRECTION('center_axis',(7.2280144832367E-17,0.,-1.)) ;
#83225 = DIRECTION('ref_axis',(-1.,0.,-7.2280144832367E-17)) ;
#83226 = DIRECTION('',(7.2280144832367E-17,0.,-1.)) ;
#83227 = DIRECTION('center_axis',(0.,0.,-1.)) ;
#83228 = DIRECTION('ref_axis',(-1.,0.,0.)) ;
#83229 = DIRECTION('center_axis',(0.,1.,0.)) ;
#83230 = DIRECTION('ref_axis',(1.,0.,0.)) ;
#83231 = DIRECTION('center_axis',(0.,0.,1.)) ;
#83232 = DIRECTION('ref_axis',(-1.,0.,0.)) ;
#83233 = DIRECTION('center_axis',(0.,1.,0.)) ;
#83234 = DIRECTION('ref_axis',(1.,0.,0.)) ;
#83235 = DIRECTION('center_axis',(1.,0.,0.)) ;
#83236 = DIRECTION('ref_axis',(0.,0.,1.)) ;
#83237 = DIRECTION('center_axis',(0.,0.,-1.)) ;
#83238 = DIRECTION('ref_axis',(1.,0.,0.)) ;
#83239 = DIRECTION('center_axis',(-1.13380619344889E-16,1.,-1.23908819712629E-16)) ;
#83240 = DIRECTION('ref_axis',(-1.40488587213121E-32,1.23908819712629E-16,
1.)) ;
#83241 = DIRECTION('center_axis',(0.,1.,0.)) ;
#83242 = DIRECTION('ref_axis',(0.,0.,1.)) ;
#83243 = DIRECTION('center_axis',(7.2280144832367E-17,0.,-1.)) ;
#83244 = DIRECTION('ref_axis',(-1.,0.,-7.2280144832367E-17)) ;
#83245 = DIRECTION('center_axis',(0.,0.,1.)) ;
#83246 = DIRECTION('ref_axis',(1.,0.,0.)) ;
#83247 = DIRECTION('center_axis',(0.,1.,0.)) ;
#83248 = DIRECTION('ref_axis',(1.,0.,0.)) ;
#83249 = DIRECTION('center_axis',(0.,1.,0.)) ;
#83250 = DIRECTION('ref_axis',(0.,0.,-1.)) ;
#83251 = DIRECTION('center_axis',(1.,2.16840434497101E-15,-2.93873587705572E-31)) ;
#83252 = DIRECTION('ref_axis',(2.16840434497101E-15,-1.,-1.03035812136257E-62)) ;
#83253 = DIRECTION('center_axis',(-8.95614743483648E-33,0.,1.)) ;
#83254 = DIRECTION('ref_axis',(1.,0.,8.95614743483648E-33)) ;
#83255 = DIRECTION('center_axis',(-1.40488587213121E-32,1.23908819712629E-16,
1.)) ;
#83256 = DIRECTION('ref_axis',(-1.74077750246726E-48,-1.,1.23908819712629E-16)) ;
#83257 = DIRECTION('center_axis',(8.95614743483648E-33,1.0154535431059E-48,
-1.)) ;
#83258 = DIRECTION('ref_axis',(-1.,9.09455164528354E-81,-8.95614743483648E-33)) ;
#83259 = DIRECTION('center_axis',(2.16840434497101E-15,0.,-1.)) ;
#83260 = DIRECTION('ref_axis',(-1.,0.,-2.16840434497101E-15)) ;
#83261 = DIRECTION('',(-8.95614743483648E-33,-1.0154535431059E-48,1.)) ;
#83262 = DIRECTION('center_axis',(-1.,-1.13380619344889E-16,0.)) ;
#83263 = DIRECTION('ref_axis',(0.,-1.,0.)) ;
#83264 = DIRECTION('center_axis',(0.,0.,1.)) ;
#83265 = DIRECTION('ref_axis',(-1.,0.,0.)) ;
#83266 = DIRECTION('center_axis',(0.,-1.,0.)) ;
#83267 = DIRECTION('ref_axis',(0.,0.,-1.)) ;
#83268 = DIRECTION('center_axis',(-1.,0.,0.)) ;
#83269 = DIRECTION('ref_axis',(0.,0.,-1.)) ;
#83270 = DIRECTION('center_axis',(1.,0.,1.40488587213121E-32)) ;
#83271 = DIRECTION('ref_axis',(1.40488587213121E-32,0.,-1.)) ;
#83272 = DIRECTION('',(1.,0.,1.40488587213121E-32)) ;
#83273 = DIRECTION('center_axis',(1.,0.,0.)) ;
#83274 = DIRECTION('ref_axis',(0.,0.,-1.)) ;
#83275 = DIRECTION('center_axis',(-1.40488587213121E-32,1.23908819712629E-16,
1.)) ;
#83276 = DIRECTION('ref_axis',(0.,-1.,0.)) ;
#83277 = DIRECTION('center_axis',(0.,-1.,0.)) ;
#83278 = DIRECTION('ref_axis',(0.,0.,1.)) ;
#83279 = DIRECTION('center_axis',(0.,1.,0.)) ;
#83280 = DIRECTION('ref_axis',(1.,0.,0.)) ;
#83281 = DIRECTION('center_axis',(1.,0.,0.)) ;
#83282 = DIRECTION('ref_axis',(0.,0.,1.)) ;
#83283 = DIRECTION('center_axis',(0.,1.,0.)) ;
#83284 = DIRECTION('ref_axis',(0.,0.,-1.)) ;
#83285 = DIRECTION('center_axis',(0.,0.,1.)) ;
#83286 = DIRECTION('ref_axis',(1.,0.,0.)) ;
#83287 = DIRECTION('center_axis',(0.,0.,1.)) ;
#83288 = DIRECTION('ref_axis',(1.,0.,0.)) ;
#83289 = DIRECTION('center_axis',(1.,0.,1.40488587213121E-32)) ;
#83290 = DIRECTION('ref_axis',(1.40488587213121E-32,0.,-1.)) ;
#83291 = DIRECTION('center_axis',(-0.707106781186552,0.707106781186543,-7.95029546083767E-15)) ;
#83292 = DIRECTION('ref_axis',(0.707106781186543,0.707106781186552,-2.58223494640614E-13)) ;
#83293 = DIRECTION('center_axis',(-1.23908819712629E-16,1.,-1.23908819712629E-16)) ;
#83294 = DIRECTION('ref_axis',(9.81657386420148E-47,1.23908819712629E-16,
1.)) ;
#83295 = DIRECTION('',(1.23908819712629E-16,-1.,1.23908819712629E-16)) ;
#83296 = DIRECTION('center_axis',(-1.,-1.13380619344889E-16,0.)) ;
#83297 = DIRECTION('ref_axis',(0.,-1.,0.)) ;
#83298 = DIRECTION('center_axis',(0.,-1.,0.)) ;
#83299 = DIRECTION('ref_axis',(0.,0.,1.)) ;
#83300 = DIRECTION('center_axis',(1.13380619344889E-16,-1.,1.23908819712629E-16)) ;
#83301 = DIRECTION('ref_axis',(1.40488587213121E-32,-1.23908819712629E-16,
-1.)) ;
#83302 = DIRECTION('center_axis',(-1.5529910948782E-31,-4.47619207437002E-16,
1.)) ;
#83303 = DIRECTION('ref_axis',(6.951486430461E-47,-1.,-4.47619207437002E-16)) ;
#83304 = DIRECTION('center_axis',(0.,2.16840434497101E-15,-1.)) ;
#83305 = DIRECTION('ref_axis',(0.,1.,2.16840434497101E-15)) ;
#83306 = DIRECTION('center_axis',(0.,1.,0.)) ;
#83307 = DIRECTION('ref_axis',(1.,0.,0.)) ;
#83308 = DIRECTION('center_axis',(3.85194802226865E-15,0.888198741900269,
-0.45945945945946)) ;
#83309 = DIRECTION('ref_axis',(3.25260651745654E-15,-0.45945945945946,-0.888198741900269)) ;
#83310 = DIRECTION('center_axis',(-1.,0.,1.22067519501986E-15)) ;
#83311 = DIRECTION('ref_axis',(-1.22067519501986E-15,1.73472347597682E-14,
-1.)) ;
#83312 = DIRECTION('center_axis',(1.5529910948782E-31,4.47619207437002E-16,
-1.)) ;
#83313 = DIRECTION('ref_axis',(-6.951486430461E-47,1.,4.47619207437002E-16)) ;
#83314 = DIRECTION('center_axis',(0.,0.,1.)) ;
#83315 = DIRECTION('ref_axis',(1.,0.,0.)) ;
#83316 = DIRECTION('center_axis',(1.,-3.46944695195361E-16,0.)) ;
#83317 = DIRECTION('ref_axis',(3.46944695195361E-16,1.,0.)) ;
#83318 = DIRECTION('center_axis',(-1.,3.46944695195361E-16,0.)) ;
#83319 = DIRECTION('ref_axis',(3.46944695195361E-16,1.,1.73472347597681E-14)) ;
#83320 = DIRECTION('center_axis',(1.,-3.46944695195361E-16,0.)) ;
#83321 = DIRECTION('ref_axis',(3.41607084500048E-16,1.,0.)) ;
#83322 = DIRECTION('center_axis',(0.,0.459459459459457,-0.888198741900271)) ;
#83323 = DIRECTION('ref_axis',(0.,0.888198741900271,0.459459459459457)) ;
#83324 = DIRECTION('center_axis',(0.,0.,1.)) ;
#83325 = DIRECTION('ref_axis',(1.,0.,0.)) ;
#83326 = DIRECTION('center_axis',(0.,0.,-1.)) ;
#83327 = DIRECTION('ref_axis',(-1.,0.,0.)) ;
#83328 = DIRECTION('center_axis',(-1.,3.46944695195361E-16,0.)) ;
#83329 = DIRECTION('ref_axis',(-3.46944695195361E-16,-1.,0.)) ;
#83330 = DIRECTION('center_axis',(-1.,3.46944695195361E-16,0.)) ;
#83331 = DIRECTION('ref_axis',(-3.46944695195361E-16,-1.,0.)) ;
#83332 = DIRECTION('center_axis',(-1.,3.46944695195361E-16,0.)) ;
#83333 = DIRECTION('ref_axis',(3.46944695195361E-16,1.,0.)) ;
#83334 = DIRECTION('center_axis',(1.,-3.46944695195361E-16,0.)) ;
#83335 = DIRECTION('ref_axis',(0.,1.,0.)) ;
#83336 = DIRECTION('center_axis',(0.,-0.888198741900269,0.459459459459461)) ;
#83337 = DIRECTION('ref_axis',(0.,0.459459459459461,0.888198741900269)) ;
#83338 = DIRECTION('center_axis',(0.,1.,0.)) ;
#83339 = DIRECTION('ref_axis',(1.,0.,0.)) ;
#83340 = DIRECTION('center_axis',(0.,1.,0.)) ;
#83341 = DIRECTION('ref_axis',(0.,0.,-1.)) ;
#83342 = DIRECTION('center_axis',(-1.,0.,0.)) ;
#83343 = DIRECTION('ref_axis',(0.,-8.67361737988409E-15,-1.)) ;
#83344 = DIRECTION('center_axis',(1.,-3.46944695195361E-16,0.)) ;
#83345 = DIRECTION('ref_axis',(3.70074341541719E-16,1.,0.)) ;
#83346 = DIRECTION('center_axis',(0.,0.63294893130157,-0.774193548387094)) ;
#83347 = DIRECTION('ref_axis',(-1.08420217248551E-15,-0.774193548387094,-0.63294893130157)) ;
#83348 = DIRECTION('center_axis',(1.,-3.46944695195361E-16,0.)) ;
#83349 = DIRECTION('ref_axis',(3.80647894157197E-16,1.,0.)) ;
#83350 = DIRECTION('center_axis',(0.,-0.45945945945946,0.888198741900269)) ;
#83351 = DIRECTION('ref_axis',(0.,-0.888198741900269,-0.45945945945946)) ;
#83352 = DIRECTION('center_axis',(1.,-3.46944695195361E-16,0.)) ;
#83353 = DIRECTION('ref_axis',(3.46944695195361E-16,1.,0.)) ;
#83354 = DIRECTION('center_axis',(-1.,3.46944695195361E-16,0.)) ;
#83355 = DIRECTION('ref_axis',(3.46944695195361E-16,1.,0.)) ;
#83356 = DIRECTION('center_axis',(-3.46944695195361E-16,-1.,-2.45739631480277E-16)) ;
#83357 = DIRECTION('ref_axis',(1.,-3.46944695195361E-16,-8.52580615413453E-32)) ;
#83358 = DIRECTION('center_axis',(0.,1.,0.)) ;
#83359 = DIRECTION('ref_axis',(0.,0.,1.)) ;
#83360 = DIRECTION('center_axis',(1.,-3.46944695195361E-16,0.)) ;
#83361 = DIRECTION('ref_axis',(3.33066907387547E-16,1.,0.)) ;
#83362 = DIRECTION('center_axis',(8.02036034720251E-16,0.293103448275862,
-0.956080733311157)) ;
#83363 = DIRECTION('ref_axis',(-1.93209005840966E-30,0.956080733311157,0.293103448275862)) ;
#83364 = DIRECTION('center_axis',(-1.,3.46944695195361E-16,0.)) ;
#83365 = DIRECTION('ref_axis',(-3.46944695195361E-16,-1.,0.)) ;
#83366 = DIRECTION('center_axis',(-1.,3.46944695195361E-16,0.)) ;
#83367 = DIRECTION('ref_axis',(-3.46944695195361E-16,-1.,0.)) ;
#83368 = DIRECTION('center_axis',(-1.,3.46944695195361E-16,0.)) ;
#83369 = DIRECTION('ref_axis',(-3.46944695195361E-16,-1.,0.)) ;
#83370 = DIRECTION('center_axis',(0.,0.,-1.)) ;
#83371 = DIRECTION('ref_axis',(-1.,0.,0.)) ;
#83372 = DIRECTION('center_axis',(0.,0.,1.)) ;
#83373 = DIRECTION('ref_axis',(1.,0.,0.)) ;
#83374 = DIRECTION('center_axis',(-1.5529910948782E-31,-4.47619207437002E-16,
-1.)) ;
#83375 = DIRECTION('ref_axis',(-6.95148643046101E-47,1.,-4.47619207437002E-16)) ;
#83376 = DIRECTION('center_axis',(2.16840434497101E-15,0.,1.)) ;
#83377 = DIRECTION('ref_axis',(1.,0.,-2.16840434497101E-15)) ;
#83378 = DIRECTION('center_axis',(1.,-3.46944695195361E-16,0.)) ;
#83379 = DIRECTION('ref_axis',(0.,1.,0.)) ;
#83380 = DIRECTION('center_axis',(0.,-1.,0.)) ;
#83381 = DIRECTION('ref_axis',(0.,0.,1.)) ;
#83382 = DIRECTION('center_axis',(0.577350269189627,0.577350269189627,0.577350269189623)) ;
#83383 = DIRECTION('ref_axis',(-0.707106781186548,2.22044604925032E-15,0.707106781186547)) ;
#83384 = DIRECTION('center_axis',(-1.,3.46944695195361E-16,0.)) ;
#83385 = DIRECTION('ref_axis',(-3.70074341541719E-16,-1.,0.)) ;
#83386 = DIRECTION('center_axis',(0.,0.63294893130157,0.774193548387094)) ;
#83387 = DIRECTION('ref_axis',(0.,0.774193548387094,-0.63294893130157)) ;
#83388 = DIRECTION('center_axis',(0.,1.,0.)) ;
#83389 = DIRECTION('ref_axis',(1.,0.,0.)) ;
#83390 = DIRECTION('center_axis',(-1.,0.,0.)) ;
#83391 = DIRECTION('ref_axis',(0.,1.73472347597682E-14,-1.)) ;
#83392 = DIRECTION('center_axis',(0.,0.888198741900271,0.459459459459457)) ;
#83393 = DIRECTION('ref_axis',(-1.08420217248551E-15,0.459459459459457,-0.888198741900271)) ;
#83394 = DIRECTION('center_axis',(3.46944695195361E-16,1.,2.45739631480277E-16)) ;
#83395 = DIRECTION('ref_axis',(-1.,3.46944695195361E-16,8.52580615413453E-32)) ;
#83396 = DIRECTION('center_axis',(-1.,3.46944695195361E-16,0.)) ;
#83397 = DIRECTION('ref_axis',(-3.33066907387547E-16,-1.,0.)) ;
#83398 = DIRECTION('center_axis',(0.,0.293103448275864,0.956080733311156)) ;
#83399 = DIRECTION('ref_axis',(0.,-0.956080733311156,0.293103448275864)) ;
#83400 = DIRECTION('center_axis',(-3.46944695195361E-16,-1.,-1.06487173641454E-15)) ;
#83401 = DIRECTION('ref_axis',(3.69451600012496E-31,1.06487173641454E-15,
-1.)) ;
#83402 = DIRECTION('center_axis',(0.,-1.,0.)) ;
#83403 = DIRECTION('ref_axis',(0.,0.,-1.)) ;
#83404 = DIRECTION('center_axis',(0.,1.,0.)) ;
#83405 = DIRECTION('ref_axis',(0.,0.,1.)) ;
#83406 = DIRECTION('center_axis',(-1.,3.46944695195361E-16,0.)) ;
#83407 = DIRECTION('ref_axis',(-3.41607084500048E-16,-1.,0.)) ;
#83408 = DIRECTION('center_axis',(-4.88154879316133E-15,0.45945945945946,
0.888198741900269)) ;
#83409 = DIRECTION('ref_axis',(-3.39148554690438E-29,-0.888198741900269,0.45945945945946)) ;
#83410 = DIRECTION('center_axis',(1.,-3.46944695195361E-16,0.)) ;
#83411 = DIRECTION('ref_axis',(3.46944695195361E-16,1.,0.)) ;
#83412 = DIRECTION('center_axis',(-1.,3.46944695195361E-16,0.)) ;
#83413 = DIRECTION('ref_axis',(3.46944695195361E-16,1.,0.)) ;
#83414 = DIRECTION('center_axis',(-1.5529910948782E-31,-4.47619207437002E-16,
-1.)) ;
#83415 = DIRECTION('ref_axis',(-6.95148643046101E-47,1.,-4.47619207437002E-16)) ;
#83416 = DIRECTION('center_axis',(0.,0.,-1.)) ;
#83417 = DIRECTION('ref_axis',(-1.,0.,0.)) ;
#83418 = DIRECTION('center_axis',(0.,0.224137931034483,-0.974557431797419)) ;
#83419 = DIRECTION('ref_axis',(0.,-0.974557431797419,-0.224137931034483)) ;
#83420 = DIRECTION('center_axis',(0.577350269189627,0.577350269189627,0.577350269189623)) ;
#83421 = DIRECTION('ref_axis',(-0.707106781186548,2.22044604925032E-15,0.707106781186547)) ;
#83422 = DIRECTION('center_axis',(0.408248290463864,-0.816496580927725,0.408248290463864)) ;
#83423 = DIRECTION('ref_axis',(0.707106781186545,-2.77555756156289E-15,-0.70710678118655)) ;
#83424 = DIRECTION('center_axis',(0.,1.,0.)) ;
#83425 = DIRECTION('ref_axis',(1.,0.,0.)) ;
#83426 = DIRECTION('center_axis',(-1.,0.,0.)) ;
#83427 = DIRECTION('ref_axis',(0.,0.,-1.)) ;
#83428 = DIRECTION('center_axis',(1.,-3.46944695195361E-16,0.)) ;
#83429 = DIRECTION('ref_axis',(0.,1.,0.)) ;
#83430 = DIRECTION('center_axis',(9.96293888229924E-16,-0.888198741900269,
-0.45945945945946)) ;
#83431 = DIRECTION('ref_axis',(-3.00809911926502E-30,-0.45945945945946,0.888198741900269)) ;
#83432 = DIRECTION('center_axis',(1.,-3.46944695195361E-16,0.)) ;
#83433 = DIRECTION('ref_axis',(-3.70074341541719E-16,-1.,0.)) ;
#83434 = DIRECTION('center_axis',(1.58436874053304E-16,-0.224137931034483,
-0.974557431797419)) ;
#83435 = DIRECTION('ref_axis',(2.18893094986727E-31,0.974557431797419,-0.224137931034483)) ;
#83436 = DIRECTION('center_axis',(1.,-3.46944695195361E-16,0.)) ;
#83437 = DIRECTION('ref_axis',(3.46944695195361E-16,1.,0.)) ;
#83438 = DIRECTION('center_axis',(-1.,3.46944695195361E-16,0.)) ;
#83439 = DIRECTION('ref_axis',(3.46944695195361E-16,1.,0.)) ;
#83440 = DIRECTION('center_axis',(1.,-3.46944695195361E-16,0.)) ;
#83441 = DIRECTION('ref_axis',(3.80647894157197E-16,1.,0.)) ;
#83442 = DIRECTION('center_axis',(0.,-0.45945945945946,-0.888198741900269)) ;
#83443 = DIRECTION('ref_axis',(0.,0.888198741900269,-0.45945945945946)) ;
#83444 = DIRECTION('center_axis',(1.,-3.46944695195361E-16,0.)) ;
#83445 = DIRECTION('ref_axis',(0.,1.,0.)) ;
#83446 = DIRECTION('center_axis',(0.,-1.,0.)) ;
#83447 = DIRECTION('ref_axis',(0.,0.,1.)) ;
#83448 = DIRECTION('center_axis',(-3.46944695195361E-16,-1.,-1.06487173641454E-15)) ;
#83449 = DIRECTION('ref_axis',(3.69451600012496E-31,1.06487173641454E-15,
-1.)) ;
#83450 = DIRECTION('center_axis',(0.,0.,1.)) ;
#83451 = DIRECTION('ref_axis',(1.,0.,0.)) ;
#83452 = DIRECTION('center_axis',(0.,-1.,0.)) ;
#83453 = DIRECTION('ref_axis',(0.,0.,-1.)) ;
#83454 = DIRECTION('center_axis',(0.,-1.,0.)) ;
#83455 = DIRECTION('ref_axis',(0.,0.,-1.)) ;
#83456 = DIRECTION('center_axis',(0.,1.,0.)) ;
#83457 = DIRECTION('ref_axis',(0.,0.,-1.)) ;
#83458 = DIRECTION('center_axis',(0.,0.,1.)) ;
#83459 = DIRECTION('ref_axis',(1.,0.,0.)) ;
#83460 = DIRECTION('center_axis',(8.67361737988404E-15,-1.,0.)) ;
#83461 = DIRECTION('ref_axis',(1.,8.67361737988404E-15,0.)) ;
#83462 = DIRECTION('center_axis',(0.497468338163091,-0.710669054518702,0.497468338163091)) ;
#83463 = DIRECTION('ref_axis',(0.81923192051904,0.573462344363328,8.04804396179112E-16)) ;
#83464 = DIRECTION('center_axis',(0.497468338163091,-0.710669054518702,0.497468338163091)) ;
#83465 = DIRECTION('ref_axis',(0.81923192051904,0.573462344363328,7.6535433881835E-16)) ;
#83466 = DIRECTION('center_axis',(0.497468338163092,-0.7106690545187,0.497468338163092)) ;
#83467 = DIRECTION('ref_axis',(-1.24903860074368E-15,-0.57346234436333,-0.819231920519039)) ;
#83468 = DIRECTION('center_axis',(0.,0.,1.)) ;
#83469 = DIRECTION('ref_axis',(1.,0.,0.)) ;
#83470 = DIRECTION('center_axis',(0.,-1.,0.)) ;
#83471 = DIRECTION('ref_axis',(0.,0.,-1.)) ;
#83472 = DIRECTION('center_axis',(0.,1.,0.)) ;
#83473 = DIRECTION('ref_axis',(0.,0.,1.)) ;
#83474 = DIRECTION('center_axis',(0.,1.,0.)) ;
#83475 = DIRECTION('ref_axis',(0.,0.,1.)) ;
#83476 = DIRECTION('center_axis',(0.,1.,0.)) ;
#83477 = DIRECTION('ref_axis',(1.,0.,0.)) ;
#83478 = DIRECTION('center_axis',(-1.98515611757154E-15,0.,1.)) ;
#83479 = DIRECTION('ref_axis',(-1.,0.,-1.98515611757154E-15)) ;
#83480 = DIRECTION('center_axis',(1.,-4.06575814682065E-16,2.84603070277446E-16)) ;
#83481 = DIRECTION('ref_axis',(-4.06575814682065E-16,-1.,6.48893816316174E-47)) ;
#83482 = DIRECTION('center_axis',(0.,1.,0.)) ;
#83483 = DIRECTION('ref_axis',(0.,0.,1.)) ;
#83484 = DIRECTION('center_axis',(0.,1.,0.)) ;
#83485 = DIRECTION('ref_axis',(0.,0.,1.)) ;
#83486 = DIRECTION('center_axis',(0.497468338163091,0.710669054518702,-0.497468338163091)) ;
#83487 = DIRECTION('ref_axis',(-0.81923192051904,0.573462344363328,7.6535433881835E-16)) ;
#83488 = DIRECTION('center_axis',(-0.497468338163091,-0.710669054518702,0.497468338163091)) ;
#83489 = DIRECTION('ref_axis',(-0.819231920519035,0.573462344363336,1.64011789552923E-14)) ;
#83490 = DIRECTION('center_axis',(-0.497468338163093,-0.7106690545187,0.497468338163091)) ;
#83491 = DIRECTION('ref_axis',(0.819231920519039,-0.573462344363331,1.48853464230757E-16)) ;
#83492 = DIRECTION('center_axis',(1.,0.,0.)) ;
#83493 = DIRECTION('ref_axis',(0.,0.,-1.)) ;
#83494 = DIRECTION('center_axis',(1.,0.,-9.9257805878577E-16)) ;
#83495 = DIRECTION('ref_axis',(-9.9257805878577E-16,0.,-1.)) ;
#83496 = DIRECTION('center_axis',(0.,0.,-1.)) ;
#83497 = DIRECTION('ref_axis',(-1.,0.,0.)) ;
#83498 = DIRECTION('center_axis',(-1.23327997120227E-15,1.76182853028895E-15,
1.)) ;
#83499 = DIRECTION('ref_axis',(-2.17282783909808E-30,-1.,1.76182853028895E-15)) ;
#83500 = DIRECTION('center_axis',(-0.497468338163091,0.710669054518702,0.497468338163091)) ;
#83501 = DIRECTION('ref_axis',(-0.81923192051904,-0.573462344363328,7.6535433881835E-16)) ;
#83502 = DIRECTION('center_axis',(0.497468338163091,-0.710669054518702,-0.497468338163091)) ;
#83503 = DIRECTION('ref_axis',(-0.819231920519018,-0.57346234436336,6.87084924063159E-14)) ;
#83504 = DIRECTION('center_axis',(0.497468338163093,-0.7106690545187,-0.497468338163091)) ;
#83505 = DIRECTION('ref_axis',(0.819231920519039,0.573462344363331,2.16059097207149E-16)) ;
#83506 = DIRECTION('center_axis',(0.,1.,0.)) ;
#83507 = DIRECTION('ref_axis',(1.,0.,0.)) ;
#83508 = DIRECTION('center_axis',(-1.13841228110978E-15,-1.62630325872826E-15,
1.)) ;
#83509 = DIRECTION('ref_axis',(3.52365706057789E-15,1.,1.62630325872826E-15)) ;
#83510 = DIRECTION('center_axis',(0.,1.,0.)) ;
#83511 = DIRECTION('ref_axis',(1.,0.,0.)) ;
#83512 = DIRECTION('center_axis',(1.,0.,-1.65429676464295E-16)) ;
#83513 = DIRECTION('ref_axis',(1.65429676464295E-16,4.33680868994204E-15,
1.)) ;
#83514 = DIRECTION('center_axis',(0.,0.,-1.)) ;
#83515 = DIRECTION('ref_axis',(-1.,0.,0.)) ;
#83516 = DIRECTION('center_axis',(3.3085935292859E-16,0.,1.)) ;
#83517 = DIRECTION('ref_axis',(1.,0.,-3.3085935292859E-16)) ;
#83518 = DIRECTION('center_axis',(1.,0.,0.)) ;
#83519 = DIRECTION('ref_axis',(0.,0.,-1.)) ;
#83520 = DIRECTION('center_axis',(1.,1.21972744404619E-15,8.53809210832338E-16)) ;
#83521 = DIRECTION('ref_axis',(-1.21972744404619E-15,1.,-2.84382165153726E-47)) ;
#83522 = DIRECTION('center_axis',(0.,1.,0.)) ;
#83523 = DIRECTION('ref_axis',(1.,0.,0.)) ;
#83524 = DIRECTION('center_axis',(0.497468338163092,0.710669054518701,0.497468338163092)) ;
#83525 = DIRECTION('ref_axis',(1.11733937654106E-14,0.573462344363324,-0.819231920519043)) ;
#83526 = DIRECTION('center_axis',(-0.497468338163091,-0.710669054518702,-0.497468338163091)) ;
#83527 = DIRECTION('ref_axis',(0.81923192051904,-0.573462344363328,7.6535433881835E-16)) ;
#83528 = DIRECTION('center_axis',(-0.497468338163091,-0.710669054518702,-0.497468338163091)) ;
#83529 = DIRECTION('ref_axis',(0.81923192051904,-0.573462344363328,7.6535433881835E-16)) ;
#83530 = DIRECTION('center_axis',(0.,-1.,0.)) ;
#83531 = DIRECTION('ref_axis',(0.,0.,-1.)) ;
#83532 = DIRECTION('center_axis',(0.,1.,0.)) ;
#83533 = DIRECTION('ref_axis',(0.,0.,-1.)) ;
#83534 = DIRECTION('center_axis',(-8.67361737988403E-15,1.,0.)) ;
#83535 = DIRECTION('ref_axis',(-1.,-8.67361737988403E-15,0.)) ;
#83536 = DIRECTION('center_axis',(0.,0.,1.)) ;
#83537 = DIRECTION('ref_axis',(1.,0.,0.)) ;
#83538 = DIRECTION('center_axis',(1.,6.67201336914158E-17,0.)) ;
#83539 = DIRECTION('ref_axis',(-6.67201336914158E-17,1.,0.)) ;
#83540 = DIRECTION('center_axis',(-1.,-6.67201336914158E-17,0.)) ;
#83541 = DIRECTION('ref_axis',(-6.67201336914158E-17,1.,0.)) ;
#83542 = DIRECTION('center_axis',(-1.,1.33440267382831E-16,0.)) ;
#83543 = DIRECTION('ref_axis',(-1.33440267382831E-16,-1.,0.)) ;
#83544 = DIRECTION('center_axis',(-1.,1.33440267382831E-16,0.)) ;
#83545 = DIRECTION('ref_axis',(-1.33440267382831E-16,-1.,0.)) ;
#83546 = DIRECTION('center_axis',(0.710669054518702,0.497468338163091,0.497468338163091)) ;
#83547 = DIRECTION('ref_axis',(-0.573462344363328,0.819231920519041,3.92980824865032E-16)) ;
#83548 = DIRECTION('center_axis',(0.710669054518702,0.497468338163091,0.497468338163091)) ;
#83549 = DIRECTION('ref_axis',(-0.573462344363328,0.819231920519041,3.92980824865032E-16)) ;
#83550 = DIRECTION('center_axis',(0.710669054518701,0.497468338163091,0.497468338163092)) ;
#83551 = DIRECTION('ref_axis',(0.57346234436333,-1.81382726107456E-15,-0.819231920519039)) ;
#83552 = DIRECTION('center_axis',(-0.710669054518702,0.497468338163091,-0.497468338163091)) ;
#83553 = DIRECTION('ref_axis',(-0.573462344363328,-0.819231920519041,6.69271761853466E-16)) ;
#83554 = DIRECTION('center_axis',(0.710669054518702,-0.497468338163091,0.497468338163091)) ;
#83555 = DIRECTION('ref_axis',(-0.573462344363335,-0.819231920519036,1.5770623553551E-14)) ;
#83556 = DIRECTION('center_axis',(0.7106690545187,-0.497468338163094,0.497468338163091)) ;
#83557 = DIRECTION('ref_axis',(0.573462344363331,0.819231920519038,2.86772422505918E-16)) ;
#83558 = DIRECTION('center_axis',(0.,1.,-9.34081871679819E-17)) ;
#83559 = DIRECTION('ref_axis',(0.,9.34081871679819E-17,1.)) ;
#83560 = DIRECTION('center_axis',(-4.33680868994205E-15,-1.,-3.03576608295944E-15)) ;
#83561 = DIRECTION('ref_axis',(1.,-4.33680868994205E-15,-1.12103877145985E-44)) ;
#83562 = DIRECTION('center_axis',(0.,1.,5.29374964685745E-15)) ;
#83563 = DIRECTION('ref_axis',(0.,-5.29374964685745E-15,1.)) ;
#83564 = DIRECTION('center_axis',(0.,1.,0.)) ;
#83565 = DIRECTION('ref_axis',(1.,0.,0.)) ;
#83566 = DIRECTION('center_axis',(0.,6.45175738210751E-15,1.)) ;
#83567 = DIRECTION('ref_axis',(0.,1.,-6.45175738210751E-15)) ;
#83568 = DIRECTION('center_axis',(-1.,-6.67201336914158E-17,0.)) ;
#83569 = DIRECTION('ref_axis',(6.67201336914158E-17,-1.,0.)) ;
#83570 = DIRECTION('center_axis',(-1.,-6.67201336914158E-17,0.)) ;
#83571 = DIRECTION('ref_axis',(6.67201336914158E-17,-1.,0.)) ;
#83572 = DIRECTION('center_axis',(1.,-1.33440267382831E-16,0.)) ;
#83573 = DIRECTION('ref_axis',(1.33440267382831E-16,1.,0.)) ;
#83574 = DIRECTION('center_axis',(-1.,1.33440267382831E-16,0.)) ;
#83575 = DIRECTION('ref_axis',(1.33440267382831E-16,1.,0.)) ;
#83576 = DIRECTION('center_axis',(0.,1.,0.)) ;
#83577 = DIRECTION('ref_axis',(1.,0.,0.)) ;
#83578 = DIRECTION('center_axis',(1.76182853028896E-15,-1.23327997120227E-15,
1.)) ;
#83579 = DIRECTION('ref_axis',(-1.,-2.1728278390981E-30,1.76182853028896E-15)) ;
#83580 = DIRECTION('center_axis',(0.,0.,-1.)) ;
#83581 = DIRECTION('ref_axis',(-1.,0.,0.)) ;
#83582 = DIRECTION('center_axis',(-2.71050543121378E-16,-1.89735380184965E-16,
1.)) ;
#83583 = DIRECTION('ref_axis',(1.,-5.14278778484758E-32,2.71050543121378E-16)) ;
#83584 = DIRECTION('center_axis',(-0.710669054518702,-0.497468338163091,0.497468338163091)) ;
#83585 = DIRECTION('ref_axis',(0.573462344363328,-0.819231920519041,3.92980824865032E-16)) ;
#83586 = DIRECTION('center_axis',(0.710669054518702,0.497468338163091,-0.497468338163091)) ;
#83587 = DIRECTION('ref_axis',(0.573462344363328,-0.819231920519041,3.92980824865032E-16)) ;
#83588 = DIRECTION('center_axis',(0.710669054518701,0.497468338163091,-0.497468338163092)) ;
#83589 = DIRECTION('ref_axis',(-0.57346234436333,1.88103289405095E-15,-0.819231920519039)) ;
#83590 = DIRECTION('center_axis',(0.710669054518702,-0.497468338163091,-0.497468338163091)) ;
#83591 = DIRECTION('ref_axis',(0.573462344363328,0.819231920519041,6.69271761853466E-16)) ;
#83592 = DIRECTION('center_axis',(0.710669054518702,-0.497468338163091,-0.497468338163091)) ;
#83593 = DIRECTION('ref_axis',(0.573462344363328,0.819231920519041,6.69271761853466E-16)) ;
#83594 = DIRECTION('center_axis',(0.7106690545187,-0.497468338163091,-0.497468338163093)) ;
#83595 = DIRECTION('ref_axis',(-0.573462344363331,-1.17187023180681E-15,-0.819231920519038)) ;
#83596 = DIRECTION('center_axis',(0.,0.,-1.)) ;
#83597 = DIRECTION('ref_axis',(-1.,0.,0.)) ;
#83598 = DIRECTION('center_axis',(0.,1.15800773525007E-15,1.)) ;
#83599 = DIRECTION('ref_axis',(0.,-1.,1.15800773525007E-15)) ;
#83600 = DIRECTION('center_axis',(0.,1.,0.)) ;
#83601 = DIRECTION('ref_axis',(1.,0.,0.)) ;
#83602 = DIRECTION('center_axis',(0.,1.,0.)) ;
#83603 = DIRECTION('ref_axis',(0.,0.,-1.)) ;
#83604 = DIRECTION('center_axis',(0.,1.,0.)) ;
#83605 = DIRECTION('ref_axis',(1.,0.,0.)) ;
#83606 = DIRECTION('center_axis',(4.33680868994204E-15,-1.,-3.03576608295944E-15)) ;
#83607 = DIRECTION('ref_axis',(-1.,-4.33680868994204E-15,5.60519385729927E-45)) ;
#83608 = DIRECTION('center_axis',(0.,1.,9.34081871679819E-17)) ;
#83609 = DIRECTION('ref_axis',(0.,-9.34081871679819E-17,1.)) ;
#83610 = DIRECTION('center_axis',(0.,0.,1.)) ;
#83611 = DIRECTION('ref_axis',(1.,0.,0.)) ;
#83612 = DIRECTION('center_axis',(-2.16840434497102E-15,-3.61400724161847E-16,
1.)) ;
#83613 = DIRECTION('ref_axis',(1.,-7.83662900548222E-31,2.16840434497102E-15)) ;
#83614 = DIRECTION('center_axis',(0.973328526784575,0.162221421130762,-0.162221421130763)) ;
#83615 = DIRECTION('ref_axis',(-0.164398987305358,9.23743777622416E-16,-0.986393923832144)) ;
#83616 = DIRECTION('center_axis',(0.973328526784574,0.162221421130765,-0.162221421130767)) ;
#83617 = DIRECTION('ref_axis',(-0.164398987305362,1.88956506020588E-16,-0.986393923832143)) ;
#83618 = DIRECTION('center_axis',(0.,1.,0.)) ;
#83619 = DIRECTION('ref_axis',(1.,0.,0.)) ;
#83620 = DIRECTION('center_axis',(0.,1.,-8.79325913341701E-15)) ;
#83621 = DIRECTION('ref_axis',(0.,-8.79325913341701E-15,-1.)) ;
#83622 = DIRECTION('center_axis',(0.,0.,1.)) ;
#83623 = DIRECTION('ref_axis',(1.,0.,0.)) ;
#83624 = DIRECTION('center_axis',(0.,-2.28569887277128E-15,1.)) ;
#83625 = DIRECTION('ref_axis',(0.,-1.,-2.28569887277128E-15)) ;
#83626 = DIRECTION('center_axis',(1.73472347597681E-15,-1.,-2.89120579329468E-16)) ;
#83627 = DIRECTION('ref_axis',(1.,1.73472347597681E-15,5.01544256350843E-31)) ;
#83628 = DIRECTION('center_axis',(8.67361737988409E-15,1.,-1.44560289664739E-15)) ;
#83629 = DIRECTION('ref_axis',(-1.,8.67361737988409E-15,-1.40129846432482E-45)) ;
#83630 = DIRECTION('center_axis',(0.,1.,0.)) ;
#83631 = DIRECTION('ref_axis',(1.,0.,0.)) ;
#83632 = DIRECTION('center_axis',(-0.937042571331634,0.312347523777217,0.156173761888611)) ;
#83633 = DIRECTION('ref_axis',(0.316227766016843,0.948683298050512,6.71158276827649E-18)) ;
#83634 = DIRECTION('center_axis',(0.937042571331636,-0.312347523777212,-0.156173761888606)) ;
#83635 = DIRECTION('ref_axis',(0.316227766016838,0.948683298050514,8.61595672567599E-16)) ;
#83636 = DIRECTION('center_axis',(-0.973328526784575,-0.162221421130762,-0.162221421130763)) ;
#83637 = DIRECTION('ref_axis',(-0.164398987305358,9.23743777622416E-16,0.986393923832144)) ;
#83638 = DIRECTION('center_axis',(0.978231976292141,-0.146734796047223,-0.146734795425461)) ;
#83639 = DIRECTION('ref_axis',(0.18231863354965,0.945435290900637,0.270022270526369)) ;
#83640 = DIRECTION('center_axis',(0.973328526784574,0.162221421130767,0.162221421130768)) ;
#83641 = DIRECTION('ref_axis',(0.164398987305363,-6.69215935033609E-18,-0.986393923832143)) ;
#83642 = DIRECTION('center_axis',(0.,0.,1.)) ;
#83643 = DIRECTION('ref_axis',(1.,0.,0.)) ;
#83644 = DIRECTION('center_axis',(0.,2.19831478335425E-15,-1.)) ;
#83645 = DIRECTION('ref_axis',(0.,1.,2.19831478335425E-15)) ;
#83646 = DIRECTION('center_axis',(0.,1.,0.)) ;
#83647 = DIRECTION('ref_axis',(1.,0.,0.)) ;
#83648 = DIRECTION('center_axis',(8.67361737988408E-15,1.,1.44560289664739E-15)) ;
#83649 = DIRECTION('ref_axis',(1.,-8.67361737988408E-15,5.60519385729927E-45)) ;
#83650 = DIRECTION('center_axis',(1.73472347597681E-15,-1.,2.89120579329468E-16)) ;
#83651 = DIRECTION('ref_axis',(1.,1.73472347597681E-15,-5.01544256350843E-31)) ;
#83652 = DIRECTION('center_axis',(0.,1.,0.)) ;
#83653 = DIRECTION('ref_axis',(0.,0.,1.)) ;
#83654 = DIRECTION('center_axis',(0.,0.,1.)) ;
#83655 = DIRECTION('ref_axis',(1.,0.,0.)) ;
#83656 = DIRECTION('center_axis',(3.25260651745652E-15,-1.08420217248553E-15,
-1.)) ;
#83657 = DIRECTION('ref_axis',(-1.,-3.52648305246695E-30,-3.25260651745652E-15)) ;
#83658 = DIRECTION('center_axis',(0.,1.,0.)) ;
#83659 = DIRECTION('ref_axis',(1.,0.,0.)) ;
#83660 = DIRECTION('center_axis',(-0.937042571331635,0.312347523777215,-0.15617376188861)) ;
#83661 = DIRECTION('ref_axis',(0.316227766016841,0.948683298050513,6.5590042956861E-18)) ;
#83662 = DIRECTION('center_axis',(-0.937042571331636,0.312347523777212,-0.156173761888606)) ;
#83663 = DIRECTION('ref_axis',(0.331350514299576,0.6540349591596,-0.680033167478254)) ;
#83664 = DIRECTION('center_axis',(0.961519724091092,0.245047216428837,-0.12422432090484)) ;
#83665 = DIRECTION('ref_axis',(0.262092069901281,-0.682554728284,0.682221950535173)) ;
#83666 = DIRECTION('center_axis',(2.65552944032596E-32,3.29043518662928E-48,
-1.)) ;
#83667 = DIRECTION('ref_axis',(-1.,8.7378475095785E-80,-2.65552944032596E-32)) ;
#83668 = DIRECTION('center_axis',(2.65552944032596E-32,3.29043518662928E-48,
-1.)) ;
#83669 = DIRECTION('ref_axis',(-1.,8.7378475095785E-80,-2.65552944032596E-32)) ;
#83670 = DIRECTION('center_axis',(-2.65552944032596E-32,-3.29043518662928E-48,
1.)) ;
#83671 = DIRECTION('ref_axis',(-1.,8.7378475095785E-80,-2.65552944032596E-32)) ;
#83672 = DIRECTION('center_axis',(0.,0.,1.)) ;
#83673 = DIRECTION('ref_axis',(1.,0.,0.)) ;
#83674 = DIRECTION('center_axis',(0.,0.,-1.)) ;
#83675 = DIRECTION('ref_axis',(-1.,0.,0.)) ;
#83676 = DIRECTION('center_axis',(0.,0.,1.)) ;
#83677 = DIRECTION('ref_axis',(1.,0.,0.)) ;
#83678 = DIRECTION('center_axis',(0.,0.,1.)) ;
#83679 = DIRECTION('ref_axis',(1.,0.,0.)) ;
#83680 = DIRECTION('center_axis',(0.,0.,-1.)) ;
#83681 = DIRECTION('ref_axis',(-1.,0.,0.)) ;
#83682 = DIRECTION('center_axis',(0.,0.,-1.)) ;
#83683 = DIRECTION('ref_axis',(-1.,0.,0.)) ;
#83684 = DIRECTION('center_axis',(1.,1.15648231731787E-15,0.)) ;
#83685 = DIRECTION('ref_axis',(1.03435541192675E-15,-1.,5.17177705963374E-16)) ;
#83686 = DIRECTION('center_axis',(7.089177613099E-16,-0.612994899008946,-0.790086864711098)) ;
#83687 = DIRECTION('ref_axis',(1.7347234759768E-14,-0.790086864711098,0.612994899008946)) ;
#83688 = DIRECTION('center_axis',(7.08917761309899E-16,-0.612994899008945,
0.790086864711098)) ;
#83689 = DIRECTION('ref_axis',(-1.7347234759768E-14,0.790086864711098,0.612994899008945)) ;
#83690 = DIRECTION('center_axis',(0.,0.,-1.)) ;
#83691 = DIRECTION('ref_axis',(-1.,0.,0.)) ;
#83692 = DIRECTION('center_axis',(0.,0.,1.)) ;
#83693 = DIRECTION('ref_axis',(-1.,2.16840434497102E-15,0.)) ;
#83694 = DIRECTION('center_axis',(1.08420217248551E-15,-1.,0.)) ;
#83695 = DIRECTION('ref_axis',(1.,1.08420217248551E-15,0.)) ;
#83696 = DIRECTION('center_axis',(1.44560289664734E-16,-1.,-2.4093381610789E-16)) ;
#83697 = DIRECTION('ref_axis',(2.28544744656275E-46,2.4093381610789E-16,-1.)) ;
#83698 = DIRECTION('center_axis',(0.,-1.,0.)) ;
#83699 = DIRECTION('ref_axis',(0.,0.,-1.)) ;
#83700 = DIRECTION('center_axis',(1.,0.,0.)) ;
#83701 = DIRECTION('ref_axis',(0.,1.,0.)) ;
#83702 = DIRECTION('center_axis',(1.,0.,0.)) ;
#83703 = DIRECTION('ref_axis',(0.,0.,-1.)) ;
#83704 = DIRECTION('center_axis',(1.,1.23908819712629E-16,8.95614743483648E-33)) ;
#83705 = DIRECTION('ref_axis',(-1.23908819712629E-16,1.,-1.10974565782288E-48)) ;
#83706 = DIRECTION('center_axis',(1.,0.,0.)) ;
#83707 = DIRECTION('ref_axis',(0.,0.,-1.)) ;
#83708 = DIRECTION('center_axis',(-1.,0.,0.)) ;
#83709 = DIRECTION('ref_axis',(0.,0.,1.)) ;
#83710 = DIRECTION('center_axis',(1.,1.23908819712629E-16,8.95614743483648E-33)) ;
#83711 = DIRECTION('ref_axis',(-1.23908819712629E-16,1.,-1.10974565782288E-48)) ;
#83712 = DIRECTION('center_axis',(-1.,0.,0.)) ;
#83713 = DIRECTION('ref_axis',(0.,0.,1.)) ;
#83714 = DIRECTION('center_axis',(1.,0.,0.)) ;
#83715 = DIRECTION('ref_axis',(0.,-1.,0.)) ;
#83716 = DIRECTION('center_axis',(0.,1.,0.)) ;
#83717 = DIRECTION('ref_axis',(0.,0.,1.)) ;
#83718 = DIRECTION('center_axis',(-1.44560289664734E-16,1.,-7.2280144832367E-17)) ;
#83719 = DIRECTION('ref_axis',(0.707106781238332,1.5332934167208E-16,0.707106781134763)) ;
#83720 = DIRECTION('center_axis',(-1.0842021724855E-15,1.,0.)) ;
#83721 = DIRECTION('ref_axis',(-1.,-1.0842021724855E-15,0.)) ;
#83722 = DIRECTION('center_axis',(0.,1.,0.)) ;
#83723 = DIRECTION('ref_axis',(0.,0.,1.)) ;
#83724 = DIRECTION('center_axis',(0.,-1.,0.)) ;
#83725 = DIRECTION('ref_axis',(0.,0.,-1.)) ;
#83726 = DIRECTION('center_axis',(0.,1.,0.)) ;
#83727 = DIRECTION('ref_axis',(0.,0.,1.)) ;
#83728 = DIRECTION('center_axis',(0.,0.,1.)) ;
#83729 = DIRECTION('ref_axis',(1.,0.,0.)) ;
#83730 = DIRECTION('center_axis',(0.431191646768307,0.0335421424106918,0.901636672080133)) ;
#83731 = DIRECTION('ref_axis',(0.899826811386771,0.0573593265856512,-0.432459960184937)) ;
#83732 = DIRECTION('center_axis',(0.,0.,1.)) ;
#83733 = DIRECTION('ref_axis',(-1.,0.,0.)) ;
#83734 = DIRECTION('center_axis',(0.,0.,-1.)) ;
#83735 = DIRECTION('ref_axis',(0.707109343403326,-0.707104218960485,0.)) ;
#83736 = DIRECTION('center_axis',(-3.25260651745653E-15,0.,1.)) ;
#83737 = DIRECTION('ref_axis',(1.,0.,3.25260651745653E-15)) ;
#83738 = DIRECTION('center_axis',(0.,0.,1.)) ;
#83739 = DIRECTION('ref_axis',(1.,0.,0.)) ;
#83740 = DIRECTION('center_axis',(0.431188264322452,0.0335835001127062,-0.901636750155389)) ;
#83741 = DIRECTION('ref_axis',(0.899831768110909,0.0572892330930879,0.432458937784851)) ;
#83742 = DIRECTION('center_axis',(0.,-1.,0.)) ;
#83743 = DIRECTION('ref_axis',(0.,0.,-1.)) ;
#83744 = DIRECTION('center_axis',(0.,1.,0.)) ;
#83745 = DIRECTION('ref_axis',(0.,0.,1.)) ;
#83746 = DIRECTION('center_axis',(0.,0.,1.)) ;
#83747 = DIRECTION('ref_axis',(1.,0.,0.)) ;
#83748 = DIRECTION('center_axis',(0.,0.,-1.)) ;
#83749 = DIRECTION('ref_axis',(-1.,0.,0.)) ;
#83750 = DIRECTION('center_axis',(0.,0.,1.)) ;
#83751 = DIRECTION('ref_axis',(-0.986393923832144,0.164398987305354,0.)) ;
#83752 = DIRECTION('center_axis',(0.98470178743927,-0.164116964573216,0.0585492250433781)) ;
#83753 = DIRECTION('ref_axis',(0.164398987305362,0.986393923832143,-7.60669428566932E-17)) ;
#83754 = DIRECTION('center_axis',(0.984834538781277,-0.164139089796902,0.0562075655416074)) ;
#83755 = DIRECTION('ref_axis',(0.164398987305379,0.98639392383214,1.87706412796466E-17)) ;
#83756 = DIRECTION('center_axis',(0.986393923832145,-0.129889480441767,0.100775740620414)) ;
#83757 = DIRECTION('ref_axis',(0.,0.612994899008951,0.790086864711094)) ;
#83758 = DIRECTION('center_axis',(0.,1.,0.)) ;
#83759 = DIRECTION('ref_axis',(1.,0.,0.)) ;
#83760 = DIRECTION('center_axis',(0.,0.,-1.)) ;
#83761 = DIRECTION('ref_axis',(-1.,0.,0.)) ;
#83762 = DIRECTION('center_axis',(1.,2.8359373108165E-15,0.)) ;
#83763 = DIRECTION('ref_axis',(-2.8359373108165E-15,1.,0.)) ;
#83764 = DIRECTION('center_axis',(0.,0.,-1.)) ;
#83765 = DIRECTION('ref_axis',(-1.,0.,0.)) ;
#83766 = DIRECTION('center_axis',(0.,0.,1.)) ;
#83767 = DIRECTION('ref_axis',(1.,0.,0.)) ;
#83768 = DIRECTION('center_axis',(1.,0.,0.)) ;
#83769 = DIRECTION('ref_axis',(0.,0.,-1.)) ;
#83770 = DIRECTION('center_axis',(1.,0.,0.)) ;
#83771 = DIRECTION('ref_axis',(0.,0.,-1.)) ;
#83772 = DIRECTION('center_axis',(0.,1.,0.)) ;
#83773 = DIRECTION('ref_axis',(1.,0.,0.)) ;
#83774 = DIRECTION('center_axis',(1.,-8.50781193244945E-15,0.)) ;
#83775 = DIRECTION('ref_axis',(8.50781193244945E-15,1.,0.)) ;
#83776 = DIRECTION('center_axis',(0.,1.,0.)) ;
#83777 = DIRECTION('ref_axis',(1.,0.,0.)) ;
#83778 = DIRECTION('center_axis',(-5.42101086242753E-16,1.70882313734897E-16,
1.)) ;
#83779 = DIRECTION('ref_axis',(1.,9.26354878953623E-32,5.42101086242753E-16)) ;
#83780 = DIRECTION('center_axis',(-1.,0.,0.)) ;
#83781 = DIRECTION('ref_axis',(0.,0.,1.)) ;
#83782 = DIRECTION('center_axis',(1.,0.,0.)) ;
#83783 = DIRECTION('ref_axis',(0.,0.,-1.)) ;
#83784 = DIRECTION('center_axis',(0.,0.,-1.)) ;
#83785 = DIRECTION('ref_axis',(-1.,0.,0.)) ;
#83786 = DIRECTION('center_axis',(0.,0.,1.)) ;
#83787 = DIRECTION('ref_axis',(1.,0.,0.)) ;
#83788 = DIRECTION('center_axis',(0.,1.,0.)) ;
#83789 = DIRECTION('ref_axis',(1.,0.,0.)) ;
#83790 = DIRECTION('center_axis',(0.,1.,0.)) ;
#83791 = DIRECTION('ref_axis',(1.,0.,0.)) ;
#83792 = DIRECTION('center_axis',(0.,0.,-1.)) ;
#83793 = DIRECTION('ref_axis',(-1.,0.,0.)) ;
#83794 = DIRECTION('center_axis',(0.,1.,0.)) ;
#83795 = DIRECTION('ref_axis',(0.,0.,1.)) ;
#83796 = DIRECTION('center_axis',(0.,0.,-1.)) ;
#83797 = DIRECTION('ref_axis',(-1.,0.,0.)) ;
#83798 = DIRECTION('center_axis',(0.,0.,1.)) ;
#83799 = DIRECTION('ref_axis',(1.,0.,0.)) ;
#83800 = DIRECTION('center_axis',(1.33440267382831E-16,1.,0.)) ;
#83801 = DIRECTION('ref_axis',(-1.,1.33440267382831E-16,0.)) ;
#83802 = DIRECTION('center_axis',(0.,1.,0.)) ;
#83803 = DIRECTION('ref_axis',(0.,0.,1.)) ;
#83804 = DIRECTION('center_axis',(0.,1.,0.)) ;
#83805 = DIRECTION('ref_axis',(1.,0.,0.)) ;
#83806 = DIRECTION('center_axis',(0.,1.,0.)) ;
#83807 = DIRECTION('ref_axis',(0.,0.,1.)) ;
#83808 = DIRECTION('center_axis',(0.,1.,0.)) ;
#83809 = DIRECTION('ref_axis',(1.,0.,0.)) ;
#83810 = DIRECTION('center_axis',(1.37797793267296E-15,-1.62630325872825E-15,
1.)) ;
#83811 = DIRECTION('ref_axis',(-2.24101000236165E-30,-1.,-1.62630325872825E-15)) ;
#83812 = DIRECTION('center_axis',(-1.33440267382831E-16,-1.,0.)) ;
#83813 = DIRECTION('ref_axis',(1.,-1.33440267382831E-16,0.)) ;
#83814 = DIRECTION('center_axis',(0.,1.,0.)) ;
#83815 = DIRECTION('ref_axis',(0.,0.,1.)) ;
#83816 = DIRECTION('center_axis',(0.,0.,-1.)) ;
#83817 = DIRECTION('ref_axis',(-1.,0.,0.)) ;
#83818 = DIRECTION('center_axis',(0.,0.,1.)) ;
#83819 = DIRECTION('ref_axis',(1.,0.,0.)) ;
#83820 = DIRECTION('center_axis',(0.,1.,0.)) ;
#83821 = DIRECTION('ref_axis',(1.,0.,0.)) ;
#83822 = DIRECTION('center_axis',(0.,0.,1.)) ;
#83823 = DIRECTION('ref_axis',(1.,0.,0.)) ;
#83824 = DIRECTION('center_axis',(0.,0.,1.)) ;
#83825 = DIRECTION('ref_axis',(1.,0.,0.)) ;
#83826 = DIRECTION('center_axis',(0.,0.,1.)) ;
#83827 = DIRECTION('ref_axis',(-0.986393923832144,0.164398987305354,0.)) ;
#83828 = DIRECTION('center_axis',(0.984701787439272,-0.164116964573205,-0.0585492250433871)) ;
#83829 = DIRECTION('ref_axis',(0.16439898730535,0.986393923832145,-3.2807868055655E-16)) ;
#83830 = DIRECTION('center_axis',(0.984834538781259,-0.164139089796881,-0.0562075655419907)) ;
#83831 = DIRECTION('ref_axis',(0.164398987305362,0.986393923832143,6.03508511856301E-17)) ;
#83832 = DIRECTION('center_axis',(0.,0.,1.)) ;
#83833 = DIRECTION('ref_axis',(-0.986393923832144,0.164398987305354,0.)) ;
#83834 = DIRECTION('center_axis',(0.,0.,1.)) ;
#83835 = DIRECTION('ref_axis',(1.,0.,0.)) ;
#83836 = DIRECTION('center_axis',(0.342346838789899,0.100237737301556,-0.934211452504853)) ;
#83837 = DIRECTION('ref_axis',(0.878411850385613,0.318727802083594,0.356097190779547)) ;
#83838 = DIRECTION('center_axis',(0.,0.,-1.)) ;
#83839 = DIRECTION('ref_axis',(-1.,0.,0.)) ;
#83840 = DIRECTION('center_axis',(0.,0.,-1.)) ;
#83841 = DIRECTION('ref_axis',(-1.,0.,0.)) ;
#83842 = DIRECTION('center_axis',(0.,0.,-1.)) ;
#83843 = DIRECTION('ref_axis',(-1.,0.,0.)) ;
#83844 = DIRECTION('center_axis',(-0.342346838789825,-0.100237737307746,-0.934211452504216)) ;
#83845 = DIRECTION('ref_axis',(0.878411777618972,0.318728007761553,-0.356097186184654)) ;
#83846 = DIRECTION('center_axis',(0.,0.,1.)) ;
#83847 = DIRECTION('ref_axis',(1.,0.,0.)) ;
#83848 = DIRECTION('center_axis',(0.967224433240076,0.25169685099469,0.0335498277606827)) ;
#83849 = DIRECTION('ref_axis',(0.148186139673085,-0.66680383883963,0.730351633473576)) ;
#83850 = DIRECTION('center_axis',(0.,0.707106781186549,-0.707106781186547)) ;
#83851 = DIRECTION('ref_axis',(0.,0.707106781186546,0.707106781186549)) ;
#83852 = DIRECTION('center_axis',(0.978007532938602,-0.147978541149587,-0.146981688909158)) ;
#83853 = DIRECTION('ref_axis',(0.193734423938717,0.383507624691585,0.902988856401092)) ;
#83854 = DIRECTION('center_axis',(0.,0.447213595499958,0.894427190999916)) ;
#83855 = DIRECTION('ref_axis',(0.,-0.894427190999916,0.447213595499958)) ;
#83856 = DIRECTION('center_axis',(0.960001452008135,0.250435160947725,-0.125217579849475)) ;
#83857 = DIRECTION('ref_axis',(0.276742394168204,-0.916645079797436,0.288401534242108)) ;
#83858 = DIRECTION('center_axis',(0.,1.,0.)) ;
#83859 = DIRECTION('ref_axis',(0.,0.,1.)) ;
#83860 = DIRECTION('center_axis',(-1.,0.,0.)) ;
#83861 = DIRECTION('ref_axis',(0.,0.413905168515859,-0.910320004984982)) ;
#83862 = DIRECTION('center_axis',(1.,1.44560289664734E-16,0.)) ;
#83863 = DIRECTION('ref_axis',(0.,1.,0.)) ;
#83864 = DIRECTION('center_axis',(1.,1.44560289664734E-16,0.)) ;
#83865 = DIRECTION('ref_axis',(-1.44560289664734E-16,1.,0.)) ;
#83866 = DIRECTION('center_axis',(0.,0.,-1.)) ;
#83867 = DIRECTION('ref_axis',(0.,-1.,0.)) ;
#83868 = DIRECTION('center_axis',(-1.,-1.44560289664734E-16,0.)) ;
#83869 = DIRECTION('ref_axis',(-1.44560289664734E-16,1.,0.)) ;
#83870 = DIRECTION('center_axis',(1.,-3.46944695195361E-16,0.)) ;
#83871 = DIRECTION('ref_axis',(2.61228946970625E-16,1.,0.)) ;
#83872 = DIRECTION('center_axis',(1.,-3.46944695195361E-16,0.)) ;
#83873 = DIRECTION('ref_axis',(3.46944695195361E-16,1.,0.)) ;
#83874 = DIRECTION('center_axis',(0.,0.,1.)) ;
#83875 = DIRECTION('ref_axis',(-3.26536183713281E-16,-1.,0.)) ;
#83876 = DIRECTION('center_axis',(-1.,3.46944695195361E-16,0.)) ;
#83877 = DIRECTION('ref_axis',(3.46944695195361E-16,1.,0.)) ;
#83878 = DIRECTION('center_axis',(-1.,3.46944695195361E-16,0.)) ;
#83879 = DIRECTION('ref_axis',(-3.46944695195361E-16,-1.,0.)) ;
#83880 = DIRECTION('center_axis',(-1.,0.,0.)) ;
#83881 = DIRECTION('ref_axis',(0.,0.,1.)) ;
#83882 = DIRECTION('',(1.,-3.46944695195361E-16,0.)) ;
#83883 = DIRECTION('center_axis',(-1.,8.01625584951926E-16,-1.08420217248551E-15)) ;
#83884 = DIRECTION('ref_axis',(1.08420217248551E-15,2.16840434497102E-15,
-1.)) ;
#83885 = DIRECTION('center_axis',(-1.,8.01625584951926E-16,-1.08420217248551E-15)) ;
#83886 = DIRECTION('ref_axis',(1.08420217248551E-15,2.16840434497102E-15,
-1.)) ;
#83887 = DIRECTION('',(-1.,3.46944695195361E-16,0.)) ;
#83888 = DIRECTION('center_axis',(-1.,3.46944695195361E-16,0.)) ;
#83889 = DIRECTION('ref_axis',(-3.46944695195361E-16,-1.,0.)) ;
#83890 = DIRECTION('center_axis',(-1.,0.,0.)) ;
#83891 = DIRECTION('ref_axis',(0.,0.,1.)) ;
#83892 = DIRECTION('',(1.,-3.46944695195361E-16,0.)) ;
#83893 = DIRECTION('center_axis',(-1.,2.2680138501079E-15,0.)) ;
#83894 = DIRECTION('ref_axis',(2.2680138501079E-15,1.,0.)) ;
#83895 = DIRECTION('',(-1.,3.46944695195361E-16,0.)) ;
#83896 = DIRECTION('center_axis',(-1.,3.18032637262401E-16,0.)) ;
#83897 = DIRECTION('ref_axis',(-5.55111512312578E-16,-1.,0.)) ;
#83898 = DIRECTION('center_axis',(1.,-3.18032637262401E-16,0.)) ;
#83899 = DIRECTION('ref_axis',(-3.18032637262401E-16,-1.,0.)) ;
#83900 = DIRECTION('center_axis',(-2.01298417874256E-16,-0.632948931301568,
-0.774193548387096)) ;
#83901 = DIRECTION('ref_axis',(1.73472347597681E-14,-0.774193548387096,0.632948931301568)) ;
#83902 = DIRECTION('center_axis',(-1.,3.18032637262401E-16,0.)) ;
#83903 = DIRECTION('ref_axis',(-3.18032637262401E-16,-1.,0.)) ;
#83904 = DIRECTION('center_axis',(-2.01298417874256E-16,-0.632948931301568,
0.774193548387096)) ;
#83905 = DIRECTION('ref_axis',(-2.5982535921668E-30,-0.774193548387096,-0.632948931301568)) ;
#83906 = DIRECTION('center_axis',(1.,1.44560289664734E-16,0.)) ;
#83907 = DIRECTION('ref_axis',(-1.44560289664734E-16,1.,0.)) ;
#83908 = DIRECTION('',(-1.,-1.44560289664734E-16,0.)) ;
#83909 = DIRECTION('center_axis',(-1.,3.46944695195361E-16,0.)) ;
#83910 = DIRECTION('ref_axis',(-3.46944695195361E-16,-1.,0.)) ;
#83911 = DIRECTION('',(-1.,3.46944695195361E-16,0.)) ;
#83912 = DIRECTION('center_axis',(-1.,3.46944695195361E-16,0.)) ;
#83913 = DIRECTION('ref_axis',(3.46944695195361E-16,1.,0.)) ;
#83914 = DIRECTION('center_axis',(-1.,3.46944695195361E-16,0.)) ;
#83915 = DIRECTION('ref_axis',(3.46944695195361E-16,1.,0.)) ;
#83916 = DIRECTION('center_axis',(-1.,3.46944695195361E-16,0.)) ;
#83917 = DIRECTION('ref_axis',(-3.46944695195361E-16,-1.,0.)) ;
#83918 = DIRECTION('',(1.,-3.46944695195361E-16,0.)) ;
#83919 = DIRECTION('center_axis',(-1.,-1.44560289664734E-16,-2.65552944032596E-32)) ;
#83920 = DIRECTION('ref_axis',(1.44560289664734E-16,-1.,-2.80018320648271E-64)) ;
#83921 = DIRECTION('',(2.65552944032596E-32,3.29043518662928E-48,-1.)) ;
#83922 = DIRECTION('',(1.44560289664734E-16,-1.,-2.4093381610789E-16)) ;
#83923 = DIRECTION('',(0.,0.,1.)) ;
#83924 = DIRECTION('center_axis',(0.999999956301289,0.000282786981395913,
8.61913163589487E-5)) ;
#83925 = DIRECTION('ref_axis',(0.000288266391231008,-0.997396273404988,-0.0721151211628269)) ;
#83926 = DIRECTION('',(-1.44560289664734E-16,1.,-7.2280144832367E-17)) ;
#83927 = DIRECTION('center_axis',(0.316227766016838,0.948683298050514,0.)) ;
#83928 = DIRECTION('ref_axis',(-0.948683298050514,0.316227766016838,0.)) ;
#83929 = DIRECTION('',(-0.948683298050514,0.316227766016838,0.)) ;
#83930 = DIRECTION('',(0.,0.,1.)) ;
#83931 = DIRECTION('',(0.937042571331636,-0.312347523777212,-0.156173761888606)) ;
#83932 = DIRECTION('',(0.,0.,-1.)) ;
#83933 = DIRECTION('center_axis',(1.,1.73472347597681E-15,0.)) ;
#83934 = DIRECTION('ref_axis',(-1.73472347597681E-15,1.,0.)) ;
#83935 = DIRECTION('',(-1.73472347597681E-15,1.,0.)) ;
#83936 = DIRECTION('',(0.,0.,1.)) ;
#83937 = DIRECTION('',(1.73472347597681E-15,-1.,-2.89120579329468E-16)) ;
#83938 = DIRECTION('',(0.,0.,-1.)) ;
#83939 = DIRECTION('center_axis',(0.164398987305357,-0.986393923832144,0.)) ;
#83940 = DIRECTION('ref_axis',(0.986393923832144,0.164398987305357,0.)) ;
#83941 = DIRECTION('',(-0.973328526784575,-0.162221421130762,0.162221421130763)) ;
#83942 = DIRECTION('',(0.,0.,-1.)) ;
#83943 = DIRECTION('',(0.986393923832144,0.164398987305357,0.)) ;
#83944 = DIRECTION('',(0.,0.,1.)) ;
#83945 = DIRECTION('center_axis',(-9.91270557701033E-17,1.,0.)) ;
#83946 = DIRECTION('ref_axis',(-1.,-9.91270557701033E-17,0.)) ;
#83947 = DIRECTION('',(1.,9.91270557701033E-17,0.)) ;
#83948 = DIRECTION('',(0.,0.,-1.)) ;
#83949 = DIRECTION('',(-1.,-9.91270557701033E-17,0.)) ;
#83950 = DIRECTION('',(0.,0.,1.)) ;
#83951 = DIRECTION('center_axis',(-9.91270557701033E-17,1.,0.)) ;
#83952 = DIRECTION('ref_axis',(-1.,-9.91270557701033E-17,0.)) ;
#83953 = DIRECTION('',(-1.,-9.91270557701033E-17,0.)) ;
#83954 = DIRECTION('',(0.,0.,-1.)) ;
#83955 = DIRECTION('',(-1.,-9.91270557701033E-17,0.)) ;
#83956 = DIRECTION('',(0.,0.,1.)) ;
#83957 = DIRECTION('center_axis',(1.,1.15648231731787E-15,0.)) ;
#83958 = DIRECTION('ref_axis',(-1.15648231731787E-15,1.,0.)) ;
#83959 = DIRECTION('',(-1.15648231731787E-15,1.,0.)) ;
#83960 = DIRECTION('',(0.,0.,-1.)) ;
#83961 = DIRECTION('',(-1.15648231731787E-15,1.,0.)) ;
#83962 = DIRECTION('',(0.,0.,1.)) ;
#83963 = DIRECTION('center_axis',(-1.,-1.15648231731787E-15,0.)) ;
#83964 = DIRECTION('ref_axis',(-1.15648231731787E-15,1.,0.)) ;
#83965 = DIRECTION('',(0.,0.,1.)) ;
#83966 = DIRECTION('center_axis',(0.,0.,1.)) ;
#83967 = DIRECTION('ref_axis',(1.,0.,0.)) ;
#83968 = DIRECTION('',(-1.,0.,0.)) ;
#83969 = DIRECTION('center_axis',(0.,0.,-1.)) ;
#83970 = DIRECTION('ref_axis',(1.,0.,0.)) ;
#83971 = DIRECTION('center_axis',(0.,0.,-1.)) ;
#83972 = DIRECTION('ref_axis',(1.,0.,0.)) ;
#83973 = DIRECTION('center_axis',(0.,0.,-1.)) ;
#83974 = DIRECTION('ref_axis',(1.,0.,0.)) ;
#83975 = DIRECTION('center_axis',(0.,0.,-1.)) ;
#83976 = DIRECTION('ref_axis',(1.,0.,0.)) ;
#83977 = DIRECTION('',(1.,0.,0.)) ;
#83978 = DIRECTION('center_axis',(0.,0.,1.)) ;
#83979 = DIRECTION('ref_axis',(1.,0.,0.)) ;
#83980 = DIRECTION('',(3.46944695195361E-16,1.,0.)) ;
#83981 = DIRECTION('center_axis',(0.,0.,1.)) ;
#83982 = DIRECTION('ref_axis',(1.,0.,0.)) ;
#83983 = DIRECTION('',(1.,-3.46944695195361E-16,0.)) ;
#83984 = DIRECTION('center_axis',(0.,0.,-1.)) ;
#83985 = DIRECTION('ref_axis',(1.,0.,0.)) ;
#83986 = DIRECTION('',(2.71050543121376E-16,1.,0.)) ;
#83987 = DIRECTION('center_axis',(0.,0.,-1.)) ;
#83988 = DIRECTION('ref_axis',(1.,0.,0.)) ;
#83989 = DIRECTION('',(-1.,3.46944695195361E-16,0.)) ;
#83990 = DIRECTION('center_axis',(0.,0.,1.)) ;
#83991 = DIRECTION('ref_axis',(1.,0.,0.)) ;
#83992 = DIRECTION('',(3.46944695195361E-16,1.,0.)) ;
#83993 = DIRECTION('center_axis',(0.,0.,1.)) ;
#83994 = DIRECTION('ref_axis',(1.,0.,0.)) ;
#83995 = DIRECTION('center_axis',(0.,0.,-1.)) ;
#83996 = DIRECTION('ref_axis',(1.,0.,0.)) ;
#83997 = DIRECTION('',(0.986393923832144,-0.164398987305354,0.)) ;
#83998 = DIRECTION('center_axis',(0.,0.,-1.)) ;
#83999 = DIRECTION('ref_axis',(1.,-6.50521303491307E-15,0.)) ;
#84000 = DIRECTION('center_axis',(0.,0.,-1.)) ;
#84001 = DIRECTION('ref_axis',(1.,0.,0.)) ;
#84002 = DIRECTION('',(1.,0.,0.)) ;
#84003 = DIRECTION('',(1.13380619344889E-16,-1.,0.)) ;
#84004 = DIRECTION('center_axis',(0.,0.,-1.)) ;
#84005 = DIRECTION('ref_axis',(1.,0.,0.)) ;
#84006 = DIRECTION('',(-1.,-1.92747052886312E-16,0.)) ;
#84007 = DIRECTION('center_axis',(0.,0.,1.)) ;
#84008 = DIRECTION('ref_axis',(1.,0.,0.)) ;
#84009 = DIRECTION('',(0.,-1.,0.)) ;
#84010 = DIRECTION('center_axis',(0.,0.,-1.)) ;
#84011 = DIRECTION('ref_axis',(1.,0.,0.)) ;
#84012 = DIRECTION('center_axis',(0.,0.,1.)) ;
#84013 = DIRECTION('ref_axis',(1.,0.,0.)) ;
#84014 = DIRECTION('',(-0.948683298050514,0.316227766016838,0.)) ;
#84015 = DIRECTION('center_axis',(0.,0.,1.)) ;
#84016 = DIRECTION('ref_axis',(1.,0.,0.)) ;
#84017 = DIRECTION('',(-1.,0.,0.)) ;
#84018 = DIRECTION('center_axis',(0.,0.,1.)) ;
#84019 = DIRECTION('ref_axis',(1.,0.,0.)) ;
#84020 = DIRECTION('',(0.,-1.,0.)) ;
#84021 = DIRECTION('center_axis',(0.,0.,-1.)) ;
#84022 = DIRECTION('ref_axis',(1.,0.,0.)) ;
#84023 = DIRECTION('',(-1.,-1.92747052886312E-16,0.)) ;
#84024 = DIRECTION('center_axis',(0.,0.,1.)) ;
#84025 = DIRECTION('ref_axis',(1.,0.,0.)) ;
#84026 = DIRECTION('',(1.13380619344889E-16,-1.,0.)) ;
#84027 = DIRECTION('',(1.,0.,0.)) ;
#84028 = DIRECTION('center_axis',(0.,0.,1.)) ;
#84029 = DIRECTION('ref_axis',(1.,0.,0.)) ;
#84030 = DIRECTION('center_axis',(0.,0.,1.)) ;
#84031 = DIRECTION('ref_axis',(1.,0.,0.)) ;
#84032 = DIRECTION('',(-0.986393923832144,0.164398987305354,0.)) ;
#84033 = DIRECTION('center_axis',(0.,0.,1.)) ;
#84034 = DIRECTION('ref_axis',(1.,0.,0.)) ;
#84035 = DIRECTION('center_axis',(0.,0.,-1.)) ;
#84036 = DIRECTION('ref_axis',(1.,0.,0.)) ;
#84037 = DIRECTION('',(-3.46944695195361E-16,-1.,0.)) ;
#84038 = DIRECTION('center_axis',(0.,0.,-1.)) ;
#84039 = DIRECTION('ref_axis',(1.,0.,0.)) ;
#84040 = DIRECTION('',(-1.,3.46944695195361E-16,0.)) ;
#84041 = DIRECTION('center_axis',(0.,0.,1.)) ;
#84042 = DIRECTION('ref_axis',(1.,0.,0.)) ;
#84043 = DIRECTION('',(3.46944695195361E-16,1.,0.)) ;
#84044 = DIRECTION('center_axis',(0.,0.,1.)) ;
#84045 = DIRECTION('ref_axis',(1.,0.,0.)) ;
#84046 = DIRECTION('',(1.,-3.46944695195361E-16,0.)) ;
#84047 = DIRECTION('center_axis',(0.,0.,-1.)) ;
#84048 = DIRECTION('ref_axis',(1.,0.,0.)) ;
#84049 = DIRECTION('',(-3.46944695195361E-16,-1.,0.)) ;
#84050 = DIRECTION('center_axis',(0.,0.,-1.)) ;
#84051 = DIRECTION('ref_axis',(1.,0.,0.)) ;
#84052 = DIRECTION('',(1.,0.,0.)) ;
#84053 = DIRECTION('center_axis',(0.,0.,1.)) ;
#84054 = DIRECTION('ref_axis',(1.,0.,0.)) ;
#84055 = DIRECTION('',(0.986393923832144,0.164398987305357,0.)) ;
#84056 = DIRECTION('center_axis',(0.,0.,1.)) ;
#84057 = DIRECTION('ref_axis',(1.,0.,0.)) ;
#84058 = DIRECTION('',(-1.73472347597681E-15,1.,0.)) ;
#84059 = DIRECTION('center_axis',(0.,0.,1.)) ;
#84060 = DIRECTION('ref_axis',(1.,0.,0.)) ;
#84061 = DIRECTION('center_axis',(-1.92747052886312E-16,1.,0.)) ;
#84062 = DIRECTION('ref_axis',(-1.,-1.92747052886312E-16,0.)) ;
#84063 = DIRECTION('',(0.,0.,1.)) ;
#84064 = DIRECTION('',(0.,0.,-1.)) ;
#84065 = DIRECTION('center_axis',(-1.,0.,0.)) ;
#84066 = DIRECTION('ref_axis',(0.,0.,1.)) ;
#84067 = DIRECTION('',(0.,0.,1.)) ;
#84068 = DIRECTION('',(0.,0.,-1.)) ;
#84069 = DIRECTION('center_axis',(0.,1.,0.)) ;
#84070 = DIRECTION('ref_axis',(0.,0.,1.)) ;
#84071 = DIRECTION('',(0.,0.,-1.)) ;
#84072 = DIRECTION('',(0.,0.,1.)) ;
#84073 = DIRECTION('',(0.,0.,-1.)) ;
#84074 = DIRECTION('',(0.,0.,-1.)) ;
#84075 = DIRECTION('center_axis',(0.316227766016838,0.948683298050514,0.)) ;
#84076 = DIRECTION('ref_axis',(-0.948683298050514,0.316227766016838,0.)) ;
#84077 = DIRECTION('center_axis',(-0.316227766016857,-0.948683298050507,-2.67178031360003E-14)) ;
#84078 = DIRECTION('ref_axis',(0.831595960751158,-0.277198653583725,-0.48125779423686)) ;
#84079 = DIRECTION('',(0.,0.,1.)) ;
#84080 = DIRECTION('',(0.,0.,-1.)) ;
#84081 = DIRECTION('',(-0.937042571331636,0.312347523777212,-0.156173761888606)) ;
#84082 = DIRECTION('center_axis',(1.,1.73472347597681E-15,0.)) ;
#84083 = DIRECTION('ref_axis',(-1.73472347597681E-15,1.,0.)) ;
#84084 = DIRECTION('',(-1.73472347597681E-15,1.,-2.89120579329468E-16)) ;
#84085 = DIRECTION('',(0.,0.,1.)) ;
#84086 = DIRECTION('',(0.,0.,-1.)) ;
#84087 = DIRECTION('center_axis',(0.164398987305357,-0.986393923832144,0.)) ;
#84088 = DIRECTION('ref_axis',(0.986393923832144,0.164398987305357,0.)) ;
#84089 = DIRECTION('',(0.973328526784575,0.162221421130762,0.162221421130763)) ;
#84090 = DIRECTION('',(0.,0.,1.)) ;
#84091 = DIRECTION('',(0.,0.,-1.)) ;
#84092 = DIRECTION('center_axis',(0.,-1.,0.)) ;
#84093 = DIRECTION('ref_axis',(0.,0.,-1.)) ;
#84094 = DIRECTION('',(0.,0.,1.)) ;
#84095 = DIRECTION('',(0.,0.,1.)) ;
#84096 = DIRECTION('',(0.,0.,1.)) ;
#84097 = DIRECTION('',(0.,0.,-1.)) ;
#84098 = DIRECTION('',(1.,0.,2.25271179641597E-31)) ;
#84099 = DIRECTION('center_axis',(0.,-1.,0.)) ;
#84100 = DIRECTION('ref_axis',(0.,0.,-1.)) ;
#84101 = DIRECTION('',(0.,0.,-1.)) ;
#84102 = DIRECTION('center_axis',(0.,-1.,0.)) ;
#84103 = DIRECTION('ref_axis',(0.,0.,-1.)) ;
#84104 = DIRECTION('',(-1.,0.,-3.21815970916568E-32)) ;
#84105 = DIRECTION('',(0.,0.,-1.)) ;
#84106 = DIRECTION('center_axis',(1.,-3.46944695195361E-16,0.)) ;
#84107 = DIRECTION('ref_axis',(3.46944695195361E-16,1.,0.)) ;
#84108 = DIRECTION('center_axis',(1.,-3.46944695195361E-16,0.)) ;
#84109 = DIRECTION('ref_axis',(3.46944695195361E-16,1.,0.)) ;
#84110 = DIRECTION('',(1.5529910948782E-31,4.47619207437002E-16,-1.)) ;
#84111 = DIRECTION('',(0.,0.,1.)) ;
#84112 = DIRECTION('center_axis',(1.,-3.46944695195361E-16,0.)) ;
#84113 = DIRECTION('ref_axis',(3.46944695195361E-16,1.,0.)) ;
#84114 = DIRECTION('center_axis',(1.,-3.46944695195361E-16,0.)) ;
#84115 = DIRECTION('ref_axis',(3.46944695195361E-16,1.,0.)) ;
#84116 = DIRECTION('center_axis',(1.,-3.46944695195361E-16,0.)) ;
#84117 = DIRECTION('ref_axis',(3.46944695195361E-16,1.,0.)) ;
#84118 = DIRECTION('',(3.46944695195361E-16,1.,9.27571383489107E-17)) ;
#84119 = DIRECTION('',(0.,0.,1.)) ;
#84120 = DIRECTION('',(-3.46944695195361E-16,-1.,-6.49299968442375E-16)) ;
#84121 = DIRECTION('center_axis',(1.,-3.46944695195361E-16,0.)) ;
#84122 = DIRECTION('ref_axis',(3.46944695195361E-16,1.,0.)) ;
#84123 = DIRECTION('center_axis',(1.,-3.46944695195361E-16,0.)) ;
#84124 = DIRECTION('ref_axis',(3.46944695195361E-16,1.,0.)) ;
#84125 = DIRECTION('center_axis',(1.,-3.46944695195361E-16,0.)) ;
#84126 = DIRECTION('ref_axis',(3.46944695195361E-16,1.,0.)) ;
#84127 = DIRECTION('',(0.,0.,1.)) ;
#84128 = DIRECTION('',(-1.5529910948782E-31,-4.47619207437002E-16,-1.)) ;
#84129 = DIRECTION('center_axis',(1.,-3.46944695195361E-16,0.)) ;
#84130 = DIRECTION('ref_axis',(3.46944695195361E-16,1.,0.)) ;
#84131 = DIRECTION('center_axis',(1.,-3.46944695195361E-16,0.)) ;
#84132 = DIRECTION('ref_axis',(3.46944695195361E-16,1.,0.)) ;
#84133 = DIRECTION('center_axis',(1.,-3.46944695195361E-16,0.)) ;
#84134 = DIRECTION('ref_axis',(3.46944695195361E-16,1.,0.)) ;
#84135 = DIRECTION('',(-3.46944695195361E-16,-1.,-1.06487173641454E-15)) ;
#84136 = DIRECTION('center_axis',(1.,-3.46944695195361E-16,0.)) ;
#84137 = DIRECTION('ref_axis',(3.46944695195361E-16,1.,0.)) ;
#84138 = DIRECTION('',(3.46944695195361E-16,1.,2.45739631480277E-16)) ;
#84139 = DIRECTION('center_axis',(1.,-3.46944695195361E-16,0.)) ;
#84140 = DIRECTION('ref_axis',(3.46944695195361E-16,1.,0.)) ;
#84141 = DIRECTION('center_axis',(1.,-3.46944695195361E-16,0.)) ;
#84142 = DIRECTION('ref_axis',(3.46944695195361E-16,1.,0.)) ;
#84143 = DIRECTION('center_axis',(0.,-1.,0.)) ;
#84144 = DIRECTION('ref_axis',(0.,0.,-1.)) ;
#84145 = DIRECTION('center_axis',(0.,-1.,0.)) ;
#84146 = DIRECTION('ref_axis',(0.,0.,-1.)) ;
#84147 = DIRECTION('',(-1.,0.,-1.40488587213121E-32)) ;
#84148 = DIRECTION('',(0.,0.,1.)) ;
#84149 = DIRECTION('',(0.,0.,1.)) ;
#84150 = DIRECTION('',(0.,0.,1.)) ;
#84151 = DIRECTION('',(1.,0.,1.40488587213121E-32)) ;
#84152 = DIRECTION('center_axis',(0.,-1.,0.)) ;
#84153 = DIRECTION('ref_axis',(0.,0.,-1.)) ;
#84154 = DIRECTION('',(7.2280144832367E-17,0.,-1.)) ;
#84155 = DIRECTION('center_axis',(-1.,-1.13380619344889E-16,0.)) ;
#84156 = DIRECTION('ref_axis',(1.13380619344889E-16,-1.,0.)) ;
#84157 = DIRECTION('center_axis',(-1.,-1.13380619344889E-16,0.)) ;
#84158 = DIRECTION('ref_axis',(1.13380619344889E-16,-1.,0.)) ;
#84159 = DIRECTION('',(1.13380619344889E-16,-1.,1.23908819712629E-16)) ;
#84160 = DIRECTION('',(0.,0.,-1.)) ;
#84161 = DIRECTION('',(-1.13380619344889E-16,1.,-1.23908819712629E-16)) ;
#84162 = DIRECTION('center_axis',(-1.,-1.13380619344889E-16,0.)) ;
#84163 = DIRECTION('ref_axis',(1.13380619344889E-16,-1.,0.)) ;
#84164 = DIRECTION('',(0.,0.,1.)) ;
#84165 = DIRECTION('center_axis',(-1.40488587213121E-32,1.23908819712629E-16,
1.)) ;
#84166 = DIRECTION('ref_axis',(0.,-1.,1.23908819712629E-16)) ;
#84167 = DIRECTION('',(-1.,0.,-1.40488587213121E-32)) ;
#84168 = DIRECTION('',(-1.13380619344889E-16,1.,-1.23908819712629E-16)) ;
#84169 = DIRECTION('center_axis',(1.40488587213121E-32,-1.23908819712629E-16,
-1.)) ;
#84170 = DIRECTION('ref_axis',(-1.74077750246726E-48,-1.,1.23908819712629E-16)) ;
#84171 = DIRECTION('center_axis',(1.40488587213121E-32,-1.23908819712629E-16,
-1.)) ;
#84172 = DIRECTION('ref_axis',(0.,1.,-1.23908819712629E-16)) ;
#84173 = DIRECTION('center_axis',(-1.40488587213121E-32,1.23908819712629E-16,
1.)) ;
#84174 = DIRECTION('ref_axis',(1.74077750246726E-48,1.,-1.23908819712629E-16)) ;
#84175 = DIRECTION('',(1.13380619344889E-16,-1.,1.23908819712629E-16)) ;
#84176 = DIRECTION('',(1.,0.,1.40488587213121E-32)) ;
#84177 = DIRECTION('center_axis',(-1.,-1.23908819712629E-16,-8.95614743483648E-33)) ;
#84178 = DIRECTION('ref_axis',(1.23908819712629E-16,-1.,5.38566640001825E-66)) ;
#84179 = DIRECTION('',(-8.95614743483648E-33,-1.10974565782288E-48,1.)) ;
#84180 = DIRECTION('',(1.23908819712629E-16,-1.,7.2280144832367E-17)) ;
#84181 = DIRECTION('',(-8.95614743483648E-33,0.,1.)) ;
#84182 = DIRECTION('',(-1.23908819712629E-16,1.,-1.23908819712629E-16)) ;
#84183 = DIRECTION('',(8.95614743483648E-33,1.0154535431059E-48,-1.)) ;
#84184 = DIRECTION('',(1.23908819712629E-16,-1.,1.23908819712629E-16)) ;
#84185 = DIRECTION('',(-8.95614743483648E-33,0.,1.)) ;
#84186 = DIRECTION('',(-1.23908819712629E-16,1.,2.4093381610789E-16)) ;
#84187 = DIRECTION('center_axis',(-1.7912294869673E-32,7.2280144832367E-17,
1.)) ;
#84188 = DIRECTION('ref_axis',(0.,-1.,7.2280144832367E-17)) ;
#84189 = DIRECTION('',(-1.23908819712629E-16,1.,-7.2280144832367E-17)) ;
#84190 = DIRECTION('',(1.,1.23908819712629E-16,8.95614743483648E-33)) ;
#84191 = DIRECTION('',(1.44560289664734E-16,-1.,7.2280144832367E-17)) ;
#84192 = DIRECTION('',(-1.,0.,-1.7912294869673E-32)) ;
#84193 = DIRECTION('center_axis',(-2.08976773479518E-32,2.4093381610789E-16,
-1.)) ;
#84194 = DIRECTION('ref_axis',(0.,1.,2.4093381610789E-16)) ;
#84195 = DIRECTION('',(-1.44560289664734E-16,1.,2.4093381610789E-16)) ;
#84196 = DIRECTION('',(-1.,-1.23908819712629E-16,-8.95614743483648E-33)) ;
#84197 = DIRECTION('',(1.23908819712629E-16,-1.,-2.4093381610789E-16)) ;
#84198 = DIRECTION('',(1.,0.,-2.08976773479518E-32)) ;
#84199 = DIRECTION('center_axis',(-1.23908819712629E-16,1.,0.)) ;
#84200 = DIRECTION('ref_axis',(-1.,-1.23908819712629E-16,0.)) ;
#84201 = DIRECTION('',(8.95614743483648E-33,1.10974565782288E-48,-1.)) ;
#84202 = DIRECTION('',(1.,1.23908819712629E-16,8.95614743483648E-33)) ;
#84203 = DIRECTION('',(-2.65552944032596E-32,-3.29043518662928E-48,1.)) ;
#84204 = DIRECTION('',(-1.,-1.23908819712629E-16,-8.95614743483648E-33)) ;
#84205 = DIRECTION('center_axis',(-1.,-1.44560289664734E-16,-2.65552944032596E-32)) ;
#84206 = DIRECTION('ref_axis',(1.44560289664734E-16,-1.,-2.80018320648271E-64)) ;
#84207 = DIRECTION('',(1.44560289664734E-16,-1.,-2.4093381610789E-16)) ;
#84208 = DIRECTION('',(-2.65552944032596E-32,0.,1.)) ;
#84209 = DIRECTION('',(-1.44560289664734E-16,1.,-7.2280144832367E-17)) ;
#84210 = DIRECTION('',(0.,0.,-1.)) ;
#84211 = DIRECTION('center_axis',(0.,1.,0.)) ;
#84212 = DIRECTION('ref_axis',(0.,0.,1.)) ;
#84213 = DIRECTION('',(8.95614743483648E-33,0.,-1.)) ;
#84214 = DIRECTION('',(1.,0.,1.40488587213121E-32)) ;
#84215 = DIRECTION('',(-7.2280144832367E-17,0.,1.)) ;
#84216 = DIRECTION('',(-1.,0.,-1.40488587213121E-32)) ;
#84217 = DIRECTION('',(8.95614743483648E-33,0.,-1.)) ;
#84218 = DIRECTION('',(1.,0.,1.7912294869673E-32)) ;
#84219 = DIRECTION('',(2.65552944032596E-32,0.,-1.)) ;
#84220 = DIRECTION('',(-1.,0.,2.08976773479518E-32)) ;
#84221 = DIRECTION('center_axis',(1.,1.44560289664734E-16,0.)) ;
#84222 = DIRECTION('ref_axis',(-1.44560289664734E-16,1.,0.)) ;
#84223 = DIRECTION('',(1.44560289664734E-16,-1.,0.)) ;
#84224 = DIRECTION('center_axis',(-1.,-1.44560289664734E-16,0.)) ;
#84225 = DIRECTION('ref_axis',(-1.44560289664734E-16,1.,-5.20417042793041E-14)) ;
#84226 = DIRECTION('',(0.,0.,-1.)) ;
#84227 = DIRECTION('center_axis',(-1.,-1.44560289664734E-16,0.)) ;
#84228 = DIRECTION('ref_axis',(-1.44560289664734E-16,1.,0.)) ;
#84229 = DIRECTION('',(1.44560289664734E-16,-1.,0.)) ;
#84230 = DIRECTION('center_axis',(-1.,-1.44560289664734E-16,0.)) ;
#84231 = DIRECTION('ref_axis',(-1.44560289664734E-16,1.,0.)) ;
#84232 = DIRECTION('',(0.,0.,1.)) ;
#84233 = DIRECTION('center_axis',(-1.,-1.44560289664734E-16,0.)) ;
#84234 = DIRECTION('ref_axis',(-1.44560289664734E-16,1.,0.)) ;
#84235 = DIRECTION('center_axis',(1.,-3.46944695195361E-16,0.)) ;
#84236 = DIRECTION('ref_axis',(3.46944695195361E-16,1.,0.)) ;
#84237 = DIRECTION('center_axis',(1.,-3.46944695195361E-16,0.)) ;
#84238 = DIRECTION('ref_axis',(3.46944695195361E-16,1.,0.)) ;
#84239 = DIRECTION('',(0.,0.,-1.)) ;
#84240 = DIRECTION('',(-1.5529910948782E-31,-4.47619207437002E-16,1.)) ;
#84241 = DIRECTION('center_axis',(-1.,3.46944695195361E-16,0.)) ;
#84242 = DIRECTION('ref_axis',(3.46944695195361E-16,1.,-1.87537673078574E-15)) ;
#84243 = DIRECTION('',(-3.46944695195361E-16,-1.,-2.45739631480277E-16)) ;
#84244 = DIRECTION('center_axis',(1.,-3.46944695195361E-16,0.)) ;
#84245 = DIRECTION('ref_axis',(3.46944695195361E-16,1.,0.)) ;
#84246 = DIRECTION('center_axis',(3.46944695195361E-16,1.,4.47619207437002E-16)) ;
#84247 = DIRECTION('ref_axis',(-8.18685017503995E-48,-4.47619207437002E-16,
1.)) ;
#84248 = DIRECTION('',(-1.5529910948782E-31,-4.47619207437002E-16,1.)) ;
#84249 = DIRECTION('',(-1.,3.46944695195361E-16,0.)) ;
#84250 = DIRECTION('',(1.5529910948782E-31,4.47619207437002E-16,-1.)) ;
#84251 = DIRECTION('center_axis',(-8.52580615413453E-32,-2.45739631480277E-16,
1.)) ;
#84252 = DIRECTION('ref_axis',(0.,-1.,-2.45739631480277E-16)) ;
#84253 = DIRECTION('',(1.,-3.46944695195361E-16,0.)) ;
#84254 = DIRECTION('',(-3.46944695195361E-16,-1.,-2.45739631480277E-16)) ;
#84255 = DIRECTION('',(3.46944695195361E-16,1.,2.45739631480277E-16)) ;
#84256 = DIRECTION('center_axis',(1.,-3.46944695195361E-16,0.)) ;
#84257 = DIRECTION('ref_axis',(3.46944695195361E-16,1.,0.)) ;
#84258 = DIRECTION('center_axis',(1.,-3.46944695195361E-16,0.)) ;
#84259 = DIRECTION('ref_axis',(3.46944695195361E-16,1.,0.)) ;
#84260 = DIRECTION('',(1.,-3.46944695195361E-16,0.)) ;
#84261 = DIRECTION('center_axis',(-1.,3.46944695195361E-16,0.)) ;
#84262 = DIRECTION('ref_axis',(3.46944695195361E-16,1.,1.98254111540207E-15)) ;
#84263 = DIRECTION('',(-1.,3.46944695195361E-16,0.)) ;
#84264 = DIRECTION('center_axis',(1.,-3.46944695195361E-16,0.)) ;
#84265 = DIRECTION('ref_axis',(3.46944695195361E-16,1.,0.)) ;
#84266 = DIRECTION('center_axis',(1.,-3.46944695195361E-16,0.)) ;
#84267 = DIRECTION('ref_axis',(-3.46944695195361E-16,-1.,-9.91270557701033E-16)) ;
#84268 = DIRECTION('',(1.,-3.46944695195361E-16,0.)) ;
#84269 = DIRECTION('center_axis',(-1.,3.46944695195361E-16,0.)) ;
#84270 = DIRECTION('ref_axis',(3.46944695195361E-16,1.,4.95635278850516E-15)) ;
#84271 = DIRECTION('',(-1.,3.46944695195361E-16,0.)) ;
#84272 = DIRECTION('center_axis',(3.69451600012496E-31,1.06487173641454E-15,
-1.)) ;
#84273 = DIRECTION('ref_axis',(0.,1.,1.06487173641454E-15)) ;
#84274 = DIRECTION('',(3.46944695195361E-16,1.,1.06487173641454E-15)) ;
#84275 = DIRECTION('',(-1.,3.46944695195361E-16,0.)) ;
#84276 = DIRECTION('',(-3.46944695195361E-16,-1.,-1.06487173641454E-15)) ;
#84277 = DIRECTION('center_axis',(3.46944695195361E-16,1.,-4.47619207437002E-16)) ;
#84278 = DIRECTION('ref_axis',(8.18685017503995E-48,4.47619207437002E-16,
1.)) ;
#84279 = DIRECTION('',(1.,-3.46944695195361E-16,0.)) ;
#84280 = DIRECTION('',(1.5529910948782E-31,4.47619207437002E-16,1.)) ;
#84281 = DIRECTION('',(-1.5529910948782E-31,-4.47619207437002E-16,-1.)) ;
#84282 = DIRECTION('center_axis',(-1.,3.46944695195361E-16,0.)) ;
#84283 = DIRECTION('ref_axis',(-3.46944695195361E-16,-1.,0.)) ;
#84284 = DIRECTION('center_axis',(-1.,3.46944695195361E-16,0.)) ;
#84285 = DIRECTION('ref_axis',(-3.46944695195361E-16,-1.,0.)) ;
#84286 = DIRECTION('',(1.5529910948782E-31,4.47619207437002E-16,1.)) ;
#84287 = DIRECTION('',(0.,0.,-1.)) ;
#84288 = DIRECTION('center_axis',(1.,-3.46944695195361E-16,0.)) ;
#84289 = DIRECTION('ref_axis',(-3.46944695195361E-16,-1.,0.)) ;
#84290 = DIRECTION('center_axis',(1.,-3.46944695195361E-16,0.)) ;
#84291 = DIRECTION('ref_axis',(-3.46944695195361E-16,-1.,0.)) ;
#84292 = DIRECTION('',(3.46944695195361E-16,1.,1.06487173641454E-15)) ;
#84293 = DIRECTION('center_axis',(1.,-3.46944695195361E-16,0.)) ;
#84294 = DIRECTION('ref_axis',(3.46944695195361E-16,1.,0.)) ;
#84295 = DIRECTION('center_axis',(-1.,3.46944695195361E-16,0.)) ;
#84296 = DIRECTION('ref_axis',(3.46944695195361E-16,1.,0.)) ;
#84297 = DIRECTION('',(0.,0.,-1.)) ;
#84298 = DIRECTION('',(0.,0.,1.)) ;
#84299 = DIRECTION('',(-3.46944695195361E-16,-1.,-9.27571383489107E-17)) ;
#84300 = DIRECTION('center_axis',(-3.46944695195361E-16,-1.,0.)) ;
#84301 = DIRECTION('ref_axis',(1.,-3.46944695195361E-16,0.)) ;
#84302 = DIRECTION('',(1.,-3.46944695195361E-16,0.)) ;
#84303 = DIRECTION('',(0.,0.,-1.)) ;
#84304 = DIRECTION('',(0.,0.,1.)) ;
#84305 = DIRECTION('center_axis',(1.,-3.46944695195361E-16,0.)) ;
#84306 = DIRECTION('ref_axis',(3.46944695195361E-16,1.,0.)) ;
#84307 = DIRECTION('center_axis',(1.,-3.46944695195361E-16,0.)) ;
#84308 = DIRECTION('ref_axis',(3.46944695195361E-16,1.,0.)) ;
#84309 = DIRECTION('',(1.,-3.46944695195361E-16,0.)) ;
#84310 = DIRECTION('center_axis',(-1.,3.46944695195361E-16,0.)) ;
#84311 = DIRECTION('ref_axis',(3.46944695195361E-16,1.,0.)) ;
#84312 = DIRECTION('',(-1.,3.46944695195361E-16,0.)) ;
#84313 = DIRECTION('center_axis',(-3.21815970916568E-32,-9.27571383489107E-17,
1.)) ;
#84314 = DIRECTION('ref_axis',(0.,-1.,-9.27571383489107E-17)) ;
#84315 = DIRECTION('',(3.46944695195361E-16,1.,9.27571383489107E-17)) ;
#84316 = DIRECTION('',(1.,0.,3.21815970916568E-32)) ;
#84317 = DIRECTION('',(-3.46944695195361E-16,-1.,-9.27571383489107E-17)) ;
#84318 = DIRECTION('',(-1.,3.46944695195361E-16,0.)) ;
#84319 = DIRECTION('center_axis',(1.,-3.46944695195361E-16,0.)) ;
#84320 = DIRECTION('ref_axis',(3.46944695195361E-16,1.,0.)) ;
#84321 = DIRECTION('center_axis',(1.,-3.46944695195361E-16,0.)) ;
#84322 = DIRECTION('ref_axis',(-3.46944695195361E-16,-1.,-2.9738116731031E-15)) ;
#84323 = DIRECTION('',(1.,-3.46944695195361E-16,0.)) ;
#84324 = DIRECTION('center_axis',(-1.,3.46944695195361E-16,0.)) ;
#84325 = DIRECTION('ref_axis',(3.46944695195361E-16,1.,-1.98254111540207E-15)) ;
#84326 = DIRECTION('',(-1.,3.46944695195361E-16,0.)) ;
#84327 = DIRECTION('center_axis',(-3.46944695195361E-16,-1.,0.)) ;
#84328 = DIRECTION('ref_axis',(1.,-3.46944695195361E-16,0.)) ;
#84329 = DIRECTION('',(0.,0.,-1.)) ;
#84330 = DIRECTION('',(-1.,3.46944695195361E-16,0.)) ;
#84331 = DIRECTION('',(0.,0.,1.)) ;
#84332 = DIRECTION('center_axis',(2.25271179641597E-31,6.49299968442375E-16,
-1.)) ;
#84333 = DIRECTION('ref_axis',(0.,1.,6.49299968442375E-16)) ;
#84334 = DIRECTION('',(3.46944695195361E-16,1.,6.49299968442375E-16)) ;
#84335 = DIRECTION('',(-1.,0.,-2.25271179641597E-31)) ;
#84336 = DIRECTION('',(-3.46944695195361E-16,-1.,-6.49299968442375E-16)) ;
#84337 = DIRECTION('',(1.,-3.46944695195361E-16,0.)) ;
#84338 = DIRECTION('center_axis',(-1.,3.46944695195361E-16,0.)) ;
#84339 = DIRECTION('ref_axis',(-3.46944695195361E-16,-1.,0.)) ;
#84340 = DIRECTION('',(3.46944695195361E-16,1.,6.49299968442375E-16)) ;
#84341 = DIRECTION('',(0.,0.,1.)) ;
#84342 = DIRECTION('',(0.,0.,-1.)) ;
#84343 = DIRECTION('center_axis',(-1.,3.46944695195361E-16,0.)) ;
#84344 = DIRECTION('ref_axis',(-3.46944695195361E-16,-1.,0.)) ;
#84345 = DIRECTION('center_axis',(-0.164398987305357,0.,-0.986393923832144)) ;
#84346 = DIRECTION('ref_axis',(-0.986393923832144,0.,0.164398987305357)) ;
#84347 = DIRECTION('',(-0.937042571331636,0.312347523777212,0.156173761888606)) ;
#84348 = DIRECTION('',(0.,-1.,0.)) ;
#84349 = DIRECTION('',(0.973328526784575,0.162221421130762,-0.162221421130763)) ;
#84350 = DIRECTION('',(-1.73472347597681E-15,1.,2.89120579329468E-16)) ;
#84351 = DIRECTION('center_axis',(-1.,0.,0.)) ;
#84352 = DIRECTION('ref_axis',(0.,0.,1.)) ;
#84353 = DIRECTION('center_axis',(-1.,0.,0.)) ;
#84354 = DIRECTION('ref_axis',(0.,0.958782009816033,-0.284142671299347)) ;
#84355 = DIRECTION('',(0.,0.,1.)) ;
#84356 = DIRECTION('',(0.,-1.,0.)) ;
#84357 = DIRECTION('center_axis',(-1.,0.,0.)) ;
#84358 = DIRECTION('ref_axis',(0.,0.758706765780369,-0.65143230159326)) ;
#84359 = DIRECTION('',(0.,0.,-1.)) ;
#84360 = DIRECTION('center_axis',(-1.,0.,0.)) ;
#84361 = DIRECTION('ref_axis',(0.,-0.654778303469126,-0.755820992898512)) ;
#84362 = DIRECTION('',(0.,1.,0.)) ;
#84363 = DIRECTION('center_axis',(-0.164398987305357,0.,0.986393923832144)) ;
#84364 = DIRECTION('ref_axis',(0.986393923832144,0.,0.164398987305357)) ;
#84365 = DIRECTION('',(-0.973328526784575,-0.162221421130762,-0.162221421130763)) ;
#84366 = DIRECTION('',(0.,1.,0.)) ;
#84367 = DIRECTION('',(0.937042571331636,-0.312347523777212,0.156173761888606)) ;
#84368 = DIRECTION('',(1.73472347597681E-15,-1.,2.89120579329468E-16)) ;
#84369 = DIRECTION('center_axis',(-0.573462344363329,0.81923192051904,0.)) ;
#84370 = DIRECTION('ref_axis',(-0.81923192051904,-0.573462344363329,0.)) ;
#84371 = DIRECTION('',(-0.710669054518702,-0.497468338163091,0.49746833816309)) ;
#84372 = DIRECTION('',(0.,0.,-1.)) ;
#84373 = DIRECTION('',(0.710669054518702,0.497468338163091,0.49746833816309)) ;
#84374 = DIRECTION('',(0.,0.,1.)) ;
#84375 = DIRECTION('center_axis',(-1.,0.,0.)) ;
#84376 = DIRECTION('ref_axis',(0.,0.,1.)) ;
#84377 = DIRECTION('',(0.,0.,1.)) ;
#84378 = DIRECTION('',(0.,-1.,-9.34081871679819E-17)) ;
#84379 = DIRECTION('',(0.,0.,-1.)) ;
#84380 = DIRECTION('',(0.,1.,-9.34081871679819E-17)) ;
#84381 = DIRECTION('center_axis',(-0.573462344363329,-0.81923192051904,0.)) ;
#84382 = DIRECTION('ref_axis',(0.81923192051904,-0.573462344363329,0.)) ;
#84383 = DIRECTION('',(-0.710669054518701,0.497468338163091,-0.497468338163091)) ;
#84384 = DIRECTION('',(0.,0.,1.)) ;
#84385 = DIRECTION('',(0.710669054518701,-0.497468338163091,-0.497468338163091)) ;
#84386 = DIRECTION('',(0.,0.,-1.)) ;
#84387 = DIRECTION('center_axis',(0.,0.,1.)) ;
#84388 = DIRECTION('ref_axis',(1.,0.,0.)) ;
#84389 = DIRECTION('',(1.,6.67201336914158E-17,0.)) ;
#84390 = DIRECTION('',(1.33440267382831E-16,1.,0.)) ;
#84391 = DIRECTION('',(-1.,1.33440267382831E-16,0.)) ;
#84392 = DIRECTION('center_axis',(0.,0.,1.)) ;
#84393 = DIRECTION('ref_axis',(1.,0.,0.)) ;
#84394 = DIRECTION('',(1.,-1.33440267382831E-16,0.)) ;
#84395 = DIRECTION('',(-1.33440267382831E-16,-1.,0.)) ;
#84396 = DIRECTION('',(-1.,-6.67201336914158E-17,0.)) ;
#84397 = DIRECTION('center_axis',(-6.67201336914158E-17,1.,0.)) ;
#84398 = DIRECTION('ref_axis',(-1.,-6.67201336914158E-17,0.)) ;
#84399 = DIRECTION('',(1.,6.67201336914158E-17,0.)) ;
#84400 = DIRECTION('',(0.,0.,1.)) ;
#84401 = DIRECTION('',(-1.,-6.67201336914158E-17,0.)) ;
#84402 = DIRECTION('center_axis',(-1.33440267382831E-16,-1.,0.)) ;
#84403 = DIRECTION('ref_axis',(1.,-1.33440267382831E-16,0.)) ;
#84404 = DIRECTION('',(1.,-1.33440267382831E-16,0.)) ;
#84405 = DIRECTION('',(0.,0.,-1.)) ;
#84406 = DIRECTION('',(-1.,1.33440267382831E-16,0.)) ;
#84407 = DIRECTION('center_axis',(0.,0.,1.)) ;
#84408 = DIRECTION('ref_axis',(1.,0.,0.)) ;
#84409 = DIRECTION('',(0.,-1.,0.)) ;
#84410 = DIRECTION('',(1.,0.,0.)) ;
#84411 = DIRECTION('',(0.,1.,0.)) ;
#84412 = DIRECTION('center_axis',(0.,0.,-1.)) ;
#84413 = DIRECTION('ref_axis',(1.,0.,0.)) ;
#84414 = DIRECTION('',(-1.44560289664734E-16,1.,-7.2280144832367E-17)) ;
#84415 = DIRECTION('center_axis',(0.,0.,1.)) ;
#84416 = DIRECTION('ref_axis',(1.,0.,0.)) ;
#84417 = DIRECTION('center_axis',(0.,0.,1.)) ;
#84418 = DIRECTION('ref_axis',(1.,0.,0.)) ;
#84419 = DIRECTION('',(0.,-1.,0.)) ;
#84420 = DIRECTION('',(-1.,0.,0.)) ;
#84421 = DIRECTION('',(0.,1.,0.)) ;
#84422 = DIRECTION('center_axis',(0.,0.,-1.)) ;
#84423 = DIRECTION('ref_axis',(1.,-1.82602471155453E-15,0.)) ;
#84424 = DIRECTION('',(1.44560289664734E-16,-1.,-2.4093381610789E-16)) ;
#84425 = DIRECTION('center_axis',(0.,0.,1.)) ;
#84426 = DIRECTION('ref_axis',(1.,0.,0.)) ;
#84427 = DIRECTION('center_axis',(0.,0.,-1.)) ;
#84428 = DIRECTION('ref_axis',(-1.,0.,0.)) ;
#84429 = DIRECTION('',(0.,0.,-1.)) ;
#84430 = DIRECTION('center_axis',(0.,0.,-1.)) ;
#84431 = DIRECTION('ref_axis',(1.,0.,0.)) ;
#84432 = DIRECTION('center_axis',(0.,0.,1.)) ;
#84433 = DIRECTION('ref_axis',(1.,0.,0.)) ;
#84434 = DIRECTION('center_axis',(1.,0.,0.)) ;
#84435 = DIRECTION('ref_axis',(0.,0.,-1.)) ;
#84436 = DIRECTION('',(0.,-1.,0.)) ;
#84437 = DIRECTION('',(0.,0.,1.)) ;
#84438 = DIRECTION('',(0.,1.,0.)) ;
#84439 = DIRECTION('center_axis',(0.81923192051904,0.573462344363329,0.)) ;
#84440 = DIRECTION('ref_axis',(-0.573462344363329,0.81923192051904,0.)) ;
#84441 = DIRECTION('',(-0.497468338163091,0.710669054518701,0.497468338163091)) ;
#84442 = DIRECTION('',(0.,0.,-1.)) ;
#84443 = DIRECTION('',(0.497468338163091,-0.710669054518701,0.497468338163091)) ;
#84444 = DIRECTION('',(0.,0.,1.)) ;
#84445 = DIRECTION('center_axis',(0.,1.,0.)) ;
#84446 = DIRECTION('ref_axis',(0.,0.,1.)) ;
#84447 = DIRECTION('',(0.,0.,1.)) ;
#84448 = DIRECTION('',(-1.,0.,0.)) ;
#84449 = DIRECTION('',(0.,0.,-1.)) ;
#84450 = DIRECTION('',(1.,0.,0.)) ;
#84451 = DIRECTION('center_axis',(-0.81923192051904,0.573462344363329,0.)) ;
#84452 = DIRECTION('ref_axis',(-0.573462344363329,-0.81923192051904,0.)) ;
#84453 = DIRECTION('',(0.497468338163091,0.710669054518701,-0.497468338163091)) ;
#84454 = DIRECTION('',(0.,0.,1.)) ;
#84455 = DIRECTION('',(-0.497468338163091,-0.710669054518701,-0.497468338163091)) ;
#84456 = DIRECTION('',(0.,0.,-1.)) ;
#84457 = DIRECTION('center_axis',(-1.,0.,0.)) ;
#84458 = DIRECTION('ref_axis',(0.,0.,1.)) ;
#84459 = DIRECTION('',(0.,-1.,0.)) ;
#84460 = DIRECTION('',(0.,0.,-1.)) ;
#84461 = DIRECTION('',(0.,1.,0.)) ;
#84462 = DIRECTION('',(0.,0.,-1.)) ;
#84463 = DIRECTION('center_axis',(0.,0.,-1.)) ;
#84464 = DIRECTION('ref_axis',(-1.,0.,0.)) ;
#84465 = DIRECTION('center_axis',(0.,0.,1.)) ;
#84466 = DIRECTION('ref_axis',(1.,0.,0.)) ;
#84467 = DIRECTION('center_axis',(0.,0.,-1.)) ;
#84468 = DIRECTION('ref_axis',(1.,5.20417042793042E-15,0.)) ;
#84469 = DIRECTION('center_axis',(-0.573462344363328,7.65229685658278E-17,
0.819231920519041)) ;
#84470 = DIRECTION('ref_axis',(0.819231920519041,1.22423955297878E-32,0.573462344363328)) ;
#84471 = DIRECTION('',(-0.710669054518702,-0.497468338163091,-0.497468338163091)) ;
#84472 = DIRECTION('',(1.33440267382831E-16,1.,-2.91413396387194E-34)) ;
#84473 = DIRECTION('',(0.710669054518701,-0.497468338163091,0.497468338163091)) ;
#84474 = DIRECTION('',(5.04890651880155E-33,-1.,9.34081871679819E-17)) ;
#84475 = DIRECTION('center_axis',(-0.573462344363328,7.65229685658278E-17,
-0.819231920519041)) ;
#84476 = DIRECTION('ref_axis',(-0.819231920519041,-1.22423955297878E-32,0.573462344363328)) ;
#84477 = DIRECTION('',(-0.710669054518701,0.497468338163091,0.497468338163091)) ;
#84478 = DIRECTION('',(-1.33440267382831E-16,-1.,7.77328292223541E-33)) ;
#84479 = DIRECTION('',(0.710669054518702,0.497468338163091,-0.497468338163091)) ;
#84480 = DIRECTION('',(-5.04890651880155E-33,1.,9.34081871679819E-17)) ;
#84481 = DIRECTION('center_axis',(0.,0.573462344363328,-0.819231920519041)) ;
#84482 = DIRECTION('ref_axis',(0.,0.819231920519041,0.573462344363328)) ;
#84483 = DIRECTION('',(0.497468338163091,0.710669054518701,0.497468338163091)) ;
#84484 = DIRECTION('',(-1.,0.,0.)) ;
#84485 = DIRECTION('',(0.497468338163091,-0.710669054518701,-0.497468338163091)) ;
#84486 = DIRECTION('',(1.,0.,0.)) ;
#84487 = DIRECTION('center_axis',(0.,0.573462344363328,0.819231920519041)) ;
#84488 = DIRECTION('ref_axis',(0.,-0.819231920519041,0.573462344363328)) ;
#84489 = DIRECTION('',(-0.497468338163091,0.710669054518701,-0.497468338163091)) ;
#84490 = DIRECTION('',(1.,0.,0.)) ;
#84491 = DIRECTION('',(-0.497468338163091,-0.710669054518701,0.497468338163091)) ;
#84492 = DIRECTION('',(-1.,0.,0.)) ;
#84493 = DIRECTION('center_axis',(-0.164398987305354,-0.986393923832144,0.)) ;
#84494 = DIRECTION('ref_axis',(0.,0.,1.)) ;
#84495 = DIRECTION('',(0.,0.,-1.)) ;
#84496 = DIRECTION('center_axis',(-0.164398987305294,-0.986393923832154,-1.08493920789696E-12)) ;
#84497 = DIRECTION('ref_axis',(-0.057729035738443,0.00962150595530534,0.998285923498805)) ;
#84498 = DIRECTION('',(0.,0.,1.)) ;
#84499 = DIRECTION('center_axis',(1.,-2.89120579329441E-16,0.)) ;
#84500 = DIRECTION('ref_axis',(-2.89120579329441E-16,-1.,1.53777331288036E-13)) ;
#84501 = DIRECTION('center_axis',(1.,1.15648231731787E-15,0.)) ;
#84502 = DIRECTION('ref_axis',(1.15648231731787E-15,-1.,0.)) ;
#84503 = DIRECTION('center_axis',(0.16668982355543,0.983956802853987,0.0635886219415135)) ;
#84504 = DIRECTION('ref_axis',(-0.0486480010755861,0.0726194153599019,-0.996172571648174)) ;
#84505 = DIRECTION('center_axis',(0.166689823544595,0.983956802870528,-0.0635886217139631)) ;
#84506 = DIRECTION('ref_axis',(-0.0462047035076799,0.072214918770576,0.996318287938511)) ;
#84507 = DIRECTION('center_axis',(-0.164398987305354,-0.986393923832144,0.)) ;
#84508 = DIRECTION('ref_axis',(0.,0.,1.)) ;
#84509 = DIRECTION('',(0.,0.,1.)) ;
#84510 = DIRECTION('center_axis',(-0.164398987305453,-0.986393923832128,-1.73590273467075E-12)) ;
#84511 = DIRECTION('ref_axis',(-0.0554192327903204,0.00923653880014933,-0.998420450004869)) ;
#84512 = DIRECTION('',(0.,0.,-1.)) ;
#84513 = DIRECTION('center_axis',(0.,0.,1.)) ;
#84514 = DIRECTION('ref_axis',(1.,0.,0.)) ;
#84515 = DIRECTION('center_axis',(0.,0.,1.)) ;
#84516 = DIRECTION('ref_axis',(1.,0.,0.)) ;
#84517 = DIRECTION('center_axis',(0.,1.,0.)) ;
#84518 = DIRECTION('ref_axis',(1.,0.,0.)) ;
#84519 = DIRECTION('center_axis',(0.,-0.888198741900269,0.45945945945946)) ;
#84520 = DIRECTION('ref_axis',(0.,0.45945945945946,0.888198741900269)) ;
#84521 = DIRECTION('center_axis',(-1.,0.,1.22067519501986E-15)) ;
#84522 = DIRECTION('ref_axis',(-1.22067519501986E-15,0.,-1.)) ;
#84523 = DIRECTION('center_axis',(0.,0.,1.)) ;
#84524 = DIRECTION('ref_axis',(1.,0.,0.)) ;
#84525 = DIRECTION('center_axis',(0.,0.,-1.)) ;
#84526 = DIRECTION('ref_axis',(-1.,0.,0.)) ;
#84527 = DIRECTION('center_axis',(1.,-3.46944695195361E-16,0.)) ;
#84528 = DIRECTION('ref_axis',(3.46944695195361E-16,1.,0.)) ;
#84529 = DIRECTION('center_axis',(-1.,3.46944695195361E-16,0.)) ;
#84530 = DIRECTION('ref_axis',(3.46944695195361E-16,1.,0.)) ;
#84531 = DIRECTION('center_axis',(-1.,3.46944695195361E-16,0.)) ;
#84532 = DIRECTION('ref_axis',(-3.41607084500048E-16,-1.,0.)) ;
#84533 = DIRECTION('center_axis',(0.,-0.459459459459457,0.888198741900271)) ;
#84534 = DIRECTION('ref_axis',(0.,-0.888198741900271,-0.459459459459457)) ;
#84535 = DIRECTION('center_axis',(1.,-3.46944695195361E-16,0.)) ;
#84536 = DIRECTION('ref_axis',(0.,1.,0.)) ;
#84537 = DIRECTION('center_axis',(0.,0.888198741900269,-0.45945945945946)) ;
#84538 = DIRECTION('ref_axis',(0.,-0.45945945945946,-0.888198741900269)) ;
#84539 = DIRECTION('center_axis',(0.,1.,0.)) ;
#84540 = DIRECTION('ref_axis',(1.,0.,0.)) ;
#84541 = DIRECTION('center_axis',(0.,-1.,0.)) ;
#84542 = DIRECTION('ref_axis',(0.,0.,1.)) ;
#84543 = DIRECTION('center_axis',(-1.,0.,0.)) ;
#84544 = DIRECTION('ref_axis',(0.,0.,-1.)) ;
#84545 = DIRECTION('center_axis',(0.,0.,-1.)) ;
#84546 = DIRECTION('ref_axis',(-1.,0.,0.)) ;
#84547 = DIRECTION('center_axis',(0.,0.,-1.)) ;
#84548 = DIRECTION('ref_axis',(-1.,0.,0.)) ;
#84549 = DIRECTION('center_axis',(1.,-3.46944695195361E-16,0.)) ;
#84550 = DIRECTION('ref_axis',(3.46944695195361E-16,1.,0.)) ;
#84551 = DIRECTION('center_axis',(-1.,3.46944695195361E-16,0.)) ;
#84552 = DIRECTION('ref_axis',(3.46944695195361E-16,1.,3.46944695195361E-14)) ;
#84553 = DIRECTION('center_axis',(1.,0.,0.)) ;
#84554 = DIRECTION('ref_axis',(0.,0.,-1.)) ;
#84555 = DIRECTION('center_axis',(0.,0.,1.)) ;
#84556 = DIRECTION('ref_axis',(1.,0.,0.)) ;
#84557 = DIRECTION('center_axis',(0.,0.,1.)) ;
#84558 = DIRECTION('ref_axis',(1.,0.,0.)) ;
#84559 = DIRECTION('center_axis',(1.,-3.46944695195361E-16,0.)) ;
#84560 = DIRECTION('ref_axis',(3.80647894157197E-16,1.,0.)) ;
#84561 = DIRECTION('center_axis',(0.,0.459459459459459,-0.888198741900269)) ;
#84562 = DIRECTION('ref_axis',(0.,0.888198741900269,0.459459459459459)) ;
#84563 = DIRECTION('center_axis',(1.,-3.46944695195361E-16,0.)) ;
#84564 = DIRECTION('ref_axis',(3.46944695195361E-16,1.,0.)) ;
#84565 = DIRECTION('center_axis',(-1.,3.46944695195361E-16,0.)) ;
#84566 = DIRECTION('ref_axis',(3.46944695195361E-16,1.,0.)) ;
#84567 = DIRECTION('center_axis',(-3.46944695195361E-16,-1.,-6.49299968442375E-16)) ;
#84568 = DIRECTION('ref_axis',(2.25271179641597E-31,6.49299968442375E-16,
-1.)) ;
#84569 = DIRECTION('center_axis',(0.,-1.,0.)) ;
#84570 = DIRECTION('ref_axis',(0.,0.,-1.)) ;
#84571 = DIRECTION('center_axis',(0.,0.,1.)) ;
#84572 = DIRECTION('ref_axis',(1.,0.,0.)) ;
#84573 = DIRECTION('center_axis',(-3.25260651745651E-15,0.,1.)) ;
#84574 = DIRECTION('ref_axis',(1.,0.,3.25260651745651E-15)) ;
#84575 = DIRECTION('center_axis',(0.,1.,0.)) ;
#84576 = DIRECTION('ref_axis',(1.,0.,0.)) ;
#84577 = DIRECTION('center_axis',(0.,-0.888198741900269,-0.45945945945946)) ;
#84578 = DIRECTION('ref_axis',(0.,-0.45945945945946,0.888198741900269)) ;
#84579 = DIRECTION('center_axis',(1.,-3.46944695195361E-16,0.)) ;
#84580 = DIRECTION('ref_axis',(0.,1.,0.)) ;
#84581 = DIRECTION('center_axis',(0.,0.888198741900269,0.45945945945946)) ;
#84582 = DIRECTION('ref_axis',(0.,0.45945945945946,-0.888198741900269)) ;
#84583 = DIRECTION('center_axis',(1.,-3.46944695195361E-16,0.)) ;
#84584 = DIRECTION('ref_axis',(0.,1.,0.)) ;
#84585 = DIRECTION('center_axis',(0.,1.,0.)) ;
#84586 = DIRECTION('ref_axis',(0.,0.,-1.)) ;
#84587 = DIRECTION('center_axis',(0.,1.,0.)) ;
#84588 = DIRECTION('ref_axis',(1.,0.,0.)) ;
#84589 = DIRECTION('center_axis',(-1.,0.,0.)) ;
#84590 = DIRECTION('ref_axis',(0.,0.,-1.)) ;
#84591 = DIRECTION('center_axis',(1.,-3.46944695195361E-16,0.)) ;
#84592 = DIRECTION('ref_axis',(3.41607084500048E-16,1.,0.)) ;
#84593 = DIRECTION('center_axis',(-9.62987005567165E-16,-0.459459459459459,
-0.88819874190027)) ;
#84594 = DIRECTION('ref_axis',(-7.31984232283282E-30,0.88819874190027,-0.459459459459459)) ;
#84595 = DIRECTION('center_axis',(1.,-3.46944695195361E-16,0.)) ;
#84596 = DIRECTION('ref_axis',(3.46944695195361E-16,1.,0.)) ;
#84597 = DIRECTION('center_axis',(-1.,3.46944695195361E-16,0.)) ;
#84598 = DIRECTION('ref_axis',(3.46944695195361E-16,1.,0.)) ;
#84599 = DIRECTION('center_axis',(1.,0.,0.)) ;
#84600 = DIRECTION('ref_axis',(0.,0.,-1.)) ;
#84601 = DIRECTION('center_axis',(1.,-3.46944695195361E-16,0.)) ;
#84602 = DIRECTION('ref_axis',(3.80647894157197E-16,1.,0.)) ;
#84603 = DIRECTION('center_axis',(0.,0.459459459459459,0.888198741900269)) ;
#84604 = DIRECTION('ref_axis',(0.,-0.888198741900269,0.459459459459459)) ;
#84605 = DIRECTION('center_axis',(-3.46944695195361E-16,-1.,-6.49299968442375E-16)) ;
#84606 = DIRECTION('ref_axis',(2.25271179641597E-31,6.49299968442375E-16,
-1.)) ;
#84607 = DIRECTION('center_axis',(0.,1.,0.)) ;
#84608 = DIRECTION('ref_axis',(0.,0.,-1.)) ;
#84609 = DIRECTION('center_axis',(1.,0.,2.25271179641597E-31)) ;
#84610 = DIRECTION('ref_axis',(2.25271179641597E-31,0.,-1.)) ;
#84611 = DIRECTION('center_axis',(-1.,0.,0.)) ;
#84612 = DIRECTION('ref_axis',(0.,0.,1.)) ;
#84613 = DIRECTION('center_axis',(0.,1.,0.)) ;
#84614 = DIRECTION('ref_axis',(1.,0.,0.)) ;
#84615 = DIRECTION('center_axis',(0.,-1.,0.)) ;
#84616 = DIRECTION('ref_axis',(-1.08420217248551E-15,0.,1.)) ;
#84617 = DIRECTION('center_axis',(1.,-3.46944695195361E-16,0.)) ;
#84618 = DIRECTION('ref_axis',(0.,1.,0.)) ;
#84619 = DIRECTION('center_axis',(0.,1.,0.)) ;
#84620 = DIRECTION('ref_axis',(0.,0.,-1.)) ;
#84621 = DIRECTION('center_axis',(0.,-1.,0.)) ;
#84622 = DIRECTION('ref_axis',(0.,0.,-1.)) ;
#84623 = DIRECTION('center_axis',(0.,0.,1.)) ;
#84624 = DIRECTION('ref_axis',(-1.,0.,0.)) ;
#84625 = DIRECTION('center_axis',(0.,0.,-1.)) ;
#84626 = DIRECTION('ref_axis',(-1.,0.,0.)) ;
#84627 = DIRECTION('center_axis',(0.,0.,-1.)) ;
#84628 = DIRECTION('ref_axis',(-1.,0.,0.)) ;
#84629 = DIRECTION('center_axis',(-3.46944695195361E-16,-1.,-9.27571383489107E-17)) ;
#84630 = DIRECTION('ref_axis',(1.,-3.46944695195361E-16,-3.21815970916568E-32)) ;
#84631 = DIRECTION('center_axis',(0.,-1.,0.)) ;
#84632 = DIRECTION('ref_axis',(0.,0.,-1.)) ;
#84633 = DIRECTION('center_axis',(3.46944695195361E-16,1.,9.27571383489107E-17)) ;
#84634 = DIRECTION('ref_axis',(-1.,3.46944695195361E-16,3.21815970916568E-32)) ;
#84635 = DIRECTION('center_axis',(0.,1.,0.)) ;
#84636 = DIRECTION('ref_axis',(0.,0.,-1.)) ;
#84637 = DIRECTION('center_axis',(0.,0.,-1.)) ;
#84638 = DIRECTION('ref_axis',(-1.,0.,0.)) ;
#84639 = DIRECTION('center_axis',(0.,0.,1.)) ;
#84640 = DIRECTION('ref_axis',(1.,0.,0.)) ;
#84641 = DIRECTION('center_axis',(0.,1.,0.)) ;
#84642 = DIRECTION('ref_axis',(1.,0.,0.)) ;
#84643 = DIRECTION('center_axis',(-1.,0.,1.0842021724855E-15)) ;
#84644 = DIRECTION('ref_axis',(-1.0842021724855E-15,0.,-1.)) ;
#84645 = DIRECTION('center_axis',(0.,-1.,0.)) ;
#84646 = DIRECTION('ref_axis',(0.,0.,-1.)) ;
#84647 = DIRECTION('center_axis',(1.,0.,0.)) ;
#84648 = DIRECTION('ref_axis',(0.,0.,1.)) ;
#84649 = DIRECTION('center_axis',(1.,0.,3.21815970916568E-32)) ;
#84650 = DIRECTION('ref_axis',(3.21815970916568E-32,0.,-1.)) ;
#84651 = DIRECTION('center_axis',(0.,1.,0.)) ;
#84652 = DIRECTION('ref_axis',(1.,0.,0.)) ;
#84653 = DIRECTION('center_axis',(0.,0.,-1.)) ;
#84654 = DIRECTION('ref_axis',(1.,0.,0.)) ;
#84655 = DIRECTION('center_axis',(1.,0.,0.)) ;
#84656 = DIRECTION('ref_axis',(0.,-1.08420217248551E-15,1.)) ;
#84657 = DIRECTION('center_axis',(1.0842021724855E-15,1.,0.)) ;
#84658 = DIRECTION('ref_axis',(1.,-1.0842021724855E-15,0.)) ;
#84659 = DIRECTION('center_axis',(1.,0.,-2.08976773479518E-32)) ;
#84660 = DIRECTION('ref_axis',(-2.08976773479518E-32,0.,-1.)) ;
#84661 = DIRECTION('center_axis',(-0.447220452189337,-7.10036081300347E-6,
-0.894423762594191)) ;
#84662 = DIRECTION('ref_axis',(0.894325663270266,0.0148067719203444,-0.44717151913052)) ;
#84663 = DIRECTION('center_axis',(-1.23908819712629E-16,1.,2.4093381610789E-16)) ;
#84664 = DIRECTION('ref_axis',(2.98538247827883E-32,-2.4093381610789E-16,
1.)) ;
#84665 = DIRECTION('center_axis',(-5.60223399549347E-6,-0.447219005480232,
-0.894424485971782)) ;
#84666 = DIRECTION('ref_axis',(0.0146917039115986,0.894327914920361,-0.447170811245964)) ;
#84667 = DIRECTION('center_axis',(-8.95614743483648E-33,0.,1.)) ;
#84668 = DIRECTION('ref_axis',(1.,0.,8.95614743483648E-33)) ;
#84669 = DIRECTION('center_axis',(1.40488587213121E-32,-1.23908819712629E-16,
-1.)) ;
#84670 = DIRECTION('ref_axis',(1.74077750246726E-48,1.,-1.23908819712629E-16)) ;
#84671 = DIRECTION('center_axis',(-2.65552944032596E-32,0.,1.)) ;
#84672 = DIRECTION('ref_axis',(1.,0.,2.65552944032596E-32)) ;
#84673 = DIRECTION('center_axis',(0.89442448597137,-5.60223466363593E-6,0.447219005481056)) ;
#84674 = DIRECTION('ref_axis',(0.447170811246728,0.0146917039220712,-0.894327914919807)) ;
#84675 = DIRECTION('center_axis',(0.894423762593715,-7.10036087598425E-6,
-0.447220452190288)) ;
#84676 = DIRECTION('ref_axis',(0.447171519131212,0.014806771959662,0.894325663269269)) ;
#84677 = DIRECTION('center_axis',(-8.95614743483648E-33,-1.10974565782288E-48,
1.)) ;
#84678 = DIRECTION('ref_axis',(1.,-9.9390457266313E-81,8.95614743483648E-33)) ;
#84679 = DIRECTION('center_axis',(-7.10036049907078E-6,0.894423762593765,
0.44722045219019)) ;
#84680 = DIRECTION('ref_axis',(-0.0148067719083974,-0.447171519131448,0.89432566327)) ;
#84681 = DIRECTION('center_axis',(-5.60223341193312E-6,0.894424485971936,
-0.447219005479926)) ;
#84682 = DIRECTION('ref_axis',(0.0146917039491787,0.447170811245404,0.894327914920024)) ;
#84683 = DIRECTION('center_axis',(1.40488587213121E-32,-1.23908819712629E-16,
-1.)) ;
#84684 = DIRECTION('ref_axis',(0.,1.,0.)) ;
#84685 = DIRECTION('center_axis',(-1.,0.,0.)) ;
#84686 = DIRECTION('ref_axis',(0.,0.,-1.)) ;
#84687 = DIRECTION('center_axis',(0.,-1.,0.)) ;
#84688 = DIRECTION('ref_axis',(0.,0.,1.)) ;
#84689 = DIRECTION('center_axis',(-1.,0.,-1.40488587213121E-32)) ;
#84690 = DIRECTION('ref_axis',(-1.40488587213121E-32,0.,1.)) ;
#84691 = DIRECTION('',(-1.,0.,-1.40488587213121E-32)) ;
#84692 = DIRECTION('center_axis',(-1.,0.,0.)) ;
#84693 = DIRECTION('ref_axis',(0.,0.,1.)) ;
#84694 = DIRECTION('center_axis',(0.,1.,0.)) ;
#84695 = DIRECTION('ref_axis',(1.,0.,0.)) ;
#84696 = DIRECTION('center_axis',(0.,1.,0.)) ;
#84697 = DIRECTION('ref_axis',(0.,0.,-1.)) ;
#84698 = DIRECTION('center_axis',(0.,0.,-1.)) ;
#84699 = DIRECTION('ref_axis',(1.,0.,0.)) ;
#84700 = DIRECTION('center_axis',(-1.,0.,-1.7912294869673E-32)) ;
#84701 = DIRECTION('ref_axis',(-1.7912294869673E-32,0.,1.)) ;
#84702 = DIRECTION('center_axis',(-0.447219005479784,-5.60223355926168E-6,
0.894424485972007)) ;
#84703 = DIRECTION('ref_axis',(0.894327914920142,0.014691703945553,0.447170811245287)) ;
#84704 = DIRECTION('center_axis',(-1.,0.,0.)) ;
#84705 = DIRECTION('ref_axis',(0.,0.,1.)) ;
#84706 = DIRECTION('center_axis',(1.23908819712629E-16,-1.,7.2280144832367E-17)) ;
#84707 = DIRECTION('ref_axis',(1.,1.23908819712629E-16,-8.95614743483648E-33)) ;
#84708 = DIRECTION('center_axis',(-7.10036028217959E-6,-0.447220452189357,
0.894423762594181)) ;
#84709 = DIRECTION('ref_axis',(-0.0148067719368954,-0.89432566327004,-0.447171519130424)) ;
#84710 = DIRECTION('center_axis',(0.,-1.,1.0842021724855E-15)) ;
#84711 = DIRECTION('ref_axis',(0.,-1.0842021724855E-15,-1.)) ;
#84712 = DIRECTION('center_axis',(1.23908819712629E-16,-1.,1.23908819712629E-16)) ;
#84713 = DIRECTION('ref_axis',(-9.81657386420148E-47,-1.23908819712629E-16,
-1.)) ;
#84714 = DIRECTION('center_axis',(0.,-1.,0.)) ;
#84715 = DIRECTION('ref_axis',(0.,0.,-1.)) ;
#84716 = DIRECTION('',(-1.23908819712629E-16,1.,-1.23908819712629E-16)) ;
#84717 = DIRECTION('center_axis',(1.,0.,1.40488587213121E-32)) ;
#84718 = DIRECTION('ref_axis',(1.40488587213121E-32,0.,-1.)) ;
#84719 = DIRECTION('center_axis',(-0.707106781186547,0.707106781186548,-6.41152859744984E-16)) ;
#84720 = DIRECTION('ref_axis',(0.707106781186548,0.707106781186547,-2.22751953561763E-12)) ;
#84721 = DIRECTION('center_axis',(1.,0.,0.)) ;
#84722 = DIRECTION('ref_axis',(0.,0.,-1.)) ;
#84723 = DIRECTION('center_axis',(0.,-1.,0.)) ;
#84724 = DIRECTION('ref_axis',(0.,0.,-1.)) ;
#84725 = DIRECTION('center_axis',(0.,0.,1.)) ;
#84726 = DIRECTION('ref_axis',(-1.,0.,0.)) ;
#84727 = DIRECTION('center_axis',(7.2280144832367E-17,0.,-1.)) ;
#84728 = DIRECTION('ref_axis',(-1.,0.,-7.2280144832367E-17)) ;
#84729 = DIRECTION('',(7.2280144832367E-17,0.,-1.)) ;
#84730 = DIRECTION('center_axis',(0.,0.,-1.)) ;
#84731 = DIRECTION('ref_axis',(-1.,0.,0.)) ;
#84732 = DIRECTION('center_axis',(0.,1.,0.)) ;
#84733 = DIRECTION('ref_axis',(1.,0.,0.)) ;
#84734 = DIRECTION('center_axis',(0.,0.,1.)) ;
#84735 = DIRECTION('ref_axis',(-1.,0.,0.)) ;
#84736 = DIRECTION('center_axis',(0.,1.,0.)) ;
#84737 = DIRECTION('ref_axis',(1.,0.,0.)) ;
#84738 = DIRECTION('center_axis',(1.,0.,0.)) ;
#84739 = DIRECTION('ref_axis',(0.,0.,1.)) ;
#84740 = DIRECTION('center_axis',(0.,0.,-1.)) ;
#84741 = DIRECTION('ref_axis',(1.,0.,0.)) ;
#84742 = DIRECTION('center_axis',(-1.13380619344889E-16,1.,-1.23908819712629E-16)) ;
#84743 = DIRECTION('ref_axis',(-1.40488587213121E-32,1.23908819712629E-16,
1.)) ;
#84744 = DIRECTION('center_axis',(0.,1.,0.)) ;
#84745 = DIRECTION('ref_axis',(0.,0.,1.)) ;
#84746 = DIRECTION('center_axis',(7.2280144832367E-17,0.,-1.)) ;
#84747 = DIRECTION('ref_axis',(-1.,0.,-7.2280144832367E-17)) ;
#84748 = DIRECTION('center_axis',(0.,0.,1.)) ;
#84749 = DIRECTION('ref_axis',(1.,0.,0.)) ;
#84750 = DIRECTION('center_axis',(0.,1.,0.)) ;
#84751 = DIRECTION('ref_axis',(1.,0.,0.)) ;
#84752 = DIRECTION('center_axis',(0.,1.,0.)) ;
#84753 = DIRECTION('ref_axis',(0.,0.,-1.)) ;
#84754 = DIRECTION('center_axis',(1.,2.16840434497101E-15,-2.93873587705572E-31)) ;
#84755 = DIRECTION('ref_axis',(2.16840434497101E-15,-1.,-1.03035812136257E-62)) ;
#84756 = DIRECTION('center_axis',(-8.95614743483648E-33,0.,1.)) ;
#84757 = DIRECTION('ref_axis',(1.,0.,8.95614743483648E-33)) ;
#84758 = DIRECTION('center_axis',(-1.40488587213121E-32,1.23908819712629E-16,
1.)) ;
#84759 = DIRECTION('ref_axis',(-1.74077750246726E-48,-1.,1.23908819712629E-16)) ;
#84760 = DIRECTION('center_axis',(8.95614743483648E-33,1.0154535431059E-48,
-1.)) ;
#84761 = DIRECTION('ref_axis',(-1.,9.09455164528354E-81,-8.95614743483648E-33)) ;
#84762 = DIRECTION('center_axis',(2.16840434497101E-15,0.,-1.)) ;
#84763 = DIRECTION('ref_axis',(-1.,0.,-2.16840434497101E-15)) ;
#84764 = DIRECTION('',(-8.95614743483648E-33,-1.0154535431059E-48,1.)) ;
#84765 = DIRECTION('center_axis',(-1.,-1.13380619344889E-16,0.)) ;
#84766 = DIRECTION('ref_axis',(0.,-1.,0.)) ;
#84767 = DIRECTION('center_axis',(0.,0.,1.)) ;
#84768 = DIRECTION('ref_axis',(-1.,0.,0.)) ;
#84769 = DIRECTION('center_axis',(0.,-1.,0.)) ;
#84770 = DIRECTION('ref_axis',(0.,0.,-1.)) ;
#84771 = DIRECTION('center_axis',(-1.,0.,0.)) ;
#84772 = DIRECTION('ref_axis',(0.,0.,-1.)) ;
#84773 = DIRECTION('center_axis',(1.,0.,1.40488587213121E-32)) ;
#84774 = DIRECTION('ref_axis',(1.40488587213121E-32,0.,-1.)) ;
#84775 = DIRECTION('',(1.,0.,1.40488587213121E-32)) ;
#84776 = DIRECTION('center_axis',(1.,0.,0.)) ;
#84777 = DIRECTION('ref_axis',(0.,0.,-1.)) ;
#84778 = DIRECTION('center_axis',(-1.40488587213121E-32,1.23908819712629E-16,
1.)) ;
#84779 = DIRECTION('ref_axis',(0.,-1.,0.)) ;
#84780 = DIRECTION('center_axis',(0.,-1.,0.)) ;
#84781 = DIRECTION('ref_axis',(0.,0.,1.)) ;
#84782 = DIRECTION('center_axis',(0.,1.,0.)) ;
#84783 = DIRECTION('ref_axis',(1.,0.,0.)) ;
#84784 = DIRECTION('center_axis',(1.,0.,0.)) ;
#84785 = DIRECTION('ref_axis',(0.,0.,1.)) ;
#84786 = DIRECTION('center_axis',(0.,1.,0.)) ;
#84787 = DIRECTION('ref_axis',(0.,0.,-1.)) ;
#84788 = DIRECTION('center_axis',(0.,0.,1.)) ;
#84789 = DIRECTION('ref_axis',(1.,0.,0.)) ;
#84790 = DIRECTION('center_axis',(0.,0.,1.)) ;
#84791 = DIRECTION('ref_axis',(1.,0.,0.)) ;
#84792 = DIRECTION('center_axis',(1.,0.,1.40488587213121E-32)) ;
#84793 = DIRECTION('ref_axis',(1.40488587213121E-32,0.,-1.)) ;
#84794 = DIRECTION('center_axis',(-0.707106781186552,0.707106781186543,-7.9502954608381E-15)) ;
#84795 = DIRECTION('ref_axis',(0.707106781186543,0.707106781186552,-7.24201771566408E-13)) ;
#84796 = DIRECTION('center_axis',(-1.23908819712629E-16,1.,-1.23908819712629E-16)) ;
#84797 = DIRECTION('ref_axis',(9.81657386420148E-47,1.23908819712629E-16,
1.)) ;
#84798 = DIRECTION('',(1.23908819712629E-16,-1.,1.23908819712629E-16)) ;
#84799 = DIRECTION('center_axis',(-1.,-1.13380619344889E-16,0.)) ;
#84800 = DIRECTION('ref_axis',(0.,-1.,0.)) ;
#84801 = DIRECTION('center_axis',(0.,-1.,0.)) ;
#84802 = DIRECTION('ref_axis',(0.,0.,1.)) ;
#84803 = DIRECTION('center_axis',(1.13380619344889E-16,-1.,1.23908819712629E-16)) ;
#84804 = DIRECTION('ref_axis',(1.40488587213121E-32,-1.23908819712629E-16,
-1.)) ;
#84805 = DIRECTION('center_axis',(-1.5529910948782E-31,-4.47619207437002E-16,
1.)) ;
#84806 = DIRECTION('ref_axis',(6.951486430461E-47,-1.,-4.47619207437002E-16)) ;
#84807 = DIRECTION('center_axis',(0.,2.16840434497101E-15,-1.)) ;
#84808 = DIRECTION('ref_axis',(0.,1.,2.16840434497101E-15)) ;
#84809 = DIRECTION('center_axis',(0.,1.,0.)) ;
#84810 = DIRECTION('ref_axis',(1.,0.,0.)) ;
#84811 = DIRECTION('center_axis',(3.85194802226865E-15,0.888198741900269,
-0.45945945945946)) ;
#84812 = DIRECTION('ref_axis',(3.25260651745654E-15,-0.45945945945946,-0.888198741900269)) ;
#84813 = DIRECTION('center_axis',(-1.,0.,1.22067519501986E-15)) ;
#84814 = DIRECTION('ref_axis',(-1.22067519501986E-15,3.46944695195364E-14,
-1.)) ;
#84815 = DIRECTION('center_axis',(1.5529910948782E-31,4.47619207437002E-16,
-1.)) ;
#84816 = DIRECTION('ref_axis',(-6.951486430461E-47,1.,4.47619207437002E-16)) ;
#84817 = DIRECTION('center_axis',(0.,0.,1.)) ;
#84818 = DIRECTION('ref_axis',(1.,0.,0.)) ;
#84819 = DIRECTION('center_axis',(1.,-3.46944695195361E-16,0.)) ;
#84820 = DIRECTION('ref_axis',(3.46944695195361E-16,1.,0.)) ;
#84821 = DIRECTION('center_axis',(-1.,3.46944695195361E-16,0.)) ;
#84822 = DIRECTION('ref_axis',(3.46944695195361E-16,1.,3.46944695195362E-14)) ;
#84823 = DIRECTION('center_axis',(1.,-3.46944695195361E-16,0.)) ;
#84824 = DIRECTION('ref_axis',(3.41607084500048E-16,1.,0.)) ;
#84825 = DIRECTION('center_axis',(0.,0.459459459459457,-0.888198741900271)) ;
#84826 = DIRECTION('ref_axis',(0.,0.888198741900271,0.459459459459457)) ;
#84827 = DIRECTION('center_axis',(0.,0.,1.)) ;
#84828 = DIRECTION('ref_axis',(1.,0.,0.)) ;
#84829 = DIRECTION('center_axis',(0.,0.,-1.)) ;
#84830 = DIRECTION('ref_axis',(-1.,0.,0.)) ;
#84831 = DIRECTION('center_axis',(-1.,3.46944695195361E-16,0.)) ;
#84832 = DIRECTION('ref_axis',(-3.46944695195361E-16,-1.,0.)) ;
#84833 = DIRECTION('center_axis',(-1.,3.46944695195361E-16,0.)) ;
#84834 = DIRECTION('ref_axis',(-3.46944695195361E-16,-1.,0.)) ;
#84835 = DIRECTION('center_axis',(-1.,3.46944695195361E-16,0.)) ;
#84836 = DIRECTION('ref_axis',(3.46944695195361E-16,1.,6.93889390390722E-14)) ;
#84837 = DIRECTION('center_axis',(1.,-3.46944695195361E-16,0.)) ;
#84838 = DIRECTION('ref_axis',(0.,1.,0.)) ;
#84839 = DIRECTION('center_axis',(0.,-0.888198741900269,0.459459459459461)) ;
#84840 = DIRECTION('ref_axis',(0.,0.459459459459461,0.888198741900269)) ;
#84841 = DIRECTION('center_axis',(0.,1.,0.)) ;
#84842 = DIRECTION('ref_axis',(1.,0.,0.)) ;
#84843 = DIRECTION('center_axis',(0.,1.,0.)) ;
#84844 = DIRECTION('ref_axis',(0.,0.,-1.)) ;
#84845 = DIRECTION('center_axis',(-1.,0.,0.)) ;
#84846 = DIRECTION('ref_axis',(0.,-8.67361737988409E-15,-1.)) ;
#84847 = DIRECTION('center_axis',(1.,-3.46944695195361E-16,0.)) ;
#84848 = DIRECTION('ref_axis',(3.70074341541719E-16,1.,0.)) ;
#84849 = DIRECTION('center_axis',(0.,0.63294893130157,-0.774193548387094)) ;
#84850 = DIRECTION('ref_axis',(-1.08420217248549E-15,-0.774193548387094,-0.63294893130157)) ;
#84851 = DIRECTION('center_axis',(1.,-3.46944695195361E-16,0.)) ;
#84852 = DIRECTION('ref_axis',(3.80647894157197E-16,1.,0.)) ;
#84853 = DIRECTION('center_axis',(0.,-0.45945945945946,0.888198741900269)) ;
#84854 = DIRECTION('ref_axis',(0.,-0.888198741900269,-0.45945945945946)) ;
#84855 = DIRECTION('center_axis',(1.,-3.46944695195361E-16,0.)) ;
#84856 = DIRECTION('ref_axis',(3.46944695195361E-16,1.,0.)) ;
#84857 = DIRECTION('center_axis',(-1.,3.46944695195361E-16,0.)) ;
#84858 = DIRECTION('ref_axis',(3.46944695195361E-16,1.,0.)) ;
#84859 = DIRECTION('center_axis',(-3.46944695195361E-16,-1.,-2.45739631480277E-16)) ;
#84860 = DIRECTION('ref_axis',(1.,-3.46944695195361E-16,-8.52580615413453E-32)) ;
#84861 = DIRECTION('center_axis',(0.,1.,0.)) ;
#84862 = DIRECTION('ref_axis',(0.,0.,1.)) ;
#84863 = DIRECTION('center_axis',(1.,-3.46944695195361E-16,0.)) ;
#84864 = DIRECTION('ref_axis',(3.33066907387547E-16,1.,0.)) ;
#84865 = DIRECTION('center_axis',(8.02036034720251E-16,0.293103448275862,
-0.956080733311157)) ;
#84866 = DIRECTION('ref_axis',(1.13164713162994E-29,0.956080733311157,0.293103448275862)) ;
#84867 = DIRECTION('center_axis',(-1.,3.46944695195361E-16,0.)) ;
#84868 = DIRECTION('ref_axis',(-3.46944695195361E-16,-1.,0.)) ;
#84869 = DIRECTION('center_axis',(-1.,3.46944695195361E-16,0.)) ;
#84870 = DIRECTION('ref_axis',(-3.46944695195361E-16,-1.,0.)) ;
#84871 = DIRECTION('center_axis',(-1.,3.46944695195361E-16,0.)) ;
#84872 = DIRECTION('ref_axis',(-3.46944695195361E-16,-1.,0.)) ;
#84873 = DIRECTION('center_axis',(0.,0.,-1.)) ;
#84874 = DIRECTION('ref_axis',(-1.,0.,0.)) ;
#84875 = DIRECTION('center_axis',(0.,0.,1.)) ;
#84876 = DIRECTION('ref_axis',(1.,0.,0.)) ;
#84877 = DIRECTION('center_axis',(-1.5529910948782E-31,-4.47619207437002E-16,
-1.)) ;
#84878 = DIRECTION('ref_axis',(-6.95148643046101E-47,1.,-4.47619207437002E-16)) ;
#84879 = DIRECTION('center_axis',(2.16840434497101E-15,0.,1.)) ;
#84880 = DIRECTION('ref_axis',(1.,0.,-2.16840434497101E-15)) ;
#84881 = DIRECTION('center_axis',(1.,-3.46944695195361E-16,0.)) ;
#84882 = DIRECTION('ref_axis',(0.,1.,0.)) ;
#84883 = DIRECTION('center_axis',(0.,-1.,0.)) ;
#84884 = DIRECTION('ref_axis',(0.,0.,1.)) ;
#84885 = DIRECTION('center_axis',(0.577350269189627,0.577350269189627,0.577350269189623)) ;
#84886 = DIRECTION('ref_axis',(-0.707106781186548,2.22044604925032E-15,0.707106781186547)) ;
#84887 = DIRECTION('center_axis',(-1.,3.46944695195361E-16,0.)) ;
#84888 = DIRECTION('ref_axis',(-3.70074341541719E-16,-1.,0.)) ;
#84889 = DIRECTION('center_axis',(0.,0.63294893130157,0.774193548387094)) ;
#84890 = DIRECTION('ref_axis',(0.,0.774193548387094,-0.63294893130157)) ;
#84891 = DIRECTION('center_axis',(0.,1.,0.)) ;
#84892 = DIRECTION('ref_axis',(1.,0.,0.)) ;
#84893 = DIRECTION('center_axis',(-1.,0.,0.)) ;
#84894 = DIRECTION('ref_axis',(0.,1.73472347597682E-14,-1.)) ;
#84895 = DIRECTION('center_axis',(0.,0.888198741900271,0.459459459459457)) ;
#84896 = DIRECTION('ref_axis',(-1.08420217248551E-15,0.459459459459457,-0.888198741900271)) ;
#84897 = DIRECTION('center_axis',(3.46944695195361E-16,1.,2.45739631480277E-16)) ;
#84898 = DIRECTION('ref_axis',(-1.,3.46944695195361E-16,8.52580615413453E-32)) ;
#84899 = DIRECTION('center_axis',(-1.,3.46944695195361E-16,0.)) ;
#84900 = DIRECTION('ref_axis',(-3.33066907387547E-16,-1.,0.)) ;
#84901 = DIRECTION('center_axis',(0.,0.293103448275864,0.956080733311156)) ;
#84902 = DIRECTION('ref_axis',(0.,-0.956080733311156,0.293103448275864)) ;
#84903 = DIRECTION('center_axis',(-3.46944695195361E-16,-1.,-1.06487173641454E-15)) ;
#84904 = DIRECTION('ref_axis',(3.69451600012496E-31,1.06487173641454E-15,
-1.)) ;
#84905 = DIRECTION('center_axis',(0.,-1.,0.)) ;
#84906 = DIRECTION('ref_axis',(0.,0.,-1.)) ;
#84907 = DIRECTION('center_axis',(0.,1.,0.)) ;
#84908 = DIRECTION('ref_axis',(0.,0.,1.)) ;
#84909 = DIRECTION('center_axis',(-1.,3.46944695195361E-16,0.)) ;
#84910 = DIRECTION('ref_axis',(-3.41607084500048E-16,-1.,0.)) ;
#84911 = DIRECTION('center_axis',(-4.88154879316133E-15,0.45945945945946,
0.888198741900269)) ;
#84912 = DIRECTION('ref_axis',(-3.39148554690438E-29,-0.888198741900269,0.45945945945946)) ;
#84913 = DIRECTION('center_axis',(1.,-3.46944695195361E-16,0.)) ;
#84914 = DIRECTION('ref_axis',(3.46944695195361E-16,1.,0.)) ;
#84915 = DIRECTION('center_axis',(-1.,3.46944695195361E-16,0.)) ;
#84916 = DIRECTION('ref_axis',(3.46944695195361E-16,1.,0.)) ;
#84917 = DIRECTION('center_axis',(-1.5529910948782E-31,-4.47619207437002E-16,
-1.)) ;
#84918 = DIRECTION('ref_axis',(-6.95148643046101E-47,1.,-4.47619207437002E-16)) ;
#84919 = DIRECTION('center_axis',(0.,0.,-1.)) ;
#84920 = DIRECTION('ref_axis',(-1.,0.,0.)) ;
#84921 = DIRECTION('center_axis',(0.,0.224137931034483,-0.974557431797419)) ;
#84922 = DIRECTION('ref_axis',(0.,-0.974557431797419,-0.224137931034483)) ;
#84923 = DIRECTION('center_axis',(0.577350269189627,0.577350269189627,0.577350269189623)) ;
#84924 = DIRECTION('ref_axis',(-0.707106781186548,2.22044604925032E-15,0.707106781186547)) ;
#84925 = DIRECTION('center_axis',(0.408248290463864,-0.816496580927725,0.408248290463864)) ;
#84926 = DIRECTION('ref_axis',(0.707106781186545,-2.77555756156289E-15,-0.70710678118655)) ;
#84927 = DIRECTION('center_axis',(0.,1.,0.)) ;
#84928 = DIRECTION('ref_axis',(1.,0.,0.)) ;
#84929 = DIRECTION('center_axis',(-1.,0.,0.)) ;
#84930 = DIRECTION('ref_axis',(0.,0.,-1.)) ;
#84931 = DIRECTION('center_axis',(1.,-3.46944695195361E-16,0.)) ;
#84932 = DIRECTION('ref_axis',(0.,1.,0.)) ;
#84933 = DIRECTION('center_axis',(9.96293888229924E-16,-0.888198741900269,
-0.45945945945946)) ;
#84934 = DIRECTION('ref_axis',(-3.00809911926502E-30,-0.45945945945946,0.888198741900269)) ;
#84935 = DIRECTION('center_axis',(1.,-3.46944695195361E-16,0.)) ;
#84936 = DIRECTION('ref_axis',(-3.70074341541719E-16,-1.,0.)) ;
#84937 = DIRECTION('center_axis',(1.58436874053304E-16,-0.224137931034483,
-0.974557431797419)) ;
#84938 = DIRECTION('ref_axis',(2.18893094986727E-31,0.974557431797419,-0.224137931034483)) ;
#84939 = DIRECTION('center_axis',(1.,-3.46944695195361E-16,0.)) ;
#84940 = DIRECTION('ref_axis',(3.46944695195361E-16,1.,0.)) ;
#84941 = DIRECTION('center_axis',(-1.,3.46944695195361E-16,0.)) ;
#84942 = DIRECTION('ref_axis',(3.46944695195361E-16,1.,0.)) ;
#84943 = DIRECTION('center_axis',(1.,-3.46944695195361E-16,0.)) ;
#84944 = DIRECTION('ref_axis',(3.80647894157197E-16,1.,0.)) ;
#84945 = DIRECTION('center_axis',(0.,-0.45945945945946,-0.888198741900269)) ;
#84946 = DIRECTION('ref_axis',(0.,0.888198741900269,-0.45945945945946)) ;
#84947 = DIRECTION('center_axis',(1.,-3.46944695195361E-16,0.)) ;
#84948 = DIRECTION('ref_axis',(0.,1.,0.)) ;
#84949 = DIRECTION('center_axis',(0.,-1.,0.)) ;
#84950 = DIRECTION('ref_axis',(0.,0.,1.)) ;
#84951 = DIRECTION('center_axis',(-3.46944695195361E-16,-1.,-1.06487173641454E-15)) ;
#84952 = DIRECTION('ref_axis',(3.69451600012496E-31,1.06487173641454E-15,
-1.)) ;
#84953 = DIRECTION('center_axis',(0.,0.,1.)) ;
#84954 = DIRECTION('ref_axis',(1.,0.,0.)) ;
#84955 = DIRECTION('center_axis',(0.,-1.,0.)) ;
#84956 = DIRECTION('ref_axis',(0.,0.,-1.)) ;
#84957 = DIRECTION('center_axis',(0.,-1.,0.)) ;
#84958 = DIRECTION('ref_axis',(0.,0.,-1.)) ;
#84959 = DIRECTION('center_axis',(0.,1.,0.)) ;
#84960 = DIRECTION('ref_axis',(0.,0.,-1.)) ;
#84961 = DIRECTION('center_axis',(0.,0.,1.)) ;
#84962 = DIRECTION('ref_axis',(1.,0.,0.)) ;
#84963 = DIRECTION('center_axis',(8.67361737988404E-15,-1.,0.)) ;
#84964 = DIRECTION('ref_axis',(1.,8.67361737988404E-15,0.)) ;
#84965 = DIRECTION('center_axis',(0.497468338163091,-0.710669054518702,0.497468338163091)) ;
#84966 = DIRECTION('ref_axis',(0.81923192051904,0.573462344363328,8.04804396179112E-16)) ;
#84967 = DIRECTION('center_axis',(0.497468338163091,-0.710669054518702,0.497468338163091)) ;
#84968 = DIRECTION('ref_axis',(0.81923192051904,0.573462344363328,7.6535433881835E-16)) ;
#84969 = DIRECTION('center_axis',(0.497468338163092,-0.7106690545187,0.497468338163092)) ;
#84970 = DIRECTION('ref_axis',(-1.24903860074368E-15,-0.57346234436333,-0.819231920519039)) ;
#84971 = DIRECTION('center_axis',(0.,0.,1.)) ;
#84972 = DIRECTION('ref_axis',(1.,0.,0.)) ;
#84973 = DIRECTION('center_axis',(0.,-1.,0.)) ;
#84974 = DIRECTION('ref_axis',(0.,0.,-1.)) ;
#84975 = DIRECTION('center_axis',(0.,1.,0.)) ;
#84976 = DIRECTION('ref_axis',(0.,0.,1.)) ;
#84977 = DIRECTION('center_axis',(0.,1.,0.)) ;
#84978 = DIRECTION('ref_axis',(0.,0.,1.)) ;
#84979 = DIRECTION('center_axis',(0.,1.,0.)) ;
#84980 = DIRECTION('ref_axis',(1.,0.,0.)) ;
#84981 = DIRECTION('center_axis',(-1.98515611757154E-15,0.,1.)) ;
#84982 = DIRECTION('ref_axis',(-1.,0.,-1.98515611757154E-15)) ;
#84983 = DIRECTION('center_axis',(1.,-4.06575814682065E-16,2.84603070277446E-16)) ;
#84984 = DIRECTION('ref_axis',(-4.06575814682065E-16,-1.,6.48893816316174E-47)) ;
#84985 = DIRECTION('center_axis',(0.,1.,0.)) ;
#84986 = DIRECTION('ref_axis',(0.,0.,1.)) ;
#84987 = DIRECTION('center_axis',(0.,1.,0.)) ;
#84988 = DIRECTION('ref_axis',(0.,0.,1.)) ;
#84989 = DIRECTION('center_axis',(0.497468338163091,0.710669054518702,-0.497468338163091)) ;
#84990 = DIRECTION('ref_axis',(-0.81923192051904,0.573462344363328,7.6535433881835E-16)) ;
#84991 = DIRECTION('center_axis',(-0.497468338163091,-0.710669054518702,0.497468338163091)) ;
#84992 = DIRECTION('ref_axis',(-0.81923192051904,0.573462344363329,2.81956803083991E-15)) ;
#84993 = DIRECTION('center_axis',(-0.497468338163093,-0.7106690545187,0.497468338163091)) ;
#84994 = DIRECTION('ref_axis',(0.819231920519039,-0.573462344363331,1.48853464230757E-16)) ;
#84995 = DIRECTION('center_axis',(1.,0.,0.)) ;
#84996 = DIRECTION('ref_axis',(0.,0.,-1.)) ;
#84997 = DIRECTION('center_axis',(1.,0.,-9.9257805878577E-16)) ;
#84998 = DIRECTION('ref_axis',(-9.9257805878577E-16,0.,-1.)) ;
#84999 = DIRECTION('center_axis',(0.,0.,-1.)) ;
#85000 = DIRECTION('ref_axis',(-1.,0.,0.)) ;
#85001 = DIRECTION('center_axis',(-1.23327997120227E-15,1.76182853028895E-15,
1.)) ;
#85002 = DIRECTION('ref_axis',(-2.17282783909808E-30,-1.,1.76182853028895E-15)) ;
#85003 = DIRECTION('center_axis',(-0.497468338163091,0.710669054518702,0.497468338163091)) ;
#85004 = DIRECTION('ref_axis',(-0.81923192051904,-0.573462344363328,7.6535433881835E-16)) ;
#85005 = DIRECTION('center_axis',(0.497468338163091,-0.710669054518702,-0.497468338163091)) ;
#85006 = DIRECTION('ref_axis',(-0.819231920519018,-0.57346234436336,6.87084924063159E-14)) ;
#85007 = DIRECTION('center_axis',(0.497468338163093,-0.7106690545187,-0.497468338163091)) ;
#85008 = DIRECTION('ref_axis',(0.819231920519039,0.573462344363331,2.16059097207149E-16)) ;
#85009 = DIRECTION('center_axis',(0.,1.,0.)) ;
#85010 = DIRECTION('ref_axis',(1.,0.,0.)) ;
#85011 = DIRECTION('center_axis',(-1.13841228110978E-15,-1.62630325872826E-15,
1.)) ;
#85012 = DIRECTION('ref_axis',(3.52365706057789E-15,1.,1.62630325872826E-15)) ;
#85013 = DIRECTION('center_axis',(0.,1.,0.)) ;
#85014 = DIRECTION('ref_axis',(1.,0.,0.)) ;
#85015 = DIRECTION('center_axis',(1.,0.,-1.65429676464295E-16)) ;
#85016 = DIRECTION('ref_axis',(1.65429676464295E-16,4.33680868994204E-15,
1.)) ;
#85017 = DIRECTION('center_axis',(0.,0.,-1.)) ;
#85018 = DIRECTION('ref_axis',(-1.,0.,0.)) ;
#85019 = DIRECTION('center_axis',(3.3085935292859E-16,0.,1.)) ;
#85020 = DIRECTION('ref_axis',(1.,0.,-3.3085935292859E-16)) ;
#85021 = DIRECTION('center_axis',(1.,0.,0.)) ;
#85022 = DIRECTION('ref_axis',(0.,0.,-1.)) ;
#85023 = DIRECTION('center_axis',(1.,1.21972744404619E-15,8.53809210832338E-16)) ;
#85024 = DIRECTION('ref_axis',(-1.21972744404619E-15,1.,-2.84382165153726E-47)) ;
#85025 = DIRECTION('center_axis',(0.,1.,0.)) ;
#85026 = DIRECTION('ref_axis',(1.,0.,0.)) ;
#85027 = DIRECTION('center_axis',(0.497468338163092,0.710669054518701,0.497468338163092)) ;
#85028 = DIRECTION('ref_axis',(1.11733937654106E-14,0.573462344363324,-0.819231920519043)) ;
#85029 = DIRECTION('center_axis',(-0.497468338163091,-0.710669054518702,-0.497468338163091)) ;
#85030 = DIRECTION('ref_axis',(0.81923192051904,-0.573462344363328,7.6535433881835E-16)) ;
#85031 = DIRECTION('center_axis',(-0.497468338163091,-0.710669054518702,-0.497468338163091)) ;
#85032 = DIRECTION('ref_axis',(0.81923192051904,-0.573462344363328,7.6535433881835E-16)) ;
#85033 = DIRECTION('center_axis',(0.,-1.,0.)) ;
#85034 = DIRECTION('ref_axis',(0.,0.,-1.)) ;
#85035 = DIRECTION('center_axis',(0.,1.,0.)) ;
#85036 = DIRECTION('ref_axis',(0.,0.,-1.)) ;
#85037 = DIRECTION('center_axis',(-8.67361737988403E-15,1.,0.)) ;
#85038 = DIRECTION('ref_axis',(-1.,-8.67361737988403E-15,0.)) ;
#85039 = DIRECTION('center_axis',(0.,0.,1.)) ;
#85040 = DIRECTION('ref_axis',(1.,0.,0.)) ;
#85041 = DIRECTION('center_axis',(1.,6.67201336914158E-17,0.)) ;
#85042 = DIRECTION('ref_axis',(-6.67201336914158E-17,1.,0.)) ;
#85043 = DIRECTION('center_axis',(-1.,-6.67201336914158E-17,0.)) ;
#85044 = DIRECTION('ref_axis',(-6.67201336914158E-17,1.,0.)) ;
#85045 = DIRECTION('center_axis',(-1.,1.33440267382831E-16,0.)) ;
#85046 = DIRECTION('ref_axis',(-1.33440267382831E-16,-1.,0.)) ;
#85047 = DIRECTION('center_axis',(-1.,1.33440267382831E-16,0.)) ;
#85048 = DIRECTION('ref_axis',(-1.33440267382831E-16,-1.,0.)) ;
#85049 = DIRECTION('center_axis',(0.710669054518702,0.497468338163091,0.497468338163091)) ;
#85050 = DIRECTION('ref_axis',(-0.573462344363328,0.819231920519041,3.92980824865032E-16)) ;
#85051 = DIRECTION('center_axis',(0.710669054518702,0.497468338163091,0.497468338163091)) ;
#85052 = DIRECTION('ref_axis',(-0.573462344363328,0.819231920519041,3.92980824865032E-16)) ;
#85053 = DIRECTION('center_axis',(0.710669054518701,0.497468338163091,0.497468338163092)) ;
#85054 = DIRECTION('ref_axis',(0.57346234436333,-1.81382726107456E-15,-0.819231920519039)) ;
#85055 = DIRECTION('center_axis',(-0.710669054518702,0.497468338163091,-0.497468338163091)) ;
#85056 = DIRECTION('ref_axis',(-0.573462344363328,-0.819231920519041,6.69271761853466E-16)) ;
#85057 = DIRECTION('center_axis',(0.710669054518702,-0.497468338163091,0.497468338163091)) ;
#85058 = DIRECTION('ref_axis',(-0.573462344363328,-0.819231920519041,6.69271761853466E-16)) ;
#85059 = DIRECTION('center_axis',(0.7106690545187,-0.497468338163094,0.497468338163091)) ;
#85060 = DIRECTION('ref_axis',(0.573462344363331,0.819231920519038,2.86772422505918E-16)) ;
#85061 = DIRECTION('center_axis',(0.,1.,-9.34081871679819E-17)) ;
#85062 = DIRECTION('ref_axis',(0.,9.34081871679819E-17,1.)) ;
#85063 = DIRECTION('center_axis',(-4.33680868994205E-15,-1.,-3.03576608295944E-15)) ;
#85064 = DIRECTION('ref_axis',(1.,-4.33680868994205E-15,-1.12103877145985E-44)) ;
#85065 = DIRECTION('center_axis',(0.,1.,5.29374964685745E-15)) ;
#85066 = DIRECTION('ref_axis',(0.,-5.29374964685745E-15,1.)) ;
#85067 = DIRECTION('center_axis',(0.,1.,0.)) ;
#85068 = DIRECTION('ref_axis',(1.,0.,0.)) ;
#85069 = DIRECTION('center_axis',(0.,6.45175738210751E-15,1.)) ;
#85070 = DIRECTION('ref_axis',(0.,1.,-6.45175738210751E-15)) ;
#85071 = DIRECTION('center_axis',(-1.,-6.67201336914158E-17,0.)) ;
#85072 = DIRECTION('ref_axis',(6.67201336914158E-17,-1.,0.)) ;
#85073 = DIRECTION('center_axis',(-1.,-6.67201336914158E-17,0.)) ;
#85074 = DIRECTION('ref_axis',(6.67201336914158E-17,-1.,0.)) ;
#85075 = DIRECTION('center_axis',(1.,-1.33440267382831E-16,0.)) ;
#85076 = DIRECTION('ref_axis',(1.33440267382831E-16,1.,0.)) ;
#85077 = DIRECTION('center_axis',(-1.,1.33440267382831E-16,0.)) ;
#85078 = DIRECTION('ref_axis',(1.33440267382831E-16,1.,0.)) ;
#85079 = DIRECTION('center_axis',(0.,1.,0.)) ;
#85080 = DIRECTION('ref_axis',(1.,0.,0.)) ;
#85081 = DIRECTION('center_axis',(1.76182853028896E-15,-1.23327997120227E-15,
1.)) ;
#85082 = DIRECTION('ref_axis',(-1.,-2.1728278390981E-30,1.76182853028896E-15)) ;
#85083 = DIRECTION('center_axis',(0.,0.,-1.)) ;
#85084 = DIRECTION('ref_axis',(-1.,0.,0.)) ;
#85085 = DIRECTION('center_axis',(-2.71050543121378E-16,-1.89735380184965E-16,
1.)) ;
#85086 = DIRECTION('ref_axis',(1.,-5.14278778484758E-32,2.71050543121378E-16)) ;
#85087 = DIRECTION('center_axis',(-0.710669054518702,-0.497468338163091,0.497468338163091)) ;
#85088 = DIRECTION('ref_axis',(0.573462344363328,-0.819231920519041,3.92980824865032E-16)) ;
#85089 = DIRECTION('center_axis',(0.710669054518702,0.497468338163091,-0.497468338163091)) ;
#85090 = DIRECTION('ref_axis',(0.573462344363328,-0.819231920519041,3.92980824865032E-16)) ;
#85091 = DIRECTION('center_axis',(0.710669054518701,0.497468338163091,-0.497468338163092)) ;
#85092 = DIRECTION('ref_axis',(-0.57346234436333,1.88103289405095E-15,-0.819231920519039)) ;
#85093 = DIRECTION('center_axis',(0.710669054518702,-0.497468338163091,-0.497468338163091)) ;
#85094 = DIRECTION('ref_axis',(0.573462344363328,0.819231920519041,6.69271761853466E-16)) ;
#85095 = DIRECTION('center_axis',(0.710669054518702,-0.497468338163091,-0.497468338163091)) ;
#85096 = DIRECTION('ref_axis',(0.573462344363328,0.819231920519041,6.69271761853466E-16)) ;
#85097 = DIRECTION('center_axis',(0.7106690545187,-0.497468338163091,-0.497468338163093)) ;
#85098 = DIRECTION('ref_axis',(-0.573462344363331,-1.17187023180681E-15,-0.819231920519038)) ;
#85099 = DIRECTION('center_axis',(0.,0.,-1.)) ;
#85100 = DIRECTION('ref_axis',(-1.,0.,0.)) ;
#85101 = DIRECTION('center_axis',(0.,1.15800773525007E-15,1.)) ;
#85102 = DIRECTION('ref_axis',(0.,-1.,1.15800773525007E-15)) ;
#85103 = DIRECTION('center_axis',(0.,1.,0.)) ;
#85104 = DIRECTION('ref_axis',(1.,0.,0.)) ;
#85105 = DIRECTION('center_axis',(0.,1.,0.)) ;
#85106 = DIRECTION('ref_axis',(0.,0.,-1.)) ;
#85107 = DIRECTION('center_axis',(0.,1.,0.)) ;
#85108 = DIRECTION('ref_axis',(1.,0.,0.)) ;
#85109 = DIRECTION('center_axis',(4.33680868994204E-15,-1.,-3.03576608295944E-15)) ;
#85110 = DIRECTION('ref_axis',(-1.,-4.33680868994204E-15,5.60519385729927E-45)) ;
#85111 = DIRECTION('center_axis',(0.,1.,9.34081871679819E-17)) ;
#85112 = DIRECTION('ref_axis',(0.,-9.34081871679819E-17,1.)) ;
#85113 = DIRECTION('center_axis',(0.,0.,1.)) ;
#85114 = DIRECTION('ref_axis',(1.,0.,0.)) ;
#85115 = DIRECTION('center_axis',(-2.16840434497102E-15,-3.61400724161847E-16,
1.)) ;
#85116 = DIRECTION('ref_axis',(1.,-7.83662900548222E-31,2.16840434497102E-15)) ;
#85117 = DIRECTION('center_axis',(0.973328526784575,0.162221421130762,-0.162221421130763)) ;
#85118 = DIRECTION('ref_axis',(-0.164398987305358,9.23743777622416E-16,-0.986393923832144)) ;
#85119 = DIRECTION('center_axis',(0.973328526784574,0.162221421130765,-0.162221421130767)) ;
#85120 = DIRECTION('ref_axis',(-0.164398987305362,1.88956506020588E-16,-0.986393923832143)) ;
#85121 = DIRECTION('center_axis',(0.,1.,0.)) ;
#85122 = DIRECTION('ref_axis',(1.,0.,0.)) ;
#85123 = DIRECTION('center_axis',(0.,1.,-8.79325913341701E-15)) ;
#85124 = DIRECTION('ref_axis',(1.73472347597682E-14,-8.79325913341701E-15,
-1.)) ;
#85125 = DIRECTION('center_axis',(0.,0.,1.)) ;
#85126 = DIRECTION('ref_axis',(1.,0.,0.)) ;
#85127 = DIRECTION('center_axis',(0.,-2.28569887277128E-15,1.)) ;
#85128 = DIRECTION('ref_axis',(0.,-1.,-2.28569887277128E-15)) ;
#85129 = DIRECTION('center_axis',(1.73472347597681E-15,-1.,-2.89120579329468E-16)) ;
#85130 = DIRECTION('ref_axis',(1.,1.73472347597681E-15,5.01544256350843E-31)) ;
#85131 = DIRECTION('center_axis',(8.67361737988409E-15,1.,-1.44560289664739E-15)) ;
#85132 = DIRECTION('ref_axis',(-1.,8.67361737988409E-15,-1.40129846432482E-45)) ;
#85133 = DIRECTION('center_axis',(0.,1.,0.)) ;
#85134 = DIRECTION('ref_axis',(1.,0.,0.)) ;
#85135 = DIRECTION('center_axis',(-0.937042571331634,0.312347523777217,0.156173761888611)) ;
#85136 = DIRECTION('ref_axis',(0.316227766016843,0.948683298050512,6.71158276827649E-18)) ;
#85137 = DIRECTION('center_axis',(0.937042571331636,-0.312347523777212,-0.156173761888606)) ;
#85138 = DIRECTION('ref_axis',(0.316227766016838,0.948683298050514,8.61595672567599E-16)) ;
#85139 = DIRECTION('center_axis',(-0.973328526784575,-0.162221421130762,-0.162221421130763)) ;
#85140 = DIRECTION('ref_axis',(-0.164398987305358,9.23743777622416E-16,0.986393923832144)) ;
#85141 = DIRECTION('center_axis',(0.978231976292136,-0.146734796047237,-0.146734795425481)) ;
#85142 = DIRECTION('ref_axis',(0.182318633544167,0.945435290916785,0.270022270473533)) ;
#85143 = DIRECTION('center_axis',(0.973328526784574,0.162221421130767,0.162221421130768)) ;
#85144 = DIRECTION('ref_axis',(0.164398987305363,-6.69215935033609E-18,-0.986393923832143)) ;
#85145 = DIRECTION('center_axis',(0.,0.,1.)) ;
#85146 = DIRECTION('ref_axis',(1.,0.,0.)) ;
#85147 = DIRECTION('center_axis',(0.,2.19831478335425E-15,-1.)) ;
#85148 = DIRECTION('ref_axis',(0.,1.,2.19831478335425E-15)) ;
#85149 = DIRECTION('center_axis',(0.,1.,0.)) ;
#85150 = DIRECTION('ref_axis',(1.,0.,0.)) ;
#85151 = DIRECTION('center_axis',(8.67361737988408E-15,1.,1.44560289664739E-15)) ;
#85152 = DIRECTION('ref_axis',(1.,-8.67361737988408E-15,5.60519385729927E-45)) ;
#85153 = DIRECTION('center_axis',(1.73472347597681E-15,-1.,2.89120579329468E-16)) ;
#85154 = DIRECTION('ref_axis',(1.,1.73472347597681E-15,-5.01544256350843E-31)) ;
#85155 = DIRECTION('center_axis',(0.,1.,0.)) ;
#85156 = DIRECTION('ref_axis',(0.,0.,1.)) ;
#85157 = DIRECTION('center_axis',(0.,0.,1.)) ;
#85158 = DIRECTION('ref_axis',(1.,0.,0.)) ;
#85159 = DIRECTION('center_axis',(3.25260651745652E-15,-1.08420217248553E-15,
-1.)) ;
#85160 = DIRECTION('ref_axis',(-1.,-3.52648305246695E-30,-3.25260651745652E-15)) ;
#85161 = DIRECTION('center_axis',(0.,1.,0.)) ;
#85162 = DIRECTION('ref_axis',(1.,0.,0.)) ;
#85163 = DIRECTION('center_axis',(-0.937042571331635,0.312347523777215,-0.15617376188861)) ;
#85164 = DIRECTION('ref_axis',(0.316227766016841,0.948683298050513,6.5590042956861E-18)) ;
#85165 = DIRECTION('center_axis',(-0.937042571331636,0.312347523777212,-0.156173761888606)) ;
#85166 = DIRECTION('ref_axis',(0.331350514299552,0.654034959159453,-0.680033167478407)) ;
#85167 = DIRECTION('center_axis',(0.96151972409117,0.245047216428557,-0.124224320904791)) ;
#85168 = DIRECTION('ref_axis',(0.262092069904638,-0.682554728314085,0.682221950503784)) ;
#85169 = DIRECTION('center_axis',(2.65552944032596E-32,3.29043518662928E-48,
-1.)) ;
#85170 = DIRECTION('ref_axis',(-1.,8.7378475095785E-80,-2.65552944032596E-32)) ;
#85171 = DIRECTION('center_axis',(2.65552944032596E-32,3.29043518662928E-48,
-1.)) ;
#85172 = DIRECTION('ref_axis',(-1.,8.7378475095785E-80,-2.65552944032596E-32)) ;
#85173 = DIRECTION('center_axis',(-2.65552944032596E-32,-3.29043518662928E-48,
1.)) ;
#85174 = DIRECTION('ref_axis',(-1.,8.7378475095785E-80,-2.65552944032596E-32)) ;
#85175 = DIRECTION('center_axis',(0.,0.,1.)) ;
#85176 = DIRECTION('ref_axis',(1.,0.,0.)) ;
#85177 = DIRECTION('center_axis',(0.,0.,-1.)) ;
#85178 = DIRECTION('ref_axis',(-1.,0.,0.)) ;
#85179 = DIRECTION('center_axis',(0.,0.,1.)) ;
#85180 = DIRECTION('ref_axis',(1.,0.,0.)) ;
#85181 = DIRECTION('center_axis',(0.,0.,1.)) ;
#85182 = DIRECTION('ref_axis',(1.,0.,0.)) ;
#85183 = DIRECTION('center_axis',(0.,0.,-1.)) ;
#85184 = DIRECTION('ref_axis',(-1.,0.,0.)) ;
#85185 = DIRECTION('center_axis',(0.,0.,-1.)) ;
#85186 = DIRECTION('ref_axis',(-1.,0.,0.)) ;
#85187 = DIRECTION('center_axis',(1.,1.15648231731787E-15,0.)) ;
#85188 = DIRECTION('ref_axis',(1.03435541192675E-15,-1.,5.17177705963374E-16)) ;
#85189 = DIRECTION('center_axis',(7.089177613099E-16,-0.612994899008946,-0.790086864711098)) ;
#85190 = DIRECTION('ref_axis',(-1.7347234759768E-14,-0.790086864711098,0.612994899008946)) ;
#85191 = DIRECTION('center_axis',(7.08917761309899E-16,-0.612994899008945,
0.790086864711098)) ;
#85192 = DIRECTION('ref_axis',(-3.46944695195361E-14,0.790086864711098,0.612994899008945)) ;
#85193 = DIRECTION('center_axis',(0.,0.,-1.)) ;
#85194 = DIRECTION('ref_axis',(-1.,0.,0.)) ;
#85195 = DIRECTION('center_axis',(0.,0.,1.)) ;
#85196 = DIRECTION('ref_axis',(-1.,2.16840434497102E-15,0.)) ;
#85197 = DIRECTION('center_axis',(1.08420217248551E-15,-1.,0.)) ;
#85198 = DIRECTION('ref_axis',(1.,1.08420217248551E-15,0.)) ;
#85199 = DIRECTION('center_axis',(1.44560289664734E-16,-1.,-2.4093381610789E-16)) ;
#85200 = DIRECTION('ref_axis',(2.28544744656275E-46,2.4093381610789E-16,-1.)) ;
#85201 = DIRECTION('center_axis',(0.,-1.,0.)) ;
#85202 = DIRECTION('ref_axis',(0.,0.,-1.)) ;
#85203 = DIRECTION('center_axis',(1.,0.,0.)) ;
#85204 = DIRECTION('ref_axis',(0.,1.,0.)) ;
#85205 = DIRECTION('center_axis',(1.,0.,0.)) ;
#85206 = DIRECTION('ref_axis',(0.,0.,-1.)) ;
#85207 = DIRECTION('center_axis',(1.,1.23908819712629E-16,8.95614743483648E-33)) ;
#85208 = DIRECTION('ref_axis',(-1.23908819712629E-16,1.,-1.10974565782288E-48)) ;
#85209 = DIRECTION('center_axis',(1.,0.,0.)) ;
#85210 = DIRECTION('ref_axis',(0.,0.,-1.)) ;
#85211 = DIRECTION('center_axis',(-1.,0.,0.)) ;
#85212 = DIRECTION('ref_axis',(0.,0.,1.)) ;
#85213 = DIRECTION('center_axis',(1.,1.23908819712629E-16,8.95614743483648E-33)) ;
#85214 = DIRECTION('ref_axis',(-1.23908819712629E-16,1.,-1.10974565782288E-48)) ;
#85215 = DIRECTION('center_axis',(-1.,0.,0.)) ;
#85216 = DIRECTION('ref_axis',(0.,0.,1.)) ;
#85217 = DIRECTION('center_axis',(1.,0.,0.)) ;
#85218 = DIRECTION('ref_axis',(0.,-1.,0.)) ;
#85219 = DIRECTION('center_axis',(0.,1.,0.)) ;
#85220 = DIRECTION('ref_axis',(0.,0.,1.)) ;
#85221 = DIRECTION('center_axis',(-1.44560289664734E-16,1.,-7.2280144832367E-17)) ;
#85222 = DIRECTION('ref_axis',(0.707106781238328,1.5332934167208E-16,0.707106781134767)) ;
#85223 = DIRECTION('center_axis',(-1.0842021724855E-15,1.,0.)) ;
#85224 = DIRECTION('ref_axis',(-1.,-1.0842021724855E-15,0.)) ;
#85225 = DIRECTION('center_axis',(0.,1.,0.)) ;
#85226 = DIRECTION('ref_axis',(0.,0.,1.)) ;
#85227 = DIRECTION('center_axis',(0.,-1.,0.)) ;
#85228 = DIRECTION('ref_axis',(0.,0.,-1.)) ;
#85229 = DIRECTION('center_axis',(0.,1.,0.)) ;
#85230 = DIRECTION('ref_axis',(0.,0.,1.)) ;
#85231 = DIRECTION('center_axis',(0.,0.,1.)) ;
#85232 = DIRECTION('ref_axis',(1.,0.,0.)) ;
#85233 = DIRECTION('center_axis',(0.43119164676634,0.0335421424328467,0.901636672080249)) ;
#85234 = DIRECTION('ref_axis',(0.899826811350493,0.0573593271358461,-0.432459960187447)) ;
#85235 = DIRECTION('center_axis',(0.,0.,1.)) ;
#85236 = DIRECTION('ref_axis',(-1.,0.,0.)) ;
#85237 = DIRECTION('center_axis',(0.,0.,-1.)) ;
#85238 = DIRECTION('ref_axis',(0.707109343403326,-0.707104218960485,0.)) ;
#85239 = DIRECTION('center_axis',(-3.25260651745653E-15,0.,1.)) ;
#85240 = DIRECTION('ref_axis',(1.,0.,3.25260651745653E-15)) ;
#85241 = DIRECTION('center_axis',(0.,0.,1.)) ;
#85242 = DIRECTION('ref_axis',(1.,0.,0.)) ;
#85243 = DIRECTION('center_axis',(0.431188264321889,0.0335835001222771,-0.901636750155302)) ;
#85244 = DIRECTION('ref_axis',(0.899831768148625,0.0572892325239029,0.432458937781775)) ;
#85245 = DIRECTION('center_axis',(0.,-1.,0.)) ;
#85246 = DIRECTION('ref_axis',(0.,0.,-1.)) ;
#85247 = DIRECTION('center_axis',(0.,1.,0.)) ;
#85248 = DIRECTION('ref_axis',(0.,0.,1.)) ;
#85249 = DIRECTION('center_axis',(0.,0.,1.)) ;
#85250 = DIRECTION('ref_axis',(1.,0.,0.)) ;
#85251 = DIRECTION('center_axis',(0.,0.,-1.)) ;
#85252 = DIRECTION('ref_axis',(-1.,0.,0.)) ;
#85253 = DIRECTION('center_axis',(0.,0.,1.)) ;
#85254 = DIRECTION('ref_axis',(-0.986393923832144,0.164398987305354,0.)) ;
#85255 = DIRECTION('center_axis',(0.98470178743927,-0.164116964573216,0.0585492250433781)) ;
#85256 = DIRECTION('ref_axis',(0.164398987305362,0.986393923832143,-7.60669428566932E-17)) ;
#85257 = DIRECTION('center_axis',(0.984834538781277,-0.164139089796902,0.0562075655416074)) ;
#85258 = DIRECTION('ref_axis',(0.164398987305379,0.98639392383214,1.87706412796466E-17)) ;
#85259 = DIRECTION('center_axis',(0.986393923832145,-0.129889480441767,0.100775740620414)) ;
#85260 = DIRECTION('ref_axis',(0.,0.612994899008951,0.790086864711094)) ;
#85261 = DIRECTION('center_axis',(0.,1.,0.)) ;
#85262 = DIRECTION('ref_axis',(1.,0.,0.)) ;
#85263 = DIRECTION('center_axis',(0.,0.,-1.)) ;
#85264 = DIRECTION('ref_axis',(-1.,0.,0.)) ;
#85265 = DIRECTION('center_axis',(1.,2.8359373108165E-15,0.)) ;
#85266 = DIRECTION('ref_axis',(-2.8359373108165E-15,1.,0.)) ;
#85267 = DIRECTION('center_axis',(0.,0.,-1.)) ;
#85268 = DIRECTION('ref_axis',(-1.,0.,0.)) ;
#85269 = DIRECTION('center_axis',(0.,0.,1.)) ;
#85270 = DIRECTION('ref_axis',(1.,0.,0.)) ;
#85271 = DIRECTION('center_axis',(1.,0.,0.)) ;
#85272 = DIRECTION('ref_axis',(0.,0.,-1.)) ;
#85273 = DIRECTION('center_axis',(1.,0.,0.)) ;
#85274 = DIRECTION('ref_axis',(0.,0.,-1.)) ;
#85275 = DIRECTION('center_axis',(0.,1.,0.)) ;
#85276 = DIRECTION('ref_axis',(1.,0.,0.)) ;
#85277 = DIRECTION('center_axis',(1.,-8.50781193244945E-15,0.)) ;
#85278 = DIRECTION('ref_axis',(8.50781193244945E-15,1.,0.)) ;
#85279 = DIRECTION('center_axis',(0.,1.,0.)) ;
#85280 = DIRECTION('ref_axis',(1.,0.,0.)) ;
#85281 = DIRECTION('center_axis',(-5.42101086242753E-16,1.70882313734897E-16,
1.)) ;
#85282 = DIRECTION('ref_axis',(1.,9.26354878953623E-32,5.42101086242753E-16)) ;
#85283 = DIRECTION('center_axis',(-1.,0.,0.)) ;
#85284 = DIRECTION('ref_axis',(0.,0.,1.)) ;
#85285 = DIRECTION('center_axis',(1.,0.,0.)) ;
#85286 = DIRECTION('ref_axis',(0.,0.,-1.)) ;
#85287 = DIRECTION('center_axis',(0.,0.,-1.)) ;
#85288 = DIRECTION('ref_axis',(-1.,0.,0.)) ;
#85289 = DIRECTION('center_axis',(0.,0.,1.)) ;
#85290 = DIRECTION('ref_axis',(1.,0.,0.)) ;
#85291 = DIRECTION('center_axis',(0.,1.,0.)) ;
#85292 = DIRECTION('ref_axis',(1.,0.,0.)) ;
#85293 = DIRECTION('center_axis',(0.,1.,0.)) ;
#85294 = DIRECTION('ref_axis',(1.,0.,0.)) ;
#85295 = DIRECTION('center_axis',(0.,0.,-1.)) ;
#85296 = DIRECTION('ref_axis',(-1.,0.,0.)) ;
#85297 = DIRECTION('center_axis',(0.,1.,0.)) ;
#85298 = DIRECTION('ref_axis',(0.,0.,1.)) ;
#85299 = DIRECTION('center_axis',(0.,0.,-1.)) ;
#85300 = DIRECTION('ref_axis',(-1.,0.,0.)) ;
#85301 = DIRECTION('center_axis',(0.,0.,1.)) ;
#85302 = DIRECTION('ref_axis',(1.,0.,0.)) ;
#85303 = DIRECTION('center_axis',(1.33440267382831E-16,1.,0.)) ;
#85304 = DIRECTION('ref_axis',(-1.,1.33440267382831E-16,0.)) ;
#85305 = DIRECTION('center_axis',(0.,1.,0.)) ;
#85306 = DIRECTION('ref_axis',(0.,0.,1.)) ;
#85307 = DIRECTION('center_axis',(0.,1.,0.)) ;
#85308 = DIRECTION('ref_axis',(1.,0.,0.)) ;
#85309 = DIRECTION('center_axis',(0.,1.,0.)) ;
#85310 = DIRECTION('ref_axis',(0.,0.,1.)) ;
#85311 = DIRECTION('center_axis',(0.,1.,0.)) ;
#85312 = DIRECTION('ref_axis',(1.,0.,0.)) ;
#85313 = DIRECTION('center_axis',(1.37797793267296E-15,-1.62630325872825E-15,
1.)) ;
#85314 = DIRECTION('ref_axis',(-2.24101000236165E-30,-1.,-1.62630325872825E-15)) ;
#85315 = DIRECTION('center_axis',(-1.33440267382831E-16,-1.,0.)) ;
#85316 = DIRECTION('ref_axis',(1.,-1.33440267382831E-16,0.)) ;
#85317 = DIRECTION('center_axis',(0.,1.,0.)) ;
#85318 = DIRECTION('ref_axis',(0.,0.,1.)) ;
#85319 = DIRECTION('center_axis',(0.,0.,-1.)) ;
#85320 = DIRECTION('ref_axis',(-1.,0.,0.)) ;
#85321 = DIRECTION('center_axis',(0.,0.,1.)) ;
#85322 = DIRECTION('ref_axis',(1.,0.,0.)) ;
#85323 = DIRECTION('center_axis',(0.,1.,0.)) ;
#85324 = DIRECTION('ref_axis',(1.,0.,0.)) ;
#85325 = DIRECTION('center_axis',(0.,0.,1.)) ;
#85326 = DIRECTION('ref_axis',(1.,0.,0.)) ;
#85327 = DIRECTION('center_axis',(0.,0.,1.)) ;
#85328 = DIRECTION('ref_axis',(1.,0.,0.)) ;
#85329 = DIRECTION('center_axis',(0.,0.,1.)) ;
#85330 = DIRECTION('ref_axis',(-0.986393923832144,0.164398987305354,0.)) ;
#85331 = DIRECTION('center_axis',(0.984701787439272,-0.164116964573205,-0.0585492250433871)) ;
#85332 = DIRECTION('ref_axis',(0.16439898730535,0.986393923832145,-3.2807868055655E-16)) ;
#85333 = DIRECTION('center_axis',(0.984834538781259,-0.164139089796881,-0.0562075655419907)) ;
#85334 = DIRECTION('ref_axis',(0.164398987305362,0.986393923832143,6.03508511856301E-17)) ;
#85335 = DIRECTION('center_axis',(0.,0.,1.)) ;
#85336 = DIRECTION('ref_axis',(-0.986393923832144,0.164398987305354,0.)) ;
#85337 = DIRECTION('center_axis',(0.,0.,1.)) ;
#85338 = DIRECTION('ref_axis',(1.,0.,0.)) ;
#85339 = DIRECTION('center_axis',(0.342346838787153,0.100237737284617,-0.934211452507677)) ;
#85340 = DIRECTION('ref_axis',(0.878411919475056,0.318727606806516,0.356097195135737)) ;
#85341 = DIRECTION('center_axis',(0.,0.,-1.)) ;
#85342 = DIRECTION('ref_axis',(-1.,0.,0.)) ;
#85343 = DIRECTION('center_axis',(0.,0.,-1.)) ;
#85344 = DIRECTION('ref_axis',(-1.,0.,0.)) ;
#85345 = DIRECTION('center_axis',(0.,0.,-1.)) ;
#85346 = DIRECTION('ref_axis',(-1.,0.,0.)) ;
#85347 = DIRECTION('center_axis',(-0.34234683878929,-0.100237737302457,-0.93421145250498)) ;
#85348 = DIRECTION('ref_axis',(0.878411847182506,0.318727811137727,-0.356097190576915)) ;
#85349 = DIRECTION('center_axis',(0.,0.,1.)) ;
#85350 = DIRECTION('ref_axis',(1.,0.,0.)) ;
#85351 = DIRECTION('center_axis',(0.967224433215112,0.251696851080207,0.0335498278387964)) ;
#85352 = DIRECTION('ref_axis',(0.148186147792394,-0.666803866446761,0.730351606621154)) ;
#85353 = DIRECTION('center_axis',(0.,0.707106781186549,-0.707106781186547)) ;
#85354 = DIRECTION('ref_axis',(0.,0.707106781186546,0.707106781186549)) ;
#85355 = DIRECTION('center_axis',(0.978007532938648,-0.147978541149372,-0.146981688909074)) ;
#85356 = DIRECTION('ref_axis',(0.193734423938021,0.383507624685324,0.9029888564039)) ;
#85357 = DIRECTION('center_axis',(0.,0.447213595499958,0.894427190999916)) ;
#85358 = DIRECTION('ref_axis',(0.,-0.894427190999916,0.447213595499958)) ;
#85359 = DIRECTION('center_axis',(0.960001452008207,0.250435160947592,-0.125217579849191)) ;
#85360 = DIRECTION('ref_axis',(0.276742394167975,-0.916645079797593,0.28840153424183)) ;
#85361 = DIRECTION('center_axis',(0.,1.,0.)) ;
#85362 = DIRECTION('ref_axis',(0.,0.,1.)) ;
#85363 = DIRECTION('center_axis',(-1.,0.,0.)) ;
#85364 = DIRECTION('ref_axis',(0.,0.41390516857167,-0.910320004959606)) ;
#85365 = DIRECTION('center_axis',(1.,1.44560289664734E-16,0.)) ;
#85366 = DIRECTION('ref_axis',(0.,1.,0.)) ;
#85367 = DIRECTION('center_axis',(1.,1.44560289664734E-16,0.)) ;
#85368 = DIRECTION('ref_axis',(-1.44560289664734E-16,1.,0.)) ;
#85369 = DIRECTION('center_axis',(0.,0.,-1.)) ;
#85370 = DIRECTION('ref_axis',(0.,-1.,0.)) ;
#85371 = DIRECTION('center_axis',(-1.,-1.44560289664734E-16,0.)) ;
#85372 = DIRECTION('ref_axis',(-1.44560289664734E-16,1.,0.)) ;
#85373 = DIRECTION('center_axis',(1.,-3.46944695195361E-16,0.)) ;
#85374 = DIRECTION('ref_axis',(2.61228946970625E-16,1.,0.)) ;
#85375 = DIRECTION('center_axis',(1.,-3.46944695195361E-16,0.)) ;
#85376 = DIRECTION('ref_axis',(3.46944695195361E-16,1.,0.)) ;
#85377 = DIRECTION('center_axis',(0.,0.,1.)) ;
#85378 = DIRECTION('ref_axis',(-3.26536183713281E-16,-1.,0.)) ;
#85379 = DIRECTION('center_axis',(-1.,3.46944695195361E-16,0.)) ;
#85380 = DIRECTION('ref_axis',(3.46944695195361E-16,1.,0.)) ;
#85381 = DIRECTION('center_axis',(-1.,3.46944695195361E-16,0.)) ;
#85382 = DIRECTION('ref_axis',(-3.46944695195361E-16,-1.,0.)) ;
#85383 = DIRECTION('center_axis',(-1.,0.,0.)) ;
#85384 = DIRECTION('ref_axis',(0.,0.,1.)) ;
#85385 = DIRECTION('',(1.,-3.46944695195361E-16,0.)) ;
#85386 = DIRECTION('center_axis',(-1.,8.01625584951926E-16,-1.08420217248551E-15)) ;
#85387 = DIRECTION('ref_axis',(1.08420217248552E-15,6.50521303491307E-15,
-1.)) ;
#85388 = DIRECTION('center_axis',(-1.,8.01625584951926E-16,-1.08420217248551E-15)) ;
#85389 = DIRECTION('ref_axis',(1.08420217248552E-15,6.50521303491307E-15,
-1.)) ;
#85390 = DIRECTION('',(-1.,3.46944695195361E-16,0.)) ;
#85391 = DIRECTION('center_axis',(-1.,3.46944695195361E-16,0.)) ;
#85392 = DIRECTION('ref_axis',(-3.46944695195361E-16,-1.,0.)) ;
#85393 = DIRECTION('center_axis',(-1.,0.,0.)) ;
#85394 = DIRECTION('ref_axis',(0.,0.,1.)) ;
#85395 = DIRECTION('',(1.,-3.46944695195361E-16,0.)) ;
#85396 = DIRECTION('center_axis',(-1.,2.2680138501079E-15,0.)) ;
#85397 = DIRECTION('ref_axis',(2.2680138501079E-15,1.,0.)) ;
#85398 = DIRECTION('',(-1.,3.46944695195361E-16,0.)) ;
#85399 = DIRECTION('center_axis',(-1.,3.18032637262401E-16,0.)) ;
#85400 = DIRECTION('ref_axis',(-5.55111512312578E-16,-1.,0.)) ;
#85401 = DIRECTION('center_axis',(1.,-3.18032637262401E-16,0.)) ;
#85402 = DIRECTION('ref_axis',(-3.18032637262401E-16,-1.,0.)) ;
#85403 = DIRECTION('center_axis',(-2.01298417874256E-16,-0.632948931301568,
-0.774193548387096)) ;
#85404 = DIRECTION('ref_axis',(-1.73472347597679E-14,-0.774193548387096,0.632948931301568)) ;
#85405 = DIRECTION('center_axis',(-1.,3.18032637262401E-16,0.)) ;
#85406 = DIRECTION('ref_axis',(-3.18032637262401E-16,-1.,0.)) ;
#85407 = DIRECTION('center_axis',(-2.01298417874256E-16,-0.632948931301568,
0.774193548387096)) ;
#85408 = DIRECTION('ref_axis',(-2.5982535921668E-30,-0.774193548387096,-0.632948931301568)) ;
#85409 = DIRECTION('center_axis',(1.,1.44560289664734E-16,0.)) ;
#85410 = DIRECTION('ref_axis',(-1.44560289664734E-16,1.,0.)) ;
#85411 = DIRECTION('',(-1.,-1.44560289664734E-16,0.)) ;
#85412 = DIRECTION('center_axis',(-1.,3.46944695195361E-16,0.)) ;
#85413 = DIRECTION('ref_axis',(-3.46944695195361E-16,-1.,0.)) ;
#85414 = DIRECTION('',(-1.,3.46944695195361E-16,0.)) ;
#85415 = DIRECTION('center_axis',(-1.,3.46944695195361E-16,0.)) ;
#85416 = DIRECTION('ref_axis',(3.46944695195361E-16,1.,0.)) ;
#85417 = DIRECTION('center_axis',(-1.,3.46944695195361E-16,0.)) ;
#85418 = DIRECTION('ref_axis',(3.46944695195361E-16,1.,0.)) ;
#85419 = DIRECTION('center_axis',(-1.,3.46944695195361E-16,0.)) ;
#85420 = DIRECTION('ref_axis',(-3.46944695195361E-16,-1.,0.)) ;
#85421 = DIRECTION('',(1.,-3.46944695195361E-16,0.)) ;
#85422 = DIRECTION('center_axis',(-1.,-1.44560289664734E-16,-2.65552944032596E-32)) ;
#85423 = DIRECTION('ref_axis',(1.44560289664734E-16,-1.,-2.80018320648271E-64)) ;
#85424 = DIRECTION('',(2.65552944032596E-32,3.29043518662928E-48,-1.)) ;
#85425 = DIRECTION('',(1.44560289664734E-16,-1.,-2.4093381610789E-16)) ;
#85426 = DIRECTION('',(0.,0.,1.)) ;
#85427 = DIRECTION('center_axis',(0.999999956301289,0.000282786981350015,
8.61913163546712E-5)) ;
#85428 = DIRECTION('ref_axis',(0.000288266391185019,-0.997396273404882,-0.0721151211643056)) ;
#85429 = DIRECTION('',(-1.44560289664734E-16,1.,-7.2280144832367E-17)) ;
#85430 = DIRECTION('center_axis',(0.316227766016838,0.948683298050514,0.)) ;
#85431 = DIRECTION('ref_axis',(-0.948683298050514,0.316227766016838,0.)) ;
#85432 = DIRECTION('',(-0.948683298050514,0.316227766016838,0.)) ;
#85433 = DIRECTION('',(0.,0.,1.)) ;
#85434 = DIRECTION('',(0.937042571331636,-0.312347523777212,-0.156173761888606)) ;
#85435 = DIRECTION('',(0.,0.,-1.)) ;
#85436 = DIRECTION('center_axis',(1.,1.73472347597681E-15,0.)) ;
#85437 = DIRECTION('ref_axis',(-1.73472347597681E-15,1.,0.)) ;
#85438 = DIRECTION('',(-1.73472347597681E-15,1.,0.)) ;
#85439 = DIRECTION('',(0.,0.,1.)) ;
#85440 = DIRECTION('',(1.73472347597681E-15,-1.,-2.89120579329468E-16)) ;
#85441 = DIRECTION('',(0.,0.,-1.)) ;
#85442 = DIRECTION('center_axis',(0.164398987305357,-0.986393923832144,0.)) ;
#85443 = DIRECTION('ref_axis',(0.986393923832144,0.164398987305357,0.)) ;
#85444 = DIRECTION('',(-0.973328526784575,-0.162221421130762,0.162221421130763)) ;
#85445 = DIRECTION('',(0.,0.,-1.)) ;
#85446 = DIRECTION('',(0.986393923832144,0.164398987305357,0.)) ;
#85447 = DIRECTION('',(0.,0.,1.)) ;
#85448 = DIRECTION('center_axis',(-9.91270557701033E-17,1.,0.)) ;
#85449 = DIRECTION('ref_axis',(-1.,-9.91270557701033E-17,0.)) ;
#85450 = DIRECTION('',(1.,9.91270557701033E-17,0.)) ;
#85451 = DIRECTION('',(0.,0.,-1.)) ;
#85452 = DIRECTION('',(-1.,-9.91270557701033E-17,0.)) ;
#85453 = DIRECTION('',(0.,0.,1.)) ;
#85454 = DIRECTION('center_axis',(-9.91270557701033E-17,1.,0.)) ;
#85455 = DIRECTION('ref_axis',(-1.,-9.91270557701033E-17,0.)) ;
#85456 = DIRECTION('',(-1.,-9.91270557701033E-17,0.)) ;
#85457 = DIRECTION('',(0.,0.,-1.)) ;
#85458 = DIRECTION('',(-1.,-9.91270557701033E-17,0.)) ;
#85459 = DIRECTION('',(0.,0.,1.)) ;
#85460 = DIRECTION('center_axis',(1.,1.15648231731787E-15,0.)) ;
#85461 = DIRECTION('ref_axis',(-1.15648231731787E-15,1.,0.)) ;
#85462 = DIRECTION('',(-1.15648231731787E-15,1.,0.)) ;
#85463 = DIRECTION('',(0.,0.,-1.)) ;
#85464 = DIRECTION('',(-1.15648231731787E-15,1.,0.)) ;
#85465 = DIRECTION('',(0.,0.,1.)) ;
#85466 = DIRECTION('center_axis',(-1.,-1.15648231731787E-15,0.)) ;
#85467 = DIRECTION('ref_axis',(-1.15648231731787E-15,1.,0.)) ;
#85468 = DIRECTION('',(0.,0.,1.)) ;
#85469 = DIRECTION('center_axis',(0.,0.,1.)) ;
#85470 = DIRECTION('ref_axis',(1.,0.,0.)) ;
#85471 = DIRECTION('',(-1.,0.,0.)) ;
#85472 = DIRECTION('center_axis',(0.,0.,-1.)) ;
#85473 = DIRECTION('ref_axis',(1.,0.,0.)) ;
#85474 = DIRECTION('center_axis',(0.,0.,-1.)) ;
#85475 = DIRECTION('ref_axis',(1.,0.,0.)) ;
#85476 = DIRECTION('center_axis',(0.,0.,-1.)) ;
#85477 = DIRECTION('ref_axis',(1.,0.,0.)) ;
#85478 = DIRECTION('center_axis',(0.,0.,-1.)) ;
#85479 = DIRECTION('ref_axis',(1.,0.,0.)) ;
#85480 = DIRECTION('',(1.,0.,0.)) ;
#85481 = DIRECTION('center_axis',(0.,0.,1.)) ;
#85482 = DIRECTION('ref_axis',(1.,0.,0.)) ;
#85483 = DIRECTION('',(3.46944695195361E-16,1.,0.)) ;
#85484 = DIRECTION('center_axis',(0.,0.,1.)) ;
#85485 = DIRECTION('ref_axis',(1.,0.,0.)) ;
#85486 = DIRECTION('',(1.,-3.46944695195361E-16,0.)) ;
#85487 = DIRECTION('center_axis',(0.,0.,-1.)) ;
#85488 = DIRECTION('ref_axis',(1.,0.,0.)) ;
#85489 = DIRECTION('',(2.71050543121376E-16,1.,0.)) ;
#85490 = DIRECTION('center_axis',(0.,0.,-1.)) ;
#85491 = DIRECTION('ref_axis',(1.,0.,0.)) ;
#85492 = DIRECTION('',(-1.,3.46944695195361E-16,0.)) ;
#85493 = DIRECTION('center_axis',(0.,0.,1.)) ;
#85494 = DIRECTION('ref_axis',(1.,0.,0.)) ;
#85495 = DIRECTION('',(3.46944695195361E-16,1.,0.)) ;
#85496 = DIRECTION('center_axis',(0.,0.,1.)) ;
#85497 = DIRECTION('ref_axis',(1.,0.,0.)) ;
#85498 = DIRECTION('center_axis',(0.,0.,-1.)) ;
#85499 = DIRECTION('ref_axis',(1.,0.,0.)) ;
#85500 = DIRECTION('',(0.986393923832144,-0.164398987305354,0.)) ;
#85501 = DIRECTION('center_axis',(0.,0.,-1.)) ;
#85502 = DIRECTION('ref_axis',(1.,-6.50521303491307E-15,0.)) ;
#85503 = DIRECTION('center_axis',(0.,0.,-1.)) ;
#85504 = DIRECTION('ref_axis',(1.,0.,0.)) ;
#85505 = DIRECTION('',(1.,0.,0.)) ;
#85506 = DIRECTION('',(1.13380619344889E-16,-1.,0.)) ;
#85507 = DIRECTION('center_axis',(0.,0.,-1.)) ;
#85508 = DIRECTION('ref_axis',(1.,0.,0.)) ;
#85509 = DIRECTION('',(-1.,-1.92747052886312E-16,0.)) ;
#85510 = DIRECTION('center_axis',(0.,0.,1.)) ;
#85511 = DIRECTION('ref_axis',(1.,0.,0.)) ;
#85512 = DIRECTION('',(0.,-1.,0.)) ;
#85513 = DIRECTION('center_axis',(0.,0.,-1.)) ;
#85514 = DIRECTION('ref_axis',(1.,0.,0.)) ;
#85515 = DIRECTION('center_axis',(0.,0.,1.)) ;
#85516 = DIRECTION('ref_axis',(1.,0.,0.)) ;
#85517 = DIRECTION('',(-0.948683298050514,0.316227766016838,0.)) ;
#85518 = DIRECTION('center_axis',(0.,0.,1.)) ;
#85519 = DIRECTION('ref_axis',(1.,0.,0.)) ;
#85520 = DIRECTION('',(-1.,0.,0.)) ;
#85521 = DIRECTION('center_axis',(0.,0.,1.)) ;
#85522 = DIRECTION('ref_axis',(1.,0.,0.)) ;
#85523 = DIRECTION('',(0.,-1.,0.)) ;
#85524 = DIRECTION('center_axis',(0.,0.,-1.)) ;
#85525 = DIRECTION('ref_axis',(1.,0.,0.)) ;
#85526 = DIRECTION('',(-1.,-1.92747052886312E-16,0.)) ;
#85527 = DIRECTION('center_axis',(0.,0.,1.)) ;
#85528 = DIRECTION('ref_axis',(1.,0.,0.)) ;
#85529 = DIRECTION('',(1.13380619344889E-16,-1.,0.)) ;
#85530 = DIRECTION('',(1.,0.,0.)) ;
#85531 = DIRECTION('center_axis',(0.,0.,1.)) ;
#85532 = DIRECTION('ref_axis',(1.,0.,0.)) ;
#85533 = DIRECTION('center_axis',(0.,0.,1.)) ;
#85534 = DIRECTION('ref_axis',(1.,0.,0.)) ;
#85535 = DIRECTION('',(-0.986393923832144,0.164398987305354,0.)) ;
#85536 = DIRECTION('center_axis',(0.,0.,1.)) ;
#85537 = DIRECTION('ref_axis',(1.,0.,0.)) ;
#85538 = DIRECTION('center_axis',(0.,0.,-1.)) ;
#85539 = DIRECTION('ref_axis',(1.,0.,0.)) ;
#85540 = DIRECTION('',(-3.46944695195361E-16,-1.,0.)) ;
#85541 = DIRECTION('center_axis',(0.,0.,-1.)) ;
#85542 = DIRECTION('ref_axis',(1.,0.,0.)) ;
#85543 = DIRECTION('',(-1.,3.46944695195361E-16,0.)) ;
#85544 = DIRECTION('center_axis',(0.,0.,1.)) ;
#85545 = DIRECTION('ref_axis',(1.,0.,0.)) ;
#85546 = DIRECTION('',(3.46944695195361E-16,1.,0.)) ;
#85547 = DIRECTION('center_axis',(0.,0.,1.)) ;
#85548 = DIRECTION('ref_axis',(1.,0.,0.)) ;
#85549 = DIRECTION('',(1.,-3.46944695195361E-16,0.)) ;
#85550 = DIRECTION('center_axis',(0.,0.,-1.)) ;
#85551 = DIRECTION('ref_axis',(1.,0.,0.)) ;
#85552 = DIRECTION('',(-3.46944695195361E-16,-1.,0.)) ;
#85553 = DIRECTION('center_axis',(0.,0.,-1.)) ;
#85554 = DIRECTION('ref_axis',(1.,0.,0.)) ;
#85555 = DIRECTION('',(1.,0.,0.)) ;
#85556 = DIRECTION('center_axis',(0.,0.,1.)) ;
#85557 = DIRECTION('ref_axis',(1.,0.,0.)) ;
#85558 = DIRECTION('',(0.986393923832144,0.164398987305357,0.)) ;
#85559 = DIRECTION('center_axis',(0.,0.,1.)) ;
#85560 = DIRECTION('ref_axis',(1.,0.,0.)) ;
#85561 = DIRECTION('',(-1.73472347597681E-15,1.,0.)) ;
#85562 = DIRECTION('center_axis',(0.,0.,1.)) ;
#85563 = DIRECTION('ref_axis',(1.,0.,0.)) ;
#85564 = DIRECTION('center_axis',(-1.92747052886312E-16,1.,0.)) ;
#85565 = DIRECTION('ref_axis',(-1.,-1.92747052886312E-16,0.)) ;
#85566 = DIRECTION('',(0.,0.,1.)) ;
#85567 = DIRECTION('',(0.,0.,-1.)) ;
#85568 = DIRECTION('center_axis',(-1.,0.,0.)) ;
#85569 = DIRECTION('ref_axis',(0.,0.,1.)) ;
#85570 = DIRECTION('',(0.,0.,1.)) ;
#85571 = DIRECTION('',(0.,0.,-1.)) ;
#85572 = DIRECTION('center_axis',(0.,1.,0.)) ;
#85573 = DIRECTION('ref_axis',(0.,0.,1.)) ;
#85574 = DIRECTION('',(0.,0.,-1.)) ;
#85575 = DIRECTION('',(0.,0.,1.)) ;
#85576 = DIRECTION('',(0.,0.,-1.)) ;
#85577 = DIRECTION('',(0.,0.,-1.)) ;
#85578 = DIRECTION('center_axis',(0.316227766016838,0.948683298050514,0.)) ;
#85579 = DIRECTION('ref_axis',(-0.948683298050514,0.316227766016838,0.)) ;
#85580 = DIRECTION('center_axis',(-0.316227766016838,-0.948683298050514,0.)) ;
#85581 = DIRECTION('ref_axis',(0.83159596074681,-0.27719865358227,-0.481257794245212)) ;
#85582 = DIRECTION('',(0.,0.,1.)) ;
#85583 = DIRECTION('',(0.,0.,-1.)) ;
#85584 = DIRECTION('',(-0.937042571331636,0.312347523777212,-0.156173761888606)) ;
#85585 = DIRECTION('center_axis',(1.,1.73472347597681E-15,0.)) ;
#85586 = DIRECTION('ref_axis',(-1.73472347597681E-15,1.,0.)) ;
#85587 = DIRECTION('',(-1.73472347597681E-15,1.,-2.89120579329468E-16)) ;
#85588 = DIRECTION('',(0.,0.,1.)) ;
#85589 = DIRECTION('',(0.,0.,-1.)) ;
#85590 = DIRECTION('center_axis',(0.164398987305357,-0.986393923832144,0.)) ;
#85591 = DIRECTION('ref_axis',(0.986393923832144,0.164398987305357,0.)) ;
#85592 = DIRECTION('',(0.973328526784575,0.162221421130762,0.162221421130763)) ;
#85593 = DIRECTION('',(0.,0.,1.)) ;
#85594 = DIRECTION('',(0.,0.,-1.)) ;
#85595 = DIRECTION('center_axis',(0.,-1.,0.)) ;
#85596 = DIRECTION('ref_axis',(0.,0.,-1.)) ;
#85597 = DIRECTION('',(0.,0.,1.)) ;
#85598 = DIRECTION('',(0.,0.,1.)) ;
#85599 = DIRECTION('',(0.,0.,1.)) ;
#85600 = DIRECTION('',(0.,0.,-1.)) ;
#85601 = DIRECTION('',(1.,0.,2.25271179641597E-31)) ;
#85602 = DIRECTION('center_axis',(0.,-1.,0.)) ;
#85603 = DIRECTION('ref_axis',(0.,0.,-1.)) ;
#85604 = DIRECTION('',(0.,0.,-1.)) ;
#85605 = DIRECTION('center_axis',(0.,-1.,0.)) ;
#85606 = DIRECTION('ref_axis',(0.,0.,-1.)) ;
#85607 = DIRECTION('',(-1.,0.,-3.21815970916568E-32)) ;
#85608 = DIRECTION('',(0.,0.,-1.)) ;
#85609 = DIRECTION('center_axis',(1.,-3.46944695195361E-16,0.)) ;
#85610 = DIRECTION('ref_axis',(3.46944695195361E-16,1.,0.)) ;
#85611 = DIRECTION('center_axis',(1.,-3.46944695195361E-16,0.)) ;
#85612 = DIRECTION('ref_axis',(3.46944695195361E-16,1.,0.)) ;
#85613 = DIRECTION('',(1.5529910948782E-31,4.47619207437002E-16,-1.)) ;
#85614 = DIRECTION('',(0.,0.,1.)) ;
#85615 = DIRECTION('center_axis',(1.,-3.46944695195361E-16,0.)) ;
#85616 = DIRECTION('ref_axis',(3.46944695195361E-16,1.,0.)) ;
#85617 = DIRECTION('center_axis',(1.,-3.46944695195361E-16,0.)) ;
#85618 = DIRECTION('ref_axis',(3.46944695195361E-16,1.,0.)) ;
#85619 = DIRECTION('center_axis',(1.,-3.46944695195361E-16,0.)) ;
#85620 = DIRECTION('ref_axis',(3.46944695195361E-16,1.,0.)) ;
#85621 = DIRECTION('',(3.46944695195361E-16,1.,9.27571383489107E-17)) ;
#85622 = DIRECTION('',(0.,0.,1.)) ;
#85623 = DIRECTION('',(-3.46944695195361E-16,-1.,-6.49299968442375E-16)) ;
#85624 = DIRECTION('center_axis',(1.,-3.46944695195361E-16,0.)) ;
#85625 = DIRECTION('ref_axis',(3.46944695195361E-16,1.,0.)) ;
#85626 = DIRECTION('center_axis',(1.,-3.46944695195361E-16,0.)) ;
#85627 = DIRECTION('ref_axis',(3.46944695195361E-16,1.,0.)) ;
#85628 = DIRECTION('center_axis',(1.,-3.46944695195361E-16,0.)) ;
#85629 = DIRECTION('ref_axis',(3.46944695195361E-16,1.,0.)) ;
#85630 = DIRECTION('',(0.,0.,1.)) ;
#85631 = DIRECTION('',(-1.5529910948782E-31,-4.47619207437002E-16,-1.)) ;
#85632 = DIRECTION('center_axis',(1.,-3.46944695195361E-16,0.)) ;
#85633 = DIRECTION('ref_axis',(3.46944695195361E-16,1.,0.)) ;
#85634 = DIRECTION('center_axis',(1.,-3.46944695195361E-16,0.)) ;
#85635 = DIRECTION('ref_axis',(3.46944695195361E-16,1.,0.)) ;
#85636 = DIRECTION('center_axis',(1.,-3.46944695195361E-16,0.)) ;
#85637 = DIRECTION('ref_axis',(3.46944695195361E-16,1.,0.)) ;
#85638 = DIRECTION('',(-3.46944695195361E-16,-1.,-1.06487173641454E-15)) ;
#85639 = DIRECTION('center_axis',(1.,-3.46944695195361E-16,0.)) ;
#85640 = DIRECTION('ref_axis',(3.46944695195361E-16,1.,0.)) ;
#85641 = DIRECTION('',(3.46944695195361E-16,1.,2.45739631480277E-16)) ;
#85642 = DIRECTION('center_axis',(1.,-3.46944695195361E-16,0.)) ;
#85643 = DIRECTION('ref_axis',(3.46944695195361E-16,1.,0.)) ;
#85644 = DIRECTION('center_axis',(1.,-3.46944695195361E-16,0.)) ;
#85645 = DIRECTION('ref_axis',(3.46944695195361E-16,1.,0.)) ;
#85646 = DIRECTION('center_axis',(0.,-1.,0.)) ;
#85647 = DIRECTION('ref_axis',(0.,0.,-1.)) ;
#85648 = DIRECTION('center_axis',(0.,-1.,0.)) ;
#85649 = DIRECTION('ref_axis',(0.,0.,-1.)) ;
#85650 = DIRECTION('',(-1.,0.,-1.40488587213121E-32)) ;
#85651 = DIRECTION('',(0.,0.,1.)) ;
#85652 = DIRECTION('',(0.,0.,1.)) ;
#85653 = DIRECTION('',(0.,0.,1.)) ;
#85654 = DIRECTION('',(1.,0.,1.40488587213121E-32)) ;
#85655 = DIRECTION('center_axis',(0.,-1.,0.)) ;
#85656 = DIRECTION('ref_axis',(0.,0.,-1.)) ;
#85657 = DIRECTION('',(7.2280144832367E-17,0.,-1.)) ;
#85658 = DIRECTION('center_axis',(-1.,-1.13380619344889E-16,0.)) ;
#85659 = DIRECTION('ref_axis',(1.13380619344889E-16,-1.,0.)) ;
#85660 = DIRECTION('center_axis',(-1.,-1.13380619344889E-16,0.)) ;
#85661 = DIRECTION('ref_axis',(1.13380619344889E-16,-1.,0.)) ;
#85662 = DIRECTION('',(1.13380619344889E-16,-1.,1.23908819712629E-16)) ;
#85663 = DIRECTION('',(0.,0.,-1.)) ;
#85664 = DIRECTION('',(-1.13380619344889E-16,1.,-1.23908819712629E-16)) ;
#85665 = DIRECTION('center_axis',(-1.,-1.13380619344889E-16,0.)) ;
#85666 = DIRECTION('ref_axis',(1.13380619344889E-16,-1.,0.)) ;
#85667 = DIRECTION('',(0.,0.,1.)) ;
#85668 = DIRECTION('center_axis',(-1.40488587213121E-32,1.23908819712629E-16,
1.)) ;
#85669 = DIRECTION('ref_axis',(0.,-1.,1.23908819712629E-16)) ;
#85670 = DIRECTION('',(-1.,0.,-1.40488587213121E-32)) ;
#85671 = DIRECTION('',(-1.13380619344889E-16,1.,-1.23908819712629E-16)) ;
#85672 = DIRECTION('center_axis',(1.40488587213121E-32,-1.23908819712629E-16,
-1.)) ;
#85673 = DIRECTION('ref_axis',(-1.74077750246726E-48,-1.,1.23908819712629E-16)) ;
#85674 = DIRECTION('center_axis',(1.40488587213121E-32,-1.23908819712629E-16,
-1.)) ;
#85675 = DIRECTION('ref_axis',(0.,1.,-1.23908819712629E-16)) ;
#85676 = DIRECTION('center_axis',(-1.40488587213121E-32,1.23908819712629E-16,
1.)) ;
#85677 = DIRECTION('ref_axis',(1.74077750246726E-48,1.,-1.23908819712629E-16)) ;
#85678 = DIRECTION('',(1.13380619344889E-16,-1.,1.23908819712629E-16)) ;
#85679 = DIRECTION('',(1.,0.,1.40488587213121E-32)) ;
#85680 = DIRECTION('center_axis',(-1.,-1.23908819712629E-16,-8.95614743483648E-33)) ;
#85681 = DIRECTION('ref_axis',(1.23908819712629E-16,-1.,5.38566640001825E-66)) ;
#85682 = DIRECTION('',(-8.95614743483648E-33,-1.10974565782288E-48,1.)) ;
#85683 = DIRECTION('',(1.23908819712629E-16,-1.,7.2280144832367E-17)) ;
#85684 = DIRECTION('',(-8.95614743483648E-33,0.,1.)) ;
#85685 = DIRECTION('',(-1.23908819712629E-16,1.,-1.23908819712629E-16)) ;
#85686 = DIRECTION('',(8.95614743483648E-33,1.0154535431059E-48,-1.)) ;
#85687 = DIRECTION('',(1.23908819712629E-16,-1.,1.23908819712629E-16)) ;
#85688 = DIRECTION('',(-8.95614743483648E-33,0.,1.)) ;
#85689 = DIRECTION('',(-1.23908819712629E-16,1.,2.4093381610789E-16)) ;
#85690 = DIRECTION('center_axis',(-1.7912294869673E-32,7.2280144832367E-17,
1.)) ;
#85691 = DIRECTION('ref_axis',(0.,-1.,7.2280144832367E-17)) ;
#85692 = DIRECTION('',(-1.23908819712629E-16,1.,-7.2280144832367E-17)) ;
#85693 = DIRECTION('',(1.,1.23908819712629E-16,8.95614743483648E-33)) ;
#85694 = DIRECTION('',(1.44560289664734E-16,-1.,7.2280144832367E-17)) ;
#85695 = DIRECTION('',(-1.,0.,-1.7912294869673E-32)) ;
#85696 = DIRECTION('center_axis',(-2.08976773479518E-32,2.4093381610789E-16,
-1.)) ;
#85697 = DIRECTION('ref_axis',(0.,1.,2.4093381610789E-16)) ;
#85698 = DIRECTION('',(-1.44560289664734E-16,1.,2.4093381610789E-16)) ;
#85699 = DIRECTION('',(-1.,-1.23908819712629E-16,-8.95614743483648E-33)) ;
#85700 = DIRECTION('',(1.23908819712629E-16,-1.,-2.4093381610789E-16)) ;
#85701 = DIRECTION('',(1.,0.,-2.08976773479518E-32)) ;
#85702 = DIRECTION('center_axis',(-1.23908819712629E-16,1.,0.)) ;
#85703 = DIRECTION('ref_axis',(-1.,-1.23908819712629E-16,0.)) ;
#85704 = DIRECTION('',(8.95614743483648E-33,1.10974565782288E-48,-1.)) ;
#85705 = DIRECTION('',(1.,1.23908819712629E-16,8.95614743483648E-33)) ;
#85706 = DIRECTION('',(-2.65552944032596E-32,-3.29043518662928E-48,1.)) ;
#85707 = DIRECTION('',(-1.,-1.23908819712629E-16,-8.95614743483648E-33)) ;
#85708 = DIRECTION('center_axis',(-1.,-1.44560289664734E-16,-2.65552944032596E-32)) ;
#85709 = DIRECTION('ref_axis',(1.44560289664734E-16,-1.,-2.80018320648271E-64)) ;
#85710 = DIRECTION('',(1.44560289664734E-16,-1.,-2.4093381610789E-16)) ;
#85711 = DIRECTION('',(-2.65552944032596E-32,0.,1.)) ;
#85712 = DIRECTION('',(-1.44560289664734E-16,1.,-7.2280144832367E-17)) ;
#85713 = DIRECTION('',(0.,0.,-1.)) ;
#85714 = DIRECTION('center_axis',(0.,1.,0.)) ;
#85715 = DIRECTION('ref_axis',(0.,0.,1.)) ;
#85716 = DIRECTION('',(8.95614743483648E-33,0.,-1.)) ;
#85717 = DIRECTION('',(1.,0.,1.40488587213121E-32)) ;
#85718 = DIRECTION('',(-7.2280144832367E-17,0.,1.)) ;
#85719 = DIRECTION('',(-1.,0.,-1.40488587213121E-32)) ;
#85720 = DIRECTION('',(8.95614743483648E-33,0.,-1.)) ;
#85721 = DIRECTION('',(1.,0.,1.7912294869673E-32)) ;
#85722 = DIRECTION('',(2.65552944032596E-32,0.,-1.)) ;
#85723 = DIRECTION('',(-1.,0.,2.08976773479518E-32)) ;
#85724 = DIRECTION('center_axis',(1.,1.44560289664734E-16,0.)) ;
#85725 = DIRECTION('ref_axis',(-1.44560289664734E-16,1.,0.)) ;
#85726 = DIRECTION('',(1.44560289664734E-16,-1.,0.)) ;
#85727 = DIRECTION('center_axis',(-1.,-1.44560289664734E-16,0.)) ;
#85728 = DIRECTION('ref_axis',(-1.44560289664734E-16,1.,0.)) ;
#85729 = DIRECTION('',(0.,0.,-1.)) ;
#85730 = DIRECTION('center_axis',(-1.,-1.44560289664734E-16,0.)) ;
#85731 = DIRECTION('ref_axis',(-1.44560289664734E-16,1.,0.)) ;
#85732 = DIRECTION('',(1.44560289664734E-16,-1.,0.)) ;
#85733 = DIRECTION('center_axis',(-1.,-1.44560289664734E-16,0.)) ;
#85734 = DIRECTION('ref_axis',(-1.44560289664734E-16,1.,0.)) ;
#85735 = DIRECTION('',(0.,0.,1.)) ;
#85736 = DIRECTION('center_axis',(-1.,-1.44560289664734E-16,0.)) ;
#85737 = DIRECTION('ref_axis',(-1.44560289664734E-16,1.,0.)) ;
#85738 = DIRECTION('center_axis',(1.,-3.46944695195361E-16,0.)) ;
#85739 = DIRECTION('ref_axis',(3.46944695195361E-16,1.,0.)) ;
#85740 = DIRECTION('center_axis',(1.,-3.46944695195361E-16,0.)) ;
#85741 = DIRECTION('ref_axis',(3.46944695195361E-16,1.,0.)) ;
#85742 = DIRECTION('',(0.,0.,-1.)) ;
#85743 = DIRECTION('',(-1.5529910948782E-31,-4.47619207437002E-16,1.)) ;
#85744 = DIRECTION('center_axis',(-1.,3.46944695195361E-16,0.)) ;
#85745 = DIRECTION('ref_axis',(3.46944695195361E-16,1.,-1.87537673078574E-15)) ;
#85746 = DIRECTION('',(-3.46944695195361E-16,-1.,-2.45739631480277E-16)) ;
#85747 = DIRECTION('center_axis',(1.,-3.46944695195361E-16,0.)) ;
#85748 = DIRECTION('ref_axis',(3.46944695195361E-16,1.,0.)) ;
#85749 = DIRECTION('center_axis',(3.46944695195361E-16,1.,4.47619207437002E-16)) ;
#85750 = DIRECTION('ref_axis',(-8.18685017503995E-48,-4.47619207437002E-16,
1.)) ;
#85751 = DIRECTION('',(-1.5529910948782E-31,-4.47619207437002E-16,1.)) ;
#85752 = DIRECTION('',(-1.,3.46944695195361E-16,0.)) ;
#85753 = DIRECTION('',(1.5529910948782E-31,4.47619207437002E-16,-1.)) ;
#85754 = DIRECTION('center_axis',(-8.52580615413453E-32,-2.45739631480277E-16,
1.)) ;
#85755 = DIRECTION('ref_axis',(0.,-1.,-2.45739631480277E-16)) ;
#85756 = DIRECTION('',(1.,-3.46944695195361E-16,0.)) ;
#85757 = DIRECTION('',(-3.46944695195361E-16,-1.,-2.45739631480277E-16)) ;
#85758 = DIRECTION('',(3.46944695195361E-16,1.,2.45739631480277E-16)) ;
#85759 = DIRECTION('center_axis',(1.,-3.46944695195361E-16,0.)) ;
#85760 = DIRECTION('ref_axis',(3.46944695195361E-16,1.,0.)) ;
#85761 = DIRECTION('center_axis',(1.,-3.46944695195361E-16,0.)) ;
#85762 = DIRECTION('ref_axis',(3.46944695195361E-16,1.,0.)) ;
#85763 = DIRECTION('',(1.,-3.46944695195361E-16,0.)) ;
#85764 = DIRECTION('center_axis',(-1.,3.46944695195361E-16,0.)) ;
#85765 = DIRECTION('ref_axis',(3.46944695195361E-16,1.,1.98254111540207E-15)) ;
#85766 = DIRECTION('',(-1.,3.46944695195361E-16,0.)) ;
#85767 = DIRECTION('center_axis',(1.,-3.46944695195361E-16,0.)) ;
#85768 = DIRECTION('ref_axis',(3.46944695195361E-16,1.,0.)) ;
#85769 = DIRECTION('center_axis',(1.,-3.46944695195361E-16,0.)) ;
#85770 = DIRECTION('ref_axis',(-3.46944695195361E-16,-1.,1.18952466924124E-14)) ;
#85771 = DIRECTION('',(1.,-3.46944695195361E-16,0.)) ;
#85772 = DIRECTION('center_axis',(-1.,3.46944695195361E-16,0.)) ;
#85773 = DIRECTION('ref_axis',(3.46944695195361E-16,1.,5.9476233462062E-15)) ;
#85774 = DIRECTION('',(-1.,3.46944695195361E-16,0.)) ;
#85775 = DIRECTION('center_axis',(3.69451600012496E-31,1.06487173641454E-15,
-1.)) ;
#85776 = DIRECTION('ref_axis',(0.,1.,1.06487173641454E-15)) ;
#85777 = DIRECTION('',(3.46944695195361E-16,1.,1.06487173641454E-15)) ;
#85778 = DIRECTION('',(-1.,3.46944695195361E-16,0.)) ;
#85779 = DIRECTION('',(-3.46944695195361E-16,-1.,-1.06487173641454E-15)) ;
#85780 = DIRECTION('center_axis',(3.46944695195361E-16,1.,-4.47619207437002E-16)) ;
#85781 = DIRECTION('ref_axis',(8.18685017503995E-48,4.47619207437002E-16,
1.)) ;
#85782 = DIRECTION('',(1.,-3.46944695195361E-16,0.)) ;
#85783 = DIRECTION('',(1.5529910948782E-31,4.47619207437002E-16,1.)) ;
#85784 = DIRECTION('',(-1.5529910948782E-31,-4.47619207437002E-16,-1.)) ;
#85785 = DIRECTION('center_axis',(-1.,3.46944695195361E-16,0.)) ;
#85786 = DIRECTION('ref_axis',(-3.46944695195361E-16,-1.,0.)) ;
#85787 = DIRECTION('center_axis',(-1.,3.46944695195361E-16,0.)) ;
#85788 = DIRECTION('ref_axis',(-3.46944695195361E-16,-1.,0.)) ;
#85789 = DIRECTION('',(1.5529910948782E-31,4.47619207437002E-16,1.)) ;
#85790 = DIRECTION('',(0.,0.,-1.)) ;
#85791 = DIRECTION('center_axis',(1.,-3.46944695195361E-16,0.)) ;
#85792 = DIRECTION('ref_axis',(-3.46944695195361E-16,-1.,0.)) ;
#85793 = DIRECTION('center_axis',(1.,-3.46944695195361E-16,0.)) ;
#85794 = DIRECTION('ref_axis',(-3.46944695195361E-16,-1.,1.07672491612354E-14)) ;
#85795 = DIRECTION('',(3.46944695195361E-16,1.,1.06487173641454E-15)) ;
#85796 = DIRECTION('center_axis',(1.,-3.46944695195361E-16,0.)) ;
#85797 = DIRECTION('ref_axis',(3.46944695195361E-16,1.,0.)) ;
#85798 = DIRECTION('center_axis',(-1.,3.46944695195361E-16,0.)) ;
#85799 = DIRECTION('ref_axis',(3.46944695195361E-16,1.,0.)) ;
#85800 = DIRECTION('',(0.,0.,-1.)) ;
#85801 = DIRECTION('',(0.,0.,1.)) ;
#85802 = DIRECTION('',(-3.46944695195361E-16,-1.,-9.27571383489107E-17)) ;
#85803 = DIRECTION('center_axis',(-3.46944695195361E-16,-1.,0.)) ;
#85804 = DIRECTION('ref_axis',(1.,-3.46944695195361E-16,0.)) ;
#85805 = DIRECTION('',(1.,-3.46944695195361E-16,0.)) ;
#85806 = DIRECTION('',(0.,0.,-1.)) ;
#85807 = DIRECTION('',(0.,0.,1.)) ;
#85808 = DIRECTION('center_axis',(1.,-3.46944695195361E-16,0.)) ;
#85809 = DIRECTION('ref_axis',(3.46944695195361E-16,1.,0.)) ;
#85810 = DIRECTION('center_axis',(1.,-3.46944695195361E-16,0.)) ;
#85811 = DIRECTION('ref_axis',(3.46944695195361E-16,1.,0.)) ;
#85812 = DIRECTION('',(1.,-3.46944695195361E-16,0.)) ;
#85813 = DIRECTION('center_axis',(-1.,3.46944695195361E-16,0.)) ;
#85814 = DIRECTION('ref_axis',(3.46944695195361E-16,1.,0.)) ;
#85815 = DIRECTION('',(-1.,3.46944695195361E-16,0.)) ;
#85816 = DIRECTION('center_axis',(-3.21815970916568E-32,-9.27571383489107E-17,
1.)) ;
#85817 = DIRECTION('ref_axis',(0.,-1.,-9.27571383489107E-17)) ;
#85818 = DIRECTION('',(3.46944695195361E-16,1.,9.27571383489107E-17)) ;
#85819 = DIRECTION('',(1.,0.,3.21815970916568E-32)) ;
#85820 = DIRECTION('',(-3.46944695195361E-16,-1.,-9.27571383489107E-17)) ;
#85821 = DIRECTION('',(-1.,3.46944695195361E-16,0.)) ;
#85822 = DIRECTION('center_axis',(1.,-3.46944695195361E-16,0.)) ;
#85823 = DIRECTION('ref_axis',(3.46944695195361E-16,1.,0.)) ;
#85824 = DIRECTION('center_axis',(1.,-3.46944695195361E-16,0.)) ;
#85825 = DIRECTION('ref_axis',(-3.46944695195361E-16,-1.,-5.9476233462062E-15)) ;
#85826 = DIRECTION('',(1.,-3.46944695195361E-16,0.)) ;
#85827 = DIRECTION('center_axis',(-1.,3.46944695195361E-16,0.)) ;
#85828 = DIRECTION('ref_axis',(3.46944695195361E-16,1.,-1.98254111540207E-15)) ;
#85829 = DIRECTION('',(-1.,3.46944695195361E-16,0.)) ;
#85830 = DIRECTION('center_axis',(-3.46944695195361E-16,-1.,0.)) ;
#85831 = DIRECTION('ref_axis',(1.,-3.46944695195361E-16,0.)) ;
#85832 = DIRECTION('',(0.,0.,-1.)) ;
#85833 = DIRECTION('',(-1.,3.46944695195361E-16,0.)) ;
#85834 = DIRECTION('',(0.,0.,1.)) ;
#85835 = DIRECTION('center_axis',(2.25271179641597E-31,6.49299968442375E-16,
-1.)) ;
#85836 = DIRECTION('ref_axis',(0.,1.,6.49299968442375E-16)) ;
#85837 = DIRECTION('',(3.46944695195361E-16,1.,6.49299968442375E-16)) ;
#85838 = DIRECTION('',(-1.,0.,-2.25271179641597E-31)) ;
#85839 = DIRECTION('',(-3.46944695195361E-16,-1.,-6.49299968442375E-16)) ;
#85840 = DIRECTION('',(1.,-3.46944695195361E-16,0.)) ;
#85841 = DIRECTION('center_axis',(-1.,3.46944695195361E-16,0.)) ;
#85842 = DIRECTION('ref_axis',(-3.46944695195361E-16,-1.,0.)) ;
#85843 = DIRECTION('',(3.46944695195361E-16,1.,6.49299968442375E-16)) ;
#85844 = DIRECTION('',(0.,0.,1.)) ;
#85845 = DIRECTION('',(0.,0.,-1.)) ;
#85846 = DIRECTION('center_axis',(-1.,3.46944695195361E-16,0.)) ;
#85847 = DIRECTION('ref_axis',(-3.46944695195361E-16,-1.,0.)) ;
#85848 = DIRECTION('center_axis',(-0.164398987305357,0.,-0.986393923832144)) ;
#85849 = DIRECTION('ref_axis',(-0.986393923832144,0.,0.164398987305357)) ;
#85850 = DIRECTION('',(-0.937042571331636,0.312347523777212,0.156173761888606)) ;
#85851 = DIRECTION('',(0.,-1.,0.)) ;
#85852 = DIRECTION('',(0.973328526784575,0.162221421130762,-0.162221421130763)) ;
#85853 = DIRECTION('',(-1.73472347597681E-15,1.,2.89120579329468E-16)) ;
#85854 = DIRECTION('center_axis',(-1.,0.,0.)) ;
#85855 = DIRECTION('ref_axis',(0.,0.,1.)) ;
#85856 = DIRECTION('center_axis',(-1.,0.,0.)) ;
#85857 = DIRECTION('ref_axis',(0.,0.958781999165857,-0.284142707236211)) ;
#85858 = DIRECTION('',(0.,0.,1.)) ;
#85859 = DIRECTION('',(0.,-1.,0.)) ;
#85860 = DIRECTION('center_axis',(-1.,0.,0.)) ;
#85861 = DIRECTION('ref_axis',(0.,0.758706341404794,-0.65143279585246)) ;
#85862 = DIRECTION('',(0.,0.,-1.)) ;
#85863 = DIRECTION('center_axis',(-1.,0.,0.)) ;
#85864 = DIRECTION('ref_axis',(0.,-0.654779380094552,-0.755820060201497)) ;
#85865 = DIRECTION('',(0.,1.,0.)) ;
#85866 = DIRECTION('center_axis',(-0.164398987305357,0.,0.986393923832144)) ;
#85867 = DIRECTION('ref_axis',(0.986393923832144,0.,0.164398987305357)) ;
#85868 = DIRECTION('',(-0.973328526784575,-0.162221421130762,-0.162221421130763)) ;
#85869 = DIRECTION('',(0.,1.,0.)) ;
#85870 = DIRECTION('',(0.937042571331636,-0.312347523777212,0.156173761888606)) ;
#85871 = DIRECTION('',(1.73472347597681E-15,-1.,2.89120579329468E-16)) ;
#85872 = DIRECTION('center_axis',(-0.573462344363329,0.81923192051904,0.)) ;
#85873 = DIRECTION('ref_axis',(-0.81923192051904,-0.573462344363329,0.)) ;
#85874 = DIRECTION('',(-0.710669054518702,-0.497468338163091,0.49746833816309)) ;
#85875 = DIRECTION('',(0.,0.,-1.)) ;
#85876 = DIRECTION('',(0.710669054518702,0.497468338163091,0.49746833816309)) ;
#85877 = DIRECTION('',(0.,0.,1.)) ;
#85878 = DIRECTION('center_axis',(-1.,0.,0.)) ;
#85879 = DIRECTION('ref_axis',(0.,0.,1.)) ;
#85880 = DIRECTION('',(0.,0.,1.)) ;
#85881 = DIRECTION('',(0.,-1.,-9.34081871679819E-17)) ;
#85882 = DIRECTION('',(0.,0.,-1.)) ;
#85883 = DIRECTION('',(0.,1.,-9.34081871679819E-17)) ;
#85884 = DIRECTION('center_axis',(-0.573462344363329,-0.81923192051904,0.)) ;
#85885 = DIRECTION('ref_axis',(0.81923192051904,-0.573462344363329,0.)) ;
#85886 = DIRECTION('',(-0.710669054518701,0.497468338163091,-0.497468338163091)) ;
#85887 = DIRECTION('',(0.,0.,1.)) ;
#85888 = DIRECTION('',(0.710669054518701,-0.497468338163091,-0.497468338163091)) ;
#85889 = DIRECTION('',(0.,0.,-1.)) ;
#85890 = DIRECTION('center_axis',(0.,0.,1.)) ;
#85891 = DIRECTION('ref_axis',(1.,0.,0.)) ;
#85892 = DIRECTION('',(1.,6.67201336914158E-17,0.)) ;
#85893 = DIRECTION('',(1.33440267382831E-16,1.,0.)) ;
#85894 = DIRECTION('',(-1.,1.33440267382831E-16,0.)) ;
#85895 = DIRECTION('center_axis',(0.,0.,1.)) ;
#85896 = DIRECTION('ref_axis',(1.,0.,0.)) ;
#85897 = DIRECTION('',(1.,-1.33440267382831E-16,0.)) ;
#85898 = DIRECTION('',(-1.33440267382831E-16,-1.,0.)) ;
#85899 = DIRECTION('',(-1.,-6.67201336914158E-17,0.)) ;
#85900 = DIRECTION('center_axis',(-6.67201336914158E-17,1.,0.)) ;
#85901 = DIRECTION('ref_axis',(-1.,-6.67201336914158E-17,0.)) ;
#85902 = DIRECTION('',(1.,6.67201336914158E-17,0.)) ;
#85903 = DIRECTION('',(0.,0.,1.)) ;
#85904 = DIRECTION('',(-1.,-6.67201336914158E-17,0.)) ;
#85905 = DIRECTION('center_axis',(-1.33440267382831E-16,-1.,0.)) ;
#85906 = DIRECTION('ref_axis',(1.,-1.33440267382831E-16,0.)) ;
#85907 = DIRECTION('',(1.,-1.33440267382831E-16,0.)) ;
#85908 = DIRECTION('',(0.,0.,-1.)) ;
#85909 = DIRECTION('',(-1.,1.33440267382831E-16,0.)) ;
#85910 = DIRECTION('center_axis',(0.,0.,1.)) ;
#85911 = DIRECTION('ref_axis',(1.,0.,0.)) ;
#85912 = DIRECTION('',(0.,-1.,0.)) ;
#85913 = DIRECTION('',(1.,0.,0.)) ;
#85914 = DIRECTION('',(0.,1.,0.)) ;
#85915 = DIRECTION('center_axis',(0.,0.,-1.)) ;
#85916 = DIRECTION('ref_axis',(1.,0.,0.)) ;
#85917 = DIRECTION('',(-1.44560289664734E-16,1.,-7.2280144832367E-17)) ;
#85918 = DIRECTION('center_axis',(0.,0.,1.)) ;
#85919 = DIRECTION('ref_axis',(1.,0.,0.)) ;
#85920 = DIRECTION('center_axis',(0.,0.,1.)) ;
#85921 = DIRECTION('ref_axis',(1.,0.,0.)) ;
#85922 = DIRECTION('',(0.,-1.,0.)) ;
#85923 = DIRECTION('',(-1.,0.,0.)) ;
#85924 = DIRECTION('',(0.,1.,0.)) ;
#85925 = DIRECTION('center_axis',(0.,0.,-1.)) ;
#85926 = DIRECTION('ref_axis',(1.,-1.82602471155453E-15,0.)) ;
#85927 = DIRECTION('',(1.44560289664734E-16,-1.,-2.4093381610789E-16)) ;
#85928 = DIRECTION('center_axis',(0.,0.,1.)) ;
#85929 = DIRECTION('ref_axis',(1.,0.,0.)) ;
#85930 = DIRECTION('center_axis',(0.,0.,-1.)) ;
#85931 = DIRECTION('ref_axis',(-1.,0.,0.)) ;
#85932 = DIRECTION('',(0.,0.,-1.)) ;
#85933 = DIRECTION('center_axis',(0.,0.,-1.)) ;
#85934 = DIRECTION('ref_axis',(1.,0.,0.)) ;
#85935 = DIRECTION('center_axis',(0.,0.,1.)) ;
#85936 = DIRECTION('ref_axis',(1.,0.,0.)) ;
#85937 = DIRECTION('center_axis',(1.,0.,0.)) ;
#85938 = DIRECTION('ref_axis',(0.,0.,-1.)) ;
#85939 = DIRECTION('',(0.,-1.,0.)) ;
#85940 = DIRECTION('',(0.,0.,1.)) ;
#85941 = DIRECTION('',(0.,1.,0.)) ;
#85942 = DIRECTION('center_axis',(0.81923192051904,0.573462344363329,0.)) ;
#85943 = DIRECTION('ref_axis',(-0.573462344363329,0.81923192051904,0.)) ;
#85944 = DIRECTION('',(-0.497468338163091,0.710669054518701,0.497468338163091)) ;
#85945 = DIRECTION('',(0.,0.,-1.)) ;
#85946 = DIRECTION('',(0.497468338163091,-0.710669054518701,0.497468338163091)) ;
#85947 = DIRECTION('',(0.,0.,1.)) ;
#85948 = DIRECTION('center_axis',(0.,1.,0.)) ;
#85949 = DIRECTION('ref_axis',(0.,0.,1.)) ;
#85950 = DIRECTION('',(0.,0.,1.)) ;
#85951 = DIRECTION('',(-1.,0.,0.)) ;
#85952 = DIRECTION('',(0.,0.,-1.)) ;
#85953 = DIRECTION('',(1.,0.,0.)) ;
#85954 = DIRECTION('center_axis',(-0.81923192051904,0.573462344363329,0.)) ;
#85955 = DIRECTION('ref_axis',(-0.573462344363329,-0.81923192051904,0.)) ;
#85956 = DIRECTION('',(0.497468338163091,0.710669054518701,-0.497468338163091)) ;
#85957 = DIRECTION('',(0.,0.,1.)) ;
#85958 = DIRECTION('',(-0.497468338163091,-0.710669054518701,-0.497468338163091)) ;
#85959 = DIRECTION('',(0.,0.,-1.)) ;
#85960 = DIRECTION('center_axis',(-1.,0.,0.)) ;
#85961 = DIRECTION('ref_axis',(0.,0.,1.)) ;
#85962 = DIRECTION('',(0.,-1.,0.)) ;
#85963 = DIRECTION('',(0.,0.,-1.)) ;
#85964 = DIRECTION('',(0.,1.,0.)) ;
#85965 = DIRECTION('',(0.,0.,-1.)) ;
#85966 = DIRECTION('center_axis',(0.,0.,-1.)) ;
#85967 = DIRECTION('ref_axis',(-1.,0.,0.)) ;
#85968 = DIRECTION('center_axis',(0.,0.,1.)) ;
#85969 = DIRECTION('ref_axis',(1.,0.,0.)) ;
#85970 = DIRECTION('center_axis',(0.,0.,-1.)) ;
#85971 = DIRECTION('ref_axis',(1.,5.20417042793042E-15,0.)) ;
#85972 = DIRECTION('center_axis',(-0.573462344363328,7.65229685658278E-17,
0.819231920519041)) ;
#85973 = DIRECTION('ref_axis',(0.819231920519041,1.22423955297878E-32,0.573462344363328)) ;
#85974 = DIRECTION('',(-0.710669054518702,-0.497468338163091,-0.497468338163091)) ;
#85975 = DIRECTION('',(1.33440267382831E-16,1.,-2.91413396387194E-34)) ;
#85976 = DIRECTION('',(0.710669054518701,-0.497468338163091,0.497468338163091)) ;
#85977 = DIRECTION('',(5.04890651880155E-33,-1.,9.34081871679819E-17)) ;
#85978 = DIRECTION('center_axis',(-0.573462344363328,7.65229685658278E-17,
-0.819231920519041)) ;
#85979 = DIRECTION('ref_axis',(-0.819231920519041,-1.22423955297878E-32,0.573462344363328)) ;
#85980 = DIRECTION('',(-0.710669054518701,0.497468338163091,0.497468338163091)) ;
#85981 = DIRECTION('',(-1.33440267382831E-16,-1.,7.77328292223541E-33)) ;
#85982 = DIRECTION('',(0.710669054518702,0.497468338163091,-0.497468338163091)) ;
#85983 = DIRECTION('',(-5.04890651880155E-33,1.,9.34081871679819E-17)) ;
#85984 = DIRECTION('center_axis',(0.,0.573462344363328,-0.819231920519041)) ;
#85985 = DIRECTION('ref_axis',(0.,0.819231920519041,0.573462344363328)) ;
#85986 = DIRECTION('',(0.497468338163091,0.710669054518701,0.497468338163091)) ;
#85987 = DIRECTION('',(-1.,0.,0.)) ;
#85988 = DIRECTION('',(0.497468338163091,-0.710669054518701,-0.497468338163091)) ;
#85989 = DIRECTION('',(1.,0.,0.)) ;
#85990 = DIRECTION('center_axis',(0.,0.573462344363328,0.819231920519041)) ;
#85991 = DIRECTION('ref_axis',(0.,-0.819231920519041,0.573462344363328)) ;
#85992 = DIRECTION('',(-0.497468338163091,0.710669054518701,-0.497468338163091)) ;
#85993 = DIRECTION('',(1.,0.,0.)) ;
#85994 = DIRECTION('',(-0.497468338163091,-0.710669054518701,0.497468338163091)) ;
#85995 = DIRECTION('',(-1.,0.,0.)) ;
#85996 = DIRECTION('center_axis',(-0.164398987305354,-0.986393923832144,0.)) ;
#85997 = DIRECTION('ref_axis',(0.,0.,1.)) ;
#85998 = DIRECTION('',(0.,0.,-1.)) ;
#85999 = DIRECTION('center_axis',(-0.164398987305316,-0.986393923832151,-6.5096352405955E-13)) ;
#86000 = DIRECTION('ref_axis',(-0.0577290357396871,0.00962150595595322,0.998285923498727)) ;
#86001 = DIRECTION('',(0.,0.,1.)) ;
#86002 = DIRECTION('center_axis',(1.,-2.89120579329441E-16,0.)) ;
#86003 = DIRECTION('ref_axis',(-2.89120579329441E-16,-1.,-7.6571373978539E-16)) ;
#86004 = DIRECTION('center_axis',(1.,1.15648231731787E-15,0.)) ;
#86005 = DIRECTION('ref_axis',(1.15648231731787E-15,-1.,0.)) ;
#86006 = DIRECTION('center_axis',(0.166689823555444,0.983956802853964,0.0635886219418303)) ;
#86007 = DIRECTION('ref_axis',(-0.048648001075619,0.072619415360229,-0.996172571648148)) ;
#86008 = DIRECTION('center_axis',(0.166689823591591,0.983956802798768,-0.0635886227011592)) ;
#86009 = DIRECTION('ref_axis',(-0.0462047033417876,0.072214919745475,0.996318287875542)) ;
#86010 = DIRECTION('center_axis',(-0.164398987305354,-0.986393923832144,0.)) ;
#86011 = DIRECTION('ref_axis',(0.,0.,1.)) ;
#86012 = DIRECTION('',(0.,0.,1.)) ;
#86013 = DIRECTION('center_axis',(-0.164398987305377,-0.98639392383214,-4.33975683666443E-13)) ;
#86014 = DIRECTION('ref_axis',(-0.0554192327903482,0.00923653879883178,-0.99842045000488)) ;
#86015 = DIRECTION('',(0.,0.,-1.)) ;
#86016 = DIRECTION('center_axis',(0.,0.,1.)) ;
#86017 = DIRECTION('ref_axis',(1.,0.,0.)) ;
#86018 = DIRECTION('center_axis',(0.,0.,1.)) ;
#86019 = DIRECTION('ref_axis',(1.,0.,0.)) ;
#86020 = DIRECTION('center_axis',(0.,1.,0.)) ;
#86021 = DIRECTION('ref_axis',(1.,0.,0.)) ;
#86022 = DIRECTION('center_axis',(0.,-0.888198741900269,0.45945945945946)) ;
#86023 = DIRECTION('ref_axis',(0.,0.45945945945946,0.888198741900269)) ;
#86024 = DIRECTION('center_axis',(-1.,0.,1.22067519501986E-15)) ;
#86025 = DIRECTION('ref_axis',(-1.22067519501986E-15,0.,-1.)) ;
#86026 = DIRECTION('center_axis',(0.,0.,1.)) ;
#86027 = DIRECTION('ref_axis',(1.,0.,0.)) ;
#86028 = DIRECTION('center_axis',(0.,0.,-1.)) ;
#86029 = DIRECTION('ref_axis',(-1.,0.,0.)) ;
#86030 = DIRECTION('center_axis',(1.,-3.46944695195361E-16,0.)) ;
#86031 = DIRECTION('ref_axis',(3.46944695195361E-16,1.,0.)) ;
#86032 = DIRECTION('center_axis',(-1.,3.46944695195361E-16,0.)) ;
#86033 = DIRECTION('ref_axis',(3.46944695195361E-16,1.,0.)) ;
#86034 = DIRECTION('center_axis',(-1.,3.46944695195361E-16,0.)) ;
#86035 = DIRECTION('ref_axis',(-3.41607084500048E-16,-1.,0.)) ;
#86036 = DIRECTION('center_axis',(0.,-0.459459459459457,0.888198741900271)) ;
#86037 = DIRECTION('ref_axis',(0.,-0.888198741900271,-0.459459459459457)) ;
#86038 = DIRECTION('center_axis',(1.,-3.46944695195361E-16,0.)) ;
#86039 = DIRECTION('ref_axis',(0.,1.,0.)) ;
#86040 = DIRECTION('center_axis',(0.,0.888198741900269,-0.45945945945946)) ;
#86041 = DIRECTION('ref_axis',(0.,-0.45945945945946,-0.888198741900269)) ;
#86042 = DIRECTION('center_axis',(0.,1.,0.)) ;
#86043 = DIRECTION('ref_axis',(1.,0.,0.)) ;
#86044 = DIRECTION('center_axis',(0.,-1.,0.)) ;
#86045 = DIRECTION('ref_axis',(0.,0.,1.)) ;
#86046 = DIRECTION('center_axis',(-1.,0.,0.)) ;
#86047 = DIRECTION('ref_axis',(0.,0.,-1.)) ;
#86048 = DIRECTION('center_axis',(0.,0.,-1.)) ;
#86049 = DIRECTION('ref_axis',(-1.,0.,0.)) ;
#86050 = DIRECTION('center_axis',(0.,0.,-1.)) ;
#86051 = DIRECTION('ref_axis',(-1.,0.,0.)) ;
#86052 = DIRECTION('center_axis',(1.,-3.46944695195361E-16,0.)) ;
#86053 = DIRECTION('ref_axis',(3.46944695195361E-16,1.,0.)) ;
#86054 = DIRECTION('center_axis',(-1.,3.46944695195361E-16,0.)) ;
#86055 = DIRECTION('ref_axis',(3.46944695195361E-16,1.,3.46944695195361E-14)) ;
#86056 = DIRECTION('center_axis',(1.,0.,0.)) ;
#86057 = DIRECTION('ref_axis',(0.,0.,-1.)) ;
#86058 = DIRECTION('center_axis',(0.,0.,1.)) ;
#86059 = DIRECTION('ref_axis',(1.,0.,0.)) ;
#86060 = DIRECTION('center_axis',(0.,0.,1.)) ;
#86061 = DIRECTION('ref_axis',(1.,0.,0.)) ;
#86062 = DIRECTION('center_axis',(1.,-3.46944695195361E-16,0.)) ;
#86063 = DIRECTION('ref_axis',(3.80647894157197E-16,1.,0.)) ;
#86064 = DIRECTION('center_axis',(0.,0.459459459459459,-0.888198741900269)) ;
#86065 = DIRECTION('ref_axis',(0.,0.888198741900269,0.459459459459459)) ;
#86066 = DIRECTION('center_axis',(1.,-3.46944695195361E-16,0.)) ;
#86067 = DIRECTION('ref_axis',(3.46944695195361E-16,1.,0.)) ;
#86068 = DIRECTION('center_axis',(-1.,3.46944695195361E-16,0.)) ;
#86069 = DIRECTION('ref_axis',(3.46944695195361E-16,1.,0.)) ;
#86070 = DIRECTION('center_axis',(-3.46944695195361E-16,-1.,-6.49299968442375E-16)) ;
#86071 = DIRECTION('ref_axis',(2.25271179641597E-31,6.49299968442375E-16,
-1.)) ;
#86072 = DIRECTION('center_axis',(0.,-1.,0.)) ;
#86073 = DIRECTION('ref_axis',(0.,0.,-1.)) ;
#86074 = DIRECTION('center_axis',(0.,0.,1.)) ;
#86075 = DIRECTION('ref_axis',(1.,0.,0.)) ;
#86076 = DIRECTION('center_axis',(-3.25260651745651E-15,0.,1.)) ;
#86077 = DIRECTION('ref_axis',(1.,0.,3.25260651745651E-15)) ;
#86078 = DIRECTION('center_axis',(0.,1.,0.)) ;
#86079 = DIRECTION('ref_axis',(1.,0.,0.)) ;
#86080 = DIRECTION('center_axis',(0.,-0.888198741900269,-0.45945945945946)) ;
#86081 = DIRECTION('ref_axis',(0.,-0.45945945945946,0.888198741900269)) ;
#86082 = DIRECTION('center_axis',(1.,-3.46944695195361E-16,0.)) ;
#86083 = DIRECTION('ref_axis',(0.,1.,0.)) ;
#86084 = DIRECTION('center_axis',(0.,0.888198741900269,0.45945945945946)) ;
#86085 = DIRECTION('ref_axis',(0.,0.45945945945946,-0.888198741900269)) ;
#86086 = DIRECTION('center_axis',(1.,-3.46944695195361E-16,0.)) ;
#86087 = DIRECTION('ref_axis',(0.,1.,0.)) ;
#86088 = DIRECTION('center_axis',(0.,1.,0.)) ;
#86089 = DIRECTION('ref_axis',(0.,0.,-1.)) ;
#86090 = DIRECTION('center_axis',(0.,1.,0.)) ;
#86091 = DIRECTION('ref_axis',(1.,0.,0.)) ;
#86092 = DIRECTION('center_axis',(-1.,0.,0.)) ;
#86093 = DIRECTION('ref_axis',(0.,0.,-1.)) ;
#86094 = DIRECTION('center_axis',(1.,-3.46944695195361E-16,0.)) ;
#86095 = DIRECTION('ref_axis',(3.41607084500048E-16,1.,0.)) ;
#86096 = DIRECTION('center_axis',(-9.62987005567165E-16,-0.459459459459459,
-0.88819874190027)) ;
#86097 = DIRECTION('ref_axis',(-7.31984232283282E-30,0.88819874190027,-0.459459459459459)) ;
#86098 = DIRECTION('center_axis',(1.,-3.46944695195361E-16,0.)) ;
#86099 = DIRECTION('ref_axis',(3.46944695195361E-16,1.,0.)) ;
#86100 = DIRECTION('center_axis',(-1.,3.46944695195361E-16,0.)) ;
#86101 = DIRECTION('ref_axis',(3.46944695195361E-16,1.,0.)) ;
#86102 = DIRECTION('center_axis',(1.,0.,0.)) ;
#86103 = DIRECTION('ref_axis',(0.,0.,-1.)) ;
#86104 = DIRECTION('center_axis',(1.,-3.46944695195361E-16,0.)) ;
#86105 = DIRECTION('ref_axis',(3.80647894157197E-16,1.,0.)) ;
#86106 = DIRECTION('center_axis',(0.,0.459459459459459,0.888198741900269)) ;
#86107 = DIRECTION('ref_axis',(0.,-0.888198741900269,0.459459459459459)) ;
#86108 = DIRECTION('center_axis',(-3.46944695195361E-16,-1.,-6.49299968442375E-16)) ;
#86109 = DIRECTION('ref_axis',(2.25271179641597E-31,6.49299968442375E-16,
-1.)) ;
#86110 = DIRECTION('center_axis',(0.,1.,0.)) ;
#86111 = DIRECTION('ref_axis',(0.,0.,-1.)) ;
#86112 = DIRECTION('center_axis',(1.,0.,2.25271179641597E-31)) ;
#86113 = DIRECTION('ref_axis',(2.25271179641597E-31,0.,-1.)) ;
#86114 = DIRECTION('center_axis',(-1.,0.,0.)) ;
#86115 = DIRECTION('ref_axis',(0.,0.,1.)) ;
#86116 = DIRECTION('center_axis',(0.,1.,0.)) ;
#86117 = DIRECTION('ref_axis',(1.,0.,0.)) ;
#86118 = DIRECTION('center_axis',(0.,-1.,0.)) ;
#86119 = DIRECTION('ref_axis',(-1.08420217248551E-15,0.,1.)) ;
#86120 = DIRECTION('center_axis',(1.,-3.46944695195361E-16,0.)) ;
#86121 = DIRECTION('ref_axis',(0.,1.,0.)) ;
#86122 = DIRECTION('center_axis',(0.,1.,0.)) ;
#86123 = DIRECTION('ref_axis',(0.,0.,-1.)) ;
#86124 = DIRECTION('center_axis',(0.,-1.,0.)) ;
#86125 = DIRECTION('ref_axis',(0.,0.,-1.)) ;
#86126 = DIRECTION('center_axis',(0.,0.,1.)) ;
#86127 = DIRECTION('ref_axis',(-1.,0.,0.)) ;
#86128 = DIRECTION('center_axis',(0.,0.,-1.)) ;
#86129 = DIRECTION('ref_axis',(-1.,0.,0.)) ;
#86130 = DIRECTION('center_axis',(0.,0.,-1.)) ;
#86131 = DIRECTION('ref_axis',(-1.,0.,0.)) ;
#86132 = DIRECTION('center_axis',(-3.46944695195361E-16,-1.,-9.27571383489107E-17)) ;
#86133 = DIRECTION('ref_axis',(1.,-3.46944695195361E-16,-3.21815970916568E-32)) ;
#86134 = DIRECTION('center_axis',(0.,-1.,0.)) ;
#86135 = DIRECTION('ref_axis',(0.,0.,-1.)) ;
#86136 = DIRECTION('center_axis',(3.46944695195361E-16,1.,9.27571383489107E-17)) ;
#86137 = DIRECTION('ref_axis',(-1.,3.46944695195361E-16,3.21815970916568E-32)) ;
#86138 = DIRECTION('center_axis',(0.,1.,0.)) ;
#86139 = DIRECTION('ref_axis',(0.,0.,-1.)) ;
#86140 = DIRECTION('center_axis',(0.,0.,-1.)) ;
#86141 = DIRECTION('ref_axis',(-1.,0.,0.)) ;
#86142 = DIRECTION('center_axis',(0.,0.,1.)) ;
#86143 = DIRECTION('ref_axis',(1.,0.,0.)) ;
#86144 = DIRECTION('center_axis',(0.,1.,0.)) ;
#86145 = DIRECTION('ref_axis',(1.,0.,0.)) ;
#86146 = DIRECTION('center_axis',(-1.,0.,1.0842021724855E-15)) ;
#86147 = DIRECTION('ref_axis',(-1.0842021724855E-15,0.,-1.)) ;
#86148 = DIRECTION('center_axis',(0.,-1.,0.)) ;
#86149 = DIRECTION('ref_axis',(0.,0.,-1.)) ;
#86150 = DIRECTION('center_axis',(1.,0.,0.)) ;
#86151 = DIRECTION('ref_axis',(0.,0.,1.)) ;
#86152 = DIRECTION('center_axis',(1.,0.,3.21815970916568E-32)) ;
#86153 = DIRECTION('ref_axis',(3.21815970916568E-32,0.,-1.)) ;
#86154 = DIRECTION('center_axis',(0.,1.,0.)) ;
#86155 = DIRECTION('ref_axis',(1.,0.,0.)) ;
#86156 = DIRECTION('center_axis',(0.,0.,-1.)) ;
#86157 = DIRECTION('ref_axis',(1.,0.,0.)) ;
#86158 = DIRECTION('center_axis',(1.,0.,0.)) ;
#86159 = DIRECTION('ref_axis',(0.,-1.08420217248551E-15,1.)) ;
#86160 = DIRECTION('center_axis',(1.0842021724855E-15,1.,0.)) ;
#86161 = DIRECTION('ref_axis',(1.,-1.0842021724855E-15,0.)) ;
#86162 = DIRECTION('center_axis',(1.,0.,-2.08976773479518E-32)) ;
#86163 = DIRECTION('ref_axis',(-2.08976773479518E-32,0.,-1.)) ;
#86164 = DIRECTION('center_axis',(-0.447220452189282,-7.10036080930881E-6,
-0.894423762594219)) ;
#86165 = DIRECTION('ref_axis',(0.894325663270107,0.0148067719344852,-0.447171519130372)) ;
#86166 = DIRECTION('center_axis',(-1.23908819712629E-16,1.,2.4093381610789E-16)) ;
#86167 = DIRECTION('ref_axis',(2.98538247827883E-32,-2.4093381610789E-16,
1.)) ;
#86168 = DIRECTION('center_axis',(-5.60223364641742E-6,-0.447219005479868,
-0.894424485971965)) ;
#86169 = DIRECTION('ref_axis',(0.0146917039307497,0.894327914920294,-0.44717081124547)) ;
#86170 = DIRECTION('center_axis',(-8.95614743483648E-33,0.,1.)) ;
#86171 = DIRECTION('ref_axis',(1.,0.,8.95614743483648E-33)) ;
#86172 = DIRECTION('center_axis',(1.40488587213121E-32,-1.23908819712629E-16,
-1.)) ;
#86173 = DIRECTION('ref_axis',(1.74077750246726E-48,1.,-1.23908819712629E-16)) ;
#86174 = DIRECTION('center_axis',(-2.65552944032596E-32,0.,1.)) ;
#86175 = DIRECTION('ref_axis',(1.,0.,2.65552944032596E-32)) ;
#86176 = DIRECTION('center_axis',(0.894424485971418,-5.60223458619776E-6,
0.447219005480961)) ;
#86177 = DIRECTION('ref_axis',(0.447170811246815,0.0146917038942881,-0.89432791492022)) ;
#86178 = DIRECTION('center_axis',(0.894423762593897,-7.10036028474965E-6,
-0.447220452189924)) ;
#86179 = DIRECTION('ref_axis',(0.447171519131165,0.0148067719106287,0.894325663270105)) ;
#86180 = DIRECTION('center_axis',(-8.95614743483648E-33,-1.10974565782288E-48,
1.)) ;
#86181 = DIRECTION('ref_axis',(1.,-9.9390457266313E-81,8.95614743483648E-33)) ;
#86182 = DIRECTION('center_axis',(-7.10036046195813E-6,0.894423762593789,
0.44722045219014)) ;
#86183 = DIRECTION('ref_axis',(-0.0148067719149123,-0.447171519131355,0.894325663269939)) ;
#86184 = DIRECTION('center_axis',(-5.60223476175893E-6,0.894424485971284,
-0.447219005481229)) ;
#86185 = DIRECTION('ref_axis',(0.0146917038893733,0.447170811247117,0.89432791492015)) ;
#86186 = DIRECTION('center_axis',(1.40488587213121E-32,-1.23908819712629E-16,
-1.)) ;
#86187 = DIRECTION('ref_axis',(0.,1.,0.)) ;
#86188 = DIRECTION('center_axis',(-1.,0.,0.)) ;
#86189 = DIRECTION('ref_axis',(0.,0.,-1.)) ;
#86190 = DIRECTION('center_axis',(0.,-1.,0.)) ;
#86191 = DIRECTION('ref_axis',(0.,0.,1.)) ;
#86192 = DIRECTION('center_axis',(-1.,0.,-1.40488587213121E-32)) ;
#86193 = DIRECTION('ref_axis',(-1.40488587213121E-32,0.,1.)) ;
#86194 = DIRECTION('',(-1.,0.,-1.40488587213121E-32)) ;
#86195 = DIRECTION('center_axis',(-1.,0.,0.)) ;
#86196 = DIRECTION('ref_axis',(0.,0.,1.)) ;
#86197 = DIRECTION('center_axis',(0.,1.,0.)) ;
#86198 = DIRECTION('ref_axis',(1.,0.,0.)) ;
#86199 = DIRECTION('center_axis',(0.,1.,0.)) ;
#86200 = DIRECTION('ref_axis',(0.,0.,-1.)) ;
#86201 = DIRECTION('center_axis',(0.,0.,-1.)) ;
#86202 = DIRECTION('ref_axis',(1.,0.,0.)) ;
#86203 = DIRECTION('center_axis',(-1.,0.,-1.7912294869673E-32)) ;
#86204 = DIRECTION('ref_axis',(-1.7912294869673E-32,0.,1.)) ;
#86205 = DIRECTION('center_axis',(-0.44721900547972,-5.60223438155825E-6,
0.894424485972038)) ;
#86206 = DIRECTION('ref_axis',(0.894327914920351,0.0146917039315984,0.447170811245326)) ;
#86207 = DIRECTION('center_axis',(-1.,0.,0.)) ;
#86208 = DIRECTION('ref_axis',(0.,0.,1.)) ;
#86209 = DIRECTION('center_axis',(1.23908819712629E-16,-1.,7.2280144832367E-17)) ;
#86210 = DIRECTION('ref_axis',(1.,1.23908819712629E-16,-8.95614743483648E-33)) ;
#86211 = DIRECTION('center_axis',(-7.10035968146942E-6,-0.447220452189183,
0.894423762594268)) ;
#86212 = DIRECTION('ref_axis',(-0.0148067719292095,-0.894325663270233,-0.447171519130293)) ;
#86213 = DIRECTION('center_axis',(0.,-1.,1.0842021724855E-15)) ;
#86214 = DIRECTION('ref_axis',(0.,-1.0842021724855E-15,-1.)) ;
#86215 = DIRECTION('center_axis',(1.23908819712629E-16,-1.,1.23908819712629E-16)) ;
#86216 = DIRECTION('ref_axis',(-9.81657386420148E-47,-1.23908819712629E-16,
-1.)) ;
#86217 = DIRECTION('center_axis',(0.,-1.,0.)) ;
#86218 = DIRECTION('ref_axis',(0.,0.,-1.)) ;
#86219 = DIRECTION('',(-1.23908819712629E-16,1.,-1.23908819712629E-16)) ;
#86220 = DIRECTION('center_axis',(1.,0.,1.40488587213121E-32)) ;
#86221 = DIRECTION('ref_axis',(1.40488587213121E-32,0.,-1.)) ;
#86222 = DIRECTION('center_axis',(-0.707106781186547,0.707106781186548,-6.41152859744984E-16)) ;
#86223 = DIRECTION('ref_axis',(0.707106781186548,0.707106781186547,-1.43971204814373E-12)) ;
#86224 = DIRECTION('center_axis',(1.,0.,0.)) ;
#86225 = DIRECTION('ref_axis',(0.,0.,-1.)) ;
#86226 = DIRECTION('center_axis',(0.,-1.,0.)) ;
#86227 = DIRECTION('ref_axis',(0.,0.,-1.)) ;
#86228 = DIRECTION('center_axis',(0.,0.,1.)) ;
#86229 = DIRECTION('ref_axis',(-1.,0.,0.)) ;
#86230 = DIRECTION('center_axis',(7.2280144832367E-17,0.,-1.)) ;
#86231 = DIRECTION('ref_axis',(-1.,0.,-7.2280144832367E-17)) ;
#86232 = DIRECTION('',(7.2280144832367E-17,0.,-1.)) ;
#86233 = DIRECTION('center_axis',(0.,0.,-1.)) ;
#86234 = DIRECTION('ref_axis',(-1.,0.,0.)) ;
#86235 = DIRECTION('center_axis',(0.,1.,0.)) ;
#86236 = DIRECTION('ref_axis',(1.,0.,0.)) ;
#86237 = DIRECTION('center_axis',(0.,0.,1.)) ;
#86238 = DIRECTION('ref_axis',(-1.,0.,0.)) ;
#86239 = DIRECTION('center_axis',(0.,1.,0.)) ;
#86240 = DIRECTION('ref_axis',(1.,0.,0.)) ;
#86241 = DIRECTION('center_axis',(1.,0.,0.)) ;
#86242 = DIRECTION('ref_axis',(0.,0.,1.)) ;
#86243 = DIRECTION('center_axis',(0.,0.,-1.)) ;
#86244 = DIRECTION('ref_axis',(1.,0.,0.)) ;
#86245 = DIRECTION('center_axis',(-1.13380619344889E-16,1.,-1.23908819712629E-16)) ;
#86246 = DIRECTION('ref_axis',(-1.40488587213121E-32,1.23908819712629E-16,
1.)) ;
#86247 = DIRECTION('center_axis',(0.,1.,0.)) ;
#86248 = DIRECTION('ref_axis',(0.,0.,1.)) ;
#86249 = DIRECTION('center_axis',(7.2280144832367E-17,0.,-1.)) ;
#86250 = DIRECTION('ref_axis',(-1.,0.,-7.2280144832367E-17)) ;
#86251 = DIRECTION('center_axis',(0.,0.,1.)) ;
#86252 = DIRECTION('ref_axis',(1.,0.,0.)) ;
#86253 = DIRECTION('center_axis',(0.,1.,0.)) ;
#86254 = DIRECTION('ref_axis',(1.,0.,0.)) ;
#86255 = DIRECTION('center_axis',(0.,1.,0.)) ;
#86256 = DIRECTION('ref_axis',(0.,0.,-1.)) ;
#86257 = DIRECTION('center_axis',(1.,2.16840434497101E-15,-2.93873587705572E-31)) ;
#86258 = DIRECTION('ref_axis',(2.16840434497101E-15,-1.,-1.03035812136257E-62)) ;
#86259 = DIRECTION('center_axis',(-8.95614743483648E-33,0.,1.)) ;
#86260 = DIRECTION('ref_axis',(1.,0.,8.95614743483648E-33)) ;
#86261 = DIRECTION('center_axis',(-1.40488587213121E-32,1.23908819712629E-16,
1.)) ;
#86262 = DIRECTION('ref_axis',(-1.74077750246726E-48,-1.,1.23908819712629E-16)) ;
#86263 = DIRECTION('center_axis',(8.95614743483648E-33,1.0154535431059E-48,
-1.)) ;
#86264 = DIRECTION('ref_axis',(-1.,9.09455164528354E-81,-8.95614743483648E-33)) ;
#86265 = DIRECTION('center_axis',(2.16840434497101E-15,0.,-1.)) ;
#86266 = DIRECTION('ref_axis',(-1.,0.,-2.16840434497101E-15)) ;
#86267 = DIRECTION('',(-8.95614743483648E-33,-1.0154535431059E-48,1.)) ;
#86268 = DIRECTION('center_axis',(-1.,-1.13380619344889E-16,0.)) ;
#86269 = DIRECTION('ref_axis',(0.,-1.,0.)) ;
#86270 = DIRECTION('center_axis',(0.,0.,1.)) ;
#86271 = DIRECTION('ref_axis',(-1.,0.,0.)) ;
#86272 = DIRECTION('center_axis',(0.,-1.,0.)) ;
#86273 = DIRECTION('ref_axis',(0.,0.,-1.)) ;
#86274 = DIRECTION('center_axis',(-1.,0.,0.)) ;
#86275 = DIRECTION('ref_axis',(0.,0.,-1.)) ;
#86276 = DIRECTION('center_axis',(1.,0.,1.40488587213121E-32)) ;
#86277 = DIRECTION('ref_axis',(1.40488587213121E-32,0.,-1.)) ;
#86278 = DIRECTION('',(1.,0.,1.40488587213121E-32)) ;
#86279 = DIRECTION('center_axis',(1.,0.,0.)) ;
#86280 = DIRECTION('ref_axis',(0.,0.,-1.)) ;
#86281 = DIRECTION('center_axis',(-1.40488587213121E-32,1.23908819712629E-16,
1.)) ;
#86282 = DIRECTION('ref_axis',(0.,-1.,0.)) ;
#86283 = DIRECTION('center_axis',(0.,-1.,0.)) ;
#86284 = DIRECTION('ref_axis',(0.,0.,1.)) ;
#86285 = DIRECTION('center_axis',(0.,1.,0.)) ;
#86286 = DIRECTION('ref_axis',(1.,0.,0.)) ;
#86287 = DIRECTION('center_axis',(1.,0.,0.)) ;
#86288 = DIRECTION('ref_axis',(0.,0.,1.)) ;
#86289 = DIRECTION('center_axis',(0.,1.,0.)) ;
#86290 = DIRECTION('ref_axis',(0.,0.,-1.)) ;
#86291 = DIRECTION('center_axis',(0.,0.,1.)) ;
#86292 = DIRECTION('ref_axis',(1.,0.,0.)) ;
#86293 = DIRECTION('center_axis',(0.,0.,1.)) ;
#86294 = DIRECTION('ref_axis',(1.,0.,0.)) ;
#86295 = DIRECTION('center_axis',(1.,0.,1.40488587213121E-32)) ;
#86296 = DIRECTION('ref_axis',(1.40488587213121E-32,0.,-1.)) ;
#86297 = DIRECTION('center_axis',(-0.707106781186552,0.707106781186543,-7.95029546083828E-15)) ;
#86298 = DIRECTION('ref_axis',(0.707106781186543,0.707106781186552,-1.6468249326304E-12)) ;
#86299 = DIRECTION('center_axis',(-1.23908819712629E-16,1.,-1.23908819712629E-16)) ;
#86300 = DIRECTION('ref_axis',(9.81657386420148E-47,1.23908819712629E-16,
1.)) ;
#86301 = DIRECTION('',(1.23908819712629E-16,-1.,1.23908819712629E-16)) ;
#86302 = DIRECTION('center_axis',(-1.,-1.13380619344889E-16,0.)) ;
#86303 = DIRECTION('ref_axis',(0.,-1.,0.)) ;
#86304 = DIRECTION('center_axis',(0.,-1.,0.)) ;
#86305 = DIRECTION('ref_axis',(0.,0.,1.)) ;
#86306 = DIRECTION('center_axis',(1.13380619344889E-16,-1.,1.23908819712629E-16)) ;
#86307 = DIRECTION('ref_axis',(1.40488587213121E-32,-1.23908819712629E-16,
-1.)) ;
#86308 = DIRECTION('center_axis',(-1.5529910948782E-31,-4.47619207437002E-16,
1.)) ;
#86309 = DIRECTION('ref_axis',(6.951486430461E-47,-1.,-4.47619207437002E-16)) ;
#86310 = DIRECTION('center_axis',(0.,2.16840434497101E-15,-1.)) ;
#86311 = DIRECTION('ref_axis',(0.,1.,2.16840434497101E-15)) ;
#86312 = DIRECTION('center_axis',(0.,1.,0.)) ;
#86313 = DIRECTION('ref_axis',(1.,0.,0.)) ;
#86314 = DIRECTION('center_axis',(3.85194802226865E-15,0.888198741900269,
-0.45945945945946)) ;
#86315 = DIRECTION('ref_axis',(3.25260651745654E-15,-0.45945945945946,-0.888198741900269)) ;
#86316 = DIRECTION('center_axis',(-1.,0.,1.22067519501986E-15)) ;
#86317 = DIRECTION('ref_axis',(-1.22067519501986E-15,3.46944695195364E-14,
-1.)) ;
#86318 = DIRECTION('center_axis',(1.5529910948782E-31,4.47619207437002E-16,
-1.)) ;
#86319 = DIRECTION('ref_axis',(-6.951486430461E-47,1.,4.47619207437002E-16)) ;
#86320 = DIRECTION('center_axis',(0.,0.,1.)) ;
#86321 = DIRECTION('ref_axis',(1.,0.,0.)) ;
#86322 = DIRECTION('center_axis',(1.,-3.46944695195361E-16,0.)) ;
#86323 = DIRECTION('ref_axis',(3.46944695195361E-16,1.,0.)) ;
#86324 = DIRECTION('center_axis',(-1.,3.46944695195361E-16,0.)) ;
#86325 = DIRECTION('ref_axis',(3.46944695195361E-16,1.,3.46944695195362E-14)) ;
#86326 = DIRECTION('center_axis',(1.,-3.46944695195361E-16,0.)) ;
#86327 = DIRECTION('ref_axis',(3.41607084500048E-16,1.,0.)) ;
#86328 = DIRECTION('center_axis',(0.,0.459459459459457,-0.888198741900271)) ;
#86329 = DIRECTION('ref_axis',(0.,0.888198741900271,0.459459459459457)) ;
#86330 = DIRECTION('center_axis',(0.,0.,1.)) ;
#86331 = DIRECTION('ref_axis',(1.,0.,0.)) ;
#86332 = DIRECTION('center_axis',(0.,0.,-1.)) ;
#86333 = DIRECTION('ref_axis',(-1.,0.,0.)) ;
#86334 = DIRECTION('center_axis',(-1.,3.46944695195361E-16,0.)) ;
#86335 = DIRECTION('ref_axis',(-3.46944695195361E-16,-1.,0.)) ;
#86336 = DIRECTION('center_axis',(-1.,3.46944695195361E-16,0.)) ;
#86337 = DIRECTION('ref_axis',(-3.46944695195361E-16,-1.,0.)) ;
#86338 = DIRECTION('center_axis',(-1.,3.46944695195361E-16,0.)) ;
#86339 = DIRECTION('ref_axis',(3.46944695195361E-16,1.,6.93889390390722E-14)) ;
#86340 = DIRECTION('center_axis',(1.,-3.46944695195361E-16,0.)) ;
#86341 = DIRECTION('ref_axis',(0.,1.,0.)) ;
#86342 = DIRECTION('center_axis',(0.,-0.888198741900269,0.459459459459461)) ;
#86343 = DIRECTION('ref_axis',(0.,0.459459459459461,0.888198741900269)) ;
#86344 = DIRECTION('center_axis',(0.,1.,0.)) ;
#86345 = DIRECTION('ref_axis',(1.,0.,0.)) ;
#86346 = DIRECTION('center_axis',(0.,1.,0.)) ;
#86347 = DIRECTION('ref_axis',(0.,0.,-1.)) ;
#86348 = DIRECTION('center_axis',(-1.,0.,0.)) ;
#86349 = DIRECTION('ref_axis',(0.,-8.67361737988409E-15,-1.)) ;
#86350 = DIRECTION('center_axis',(1.,-3.46944695195361E-16,0.)) ;
#86351 = DIRECTION('ref_axis',(3.70074341541719E-16,1.,0.)) ;
#86352 = DIRECTION('center_axis',(0.,0.63294893130157,-0.774193548387094)) ;
#86353 = DIRECTION('ref_axis',(-1.08420217248549E-15,-0.774193548387094,-0.63294893130157)) ;
#86354 = DIRECTION('center_axis',(1.,-3.46944695195361E-16,0.)) ;
#86355 = DIRECTION('ref_axis',(3.80647894157197E-16,1.,0.)) ;
#86356 = DIRECTION('center_axis',(0.,-0.45945945945946,0.888198741900269)) ;
#86357 = DIRECTION('ref_axis',(0.,-0.888198741900269,-0.45945945945946)) ;
#86358 = DIRECTION('center_axis',(1.,-3.46944695195361E-16,0.)) ;
#86359 = DIRECTION('ref_axis',(3.46944695195361E-16,1.,0.)) ;
#86360 = DIRECTION('center_axis',(-1.,3.46944695195361E-16,0.)) ;
#86361 = DIRECTION('ref_axis',(3.46944695195361E-16,1.,0.)) ;
#86362 = DIRECTION('center_axis',(-3.46944695195361E-16,-1.,-2.45739631480277E-16)) ;
#86363 = DIRECTION('ref_axis',(1.,-3.46944695195361E-16,-8.52580615413453E-32)) ;
#86364 = DIRECTION('center_axis',(0.,1.,0.)) ;
#86365 = DIRECTION('ref_axis',(0.,0.,1.)) ;
#86366 = DIRECTION('center_axis',(1.,-3.46944695195361E-16,0.)) ;
#86367 = DIRECTION('ref_axis',(3.33066907387547E-16,1.,0.)) ;
#86368 = DIRECTION('center_axis',(8.02036034720251E-16,0.293103448275862,
-0.956080733311157)) ;
#86369 = DIRECTION('ref_axis',(1.13164713162994E-29,0.956080733311157,0.293103448275862)) ;
#86370 = DIRECTION('center_axis',(-1.,3.46944695195361E-16,0.)) ;
#86371 = DIRECTION('ref_axis',(-3.46944695195361E-16,-1.,0.)) ;
#86372 = DIRECTION('center_axis',(-1.,3.46944695195361E-16,0.)) ;
#86373 = DIRECTION('ref_axis',(-3.46944695195361E-16,-1.,0.)) ;
#86374 = DIRECTION('center_axis',(-1.,3.46944695195361E-16,0.)) ;
#86375 = DIRECTION('ref_axis',(-3.46944695195361E-16,-1.,0.)) ;
#86376 = DIRECTION('center_axis',(0.,0.,-1.)) ;
#86377 = DIRECTION('ref_axis',(-1.,0.,0.)) ;
#86378 = DIRECTION('center_axis',(0.,0.,1.)) ;
#86379 = DIRECTION('ref_axis',(1.,0.,0.)) ;
#86380 = DIRECTION('center_axis',(-1.5529910948782E-31,-4.47619207437002E-16,
-1.)) ;
#86381 = DIRECTION('ref_axis',(-6.95148643046101E-47,1.,-4.47619207437002E-16)) ;
#86382 = DIRECTION('center_axis',(2.16840434497101E-15,0.,1.)) ;
#86383 = DIRECTION('ref_axis',(1.,0.,-2.16840434497101E-15)) ;
#86384 = DIRECTION('center_axis',(1.,-3.46944695195361E-16,0.)) ;
#86385 = DIRECTION('ref_axis',(0.,1.,0.)) ;
#86386 = DIRECTION('center_axis',(0.,-1.,0.)) ;
#86387 = DIRECTION('ref_axis',(0.,0.,1.)) ;
#86388 = DIRECTION('center_axis',(0.577350269189627,0.577350269189627,0.577350269189623)) ;
#86389 = DIRECTION('ref_axis',(-0.707106781186548,2.22044604925032E-15,0.707106781186547)) ;
#86390 = DIRECTION('center_axis',(-1.,3.46944695195361E-16,0.)) ;
#86391 = DIRECTION('ref_axis',(-3.70074341541719E-16,-1.,0.)) ;
#86392 = DIRECTION('center_axis',(0.,0.63294893130157,0.774193548387094)) ;
#86393 = DIRECTION('ref_axis',(0.,0.774193548387094,-0.63294893130157)) ;
#86394 = DIRECTION('center_axis',(0.,1.,0.)) ;
#86395 = DIRECTION('ref_axis',(1.,0.,0.)) ;
#86396 = DIRECTION('center_axis',(-1.,0.,0.)) ;
#86397 = DIRECTION('ref_axis',(0.,3.46944695195364E-14,-1.)) ;
#86398 = DIRECTION('center_axis',(0.,0.888198741900271,0.459459459459457)) ;
#86399 = DIRECTION('ref_axis',(-1.08420217248551E-15,0.459459459459457,-0.888198741900271)) ;
#86400 = DIRECTION('center_axis',(3.46944695195361E-16,1.,2.45739631480277E-16)) ;
#86401 = DIRECTION('ref_axis',(-1.,3.46944695195361E-16,8.52580615413453E-32)) ;
#86402 = DIRECTION('center_axis',(-1.,3.46944695195361E-16,0.)) ;
#86403 = DIRECTION('ref_axis',(-3.33066907387547E-16,-1.,0.)) ;
#86404 = DIRECTION('center_axis',(0.,0.293103448275864,0.956080733311156)) ;
#86405 = DIRECTION('ref_axis',(0.,-0.956080733311156,0.293103448275864)) ;
#86406 = DIRECTION('center_axis',(-3.46944695195361E-16,-1.,-1.06487173641454E-15)) ;
#86407 = DIRECTION('ref_axis',(3.69451600012496E-31,1.06487173641454E-15,
-1.)) ;
#86408 = DIRECTION('center_axis',(0.,-1.,0.)) ;
#86409 = DIRECTION('ref_axis',(0.,0.,-1.)) ;
#86410 = DIRECTION('center_axis',(0.,1.,0.)) ;
#86411 = DIRECTION('ref_axis',(0.,0.,1.)) ;
#86412 = DIRECTION('center_axis',(-1.,3.46944695195361E-16,0.)) ;
#86413 = DIRECTION('ref_axis',(-3.41607084500048E-16,-1.,0.)) ;
#86414 = DIRECTION('center_axis',(-4.88154879316133E-15,0.45945945945946,
0.888198741900269)) ;
#86415 = DIRECTION('ref_axis',(-3.39148554690438E-29,-0.888198741900269,0.45945945945946)) ;
#86416 = DIRECTION('center_axis',(1.,-3.46944695195361E-16,0.)) ;
#86417 = DIRECTION('ref_axis',(3.46944695195361E-16,1.,0.)) ;
#86418 = DIRECTION('center_axis',(-1.,3.46944695195361E-16,0.)) ;
#86419 = DIRECTION('ref_axis',(3.46944695195361E-16,1.,0.)) ;
#86420 = DIRECTION('center_axis',(-1.5529910948782E-31,-4.47619207437002E-16,
-1.)) ;
#86421 = DIRECTION('ref_axis',(-6.95148643046101E-47,1.,-4.47619207437002E-16)) ;
#86422 = DIRECTION('center_axis',(0.,0.,-1.)) ;
#86423 = DIRECTION('ref_axis',(-1.,0.,0.)) ;
#86424 = DIRECTION('center_axis',(0.,0.224137931034483,-0.974557431797419)) ;
#86425 = DIRECTION('ref_axis',(0.,-0.974557431797419,-0.224137931034483)) ;
#86426 = DIRECTION('center_axis',(0.577350269189627,0.577350269189627,0.577350269189623)) ;
#86427 = DIRECTION('ref_axis',(-0.707106781186548,2.22044604925032E-15,0.707106781186547)) ;
#86428 = DIRECTION('center_axis',(0.408248290463864,-0.816496580927725,0.408248290463864)) ;
#86429 = DIRECTION('ref_axis',(0.707106781186545,-2.77555756156289E-15,-0.70710678118655)) ;
#86430 = DIRECTION('center_axis',(0.,1.,0.)) ;
#86431 = DIRECTION('ref_axis',(1.,0.,0.)) ;
#86432 = DIRECTION('center_axis',(-1.,0.,0.)) ;
#86433 = DIRECTION('ref_axis',(0.,0.,-1.)) ;
#86434 = DIRECTION('center_axis',(1.,-3.46944695195361E-16,0.)) ;
#86435 = DIRECTION('ref_axis',(0.,1.,0.)) ;
#86436 = DIRECTION('center_axis',(9.96293888229924E-16,-0.888198741900269,
-0.45945945945946)) ;
#86437 = DIRECTION('ref_axis',(-3.00809911926502E-30,-0.45945945945946,0.888198741900269)) ;
#86438 = DIRECTION('center_axis',(1.,-3.46944695195361E-16,0.)) ;
#86439 = DIRECTION('ref_axis',(-3.70074341541719E-16,-1.,-1.1842378929335E-15)) ;
#86440 = DIRECTION('center_axis',(1.58436874053304E-16,-0.224137931034483,
-0.974557431797419)) ;
#86441 = DIRECTION('ref_axis',(-2.46331010218511E-30,0.974557431797419,-0.224137931034483)) ;
#86442 = DIRECTION('center_axis',(1.,-3.46944695195361E-16,0.)) ;
#86443 = DIRECTION('ref_axis',(3.46944695195361E-16,1.,0.)) ;
#86444 = DIRECTION('center_axis',(-1.,3.46944695195361E-16,0.)) ;
#86445 = DIRECTION('ref_axis',(3.46944695195361E-16,1.,0.)) ;
#86446 = DIRECTION('center_axis',(1.,-3.46944695195361E-16,0.)) ;
#86447 = DIRECTION('ref_axis',(3.80647894157197E-16,1.,0.)) ;
#86448 = DIRECTION('center_axis',(0.,-0.45945945945946,-0.888198741900269)) ;
#86449 = DIRECTION('ref_axis',(0.,0.888198741900269,-0.45945945945946)) ;
#86450 = DIRECTION('center_axis',(1.,-3.46944695195361E-16,0.)) ;
#86451 = DIRECTION('ref_axis',(0.,1.,0.)) ;
#86452 = DIRECTION('center_axis',(0.,-1.,0.)) ;
#86453 = DIRECTION('ref_axis',(0.,0.,1.)) ;
#86454 = DIRECTION('center_axis',(-3.46944695195361E-16,-1.,-1.06487173641454E-15)) ;
#86455 = DIRECTION('ref_axis',(3.69451600012496E-31,1.06487173641454E-15,
-1.)) ;
#86456 = DIRECTION('center_axis',(0.,0.,1.)) ;
#86457 = DIRECTION('ref_axis',(1.,0.,0.)) ;
#86458 = DIRECTION('center_axis',(0.,-1.,0.)) ;
#86459 = DIRECTION('ref_axis',(0.,0.,-1.)) ;
#86460 = DIRECTION('center_axis',(0.,-1.,0.)) ;
#86461 = DIRECTION('ref_axis',(0.,0.,-1.)) ;
#86462 = DIRECTION('center_axis',(0.,1.,0.)) ;
#86463 = DIRECTION('ref_axis',(0.,0.,-1.)) ;
#86464 = DIRECTION('center_axis',(0.,0.,1.)) ;
#86465 = DIRECTION('ref_axis',(1.,0.,0.)) ;
#86466 = DIRECTION('center_axis',(8.67361737988404E-15,-1.,0.)) ;
#86467 = DIRECTION('ref_axis',(1.,8.67361737988404E-15,0.)) ;
#86468 = DIRECTION('center_axis',(0.497468338163091,-0.710669054518702,0.497468338163091)) ;
#86469 = DIRECTION('ref_axis',(0.81923192051904,0.573462344363328,8.04804396179112E-16)) ;
#86470 = DIRECTION('center_axis',(0.497468338163091,-0.710669054518702,0.497468338163091)) ;
#86471 = DIRECTION('ref_axis',(0.81923192051904,0.573462344363328,7.6535433881835E-16)) ;
#86472 = DIRECTION('center_axis',(0.497468338163092,-0.7106690545187,0.497468338163092)) ;
#86473 = DIRECTION('ref_axis',(-1.24903860074368E-15,-0.57346234436333,-0.819231920519039)) ;
#86474 = DIRECTION('center_axis',(0.,0.,1.)) ;
#86475 = DIRECTION('ref_axis',(1.,0.,0.)) ;
#86476 = DIRECTION('center_axis',(0.,-1.,0.)) ;
#86477 = DIRECTION('ref_axis',(0.,0.,-1.)) ;
#86478 = DIRECTION('center_axis',(0.,1.,0.)) ;
#86479 = DIRECTION('ref_axis',(0.,0.,1.)) ;
#86480 = DIRECTION('center_axis',(0.,1.,0.)) ;
#86481 = DIRECTION('ref_axis',(0.,0.,1.)) ;
#86482 = DIRECTION('center_axis',(0.,1.,0.)) ;
#86483 = DIRECTION('ref_axis',(1.,0.,0.)) ;
#86484 = DIRECTION('center_axis',(-1.98515611757154E-15,0.,1.)) ;
#86485 = DIRECTION('ref_axis',(-1.,0.,-1.98515611757154E-15)) ;
#86486 = DIRECTION('center_axis',(1.,-4.06575814682065E-16,2.84603070277446E-16)) ;
#86487 = DIRECTION('ref_axis',(-4.06575814682065E-16,-1.,6.48893816316174E-47)) ;
#86488 = DIRECTION('center_axis',(0.,1.,0.)) ;
#86489 = DIRECTION('ref_axis',(0.,0.,1.)) ;
#86490 = DIRECTION('center_axis',(0.,1.,0.)) ;
#86491 = DIRECTION('ref_axis',(0.,0.,1.)) ;
#86492 = DIRECTION('center_axis',(0.497468338163091,0.710669054518702,-0.497468338163091)) ;
#86493 = DIRECTION('ref_axis',(-0.81923192051904,0.573462344363328,7.6535433881835E-16)) ;
#86494 = DIRECTION('center_axis',(-0.497468338163091,-0.710669054518702,0.497468338163091)) ;
#86495 = DIRECTION('ref_axis',(-0.81923192051904,0.573462344363329,2.81956803083991E-15)) ;
#86496 = DIRECTION('center_axis',(-0.497468338163093,-0.7106690545187,0.497468338163091)) ;
#86497 = DIRECTION('ref_axis',(0.819231920519039,-0.573462344363331,1.48853464230757E-16)) ;
#86498 = DIRECTION('center_axis',(1.,0.,0.)) ;
#86499 = DIRECTION('ref_axis',(0.,0.,-1.)) ;
#86500 = DIRECTION('center_axis',(1.,0.,-9.9257805878577E-16)) ;
#86501 = DIRECTION('ref_axis',(-9.9257805878577E-16,0.,-1.)) ;
#86502 = DIRECTION('center_axis',(0.,0.,-1.)) ;
#86503 = DIRECTION('ref_axis',(-1.,0.,0.)) ;
#86504 = DIRECTION('center_axis',(-1.23327997120227E-15,1.76182853028895E-15,
1.)) ;
#86505 = DIRECTION('ref_axis',(-2.17282783909808E-30,-1.,1.76182853028895E-15)) ;
#86506 = DIRECTION('center_axis',(-0.497468338163091,0.710669054518702,0.497468338163091)) ;
#86507 = DIRECTION('ref_axis',(-0.81923192051904,-0.573462344363328,7.6535433881835E-16)) ;
#86508 = DIRECTION('center_axis',(0.497468338163091,-0.710669054518702,-0.497468338163091)) ;
#86509 = DIRECTION('ref_axis',(-0.81923192051904,-0.57346234436333,3.28127423742392E-15)) ;
#86510 = DIRECTION('center_axis',(0.497468338163093,-0.7106690545187,-0.497468338163091)) ;
#86511 = DIRECTION('ref_axis',(0.819231920519039,0.573462344363331,2.16059097207149E-16)) ;
#86512 = DIRECTION('center_axis',(0.,1.,0.)) ;
#86513 = DIRECTION('ref_axis',(1.,0.,0.)) ;
#86514 = DIRECTION('center_axis',(-1.13841228110978E-15,-1.62630325872826E-15,
1.)) ;
#86515 = DIRECTION('ref_axis',(3.52365706057789E-15,1.,1.62630325872826E-15)) ;
#86516 = DIRECTION('center_axis',(0.,1.,0.)) ;
#86517 = DIRECTION('ref_axis',(1.,0.,0.)) ;
#86518 = DIRECTION('center_axis',(1.,0.,-1.65429676464295E-16)) ;
#86519 = DIRECTION('ref_axis',(1.65429676464295E-16,2.60208521396523E-14,
1.)) ;
#86520 = DIRECTION('center_axis',(0.,0.,-1.)) ;
#86521 = DIRECTION('ref_axis',(-1.,0.,0.)) ;
#86522 = DIRECTION('center_axis',(3.3085935292859E-16,0.,1.)) ;
#86523 = DIRECTION('ref_axis',(1.,0.,-3.3085935292859E-16)) ;
#86524 = DIRECTION('center_axis',(1.,0.,0.)) ;
#86525 = DIRECTION('ref_axis',(0.,0.,-1.)) ;
#86526 = DIRECTION('center_axis',(1.,1.21972744404619E-15,8.53809210832338E-16)) ;
#86527 = DIRECTION('ref_axis',(-1.21972744404619E-15,1.,-2.84382165153726E-47)) ;
#86528 = DIRECTION('center_axis',(0.,1.,0.)) ;
#86529 = DIRECTION('ref_axis',(1.,0.,0.)) ;
#86530 = DIRECTION('center_axis',(0.497468338163092,0.710669054518701,0.497468338163092)) ;
#86531 = DIRECTION('ref_axis',(1.16990632765504E-14,0.573462344363324,-0.819231920519044)) ;
#86532 = DIRECTION('center_axis',(-0.497468338163091,-0.710669054518702,-0.497468338163091)) ;
#86533 = DIRECTION('ref_axis',(0.81923192051904,-0.573462344363328,7.6535433881835E-16)) ;
#86534 = DIRECTION('center_axis',(-0.497468338163091,-0.710669054518702,-0.497468338163091)) ;
#86535 = DIRECTION('ref_axis',(0.81923192051904,-0.573462344363328,7.6535433881835E-16)) ;
#86536 = DIRECTION('center_axis',(0.,-1.,0.)) ;
#86537 = DIRECTION('ref_axis',(0.,0.,-1.)) ;
#86538 = DIRECTION('center_axis',(0.,1.,0.)) ;
#86539 = DIRECTION('ref_axis',(0.,0.,-1.)) ;
#86540 = DIRECTION('center_axis',(-8.67361737988403E-15,1.,0.)) ;
#86541 = DIRECTION('ref_axis',(-1.,-8.67361737988403E-15,0.)) ;
#86542 = DIRECTION('center_axis',(0.,0.,1.)) ;
#86543 = DIRECTION('ref_axis',(1.,0.,0.)) ;
#86544 = DIRECTION('center_axis',(1.,6.67201336914158E-17,0.)) ;
#86545 = DIRECTION('ref_axis',(-6.67201336914158E-17,1.,0.)) ;
#86546 = DIRECTION('center_axis',(-1.,-6.67201336914158E-17,0.)) ;
#86547 = DIRECTION('ref_axis',(-6.67201336914158E-17,1.,0.)) ;
#86548 = DIRECTION('center_axis',(-1.,1.33440267382831E-16,0.)) ;
#86549 = DIRECTION('ref_axis',(-1.33440267382831E-16,-1.,0.)) ;
#86550 = DIRECTION('center_axis',(-1.,1.33440267382831E-16,0.)) ;
#86551 = DIRECTION('ref_axis',(-1.33440267382831E-16,-1.,0.)) ;
#86552 = DIRECTION('center_axis',(0.710669054518702,0.497468338163091,0.497468338163091)) ;
#86553 = DIRECTION('ref_axis',(-0.573462344363328,0.819231920519041,3.92980824865032E-16)) ;
#86554 = DIRECTION('center_axis',(0.710669054518702,0.497468338163091,0.497468338163091)) ;
#86555 = DIRECTION('ref_axis',(-0.573462344363328,0.819231920519041,3.92980824865032E-16)) ;
#86556 = DIRECTION('center_axis',(0.710669054518701,0.497468338163091,0.497468338163092)) ;
#86557 = DIRECTION('ref_axis',(0.57346234436333,-1.81382726107456E-15,-0.819231920519039)) ;
#86558 = DIRECTION('center_axis',(-0.710669054518702,0.497468338163091,-0.497468338163091)) ;
#86559 = DIRECTION('ref_axis',(-0.573462344363328,-0.819231920519041,6.69271761853466E-16)) ;
#86560 = DIRECTION('center_axis',(0.710669054518702,-0.497468338163091,0.497468338163091)) ;
#86561 = DIRECTION('ref_axis',(-0.573462344363328,-0.819231920519041,6.69271761853466E-16)) ;
#86562 = DIRECTION('center_axis',(0.7106690545187,-0.497468338163094,0.497468338163091)) ;
#86563 = DIRECTION('ref_axis',(0.573462344363331,0.819231920519038,2.86772422505918E-16)) ;
#86564 = DIRECTION('center_axis',(0.,1.,-9.34081871679819E-17)) ;
#86565 = DIRECTION('ref_axis',(0.,9.34081871679819E-17,1.)) ;
#86566 = DIRECTION('center_axis',(-4.33680868994205E-15,-1.,-3.03576608295944E-15)) ;
#86567 = DIRECTION('ref_axis',(1.,-4.33680868994205E-15,-1.12103877145985E-44)) ;
#86568 = DIRECTION('center_axis',(0.,1.,5.29374964685745E-15)) ;
#86569 = DIRECTION('ref_axis',(0.,-5.29374964685745E-15,1.)) ;
#86570 = DIRECTION('center_axis',(0.,1.,0.)) ;
#86571 = DIRECTION('ref_axis',(1.,0.,0.)) ;
#86572 = DIRECTION('center_axis',(0.,6.45175738210751E-15,1.)) ;
#86573 = DIRECTION('ref_axis',(0.,1.,-6.45175738210751E-15)) ;
#86574 = DIRECTION('center_axis',(-1.,-6.67201336914158E-17,0.)) ;
#86575 = DIRECTION('ref_axis',(6.67201336914158E-17,-1.,0.)) ;
#86576 = DIRECTION('center_axis',(-1.,-6.67201336914158E-17,0.)) ;
#86577 = DIRECTION('ref_axis',(6.67201336914158E-17,-1.,0.)) ;
#86578 = DIRECTION('center_axis',(1.,-1.33440267382831E-16,0.)) ;
#86579 = DIRECTION('ref_axis',(1.33440267382831E-16,1.,0.)) ;
#86580 = DIRECTION('center_axis',(-1.,1.33440267382831E-16,0.)) ;
#86581 = DIRECTION('ref_axis',(1.33440267382831E-16,1.,0.)) ;
#86582 = DIRECTION('center_axis',(0.,1.,0.)) ;
#86583 = DIRECTION('ref_axis',(1.,0.,0.)) ;
#86584 = DIRECTION('center_axis',(1.76182853028896E-15,-1.23327997120227E-15,
1.)) ;
#86585 = DIRECTION('ref_axis',(-1.,-2.1728278390981E-30,1.76182853028896E-15)) ;
#86586 = DIRECTION('center_axis',(0.,0.,-1.)) ;
#86587 = DIRECTION('ref_axis',(-1.,0.,0.)) ;
#86588 = DIRECTION('center_axis',(-2.71050543121378E-16,-1.89735380184965E-16,
1.)) ;
#86589 = DIRECTION('ref_axis',(1.,-5.14278778484758E-32,2.71050543121378E-16)) ;
#86590 = DIRECTION('center_axis',(-0.710669054518702,-0.497468338163091,0.497468338163091)) ;
#86591 = DIRECTION('ref_axis',(0.573462344363328,-0.819231920519041,3.92980824865032E-16)) ;
#86592 = DIRECTION('center_axis',(0.710669054518702,0.497468338163091,-0.497468338163091)) ;
#86593 = DIRECTION('ref_axis',(0.573462344363345,-0.819231920519029,3.5916041727749E-14)) ;
#86594 = DIRECTION('center_axis',(0.710669054518701,0.497468338163091,-0.497468338163092)) ;
#86595 = DIRECTION('ref_axis',(-0.57346234436333,1.88103289405095E-15,-0.819231920519039)) ;
#86596 = DIRECTION('center_axis',(0.710669054518702,-0.497468338163091,-0.497468338163091)) ;
#86597 = DIRECTION('ref_axis',(0.573462344363328,0.819231920519041,6.69271761853466E-16)) ;
#86598 = DIRECTION('center_axis',(0.710669054518702,-0.497468338163091,-0.497468338163091)) ;
#86599 = DIRECTION('ref_axis',(0.573462344363328,0.819231920519041,6.69271761853466E-16)) ;
#86600 = DIRECTION('center_axis',(0.7106690545187,-0.497468338163091,-0.497468338163093)) ;
#86601 = DIRECTION('ref_axis',(-0.573462344363331,-1.17187023180681E-15,-0.819231920519038)) ;
#86602 = DIRECTION('center_axis',(0.,0.,-1.)) ;
#86603 = DIRECTION('ref_axis',(-1.,0.,0.)) ;
#86604 = DIRECTION('center_axis',(0.,1.15800773525007E-15,1.)) ;
#86605 = DIRECTION('ref_axis',(0.,-1.,1.15800773525007E-15)) ;
#86606 = DIRECTION('center_axis',(0.,1.,0.)) ;
#86607 = DIRECTION('ref_axis',(1.,0.,0.)) ;
#86608 = DIRECTION('center_axis',(0.,1.,0.)) ;
#86609 = DIRECTION('ref_axis',(1.04083408558609E-13,0.,-1.)) ;
#86610 = DIRECTION('center_axis',(0.,1.,0.)) ;
#86611 = DIRECTION('ref_axis',(1.,0.,0.)) ;
#86612 = DIRECTION('center_axis',(4.33680868994204E-15,-1.,-3.03576608295944E-15)) ;
#86613 = DIRECTION('ref_axis',(-1.,-4.33680868994225E-15,6.93889390390727E-14)) ;
#86614 = DIRECTION('center_axis',(0.,1.,9.34081871679819E-17)) ;
#86615 = DIRECTION('ref_axis',(0.,-9.34081871679819E-17,1.)) ;
#86616 = DIRECTION('center_axis',(0.,0.,1.)) ;
#86617 = DIRECTION('ref_axis',(1.,0.,0.)) ;
#86618 = DIRECTION('center_axis',(-2.16840434497102E-15,-3.61400724161847E-16,
1.)) ;
#86619 = DIRECTION('ref_axis',(1.,-7.83662900548222E-31,2.16840434497102E-15)) ;
#86620 = DIRECTION('center_axis',(0.973328526784575,0.162221421130762,-0.162221421130763)) ;
#86621 = DIRECTION('ref_axis',(-0.164398987305358,9.23743777622416E-16,-0.986393923832144)) ;
#86622 = DIRECTION('center_axis',(0.973328526784574,0.162221421130765,-0.162221421130767)) ;
#86623 = DIRECTION('ref_axis',(-0.164398987305362,1.88956506020588E-16,-0.986393923832143)) ;
#86624 = DIRECTION('center_axis',(0.,1.,0.)) ;
#86625 = DIRECTION('ref_axis',(1.,0.,0.)) ;
#86626 = DIRECTION('center_axis',(0.,1.,-8.79325913341701E-15)) ;
#86627 = DIRECTION('ref_axis',(1.73472347597682E-14,-8.79325913341701E-15,
-1.)) ;
#86628 = DIRECTION('center_axis',(0.,0.,1.)) ;
#86629 = DIRECTION('ref_axis',(1.,0.,0.)) ;
#86630 = DIRECTION('center_axis',(0.,-2.28569887277128E-15,1.)) ;
#86631 = DIRECTION('ref_axis',(0.,-1.,-2.28569887277128E-15)) ;
#86632 = DIRECTION('center_axis',(1.73472347597681E-15,-1.,-2.89120579329468E-16)) ;
#86633 = DIRECTION('ref_axis',(1.,1.73472347597681E-15,5.01544256350843E-31)) ;
#86634 = DIRECTION('center_axis',(8.67361737988409E-15,1.,-1.44560289664739E-15)) ;
#86635 = DIRECTION('ref_axis',(-1.,8.67361737988409E-15,-1.40129846432482E-45)) ;
#86636 = DIRECTION('center_axis',(0.,1.,0.)) ;
#86637 = DIRECTION('ref_axis',(1.,0.,0.)) ;
#86638 = DIRECTION('center_axis',(-0.937042571331634,0.312347523777217,0.156173761888611)) ;
#86639 = DIRECTION('ref_axis',(0.316227766016843,0.948683298050512,6.71158276827649E-18)) ;
#86640 = DIRECTION('center_axis',(0.937042571331636,-0.312347523777212,-0.156173761888606)) ;
#86641 = DIRECTION('ref_axis',(0.316227766016838,0.948683298050514,8.61595672567599E-16)) ;
#86642 = DIRECTION('center_axis',(-0.973328526784575,-0.162221421130762,-0.162221421130763)) ;
#86643 = DIRECTION('ref_axis',(-0.164398987305358,9.23743777622416E-16,0.986393923832144)) ;
#86644 = DIRECTION('center_axis',(0.978231976292088,-0.146734796047319,-0.146734795425719)) ;
#86645 = DIRECTION('ref_axis',(0.182318633536231,0.945435290940488,0.270022270395899)) ;
#86646 = DIRECTION('center_axis',(0.973328526784574,0.162221421130767,0.162221421130768)) ;
#86647 = DIRECTION('ref_axis',(0.164398987305363,-6.69215935033609E-18,-0.986393923832143)) ;
#86648 = DIRECTION('center_axis',(0.,0.,1.)) ;
#86649 = DIRECTION('ref_axis',(1.,0.,0.)) ;
#86650 = DIRECTION('center_axis',(0.,2.19831478335425E-15,-1.)) ;
#86651 = DIRECTION('ref_axis',(0.,1.,2.19831478335425E-15)) ;
#86652 = DIRECTION('center_axis',(0.,1.,0.)) ;
#86653 = DIRECTION('ref_axis',(1.,0.,0.)) ;
#86654 = DIRECTION('center_axis',(8.67361737988408E-15,1.,1.44560289664739E-15)) ;
#86655 = DIRECTION('ref_axis',(1.,-8.67361737988408E-15,5.60519385729927E-45)) ;
#86656 = DIRECTION('center_axis',(1.73472347597681E-15,-1.,2.89120579329468E-16)) ;
#86657 = DIRECTION('ref_axis',(1.,1.73472347597681E-15,-5.01544256350843E-31)) ;
#86658 = DIRECTION('center_axis',(0.,1.,0.)) ;
#86659 = DIRECTION('ref_axis',(0.,0.,1.)) ;
#86660 = DIRECTION('center_axis',(0.,0.,1.)) ;
#86661 = DIRECTION('ref_axis',(1.,0.,0.)) ;
#86662 = DIRECTION('center_axis',(3.25260651745652E-15,-1.08420217248553E-15,
-1.)) ;
#86663 = DIRECTION('ref_axis',(-1.,-3.52648305246695E-30,-3.25260651745652E-15)) ;
#86664 = DIRECTION('center_axis',(0.,1.,0.)) ;
#86665 = DIRECTION('ref_axis',(1.,0.,0.)) ;
#86666 = DIRECTION('center_axis',(-0.937042571331635,0.312347523777215,-0.15617376188861)) ;
#86667 = DIRECTION('ref_axis',(0.316227766016841,0.948683298050513,6.5590042956861E-18)) ;
#86668 = DIRECTION('center_axis',(-0.937042571331636,0.312347523777212,-0.156173761888606)) ;
#86669 = DIRECTION('ref_axis',(0.331350514299552,0.654034959159455,-0.680033167478405)) ;
#86670 = DIRECTION('center_axis',(0.96151972409117,0.245047216428555,-0.124224320904791)) ;
#86671 = DIRECTION('ref_axis',(0.262092069886556,-0.68255472816298,0.68222195066191)) ;
#86672 = DIRECTION('center_axis',(2.65552944032596E-32,3.29043518662928E-48,
-1.)) ;
#86673 = DIRECTION('ref_axis',(-1.,8.7378475095785E-80,-2.65552944032596E-32)) ;
#86674 = DIRECTION('center_axis',(2.65552944032596E-32,3.29043518662928E-48,
-1.)) ;
#86675 = DIRECTION('ref_axis',(-1.,8.7378475095785E-80,-2.65552944032596E-32)) ;
#86676 = DIRECTION('center_axis',(-2.65552944032596E-32,-3.29043518662928E-48,
1.)) ;
#86677 = DIRECTION('ref_axis',(-1.,8.7378475095785E-80,-2.65552944032596E-32)) ;
#86678 = DIRECTION('center_axis',(0.,0.,1.)) ;
#86679 = DIRECTION('ref_axis',(1.,0.,0.)) ;
#86680 = DIRECTION('center_axis',(0.,0.,-1.)) ;
#86681 = DIRECTION('ref_axis',(-1.,0.,0.)) ;
#86682 = DIRECTION('center_axis',(0.,0.,1.)) ;
#86683 = DIRECTION('ref_axis',(1.,0.,0.)) ;
#86684 = DIRECTION('center_axis',(0.,0.,1.)) ;
#86685 = DIRECTION('ref_axis',(1.,0.,0.)) ;
#86686 = DIRECTION('center_axis',(0.,0.,-1.)) ;
#86687 = DIRECTION('ref_axis',(-1.,0.,0.)) ;
#86688 = DIRECTION('center_axis',(0.,0.,-1.)) ;
#86689 = DIRECTION('ref_axis',(-1.,0.,0.)) ;
#86690 = DIRECTION('center_axis',(1.,1.15648231731787E-15,0.)) ;
#86691 = DIRECTION('ref_axis',(1.03435541192675E-15,-1.,0.)) ;
#86692 = DIRECTION('center_axis',(7.089177613099E-16,-0.612994899008946,-0.790086864711098)) ;
#86693 = DIRECTION('ref_axis',(-5.20417042793041E-14,-0.790086864711098,0.612994899008946)) ;
#86694 = DIRECTION('center_axis',(7.08917761309899E-16,-0.612994899008945,
0.790086864711098)) ;
#86695 = DIRECTION('ref_axis',(-3.46944695195361E-14,0.790086864711098,0.612994899008945)) ;
#86696 = DIRECTION('center_axis',(0.,0.,-1.)) ;
#86697 = DIRECTION('ref_axis',(-1.,0.,0.)) ;
#86698 = DIRECTION('center_axis',(0.,0.,1.)) ;
#86699 = DIRECTION('ref_axis',(-1.,2.16840434497102E-15,0.)) ;
#86700 = DIRECTION('center_axis',(1.08420217248551E-15,-1.,0.)) ;
#86701 = DIRECTION('ref_axis',(1.,1.08420217248551E-15,0.)) ;
#86702 = DIRECTION('center_axis',(1.44560289664734E-16,-1.,-2.4093381610789E-16)) ;
#86703 = DIRECTION('ref_axis',(2.28544744656275E-46,2.4093381610789E-16,-1.)) ;
#86704 = DIRECTION('center_axis',(0.,-1.,0.)) ;
#86705 = DIRECTION('ref_axis',(0.,0.,-1.)) ;
#86706 = DIRECTION('center_axis',(1.,0.,0.)) ;
#86707 = DIRECTION('ref_axis',(0.,1.,0.)) ;
#86708 = DIRECTION('center_axis',(1.,0.,0.)) ;
#86709 = DIRECTION('ref_axis',(0.,0.,-1.)) ;
#86710 = DIRECTION('center_axis',(1.,1.23908819712629E-16,8.95614743483648E-33)) ;
#86711 = DIRECTION('ref_axis',(-1.23908819712629E-16,1.,-1.10974565782288E-48)) ;
#86712 = DIRECTION('center_axis',(1.,0.,0.)) ;
#86713 = DIRECTION('ref_axis',(0.,0.,-1.)) ;
#86714 = DIRECTION('center_axis',(-1.,0.,0.)) ;
#86715 = DIRECTION('ref_axis',(0.,0.,1.)) ;
#86716 = DIRECTION('center_axis',(1.,1.23908819712629E-16,8.95614743483648E-33)) ;
#86717 = DIRECTION('ref_axis',(-1.23908819712629E-16,1.,-1.10974565782288E-48)) ;
#86718 = DIRECTION('center_axis',(-1.,0.,0.)) ;
#86719 = DIRECTION('ref_axis',(0.,0.,1.)) ;
#86720 = DIRECTION('center_axis',(1.,0.,0.)) ;
#86721 = DIRECTION('ref_axis',(0.,-1.,0.)) ;
#86722 = DIRECTION('center_axis',(0.,1.,0.)) ;
#86723 = DIRECTION('ref_axis',(0.,0.,1.)) ;
#86724 = DIRECTION('center_axis',(-1.44560289664734E-16,1.,-7.2280144832367E-17)) ;
#86725 = DIRECTION('ref_axis',(0.707106781238304,1.53329341672078E-16,0.707106781134791)) ;
#86726 = DIRECTION('center_axis',(-1.0842021724855E-15,1.,0.)) ;
#86727 = DIRECTION('ref_axis',(-1.,-1.0842021724855E-15,0.)) ;
#86728 = DIRECTION('center_axis',(0.,1.,0.)) ;
#86729 = DIRECTION('ref_axis',(0.,0.,1.)) ;
#86730 = DIRECTION('center_axis',(0.,-1.,0.)) ;
#86731 = DIRECTION('ref_axis',(0.,0.,-1.)) ;
#86732 = DIRECTION('center_axis',(0.,1.,0.)) ;
#86733 = DIRECTION('ref_axis',(0.,0.,1.)) ;
#86734 = DIRECTION('center_axis',(0.,0.,1.)) ;
#86735 = DIRECTION('ref_axis',(1.,0.,0.)) ;
#86736 = DIRECTION('center_axis',(0.431191646766499,0.0335421424315027,0.901636672080223)) ;
#86737 = DIRECTION('ref_axis',(0.899826811355995,0.0573593270524375,-0.432459960187061)) ;
#86738 = DIRECTION('center_axis',(0.,0.,1.)) ;
#86739 = DIRECTION('ref_axis',(-1.,0.,0.)) ;
#86740 = DIRECTION('center_axis',(0.,0.,-1.)) ;
#86741 = DIRECTION('ref_axis',(0.707109343403322,-0.707104218960488,0.)) ;
#86742 = DIRECTION('center_axis',(-3.25260651745653E-15,0.,1.)) ;
#86743 = DIRECTION('ref_axis',(1.,0.,3.25260651745653E-15)) ;
#86744 = DIRECTION('center_axis',(0.,0.,1.)) ;
#86745 = DIRECTION('ref_axis',(1.,0.,0.)) ;
#86746 = DIRECTION('center_axis',(0.431188264324026,0.0335835000973875,-0.901636750155207)) ;
#86747 = DIRECTION('ref_axis',(0.899831768145072,0.0572892325739573,0.432458937782537)) ;
#86748 = DIRECTION('center_axis',(0.,-1.,0.)) ;
#86749 = DIRECTION('ref_axis',(0.,0.,-1.)) ;
#86750 = DIRECTION('center_axis',(0.,1.,0.)) ;
#86751 = DIRECTION('ref_axis',(0.,0.,1.)) ;
#86752 = DIRECTION('center_axis',(0.,0.,1.)) ;
#86753 = DIRECTION('ref_axis',(1.,0.,0.)) ;
#86754 = DIRECTION('center_axis',(0.,0.,-1.)) ;
#86755 = DIRECTION('ref_axis',(-1.,0.,0.)) ;
#86756 = DIRECTION('center_axis',(0.,0.,1.)) ;
#86757 = DIRECTION('ref_axis',(-0.986393923832144,0.164398987305354,0.)) ;
#86758 = DIRECTION('center_axis',(0.98470178743927,-0.164116964573216,0.0585492250433781)) ;
#86759 = DIRECTION('ref_axis',(0.164398987305362,0.986393923832143,-7.60669428566932E-17)) ;
#86760 = DIRECTION('center_axis',(0.984834538781277,-0.164139089796902,0.0562075655416074)) ;
#86761 = DIRECTION('ref_axis',(0.164398987305379,0.98639392383214,1.87706412796466E-17)) ;
#86762 = DIRECTION('center_axis',(0.986393923832145,-0.129889480441767,0.100775740620414)) ;
#86763 = DIRECTION('ref_axis',(0.,0.612994899008949,0.790086864711095)) ;
#86764 = DIRECTION('center_axis',(0.,1.,0.)) ;
#86765 = DIRECTION('ref_axis',(1.,0.,0.)) ;
#86766 = DIRECTION('center_axis',(0.,0.,-1.)) ;
#86767 = DIRECTION('ref_axis',(-1.,0.,0.)) ;
#86768 = DIRECTION('center_axis',(1.,2.8359373108165E-15,0.)) ;
#86769 = DIRECTION('ref_axis',(-2.8359373108165E-15,1.,0.)) ;
#86770 = DIRECTION('center_axis',(0.,0.,-1.)) ;
#86771 = DIRECTION('ref_axis',(-1.,0.,0.)) ;
#86772 = DIRECTION('center_axis',(0.,0.,1.)) ;
#86773 = DIRECTION('ref_axis',(1.,0.,0.)) ;
#86774 = DIRECTION('center_axis',(1.,0.,0.)) ;
#86775 = DIRECTION('ref_axis',(0.,0.,-1.)) ;
#86776 = DIRECTION('center_axis',(1.,0.,0.)) ;
#86777 = DIRECTION('ref_axis',(0.,0.,-1.)) ;
#86778 = DIRECTION('center_axis',(0.,1.,0.)) ;
#86779 = DIRECTION('ref_axis',(1.,0.,0.)) ;
#86780 = DIRECTION('center_axis',(1.,-8.50781193244945E-15,0.)) ;
#86781 = DIRECTION('ref_axis',(8.50781193244945E-15,1.,0.)) ;
#86782 = DIRECTION('center_axis',(0.,1.,0.)) ;
#86783 = DIRECTION('ref_axis',(1.,0.,0.)) ;
#86784 = DIRECTION('center_axis',(-5.42101086242753E-16,1.70882313734897E-16,
1.)) ;
#86785 = DIRECTION('ref_axis',(1.,9.26354878953623E-32,5.42101086242753E-16)) ;
#86786 = DIRECTION('center_axis',(-1.,0.,0.)) ;
#86787 = DIRECTION('ref_axis',(0.,0.,1.)) ;
#86788 = DIRECTION('center_axis',(1.,0.,0.)) ;
#86789 = DIRECTION('ref_axis',(0.,0.,-1.)) ;
#86790 = DIRECTION('center_axis',(0.,0.,-1.)) ;
#86791 = DIRECTION('ref_axis',(-1.,0.,0.)) ;
#86792 = DIRECTION('center_axis',(0.,0.,1.)) ;
#86793 = DIRECTION('ref_axis',(1.,0.,0.)) ;
#86794 = DIRECTION('center_axis',(0.,1.,0.)) ;
#86795 = DIRECTION('ref_axis',(1.,0.,0.)) ;
#86796 = DIRECTION('center_axis',(0.,1.,0.)) ;
#86797 = DIRECTION('ref_axis',(1.,0.,0.)) ;
#86798 = DIRECTION('center_axis',(0.,0.,-1.)) ;
#86799 = DIRECTION('ref_axis',(-1.,0.,0.)) ;
#86800 = DIRECTION('center_axis',(0.,1.,0.)) ;
#86801 = DIRECTION('ref_axis',(0.,0.,1.)) ;
#86802 = DIRECTION('center_axis',(0.,0.,-1.)) ;
#86803 = DIRECTION('ref_axis',(-1.,0.,0.)) ;
#86804 = DIRECTION('center_axis',(0.,0.,1.)) ;
#86805 = DIRECTION('ref_axis',(1.,0.,0.)) ;
#86806 = DIRECTION('center_axis',(1.33440267382831E-16,1.,0.)) ;
#86807 = DIRECTION('ref_axis',(-1.,1.33440267382831E-16,0.)) ;
#86808 = DIRECTION('center_axis',(0.,1.,0.)) ;
#86809 = DIRECTION('ref_axis',(0.,0.,1.)) ;
#86810 = DIRECTION('center_axis',(0.,1.,0.)) ;
#86811 = DIRECTION('ref_axis',(1.,0.,0.)) ;
#86812 = DIRECTION('center_axis',(0.,1.,0.)) ;
#86813 = DIRECTION('ref_axis',(0.,0.,1.)) ;
#86814 = DIRECTION('center_axis',(0.,1.,0.)) ;
#86815 = DIRECTION('ref_axis',(1.,0.,0.)) ;
#86816 = DIRECTION('center_axis',(1.37797793267296E-15,-1.62630325872825E-15,
1.)) ;
#86817 = DIRECTION('ref_axis',(-2.24101000236165E-30,-1.,-1.62630325872825E-15)) ;
#86818 = DIRECTION('center_axis',(-1.33440267382831E-16,-1.,0.)) ;
#86819 = DIRECTION('ref_axis',(1.,-1.33440267382831E-16,0.)) ;
#86820 = DIRECTION('center_axis',(0.,1.,0.)) ;
#86821 = DIRECTION('ref_axis',(0.,0.,1.)) ;
#86822 = DIRECTION('center_axis',(0.,0.,-1.)) ;
#86823 = DIRECTION('ref_axis',(-1.,0.,0.)) ;
#86824 = DIRECTION('center_axis',(0.,0.,1.)) ;
#86825 = DIRECTION('ref_axis',(1.,0.,0.)) ;
#86826 = DIRECTION('center_axis',(0.,1.,0.)) ;
#86827 = DIRECTION('ref_axis',(1.,0.,0.)) ;
#86828 = DIRECTION('center_axis',(0.,0.,1.)) ;
#86829 = DIRECTION('ref_axis',(1.,0.,0.)) ;
#86830 = DIRECTION('center_axis',(0.,0.,1.)) ;
#86831 = DIRECTION('ref_axis',(1.,0.,0.)) ;
#86832 = DIRECTION('center_axis',(0.,0.,1.)) ;
#86833 = DIRECTION('ref_axis',(-0.986393923832144,0.164398987305354,0.)) ;
#86834 = DIRECTION('center_axis',(0.984701787439272,-0.164116964573205,-0.0585492250433871)) ;
#86835 = DIRECTION('ref_axis',(0.16439898730535,0.986393923832145,-3.2807868055655E-16)) ;
#86836 = DIRECTION('center_axis',(0.984834538781259,-0.164139089796881,-0.0562075655419907)) ;
#86837 = DIRECTION('ref_axis',(0.164398987305362,0.986393923832143,6.03508511856301E-17)) ;
#86838 = DIRECTION('center_axis',(0.,0.,1.)) ;
#86839 = DIRECTION('ref_axis',(-0.986393923832144,0.164398987305354,0.)) ;
#86840 = DIRECTION('center_axis',(0.,0.,1.)) ;
#86841 = DIRECTION('ref_axis',(1.,0.,0.)) ;
#86842 = DIRECTION('center_axis',(0.342346838786525,0.100237737278944,-0.934211452508516)) ;
#86843 = DIRECTION('ref_axis',(0.878411850175152,0.318727802690732,0.356097190755283)) ;
#86844 = DIRECTION('center_axis',(0.,0.,-1.)) ;
#86845 = DIRECTION('ref_axis',(-1.,0.,0.)) ;
#86846 = DIRECTION('center_axis',(0.,0.,-1.)) ;
#86847 = DIRECTION('ref_axis',(-1.,0.,0.)) ;
#86848 = DIRECTION('center_axis',(0.,0.,-1.)) ;
#86849 = DIRECTION('ref_axis',(-1.,0.,0.)) ;
#86850 = DIRECTION('center_axis',(-0.342346838787816,-0.100237737288811,-0.934211452506984)) ;
#86851 = DIRECTION('ref_axis',(0.878411919034117,0.318727608050549,-0.356097195109952)) ;
#86852 = DIRECTION('center_axis',(0.,0.,1.)) ;
#86853 = DIRECTION('ref_axis',(1.,0.,0.)) ;
#86854 = DIRECTION('axis',(0.,0.,1.)) ;
#86855 = DIRECTION('refdir',(1.,0.,0.)) ;
#86856 = DIRECTION('center_axis',(0.,-1.,0.)) ;
#86857 = DIRECTION('ref_axis',(0.,0.,-1.)) ;
#86858 = DIRECTION('center_axis',(0.,1.,0.)) ;
#86859 = DIRECTION('ref_axis',(0.,0.,1.)) ;
#86860 = DIRECTION('',(0.,1.,0.)) ;
#86861 = DIRECTION('center_axis',(0.,-1.,0.)) ;
#86862 = DIRECTION('ref_axis',(0.,0.,-1.)) ;
#86863 = DIRECTION('center_axis',(0.,-1.,0.)) ;
#86864 = DIRECTION('ref_axis',(0.,0.,-1.)) ;
#86865 = DIRECTION('center_axis',(0.,-1.,0.)) ;
#86866 = DIRECTION('ref_axis',(0.,0.,-1.)) ;
#86867 = DIRECTION('center_axis',(0.,1.,0.)) ;
#86868 = DIRECTION('ref_axis',(0.,0.,1.)) ;
#86869 = DIRECTION('',(0.,-1.,0.)) ;
#86870 = DIRECTION('center_axis',(0.,1.,0.)) ;
#86871 = DIRECTION('ref_axis',(0.,0.,1.)) ;
#86872 = DIRECTION('',(0.,-1.,0.)) ;
#86873 = DIRECTION('center_axis',(0.,0.,-1.)) ;
#86874 = DIRECTION('ref_axis',(-1.,0.,0.)) ;
#86875 = DIRECTION('center_axis',(0.,0.,-1.)) ;
#86876 = DIRECTION('ref_axis',(-1.,0.,0.)) ;
#86877 = DIRECTION('',(0.,-1.,0.)) ;
#86878 = DIRECTION('',(1.,0.,0.)) ;
#86879 = DIRECTION('center_axis',(0.,0.,1.)) ;
#86880 = DIRECTION('ref_axis',(-1.,-1.81411780829267E-15,0.)) ;
#86881 = DIRECTION('',(0.,-1.,0.)) ;
#86882 = DIRECTION('',(-1.,0.,0.)) ;
#86883 = DIRECTION('',(0.,1.,0.)) ;
#86884 = DIRECTION('center_axis',(0.,0.,1.)) ;
#86885 = DIRECTION('ref_axis',(1.,0.,0.)) ;
#86886 = DIRECTION('',(-1.,0.,0.)) ;
#86887 = DIRECTION('',(0.,-1.,0.)) ;
#86888 = DIRECTION('center_axis',(0.,0.,1.)) ;
#86889 = DIRECTION('ref_axis',(1.,0.,0.)) ;
#86890 = DIRECTION('',(0.,1.,0.)) ;
#86891 = DIRECTION('',(1.,0.,0.)) ;
#86892 = DIRECTION('',(0.,-1.,0.)) ;
#86893 = DIRECTION('center_axis',(0.,0.,-1.)) ;
#86894 = DIRECTION('ref_axis',(1.,0.,0.)) ;
#86895 = DIRECTION('center_axis',(1.,0.,-1.0671281225251E-16)) ;
#86896 = DIRECTION('ref_axis',(-1.0671281225251E-16,0.,-1.)) ;
#86897 = DIRECTION('',(-1.0671281225251E-16,0.,-1.)) ;
#86898 = DIRECTION('',(0.,0.,-1.)) ;
#86899 = DIRECTION('center_axis',(0.,0.,-1.)) ;
#86900 = DIRECTION('ref_axis',(-1.,0.,0.)) ;
#86901 = DIRECTION('',(1.,0.,0.)) ;
#86902 = DIRECTION('',(0.,1.,0.)) ;
#86903 = DIRECTION('center_axis',(0.,0.,-1.)) ;
#86904 = DIRECTION('ref_axis',(-1.,0.,0.)) ;
#86905 = DIRECTION('',(0.,1.,0.)) ;
#86906 = DIRECTION('',(-1.,0.,-1.0671281225251E-16)) ;
#86907 = DIRECTION('',(0.,-1.,0.)) ;
#86908 = DIRECTION('center_axis',(0.,0.,1.)) ;
#86909 = DIRECTION('ref_axis',(-1.,0.,0.)) ;
#86910 = DIRECTION('center_axis',(-1.,0.,0.)) ;
#86911 = DIRECTION('ref_axis',(0.,0.,1.)) ;
#86912 = DIRECTION('',(0.,-1.,0.)) ;
#86913 = DIRECTION('',(0.,0.,1.)) ;
#86914 = DIRECTION('',(0.,0.,1.)) ;
#86915 = DIRECTION('center_axis',(0.,0.,1.)) ;
#86916 = DIRECTION('ref_axis',(1.,0.,0.)) ;
#86917 = DIRECTION('center_axis',(0.,0.,1.)) ;
#86918 = DIRECTION('ref_axis',(1.,0.,0.)) ;
#86919 = DIRECTION('',(0.,1.,0.)) ;
#86920 = DIRECTION('',(-1.,0.,0.)) ;
#86921 = DIRECTION('center_axis',(0.,0.,-1.)) ;
#86922 = DIRECTION('ref_axis',(1.,-1.81411780829268E-15,0.)) ;
#86923 = DIRECTION('',(1.,0.,0.)) ;
#86924 = DIRECTION('',(0.,1.,0.)) ;
#86925 = DIRECTION('center_axis',(-1.,0.,-2.13425624505021E-16)) ;
#86926 = DIRECTION('ref_axis',(-2.13425624505021E-16,0.,1.)) ;
#86927 = DIRECTION('',(-2.13425624505021E-16,0.,1.)) ;
#86928 = DIRECTION('',(-2.13425624505021E-16,0.,1.)) ;
#86929 = DIRECTION('center_axis',(0.,-1.,0.)) ;
#86930 = DIRECTION('ref_axis',(0.,0.,-1.)) ;
#86931 = DIRECTION('center_axis',(1.,0.,0.)) ;
#86932 = DIRECTION('ref_axis',(0.,0.,-1.)) ;
#86933 = DIRECTION('',(0.,0.,-1.)) ;
#86934 = DIRECTION('',(0.,0.,-1.)) ;
#86935 = DIRECTION('center_axis',(0.,1.,0.)) ;
#86936 = DIRECTION('ref_axis',(0.,0.,1.)) ;
#86937 = DIRECTION('center_axis',(-1.0671281225251E-16,0.,-1.)) ;
#86938 = DIRECTION('ref_axis',(-1.,0.,1.0671281225251E-16)) ;
#86939 = DIRECTION('',(1.0671281225251E-16,0.,1.)) ;
#86940 = DIRECTION('center_axis',(0.,0.,1.)) ;
#86941 = DIRECTION('ref_axis',(1.,0.,0.)) ;
#86942 = DIRECTION('',(0.,0.,-1.)) ;
#86943 = DIRECTION('center_axis',(2.13425624505021E-16,0.,-1.)) ;
#86944 = DIRECTION('ref_axis',(-1.,0.,-2.13425624505021E-16)) ;
#86945 = DIRECTION('',(2.13425624505021E-16,0.,-1.)) ;
#86946 = DIRECTION('center_axis',(0.,0.,1.)) ;
#86947 = DIRECTION('ref_axis',(1.,0.,0.)) ;
#86948 = DIRECTION('',(0.,0.,1.)) ;
#86949 = DIRECTION('center_axis',(0.,1.,0.)) ;
#86950 = DIRECTION('ref_axis',(0.,0.,1.)) ;
#86951 = DIRECTION('',(1.,0.,0.)) ;
#86952 = DIRECTION('',(0.,0.,1.)) ;
#86953 = DIRECTION('',(0.,0.,1.)) ;
#86954 = DIRECTION('center_axis',(0.,0.,-1.)) ;
#86955 = DIRECTION('ref_axis',(-1.,0.,0.)) ;
#86956 = DIRECTION('',(1.,0.,0.)) ;
#86957 = DIRECTION('',(1.,0.,0.)) ;
#86958 = DIRECTION('center_axis',(0.,1.,0.)) ;
#86959 = DIRECTION('ref_axis',(0.,0.,1.)) ;
#86960 = DIRECTION('center_axis',(0.,1.,0.)) ;
#86961 = DIRECTION('ref_axis',(1.,0.,0.)) ;
#86962 = DIRECTION('center_axis',(1.22464679914735E-16,0.,1.)) ;
#86963 = DIRECTION('ref_axis',(-1.,0.,1.22464679914735E-16)) ;
#86964 = DIRECTION('center_axis',(-1.,0.,0.)) ;
#86965 = DIRECTION('ref_axis',(0.,0.,1.)) ;
#86966 = DIRECTION('center_axis',(1.,0.,0.)) ;
#86967 = DIRECTION('ref_axis',(0.,0.,-1.)) ;
#86968 = DIRECTION('axis',(0.,0.,1.)) ;
#86969 = DIRECTION('refdir',(1.,0.,0.)) ;
#86970 = DIRECTION('center_axis',(1.,0.,0.)) ;
#86971 = DIRECTION('ref_axis',(0.,0.,-1.)) ;
#86972 = DIRECTION('center_axis',(1.,0.,0.)) ;
#86973 = DIRECTION('ref_axis',(0.,0.,-1.)) ;
#86974 = DIRECTION('center_axis',(0.,-1.,-1.22464679914735E-16)) ;
#86975 = DIRECTION('ref_axis',(0.,-1.22464679914735E-16,1.)) ;
#86976 = DIRECTION('center_axis',(-1.,0.,0.)) ;
#86977 = DIRECTION('ref_axis',(0.,0.,-1.)) ;
#86978 = DIRECTION('center_axis',(-1.,0.,0.)) ;
#86979 = DIRECTION('ref_axis',(0.,0.,-1.)) ;
#86980 = DIRECTION('center_axis',(-1.,0.,0.)) ;
#86981 = DIRECTION('ref_axis',(0.,0.,1.)) ;
#86982 = DIRECTION('center_axis',(-1.,0.,0.)) ;
#86983 = DIRECTION('ref_axis',(0.,0.,1.)) ;
#86984 = DIRECTION('center_axis',(0.,1.,-1.22464679914735E-16)) ;
#86985 = DIRECTION('ref_axis',(0.,-1.22464679914735E-16,-1.)) ;
#86986 = DIRECTION('center_axis',(1.,0.,0.)) ;
#86987 = DIRECTION('ref_axis',(0.,0.,1.)) ;
#86988 = DIRECTION('center_axis',(0.,1.,0.)) ;
#86989 = DIRECTION('ref_axis',(0.,0.,1.)) ;
#86990 = DIRECTION('center_axis',(-1.,0.,0.)) ;
#86991 = DIRECTION('ref_axis',(0.,0.,-1.)) ;
#86992 = DIRECTION('center_axis',(0.,0.707106781186532,0.707106781186563)) ;
#86993 = DIRECTION('ref_axis',(0.,-0.707106781186563,0.707106781186532)) ;
#86994 = DIRECTION('center_axis',(0.,0.,-1.)) ;
#86995 = DIRECTION('ref_axis',(-1.,0.,0.)) ;
#86996 = DIRECTION('center_axis',(2.16840434497101E-16,-1.,1.30104260698261E-16)) ;
#86997 = DIRECTION('ref_axis',(1.,2.16840434497101E-16,-1.09476442525376E-47)) ;
#86998 = DIRECTION('center_axis',(-2.25262403289994E-12,-0.707106781186411,
-0.707106781186684)) ;
#86999 = DIRECTION('ref_axis',(2.77642807980434E-11,0.707106781186684,-0.707106781186411)) ;
#87000 = DIRECTION('center_axis',(-5.42101086242752E-16,1.,0.)) ;
#87001 = DIRECTION('ref_axis',(1.,5.42101086242752E-16,0.)) ;
#87002 = DIRECTION('',(-2.16840434497101E-16,1.,-1.30104260698261E-16)) ;
#87003 = DIRECTION('center_axis',(0.,1.,0.)) ;
#87004 = DIRECTION('ref_axis',(0.,0.,1.)) ;
#87005 = DIRECTION('',(2.16840434497101E-16,-1.,1.30104260698261E-16)) ;
#87006 = DIRECTION('',(2.16840434497101E-16,-1.,1.30104260698261E-16)) ;
#87007 = DIRECTION('center_axis',(1.,0.,0.)) ;
#87008 = DIRECTION('ref_axis',(0.,0.,-1.)) ;
#87009 = DIRECTION('center_axis',(1.,0.,0.)) ;
#87010 = DIRECTION('ref_axis',(0.,0.,-1.)) ;
#87011 = DIRECTION('center_axis',(0.,-1.,-1.22464679914735E-16)) ;
#87012 = DIRECTION('ref_axis',(0.,-1.22464679914735E-16,1.)) ;
#87013 = DIRECTION('center_axis',(-1.,0.,0.)) ;
#87014 = DIRECTION('ref_axis',(0.,0.,-1.)) ;
#87015 = DIRECTION('center_axis',(-1.,0.,0.)) ;
#87016 = DIRECTION('ref_axis',(0.,0.,-1.)) ;
#87017 = DIRECTION('center_axis',(-1.,0.,0.)) ;
#87018 = DIRECTION('ref_axis',(0.,0.,1.)) ;
#87019 = DIRECTION('center_axis',(-1.,0.,0.)) ;
#87020 = DIRECTION('ref_axis',(0.,0.,1.)) ;
#87021 = DIRECTION('center_axis',(0.,1.,-1.22464679914735E-16)) ;
#87022 = DIRECTION('ref_axis',(0.,-1.22464679914735E-16,-1.)) ;
#87023 = DIRECTION('center_axis',(1.,0.,0.)) ;
#87024 = DIRECTION('ref_axis',(0.,0.,1.)) ;
#87025 = DIRECTION('center_axis',(0.,1.,0.)) ;
#87026 = DIRECTION('ref_axis',(0.,0.,1.)) ;
#87027 = DIRECTION('center_axis',(-1.,0.,0.)) ;
#87028 = DIRECTION('ref_axis',(0.,0.,-1.)) ;
#87029 = DIRECTION('center_axis',(0.,0.707106781186558,0.707106781186537)) ;
#87030 = DIRECTION('ref_axis',(0.,-0.707106781186537,0.707106781186558)) ;
#87031 = DIRECTION('center_axis',(0.,0.,-1.)) ;
#87032 = DIRECTION('ref_axis',(-1.,0.,0.)) ;
#87033 = DIRECTION('center_axis',(2.16840434497101E-16,-1.,1.30104260698261E-16)) ;
#87034 = DIRECTION('ref_axis',(1.,2.16840434497101E-16,-1.09476442525376E-47)) ;
#87035 = DIRECTION('center_axis',(-2.85488809725132E-13,-0.707106781186525,
-0.70710678118657)) ;
#87036 = DIRECTION('ref_axis',(7.82804041694617E-11,0.70710678118657,-0.707106781186525)) ;
#87037 = DIRECTION('center_axis',(-5.42101086242752E-16,1.,0.)) ;
#87038 = DIRECTION('ref_axis',(1.,5.42101086242752E-16,0.)) ;
#87039 = DIRECTION('',(-2.16840434497101E-16,1.,-1.30104260698261E-16)) ;
#87040 = DIRECTION('center_axis',(0.,1.,0.)) ;
#87041 = DIRECTION('ref_axis',(0.,0.,1.)) ;
#87042 = DIRECTION('',(2.16840434497101E-16,-1.,1.30104260698261E-16)) ;
#87043 = DIRECTION('',(2.16840434497101E-16,-1.,1.30104260698261E-16)) ;
#87044 = DIRECTION('center_axis',(1.,0.,0.)) ;
#87045 = DIRECTION('ref_axis',(0.,0.,-1.)) ;
#87046 = DIRECTION('center_axis',(1.,0.,0.)) ;
#87047 = DIRECTION('ref_axis',(0.,0.,-1.)) ;
#87048 = DIRECTION('center_axis',(0.,-1.,-1.22464679914735E-16)) ;
#87049 = DIRECTION('ref_axis',(0.,-1.22464679914735E-16,1.)) ;
#87050 = DIRECTION('center_axis',(-1.,0.,0.)) ;
#87051 = DIRECTION('ref_axis',(0.,0.,-1.)) ;
#87052 = DIRECTION('center_axis',(-1.,0.,0.)) ;
#87053 = DIRECTION('ref_axis',(0.,0.,-1.)) ;
#87054 = DIRECTION('center_axis',(-1.,0.,0.)) ;
#87055 = DIRECTION('ref_axis',(0.,0.,1.)) ;
#87056 = DIRECTION('center_axis',(-1.,0.,0.)) ;
#87057 = DIRECTION('ref_axis',(0.,0.,1.)) ;
#87058 = DIRECTION('center_axis',(0.,1.,-1.22464679914735E-16)) ;
#87059 = DIRECTION('ref_axis',(0.,-1.22464679914735E-16,-1.)) ;
#87060 = DIRECTION('center_axis',(1.,0.,0.)) ;
#87061 = DIRECTION('ref_axis',(0.,0.,1.)) ;
#87062 = DIRECTION('center_axis',(0.,1.,0.)) ;
#87063 = DIRECTION('ref_axis',(0.,0.,1.)) ;
#87064 = DIRECTION('center_axis',(-1.,0.,0.)) ;
#87065 = DIRECTION('ref_axis',(0.,0.,-1.)) ;
#87066 = DIRECTION('center_axis',(0.,0.707106781186558,0.707106781186537)) ;
#87067 = DIRECTION('ref_axis',(0.,-0.707106781186537,0.707106781186558)) ;
#87068 = DIRECTION('center_axis',(0.,0.,-1.)) ;
#87069 = DIRECTION('ref_axis',(-1.,0.,0.)) ;
#87070 = DIRECTION('center_axis',(2.16840434497101E-16,-1.,1.30104260698261E-16)) ;
#87071 = DIRECTION('ref_axis',(1.,2.16840434497101E-16,-1.09476442525376E-47)) ;
#87072 = DIRECTION('center_axis',(-4.61475062295438E-13,-0.707106781186512,
-0.707106781186583)) ;
#87073 = DIRECTION('ref_axis',(8.02352901261504E-11,0.707106781186583,-0.707106781186512)) ;
#87074 = DIRECTION('center_axis',(-5.42101086242752E-16,1.,0.)) ;
#87075 = DIRECTION('ref_axis',(1.,5.42101086242752E-16,0.)) ;
#87076 = DIRECTION('',(-2.16840434497101E-16,1.,-1.30104260698261E-16)) ;
#87077 = DIRECTION('center_axis',(0.,1.,0.)) ;
#87078 = DIRECTION('ref_axis',(0.,0.,1.)) ;
#87079 = DIRECTION('',(2.16840434497101E-16,-1.,1.30104260698261E-16)) ;
#87080 = DIRECTION('',(2.16840434497101E-16,-1.,1.30104260698261E-16)) ;
#87081 = DIRECTION('center_axis',(1.,0.,0.)) ;
#87082 = DIRECTION('ref_axis',(0.,0.,-1.)) ;
#87083 = DIRECTION('center_axis',(1.,0.,0.)) ;
#87084 = DIRECTION('ref_axis',(0.,0.,-1.)) ;
#87085 = DIRECTION('center_axis',(0.,-1.,-1.22464679914735E-16)) ;
#87086 = DIRECTION('ref_axis',(0.,-1.22464679914735E-16,1.)) ;
#87087 = DIRECTION('center_axis',(-1.,0.,0.)) ;
#87088 = DIRECTION('ref_axis',(0.,0.,-1.)) ;
#87089 = DIRECTION('center_axis',(-1.,0.,0.)) ;
#87090 = DIRECTION('ref_axis',(0.,0.,-1.)) ;
#87091 = DIRECTION('center_axis',(-1.,0.,0.)) ;
#87092 = DIRECTION('ref_axis',(0.,0.,1.)) ;
#87093 = DIRECTION('center_axis',(-1.,0.,0.)) ;
#87094 = DIRECTION('ref_axis',(0.,0.,1.)) ;
#87095 = DIRECTION('center_axis',(0.,1.,-1.22464679914735E-16)) ;
#87096 = DIRECTION('ref_axis',(0.,-1.22464679914735E-16,-1.)) ;
#87097 = DIRECTION('center_axis',(1.,0.,0.)) ;
#87098 = DIRECTION('ref_axis',(0.,0.,1.)) ;
#87099 = DIRECTION('center_axis',(0.,1.,0.)) ;
#87100 = DIRECTION('ref_axis',(0.,0.,1.)) ;
#87101 = DIRECTION('center_axis',(-1.,0.,0.)) ;
#87102 = DIRECTION('ref_axis',(0.,0.,-1.)) ;
#87103 = DIRECTION('center_axis',(0.,0.707106781186558,0.707106781186537)) ;
#87104 = DIRECTION('ref_axis',(0.,-0.707106781186537,0.707106781186558)) ;
#87105 = DIRECTION('center_axis',(0.,0.,-1.)) ;
#87106 = DIRECTION('ref_axis',(-1.,0.,0.)) ;
#87107 = DIRECTION('center_axis',(2.16840434497101E-16,-1.,1.30104260698261E-16)) ;
#87108 = DIRECTION('ref_axis',(1.,2.16840434497101E-16,-1.09476442525376E-47)) ;
#87109 = DIRECTION('center_axis',(-5.4946818858058E-13,-0.707106781186505,
-0.70710678118659)) ;
#87110 = DIRECTION('ref_axis',(1.03835885983909E-10,0.70710678118659,-0.707106781186505)) ;
#87111 = DIRECTION('center_axis',(-5.42101086242752E-16,1.,0.)) ;
#87112 = DIRECTION('ref_axis',(1.,5.42101086242752E-16,0.)) ;
#87113 = DIRECTION('',(-2.16840434497101E-16,1.,-1.30104260698261E-16)) ;
#87114 = DIRECTION('center_axis',(0.,1.,0.)) ;
#87115 = DIRECTION('ref_axis',(0.,0.,1.)) ;
#87116 = DIRECTION('',(2.16840434497101E-16,-1.,1.30104260698261E-16)) ;
#87117 = DIRECTION('',(2.16840434497101E-16,-1.,1.30104260698261E-16)) ;
#87118 = DIRECTION('center_axis',(1.,0.,0.)) ;
#87119 = DIRECTION('ref_axis',(0.,0.,-1.)) ;
#87120 = DIRECTION('center_axis',(1.,0.,0.)) ;
#87121 = DIRECTION('ref_axis',(0.,0.,-1.)) ;
#87122 = DIRECTION('center_axis',(0.,-1.,-1.22464679914735E-16)) ;
#87123 = DIRECTION('ref_axis',(0.,-1.22464679914735E-16,1.)) ;
#87124 = DIRECTION('center_axis',(-1.,0.,0.)) ;
#87125 = DIRECTION('ref_axis',(0.,0.,-1.)) ;
#87126 = DIRECTION('center_axis',(-1.,0.,0.)) ;
#87127 = DIRECTION('ref_axis',(0.,0.,-1.)) ;
#87128 = DIRECTION('center_axis',(-1.,0.,0.)) ;
#87129 = DIRECTION('ref_axis',(0.,0.,1.)) ;
#87130 = DIRECTION('center_axis',(-1.,0.,0.)) ;
#87131 = DIRECTION('ref_axis',(0.,0.,1.)) ;
#87132 = DIRECTION('center_axis',(0.,1.,-1.22464679914735E-16)) ;
#87133 = DIRECTION('ref_axis',(0.,-1.22464679914735E-16,-1.)) ;
#87134 = DIRECTION('center_axis',(1.,0.,0.)) ;
#87135 = DIRECTION('ref_axis',(0.,0.,1.)) ;
#87136 = DIRECTION('center_axis',(0.,1.,0.)) ;
#87137 = DIRECTION('ref_axis',(0.,0.,1.)) ;
#87138 = DIRECTION('center_axis',(-1.,0.,0.)) ;
#87139 = DIRECTION('ref_axis',(0.,0.,-1.)) ;
#87140 = DIRECTION('center_axis',(0.,0.707106781186558,0.707106781186537)) ;
#87141 = DIRECTION('ref_axis',(0.,-0.707106781186537,0.707106781186558)) ;
#87142 = DIRECTION('center_axis',(0.,0.,-1.)) ;
#87143 = DIRECTION('ref_axis',(-1.,0.,0.)) ;
#87144 = DIRECTION('center_axis',(2.16840434497101E-16,-1.,1.30104260698261E-16)) ;
#87145 = DIRECTION('ref_axis',(1.,2.16840434497101E-16,-1.09476442525376E-47)) ;
#87146 = DIRECTION('center_axis',(-4.61475062295467E-13,-0.707106781186512,
-0.707106781186583)) ;
#87147 = DIRECTION('ref_axis',(8.2666922773353E-11,0.707106781186583,-0.707106781186512)) ;
#87148 = DIRECTION('center_axis',(-5.42101086242752E-16,1.,0.)) ;
#87149 = DIRECTION('ref_axis',(1.,5.42101086242752E-16,0.)) ;
#87150 = DIRECTION('',(-2.16840434497101E-16,1.,-1.30104260698261E-16)) ;
#87151 = DIRECTION('center_axis',(0.,1.,0.)) ;
#87152 = DIRECTION('ref_axis',(0.,0.,1.)) ;
#87153 = DIRECTION('',(2.16840434497101E-16,-1.,1.30104260698261E-16)) ;
#87154 = DIRECTION('',(2.16840434497101E-16,-1.,1.30104260698261E-16)) ;
#87155 = DIRECTION('center_axis',(1.,0.,0.)) ;
#87156 = DIRECTION('ref_axis',(0.,0.,-1.)) ;
#87157 = DIRECTION('center_axis',(1.,0.,0.)) ;
#87158 = DIRECTION('ref_axis',(0.,0.,-1.)) ;
#87159 = DIRECTION('center_axis',(0.,-1.,-1.22464679914735E-16)) ;
#87160 = DIRECTION('ref_axis',(0.,-1.22464679914735E-16,1.)) ;
#87161 = DIRECTION('center_axis',(-1.,0.,0.)) ;
#87162 = DIRECTION('ref_axis',(0.,0.,-1.)) ;
#87163 = DIRECTION('center_axis',(-1.,0.,0.)) ;
#87164 = DIRECTION('ref_axis',(0.,0.,-1.)) ;
#87165 = DIRECTION('center_axis',(-1.,0.,0.)) ;
#87166 = DIRECTION('ref_axis',(0.,0.,1.)) ;
#87167 = DIRECTION('center_axis',(-1.,0.,0.)) ;
#87168 = DIRECTION('ref_axis',(0.,0.,1.)) ;
#87169 = DIRECTION('center_axis',(0.,1.,-1.22464679914735E-16)) ;
#87170 = DIRECTION('ref_axis',(0.,-1.22464679914735E-16,-1.)) ;
#87171 = DIRECTION('center_axis',(1.,0.,0.)) ;
#87172 = DIRECTION('ref_axis',(0.,0.,1.)) ;
#87173 = DIRECTION('center_axis',(0.,1.,0.)) ;
#87174 = DIRECTION('ref_axis',(0.,0.,1.)) ;
#87175 = DIRECTION('center_axis',(-1.,0.,0.)) ;
#87176 = DIRECTION('ref_axis',(0.,0.,-1.)) ;
#87177 = DIRECTION('center_axis',(0.,0.707106781186545,0.70710678118655)) ;
#87178 = DIRECTION('ref_axis',(0.,-0.70710678118655,0.707106781186545)) ;
#87179 = DIRECTION('center_axis',(0.,0.,-1.)) ;
#87180 = DIRECTION('ref_axis',(-1.,0.,0.)) ;
#87181 = DIRECTION('center_axis',(2.16840434497101E-16,-1.,1.30104260698261E-16)) ;
#87182 = DIRECTION('ref_axis',(1.,2.16840434497101E-16,-1.09476442525376E-47)) ;
#87183 = DIRECTION('center_axis',(-6.37461314865721E-13,-0.707106781186499,
-0.707106781186596)) ;
#87184 = DIRECTION('ref_axis',(-7.23831307879934E-11,0.707106781186596,-0.707106781186499)) ;
#87185 = DIRECTION('center_axis',(-5.42101086242752E-16,1.,0.)) ;
#87186 = DIRECTION('ref_axis',(1.,5.42101086242752E-16,0.)) ;
#87187 = DIRECTION('',(-2.16840434497101E-16,1.,-1.30104260698261E-16)) ;
#87188 = DIRECTION('center_axis',(0.,1.,0.)) ;
#87189 = DIRECTION('ref_axis',(0.,0.,1.)) ;
#87190 = DIRECTION('',(2.16840434497101E-16,-1.,1.30104260698261E-16)) ;
#87191 = DIRECTION('',(2.16840434497101E-16,-1.,1.30104260698261E-16)) ;
#87192 = DIRECTION('center_axis',(1.,0.,0.)) ;
#87193 = DIRECTION('ref_axis',(0.,0.,-1.)) ;
#87194 = DIRECTION('center_axis',(1.,0.,0.)) ;
#87195 = DIRECTION('ref_axis',(0.,0.,-1.)) ;
#87196 = DIRECTION('center_axis',(0.,-1.,-1.22464679914735E-16)) ;
#87197 = DIRECTION('ref_axis',(0.,-1.22464679914735E-16,1.)) ;
#87198 = DIRECTION('center_axis',(-1.,0.,0.)) ;
#87199 = DIRECTION('ref_axis',(0.,0.,-1.)) ;
#87200 = DIRECTION('center_axis',(-1.,0.,0.)) ;
#87201 = DIRECTION('ref_axis',(0.,0.,-1.)) ;
#87202 = DIRECTION('center_axis',(-1.,0.,0.)) ;
#87203 = DIRECTION('ref_axis',(0.,0.,1.)) ;
#87204 = DIRECTION('center_axis',(-1.,0.,0.)) ;
#87205 = DIRECTION('ref_axis',(0.,0.,1.)) ;
#87206 = DIRECTION('center_axis',(0.,1.,-1.22464679914735E-16)) ;
#87207 = DIRECTION('ref_axis',(0.,-1.22464679914735E-16,-1.)) ;
#87208 = DIRECTION('center_axis',(1.,0.,0.)) ;
#87209 = DIRECTION('ref_axis',(0.,0.,1.)) ;
#87210 = DIRECTION('center_axis',(0.,1.,0.)) ;
#87211 = DIRECTION('ref_axis',(0.,0.,1.)) ;
#87212 = DIRECTION('center_axis',(-1.,0.,0.)) ;
#87213 = DIRECTION('ref_axis',(0.,0.,-1.)) ;
#87214 = DIRECTION('center_axis',(0.,0.707106781186545,0.70710678118655)) ;
#87215 = DIRECTION('ref_axis',(0.,-0.70710678118655,0.707106781186545)) ;
#87216 = DIRECTION('center_axis',(0.,0.,-1.)) ;
#87217 = DIRECTION('ref_axis',(-1.,0.,0.)) ;
#87218 = DIRECTION('center_axis',(2.16840434497101E-16,-1.,1.30104260698261E-16)) ;
#87219 = DIRECTION('ref_axis',(1.,2.16840434497101E-16,-1.09476442525376E-47)) ;
#87220 = DIRECTION('center_axis',(-2.04144052981523E-12,-0.707106781186384,
-0.707106781186711)) ;
#87221 = DIRECTION('ref_axis',(3.79286005912221E-12,0.707106781186711,-0.707106781186384)) ;
#87222 = DIRECTION('center_axis',(-5.42101086242752E-16,1.,0.)) ;
#87223 = DIRECTION('ref_axis',(1.,5.42101086242752E-16,0.)) ;
#87224 = DIRECTION('',(-2.16840434497101E-16,1.,-1.30104260698261E-16)) ;
#87225 = DIRECTION('center_axis',(0.,1.,0.)) ;
#87226 = DIRECTION('ref_axis',(0.,0.,1.)) ;
#87227 = DIRECTION('',(2.16840434497101E-16,-1.,1.30104260698261E-16)) ;
#87228 = DIRECTION('',(2.16840434497101E-16,-1.,1.30104260698261E-16)) ;
#87229 = DIRECTION('center_axis',(1.,0.,0.)) ;
#87230 = DIRECTION('ref_axis',(0.,0.,-1.)) ;
#87231 = DIRECTION('center_axis',(1.,0.,0.)) ;
#87232 = DIRECTION('ref_axis',(0.,0.,-1.)) ;
#87233 = DIRECTION('center_axis',(0.,-1.,-1.22464679914735E-16)) ;
#87234 = DIRECTION('ref_axis',(0.,-1.22464679914735E-16,1.)) ;
#87235 = DIRECTION('center_axis',(-1.,0.,0.)) ;
#87236 = DIRECTION('ref_axis',(0.,0.,-1.)) ;
#87237 = DIRECTION('center_axis',(-1.,0.,0.)) ;
#87238 = DIRECTION('ref_axis',(0.,0.,-1.)) ;
#87239 = DIRECTION('center_axis',(-1.,0.,0.)) ;
#87240 = DIRECTION('ref_axis',(0.,0.,1.)) ;
#87241 = DIRECTION('center_axis',(-1.,0.,0.)) ;
#87242 = DIRECTION('ref_axis',(0.,0.,1.)) ;
#87243 = DIRECTION('center_axis',(0.,1.,-1.22464679914735E-16)) ;
#87244 = DIRECTION('ref_axis',(0.,-1.22464679914735E-16,-1.)) ;
#87245 = DIRECTION('center_axis',(1.,0.,0.)) ;
#87246 = DIRECTION('ref_axis',(0.,0.,1.)) ;
#87247 = DIRECTION('center_axis',(0.,1.,0.)) ;
#87248 = DIRECTION('ref_axis',(0.,0.,1.)) ;
#87249 = DIRECTION('center_axis',(-1.,0.,0.)) ;
#87250 = DIRECTION('ref_axis',(0.,0.,-1.)) ;
#87251 = DIRECTION('center_axis',(0.,0.707106781186545,0.70710678118655)) ;
#87252 = DIRECTION('ref_axis',(0.,-0.70710678118655,0.707106781186545)) ;
#87253 = DIRECTION('center_axis',(0.,0.,-1.)) ;
#87254 = DIRECTION('ref_axis',(-1.,0.,0.)) ;
#87255 = DIRECTION('center_axis',(2.16840434497101E-16,-1.,1.30104260698261E-16)) ;
#87256 = DIRECTION('ref_axis',(1.,2.16840434497101E-16,-1.09476442525376E-47)) ;
#87257 = DIRECTION('center_axis',(-1.65035996854789E-12,-0.707106781186426,
-0.707106781186669)) ;
#87258 = DIRECTION('ref_axis',(-9.42995735618098E-12,0.707106781186669,-0.707106781186426)) ;
#87259 = DIRECTION('center_axis',(-5.42101086242752E-16,1.,0.)) ;
#87260 = DIRECTION('ref_axis',(1.,5.42101086242752E-16,0.)) ;
#87261 = DIRECTION('',(-2.16840434497101E-16,1.,-1.30104260698261E-16)) ;
#87262 = DIRECTION('center_axis',(0.,1.,0.)) ;
#87263 = DIRECTION('ref_axis',(0.,0.,1.)) ;
#87264 = DIRECTION('',(2.16840434497101E-16,-1.,1.30104260698261E-16)) ;
#87265 = DIRECTION('',(2.16840434497101E-16,-1.,1.30104260698261E-16)) ;
#87266 = DIRECTION('center_axis',(1.,0.,0.)) ;
#87267 = DIRECTION('ref_axis',(0.,0.,-1.)) ;
#87268 = DIRECTION('center_axis',(1.,0.,0.)) ;
#87269 = DIRECTION('ref_axis',(0.,0.,-1.)) ;
#87270 = DIRECTION('center_axis',(0.,-1.,-1.22464679914735E-16)) ;
#87271 = DIRECTION('ref_axis',(0.,-1.22464679914735E-16,1.)) ;
#87272 = DIRECTION('center_axis',(-1.,0.,0.)) ;
#87273 = DIRECTION('ref_axis',(0.,0.,-1.)) ;
#87274 = DIRECTION('center_axis',(-1.,0.,0.)) ;
#87275 = DIRECTION('ref_axis',(0.,0.,-1.)) ;
#87276 = DIRECTION('center_axis',(1.,0.,0.)) ;
#87277 = DIRECTION('ref_axis',(0.,0.,-1.)) ;
#87278 = DIRECTION('center_axis',(-1.,0.,0.)) ;
#87279 = DIRECTION('ref_axis',(0.,0.,-1.)) ;
#87280 = DIRECTION('center_axis',(0.,0.,1.)) ;
#87281 = DIRECTION('ref_axis',(1.,0.,0.)) ;
#87282 = DIRECTION('center_axis',(1.,0.,0.)) ;
#87283 = DIRECTION('ref_axis',(0.,0.,-1.)) ;
#87284 = DIRECTION('center_axis',(0.,0.707106781186548,-0.707106781186548)) ;
#87285 = DIRECTION('ref_axis',(0.,0.707106781186548,0.707106781186548)) ;
#87286 = DIRECTION('center_axis',(1.,0.,0.)) ;
#87287 = DIRECTION('ref_axis',(0.,0.,-1.)) ;
#87288 = DIRECTION('center_axis',(-1.,0.,0.)) ;
#87289 = DIRECTION('ref_axis',(0.,0.,-1.)) ;
#87290 = DIRECTION('center_axis',(0.,0.,1.)) ;
#87291 = DIRECTION('ref_axis',(1.,0.,0.)) ;
#87292 = DIRECTION('center_axis',(1.,0.,0.)) ;
#87293 = DIRECTION('ref_axis',(0.,0.,-1.)) ;
#87294 = DIRECTION('center_axis',(0.,0.707106781186548,-0.707106781186548)) ;
#87295 = DIRECTION('ref_axis',(0.,0.707106781186548,0.707106781186548)) ;
#87296 = DIRECTION('center_axis',(1.,0.,0.)) ;
#87297 = DIRECTION('ref_axis',(0.,0.,-1.)) ;
#87298 = DIRECTION('center_axis',(-1.,0.,0.)) ;
#87299 = DIRECTION('ref_axis',(0.,0.,-1.)) ;
#87300 = DIRECTION('center_axis',(0.,0.,1.)) ;
#87301 = DIRECTION('ref_axis',(1.,0.,0.)) ;
#87302 = DIRECTION('center_axis',(1.,0.,0.)) ;
#87303 = DIRECTION('ref_axis',(0.,0.,-1.)) ;
#87304 = DIRECTION('center_axis',(0.,0.707106781186548,-0.707106781186548)) ;
#87305 = DIRECTION('ref_axis',(0.,0.707106781186548,0.707106781186548)) ;
#87306 = DIRECTION('center_axis',(1.,0.,0.)) ;
#87307 = DIRECTION('ref_axis',(0.,0.,-1.)) ;
#87308 = DIRECTION('center_axis',(-1.,0.,0.)) ;
#87309 = DIRECTION('ref_axis',(0.,0.,-1.)) ;
#87310 = DIRECTION('center_axis',(0.,0.,1.)) ;
#87311 = DIRECTION('ref_axis',(1.,0.,0.)) ;
#87312 = DIRECTION('center_axis',(1.,0.,0.)) ;
#87313 = DIRECTION('ref_axis',(0.,0.,-1.)) ;
#87314 = DIRECTION('center_axis',(0.,0.707106781186539,-0.707106781186556)) ;
#87315 = DIRECTION('ref_axis',(0.,0.707106781186556,0.707106781186539)) ;
#87316 = DIRECTION('center_axis',(1.,0.,0.)) ;
#87317 = DIRECTION('ref_axis',(0.,0.,-1.)) ;
#87318 = DIRECTION('center_axis',(-1.,0.,0.)) ;
#87319 = DIRECTION('ref_axis',(0.,0.,-1.)) ;
#87320 = DIRECTION('center_axis',(0.,0.,1.)) ;
#87321 = DIRECTION('ref_axis',(1.,0.,0.)) ;
#87322 = DIRECTION('center_axis',(1.,0.,0.)) ;
#87323 = DIRECTION('ref_axis',(0.,0.,-1.)) ;
#87324 = DIRECTION('center_axis',(0.,0.707106781186539,-0.707106781186556)) ;
#87325 = DIRECTION('ref_axis',(0.,0.707106781186556,0.707106781186539)) ;
#87326 = DIRECTION('center_axis',(1.,0.,0.)) ;
#87327 = DIRECTION('ref_axis',(0.,0.,-1.)) ;
#87328 = DIRECTION('center_axis',(-1.,0.,0.)) ;
#87329 = DIRECTION('ref_axis',(0.,0.,-1.)) ;
#87330 = DIRECTION('center_axis',(0.,0.,1.)) ;
#87331 = DIRECTION('ref_axis',(1.,0.,0.)) ;
#87332 = DIRECTION('center_axis',(1.,0.,0.)) ;
#87333 = DIRECTION('ref_axis',(0.,0.,-1.)) ;
#87334 = DIRECTION('center_axis',(0.,0.707106781186539,-0.707106781186556)) ;
#87335 = DIRECTION('ref_axis',(0.,0.707106781186556,0.707106781186539)) ;
#87336 = DIRECTION('center_axis',(1.,0.,0.)) ;
#87337 = DIRECTION('ref_axis',(0.,0.,-1.)) ;
#87338 = DIRECTION('center_axis',(-1.,0.,0.)) ;
#87339 = DIRECTION('ref_axis',(0.,0.,-1.)) ;
#87340 = DIRECTION('center_axis',(0.,0.,1.)) ;
#87341 = DIRECTION('ref_axis',(1.,0.,0.)) ;
#87342 = DIRECTION('center_axis',(1.,0.,0.)) ;
#87343 = DIRECTION('ref_axis',(0.,0.,-1.)) ;
#87344 = DIRECTION('center_axis',(0.,0.707106781186539,-0.707106781186556)) ;
#87345 = DIRECTION('ref_axis',(0.,0.707106781186556,0.707106781186539)) ;
#87346 = DIRECTION('center_axis',(1.,0.,0.)) ;
#87347 = DIRECTION('ref_axis',(0.,0.,-1.)) ;
#87348 = DIRECTION('center_axis',(-1.,0.,0.)) ;
#87349 = DIRECTION('ref_axis',(0.,0.,-1.)) ;
#87350 = DIRECTION('center_axis',(0.,0.,1.)) ;
#87351 = DIRECTION('ref_axis',(1.,0.,0.)) ;
#87352 = DIRECTION('center_axis',(1.,0.,0.)) ;
#87353 = DIRECTION('ref_axis',(0.,0.,-1.)) ;
#87354 = DIRECTION('center_axis',(-6.13317366673346E-15,0.707106781186539,
-0.707106781186556)) ;
#87355 = DIRECTION('ref_axis',(3.80912633391397E-29,0.707106781186556,0.707106781186539)) ;
#87356 = DIRECTION('center_axis',(1.,0.,0.)) ;
#87357 = DIRECTION('ref_axis',(0.,0.,-1.)) ;
#87358 = DIRECTION('center_axis',(-1.,0.,0.)) ;
#87359 = DIRECTION('ref_axis',(0.,0.,-1.)) ;
#87360 = DIRECTION('center_axis',(0.,0.,1.)) ;
#87361 = DIRECTION('ref_axis',(1.,0.,0.)) ;
#87362 = DIRECTION('center_axis',(1.,0.,0.)) ;
#87363 = DIRECTION('ref_axis',(0.,0.,-1.)) ;
#87364 = DIRECTION('center_axis',(-6.13317366673346E-15,0.707106781186539,
-0.707106781186556)) ;
#87365 = DIRECTION('ref_axis',(3.80912633391397E-29,0.707106781186556,0.707106781186539)) ;
#87366 = DIRECTION('center_axis',(-1.,0.,0.)) ;
#87367 = DIRECTION('ref_axis',(0.,0.,1.)) ;
#87368 = DIRECTION('center_axis',(-1.,0.,0.)) ;
#87369 = DIRECTION('ref_axis',(0.,0.,1.)) ;
#87370 = DIRECTION('center_axis',(0.,1.,-1.22464679914735E-16)) ;
#87371 = DIRECTION('ref_axis',(0.,-1.22464679914735E-16,-1.)) ;
#87372 = DIRECTION('center_axis',(1.,0.,0.)) ;
#87373 = DIRECTION('ref_axis',(0.,0.,1.)) ;
#87374 = DIRECTION('center_axis',(0.,1.,0.)) ;
#87375 = DIRECTION('ref_axis',(0.,0.,1.)) ;
#87376 = DIRECTION('center_axis',(-1.,0.,0.)) ;
#87377 = DIRECTION('ref_axis',(0.,0.,-1.)) ;
#87378 = DIRECTION('center_axis',(0.,0.70710678118655,0.707106781186545)) ;
#87379 = DIRECTION('ref_axis',(0.,-0.707106781186545,0.70710678118655)) ;
#87380 = DIRECTION('center_axis',(0.,0.,-1.)) ;
#87381 = DIRECTION('ref_axis',(-1.,0.,0.)) ;
#87382 = DIRECTION('center_axis',(2.16840434497101E-16,-1.,1.30104260698261E-16)) ;
#87383 = DIRECTION('ref_axis',(1.,2.16840434497101E-16,-1.09476442525376E-47)) ;
#87384 = DIRECTION('center_axis',(6.64836954154425E-14,-0.707106781186552,
-0.707106781186543)) ;
#87385 = DIRECTION('ref_axis',(-1.70648371771735E-11,0.707106781186543,-0.707106781186552)) ;
#87386 = DIRECTION('center_axis',(-5.42101086242752E-16,1.,0.)) ;
#87387 = DIRECTION('ref_axis',(1.,5.42101086242752E-16,0.)) ;
#87388 = DIRECTION('',(-2.16840434497101E-16,1.,-1.30104260698261E-16)) ;
#87389 = DIRECTION('center_axis',(0.,1.,0.)) ;
#87390 = DIRECTION('ref_axis',(0.,0.,1.)) ;
#87391 = DIRECTION('',(2.16840434497101E-16,-1.,1.30104260698261E-16)) ;
#87392 = DIRECTION('',(2.16840434497101E-16,-1.,1.30104260698261E-16)) ;
#87393 = DIRECTION('center_axis',(-1.,0.,0.)) ;
#87394 = DIRECTION('ref_axis',(0.,0.,1.)) ;
#87395 = DIRECTION('',(1.,0.,0.)) ;
#87396 = DIRECTION('center_axis',(-1.,0.,0.)) ;
#87397 = DIRECTION('ref_axis',(0.,0.,1.)) ;
#87398 = DIRECTION('',(1.,0.,0.)) ;
#87399 = DIRECTION('center_axis',(-1.,0.,0.)) ;
#87400 = DIRECTION('ref_axis',(0.,0.,1.)) ;
#87401 = DIRECTION('',(1.,0.,0.)) ;
#87402 = DIRECTION('center_axis',(-1.,0.,0.)) ;
#87403 = DIRECTION('ref_axis',(0.,0.,1.)) ;
#87404 = DIRECTION('',(1.,0.,0.)) ;
#87405 = DIRECTION('center_axis',(-1.,0.,0.)) ;
#87406 = DIRECTION('ref_axis',(0.,0.,1.)) ;
#87407 = DIRECTION('',(1.,0.,0.)) ;
#87408 = DIRECTION('center_axis',(-1.,0.,0.)) ;
#87409 = DIRECTION('ref_axis',(0.,0.,1.)) ;
#87410 = DIRECTION('',(1.,0.,0.)) ;
#87411 = DIRECTION('center_axis',(-1.,0.,0.)) ;
#87412 = DIRECTION('ref_axis',(0.,0.,1.)) ;
#87413 = DIRECTION('',(1.,0.,0.)) ;
#87414 = DIRECTION('center_axis',(-1.,0.,0.)) ;
#87415 = DIRECTION('ref_axis',(0.,0.,1.)) ;
#87416 = DIRECTION('',(1.,0.,0.)) ;
#87417 = DIRECTION('center_axis',(-1.,0.,0.)) ;
#87418 = DIRECTION('ref_axis',(0.,0.,1.)) ;
#87419 = DIRECTION('',(1.,0.,0.)) ;
#87420 = DIRECTION('center_axis',(1.,0.,0.)) ;
#87421 = DIRECTION('ref_axis',(0.,0.,-1.)) ;
#87422 = DIRECTION('center_axis',(-1.,0.,0.)) ;
#87423 = DIRECTION('ref_axis',(0.,0.,-1.)) ;
#87424 = DIRECTION('',(1.,0.,0.)) ;
#87425 = DIRECTION('',(1.,0.,0.)) ;
#87426 = DIRECTION('center_axis',(1.,0.,0.)) ;
#87427 = DIRECTION('ref_axis',(0.,0.,-1.)) ;
#87428 = DIRECTION('center_axis',(-1.,0.,0.)) ;
#87429 = DIRECTION('ref_axis',(0.,0.,-1.)) ;
#87430 = DIRECTION('',(1.,0.,0.)) ;
#87431 = DIRECTION('',(1.,0.,0.)) ;
#87432 = DIRECTION('center_axis',(1.,0.,0.)) ;
#87433 = DIRECTION('ref_axis',(0.,0.,-1.)) ;
#87434 = DIRECTION('center_axis',(-1.,0.,0.)) ;
#87435 = DIRECTION('ref_axis',(0.,0.,-1.)) ;
#87436 = DIRECTION('',(1.,0.,0.)) ;
#87437 = DIRECTION('',(1.,0.,0.)) ;
#87438 = DIRECTION('center_axis',(1.,0.,0.)) ;
#87439 = DIRECTION('ref_axis',(0.,0.,-1.)) ;
#87440 = DIRECTION('center_axis',(-1.,0.,0.)) ;
#87441 = DIRECTION('ref_axis',(0.,0.,-1.)) ;
#87442 = DIRECTION('',(1.,0.,0.)) ;
#87443 = DIRECTION('',(1.,0.,0.)) ;
#87444 = DIRECTION('center_axis',(1.,0.,0.)) ;
#87445 = DIRECTION('ref_axis',(0.,0.,-1.)) ;
#87446 = DIRECTION('center_axis',(-1.,0.,0.)) ;
#87447 = DIRECTION('ref_axis',(0.,0.,-1.)) ;
#87448 = DIRECTION('',(1.,0.,0.)) ;
#87449 = DIRECTION('',(1.,0.,0.)) ;
#87450 = DIRECTION('center_axis',(1.,0.,0.)) ;
#87451 = DIRECTION('ref_axis',(0.,0.,-1.)) ;
#87452 = DIRECTION('center_axis',(-1.,0.,0.)) ;
#87453 = DIRECTION('ref_axis',(0.,0.,-1.)) ;
#87454 = DIRECTION('',(1.,0.,0.)) ;
#87455 = DIRECTION('',(1.,0.,0.)) ;
#87456 = DIRECTION('center_axis',(1.,0.,0.)) ;
#87457 = DIRECTION('ref_axis',(0.,0.,-1.)) ;
#87458 = DIRECTION('center_axis',(-1.,0.,0.)) ;
#87459 = DIRECTION('ref_axis',(0.,0.,-1.)) ;
#87460 = DIRECTION('',(1.,0.,0.)) ;
#87461 = DIRECTION('',(1.,0.,0.)) ;
#87462 = DIRECTION('center_axis',(1.,0.,0.)) ;
#87463 = DIRECTION('ref_axis',(0.,0.,-1.)) ;
#87464 = DIRECTION('center_axis',(-1.,0.,0.)) ;
#87465 = DIRECTION('ref_axis',(0.,0.,-1.)) ;
#87466 = DIRECTION('',(1.,0.,0.)) ;
#87467 = DIRECTION('',(1.,0.,0.)) ;
#87468 = DIRECTION('center_axis',(1.,0.,0.)) ;
#87469 = DIRECTION('ref_axis',(0.,0.,-1.)) ;
#87470 = DIRECTION('center_axis',(-1.,0.,0.)) ;
#87471 = DIRECTION('ref_axis',(0.,0.,-1.)) ;
#87472 = DIRECTION('',(1.,0.,0.)) ;
#87473 = DIRECTION('',(1.,0.,0.)) ;
#87474 = DIRECTION('center_axis',(1.,0.,0.)) ;
#87475 = DIRECTION('ref_axis',(0.,0.,-1.)) ;
#87476 = DIRECTION('center_axis',(1.,0.,0.)) ;
#87477 = DIRECTION('ref_axis',(0.,0.,-1.)) ;
#87478 = DIRECTION('center_axis',(0.,-1.,-1.22464679914735E-16)) ;
#87479 = DIRECTION('ref_axis',(0.,-1.22464679914735E-16,1.)) ;
#87480 = DIRECTION('center_axis',(-1.,0.,0.)) ;
#87481 = DIRECTION('ref_axis',(0.,0.,-1.)) ;
#87482 = DIRECTION('center_axis',(-1.,0.,0.)) ;
#87483 = DIRECTION('ref_axis',(0.,0.,-1.)) ;
#87484 = DIRECTION('center_axis',(1.,0.,0.)) ;
#87485 = DIRECTION('ref_axis',(0.,0.,-1.)) ;
#87486 = DIRECTION('center_axis',(-1.,0.,0.)) ;
#87487 = DIRECTION('ref_axis',(0.,0.,-1.)) ;
#87488 = DIRECTION('center_axis',(0.,0.,1.)) ;
#87489 = DIRECTION('ref_axis',(1.,0.,0.)) ;
#87490 = DIRECTION('center_axis',(1.,0.,0.)) ;
#87491 = DIRECTION('ref_axis',(0.,0.,-1.)) ;
#87492 = DIRECTION('center_axis',(0.,0.707106781186548,-0.707106781186548)) ;
#87493 = DIRECTION('ref_axis',(0.,0.707106781186548,0.707106781186548)) ;
#87494 = DIRECTION('center_axis',(-1.,0.,0.)) ;
#87495 = DIRECTION('ref_axis',(0.,0.,1.)) ;
#87496 = DIRECTION('center_axis',(-1.,0.,0.)) ;
#87497 = DIRECTION('ref_axis',(0.,0.,1.)) ;
#87498 = DIRECTION('center_axis',(0.,1.,-1.22464679914735E-16)) ;
#87499 = DIRECTION('ref_axis',(0.,-1.22464679914735E-16,-1.)) ;
#87500 = DIRECTION('center_axis',(1.,0.,0.)) ;
#87501 = DIRECTION('ref_axis',(0.,0.,1.)) ;
#87502 = DIRECTION('center_axis',(0.,1.,0.)) ;
#87503 = DIRECTION('ref_axis',(0.,0.,1.)) ;
#87504 = DIRECTION('center_axis',(-1.,0.,0.)) ;
#87505 = DIRECTION('ref_axis',(0.,0.,-1.)) ;
#87506 = DIRECTION('center_axis',(0.,0.70710678118655,0.707106781186545)) ;
#87507 = DIRECTION('ref_axis',(0.,-0.707106781186545,0.70710678118655)) ;
#87508 = DIRECTION('center_axis',(0.,0.,-1.)) ;
#87509 = DIRECTION('ref_axis',(-1.,0.,0.)) ;
#87510 = DIRECTION('center_axis',(2.16840434497101E-16,-1.,1.30104260698261E-16)) ;
#87511 = DIRECTION('ref_axis',(1.,2.16840434497101E-16,-1.09476442525376E-47)) ;
#87512 = DIRECTION('center_axis',(-1.95540280633655E-15,-0.707106781186549,
-0.707106781186546)) ;
#87513 = DIRECTION('ref_axis',(-2.18299406319968E-11,0.707106781186546,-0.707106781186549)) ;
#87514 = DIRECTION('center_axis',(-5.42101086242752E-16,1.,0.)) ;
#87515 = DIRECTION('ref_axis',(1.,5.42101086242752E-16,0.)) ;
#87516 = DIRECTION('',(-2.16840434497101E-16,1.,-1.30104260698261E-16)) ;
#87517 = DIRECTION('center_axis',(0.,1.,0.)) ;
#87518 = DIRECTION('ref_axis',(0.,0.,1.)) ;
#87519 = DIRECTION('',(2.16840434497101E-16,-1.,1.30104260698261E-16)) ;
#87520 = DIRECTION('',(2.16840434497101E-16,-1.,1.30104260698261E-16)) ;
#87521 = DIRECTION('center_axis',(-1.,0.,0.)) ;
#87522 = DIRECTION('ref_axis',(0.,0.,1.)) ;
#87523 = DIRECTION('',(1.,0.,0.)) ;
#87524 = DIRECTION('center_axis',(1.,0.,0.)) ;
#87525 = DIRECTION('ref_axis',(0.,0.,-1.)) ;
#87526 = DIRECTION('center_axis',(-1.,0.,0.)) ;
#87527 = DIRECTION('ref_axis',(0.,0.,-1.)) ;
#87528 = DIRECTION('',(1.,0.,0.)) ;
#87529 = DIRECTION('',(1.,0.,0.)) ;
#87530 = DIRECTION('center_axis',(-1.,-2.16840434497101E-16,0.)) ;
#87531 = DIRECTION('ref_axis',(2.16840434497101E-16,-1.,0.)) ;
#87532 = DIRECTION('',(-2.16840434497101E-16,1.,1.30104260698261E-16)) ;
#87533 = DIRECTION('center_axis',(1.,2.16840434497101E-16,0.)) ;
#87534 = DIRECTION('ref_axis',(2.16840434497101E-16,-1.,0.)) ;
#87535 = DIRECTION('',(0.,0.,-1.)) ;
#87536 = DIRECTION('center_axis',(1.,2.16840434497101E-16,0.)) ;
#87537 = DIRECTION('ref_axis',(2.16840434497101E-16,-1.,0.)) ;
#87538 = DIRECTION('center_axis',(-1.,-2.16840434497101E-16,0.)) ;
#87539 = DIRECTION('ref_axis',(2.16840434497101E-16,-1.,0.)) ;
#87540 = DIRECTION('',(0.,0.,-1.)) ;
#87541 = DIRECTION('',(2.16840434497101E-16,-1.,5.10212787052002E-17)) ;
#87542 = DIRECTION('',(0.,0.,1.)) ;
#87543 = DIRECTION('',(-2.16840434497101E-16,1.,-1.020425574104E-16)) ;
#87544 = DIRECTION('',(0.,0.,-1.)) ;
#87545 = DIRECTION('center_axis',(-1.,-2.16840434497101E-16,0.)) ;
#87546 = DIRECTION('ref_axis',(2.16840434497101E-16,-1.,0.)) ;
#87547 = DIRECTION('center_axis',(-1.,-2.16840434497101E-16,0.)) ;
#87548 = DIRECTION('ref_axis',(2.16840434497101E-16,-1.,0.)) ;
#87549 = DIRECTION('',(-2.16840434497101E-16,1.,1.30104260698261E-16)) ;
#87550 = DIRECTION('center_axis',(1.,2.16840434497101E-16,0.)) ;
#87551 = DIRECTION('ref_axis',(2.16840434497101E-16,-1.,0.)) ;
#87552 = DIRECTION('',(0.,0.,-1.)) ;
#87553 = DIRECTION('center_axis',(1.,2.16840434497101E-16,0.)) ;
#87554 = DIRECTION('ref_axis',(2.16840434497101E-16,-1.,0.)) ;
#87555 = DIRECTION('center_axis',(-1.,-2.16840434497101E-16,0.)) ;
#87556 = DIRECTION('ref_axis',(2.16840434497101E-16,-1.,0.)) ;
#87557 = DIRECTION('',(0.,0.,-1.)) ;
#87558 = DIRECTION('',(2.16840434497101E-16,-1.,5.10212787052002E-17)) ;
#87559 = DIRECTION('',(0.,0.,1.)) ;
#87560 = DIRECTION('',(-2.16840434497101E-16,1.,-1.020425574104E-16)) ;
#87561 = DIRECTION('',(0.,0.,-1.)) ;
#87562 = DIRECTION('center_axis',(-1.,-2.16840434497101E-16,0.)) ;
#87563 = DIRECTION('ref_axis',(2.16840434497101E-16,-1.,0.)) ;
#87564 = DIRECTION('center_axis',(-1.,-2.16840434497101E-16,0.)) ;
#87565 = DIRECTION('ref_axis',(2.16840434497101E-16,-1.,0.)) ;
#87566 = DIRECTION('',(-2.16840434497101E-16,1.,1.30104260698261E-16)) ;
#87567 = DIRECTION('center_axis',(1.,2.16840434497101E-16,0.)) ;
#87568 = DIRECTION('ref_axis',(2.16840434497101E-16,-1.,0.)) ;
#87569 = DIRECTION('',(0.,0.,-1.)) ;
#87570 = DIRECTION('center_axis',(1.,2.16840434497101E-16,0.)) ;
#87571 = DIRECTION('ref_axis',(2.16840434497101E-16,-1.,0.)) ;
#87572 = DIRECTION('center_axis',(-1.,-2.16840434497101E-16,0.)) ;
#87573 = DIRECTION('ref_axis',(2.16840434497101E-16,-1.,0.)) ;
#87574 = DIRECTION('',(0.,0.,-1.)) ;
#87575 = DIRECTION('',(2.16840434497101E-16,-1.,5.10212787052002E-17)) ;
#87576 = DIRECTION('',(0.,0.,1.)) ;
#87577 = DIRECTION('',(-2.16840434497101E-16,1.,-1.020425574104E-16)) ;
#87578 = DIRECTION('',(0.,0.,-1.)) ;
#87579 = DIRECTION('center_axis',(-1.,-2.16840434497101E-16,0.)) ;
#87580 = DIRECTION('ref_axis',(2.16840434497101E-16,-1.,0.)) ;
#87581 = DIRECTION('center_axis',(-1.,-2.16840434497101E-16,0.)) ;
#87582 = DIRECTION('ref_axis',(2.16840434497101E-16,-1.,0.)) ;
#87583 = DIRECTION('',(-2.16840434497101E-16,1.,1.30104260698261E-16)) ;
#87584 = DIRECTION('center_axis',(1.,2.16840434497101E-16,0.)) ;
#87585 = DIRECTION('ref_axis',(2.16840434497101E-16,-1.,0.)) ;
#87586 = DIRECTION('',(0.,0.,-1.)) ;
#87587 = DIRECTION('center_axis',(1.,2.16840434497101E-16,0.)) ;
#87588 = DIRECTION('ref_axis',(2.16840434497101E-16,-1.,0.)) ;
#87589 = DIRECTION('center_axis',(-1.,-2.16840434497101E-16,0.)) ;
#87590 = DIRECTION('ref_axis',(2.16840434497101E-16,-1.,0.)) ;
#87591 = DIRECTION('',(0.,0.,-1.)) ;
#87592 = DIRECTION('',(2.16840434497101E-16,-1.,5.10212787052002E-17)) ;
#87593 = DIRECTION('',(0.,0.,1.)) ;
#87594 = DIRECTION('',(-2.16840434497101E-16,1.,-1.020425574104E-16)) ;
#87595 = DIRECTION('',(0.,0.,-1.)) ;
#87596 = DIRECTION('center_axis',(-1.,-2.16840434497101E-16,0.)) ;
#87597 = DIRECTION('ref_axis',(2.16840434497101E-16,-1.,0.)) ;
#87598 = DIRECTION('center_axis',(-1.,-2.16840434497101E-16,0.)) ;
#87599 = DIRECTION('ref_axis',(2.16840434497101E-16,-1.,0.)) ;
#87600 = DIRECTION('',(-2.16840434497101E-16,1.,1.30104260698261E-16)) ;
#87601 = DIRECTION('center_axis',(1.,2.16840434497101E-16,0.)) ;
#87602 = DIRECTION('ref_axis',(2.16840434497101E-16,-1.,0.)) ;
#87603 = DIRECTION('',(0.,0.,-1.)) ;
#87604 = DIRECTION('center_axis',(1.,2.16840434497101E-16,0.)) ;
#87605 = DIRECTION('ref_axis',(2.16840434497101E-16,-1.,0.)) ;
#87606 = DIRECTION('center_axis',(-1.,-2.16840434497101E-16,0.)) ;
#87607 = DIRECTION('ref_axis',(2.16840434497101E-16,-1.,0.)) ;
#87608 = DIRECTION('',(0.,0.,-1.)) ;
#87609 = DIRECTION('',(2.16840434497101E-16,-1.,5.10212787052002E-17)) ;
#87610 = DIRECTION('',(0.,0.,1.)) ;
#87611 = DIRECTION('',(-2.16840434497101E-16,1.,-1.020425574104E-16)) ;
#87612 = DIRECTION('',(0.,0.,-1.)) ;
#87613 = DIRECTION('center_axis',(-1.,-2.16840434497101E-16,0.)) ;
#87614 = DIRECTION('ref_axis',(2.16840434497101E-16,-1.,0.)) ;
#87615 = DIRECTION('center_axis',(-1.,-2.16840434497101E-16,0.)) ;
#87616 = DIRECTION('ref_axis',(2.16840434497101E-16,-1.,0.)) ;
#87617 = DIRECTION('',(-2.16840434497101E-16,1.,1.30104260698261E-16)) ;
#87618 = DIRECTION('center_axis',(1.,2.16840434497101E-16,0.)) ;
#87619 = DIRECTION('ref_axis',(2.16840434497101E-16,-1.,0.)) ;
#87620 = DIRECTION('',(0.,0.,-1.)) ;
#87621 = DIRECTION('center_axis',(1.,2.16840434497101E-16,0.)) ;
#87622 = DIRECTION('ref_axis',(2.16840434497101E-16,-1.,0.)) ;
#87623 = DIRECTION('center_axis',(-1.,-2.16840434497101E-16,0.)) ;
#87624 = DIRECTION('ref_axis',(2.16840434497101E-16,-1.,0.)) ;
#87625 = DIRECTION('',(0.,0.,-1.)) ;
#87626 = DIRECTION('',(2.16840434497101E-16,-1.,5.10212787052002E-17)) ;
#87627 = DIRECTION('',(0.,0.,1.)) ;
#87628 = DIRECTION('',(-2.16840434497101E-16,1.,-1.020425574104E-16)) ;
#87629 = DIRECTION('',(0.,0.,-1.)) ;
#87630 = DIRECTION('center_axis',(-1.,-2.16840434497101E-16,0.)) ;
#87631 = DIRECTION('ref_axis',(2.16840434497101E-16,-1.,0.)) ;
#87632 = DIRECTION('center_axis',(-1.,-2.16840434497101E-16,0.)) ;
#87633 = DIRECTION('ref_axis',(2.16840434497101E-16,-1.,0.)) ;
#87634 = DIRECTION('',(-2.16840434497101E-16,1.,1.30104260698261E-16)) ;
#87635 = DIRECTION('center_axis',(1.,2.16840434497101E-16,0.)) ;
#87636 = DIRECTION('ref_axis',(2.16840434497101E-16,-1.,0.)) ;
#87637 = DIRECTION('',(0.,0.,-1.)) ;
#87638 = DIRECTION('center_axis',(1.,2.16840434497101E-16,0.)) ;
#87639 = DIRECTION('ref_axis',(2.16840434497101E-16,-1.,0.)) ;
#87640 = DIRECTION('center_axis',(-1.,-2.16840434497101E-16,0.)) ;
#87641 = DIRECTION('ref_axis',(2.16840434497101E-16,-1.,0.)) ;
#87642 = DIRECTION('',(0.,0.,-1.)) ;
#87643 = DIRECTION('',(2.16840434497101E-16,-1.,5.10212787052002E-17)) ;
#87644 = DIRECTION('',(0.,0.,1.)) ;
#87645 = DIRECTION('',(-2.16840434497101E-16,1.,-1.020425574104E-16)) ;
#87646 = DIRECTION('',(0.,0.,-1.)) ;
#87647 = DIRECTION('center_axis',(-1.,-2.16840434497101E-16,0.)) ;
#87648 = DIRECTION('ref_axis',(2.16840434497101E-16,-1.,0.)) ;
#87649 = DIRECTION('center_axis',(-1.,-2.16840434497101E-16,0.)) ;
#87650 = DIRECTION('ref_axis',(2.16840434497101E-16,-1.,0.)) ;
#87651 = DIRECTION('',(-2.16840434497101E-16,1.,1.30104260698261E-16)) ;
#87652 = DIRECTION('center_axis',(1.,2.16840434497101E-16,0.)) ;
#87653 = DIRECTION('ref_axis',(2.16840434497101E-16,-1.,0.)) ;
#87654 = DIRECTION('',(0.,0.,-1.)) ;
#87655 = DIRECTION('center_axis',(1.,2.16840434497101E-16,0.)) ;
#87656 = DIRECTION('ref_axis',(2.16840434497101E-16,-1.,0.)) ;
#87657 = DIRECTION('center_axis',(-1.,-2.16840434497101E-16,0.)) ;
#87658 = DIRECTION('ref_axis',(2.16840434497101E-16,-1.,0.)) ;
#87659 = DIRECTION('',(0.,0.,-1.)) ;
#87660 = DIRECTION('',(2.16840434497101E-16,-1.,5.10212787052002E-17)) ;
#87661 = DIRECTION('',(0.,0.,1.)) ;
#87662 = DIRECTION('',(-2.16840434497101E-16,1.,-1.020425574104E-16)) ;
#87663 = DIRECTION('',(0.,0.,-1.)) ;
#87664 = DIRECTION('center_axis',(-1.,-2.16840434497101E-16,0.)) ;
#87665 = DIRECTION('ref_axis',(2.16840434497101E-16,-1.,0.)) ;
#87666 = DIRECTION('center_axis',(-1.,-2.16840434497101E-16,0.)) ;
#87667 = DIRECTION('ref_axis',(2.16840434497101E-16,-1.,0.)) ;
#87668 = DIRECTION('',(-2.16840434497101E-16,1.,1.30104260698261E-16)) ;
#87669 = DIRECTION('center_axis',(1.,2.16840434497101E-16,0.)) ;
#87670 = DIRECTION('ref_axis',(2.16840434497101E-16,-1.,0.)) ;
#87671 = DIRECTION('',(0.,0.,-1.)) ;
#87672 = DIRECTION('center_axis',(1.,2.16840434497101E-16,0.)) ;
#87673 = DIRECTION('ref_axis',(2.16840434497101E-16,-1.,0.)) ;
#87674 = DIRECTION('center_axis',(-1.,-2.16840434497101E-16,0.)) ;
#87675 = DIRECTION('ref_axis',(2.16840434497101E-16,-1.,0.)) ;
#87676 = DIRECTION('',(0.,0.,-1.)) ;
#87677 = DIRECTION('',(2.16840434497101E-16,-1.,5.10212787052002E-17)) ;
#87678 = DIRECTION('',(0.,0.,1.)) ;
#87679 = DIRECTION('',(-2.16840434497101E-16,1.,-1.020425574104E-16)) ;
#87680 = DIRECTION('',(0.,0.,-1.)) ;
#87681 = DIRECTION('center_axis',(-1.,-2.16840434497101E-16,0.)) ;
#87682 = DIRECTION('ref_axis',(2.16840434497101E-16,-1.,0.)) ;
#87683 = DIRECTION('center_axis',(6.27714964143733E-33,-5.10212787052002E-17,
-1.)) ;
#87684 = DIRECTION('ref_axis',(0.,1.,-5.10212787052002E-17)) ;
#87685 = DIRECTION('center_axis',(-6.27714964143733E-33,5.10212787052002E-17,
1.)) ;
#87686 = DIRECTION('ref_axis',(3.20268201330022E-49,1.,-5.10212787052002E-17)) ;
#87687 = DIRECTION('',(1.2303003375722E-16,-1.,5.10212787052002E-17)) ;
#87688 = DIRECTION('',(1.,0.,6.27714964143733E-33)) ;
#87689 = DIRECTION('',(-2.16840434497101E-16,1.,-5.10212787052002E-17)) ;
#87690 = DIRECTION('',(-1.,-1.53063836115601E-16,1.53236300070382E-33)) ;
#87691 = DIRECTION('center_axis',(-1.25542992828747E-32,1.020425574104E-16,
1.)) ;
#87692 = DIRECTION('ref_axis',(0.,-1.,1.020425574104E-16)) ;
#87693 = DIRECTION('center_axis',(1.25542992828747E-32,-1.020425574104E-16,
-1.)) ;
#87694 = DIRECTION('ref_axis',(-1.28107280532009E-48,-1.,1.020425574104E-16)) ;
#87695 = DIRECTION('',(1.,1.53063836115601E-16,-3.06472600140763E-33)) ;
#87696 = DIRECTION('',(2.16840434497101E-16,-1.,1.020425574104E-16)) ;
#87697 = DIRECTION('',(-1.,0.,-1.25542992828747E-32)) ;
#87698 = DIRECTION('',(-1.2303003375722E-16,1.,-1.020425574104E-16)) ;
#87699 = DIRECTION('center_axis',(6.27714964143733E-33,-5.10212787052002E-17,
-1.)) ;
#87700 = DIRECTION('ref_axis',(0.,1.,-5.10212787052002E-17)) ;
#87701 = DIRECTION('center_axis',(-6.27714964143733E-33,5.10212787052002E-17,
1.)) ;
#87702 = DIRECTION('ref_axis',(3.20268201330022E-49,1.,-5.10212787052002E-17)) ;
#87703 = DIRECTION('',(1.2303003375722E-16,-1.,5.10212787052002E-17)) ;
#87704 = DIRECTION('',(1.,0.,6.27714964143733E-33)) ;
#87705 = DIRECTION('',(-2.16840434497101E-16,1.,-5.10212787052002E-17)) ;
#87706 = DIRECTION('',(-1.,-1.53063836115601E-16,1.53236300070382E-33)) ;
#87707 = DIRECTION('center_axis',(-1.25542992828747E-32,1.020425574104E-16,
1.)) ;
#87708 = DIRECTION('ref_axis',(0.,-1.,1.020425574104E-16)) ;
#87709 = DIRECTION('center_axis',(1.25542992828747E-32,-1.020425574104E-16,
-1.)) ;
#87710 = DIRECTION('ref_axis',(-1.28107280532009E-48,-1.,1.020425574104E-16)) ;
#87711 = DIRECTION('',(1.,1.53063836115601E-16,-3.06472600140763E-33)) ;
#87712 = DIRECTION('',(2.16840434497101E-16,-1.,1.020425574104E-16)) ;
#87713 = DIRECTION('',(-1.,0.,-1.25542992828747E-32)) ;
#87714 = DIRECTION('',(-1.2303003375722E-16,1.,-1.020425574104E-16)) ;
#87715 = DIRECTION('center_axis',(6.27714964143733E-33,-5.10212787052002E-17,
-1.)) ;
#87716 = DIRECTION('ref_axis',(0.,1.,-5.10212787052002E-17)) ;
#87717 = DIRECTION('center_axis',(-6.27714964143733E-33,5.10212787052002E-17,
1.)) ;
#87718 = DIRECTION('ref_axis',(3.20268201330022E-49,1.,-5.10212787052002E-17)) ;
#87719 = DIRECTION('',(1.2303003375722E-16,-1.,5.10212787052002E-17)) ;
#87720 = DIRECTION('',(1.,0.,6.27714964143733E-33)) ;
#87721 = DIRECTION('',(-2.16840434497101E-16,1.,-5.10212787052002E-17)) ;
#87722 = DIRECTION('',(-1.,-1.53063836115601E-16,1.53236300070382E-33)) ;
#87723 = DIRECTION('center_axis',(-1.25542992828747E-32,1.020425574104E-16,
1.)) ;
#87724 = DIRECTION('ref_axis',(0.,-1.,1.020425574104E-16)) ;
#87725 = DIRECTION('center_axis',(1.25542992828747E-32,-1.020425574104E-16,
-1.)) ;
#87726 = DIRECTION('ref_axis',(-1.28107280532009E-48,-1.,1.020425574104E-16)) ;
#87727 = DIRECTION('',(1.,1.53063836115601E-16,-3.06472600140763E-33)) ;
#87728 = DIRECTION('',(2.16840434497101E-16,-1.,1.020425574104E-16)) ;
#87729 = DIRECTION('',(-1.,0.,-1.25542992828747E-32)) ;
#87730 = DIRECTION('',(-1.2303003375722E-16,1.,-1.020425574104E-16)) ;
#87731 = DIRECTION('center_axis',(6.27714964143733E-33,-5.10212787052002E-17,
-1.)) ;
#87732 = DIRECTION('ref_axis',(0.,1.,-5.10212787052002E-17)) ;
#87733 = DIRECTION('center_axis',(-6.27714964143733E-33,5.10212787052002E-17,
1.)) ;
#87734 = DIRECTION('ref_axis',(3.20268201330022E-49,1.,-5.10212787052002E-17)) ;
#87735 = DIRECTION('',(1.2303003375722E-16,-1.,5.10212787052002E-17)) ;
#87736 = DIRECTION('',(1.,0.,6.27714964143733E-33)) ;
#87737 = DIRECTION('',(-2.16840434497101E-16,1.,-5.10212787052002E-17)) ;
#87738 = DIRECTION('',(-1.,-1.53063836115601E-16,1.53236300070382E-33)) ;
#87739 = DIRECTION('center_axis',(-1.25542992828747E-32,1.020425574104E-16,
1.)) ;
#87740 = DIRECTION('ref_axis',(0.,-1.,1.020425574104E-16)) ;
#87741 = DIRECTION('center_axis',(1.25542992828747E-32,-1.020425574104E-16,
-1.)) ;
#87742 = DIRECTION('ref_axis',(-1.28107280532009E-48,-1.,1.020425574104E-16)) ;
#87743 = DIRECTION('',(1.,1.53063836115601E-16,-3.06472600140763E-33)) ;
#87744 = DIRECTION('',(2.16840434497101E-16,-1.,1.020425574104E-16)) ;
#87745 = DIRECTION('',(-1.,0.,-1.25542992828747E-32)) ;
#87746 = DIRECTION('',(-1.2303003375722E-16,1.,-1.020425574104E-16)) ;
#87747 = DIRECTION('center_axis',(6.27714964143733E-33,-5.10212787052002E-17,
-1.)) ;
#87748 = DIRECTION('ref_axis',(0.,1.,-5.10212787052002E-17)) ;
#87749 = DIRECTION('center_axis',(-6.27714964143733E-33,5.10212787052002E-17,
1.)) ;
#87750 = DIRECTION('ref_axis',(3.20268201330022E-49,1.,-5.10212787052002E-17)) ;
#87751 = DIRECTION('',(1.2303003375722E-16,-1.,5.10212787052002E-17)) ;
#87752 = DIRECTION('',(1.,0.,6.27714964143733E-33)) ;
#87753 = DIRECTION('',(-2.16840434497101E-16,1.,-5.10212787052002E-17)) ;
#87754 = DIRECTION('',(-1.,-1.53063836115601E-16,1.53236300070382E-33)) ;
#87755 = DIRECTION('center_axis',(-1.25542992828747E-32,1.020425574104E-16,
1.)) ;
#87756 = DIRECTION('ref_axis',(0.,-1.,1.020425574104E-16)) ;
#87757 = DIRECTION('center_axis',(1.25542992828747E-32,-1.020425574104E-16,
-1.)) ;
#87758 = DIRECTION('ref_axis',(-1.28107280532009E-48,-1.,1.020425574104E-16)) ;
#87759 = DIRECTION('',(1.,1.53063836115601E-16,-3.06472600140763E-33)) ;
#87760 = DIRECTION('',(2.16840434497101E-16,-1.,1.020425574104E-16)) ;
#87761 = DIRECTION('',(-1.,0.,-1.25542992828747E-32)) ;
#87762 = DIRECTION('',(-1.2303003375722E-16,1.,-1.020425574104E-16)) ;
#87763 = DIRECTION('center_axis',(6.27714964143733E-33,-5.10212787052002E-17,
-1.)) ;
#87764 = DIRECTION('ref_axis',(0.,1.,-5.10212787052002E-17)) ;
#87765 = DIRECTION('center_axis',(-6.27714964143733E-33,5.10212787052002E-17,
1.)) ;
#87766 = DIRECTION('ref_axis',(3.20268201330022E-49,1.,-5.10212787052002E-17)) ;
#87767 = DIRECTION('',(1.2303003375722E-16,-1.,5.10212787052002E-17)) ;
#87768 = DIRECTION('',(1.,0.,6.27714964143733E-33)) ;
#87769 = DIRECTION('',(-2.16840434497101E-16,1.,-5.10212787052002E-17)) ;
#87770 = DIRECTION('',(-1.,-1.53063836115601E-16,1.53236300070382E-33)) ;
#87771 = DIRECTION('center_axis',(-1.25542992828747E-32,1.020425574104E-16,
1.)) ;
#87772 = DIRECTION('ref_axis',(0.,-1.,1.020425574104E-16)) ;
#87773 = DIRECTION('center_axis',(1.25542992828747E-32,-1.020425574104E-16,
-1.)) ;
#87774 = DIRECTION('ref_axis',(-1.28107280532009E-48,-1.,1.020425574104E-16)) ;
#87775 = DIRECTION('',(1.,1.53063836115601E-16,-3.06472600140763E-33)) ;
#87776 = DIRECTION('',(2.16840434497101E-16,-1.,1.020425574104E-16)) ;
#87777 = DIRECTION('',(-1.,0.,-1.25542992828747E-32)) ;
#87778 = DIRECTION('',(-1.2303003375722E-16,1.,-1.020425574104E-16)) ;
#87779 = DIRECTION('center_axis',(6.27714964143733E-33,-5.10212787052002E-17,
-1.)) ;
#87780 = DIRECTION('ref_axis',(0.,1.,-5.10212787052002E-17)) ;
#87781 = DIRECTION('center_axis',(-6.27714964143733E-33,5.10212787052002E-17,
1.)) ;
#87782 = DIRECTION('ref_axis',(3.20268201330022E-49,1.,-5.10212787052002E-17)) ;
#87783 = DIRECTION('',(1.2303003375722E-16,-1.,5.10212787052002E-17)) ;
#87784 = DIRECTION('',(1.,0.,6.27714964143733E-33)) ;
#87785 = DIRECTION('',(-2.16840434497101E-16,1.,-5.10212787052002E-17)) ;
#87786 = DIRECTION('',(-1.,-1.53063836115601E-16,1.53236300070382E-33)) ;
#87787 = DIRECTION('center_axis',(-1.25542992828747E-32,1.020425574104E-16,
1.)) ;
#87788 = DIRECTION('ref_axis',(0.,-1.,1.020425574104E-16)) ;
#87789 = DIRECTION('center_axis',(1.25542992828747E-32,-1.020425574104E-16,
-1.)) ;
#87790 = DIRECTION('ref_axis',(-1.28107280532009E-48,-1.,1.020425574104E-16)) ;
#87791 = DIRECTION('',(1.,1.53063836115601E-16,-3.06472600140763E-33)) ;
#87792 = DIRECTION('',(2.16840434497101E-16,-1.,1.020425574104E-16)) ;
#87793 = DIRECTION('',(-1.,0.,-1.25542992828747E-32)) ;
#87794 = DIRECTION('',(-1.2303003375722E-16,1.,-1.020425574104E-16)) ;
#87795 = DIRECTION('center_axis',(6.27714964143733E-33,-5.10212787052002E-17,
-1.)) ;
#87796 = DIRECTION('ref_axis',(0.,1.,-5.10212787052002E-17)) ;
#87797 = DIRECTION('center_axis',(-6.27714964143733E-33,5.10212787052002E-17,
1.)) ;
#87798 = DIRECTION('ref_axis',(3.20268201330022E-49,1.,-5.10212787052002E-17)) ;
#87799 = DIRECTION('',(1.2303003375722E-16,-1.,5.10212787052002E-17)) ;
#87800 = DIRECTION('',(1.,0.,6.27714964143733E-33)) ;
#87801 = DIRECTION('',(-2.16840434497101E-16,1.,-5.10212787052002E-17)) ;
#87802 = DIRECTION('',(-1.,-1.53063836115601E-16,1.53236300070382E-33)) ;
#87803 = DIRECTION('center_axis',(-1.25542992828747E-32,1.020425574104E-16,
1.)) ;
#87804 = DIRECTION('ref_axis',(0.,-1.,1.020425574104E-16)) ;
#87805 = DIRECTION('center_axis',(1.25542992828747E-32,-1.020425574104E-16,
-1.)) ;
#87806 = DIRECTION('ref_axis',(-1.28107280532009E-48,-1.,1.020425574104E-16)) ;
#87807 = DIRECTION('',(1.,1.53063836115601E-16,-3.06472600140763E-33)) ;
#87808 = DIRECTION('',(2.16840434497101E-16,-1.,1.020425574104E-16)) ;
#87809 = DIRECTION('',(-1.,0.,-1.25542992828747E-32)) ;
#87810 = DIRECTION('',(-1.2303003375722E-16,1.,-1.020425574104E-16)) ;
#87811 = DIRECTION('center_axis',(6.27714964143733E-33,-5.10212787052002E-17,
-1.)) ;
#87812 = DIRECTION('ref_axis',(0.,1.,-5.10212787052002E-17)) ;
#87813 = DIRECTION('center_axis',(-6.27714964143733E-33,5.10212787052002E-17,
1.)) ;
#87814 = DIRECTION('ref_axis',(3.20268201330022E-49,1.,-5.10212787052002E-17)) ;
#87815 = DIRECTION('',(1.2303003375722E-16,-1.,5.10212787052002E-17)) ;
#87816 = DIRECTION('',(1.,0.,6.27714964143733E-33)) ;
#87817 = DIRECTION('',(-2.16840434497101E-16,1.,-5.10212787052002E-17)) ;
#87818 = DIRECTION('',(-1.,-1.53063836115601E-16,1.53236300070382E-33)) ;
#87819 = DIRECTION('center_axis',(-1.25542992828747E-32,1.020425574104E-16,
1.)) ;
#87820 = DIRECTION('ref_axis',(0.,-1.,1.020425574104E-16)) ;
#87821 = DIRECTION('center_axis',(1.25542992828747E-32,-1.020425574104E-16,
-1.)) ;
#87822 = DIRECTION('ref_axis',(-1.28107280532009E-48,-1.,1.020425574104E-16)) ;
#87823 = DIRECTION('',(1.,1.53063836115601E-16,-3.06472600140763E-33)) ;
#87824 = DIRECTION('',(2.16840434497101E-16,-1.,1.020425574104E-16)) ;
#87825 = DIRECTION('',(-1.,0.,-1.25542992828747E-32)) ;
#87826 = DIRECTION('',(-1.2303003375722E-16,1.,-1.020425574104E-16)) ;
#87827 = DIRECTION('center_axis',(0.,0.,1.)) ;
#87828 = DIRECTION('ref_axis',(1.,0.,0.)) ;
#87829 = DIRECTION('',(0.,0.,1.)) ;
#87830 = DIRECTION('center_axis',(0.,0.,1.)) ;
#87831 = DIRECTION('ref_axis',(1.,0.,0.)) ;
#87832 = DIRECTION('',(0.,0.,1.)) ;
#87833 = DIRECTION('center_axis',(0.,0.,-1.)) ;
#87834 = DIRECTION('ref_axis',(1.,0.,0.)) ;
#87835 = DIRECTION('center_axis',(0.,0.,1.)) ;
#87836 = DIRECTION('ref_axis',(1.,0.,0.)) ;
#87837 = DIRECTION('',(0.,0.,1.)) ;
#87838 = DIRECTION('center_axis',(0.,0.,1.)) ;
#87839 = DIRECTION('ref_axis',(1.,0.,0.)) ;
#87840 = DIRECTION('',(0.,0.,1.)) ;
#87841 = DIRECTION('center_axis',(0.,0.,-1.)) ;
#87842 = DIRECTION('ref_axis',(1.,0.,0.)) ;
#87843 = DIRECTION('center_axis',(0.,0.,1.)) ;
#87844 = DIRECTION('ref_axis',(1.,0.,0.)) ;
#87845 = DIRECTION('',(0.,0.,1.)) ;
#87846 = DIRECTION('center_axis',(0.,0.,1.)) ;
#87847 = DIRECTION('ref_axis',(1.,0.,0.)) ;
#87848 = DIRECTION('',(0.,0.,1.)) ;
#87849 = DIRECTION('center_axis',(0.,0.,-1.)) ;
#87850 = DIRECTION('ref_axis',(1.,0.,0.)) ;
#87851 = DIRECTION('center_axis',(0.,0.,1.)) ;
#87852 = DIRECTION('ref_axis',(1.,0.,0.)) ;
#87853 = DIRECTION('',(0.,0.,1.)) ;
#87854 = DIRECTION('center_axis',(0.,0.,1.)) ;
#87855 = DIRECTION('ref_axis',(1.,0.,0.)) ;
#87856 = DIRECTION('',(0.,0.,1.)) ;
#87857 = DIRECTION('center_axis',(0.,0.,-1.)) ;
#87858 = DIRECTION('ref_axis',(1.,0.,0.)) ;
#87859 = DIRECTION('center_axis',(0.,0.,1.)) ;
#87860 = DIRECTION('ref_axis',(1.,0.,0.)) ;
#87861 = DIRECTION('',(0.,0.,1.)) ;
#87862 = DIRECTION('center_axis',(0.,0.,1.)) ;
#87863 = DIRECTION('ref_axis',(1.,0.,0.)) ;
#87864 = DIRECTION('',(0.,0.,1.)) ;
#87865 = DIRECTION('center_axis',(0.,0.,-1.)) ;
#87866 = DIRECTION('ref_axis',(1.,0.,0.)) ;
#87867 = DIRECTION('center_axis',(0.,0.,1.)) ;
#87868 = DIRECTION('ref_axis',(1.,0.,0.)) ;
#87869 = DIRECTION('',(0.,0.,1.)) ;
#87870 = DIRECTION('center_axis',(0.,0.,1.)) ;
#87871 = DIRECTION('ref_axis',(1.,0.,0.)) ;
#87872 = DIRECTION('',(0.,0.,1.)) ;
#87873 = DIRECTION('center_axis',(0.,0.,-1.)) ;
#87874 = DIRECTION('ref_axis',(1.,0.,0.)) ;
#87875 = DIRECTION('center_axis',(0.,0.,1.)) ;
#87876 = DIRECTION('ref_axis',(1.,0.,0.)) ;
#87877 = DIRECTION('',(0.,0.,1.)) ;
#87878 = DIRECTION('center_axis',(0.,0.,1.)) ;
#87879 = DIRECTION('ref_axis',(1.,0.,0.)) ;
#87880 = DIRECTION('',(0.,0.,1.)) ;
#87881 = DIRECTION('center_axis',(0.,0.,-1.)) ;
#87882 = DIRECTION('ref_axis',(1.,0.,0.)) ;
#87883 = DIRECTION('center_axis',(0.,0.,1.)) ;
#87884 = DIRECTION('ref_axis',(1.,0.,0.)) ;
#87885 = DIRECTION('',(0.,0.,1.)) ;
#87886 = DIRECTION('center_axis',(0.,0.,1.)) ;
#87887 = DIRECTION('ref_axis',(1.,0.,0.)) ;
#87888 = DIRECTION('',(0.,0.,1.)) ;
#87889 = DIRECTION('center_axis',(0.,0.,-1.)) ;
#87890 = DIRECTION('ref_axis',(1.,0.,0.)) ;
#87891 = DIRECTION('center_axis',(0.,0.,1.)) ;
#87892 = DIRECTION('ref_axis',(1.,0.,0.)) ;
#87893 = DIRECTION('',(0.,0.,1.)) ;
#87894 = DIRECTION('center_axis',(0.,0.,1.)) ;
#87895 = DIRECTION('ref_axis',(1.,0.,0.)) ;
#87896 = DIRECTION('',(0.,0.,1.)) ;
#87897 = DIRECTION('center_axis',(0.,0.,-1.)) ;
#87898 = DIRECTION('ref_axis',(1.,0.,0.)) ;
#87899 = DIRECTION('center_axis',(-1.,-2.16840434497101E-16,0.)) ;
#87900 = DIRECTION('ref_axis',(2.16840434497101E-16,-1.,0.)) ;
#87901 = DIRECTION('',(-2.16840434497101E-16,1.,1.30104260698261E-16)) ;
#87902 = DIRECTION('center_axis',(1.,2.16840434497101E-16,0.)) ;
#87903 = DIRECTION('ref_axis',(2.16840434497101E-16,-1.,0.)) ;
#87904 = DIRECTION('',(0.,0.,-1.)) ;
#87905 = DIRECTION('center_axis',(1.,2.16840434497101E-16,0.)) ;
#87906 = DIRECTION('ref_axis',(2.16840434497101E-16,-1.,0.)) ;
#87907 = DIRECTION('center_axis',(-1.,-2.16840434497101E-16,0.)) ;
#87908 = DIRECTION('ref_axis',(2.16840434497101E-16,-1.,0.)) ;
#87909 = DIRECTION('',(0.,0.,-1.)) ;
#87910 = DIRECTION('',(2.16840434497101E-16,-1.,5.10212787052002E-17)) ;
#87911 = DIRECTION('',(0.,0.,1.)) ;
#87912 = DIRECTION('',(-2.16840434497101E-16,1.,-1.020425574104E-16)) ;
#87913 = DIRECTION('',(0.,0.,-1.)) ;
#87914 = DIRECTION('center_axis',(-1.,-2.16840434497101E-16,0.)) ;
#87915 = DIRECTION('ref_axis',(2.16840434497101E-16,-1.,0.)) ;
#87916 = DIRECTION('center_axis',(6.27714964143733E-33,-5.10212787052002E-17,
-1.)) ;
#87917 = DIRECTION('ref_axis',(0.,1.,-5.10212787052002E-17)) ;
#87918 = DIRECTION('center_axis',(-6.27714964143733E-33,5.10212787052002E-17,
1.)) ;
#87919 = DIRECTION('ref_axis',(3.20268201330022E-49,1.,-5.10212787052002E-17)) ;
#87920 = DIRECTION('',(1.2303003375722E-16,-1.,5.10212787052002E-17)) ;
#87921 = DIRECTION('',(1.,0.,6.27714964143733E-33)) ;
#87922 = DIRECTION('',(-2.16840434497101E-16,1.,-5.10212787052002E-17)) ;
#87923 = DIRECTION('',(-1.,-1.53063836115601E-16,1.53236300070382E-33)) ;
#87924 = DIRECTION('center_axis',(-1.25542992828747E-32,1.020425574104E-16,
1.)) ;
#87925 = DIRECTION('ref_axis',(0.,-1.,1.020425574104E-16)) ;
#87926 = DIRECTION('center_axis',(1.25542992828747E-32,-1.020425574104E-16,
-1.)) ;
#87927 = DIRECTION('ref_axis',(-1.28107280532009E-48,-1.,1.020425574104E-16)) ;
#87928 = DIRECTION('',(1.,1.53063836115601E-16,-3.06472600140763E-33)) ;
#87929 = DIRECTION('',(2.16840434497101E-16,-1.,1.020425574104E-16)) ;
#87930 = DIRECTION('',(-1.,0.,-1.25542992828747E-32)) ;
#87931 = DIRECTION('',(-1.2303003375722E-16,1.,-1.020425574104E-16)) ;
#87932 = DIRECTION('center_axis',(0.,0.,1.)) ;
#87933 = DIRECTION('ref_axis',(1.,0.,0.)) ;
#87934 = DIRECTION('',(0.,0.,1.)) ;
#87935 = DIRECTION('center_axis',(0.,0.,1.)) ;
#87936 = DIRECTION('ref_axis',(1.,0.,0.)) ;
#87937 = DIRECTION('',(0.,0.,1.)) ;
#87938 = DIRECTION('center_axis',(0.,0.,-1.)) ;
#87939 = DIRECTION('ref_axis',(1.,0.,0.)) ;
#87940 = DIRECTION('center_axis',(0.,0.,1.)) ;
#87941 = DIRECTION('ref_axis',(1.,0.,0.)) ;
#87942 = DIRECTION('',(0.,0.,1.)) ;
#87943 = DIRECTION('center_axis',(0.,0.,1.)) ;
#87944 = DIRECTION('ref_axis',(1.,0.,0.)) ;
#87945 = DIRECTION('',(0.,0.,1.)) ;
#87946 = DIRECTION('center_axis',(0.,0.,-1.)) ;
#87947 = DIRECTION('ref_axis',(1.,0.,0.)) ;
#87948 = DIRECTION('center_axis',(0.,-1.,0.)) ;
#87949 = DIRECTION('ref_axis',(0.,0.,-1.)) ;
#87950 = DIRECTION('center_axis',(0.,-1.,0.)) ;
#87951 = DIRECTION('ref_axis',(0.,0.,-1.)) ;
#87952 = DIRECTION('',(-1.,0.,-6.27714964143733E-33)) ;
#87953 = DIRECTION('',(0.,0.,1.)) ;
#87954 = DIRECTION('',(1.,0.,0.)) ;
#87955 = DIRECTION('',(-1.,0.,0.)) ;
#87956 = DIRECTION('',(1.,0.,1.25542992828747E-32)) ;
#87957 = DIRECTION('center_axis',(0.,-1.,0.)) ;
#87958 = DIRECTION('ref_axis',(0.,0.,-1.)) ;
#87959 = DIRECTION('',(0.,0.,-1.)) ;
#87960 = DIRECTION('center_axis',(0.,-1.,0.)) ;
#87961 = DIRECTION('ref_axis',(0.,0.,-1.)) ;
#87962 = DIRECTION('',(-1.,0.,-6.27714964143733E-33)) ;
#87963 = DIRECTION('',(1.,0.,1.25542992828747E-32)) ;
#87964 = DIRECTION('center_axis',(0.,-1.,0.)) ;
#87965 = DIRECTION('ref_axis',(0.,0.,-1.)) ;
#87966 = DIRECTION('',(0.,0.,-1.)) ;
#87967 = DIRECTION('center_axis',(0.,-1.,0.)) ;
#87968 = DIRECTION('ref_axis',(0.,0.,-1.)) ;
#87969 = DIRECTION('',(-1.,0.,-6.27714964143733E-33)) ;
#87970 = DIRECTION('',(1.,0.,1.25542992828747E-32)) ;
#87971 = DIRECTION('center_axis',(0.,-1.,0.)) ;
#87972 = DIRECTION('ref_axis',(0.,0.,-1.)) ;
#87973 = DIRECTION('',(0.,0.,-1.)) ;
#87974 = DIRECTION('center_axis',(0.,-1.,0.)) ;
#87975 = DIRECTION('ref_axis',(0.,0.,-1.)) ;
#87976 = DIRECTION('',(-1.,0.,-6.27714964143733E-33)) ;
#87977 = DIRECTION('',(1.,0.,1.25542992828747E-32)) ;
#87978 = DIRECTION('center_axis',(0.,-1.,0.)) ;
#87979 = DIRECTION('ref_axis',(0.,0.,-1.)) ;
#87980 = DIRECTION('',(0.,0.,-1.)) ;
#87981 = DIRECTION('center_axis',(0.,-1.,0.)) ;
#87982 = DIRECTION('ref_axis',(0.,0.,-1.)) ;
#87983 = DIRECTION('',(-1.,0.,-6.27714964143733E-33)) ;
#87984 = DIRECTION('',(1.,0.,1.25542992828747E-32)) ;
#87985 = DIRECTION('center_axis',(0.,-1.,0.)) ;
#87986 = DIRECTION('ref_axis',(0.,0.,-1.)) ;
#87987 = DIRECTION('',(0.,0.,-1.)) ;
#87988 = DIRECTION('center_axis',(0.,-1.,0.)) ;
#87989 = DIRECTION('ref_axis',(0.,0.,-1.)) ;
#87990 = DIRECTION('',(-1.,0.,-6.27714964143733E-33)) ;
#87991 = DIRECTION('',(1.,0.,1.25542992828747E-32)) ;
#87992 = DIRECTION('center_axis',(0.,-1.,0.)) ;
#87993 = DIRECTION('ref_axis',(0.,0.,-1.)) ;
#87994 = DIRECTION('',(0.,0.,-1.)) ;
#87995 = DIRECTION('center_axis',(0.,-1.,0.)) ;
#87996 = DIRECTION('ref_axis',(0.,0.,-1.)) ;
#87997 = DIRECTION('',(-1.,0.,-6.27714964143733E-33)) ;
#87998 = DIRECTION('',(1.,0.,1.25542992828747E-32)) ;
#87999 = DIRECTION('center_axis',(0.,-1.,0.)) ;
#88000 = DIRECTION('ref_axis',(0.,0.,-1.)) ;
#88001 = DIRECTION('',(0.,0.,-1.)) ;
#88002 = DIRECTION('center_axis',(0.,-1.,0.)) ;
#88003 = DIRECTION('ref_axis',(0.,0.,-1.)) ;
#88004 = DIRECTION('',(-1.,0.,-6.27714964143733E-33)) ;
#88005 = DIRECTION('',(1.,0.,1.25542992828747E-32)) ;
#88006 = DIRECTION('center_axis',(0.,-1.,0.)) ;
#88007 = DIRECTION('ref_axis',(0.,0.,-1.)) ;
#88008 = DIRECTION('',(0.,0.,-1.)) ;
#88009 = DIRECTION('center_axis',(0.,-1.,0.)) ;
#88010 = DIRECTION('ref_axis',(0.,0.,-1.)) ;
#88011 = DIRECTION('',(-1.,0.,-6.27714964143733E-33)) ;
#88012 = DIRECTION('',(1.,0.,1.25542992828747E-32)) ;
#88013 = DIRECTION('center_axis',(0.,-1.,0.)) ;
#88014 = DIRECTION('ref_axis',(0.,0.,-1.)) ;
#88015 = DIRECTION('',(0.,0.,-1.)) ;
#88016 = DIRECTION('center_axis',(0.,-1.,0.)) ;
#88017 = DIRECTION('ref_axis',(0.,0.,-1.)) ;
#88018 = DIRECTION('',(-1.,0.,-6.27714964143733E-33)) ;
#88019 = DIRECTION('',(1.,0.,1.25542992828747E-32)) ;
#88020 = DIRECTION('center_axis',(0.,-1.,0.)) ;
#88021 = DIRECTION('ref_axis',(0.,0.,-1.)) ;
#88022 = DIRECTION('',(0.,0.,-1.)) ;
#88023 = DIRECTION('center_axis',(0.,0.,1.)) ;
#88024 = DIRECTION('ref_axis',(1.,0.,0.)) ;
#88025 = DIRECTION('center_axis',(0.,0.,-1.)) ;
#88026 = DIRECTION('ref_axis',(1.,0.,0.)) ;
#88027 = DIRECTION('',(0.,0.,1.)) ;
#88028 = DIRECTION('center_axis',(0.,0.,1.)) ;
#88029 = DIRECTION('ref_axis',(1.,0.,0.)) ;
#88030 = DIRECTION('center_axis',(-1.,-1.2303003375722E-16,0.)) ;
#88031 = DIRECTION('ref_axis',(1.2303003375722E-16,-1.,0.)) ;
#88032 = DIRECTION('center_axis',(-1.,-1.2303003375722E-16,0.)) ;
#88033 = DIRECTION('ref_axis',(1.2303003375722E-16,-1.,0.)) ;
#88034 = DIRECTION('',(1.2303003375722E-16,-1.,1.020425574104E-16)) ;
#88035 = DIRECTION('',(-1.2303003375722E-16,1.,-5.10212787052002E-17)) ;
#88036 = DIRECTION('center_axis',(-1.,-1.2303003375722E-16,0.)) ;
#88037 = DIRECTION('ref_axis',(1.2303003375722E-16,-1.,0.)) ;
#88038 = DIRECTION('',(0.,0.,1.)) ;
#88039 = DIRECTION('center_axis',(-1.,-1.2303003375722E-16,0.)) ;
#88040 = DIRECTION('ref_axis',(1.2303003375722E-16,-1.,0.)) ;
#88041 = DIRECTION('',(1.2303003375722E-16,-1.,1.020425574104E-16)) ;
#88042 = DIRECTION('',(-1.2303003375722E-16,1.,-5.10212787052002E-17)) ;
#88043 = DIRECTION('center_axis',(-1.,-1.2303003375722E-16,0.)) ;
#88044 = DIRECTION('ref_axis',(1.2303003375722E-16,-1.,0.)) ;
#88045 = DIRECTION('',(0.,0.,1.)) ;
#88046 = DIRECTION('center_axis',(-1.,-1.2303003375722E-16,0.)) ;
#88047 = DIRECTION('ref_axis',(1.2303003375722E-16,-1.,0.)) ;
#88048 = DIRECTION('',(1.2303003375722E-16,-1.,1.020425574104E-16)) ;
#88049 = DIRECTION('',(-1.2303003375722E-16,1.,-5.10212787052002E-17)) ;
#88050 = DIRECTION('center_axis',(-1.,-1.2303003375722E-16,0.)) ;
#88051 = DIRECTION('ref_axis',(1.2303003375722E-16,-1.,0.)) ;
#88052 = DIRECTION('',(0.,0.,1.)) ;
#88053 = DIRECTION('center_axis',(-1.,-1.2303003375722E-16,0.)) ;
#88054 = DIRECTION('ref_axis',(1.2303003375722E-16,-1.,0.)) ;
#88055 = DIRECTION('',(1.2303003375722E-16,-1.,1.020425574104E-16)) ;
#88056 = DIRECTION('',(-1.2303003375722E-16,1.,-5.10212787052002E-17)) ;
#88057 = DIRECTION('center_axis',(-1.,-1.2303003375722E-16,0.)) ;
#88058 = DIRECTION('ref_axis',(1.2303003375722E-16,-1.,0.)) ;
#88059 = DIRECTION('',(0.,0.,1.)) ;
#88060 = DIRECTION('center_axis',(-1.,-1.2303003375722E-16,0.)) ;
#88061 = DIRECTION('ref_axis',(1.2303003375722E-16,-1.,0.)) ;
#88062 = DIRECTION('',(1.2303003375722E-16,-1.,1.020425574104E-16)) ;
#88063 = DIRECTION('',(-1.2303003375722E-16,1.,-5.10212787052002E-17)) ;
#88064 = DIRECTION('center_axis',(-1.,-1.2303003375722E-16,0.)) ;
#88065 = DIRECTION('ref_axis',(1.2303003375722E-16,-1.,0.)) ;
#88066 = DIRECTION('',(0.,0.,1.)) ;
#88067 = DIRECTION('center_axis',(-1.,-1.2303003375722E-16,0.)) ;
#88068 = DIRECTION('ref_axis',(1.2303003375722E-16,-1.,0.)) ;
#88069 = DIRECTION('',(1.2303003375722E-16,-1.,1.020425574104E-16)) ;
#88070 = DIRECTION('',(-1.2303003375722E-16,1.,-5.10212787052002E-17)) ;
#88071 = DIRECTION('center_axis',(-1.,-1.2303003375722E-16,0.)) ;
#88072 = DIRECTION('ref_axis',(1.2303003375722E-16,-1.,0.)) ;
#88073 = DIRECTION('',(0.,0.,1.)) ;
#88074 = DIRECTION('center_axis',(-1.,-1.2303003375722E-16,0.)) ;
#88075 = DIRECTION('ref_axis',(1.2303003375722E-16,-1.,0.)) ;
#88076 = DIRECTION('',(1.2303003375722E-16,-1.,1.020425574104E-16)) ;
#88077 = DIRECTION('',(-1.2303003375722E-16,1.,-5.10212787052002E-17)) ;
#88078 = DIRECTION('center_axis',(-1.,-1.2303003375722E-16,0.)) ;
#88079 = DIRECTION('ref_axis',(1.2303003375722E-16,-1.,0.)) ;
#88080 = DIRECTION('',(0.,0.,1.)) ;
#88081 = DIRECTION('center_axis',(-1.,-1.2303003375722E-16,0.)) ;
#88082 = DIRECTION('ref_axis',(1.2303003375722E-16,-1.,0.)) ;
#88083 = DIRECTION('',(1.2303003375722E-16,-1.,1.020425574104E-16)) ;
#88084 = DIRECTION('',(-1.2303003375722E-16,1.,-5.10212787052002E-17)) ;
#88085 = DIRECTION('center_axis',(-1.,-1.2303003375722E-16,0.)) ;
#88086 = DIRECTION('ref_axis',(1.2303003375722E-16,-1.,0.)) ;
#88087 = DIRECTION('',(0.,0.,1.)) ;
#88088 = DIRECTION('center_axis',(-1.,-1.2303003375722E-16,0.)) ;
#88089 = DIRECTION('ref_axis',(1.2303003375722E-16,-1.,0.)) ;
#88090 = DIRECTION('',(1.2303003375722E-16,-1.,1.020425574104E-16)) ;
#88091 = DIRECTION('',(-1.2303003375722E-16,1.,-5.10212787052002E-17)) ;
#88092 = DIRECTION('center_axis',(-1.,-1.2303003375722E-16,0.)) ;
#88093 = DIRECTION('ref_axis',(1.2303003375722E-16,-1.,0.)) ;
#88094 = DIRECTION('',(0.,0.,1.)) ;
#88095 = DIRECTION('center_axis',(-1.,-1.2303003375722E-16,0.)) ;
#88096 = DIRECTION('ref_axis',(1.2303003375722E-16,-1.,0.)) ;
#88097 = DIRECTION('',(1.2303003375722E-16,-1.,1.020425574104E-16)) ;
#88098 = DIRECTION('',(-1.2303003375722E-16,1.,0.)) ;
#88099 = DIRECTION('',(0.,0.,1.)) ;
#88100 = DIRECTION('',(1.2303003375722E-16,-1.,0.)) ;
#88101 = DIRECTION('',(-1.2303003375722E-16,1.,-5.10212787052002E-17)) ;
#88102 = DIRECTION('center_axis',(-1.,-1.2303003375722E-16,0.)) ;
#88103 = DIRECTION('ref_axis',(1.2303003375722E-16,-1.,0.)) ;
#88104 = DIRECTION('',(0.,0.,1.)) ;
#88105 = DIRECTION('center_axis',(0.,0.,1.)) ;
#88106 = DIRECTION('ref_axis',(1.,0.,0.)) ;
#88107 = DIRECTION('',(0.,0.,1.)) ;
#88108 = DIRECTION('center_axis',(0.,0.,1.)) ;
#88109 = DIRECTION('ref_axis',(1.,0.,0.)) ;
#88110 = DIRECTION('center_axis',(0.,0.,-1.)) ;
#88111 = DIRECTION('ref_axis',(1.,0.,0.)) ;
#88112 = DIRECTION('center_axis',(-1.59148942750166E-16,1.,0.)) ;
#88113 = DIRECTION('ref_axis',(-1.,-1.59148942750166E-16,0.)) ;
#88114 = DIRECTION('',(0.,0.,1.)) ;
#88115 = DIRECTION('',(-1.,-1.59148942750166E-16,0.)) ;
#88116 = DIRECTION('',(1.,1.59148942750166E-16,0.)) ;
#88117 = DIRECTION('center_axis',(0.,0.,1.)) ;
#88118 = DIRECTION('ref_axis',(1.,0.,0.)) ;
#88119 = DIRECTION('',(0.,0.,1.)) ;
#88120 = DIRECTION('center_axis',(0.,0.,-1.)) ;
#88121 = DIRECTION('ref_axis',(1.,0.,0.)) ;
#88122 = DIRECTION('center_axis',(0.,0.,1.)) ;
#88123 = DIRECTION('ref_axis',(1.,0.,0.)) ;
#88124 = DIRECTION('center_axis',(-1.,0.,0.)) ;
#88125 = DIRECTION('ref_axis',(0.,0.,1.)) ;
#88126 = DIRECTION('',(0.,0.,1.)) ;
#88127 = DIRECTION('',(0.,-1.,0.)) ;
#88128 = DIRECTION('',(0.,1.,0.)) ;
#88129 = DIRECTION('center_axis',(0.,0.,1.)) ;
#88130 = DIRECTION('ref_axis',(1.,0.,0.)) ;
#88131 = DIRECTION('',(0.,0.,1.)) ;
#88132 = DIRECTION('center_axis',(0.,0.,1.)) ;
#88133 = DIRECTION('ref_axis',(1.,0.,0.)) ;
#88134 = DIRECTION('center_axis',(0.,0.,-1.)) ;
#88135 = DIRECTION('ref_axis',(1.,0.,0.)) ;
#88136 = DIRECTION('center_axis',(0.,1.,0.)) ;
#88137 = DIRECTION('ref_axis',(0.,0.,1.)) ;
#88138 = DIRECTION('',(0.,0.,1.)) ;
#88139 = DIRECTION('',(-1.,0.,0.)) ;
#88140 = DIRECTION('',(1.,0.,0.)) ;
#88141 = DIRECTION('center_axis',(0.,0.,1.)) ;
#88142 = DIRECTION('ref_axis',(1.,0.,0.)) ;
#88143 = DIRECTION('',(0.,0.,1.)) ;
#88144 = DIRECTION('center_axis',(0.,0.,1.)) ;
#88145 = DIRECTION('ref_axis',(1.,0.,0.)) ;
#88146 = DIRECTION('center_axis',(0.,0.,-1.)) ;
#88147 = DIRECTION('ref_axis',(1.,0.,0.)) ;
#88148 = DIRECTION('center_axis',(1.,-4.33680868994203E-15,0.)) ;
#88149 = DIRECTION('ref_axis',(4.33680868994203E-15,1.,0.)) ;
#88150 = DIRECTION('',(0.,0.,1.)) ;
#88151 = DIRECTION('',(4.33680868994203E-15,1.,0.)) ;
#88152 = DIRECTION('',(-4.33680868994203E-15,-1.,0.)) ;
#88153 = DIRECTION('center_axis',(0.,0.,1.)) ;
#88154 = DIRECTION('ref_axis',(1.,0.,0.)) ;
#88155 = DIRECTION('',(0.,0.,1.)) ;
#88156 = DIRECTION('center_axis',(0.,0.,-1.)) ;
#88157 = DIRECTION('ref_axis',(1.,0.,0.)) ;
#88158 = DIRECTION('center_axis',(0.,0.,1.)) ;
#88159 = DIRECTION('ref_axis',(1.,0.,0.)) ;
#88160 = DIRECTION('center_axis',(5.88041856263325E-16,1.,0.)) ;
#88161 = DIRECTION('ref_axis',(-1.,5.88041856263325E-16,0.)) ;
#88162 = DIRECTION('',(0.,0.,1.)) ;
#88163 = DIRECTION('',(-1.,5.88041856263325E-16,0.)) ;
#88164 = DIRECTION('',(1.,-5.88041856263325E-16,0.)) ;
#88165 = DIRECTION('center_axis',(0.,0.,1.)) ;
#88166 = DIRECTION('ref_axis',(1.,0.,0.)) ;
#88167 = DIRECTION('',(0.,0.,1.)) ;
#88168 = DIRECTION('center_axis',(0.,0.,1.)) ;
#88169 = DIRECTION('ref_axis',(1.,0.,0.)) ;
#88170 = DIRECTION('center_axis',(0.,0.,-1.)) ;
#88171 = DIRECTION('ref_axis',(1.,0.,0.)) ;
#88172 = DIRECTION('center_axis',(1.,0.,0.)) ;
#88173 = DIRECTION('ref_axis',(0.,0.,-1.)) ;
#88174 = DIRECTION('',(0.,1.,0.)) ;
#88175 = DIRECTION('',(0.,-1.,0.)) ;
#88176 = DIRECTION('center_axis',(-1.,0.,0.)) ;
#88177 = DIRECTION('ref_axis',(0.,0.,-1.)) ;
#88178 = DIRECTION('',(0.,0.,-1.)) ;
#88179 = DIRECTION('',(0.,1.,0.)) ;
#88180 = DIRECTION('',(0.,3.99416362155027E-15,1.)) ;
#88181 = DIRECTION('center_axis',(-1.,0.,0.)) ;
#88182 = DIRECTION('ref_axis',(0.,6.50521303491307E-15,-1.)) ;
#88183 = DIRECTION('',(0.,0.707106781186546,0.707106781186549)) ;
#88184 = DIRECTION('center_axis',(-1.,0.,0.)) ;
#88185 = DIRECTION('ref_axis',(0.,-1.51788304147972E-14,-1.)) ;
#88186 = DIRECTION('',(0.,0.,-1.)) ;
#88187 = DIRECTION('',(0.,-0.707106781186548,0.707106781186547)) ;
#88188 = DIRECTION('center_axis',(-1.,0.,0.)) ;
#88189 = DIRECTION('ref_axis',(0.,1.30104260698261E-14,-1.)) ;
#88190 = DIRECTION('',(0.,0.,1.)) ;
#88191 = DIRECTION('',(0.,-1.,0.)) ;
#88192 = DIRECTION('',(0.,0.,-1.)) ;
#88193 = DIRECTION('center_axis',(-1.,0.,0.)) ;
#88194 = DIRECTION('ref_axis',(0.,1.19262238973406E-14,-1.)) ;
#88195 = DIRECTION('',(0.,-1.,-1.07081696047951E-16)) ;
#88196 = DIRECTION('center_axis',(-1.,0.,0.)) ;
#88197 = DIRECTION('ref_axis',(0.,0.,-1.)) ;
#88198 = DIRECTION('',(0.,0.,1.)) ;
#88199 = DIRECTION('center_axis',(-1.,0.,0.)) ;
#88200 = DIRECTION('ref_axis',(0.,4.33680868994204E-15,-1.)) ;
#88201 = DIRECTION('center_axis',(1.,0.,0.)) ;
#88202 = DIRECTION('ref_axis',(0.,0.,-1.)) ;
#88203 = DIRECTION('center_axis',(-1.,0.,0.)) ;
#88204 = DIRECTION('ref_axis',(0.,8.67361737988409E-15,-1.)) ;
#88205 = DIRECTION('',(0.,0.,1.)) ;
#88206 = DIRECTION('center_axis',(-1.,0.,0.)) ;
#88207 = DIRECTION('ref_axis',(0.,0.,-1.)) ;
#88208 = DIRECTION('',(0.,1.,1.07081696047951E-16)) ;
#88209 = DIRECTION('center_axis',(-1.,0.,0.)) ;
#88210 = DIRECTION('ref_axis',(0.,0.,-1.)) ;
#88211 = DIRECTION('',(0.,0.,-1.)) ;
#88212 = DIRECTION('',(0.,1.,0.)) ;
#88213 = DIRECTION('',(0.,3.99416362155027E-15,1.)) ;
#88214 = DIRECTION('center_axis',(-1.,0.,0.)) ;
#88215 = DIRECTION('ref_axis',(0.,6.50521303491307E-15,-1.)) ;
#88216 = DIRECTION('',(0.,0.707106781186546,0.707106781186549)) ;
#88217 = DIRECTION('center_axis',(-1.,0.,0.)) ;
#88218 = DIRECTION('ref_axis',(0.,0.,-1.)) ;
#88219 = DIRECTION('',(0.,0.,-1.)) ;
#88220 = DIRECTION('',(0.,-0.707106781186548,0.707106781186547)) ;
#88221 = DIRECTION('center_axis',(-1.,0.,0.)) ;
#88222 = DIRECTION('ref_axis',(0.,1.30104260698261E-14,-1.)) ;
#88223 = DIRECTION('',(0.,0.,1.)) ;
#88224 = DIRECTION('',(0.,-1.,0.)) ;
#88225 = DIRECTION('',(0.,0.,-1.)) ;
#88226 = DIRECTION('center_axis',(-1.,0.,0.)) ;
#88227 = DIRECTION('ref_axis',(0.,1.08420217248551E-14,-1.)) ;
#88228 = DIRECTION('',(0.,-1.,-1.07081696047951E-16)) ;
#88229 = DIRECTION('center_axis',(-1.,0.,0.)) ;
#88230 = DIRECTION('ref_axis',(0.,0.,-1.)) ;
#88231 = DIRECTION('',(0.,0.,1.)) ;
#88232 = DIRECTION('center_axis',(-1.,0.,0.)) ;
#88233 = DIRECTION('ref_axis',(0.,4.33680868994204E-15,-1.)) ;
#88234 = DIRECTION('center_axis',(1.,0.,0.)) ;
#88235 = DIRECTION('ref_axis',(0.,0.,-1.)) ;
#88236 = DIRECTION('center_axis',(-1.,0.,0.)) ;
#88237 = DIRECTION('ref_axis',(0.,-2.16840434497102E-15,-1.)) ;
#88238 = DIRECTION('',(0.,0.,1.)) ;
#88239 = DIRECTION('center_axis',(-1.,0.,0.)) ;
#88240 = DIRECTION('ref_axis',(0.,0.,-1.)) ;
#88241 = DIRECTION('',(0.,1.,1.07081696047951E-16)) ;
#88242 = DIRECTION('center_axis',(-1.,0.,0.)) ;
#88243 = DIRECTION('ref_axis',(0.,0.,-1.)) ;
#88244 = DIRECTION('',(0.,0.,-1.)) ;
#88245 = DIRECTION('',(0.,1.,0.)) ;
#88246 = DIRECTION('',(0.,3.99416362155027E-15,1.)) ;
#88247 = DIRECTION('center_axis',(-1.,0.,0.)) ;
#88248 = DIRECTION('ref_axis',(0.,6.50521303491307E-15,-1.)) ;
#88249 = DIRECTION('',(0.,0.707106781186546,0.707106781186549)) ;
#88250 = DIRECTION('center_axis',(-1.,0.,0.)) ;
#88251 = DIRECTION('ref_axis',(0.,0.,-1.)) ;
#88252 = DIRECTION('',(0.,0.,-1.)) ;
#88253 = DIRECTION('',(0.,-0.707106781186548,0.707106781186547)) ;
#88254 = DIRECTION('center_axis',(-1.,0.,0.)) ;
#88255 = DIRECTION('ref_axis',(0.,0.,-1.)) ;
#88256 = DIRECTION('',(0.,0.,1.)) ;
#88257 = DIRECTION('',(0.,-1.,0.)) ;
#88258 = DIRECTION('',(0.,0.,-1.)) ;
#88259 = DIRECTION('center_axis',(-1.,0.,0.)) ;
#88260 = DIRECTION('ref_axis',(0.,1.08420217248551E-14,-1.)) ;
#88261 = DIRECTION('',(0.,-1.,-1.07081696047951E-16)) ;
#88262 = DIRECTION('center_axis',(-1.,0.,0.)) ;
#88263 = DIRECTION('ref_axis',(0.,0.,-1.)) ;
#88264 = DIRECTION('',(0.,0.,1.)) ;
#88265 = DIRECTION('center_axis',(-1.,0.,0.)) ;
#88266 = DIRECTION('ref_axis',(0.,0.,-1.)) ;
#88267 = DIRECTION('center_axis',(1.,0.,0.)) ;
#88268 = DIRECTION('ref_axis',(0.,0.,-1.)) ;
#88269 = DIRECTION('center_axis',(-1.,0.,0.)) ;
#88270 = DIRECTION('ref_axis',(0.,-2.16840434497102E-15,-1.)) ;
#88271 = DIRECTION('',(0.,0.,1.)) ;
#88272 = DIRECTION('center_axis',(-1.,0.,0.)) ;
#88273 = DIRECTION('ref_axis',(0.,0.,-1.)) ;
#88274 = DIRECTION('',(0.,1.,1.07081696047951E-16)) ;
#88275 = DIRECTION('center_axis',(-1.,0.,0.)) ;
#88276 = DIRECTION('ref_axis',(0.,0.,-1.)) ;
#88277 = DIRECTION('',(0.,0.,-1.)) ;
#88278 = DIRECTION('',(0.,1.,0.)) ;
#88279 = DIRECTION('',(0.,3.99416362155027E-15,1.)) ;
#88280 = DIRECTION('center_axis',(-1.,0.,0.)) ;
#88281 = DIRECTION('ref_axis',(0.,6.50521303491307E-15,-1.)) ;
#88282 = DIRECTION('',(0.,0.707106781186546,0.707106781186549)) ;
#88283 = DIRECTION('center_axis',(-1.,0.,0.)) ;
#88284 = DIRECTION('ref_axis',(0.,0.,-1.)) ;
#88285 = DIRECTION('',(0.,0.,-1.)) ;
#88286 = DIRECTION('',(0.,-0.707106781186548,0.707106781186547)) ;
#88287 = DIRECTION('center_axis',(-1.,0.,0.)) ;
#88288 = DIRECTION('ref_axis',(0.,0.,-1.)) ;
#88289 = DIRECTION('',(0.,0.,1.)) ;
#88290 = DIRECTION('',(0.,-1.,0.)) ;
#88291 = DIRECTION('',(0.,0.,-1.)) ;
#88292 = DIRECTION('center_axis',(-1.,0.,0.)) ;
#88293 = DIRECTION('ref_axis',(0.,1.08420217248551E-14,-1.)) ;
#88294 = DIRECTION('',(0.,-1.,-1.07081696047951E-16)) ;
#88295 = DIRECTION('center_axis',(-1.,0.,0.)) ;
#88296 = DIRECTION('ref_axis',(0.,0.,-1.)) ;
#88297 = DIRECTION('',(0.,0.,1.)) ;
#88298 = DIRECTION('center_axis',(-1.,0.,0.)) ;
#88299 = DIRECTION('ref_axis',(0.,0.,-1.)) ;
#88300 = DIRECTION('center_axis',(1.,0.,0.)) ;
#88301 = DIRECTION('ref_axis',(0.,0.,-1.)) ;
#88302 = DIRECTION('center_axis',(-1.,0.,0.)) ;
#88303 = DIRECTION('ref_axis',(0.,-2.16840434497102E-15,-1.)) ;
#88304 = DIRECTION('',(0.,0.,1.)) ;
#88305 = DIRECTION('center_axis',(-1.,0.,0.)) ;
#88306 = DIRECTION('ref_axis',(0.,0.,-1.)) ;
#88307 = DIRECTION('',(0.,1.,1.07081696047951E-16)) ;
#88308 = DIRECTION('center_axis',(-1.,0.,0.)) ;
#88309 = DIRECTION('ref_axis',(0.,0.,-1.)) ;
#88310 = DIRECTION('',(0.,0.,-1.)) ;
#88311 = DIRECTION('',(0.,1.,0.)) ;
#88312 = DIRECTION('',(0.,3.99416362155027E-15,1.)) ;
#88313 = DIRECTION('center_axis',(-1.,0.,0.)) ;
#88314 = DIRECTION('ref_axis',(0.,6.50521303491307E-15,-1.)) ;
#88315 = DIRECTION('',(0.,0.707106781186546,0.707106781186549)) ;
#88316 = DIRECTION('center_axis',(-1.,0.,0.)) ;
#88317 = DIRECTION('ref_axis',(0.,0.,-1.)) ;
#88318 = DIRECTION('',(0.,0.,-1.)) ;
#88319 = DIRECTION('',(0.,-0.707106781186548,0.707106781186547)) ;
#88320 = DIRECTION('center_axis',(-1.,0.,0.)) ;
#88321 = DIRECTION('ref_axis',(0.,0.,-1.)) ;
#88322 = DIRECTION('',(0.,0.,1.)) ;
#88323 = DIRECTION('',(0.,-1.,0.)) ;
#88324 = DIRECTION('',(0.,0.,-1.)) ;
#88325 = DIRECTION('center_axis',(-1.,0.,0.)) ;
#88326 = DIRECTION('ref_axis',(0.,1.08420217248551E-14,-1.)) ;
#88327 = DIRECTION('',(0.,-1.,-1.07081696047951E-16)) ;
#88328 = DIRECTION('center_axis',(-1.,0.,0.)) ;
#88329 = DIRECTION('ref_axis',(0.,0.,-1.)) ;
#88330 = DIRECTION('',(0.,0.,1.)) ;
#88331 = DIRECTION('center_axis',(-1.,0.,0.)) ;
#88332 = DIRECTION('ref_axis',(0.,0.,-1.)) ;
#88333 = DIRECTION('center_axis',(1.,0.,0.)) ;
#88334 = DIRECTION('ref_axis',(0.,0.,-1.)) ;
#88335 = DIRECTION('center_axis',(-1.,0.,0.)) ;
#88336 = DIRECTION('ref_axis',(0.,-2.16840434497102E-15,-1.)) ;
#88337 = DIRECTION('',(0.,0.,1.)) ;
#88338 = DIRECTION('center_axis',(-1.,0.,0.)) ;
#88339 = DIRECTION('ref_axis',(0.,0.,-1.)) ;
#88340 = DIRECTION('',(0.,1.,1.07081696047951E-16)) ;
#88341 = DIRECTION('center_axis',(-1.,0.,0.)) ;
#88342 = DIRECTION('ref_axis',(0.,0.,-1.)) ;
#88343 = DIRECTION('',(0.,0.,-1.)) ;
#88344 = DIRECTION('',(0.,1.,0.)) ;
#88345 = DIRECTION('',(0.,3.99416362155027E-15,1.)) ;
#88346 = DIRECTION('center_axis',(-1.,0.,0.)) ;
#88347 = DIRECTION('ref_axis',(0.,2.16840434497102E-15,-1.)) ;
#88348 = DIRECTION('',(0.,0.707106781186546,0.707106781186549)) ;
#88349 = DIRECTION('center_axis',(-1.,0.,0.)) ;
#88350 = DIRECTION('ref_axis',(0.,0.,-1.)) ;
#88351 = DIRECTION('',(0.,0.,-1.)) ;
#88352 = DIRECTION('',(0.,-0.707106781186548,0.707106781186547)) ;
#88353 = DIRECTION('center_axis',(-1.,0.,0.)) ;
#88354 = DIRECTION('ref_axis',(0.,0.,-1.)) ;
#88355 = DIRECTION('',(0.,0.,1.)) ;
#88356 = DIRECTION('',(0.,-1.,0.)) ;
#88357 = DIRECTION('',(0.,0.,-1.)) ;
#88358 = DIRECTION('center_axis',(-1.,0.,0.)) ;
#88359 = DIRECTION('ref_axis',(0.,1.08420217248551E-14,-1.)) ;
#88360 = DIRECTION('',(0.,-1.,-1.07081696047951E-16)) ;
#88361 = DIRECTION('center_axis',(-1.,0.,0.)) ;
#88362 = DIRECTION('ref_axis',(0.,0.,-1.)) ;
#88363 = DIRECTION('',(0.,0.,1.)) ;
#88364 = DIRECTION('center_axis',(-1.,0.,0.)) ;
#88365 = DIRECTION('ref_axis',(0.,0.,-1.)) ;
#88366 = DIRECTION('center_axis',(1.,0.,0.)) ;
#88367 = DIRECTION('ref_axis',(0.,0.,-1.)) ;
#88368 = DIRECTION('center_axis',(-1.,0.,0.)) ;
#88369 = DIRECTION('ref_axis',(0.,-2.168404344971E-15,-1.)) ;
#88370 = DIRECTION('',(0.,0.,1.)) ;
#88371 = DIRECTION('center_axis',(-1.,0.,0.)) ;
#88372 = DIRECTION('ref_axis',(0.,0.,-1.)) ;
#88373 = DIRECTION('',(0.,1.,1.07081696047951E-16)) ;
#88374 = DIRECTION('center_axis',(-1.,0.,0.)) ;
#88375 = DIRECTION('ref_axis',(0.,0.,-1.)) ;
#88376 = DIRECTION('',(0.,0.,-1.)) ;
#88377 = DIRECTION('',(0.,1.,0.)) ;
#88378 = DIRECTION('',(0.,3.99416362155027E-15,1.)) ;
#88379 = DIRECTION('center_axis',(-1.,0.,0.)) ;
#88380 = DIRECTION('ref_axis',(0.,2.16840434497102E-15,-1.)) ;
#88381 = DIRECTION('',(0.,0.707106781186546,0.707106781186549)) ;
#88382 = DIRECTION('center_axis',(-1.,0.,0.)) ;
#88383 = DIRECTION('ref_axis',(0.,0.,-1.)) ;
#88384 = DIRECTION('',(0.,0.,-1.)) ;
#88385 = DIRECTION('',(0.,-0.707106781186548,0.707106781186547)) ;
#88386 = DIRECTION('center_axis',(-1.,0.,0.)) ;
#88387 = DIRECTION('ref_axis',(0.,0.,-1.)) ;
#88388 = DIRECTION('',(0.,0.,1.)) ;
#88389 = DIRECTION('',(0.,-1.,0.)) ;
#88390 = DIRECTION('',(0.,0.,-1.)) ;
#88391 = DIRECTION('center_axis',(-1.,0.,0.)) ;
#88392 = DIRECTION('ref_axis',(0.,1.0842021724855E-14,-1.)) ;
#88393 = DIRECTION('',(0.,-1.,-1.07081696047951E-16)) ;
#88394 = DIRECTION('center_axis',(-1.,0.,0.)) ;
#88395 = DIRECTION('ref_axis',(0.,0.,-1.)) ;
#88396 = DIRECTION('',(0.,0.,1.)) ;
#88397 = DIRECTION('center_axis',(-1.,0.,0.)) ;
#88398 = DIRECTION('ref_axis',(0.,-2.168404344971E-15,-1.)) ;
#88399 = DIRECTION('center_axis',(1.,0.,0.)) ;
#88400 = DIRECTION('ref_axis',(0.,0.,-1.)) ;
#88401 = DIRECTION('center_axis',(-1.,0.,0.)) ;
#88402 = DIRECTION('ref_axis',(0.,-2.168404344971E-15,-1.)) ;
#88403 = DIRECTION('',(0.,0.,1.)) ;
#88404 = DIRECTION('center_axis',(-1.,0.,0.)) ;
#88405 = DIRECTION('ref_axis',(0.,0.,-1.)) ;
#88406 = DIRECTION('',(0.,1.,1.07081696047951E-16)) ;
#88407 = DIRECTION('center_axis',(-1.,0.,0.)) ;
#88408 = DIRECTION('ref_axis',(0.,0.,-1.)) ;
#88409 = DIRECTION('',(0.,0.,-1.)) ;
#88410 = DIRECTION('',(0.,1.,0.)) ;
#88411 = DIRECTION('',(0.,3.99416362155027E-15,1.)) ;
#88412 = DIRECTION('center_axis',(-1.,0.,0.)) ;
#88413 = DIRECTION('ref_axis',(0.,0.,-1.)) ;
#88414 = DIRECTION('',(0.,0.707106781186546,0.707106781186549)) ;
#88415 = DIRECTION('center_axis',(-1.,0.,0.)) ;
#88416 = DIRECTION('ref_axis',(0.,0.,-1.)) ;
#88417 = DIRECTION('',(0.,0.,-1.)) ;
#88418 = DIRECTION('',(0.,-0.707106781186548,0.707106781186547)) ;
#88419 = DIRECTION('center_axis',(-1.,0.,0.)) ;
#88420 = DIRECTION('ref_axis',(0.,0.,-1.)) ;
#88421 = DIRECTION('',(0.,0.,1.)) ;
#88422 = DIRECTION('',(0.,-1.,0.)) ;
#88423 = DIRECTION('',(0.,0.,-1.)) ;
#88424 = DIRECTION('center_axis',(-1.,0.,0.)) ;
#88425 = DIRECTION('ref_axis',(0.,1.0842021724855E-14,-1.)) ;
#88426 = DIRECTION('',(0.,-1.,-1.07081696047951E-16)) ;
#88427 = DIRECTION('center_axis',(-1.,0.,0.)) ;
#88428 = DIRECTION('ref_axis',(0.,0.,-1.)) ;
#88429 = DIRECTION('',(0.,0.,1.)) ;
#88430 = DIRECTION('center_axis',(-1.,0.,0.)) ;
#88431 = DIRECTION('ref_axis',(0.,-2.168404344971E-15,-1.)) ;
#88432 = DIRECTION('center_axis',(1.,0.,0.)) ;
#88433 = DIRECTION('ref_axis',(0.,0.,-1.)) ;
#88434 = DIRECTION('center_axis',(-1.,0.,0.)) ;
#88435 = DIRECTION('ref_axis',(0.,0.,-1.)) ;
#88436 = DIRECTION('',(0.,0.,1.)) ;
#88437 = DIRECTION('center_axis',(-1.,0.,0.)) ;
#88438 = DIRECTION('ref_axis',(0.,0.,-1.)) ;
#88439 = DIRECTION('',(0.,1.,1.07081696047951E-16)) ;
#88440 = DIRECTION('center_axis',(-1.,0.,0.)) ;
#88441 = DIRECTION('ref_axis',(0.,0.,-1.)) ;
#88442 = DIRECTION('',(0.,0.,-1.)) ;
#88443 = DIRECTION('',(0.,1.,0.)) ;
#88444 = DIRECTION('',(0.,3.99416362155027E-15,1.)) ;
#88445 = DIRECTION('center_axis',(-1.,0.,0.)) ;
#88446 = DIRECTION('ref_axis',(0.,0.,-1.)) ;
#88447 = DIRECTION('',(0.,0.707106781186546,0.707106781186549)) ;
#88448 = DIRECTION('center_axis',(-1.,0.,0.)) ;
#88449 = DIRECTION('ref_axis',(0.,0.,-1.)) ;
#88450 = DIRECTION('',(0.,0.,-1.)) ;
#88451 = DIRECTION('',(0.,-0.707106781186548,0.707106781186547)) ;
#88452 = DIRECTION('center_axis',(-1.,0.,0.)) ;
#88453 = DIRECTION('ref_axis',(0.,0.,-1.)) ;
#88454 = DIRECTION('',(0.,0.,1.)) ;
#88455 = DIRECTION('',(0.,-1.,0.)) ;
#88456 = DIRECTION('',(0.,0.,-1.)) ;
#88457 = DIRECTION('center_axis',(-1.,0.,0.)) ;
#88458 = DIRECTION('ref_axis',(0.,9.75781955236956E-15,-1.)) ;
#88459 = DIRECTION('',(0.,-1.,-1.07081696047951E-16)) ;
#88460 = DIRECTION('center_axis',(-1.,0.,0.)) ;
#88461 = DIRECTION('ref_axis',(0.,0.,-1.)) ;
#88462 = DIRECTION('',(0.,0.,1.)) ;
#88463 = DIRECTION('center_axis',(-1.,0.,0.)) ;
#88464 = DIRECTION('ref_axis',(0.,-2.16840434497101E-15,-1.)) ;
#88465 = DIRECTION('center_axis',(1.,0.,0.)) ;
#88466 = DIRECTION('ref_axis',(0.,0.,-1.)) ;
#88467 = DIRECTION('center_axis',(-1.,0.,0.)) ;
#88468 = DIRECTION('ref_axis',(0.,0.,-1.)) ;
#88469 = DIRECTION('',(0.,0.,1.)) ;
#88470 = DIRECTION('center_axis',(-1.,0.,0.)) ;
#88471 = DIRECTION('ref_axis',(0.,0.,-1.)) ;
#88472 = DIRECTION('',(0.,1.,1.07081696047951E-16)) ;
#88473 = DIRECTION('center_axis',(-1.,0.,0.)) ;
#88474 = DIRECTION('ref_axis',(0.,-1.0842021724855E-15,-1.)) ;
#88475 = DIRECTION('',(0.,0.,-1.)) ;
#88476 = DIRECTION('',(0.,1.,0.)) ;
#88477 = DIRECTION('',(0.,3.99416362155027E-15,1.)) ;
#88478 = DIRECTION('center_axis',(-1.,0.,0.)) ;
#88479 = DIRECTION('ref_axis',(0.,2.16840434497101E-15,-1.)) ;
#88480 = DIRECTION('',(0.,0.707106781186546,0.707106781186549)) ;
#88481 = DIRECTION('center_axis',(-1.,0.,0.)) ;
#88482 = DIRECTION('ref_axis',(0.,0.,-1.)) ;
#88483 = DIRECTION('',(0.,0.,-1.)) ;
#88484 = DIRECTION('',(0.,-0.707106781186548,0.707106781186547)) ;
#88485 = DIRECTION('center_axis',(-1.,0.,0.)) ;
#88486 = DIRECTION('ref_axis',(0.,0.,-1.)) ;
#88487 = DIRECTION('',(0.,0.,1.)) ;
#88488 = DIRECTION('',(0.,-1.,0.)) ;
#88489 = DIRECTION('',(0.,0.,-1.)) ;
#88490 = DIRECTION('center_axis',(-1.,0.,0.)) ;
#88491 = DIRECTION('ref_axis',(0.,8.67361737988403E-15,-1.)) ;
#88492 = DIRECTION('',(0.,-1.,-1.07081696047951E-16)) ;
#88493 = DIRECTION('center_axis',(-1.,0.,0.)) ;
#88494 = DIRECTION('ref_axis',(0.,0.,-1.)) ;
#88495 = DIRECTION('',(0.,0.,1.)) ;
#88496 = DIRECTION('center_axis',(-1.,0.,0.)) ;
#88497 = DIRECTION('ref_axis',(0.,2.16840434497101E-15,-1.)) ;
#88498 = DIRECTION('center_axis',(1.,0.,0.)) ;
#88499 = DIRECTION('ref_axis',(0.,0.,-1.)) ;
#88500 = DIRECTION('center_axis',(-1.,0.,0.)) ;
#88501 = DIRECTION('ref_axis',(0.,0.,-1.)) ;
#88502 = DIRECTION('',(0.,0.,1.)) ;
#88503 = DIRECTION('center_axis',(-1.,0.,0.)) ;
#88504 = DIRECTION('ref_axis',(0.,0.,-1.)) ;
#88505 = DIRECTION('',(0.,1.,1.07081696047951E-16)) ;
#88506 = DIRECTION('center_axis',(0.,0.,1.)) ;
#88507 = DIRECTION('ref_axis',(1.,0.,0.)) ;
#88508 = DIRECTION('',(0.,-1.,0.)) ;
#88509 = DIRECTION('',(-1.,0.,0.)) ;
#88510 = DIRECTION('',(-1.2303003375722E-16,1.,0.)) ;
#88511 = DIRECTION('',(1.,1.59148942750166E-16,0.)) ;
#88512 = DIRECTION('center_axis',(0.,0.,1.)) ;
#88513 = DIRECTION('ref_axis',(1.,0.,0.)) ;
#88514 = DIRECTION('',(0.,1.,0.)) ;
#88515 = DIRECTION('',(1.,0.,0.)) ;
#88516 = DIRECTION('',(-4.33680868994203E-15,-1.,0.)) ;
#88517 = DIRECTION('center_axis',(0.,0.,1.)) ;
#88518 = DIRECTION('ref_axis',(1.,0.,0.)) ;
#88519 = DIRECTION('',(1.,-5.88041856263325E-16,0.)) ;
#88520 = DIRECTION('center_axis',(0.,0.,1.)) ;
#88521 = DIRECTION('ref_axis',(1.,0.,0.)) ;
#88522 = DIRECTION('',(1.2303003375722E-16,-1.,0.)) ;
#88523 = DIRECTION('',(1.,0.,0.)) ;
#88524 = DIRECTION('',(0.,1.,0.)) ;
#88525 = DIRECTION('',(-1.,5.88041856263325E-16,0.)) ;
#88526 = DIRECTION('center_axis',(0.,0.,-1.)) ;
#88527 = DIRECTION('ref_axis',(1.,0.,0.)) ;
#88528 = DIRECTION('',(4.33680868994203E-15,1.,0.)) ;
#88529 = DIRECTION('',(-1.,0.,0.)) ;
#88530 = DIRECTION('',(0.,-1.,0.)) ;
#88531 = DIRECTION('center_axis',(0.,0.,-1.)) ;
#88532 = DIRECTION('ref_axis',(1.,0.,0.)) ;
#88533 = DIRECTION('',(-1.,-1.59148942750166E-16,0.)) ;
#88534 = DIRECTION('center_axis',(-1.,-1.53063836115601E-16,0.)) ;
#88535 = DIRECTION('ref_axis',(1.53063836115601E-16,-1.,0.)) ;
#88536 = DIRECTION('',(0.,0.,1.)) ;
#88537 = DIRECTION('',(-1.53063836115601E-16,1.,-1.020425574104E-16)) ;
#88538 = DIRECTION('',(0.,0.,-1.)) ;
#88539 = DIRECTION('',(1.53063836115601E-16,-1.,5.10212787052002E-17)) ;
#88540 = DIRECTION('',(0.,0.,1.)) ;
#88541 = DIRECTION('',(-1.53063836115601E-16,1.,-1.30104260698261E-16)) ;
#88542 = DIRECTION('center_axis',(-1.,-1.53063836115601E-16,0.)) ;
#88543 = DIRECTION('ref_axis',(1.53063836115601E-16,-1.,0.)) ;
#88544 = DIRECTION('',(0.,0.,1.)) ;
#88545 = DIRECTION('center_axis',(-1.,-1.53063836115601E-16,0.)) ;
#88546 = DIRECTION('ref_axis',(1.53063836115601E-16,-1.,0.)) ;
#88547 = DIRECTION('',(1.53063836115601E-16,-1.,-1.30104260698261E-16)) ;
#88548 = DIRECTION('center_axis',(-1.53063836115601E-16,1.,0.)) ;
#88549 = DIRECTION('ref_axis',(-1.,-1.53063836115601E-16,0.)) ;
#88550 = DIRECTION('',(-1.,-1.53063836115601E-16,2.73691106313441E-48)) ;
#88551 = DIRECTION('',(0.,0.,-1.)) ;
#88552 = DIRECTION('',(1.,1.53063836115601E-16,-1.53236300070382E-33)) ;
#88553 = DIRECTION('',(0.,0.,1.)) ;
#88554 = DIRECTION('center_axis',(1.99142572374599E-32,-1.30104260698261E-16,
-1.)) ;
#88555 = DIRECTION('ref_axis',(0.,1.,-1.30104260698261E-16)) ;
#88556 = DIRECTION('',(-1.,-1.53063836115601E-16,2.73691106313441E-48)) ;
#88557 = DIRECTION('',(1.53063836115601E-16,-1.,1.30104260698261E-16)) ;
#88558 = DIRECTION('',(1.,1.53063836115601E-16,-2.73691106313441E-48)) ;
#88559 = DIRECTION('center_axis',(-1.53063836115601E-16,1.,0.)) ;
#88560 = DIRECTION('ref_axis',(-1.,-1.53063836115601E-16,0.)) ;
#88561 = DIRECTION('',(-1.,-1.53063836115601E-16,-2.73691106313441E-48)) ;
#88562 = DIRECTION('',(0.,0.,-1.)) ;
#88563 = DIRECTION('',(1.,1.53063836115601E-16,-2.73691106313441E-48)) ;
#88564 = DIRECTION('',(0.,0.,1.)) ;
#88565 = DIRECTION('center_axis',(1.99142572374599E-32,-1.30104260698261E-16,
1.)) ;
#88566 = DIRECTION('ref_axis',(0.,-1.,-1.30104260698261E-16)) ;
#88567 = DIRECTION('',(-1.,-1.53063836115601E-16,-2.73691106313441E-48)) ;
#88568 = DIRECTION('',(-1.53063836115601E-16,1.,1.30104260698261E-16)) ;
#88569 = DIRECTION('',(1.,1.53063836115601E-16,2.73691106313441E-48)) ;
#88570 = DIRECTION('',(2.16840434497101E-16,-1.,-1.30104260698261E-16)) ;
#88571 = DIRECTION('center_axis',(-1.53063836115601E-16,1.,0.)) ;
#88572 = DIRECTION('ref_axis',(-1.,-1.53063836115601E-16,0.)) ;
#88573 = DIRECTION('',(-1.,-1.53063836115601E-16,3.06472600140763E-33)) ;
#88574 = DIRECTION('',(0.,0.,-1.)) ;
#88575 = DIRECTION('',(1.,1.53063836115601E-16,2.73691106313441E-48)) ;
#88576 = DIRECTION('',(0.,0.,1.)) ;
#88577 = DIRECTION('center_axis',(1.,0.,0.)) ;
#88578 = DIRECTION('ref_axis',(0.,0.,-1.)) ;
#88579 = DIRECTION('',(1.,0.,0.)) ;
#88580 = DIRECTION('center_axis',(1.,0.,0.)) ;
#88581 = DIRECTION('ref_axis',(0.,0.,1.)) ;
#88582 = DIRECTION('',(1.,0.,0.)) ;
#88583 = DIRECTION('center_axis',(-1.,0.,0.)) ;
#88584 = DIRECTION('ref_axis',(0.,0.,-1.)) ;
#88585 = DIRECTION('center_axis',(0.,0.,1.)) ;
#88586 = DIRECTION('ref_axis',(1.,0.,0.)) ;
#88587 = DIRECTION('',(0.,1.,0.)) ;
#88588 = DIRECTION('',(1.,0.,0.)) ;
#88589 = DIRECTION('',(0.,-1.,0.)) ;
#88590 = DIRECTION('center_axis',(1.,0.,0.)) ;
#88591 = DIRECTION('ref_axis',(0.,0.,-1.)) ;
#88592 = DIRECTION('center_axis',(1.,0.,0.)) ;
#88593 = DIRECTION('ref_axis',(0.,0.,1.)) ;
#88594 = DIRECTION('',(1.,0.,0.)) ;
#88595 = DIRECTION('center_axis',(-1.,0.,0.)) ;
#88596 = DIRECTION('ref_axis',(0.,0.,-1.)) ;
#88597 = DIRECTION('center_axis',(0.,-1.,3.99416362155027E-15)) ;
#88598 = DIRECTION('ref_axis',(0.,-3.99416362155027E-15,-1.)) ;
#88599 = DIRECTION('',(0.,3.99416362155027E-15,1.)) ;
#88600 = DIRECTION('',(1.,0.,0.)) ;
#88601 = DIRECTION('',(0.,-3.99416362155027E-15,-1.)) ;
#88602 = DIRECTION('center_axis',(1.,0.,0.)) ;
#88603 = DIRECTION('ref_axis',(0.,0.,-1.)) ;
#88604 = DIRECTION('center_axis',(-1.,0.,0.)) ;
#88605 = DIRECTION('ref_axis',(0.,0.,-1.)) ;
#88606 = DIRECTION('',(1.,0.,0.)) ;
#88607 = DIRECTION('center_axis',(1.,0.,0.)) ;
#88608 = DIRECTION('ref_axis',(0.,0.,-1.)) ;
#88609 = DIRECTION('center_axis',(0.,-0.707106781186549,0.707106781186546)) ;
#88610 = DIRECTION('ref_axis',(0.,-0.707106781186546,-0.707106781186549)) ;
#88611 = DIRECTION('',(0.,0.707106781186546,0.707106781186549)) ;
#88612 = DIRECTION('',(1.,0.,0.)) ;
#88613 = DIRECTION('',(0.,-0.707106781186546,-0.707106781186549)) ;
#88614 = DIRECTION('center_axis',(1.,0.,0.)) ;
#88615 = DIRECTION('ref_axis',(0.,0.382683432365091,0.923879532511286)) ;
#88616 = DIRECTION('',(1.,0.,0.)) ;
#88617 = DIRECTION('center_axis',(1.,0.,0.)) ;
#88618 = DIRECTION('ref_axis',(0.,0.,-1.)) ;
#88619 = DIRECTION('center_axis',(0.,1.,0.)) ;
#88620 = DIRECTION('ref_axis',(0.,0.,1.)) ;
#88621 = DIRECTION('',(0.,0.,-1.)) ;
#88622 = DIRECTION('',(0.,0.,1.)) ;
#88623 = DIRECTION('center_axis',(0.,-0.707106781186547,-0.707106781186548)) ;
#88624 = DIRECTION('ref_axis',(0.,0.707106781186548,-0.707106781186547)) ;
#88625 = DIRECTION('',(0.,-0.707106781186548,0.707106781186547)) ;
#88626 = DIRECTION('',(1.,0.,0.)) ;
#88627 = DIRECTION('',(0.,0.707106781186548,-0.707106781186547)) ;
#88628 = DIRECTION('center_axis',(1.,0.,0.)) ;
#88629 = DIRECTION('ref_axis',(0.,0.,-1.)) ;
#88630 = DIRECTION('center_axis',(-1.,0.,0.)) ;
#88631 = DIRECTION('ref_axis',(0.,0.,-1.)) ;
#88632 = DIRECTION('',(1.,0.,0.)) ;
#88633 = DIRECTION('center_axis',(1.,0.,0.)) ;
#88634 = DIRECTION('ref_axis',(0.,0.,-1.)) ;
#88635 = DIRECTION('center_axis',(0.,-1.,0.)) ;
#88636 = DIRECTION('ref_axis',(0.,0.,-1.)) ;
#88637 = DIRECTION('',(0.,0.,1.)) ;
#88638 = DIRECTION('',(1.,0.,0.)) ;
#88639 = DIRECTION('',(0.,0.,-1.)) ;
#88640 = DIRECTION('center_axis',(1.,0.,0.)) ;
#88641 = DIRECTION('ref_axis',(0.,0.,-1.)) ;
#88642 = DIRECTION('center_axis',(1.,0.,0.)) ;
#88643 = DIRECTION('ref_axis',(0.,0.,1.)) ;
#88644 = DIRECTION('',(1.,0.,0.)) ;
#88645 = DIRECTION('center_axis',(-1.,0.,0.)) ;
#88646 = DIRECTION('ref_axis',(0.,0.,-1.)) ;
#88647 = DIRECTION('center_axis',(0.,0.,-1.)) ;
#88648 = DIRECTION('ref_axis',(-1.,0.,0.)) ;
#88649 = DIRECTION('',(0.,-1.,0.)) ;
#88650 = DIRECTION('',(1.,0.,0.)) ;
#88651 = DIRECTION('',(0.,1.,0.)) ;
#88652 = DIRECTION('center_axis',(1.,0.,0.)) ;
#88653 = DIRECTION('ref_axis',(0.,0.,-1.)) ;
#88654 = DIRECTION('center_axis',(1.,0.,0.)) ;
#88655 = DIRECTION('ref_axis',(0.,0.,1.)) ;
#88656 = DIRECTION('',(1.,0.,0.)) ;
#88657 = DIRECTION('center_axis',(-1.,0.,0.)) ;
#88658 = DIRECTION('ref_axis',(0.,0.,-1.)) ;
#88659 = DIRECTION('center_axis',(0.,1.,0.)) ;
#88660 = DIRECTION('ref_axis',(0.,0.,1.)) ;
#88661 = DIRECTION('',(0.,0.,-1.)) ;
#88662 = DIRECTION('',(1.,0.,0.)) ;
#88663 = DIRECTION('',(0.,0.,1.)) ;
#88664 = DIRECTION('center_axis',(1.,0.,0.)) ;
#88665 = DIRECTION('ref_axis',(0.,0.,-1.)) ;
#88666 = DIRECTION('center_axis',(-1.,0.,0.)) ;
#88667 = DIRECTION('ref_axis',(0.,1.51788304147971E-14,-1.)) ;
#88668 = DIRECTION('',(1.,0.,0.)) ;
#88669 = DIRECTION('center_axis',(1.,0.,0.)) ;
#88670 = DIRECTION('ref_axis',(0.,0.,-1.)) ;
#88671 = DIRECTION('center_axis',(0.,1.07081696047951E-16,-1.)) ;
#88672 = DIRECTION('ref_axis',(0.,1.,1.07081696047951E-16)) ;
#88673 = DIRECTION('',(0.,-1.,-1.07081696047951E-16)) ;
#88674 = DIRECTION('',(1.,0.,0.)) ;
#88675 = DIRECTION('',(0.,1.,1.07081696047951E-16)) ;
#88676 = DIRECTION('center_axis',(1.,0.,0.)) ;
#88677 = DIRECTION('ref_axis',(0.,0.,-1.)) ;
#88678 = DIRECTION('center_axis',(-1.,0.,0.)) ;
#88679 = DIRECTION('ref_axis',(0.,0.,-1.)) ;
#88680 = DIRECTION('',(1.,0.,0.)) ;
#88681 = DIRECTION('center_axis',(1.,0.,0.)) ;
#88682 = DIRECTION('ref_axis',(0.,0.,-1.)) ;
#88683 = DIRECTION('center_axis',(0.,-1.,0.)) ;
#88684 = DIRECTION('ref_axis',(0.,0.,-1.)) ;
#88685 = DIRECTION('',(0.,0.,1.)) ;
#88686 = DIRECTION('',(1.,0.,0.)) ;
#88687 = DIRECTION('',(0.,0.,-1.)) ;
#88688 = DIRECTION('center_axis',(1.,0.,0.)) ;
#88689 = DIRECTION('ref_axis',(0.,0.,-1.)) ;
#88690 = DIRECTION('center_axis',(-1.,0.,0.)) ;
#88691 = DIRECTION('ref_axis',(0.,0.,-1.)) ;
#88692 = DIRECTION('',(1.,0.,0.)) ;
#88693 = DIRECTION('center_axis',(1.,0.,0.)) ;
#88694 = DIRECTION('ref_axis',(0.,0.,-1.)) ;
#88695 = DIRECTION('center_axis',(1.,0.,0.)) ;
#88696 = DIRECTION('ref_axis',(0.,0.,-1.)) ;
#88697 = DIRECTION('center_axis',(1.,0.,0.)) ;
#88698 = DIRECTION('ref_axis',(0.,0.,1.)) ;
#88699 = DIRECTION('',(1.,0.,0.)) ;
#88700 = DIRECTION('center_axis',(-1.,0.,0.)) ;
#88701 = DIRECTION('ref_axis',(0.,0.,-1.)) ;
#88702 = DIRECTION('center_axis',(1.,0.,0.)) ;
#88703 = DIRECTION('ref_axis',(0.,0.,-1.)) ;
#88704 = DIRECTION('center_axis',(-1.,0.,0.)) ;
#88705 = DIRECTION('ref_axis',(0.,0.,-1.)) ;
#88706 = DIRECTION('',(1.,0.,0.)) ;
#88707 = DIRECTION('center_axis',(1.,0.,0.)) ;
#88708 = DIRECTION('ref_axis',(0.,0.,-1.)) ;
#88709 = DIRECTION('center_axis',(0.,-1.,0.)) ;
#88710 = DIRECTION('ref_axis',(0.,0.,-1.)) ;
#88711 = DIRECTION('',(0.,0.,1.)) ;
#88712 = DIRECTION('',(1.,0.,0.)) ;
#88713 = DIRECTION('',(0.,0.,-1.)) ;
#88714 = DIRECTION('center_axis',(1.,0.,0.)) ;
#88715 = DIRECTION('ref_axis',(0.,0.,-1.)) ;
#88716 = DIRECTION('center_axis',(-1.,0.,0.)) ;
#88717 = DIRECTION('ref_axis',(0.,0.,-1.)) ;
#88718 = DIRECTION('',(1.,0.,0.)) ;
#88719 = DIRECTION('center_axis',(1.,0.,0.)) ;
#88720 = DIRECTION('ref_axis',(0.,0.,-1.)) ;
#88721 = DIRECTION('center_axis',(0.,-1.07081696047951E-16,1.)) ;
#88722 = DIRECTION('ref_axis',(0.,-1.,-1.07081696047951E-16)) ;
#88723 = DIRECTION('',(0.,1.,1.07081696047951E-16)) ;
#88724 = DIRECTION('',(1.,0.,0.)) ;
#88725 = DIRECTION('',(0.,-1.,-1.07081696047951E-16)) ;
#88726 = DIRECTION('center_axis',(1.,0.,0.)) ;
#88727 = DIRECTION('ref_axis',(0.,0.,-1.)) ;
#88728 = DIRECTION('center_axis',(-1.,0.,0.)) ;
#88729 = DIRECTION('ref_axis',(0.,0.,-1.)) ;
#88730 = DIRECTION('',(1.,0.,0.)) ;
#88731 = DIRECTION('center_axis',(1.,0.,0.)) ;
#88732 = DIRECTION('ref_axis',(0.,0.,-1.)) ;
#88733 = DIRECTION('center_axis',(0.,1.,0.)) ;
#88734 = DIRECTION('ref_axis',(0.,0.,1.)) ;
#88735 = DIRECTION('',(0.,0.,-1.)) ;
#88736 = DIRECTION('',(0.,0.,1.)) ;
#88737 = DIRECTION('center_axis',(-1.,0.,0.)) ;
#88738 = DIRECTION('ref_axis',(0.,0.,1.)) ;
#88739 = DIRECTION('center_axis',(-1.,0.,0.)) ;
#88740 = DIRECTION('ref_axis',(0.,0.,1.)) ;
#88741 = DIRECTION('',(0.,-1.,0.)) ;
#88742 = DIRECTION('center_axis',(-1.,0.,0.)) ;
#88743 = DIRECTION('ref_axis',(0.,0.,1.)) ;
#88744 = DIRECTION('',(0.,0.,1.)) ;
#88745 = DIRECTION('',(0.,-1.,-1.07081696047951E-16)) ;
#88746 = DIRECTION('',(0.,0.,-1.)) ;
#88747 = DIRECTION('center_axis',(-1.,0.,0.)) ;
#88748 = DIRECTION('ref_axis',(0.,0.,1.)) ;
#88749 = DIRECTION('',(0.,0.,-1.)) ;
#88750 = DIRECTION('',(0.,1.,1.07081696047951E-16)) ;
#88751 = DIRECTION('',(0.,0.,1.)) ;
#88752 = DIRECTION('center_axis',(-1.,0.,0.)) ;
#88753 = DIRECTION('ref_axis',(0.,0.,1.)) ;
#88754 = DIRECTION('',(0.,1.,0.)) ;
#88755 = DIRECTION('center_axis',(-1.,0.,0.)) ;
#88756 = DIRECTION('ref_axis',(0.,0.,1.)) ;
#88757 = DIRECTION('',(0.,0.,-1.)) ;
#88758 = DIRECTION('',(0.,0.707106781186548,-0.707106781186547)) ;
#88759 = DIRECTION('',(0.,0.,1.)) ;
#88760 = DIRECTION('',(0.,-0.707106781186546,-0.707106781186549)) ;
#88761 = DIRECTION('',(0.,-3.99416362155027E-15,-1.)) ;
#88762 = DIRECTION('center_axis',(1.,0.,0.)) ;
#88763 = DIRECTION('ref_axis',(0.,0.,-1.)) ;
#88764 = DIRECTION('',(0.,-1.,0.)) ;
#88765 = DIRECTION('center_axis',(-1.,0.,0.)) ;
#88766 = DIRECTION('ref_axis',(0.,0.,-1.)) ;
#88767 = DIRECTION('',(0.,0.,-1.)) ;
#88768 = DIRECTION('center_axis',(-1.,0.,0.)) ;
#88769 = DIRECTION('ref_axis',(0.,-1.0842021724855E-15,-1.)) ;
#88770 = DIRECTION('',(0.,-1.,0.)) ;
#88771 = DIRECTION('center_axis',(-1.,0.,0.)) ;
#88772 = DIRECTION('ref_axis',(0.,0.,-1.)) ;
#88773 = DIRECTION('',(0.,0.,1.)) ;
#88774 = DIRECTION('center_axis',(-1.,0.,0.)) ;
#88775 = DIRECTION('ref_axis',(0.,0.,-1.)) ;
#88776 = DIRECTION('center_axis',(1.53063836115601E-16,-1.,-1.30104260698261E-16)) ;
#88777 = DIRECTION('ref_axis',(1.,1.53063836115601E-16,1.99142572374599E-32)) ;
#88778 = DIRECTION('center_axis',(0.,1.,0.)) ;
#88779 = DIRECTION('ref_axis',(0.,0.,1.)) ;
#88780 = DIRECTION('center_axis',(0.,-1.,0.)) ;
#88781 = DIRECTION('ref_axis',(0.,0.,-1.)) ;
#88782 = DIRECTION('center_axis',(1.,1.53063836115601E-16,2.73691106313441E-48)) ;
#88783 = DIRECTION('ref_axis',(-1.53063836115601E-16,1.,-4.18922106430579E-64)) ;
#88784 = DIRECTION('center_axis',(-1.,0.,0.)) ;
#88785 = DIRECTION('ref_axis',(0.,0.,1.)) ;
#88786 = DIRECTION('center_axis',(1.,1.53063836115601E-16,0.)) ;
#88787 = DIRECTION('ref_axis',(1.53063836115601E-16,-1.,0.)) ;
#88788 = DIRECTION('center_axis',(0.,1.,0.)) ;
#88789 = DIRECTION('ref_axis',(1.,0.,0.)) ;
#88790 = DIRECTION('center_axis',(0.,1.,0.)) ;
#88791 = DIRECTION('ref_axis',(0.,0.,-1.)) ;
#88792 = DIRECTION('center_axis',(0.,0.,1.)) ;
#88793 = DIRECTION('ref_axis',(-1.,0.,0.)) ;
#88794 = DIRECTION('center_axis',(0.,1.,0.)) ;
#88795 = DIRECTION('ref_axis',(1.,0.,0.)) ;
#88796 = DIRECTION('center_axis',(0.,0.,1.)) ;
#88797 = DIRECTION('ref_axis',(-1.,0.,0.)) ;
#88798 = DIRECTION('center_axis',(1.,1.0842021724855E-15,0.)) ;
#88799 = DIRECTION('ref_axis',(1.0842021724855E-15,-1.,0.)) ;
#88800 = DIRECTION('center_axis',(-1.,-1.53063836115601E-16,0.)) ;
#88801 = DIRECTION('ref_axis',(0.,-1.,0.)) ;
#88802 = DIRECTION('center_axis',(0.,0.,-1.)) ;
#88803 = DIRECTION('ref_axis',(1.,0.,0.)) ;
#88804 = DIRECTION('center_axis',(0.,0.,-1.)) ;
#88805 = DIRECTION('ref_axis',(0.804034447892617,0.594582716366709,0.)) ;
#88806 = DIRECTION('center_axis',(0.,0.,1.)) ;
#88807 = DIRECTION('ref_axis',(1.,0.,0.)) ;
#88808 = DIRECTION('',(0.,0.,-1.)) ;
#88809 = DIRECTION('center_axis',(-2.16840434497101E-16,1.,1.30104260698261E-16)) ;
#88810 = DIRECTION('ref_axis',(1.,2.16840434497101E-16,1.22464679914735E-16)) ;
#88811 = DIRECTION('',(-2.16840434497101E-16,1.,1.30104260698261E-16)) ;
#88812 = DIRECTION('center_axis',(0.,1.,0.)) ;
#88813 = DIRECTION('ref_axis',(0.,0.,1.)) ;
#88814 = DIRECTION('center_axis',(-1.,-1.53063836115601E-16,-2.73691106313441E-48)) ;
#88815 = DIRECTION('ref_axis',(1.53063836115601E-16,-1.,4.18922106430579E-64)) ;
#88816 = DIRECTION('center_axis',(1.,2.16840434497101E-16,0.)) ;
#88817 = DIRECTION('ref_axis',(2.16840434497101E-16,-1.,0.)) ;
#88818 = DIRECTION('center_axis',(0.,0.,1.)) ;
#88819 = DIRECTION('ref_axis',(1.,0.,0.)) ;
#88820 = DIRECTION('center_axis',(-1.25542992828747E-32,1.020425574104E-16,
1.)) ;
#88821 = DIRECTION('ref_axis',(-1.28107280532009E-48,-1.,1.020425574104E-16)) ;
#88822 = DIRECTION('center_axis',(0.,0.,1.)) ;
#88823 = DIRECTION('ref_axis',(1.,0.,0.)) ;
#88824 = DIRECTION('center_axis',(0.,0.,-1.)) ;
#88825 = DIRECTION('ref_axis',(-1.,0.,0.)) ;
#88826 = DIRECTION('center_axis',(1.,1.53063836115601E-16,-2.73691106313441E-48)) ;
#88827 = DIRECTION('ref_axis',(-1.53063836115601E-16,1.,4.18922106430579E-64)) ;
#88828 = DIRECTION('center_axis',(-1.,0.,0.)) ;
#88829 = DIRECTION('ref_axis',(0.,0.,1.)) ;
#88830 = DIRECTION('center_axis',(1.,1.53063836115601E-16,0.)) ;
#88831 = DIRECTION('ref_axis',(1.53063836115601E-16,-1.,0.)) ;
#88832 = DIRECTION('center_axis',(0.,1.,0.)) ;
#88833 = DIRECTION('ref_axis',(1.,0.,0.)) ;
#88834 = DIRECTION('center_axis',(-1.,-2.16840434497101E-16,0.)) ;
#88835 = DIRECTION('ref_axis',(0.,-1.,0.)) ;
#88836 = DIRECTION('center_axis',(0.,0.,-1.)) ;
#88837 = DIRECTION('ref_axis',(1.,0.,0.)) ;
#88838 = DIRECTION('center_axis',(-1.25542992828747E-32,1.020425574104E-16,
1.)) ;
#88839 = DIRECTION('ref_axis',(0.,-1.,0.)) ;
#88840 = DIRECTION('center_axis',(0.,-1.,0.)) ;
#88841 = DIRECTION('ref_axis',(-6.50521303491302E-15,0.,1.)) ;
#88842 = DIRECTION('center_axis',(-1.,0.,0.)) ;
#88843 = DIRECTION('ref_axis',(0.,0.,-1.)) ;
#88844 = DIRECTION('center_axis',(-1.,-1.53063836115601E-16,0.)) ;
#88845 = DIRECTION('ref_axis',(0.,-1.,0.)) ;
#88846 = DIRECTION('center_axis',(0.,-1.,0.)) ;
#88847 = DIRECTION('ref_axis',(0.,0.,1.)) ;
#88848 = DIRECTION('center_axis',(0.,0.,-1.)) ;
#88849 = DIRECTION('ref_axis',(-1.,0.,0.)) ;
#88850 = DIRECTION('center_axis',(0.,0.,-1.)) ;
#88851 = DIRECTION('ref_axis',(-1.,0.,0.)) ;
#88852 = DIRECTION('center_axis',(1.,1.53063836115601E-16,-3.06472600140763E-33)) ;
#88853 = DIRECTION('ref_axis',(-1.53063836115601E-16,1.,4.69098718418678E-49)) ;
#88854 = DIRECTION('center_axis',(-1.,0.,0.)) ;
#88855 = DIRECTION('ref_axis',(0.,0.,1.)) ;
#88856 = DIRECTION('center_axis',(-1.53063836115601E-16,1.,-1.020425574104E-16)) ;
#88857 = DIRECTION('ref_axis',(-1.,-1.53063836115601E-16,1.3684555315672E-47)) ;
#88858 = DIRECTION('',(1.53063836115601E-16,-1.,1.020425574104E-16)) ;
#88859 = DIRECTION('center_axis',(0.,-1.,0.)) ;
#88860 = DIRECTION('ref_axis',(0.,0.,-1.)) ;
#88861 = DIRECTION('center_axis',(-1.53063836115601E-16,1.,-1.30104260698261E-16)) ;
#88862 = DIRECTION('ref_axis',(-1.,-1.53063836115601E-16,1.99142572374599E-32)) ;
#88863 = DIRECTION('center_axis',(0.,-1.,0.)) ;
#88864 = DIRECTION('ref_axis',(0.,0.,-1.)) ;
#88865 = DIRECTION('center_axis',(-1.,-1.53063836115601E-16,2.73691106313441E-48)) ;
#88866 = DIRECTION('ref_axis',(1.53063836115601E-16,-1.,-4.18922106430579E-64)) ;
#88867 = DIRECTION('center_axis',(1.,2.16840434497101E-16,0.)) ;
#88868 = DIRECTION('ref_axis',(2.16840434497101E-16,-1.,0.)) ;
#88869 = DIRECTION('center_axis',(-1.,0.,2.16840434497101E-15)) ;
#88870 = DIRECTION('ref_axis',(2.16840434497101E-15,0.,1.)) ;
#88871 = DIRECTION('center_axis',(-1.,-2.16840434497101E-16,0.)) ;
#88872 = DIRECTION('ref_axis',(0.,-1.,0.)) ;
#88873 = DIRECTION('center_axis',(0.,0.,1.)) ;
#88874 = DIRECTION('ref_axis',(-1.,0.,0.)) ;
#88875 = DIRECTION('center_axis',(0.,1.,0.)) ;
#88876 = DIRECTION('ref_axis',(1.,0.,0.)) ;
#88877 = DIRECTION('center_axis',(0.,1.,0.)) ;
#88878 = DIRECTION('ref_axis',(0.,0.,-1.)) ;
#88879 = DIRECTION('center_axis',(1.,0.,0.)) ;
#88880 = DIRECTION('ref_axis',(0.,-1.,0.)) ;
#88881 = DIRECTION('center_axis',(1.,6.50521303491304E-15,0.)) ;
#88882 = DIRECTION('ref_axis',(-6.50521303491304E-15,1.,0.)) ;
#88883 = DIRECTION('center_axis',(8.67361737988403E-15,1.,0.)) ;
#88884 = DIRECTION('ref_axis',(-1.,8.67361737988403E-15,0.)) ;
#88885 = DIRECTION('center_axis',(1.2303003375722E-16,-1.,1.020425574104E-16)) ;
#88886 = DIRECTION('ref_axis',(1.,1.2303003375722E-16,-1.25542992828747E-32)) ;
#88887 = DIRECTION('center_axis',(0.,1.,0.)) ;
#88888 = DIRECTION('ref_axis',(0.,0.,1.)) ;
#88889 = DIRECTION('center_axis',(0.,1.,0.)) ;
#88890 = DIRECTION('ref_axis',(1.,0.,0.)) ;
#88891 = DIRECTION('center_axis',(1.,1.2303003375722E-16,0.)) ;
#88892 = DIRECTION('ref_axis',(1.2303003375722E-16,-1.,0.)) ;
#88893 = DIRECTION('center_axis',(-2.16840434497101E-15,0.,1.)) ;
#88894 = DIRECTION('ref_axis',(-1.,0.,-2.16840434497101E-15)) ;
#88895 = DIRECTION('center_axis',(0.,1.,0.)) ;
#88896 = DIRECTION('ref_axis',(1.,0.,0.)) ;
#88897 = DIRECTION('center_axis',(0.,0.,-1.)) ;
#88898 = DIRECTION('ref_axis',(1.,0.,0.)) ;
#88899 = DIRECTION('center_axis',(0.,0.,-1.)) ;
#88900 = DIRECTION('ref_axis',(-1.,0.,0.)) ;
#88901 = DIRECTION('center_axis',(0.,0.,1.)) ;
#88902 = DIRECTION('ref_axis',(1.,0.,0.)) ;
#88903 = DIRECTION('center_axis',(-2.16840434497101E-16,1.,-1.020425574104E-16)) ;
#88904 = DIRECTION('ref_axis',(-1.,-2.16840434497101E-16,5.47382212626882E-48)) ;
#88905 = DIRECTION('center_axis',(0.,1.,0.)) ;
#88906 = DIRECTION('ref_axis',(0.,0.,-1.)) ;
#88907 = DIRECTION('center_axis',(1.,0.,1.25542992828747E-32)) ;
#88908 = DIRECTION('ref_axis',(1.25542992828747E-32,0.,-1.)) ;
#88909 = DIRECTION('center_axis',(1.,0.,0.)) ;
#88910 = DIRECTION('ref_axis',(0.,0.,-1.)) ;
#88911 = DIRECTION('center_axis',(-1.,-1.2303003375722E-16,0.)) ;
#88912 = DIRECTION('ref_axis',(0.,-1.,0.)) ;
#88913 = DIRECTION('center_axis',(0.,0.,-1.)) ;
#88914 = DIRECTION('ref_axis',(1.,0.,0.)) ;
#88915 = DIRECTION('center_axis',(0.,0.,-1.)) ;
#88916 = DIRECTION('ref_axis',(-1.,0.,0.)) ;
#88917 = DIRECTION('',(0.,0.,1.)) ;
#88918 = DIRECTION('center_axis',(0.,-2.16840434497101E-15,1.)) ;
#88919 = DIRECTION('ref_axis',(0.,-1.,-2.16840434497101E-15)) ;
#88920 = DIRECTION('center_axis',(0.,0.,1.)) ;
#88921 = DIRECTION('ref_axis',(1.,0.,0.)) ;
#88922 = DIRECTION('center_axis',(6.27714964143733E-33,-5.10212787052002E-17,
-1.)) ;
#88923 = DIRECTION('ref_axis',(3.20268201330022E-49,1.,-5.10212787052002E-17)) ;
#88924 = DIRECTION('center_axis',(1.,1.53063836115601E-16,-1.53236300070382E-33)) ;
#88925 = DIRECTION('ref_axis',(-1.53063836115601E-16,1.,2.34549359209339E-49)) ;
#88926 = DIRECTION('center_axis',(-1.,0.,0.)) ;
#88927 = DIRECTION('ref_axis',(0.,0.,1.)) ;
#88928 = DIRECTION('center_axis',(1.,0.,0.)) ;
#88929 = DIRECTION('ref_axis',(0.,0.,-1.)) ;
#88930 = DIRECTION('center_axis',(0.,1.,0.)) ;
#88931 = DIRECTION('ref_axis',(1.,0.,0.)) ;
#88932 = DIRECTION('center_axis',(-4.33680868994202E-15,1.,0.)) ;
#88933 = DIRECTION('ref_axis',(1.,4.33680868994202E-15,0.)) ;
#88934 = DIRECTION('center_axis',(0.,-1.,0.)) ;
#88935 = DIRECTION('ref_axis',(0.,0.,-1.)) ;
#88936 = DIRECTION('center_axis',(0.,0.,-1.)) ;
#88937 = DIRECTION('ref_axis',(1.,0.,0.)) ;
#88938 = DIRECTION('center_axis',(0.,0.,1.)) ;
#88939 = DIRECTION('ref_axis',(1.,0.,0.)) ;
#88940 = DIRECTION('center_axis',(0.,0.,-1.)) ;
#88941 = DIRECTION('ref_axis',(-1.,0.,0.)) ;
#88942 = DIRECTION('center_axis',(0.,1.,0.)) ;
#88943 = DIRECTION('ref_axis',(1.,0.,0.)) ;
#88944 = DIRECTION('center_axis',(1.,1.2303003375722E-16,0.)) ;
#88945 = DIRECTION('ref_axis',(1.2303003375722E-16,-1.,0.)) ;
#88946 = DIRECTION('center_axis',(0.,1.,0.)) ;
#88947 = DIRECTION('ref_axis',(-6.50521303491302E-15,0.,-1.)) ;
#88948 = DIRECTION('center_axis',(6.27714964143733E-33,-5.10212787052002E-17,
-1.)) ;
#88949 = DIRECTION('ref_axis',(0.,1.,0.)) ;
#88950 = DIRECTION('center_axis',(0.,-1.,0.)) ;
#88951 = DIRECTION('ref_axis',(0.,0.,1.)) ;
#88952 = DIRECTION('center_axis',(2.16840434497101E-16,-1.,5.10212787052002E-17)) ;
#88953 = DIRECTION('ref_axis',(1.,2.16840434497101E-16,-5.47382212626882E-48)) ;
#88954 = DIRECTION('center_axis',(0.,1.,0.)) ;
#88955 = DIRECTION('ref_axis',(0.,0.,-1.)) ;
#88956 = DIRECTION('center_axis',(0.,0.,1.)) ;
#88957 = DIRECTION('ref_axis',(1.,0.,0.)) ;
#88958 = DIRECTION('center_axis',(0.,0.,-1.)) ;
#88959 = DIRECTION('ref_axis',(-1.,0.,0.)) ;
#88960 = DIRECTION('center_axis',(-1.,-1.2303003375722E-16,0.)) ;
#88961 = DIRECTION('ref_axis',(0.,-1.,0.)) ;
#88962 = DIRECTION('center_axis',(0.,-1.,0.)) ;
#88963 = DIRECTION('ref_axis',(0.,0.,1.)) ;
#88964 = DIRECTION('center_axis',(1.53063836115601E-16,-1.,5.10212787052002E-17)) ;
#88965 = DIRECTION('ref_axis',(1.,1.53063836115601E-16,-6.84227765783602E-48)) ;
#88966 = DIRECTION('',(-1.53063836115601E-16,1.,-5.10212787052002E-17)) ;
#88967 = DIRECTION('center_axis',(0.,-1.,0.)) ;
#88968 = DIRECTION('ref_axis',(0.,0.,-1.)) ;
#88969 = DIRECTION('center_axis',(-1.,0.,0.)) ;
#88970 = DIRECTION('ref_axis',(0.,0.,-1.)) ;
#88971 = DIRECTION('center_axis',(-1.2303003375722E-16,1.,-5.10212787052002E-17)) ;
#88972 = DIRECTION('ref_axis',(-1.,-1.2303003375722E-16,6.27714964143733E-33)) ;
#88973 = DIRECTION('center_axis',(-8.67361737988403E-15,-1.,0.)) ;
#88974 = DIRECTION('ref_axis',(1.,-8.67361737988403E-15,0.)) ;
#88975 = DIRECTION('center_axis',(1.,0.,6.27714964143733E-33)) ;
#88976 = DIRECTION('ref_axis',(6.27714964143733E-33,0.,-1.)) ;
#88977 = DIRECTION('center_axis',(-1.,0.,-6.5052130349128E-15)) ;
#88978 = DIRECTION('ref_axis',(-6.5052130349128E-15,0.,1.)) ;
#88979 = DIRECTION('center_axis',(1.,0.,0.)) ;
#88980 = DIRECTION('ref_axis',(0.,1.,0.)) ;
#88981 = DIRECTION('center_axis',(0.,1.,0.)) ;
#88982 = DIRECTION('ref_axis',(1.,0.,0.)) ;
#88983 = DIRECTION('center_axis',(1.,0.,0.)) ;
#88984 = DIRECTION('ref_axis',(0.,0.,-1.)) ;
#88985 = DIRECTION('center_axis',(0.,-1.,0.)) ;
#88986 = DIRECTION('ref_axis',(0.,0.,-1.)) ;
#88987 = DIRECTION('center_axis',(0.,1.,0.)) ;
#88988 = DIRECTION('ref_axis',(0.,0.,1.)) ;
#88989 = DIRECTION('center_axis',(0.,-1.,0.)) ;
#88990 = DIRECTION('ref_axis',(0.,0.,-1.)) ;
#88991 = DIRECTION('center_axis',(1.,0.,0.)) ;
#88992 = DIRECTION('ref_axis',(0.,0.,-1.)) ;
#88993 = DIRECTION('center_axis',(1.,0.,0.)) ;
#88994 = DIRECTION('ref_axis',(0.,0.,-1.)) ;
#88995 = DIRECTION('center_axis',(0.,0.,1.)) ;
#88996 = DIRECTION('ref_axis',(1.,0.,0.)) ;
#88997 = DIRECTION('center_axis',(-1.,8.67361737988401E-15,-8.67361737988379E-15)) ;
#88998 = DIRECTION('ref_axis',(-8.67361737988401E-15,-1.,1.07724819444908E-44)) ;
#88999 = DIRECTION('center_axis',(0.,1.,0.)) ;
#89000 = DIRECTION('ref_axis',(1.,0.,0.)) ;
#89001 = DIRECTION('center_axis',(0.,-1.,0.)) ;
#89002 = DIRECTION('ref_axis',(0.,0.,-1.)) ;
#89003 = DIRECTION('center_axis',(1.,1.59148942750166E-16,0.)) ;
#89004 = DIRECTION('ref_axis',(-1.59148942750166E-16,1.,0.)) ;
#89005 = DIRECTION('center_axis',(-1.,0.,6.50521303491284E-15)) ;
#89006 = DIRECTION('ref_axis',(6.50521303491284E-15,0.,1.)) ;
#89007 = DIRECTION('center_axis',(-4.33680868994203E-15,-1.,0.)) ;
#89008 = DIRECTION('ref_axis',(1.,-4.33680868994203E-15,0.)) ;
#89009 = DIRECTION('center_axis',(-8.67361737988401E-15,-1.,0.)) ;
#89010 = DIRECTION('ref_axis',(1.,-8.67361737988401E-15,0.)) ;
#89011 = DIRECTION('center_axis',(0.,1.,0.)) ;
#89012 = DIRECTION('ref_axis',(1.,0.,0.)) ;
#89013 = DIRECTION('center_axis',(8.67361737988403E-15,-1.,0.)) ;
#89014 = DIRECTION('ref_axis',(1.,8.67361737988403E-15,0.)) ;
#89015 = DIRECTION('center_axis',(0.,0.,1.)) ;
#89016 = DIRECTION('ref_axis',(1.,0.,0.)) ;
#89017 = DIRECTION('center_axis',(1.,8.67361737988401E-15,0.)) ;
#89018 = DIRECTION('ref_axis',(-8.67361737988401E-15,1.,0.)) ;
#89019 = DIRECTION('center_axis',(-1.2303003375722E-16,1.,0.)) ;
#89020 = DIRECTION('ref_axis',(-1.,-1.2303003375722E-16,0.)) ;
#89021 = DIRECTION('center_axis',(0.,-1.,8.67361737988379E-15)) ;
#89022 = DIRECTION('ref_axis',(0.,-8.67361737988379E-15,-1.)) ;
#89023 = DIRECTION('center_axis',(1.,-5.88041856263325E-16,0.)) ;
#89024 = DIRECTION('ref_axis',(5.88041856263325E-16,1.,0.)) ;
#89025 = DIRECTION('center_axis',(1.,0.,0.)) ;
#89026 = DIRECTION('ref_axis',(0.,0.,-1.)) ;
#89027 = DIRECTION('center_axis',(0.,1.,0.)) ;
#89028 = DIRECTION('ref_axis',(1.,0.,0.)) ;
#89029 = DIRECTION('center_axis',(1.,6.50521303491304E-15,0.)) ;
#89030 = DIRECTION('ref_axis',(-6.50521303491304E-15,1.,0.)) ;
#89031 = DIRECTION('center_axis',(0.,1.,0.)) ;
#89032 = DIRECTION('ref_axis',(1.,0.,0.)) ;
#89033 = DIRECTION('center_axis',(0.,-1.,0.)) ;
#89034 = DIRECTION('ref_axis',(0.,0.,-1.)) ;
#89035 = DIRECTION('center_axis',(-1.,0.,0.)) ;
#89036 = DIRECTION('ref_axis',(0.,0.,1.)) ;
#89037 = DIRECTION('center_axis',(1.,0.,1.73472347597676E-14)) ;
#89038 = DIRECTION('ref_axis',(1.73472347597676E-14,0.,-1.)) ;
#89039 = DIRECTION('center_axis',(0.,-1.,0.)) ;
#89040 = DIRECTION('ref_axis',(0.,0.,-1.)) ;
#89041 = DIRECTION('center_axis',(8.67361737988409E-15,-1.,0.)) ;
#89042 = DIRECTION('ref_axis',(1.,8.67361737988409E-15,0.)) ;
#89043 = DIRECTION('center_axis',(0.,1.,0.)) ;
#89044 = DIRECTION('ref_axis',(1.,0.,0.)) ;
#89045 = DIRECTION('center_axis',(0.,1.,0.)) ;
#89046 = DIRECTION('ref_axis',(1.,0.,0.)) ;
#89047 = DIRECTION('center_axis',(1.,0.,0.)) ;
#89048 = DIRECTION('ref_axis',(0.,0.,-1.)) ;
#89049 = DIRECTION('center_axis',(0.,-1.,0.)) ;
#89050 = DIRECTION('ref_axis',(0.,0.,-1.)) ;
#89051 = DIRECTION('center_axis',(0.,-1.,0.)) ;
#89052 = DIRECTION('ref_axis',(0.,0.,-1.)) ;
#89053 = DIRECTION('center_axis',(0.,-1.,0.)) ;
#89054 = DIRECTION('ref_axis',(0.,0.,-1.)) ;
#89055 = DIRECTION('center_axis',(-1.,0.,0.)) ;
#89056 = DIRECTION('ref_axis',(0.,0.,1.)) ;
#89057 = DIRECTION('center_axis',(1.,0.,0.)) ;
#89058 = DIRECTION('ref_axis',(0.,0.,-1.)) ;
#89059 = DIRECTION('center_axis',(0.,0.,1.)) ;
#89060 = DIRECTION('ref_axis',(1.,0.,0.)) ;
#89061 = DIRECTION('center_axis',(-1.,0.,0.)) ;
#89062 = DIRECTION('ref_axis',(0.,0.,1.)) ;
#89063 = DIRECTION('center_axis',(0.,1.,0.)) ;
#89064 = DIRECTION('ref_axis',(1.,0.,0.)) ;
#89065 = DIRECTION('center_axis',(0.,-1.,0.)) ;
#89066 = DIRECTION('ref_axis',(0.,0.,-1.)) ;
#89067 = DIRECTION('center_axis',(-1.,-1.59148942750166E-16,0.)) ;
#89068 = DIRECTION('ref_axis',(1.59148942750166E-16,-1.,0.)) ;
#89069 = DIRECTION('center_axis',(-1.,6.50521303491307E-15,0.)) ;
#89070 = DIRECTION('ref_axis',(-6.50521303491307E-15,-1.,0.)) ;
#89071 = DIRECTION('center_axis',(4.33680868994203E-15,1.,0.)) ;
#89072 = DIRECTION('ref_axis',(-1.,4.33680868994203E-15,0.)) ;
#89073 = DIRECTION('center_axis',(-8.67361737988401E-15,-1.,0.)) ;
#89074 = DIRECTION('ref_axis',(1.,-8.67361737988401E-15,0.)) ;
#89075 = DIRECTION('center_axis',(0.,1.,0.)) ;
#89076 = DIRECTION('ref_axis',(1.,0.,0.)) ;
#89077 = DIRECTION('center_axis',(8.67361737988403E-15,-1.,0.)) ;
#89078 = DIRECTION('ref_axis',(1.,8.67361737988403E-15,0.)) ;
#89079 = DIRECTION('center_axis',(0.,0.,1.)) ;
#89080 = DIRECTION('ref_axis',(1.,0.,0.)) ;
#89081 = DIRECTION('center_axis',(1.,8.67361737988401E-15,0.)) ;
#89082 = DIRECTION('ref_axis',(-8.67361737988401E-15,1.,0.)) ;
#89083 = DIRECTION('center_axis',(1.2303003375722E-16,-1.,0.)) ;
#89084 = DIRECTION('ref_axis',(1.,1.2303003375722E-16,0.)) ;
#89085 = DIRECTION('center_axis',(-8.67361737988416E-15,-1.,0.)) ;
#89086 = DIRECTION('ref_axis',(1.,-8.67361737988416E-15,0.)) ;
#89087 = DIRECTION('center_axis',(-1.,5.88041856263325E-16,0.)) ;
#89088 = DIRECTION('ref_axis',(-5.88041856263325E-16,-1.,0.)) ;
#89089 = DIRECTION('center_axis',(1.,0.,0.)) ;
#89090 = DIRECTION('ref_axis',(0.,0.,-1.)) ;
#89091 = DIRECTION('center_axis',(0.,1.,0.)) ;
#89092 = DIRECTION('ref_axis',(1.,0.,0.)) ;
#89093 = DIRECTION('center_axis',(1.,6.50521303491304E-15,0.)) ;
#89094 = DIRECTION('ref_axis',(-6.50521303491304E-15,1.,0.)) ;
#89095 = DIRECTION('center_axis',(0.,1.,0.)) ;
#89096 = DIRECTION('ref_axis',(1.,0.,0.)) ;
#89097 = DIRECTION('center_axis',(0.,-1.,0.)) ;
#89098 = DIRECTION('ref_axis',(0.,0.,-1.)) ;
#89099 = DIRECTION('center_axis',(1.,0.,0.)) ;
#89100 = DIRECTION('ref_axis',(0.,0.,-1.)) ;
#89101 = DIRECTION('center_axis',(1.,-1.73472347597681E-14,0.)) ;
#89102 = DIRECTION('ref_axis',(1.73472347597681E-14,1.,0.)) ;
#89103 = DIRECTION('center_axis',(0.,1.,0.)) ;
#89104 = DIRECTION('ref_axis',(0.,0.,1.)) ;
#89105 = DIRECTION('center_axis',(0.,-1.,-8.67361737988405E-15)) ;
#89106 = DIRECTION('ref_axis',(0.,8.67361737988405E-15,-1.)) ;
#89107 = DIRECTION('center_axis',(0.,1.,0.)) ;
#89108 = DIRECTION('ref_axis',(1.,0.,0.)) ;
#89109 = DIRECTION('center_axis',(0.,0.,-1.)) ;
#89110 = DIRECTION('ref_axis',(-1.,0.,0.)) ;
#89111 = DIRECTION('center_axis',(0.,0.,1.)) ;
#89112 = DIRECTION('ref_axis',(1.,0.,0.)) ;
#89113 = DIRECTION('center_axis',(0.,0.,-1.)) ;
#89114 = DIRECTION('ref_axis',(-1.,0.,0.)) ;
#89115 = DIRECTION('center_axis',(-1.,0.,0.)) ;
#89116 = DIRECTION('ref_axis',(0.,0.,1.)) ;
#89117 = DIRECTION('center_axis',(0.,-1.,0.)) ;
#89118 = DIRECTION('ref_axis',(0.,0.,-1.)) ;
#89119 = DIRECTION('center_axis',(0.,1.,0.)) ;
#89120 = DIRECTION('ref_axis',(0.,0.,1.)) ;
#89121 = DIRECTION('center_axis',(0.,1.,-6.50521303491302E-15)) ;
#89122 = DIRECTION('ref_axis',(0.,6.50521303491302E-15,1.)) ;
#89123 = DIRECTION('center_axis',(0.,-1.,0.)) ;
#89124 = DIRECTION('ref_axis',(0.,0.,-1.)) ;
#89125 = DIRECTION('center_axis',(0.,-1.,0.)) ;
#89126 = DIRECTION('ref_axis',(0.,0.,-1.)) ;
#89127 = DIRECTION('center_axis',(0.,-1.,-1.07081696047951E-16)) ;
#89128 = DIRECTION('ref_axis',(0.,1.07081696047951E-16,-1.)) ;
#89129 = DIRECTION('center_axis',(0.,1.,0.)) ;
#89130 = DIRECTION('ref_axis',(0.,0.,1.)) ;
#89131 = DIRECTION('center_axis',(-1.,0.,0.)) ;
#89132 = DIRECTION('ref_axis',(0.,0.,1.)) ;
#89133 = DIRECTION('center_axis',(0.,0.,1.)) ;
#89134 = DIRECTION('ref_axis',(1.,0.,0.)) ;
#89135 = DIRECTION('center_axis',(0.,1.,0.)) ;
#89136 = DIRECTION('ref_axis',(0.,0.,1.)) ;
#89137 = DIRECTION('center_axis',(0.,-6.50521303491304E-15,-1.)) ;
#89138 = DIRECTION('ref_axis',(0.,1.,-6.50521303491304E-15)) ;
#89139 = DIRECTION('center_axis',(0.,0.,1.)) ;
#89140 = DIRECTION('ref_axis',(1.,0.,0.)) ;
#89141 = DIRECTION('center_axis',(0.,-1.08420217248551E-15,1.)) ;
#89142 = DIRECTION('ref_axis',(0.,-1.,-1.08420217248551E-15)) ;
#89143 = DIRECTION('center_axis',(0.,0.,1.)) ;
#89144 = DIRECTION('ref_axis',(1.,0.,0.)) ;
#89145 = DIRECTION('center_axis',(0.,0.,-1.)) ;
#89146 = DIRECTION('ref_axis',(-1.,0.,0.)) ;
#89147 = DIRECTION('center_axis',(0.,1.,0.)) ;
#89148 = DIRECTION('ref_axis',(0.,0.,1.)) ;
#89149 = DIRECTION('center_axis',(0.,-0.707106781186548,0.707106781186547)) ;
#89150 = DIRECTION('ref_axis',(0.,-0.707106781186547,-0.707106781186548)) ;
#89151 = DIRECTION('center_axis',(0.,1.,0.)) ;
#89152 = DIRECTION('ref_axis',(0.,0.,1.)) ;
#89153 = DIRECTION('center_axis',(0.,-0.5142317969591,-0.857651245551602)) ;
#89154 = DIRECTION('ref_axis',(0.,0.857651245551602,-0.5142317969591)) ;
#89155 = DIRECTION('center_axis',(0.,-0.707106781186548,0.707106781186547)) ;
#89156 = DIRECTION('ref_axis',(0.,-0.707106781186547,-0.707106781186548)) ;
#89157 = DIRECTION('center_axis',(0.,-0.70710678118655,0.707106781186545)) ;
#89158 = DIRECTION('ref_axis',(0.,-0.707106781186545,-0.70710678118655)) ;
#89159 = DIRECTION('center_axis',(-1.,0.,0.)) ;
#89160 = DIRECTION('ref_axis',(0.,0.,1.)) ;
#89161 = DIRECTION('center_axis',(0.,0.514231796959101,-0.857651245551602)) ;
#89162 = DIRECTION('ref_axis',(0.,0.857651245551602,0.514231796959101)) ;
#89163 = DIRECTION('center_axis',(0.,1.,0.)) ;
#89164 = DIRECTION('ref_axis',(0.,0.,1.)) ;
#89165 = DIRECTION('center_axis',(0.,0.,-1.)) ;
#89166 = DIRECTION('ref_axis',(-1.,0.,0.)) ;
#89167 = DIRECTION('center_axis',(0.,1.,0.)) ;
#89168 = DIRECTION('ref_axis',(0.,0.,1.)) ;
#89169 = DIRECTION('center_axis',(0.,0.,-1.)) ;
#89170 = DIRECTION('ref_axis',(-1.,0.,0.)) ;
#89171 = DIRECTION('center_axis',(0.,0.,-1.)) ;
#89172 = DIRECTION('ref_axis',(-1.,0.,0.)) ;
#89173 = DIRECTION('center_axis',(0.,0.,1.)) ;
#89174 = DIRECTION('ref_axis',(1.,0.,0.)) ;
#89175 = DIRECTION('center_axis',(0.,0.,-1.)) ;
#89176 = DIRECTION('ref_axis',(-1.,0.,0.)) ;
#89177 = DIRECTION('center_axis',(0.,1.,0.)) ;
#89178 = DIRECTION('ref_axis',(0.,0.,1.)) ;
#89179 = DIRECTION('center_axis',(0.,-1.,8.67361737988403E-15)) ;
#89180 = DIRECTION('ref_axis',(0.,-8.67361737988403E-15,-1.)) ;
#89181 = DIRECTION('center_axis',(0.,0.707106781186546,0.707106781186549)) ;
#89182 = DIRECTION('ref_axis',(0.,-0.707106781186549,0.707106781186546)) ;
#89183 = DIRECTION('center_axis',(0.,0.707106781186547,0.707106781186548)) ;
#89184 = DIRECTION('ref_axis',(0.,-0.707106781186548,0.707106781186547)) ;
#89185 = DIRECTION('center_axis',(0.,1.,1.07081696047951E-16)) ;
#89186 = DIRECTION('ref_axis',(0.,-1.07081696047951E-16,1.)) ;
#89187 = DIRECTION('center_axis',(0.,-1.,0.)) ;
#89188 = DIRECTION('ref_axis',(0.,0.,-1.)) ;
#89189 = DIRECTION('center_axis',(0.,1.,0.)) ;
#89190 = DIRECTION('ref_axis',(0.,0.,1.)) ;
#89191 = DIRECTION('center_axis',(0.,-1.08420217248551E-15,1.)) ;
#89192 = DIRECTION('ref_axis',(0.,-1.,-1.08420217248551E-15)) ;
#89193 = DIRECTION('center_axis',(0.,1.,0.)) ;
#89194 = DIRECTION('ref_axis',(0.,0.,1.)) ;
#89195 = DIRECTION('center_axis',(0.,6.50521303491302E-15,1.)) ;
#89196 = DIRECTION('ref_axis',(0.,-1.,6.50521303491302E-15)) ;
#89197 = DIRECTION('center_axis',(0.,3.99416362155027E-15,1.)) ;
#89198 = DIRECTION('ref_axis',(0.,-1.,3.99416362155027E-15)) ;
#89199 = DIRECTION('center_axis',(0.,0.,1.)) ;
#89200 = DIRECTION('ref_axis',(1.,0.,0.)) ;
#89201 = DIRECTION('center_axis',(0.,0.,-1.)) ;
#89202 = DIRECTION('ref_axis',(-1.,0.,0.)) ;
#89203 = DIRECTION('center_axis',(0.,0.,1.)) ;
#89204 = DIRECTION('ref_axis',(1.,0.,0.)) ;
#89205 = DIRECTION('center_axis',(-1.,0.,0.)) ;
#89206 = DIRECTION('ref_axis',(0.,0.,1.)) ;
#89207 = DIRECTION('center_axis',(0.,1.,0.)) ;
#89208 = DIRECTION('ref_axis',(0.,0.,1.)) ;
#89209 = DIRECTION('center_axis',(-1.,0.,0.)) ;
#89210 = DIRECTION('ref_axis',(0.,0.,1.)) ;
#89211 = DIRECTION('center_axis',(0.,-1.,0.)) ;
#89212 = DIRECTION('ref_axis',(0.,0.,-1.)) ;
#89213 = DIRECTION('center_axis',(0.,1.,0.)) ;
#89214 = DIRECTION('ref_axis',(0.,0.,1.)) ;
#89215 = DIRECTION('center_axis',(0.,-1.,0.)) ;
#89216 = DIRECTION('ref_axis',(0.,0.,-1.)) ;
#89217 = DIRECTION('center_axis',(0.,1.,0.)) ;
#89218 = DIRECTION('ref_axis',(0.,0.,1.)) ;
#89219 = DIRECTION('center_axis',(0.,-1.,0.)) ;
#89220 = DIRECTION('ref_axis',(0.,0.,-1.)) ;
#89221 = DIRECTION('center_axis',(0.,1.,0.)) ;
#89222 = DIRECTION('ref_axis',(0.,0.,-1.)) ;
#89223 = DIRECTION('center_axis',(-4.70197740328919E-30,-1.08420217248551E-15,
-1.)) ;
#89224 = DIRECTION('ref_axis',(6.22301527786114E-61,1.,-1.08420217248551E-15)) ;
#89225 = DIRECTION('center_axis',(0.,1.,0.)) ;
#89226 = DIRECTION('ref_axis',(0.,0.,-1.)) ;
#89227 = DIRECTION('center_axis',(0.,0.,-1.)) ;
#89228 = DIRECTION('ref_axis',(-1.,0.,0.)) ;
#89229 = DIRECTION('center_axis',(0.,0.,1.)) ;
#89230 = DIRECTION('ref_axis',(1.,0.,0.)) ;
#89231 = DIRECTION('center_axis',(0.,0.,-1.)) ;
#89232 = DIRECTION('ref_axis',(-1.,0.,0.)) ;
#89233 = DIRECTION('center_axis',(0.,0.,-1.)) ;
#89234 = DIRECTION('ref_axis',(-1.,0.,0.)) ;
#89235 = DIRECTION('center_axis',(0.,6.50521303491304E-15,-1.)) ;
#89236 = DIRECTION('ref_axis',(0.,1.,6.50521303491304E-15)) ;
#89237 = DIRECTION('center_axis',(1.,0.,0.)) ;
#89238 = DIRECTION('ref_axis',(0.,0.,-1.)) ;
#89239 = DIRECTION('center_axis',(0.,0.707106781186548,-0.707106781186548)) ;
#89240 = DIRECTION('ref_axis',(0.,0.707106781186548,0.707106781186548)) ;
#89241 = DIRECTION('center_axis',(1.,0.,0.)) ;
#89242 = DIRECTION('ref_axis',(0.,0.,-1.)) ;
#89243 = DIRECTION('center_axis',(0.,-1.,0.)) ;
#89244 = DIRECTION('ref_axis',(0.,0.,-1.)) ;
#89245 = DIRECTION('center_axis',(0.,-0.707106781186548,0.707106781186547)) ;
#89246 = DIRECTION('ref_axis',(0.,-0.707106781186547,-0.707106781186548)) ;
#89247 = DIRECTION('center_axis',(0.,-1.,-1.07081696047951E-16)) ;
#89248 = DIRECTION('ref_axis',(0.,1.07081696047951E-16,-1.)) ;
#89249 = DIRECTION('center_axis',(0.,-1.,-8.67361737988403E-15)) ;
#89250 = DIRECTION('ref_axis',(0.,8.67361737988403E-15,-1.)) ;
#89251 = DIRECTION('center_axis',(1.,0.,0.)) ;
#89252 = DIRECTION('ref_axis',(0.,0.,-1.)) ;
#89253 = DIRECTION('center_axis',(0.,0.,1.)) ;
#89254 = DIRECTION('ref_axis',(1.,0.,0.)) ;
#89255 = DIRECTION('center_axis',(0.,0.,-1.)) ;
#89256 = DIRECTION('ref_axis',(-1.,0.,0.)) ;
#89257 = DIRECTION('center_axis',(0.,0.,1.)) ;
#89258 = DIRECTION('ref_axis',(1.,0.,0.)) ;
#89259 = DIRECTION('center_axis',(0.,0.,1.)) ;
#89260 = DIRECTION('ref_axis',(1.,0.,0.)) ;
#89261 = DIRECTION('center_axis',(0.,0.,1.)) ;
#89262 = DIRECTION('ref_axis',(1.,0.,0.)) ;
#89263 = DIRECTION('center_axis',(1.,0.,0.)) ;
#89264 = DIRECTION('ref_axis',(0.,0.382683432365091,0.923879532511286)) ;
#89265 = DIRECTION('center_axis',(0.,-0.707106781186551,-0.707106781186544)) ;
#89266 = DIRECTION('ref_axis',(0.,0.707106781186544,-0.707106781186551)) ;
#89267 = DIRECTION('center_axis',(1.,0.,0.)) ;
#89268 = DIRECTION('ref_axis',(0.,0.,-1.)) ;
#89269 = DIRECTION('center_axis',(0.,0.5142317969591,0.857651245551602)) ;
#89270 = DIRECTION('ref_axis',(0.,-0.857651245551602,0.5142317969591)) ;
#89271 = DIRECTION('center_axis',(0.,0.707106781186546,0.707106781186549)) ;
#89272 = DIRECTION('ref_axis',(0.,-0.707106781186549,0.707106781186546)) ;
#89273 = DIRECTION('center_axis',(0.,-0.707106781186546,-0.707106781186549)) ;
#89274 = DIRECTION('ref_axis',(0.,0.707106781186549,-0.707106781186546)) ;
#89275 = DIRECTION('center_axis',(1.,0.,0.)) ;
#89276 = DIRECTION('ref_axis',(0.,0.,-1.)) ;
#89277 = DIRECTION('center_axis',(0.,-0.514231796959099,0.857651245551603)) ;
#89278 = DIRECTION('ref_axis',(0.,-0.857651245551603,-0.514231796959099)) ;
#89279 = DIRECTION('center_axis',(1.,0.,0.)) ;
#89280 = DIRECTION('ref_axis',(0.,0.,-1.)) ;
#89281 = DIRECTION('center_axis',(0.,1.08420217248551E-15,-1.)) ;
#89282 = DIRECTION('ref_axis',(0.,1.,1.08420217248551E-15)) ;
#89283 = DIRECTION('center_axis',(1.,0.,0.)) ;
#89284 = DIRECTION('ref_axis',(0.,0.,-1.)) ;
#89285 = DIRECTION('center_axis',(0.,0.,1.)) ;
#89286 = DIRECTION('ref_axis',(1.,0.,0.)) ;
#89287 = DIRECTION('center_axis',(0.,3.99416362155027E-15,1.)) ;
#89288 = DIRECTION('ref_axis',(0.,-1.,3.99416362155027E-15)) ;
#89289 = DIRECTION('center_axis',(0.,-4.33680868994202E-15,-1.)) ;
#89290 = DIRECTION('ref_axis',(0.,1.,-4.33680868994202E-15)) ;
#89291 = DIRECTION('center_axis',(0.,0.,1.)) ;
#89292 = DIRECTION('ref_axis',(1.,0.,0.)) ;
#89293 = DIRECTION('center_axis',(0.,-6.50521303491304E-15,1.)) ;
#89294 = DIRECTION('ref_axis',(0.,-1.,-6.50521303491304E-15)) ;
#89295 = DIRECTION('center_axis',(0.,1.,0.)) ;
#89296 = DIRECTION('ref_axis',(0.,0.,-1.)) ;
#89297 = DIRECTION('center_axis',(0.,-1.,0.)) ;
#89298 = DIRECTION('ref_axis',(0.,0.,-1.)) ;
#89299 = DIRECTION('center_axis',(1.,0.,0.)) ;
#89300 = DIRECTION('ref_axis',(0.,0.,-1.)) ;
#89301 = DIRECTION('center_axis',(0.,1.,0.)) ;
#89302 = DIRECTION('ref_axis',(0.,0.,1.)) ;
#89303 = DIRECTION('center_axis',(0.,1.,0.)) ;
#89304 = DIRECTION('ref_axis',(0.,0.,1.)) ;
#89305 = DIRECTION('center_axis',(0.,-1.,0.)) ;
#89306 = DIRECTION('ref_axis',(0.,0.,-1.)) ;
#89307 = DIRECTION('center_axis',(0.,1.,1.07081696047951E-16)) ;
#89308 = DIRECTION('ref_axis',(0.,-1.07081696047951E-16,1.)) ;
#89309 = DIRECTION('center_axis',(0.,1.,6.50521303491302E-15)) ;
#89310 = DIRECTION('ref_axis',(0.,-6.50521303491302E-15,1.)) ;
#89311 = DIRECTION('center_axis',(0.,1.,0.)) ;
#89312 = DIRECTION('ref_axis',(0.,0.,-1.)) ;
#89313 = DIRECTION('center_axis',(0.,0.,1.)) ;
#89314 = DIRECTION('ref_axis',(1.,0.,0.)) ;
#89315 = DIRECTION('center_axis',(1.,0.,0.)) ;
#89316 = DIRECTION('ref_axis',(0.,0.,-1.)) ;
#89317 = DIRECTION('center_axis',(0.,0.,-1.)) ;
#89318 = DIRECTION('ref_axis',(-1.,0.,0.)) ;
#89319 = DIRECTION('center_axis',(0.,0.,-1.)) ;
#89320 = DIRECTION('ref_axis',(-1.,0.,0.)) ;
#89321 = DIRECTION('center_axis',(1.,-9.85638338623186E-18,0.)) ;
#89322 = DIRECTION('ref_axis',(9.85638338623186E-18,1.,0.)) ;
#89323 = DIRECTION('',(0.,0.,-1.)) ;
#89324 = DIRECTION('',(-9.85638338623186E-18,-1.,0.)) ;
#89325 = DIRECTION('',(0.,0.,1.)) ;
#89326 = DIRECTION('',(9.85638338623186E-18,1.,0.)) ;
#89327 = DIRECTION('center_axis',(0.707106781186548,0.707106781186548,0.)) ;
#89328 = DIRECTION('ref_axis',(-0.707106781186548,0.707106781186548,0.)) ;
#89329 = DIRECTION('',(0.,0.,1.)) ;
#89330 = DIRECTION('',(-0.577350269189625,0.577350269189625,0.577350269189627)) ;
#89331 = DIRECTION('',(0.,0.,-1.)) ;
#89332 = DIRECTION('',(0.577350269189625,-0.577350269189625,0.577350269189627)) ;
#89333 = DIRECTION('center_axis',(0.,1.,0.)) ;
#89334 = DIRECTION('ref_axis',(0.,0.,1.)) ;
#89335 = DIRECTION('',(0.,0.,1.)) ;
#89336 = DIRECTION('',(-1.,0.,-9.8563833862319E-18)) ;
#89337 = DIRECTION('',(0.,0.,-1.)) ;
#89338 = DIRECTION('',(1.,0.,-9.8563833862319E-18)) ;
#89339 = DIRECTION('center_axis',(-0.707106781186548,0.707106781186548,0.)) ;
#89340 = DIRECTION('ref_axis',(-0.707106781186548,-0.707106781186548,0.)) ;
#89341 = DIRECTION('',(0.,0.,1.)) ;
#89342 = DIRECTION('',(-0.577350269189625,-0.577350269189625,-0.577350269189627)) ;
#89343 = DIRECTION('',(0.,0.,-1.)) ;
#89344 = DIRECTION('',(0.577350269189625,0.577350269189625,-0.577350269189627)) ;
#89345 = DIRECTION('center_axis',(-1.,9.85638338623186E-18,0.)) ;
#89346 = DIRECTION('ref_axis',(-9.85638338623186E-18,-1.,0.)) ;
#89347 = DIRECTION('',(0.,0.,-1.)) ;
#89348 = DIRECTION('',(9.85638338623186E-18,1.,0.)) ;
#89349 = DIRECTION('',(0.,0.,-1.)) ;
#89350 = DIRECTION('',(-9.85638338623186E-18,-1.,0.)) ;
#89351 = DIRECTION('center_axis',(0.,0.,1.)) ;
#89352 = DIRECTION('ref_axis',(1.,0.,0.)) ;
#89353 = DIRECTION('',(9.85638338623186E-18,1.,0.)) ;
#89354 = DIRECTION('center_axis',(0.,0.,-1.)) ;
#89355 = DIRECTION('ref_axis',(1.,0.,0.)) ;
#89356 = DIRECTION('center_axis',(0.,0.,1.)) ;
#89357 = DIRECTION('ref_axis',(1.,0.,0.)) ;
#89358 = DIRECTION('',(-9.85638338623186E-18,-1.,0.)) ;
#89359 = DIRECTION('',(1.,-9.85638338623186E-18,0.)) ;
#89360 = DIRECTION('center_axis',(0.,0.,1.)) ;
#89361 = DIRECTION('ref_axis',(1.,0.,0.)) ;
#89362 = DIRECTION('',(9.85638338623186E-18,1.,0.)) ;
#89363 = DIRECTION('center_axis',(0.,0.,-1.)) ;
#89364 = DIRECTION('ref_axis',(1.,0.,0.)) ;
#89365 = DIRECTION('center_axis',(0.,0.,1.)) ;
#89366 = DIRECTION('ref_axis',(1.,0.,0.)) ;
#89367 = DIRECTION('',(-9.85638338623186E-18,-1.,0.)) ;
#89368 = DIRECTION('',(-1.,9.85638338623186E-18,0.)) ;
#89369 = DIRECTION('center_axis',(0.,0.,-1.)) ;
#89370 = DIRECTION('ref_axis',(-1.,0.,0.)) ;
#89371 = DIRECTION('center_axis',(0.,0.,1.)) ;
#89372 = DIRECTION('ref_axis',(1.,0.,0.)) ;
#89373 = DIRECTION('center_axis',(0.,0.,-1.)) ;
#89374 = DIRECTION('ref_axis',(1.,0.,0.)) ;
#89375 = DIRECTION('center_axis',(0.,0.,-1.)) ;
#89376 = DIRECTION('ref_axis',(-1.,0.,0.)) ;
#89377 = DIRECTION('center_axis',(0.,0.,-1.)) ;
#89378 = DIRECTION('ref_axis',(1.,0.,0.)) ;
#89379 = DIRECTION('center_axis',(0.,0.,1.)) ;
#89380 = DIRECTION('ref_axis',(1.,0.,0.)) ;
#89381 = DIRECTION('center_axis',(-0.707106781186548,-0.707106781186547,0.)) ;
#89382 = DIRECTION('ref_axis',(0.707106781186547,-0.707106781186548,0.)) ;
#89383 = DIRECTION('',(0.,0.,1.)) ;
#89384 = DIRECTION('',(0.577350269189625,-0.577350269189626,-0.577350269189626)) ;
#89385 = DIRECTION('',(0.,0.,-1.)) ;
#89386 = DIRECTION('',(-0.577350269189625,0.577350269189626,-0.577350269189626)) ;
#89387 = DIRECTION('center_axis',(1.95511867169517E-16,-1.,0.)) ;
#89388 = DIRECTION('ref_axis',(1.,1.95511867169517E-16,0.)) ;
#89389 = DIRECTION('',(0.,0.,-1.)) ;
#89390 = DIRECTION('',(-1.,-1.95511867169517E-16,0.)) ;
#89391 = DIRECTION('',(1.,1.95511867169517E-16,0.)) ;
#89392 = DIRECTION('center_axis',(1.06642836637918E-16,1.,0.)) ;
#89393 = DIRECTION('ref_axis',(-1.,1.06642836637918E-16,0.)) ;
#89394 = DIRECTION('',(1.,-1.06642836637919E-16,0.)) ;
#89395 = DIRECTION('',(0.,0.,1.)) ;
#89396 = DIRECTION('',(-1.,1.06642836637919E-16,0.)) ;
#89397 = DIRECTION('center_axis',(-0.707106781186548,0.707106781186547,0.)) ;
#89398 = DIRECTION('ref_axis',(-0.707106781186547,-0.707106781186548,0.)) ;
#89399 = DIRECTION('',(0.,0.,1.)) ;
#89400 = DIRECTION('',(-0.577350269189625,-0.577350269189626,0.577350269189627)) ;
#89401 = DIRECTION('',(0.,0.,-1.)) ;
#89402 = DIRECTION('',(0.577350269189625,0.577350269189626,0.577350269189627)) ;
#89403 = DIRECTION('center_axis',(-1.,0.,0.)) ;
#89404 = DIRECTION('ref_axis',(0.,0.,1.)) ;
#89405 = DIRECTION('',(0.,0.,-1.)) ;
#89406 = DIRECTION('',(0.,1.,1.95511867169518E-16)) ;
#89407 = DIRECTION('',(0.,0.,1.)) ;
#89408 = DIRECTION('',(0.,-1.,1.95511867169518E-16)) ;
#89409 = DIRECTION('center_axis',(0.,0.,1.)) ;
#89410 = DIRECTION('ref_axis',(1.,0.,0.)) ;
#89411 = DIRECTION('',(-1.95511867169517E-16,1.,0.)) ;
#89412 = DIRECTION('',(-1.,-1.95511867169517E-16,0.)) ;
#89413 = DIRECTION('',(1.,-1.06642836637919E-16,0.)) ;
#89414 = DIRECTION('center_axis',(0.,0.,1.)) ;
#89415 = DIRECTION('ref_axis',(1.,0.,0.)) ;
#89416 = DIRECTION('',(1.,1.95511867169517E-16,0.)) ;
#89417 = DIRECTION('',(1.95511867169517E-16,-1.,0.)) ;
#89418 = DIRECTION('',(-1.,1.06642836637919E-16,0.)) ;
#89419 = DIRECTION('center_axis',(6.96951553037899E-18,0.707106781186549,
0.707106781186546)) ;
#89420 = DIRECTION('ref_axis',(-8.6424177776148E-34,-0.707106781186546,0.707106781186549)) ;
#89421 = DIRECTION('',(-0.577350269189625,0.577350269189625,-0.577350269189627)) ;
#89422 = DIRECTION('',(1.,-9.85638338623186E-18,0.)) ;
#89423 = DIRECTION('',(-0.577350269189625,-0.577350269189625,0.577350269189627)) ;
#89424 = DIRECTION('',(-1.,7.70371977754894E-34,9.8563833862319E-18)) ;
#89425 = DIRECTION('center_axis',(6.96951553037899E-18,0.707106781186549,
-0.707106781186546)) ;
#89426 = DIRECTION('ref_axis',(8.6424177776148E-34,0.707106781186546,0.707106781186549)) ;
#89427 = DIRECTION('',(0.577350269189625,0.577350269189625,0.577350269189627)) ;
#89428 = DIRECTION('',(-1.,9.85638338623186E-18,0.)) ;
#89429 = DIRECTION('',(0.577350269189625,-0.577350269189625,-0.577350269189627)) ;
#89430 = DIRECTION('',(1.,-7.70371977754894E-34,9.8563833862319E-18)) ;
#89431 = DIRECTION('center_axis',(-0.707106781186548,-1.38247767078009E-16,
0.707106781186547)) ;
#89432 = DIRECTION('ref_axis',(0.707106781186547,8.815972061965E-34,0.707106781186548)) ;
#89433 = DIRECTION('',(-0.577350269189625,-0.577350269189626,-0.577350269189626)) ;
#89434 = DIRECTION('',(-1.95511867169517E-16,1.,0.)) ;
#89435 = DIRECTION('',(0.577350269189625,-0.577350269189626,0.577350269189626)) ;
#89436 = DIRECTION('',(0.,-1.,-1.95511867169518E-16)) ;
#89437 = DIRECTION('center_axis',(-0.707106781186548,-1.38247767078009E-16,
-0.707106781186547)) ;
#89438 = DIRECTION('ref_axis',(-0.707106781186547,-8.815972061965E-34,0.707106781186548)) ;
#89439 = DIRECTION('',(-0.577350269189625,0.577350269189626,0.577350269189626)) ;
#89440 = DIRECTION('',(1.95511867169517E-16,-1.,0.)) ;
#89441 = DIRECTION('',(0.577350269189625,0.577350269189626,-0.577350269189626)) ;
#89442 = DIRECTION('',(0.,1.,-1.95511867169518E-16)) ;
#89443 = DIRECTION('center_axis',(0.577350269189625,0.577350269189625,-0.577350269189628)) ;
#89444 = DIRECTION('ref_axis',(-0.707106781186549,-3.37019869349033E-16,-0.707106781186546)) ;
#89445 = DIRECTION('center_axis',(-0.577350269189625,-0.577350269189625,0.577350269189628)) ;
#89446 = DIRECTION('ref_axis',(-0.707106781186549,-5.7623968423712E-16,-0.707106781186546)) ;
#89447 = DIRECTION('center_axis',(-0.577350269189625,-0.577350269189625,0.577350269189627)) ;
#89448 = DIRECTION('ref_axis',(0.707106781186549,-3.64954285315842E-16,0.707106781186546)) ;
#89449 = DIRECTION('center_axis',(0.,0.,-1.)) ;
#89450 = DIRECTION('ref_axis',(-1.,0.,0.)) ;
#89451 = DIRECTION('center_axis',(0.,0.,1.)) ;
#89452 = DIRECTION('ref_axis',(-1.,0.,0.)) ;
#89453 = DIRECTION('center_axis',(0.,0.,-1.)) ;
#89454 = DIRECTION('ref_axis',(-1.,0.,0.)) ;
#89455 = DIRECTION('center_axis',(2.08166817117218E-16,1.,0.)) ;
#89456 = DIRECTION('ref_axis',(1.,0.,0.)) ;
#89457 = DIRECTION('center_axis',(-1.,0.,-3.25824851045218E-15)) ;
#89458 = DIRECTION('ref_axis',(3.25824851045218E-15,0.,-1.)) ;
#89459 = DIRECTION('center_axis',(2.71050543121376E-15,2.71050543121375E-15,
1.)) ;
#89460 = DIRECTION('ref_axis',(-1.,-1.07215069759461E-44,2.71050543121376E-15)) ;
#89461 = DIRECTION('center_axis',(-0.577350269189625,-0.577350269189625,-0.577350269189628)) ;
#89462 = DIRECTION('ref_axis',(-0.707106781186549,-3.37019869349033E-16,0.707106781186546)) ;
#89463 = DIRECTION('center_axis',(-0.577350269189625,-0.577350269189625,-0.577350269189628)) ;
#89464 = DIRECTION('ref_axis',(-0.707106781186549,-3.64775444964662E-16,0.707106781186546)) ;
#89465 = DIRECTION('center_axis',(-0.577350269189625,-0.577350269189625,-0.577350269189628)) ;
#89466 = DIRECTION('ref_axis',(-0.707106781186549,-3.37019869349033E-16,0.707106781186546)) ;
#89467 = DIRECTION('center_axis',(0.,0.,-1.)) ;
#89468 = DIRECTION('ref_axis',(-1.,0.,0.)) ;
#89469 = DIRECTION('center_axis',(6.99565121361789E-15,0.,1.)) ;
#89470 = DIRECTION('ref_axis',(1.,0.,-6.99565121361789E-15)) ;
#89471 = DIRECTION('center_axis',(-1.,0.,9.8563833862319E-18)) ;
#89472 = DIRECTION('ref_axis',(9.8563833862319E-18,0.,1.)) ;
#89473 = DIRECTION('center_axis',(-1.,-1.62630325872825E-15,1.62630325872826E-15)) ;
#89474 = DIRECTION('ref_axis',(1.62630325872826E-15,2.45227231256843E-45,
1.)) ;
#89475 = DIRECTION('center_axis',(2.08166817117218E-16,1.,0.)) ;
#89476 = DIRECTION('ref_axis',(1.,0.,0.)) ;
#89477 = DIRECTION('center_axis',(-1.,-5.82758667710957E-15,-5.82758667710959E-15)) ;
#89478 = DIRECTION('ref_axis',(5.82758667710959E-15,3.92363570010949E-44,
-1.)) ;
#89479 = DIRECTION('center_axis',(2.08166817117218E-16,1.,0.)) ;
#89480 = DIRECTION('ref_axis',(1.,0.,0.)) ;
#89481 = DIRECTION('center_axis',(-0.577350269189626,0.577350269189625,-0.577350269189627)) ;
#89482 = DIRECTION('ref_axis',(0.707106781186548,-3.45739798078984E-16,-0.707106781186547)) ;
#89483 = DIRECTION('center_axis',(-1.91661677085422E-15,0.,1.)) ;
#89484 = DIRECTION('ref_axis',(-1.,0.,-1.91661677085422E-15)) ;
#89485 = DIRECTION('center_axis',(-1.,0.,-9.8563833862319E-18)) ;
#89486 = DIRECTION('ref_axis',(-9.8563833862319E-18,0.,1.)) ;
#89487 = DIRECTION('center_axis',(-1.,0.,-2.77909431773862E-15)) ;
#89488 = DIRECTION('ref_axis',(-2.77909431773862E-15,0.,1.)) ;
#89489 = DIRECTION('center_axis',(0.,0.,-1.)) ;
#89490 = DIRECTION('ref_axis',(-1.,0.,0.)) ;
#89491 = DIRECTION('center_axis',(1.49077798716757E-15,-1.49077798716756E-15,
1.)) ;
#89492 = DIRECTION('ref_axis',(1.,-2.47036158412635E-45,-1.49077798716757E-15)) ;
#89493 = DIRECTION('center_axis',(0.577350269189625,-0.577350269189625,0.577350269189628)) ;
#89494 = DIRECTION('ref_axis',(0.707106781186549,-3.37019869349033E-16,-0.707106781186546)) ;
#89495 = DIRECTION('center_axis',(0.577350269189625,-0.577350269189625,0.577350269189628)) ;
#89496 = DIRECTION('ref_axis',(0.707106781186549,-3.64775444964662E-16,-0.707106781186546)) ;
#89497 = DIRECTION('center_axis',(2.08166817117218E-16,1.,0.)) ;
#89498 = DIRECTION('ref_axis',(1.,0.,0.)) ;
#89499 = DIRECTION('center_axis',(-0.577350269189626,0.577350269189625,0.577350269189627)) ;
#89500 = DIRECTION('ref_axis',(-0.707106781186549,-1.20060139371205E-15,-0.707106781186546)) ;
#89501 = DIRECTION('center_axis',(0.,0.,-1.)) ;
#89502 = DIRECTION('ref_axis',(-1.,0.,0.)) ;
#89503 = DIRECTION('center_axis',(0.,0.,1.)) ;
#89504 = DIRECTION('ref_axis',(-1.,0.,0.)) ;
#89505 = DIRECTION('center_axis',(0.,0.,-1.)) ;
#89506 = DIRECTION('ref_axis',(-1.,0.,0.)) ;
#89507 = DIRECTION('center_axis',(-0.577350269189625,0.577350269189625,0.577350269189628)) ;
#89508 = DIRECTION('ref_axis',(0.707106781186549,-3.64775444964662E-16,0.707106781186546)) ;
#89509 = DIRECTION('center_axis',(0.577350269189625,-0.577350269189625,-0.577350269189628)) ;
#89510 = DIRECTION('ref_axis',(0.707106781186549,-4.84385352408706E-16,0.707106781186546)) ;
#89511 = DIRECTION('center_axis',(-0.577350269189625,0.577350269189626,-0.577350269189626)) ;
#89512 = DIRECTION('ref_axis',(5.0289788758123E-16,0.707106781186548,0.707106781186547)) ;
#89513 = DIRECTION('center_axis',(0.577350269189625,-0.577350269189626,0.577350269189626)) ;
#89514 = DIRECTION('ref_axis',(5.0289788758123E-16,0.707106781186548,0.707106781186547)) ;
#89515 = DIRECTION('center_axis',(0.577350269189625,-0.577350269189627,0.577350269189626)) ;
#89516 = DIRECTION('ref_axis',(-1.3856936129729E-16,-0.707106781186547,-0.707106781186548)) ;
#89517 = DIRECTION('center_axis',(0.,0.,-1.)) ;
#89518 = DIRECTION('ref_axis',(-1.,0.,0.)) ;
#89519 = DIRECTION('center_axis',(0.,0.,1.)) ;
#89520 = DIRECTION('ref_axis',(-1.,-5.42101086242751E-15,0.)) ;
#89521 = DIRECTION('center_axis',(0.,0.,-1.)) ;
#89522 = DIRECTION('ref_axis',(-1.,0.,0.)) ;
#89523 = DIRECTION('center_axis',(0.,1.,0.)) ;
#89524 = DIRECTION('ref_axis',(1.,0.,0.)) ;
#89525 = DIRECTION('center_axis',(0.,-1.,-4.79154192713555E-15)) ;
#89526 = DIRECTION('ref_axis',(0.,-4.79154192713555E-15,1.)) ;
#89527 = DIRECTION('center_axis',(-3.18484388167616E-15,3.18484388167617E-15,
1.)) ;
#89528 = DIRECTION('ref_axis',(-4.20389539297445E-45,1.,-3.18484388167617E-15)) ;
#89529 = DIRECTION('center_axis',(0.577350269189625,-0.577350269189626,-0.577350269189626)) ;
#89530 = DIRECTION('ref_axis',(5.0289788758123E-16,0.707106781186548,-0.707106781186547)) ;
#89531 = DIRECTION('center_axis',(0.577350269189625,-0.577350269189626,-0.577350269189626)) ;
#89532 = DIRECTION('ref_axis',(5.0289788758123E-16,0.707106781186548,-0.707106781186547)) ;
#89533 = DIRECTION('center_axis',(0.577350269189625,-0.577350269189626,-0.577350269189626)) ;
#89534 = DIRECTION('ref_axis',(5.0289788758123E-16,0.707106781186548,-0.707106781186547)) ;
#89535 = DIRECTION('center_axis',(0.,0.,-1.)) ;
#89536 = DIRECTION('ref_axis',(-1.,0.,0.)) ;
#89537 = DIRECTION('center_axis',(0.,-2.87492515628133E-15,1.)) ;
#89538 = DIRECTION('ref_axis',(0.,-1.,-2.87492515628133E-15)) ;
#89539 = DIRECTION('center_axis',(0.,1.,1.95511867169518E-16)) ;
#89540 = DIRECTION('ref_axis',(0.,-1.95511867169518E-16,1.)) ;
#89541 = DIRECTION('center_axis',(2.71050543121375E-15,-1.,2.51884375412834E-15)) ;
#89542 = DIRECTION('ref_axis',(1.,2.71050543121375E-15,2.80259692864963E-45)) ;
#89543 = DIRECTION('center_axis',(0.,1.,0.)) ;
#89544 = DIRECTION('ref_axis',(1.,0.,0.)) ;
#89545 = DIRECTION('center_axis',(-2.30392961653169E-15,-1.,2.49559129361712E-15)) ;
#89546 = DIRECTION('ref_axis',(-2.67860162145163E-32,2.49559129361712E-15,
1.)) ;
#89547 = DIRECTION('center_axis',(0.,1.,0.)) ;
#89548 = DIRECTION('ref_axis',(1.,0.,0.)) ;
#89549 = DIRECTION('center_axis',(-0.577350269189625,-0.577350269189626,-0.577350269189627)) ;
#89550 = DIRECTION('ref_axis',(-8.18676000863892E-15,-0.707106781186544,0.707106781186551)) ;
#89551 = DIRECTION('center_axis',(0.,-4.50404941150742E-15,1.)) ;
#89552 = DIRECTION('ref_axis',(0.,1.,4.50404941150742E-15)) ;
#89553 = DIRECTION('center_axis',(0.,1.,-1.95511867169518E-16)) ;
#89554 = DIRECTION('ref_axis',(0.,1.95511867169518E-16,1.)) ;
#89555 = DIRECTION('center_axis',(0.,-1.,-2.10827844793964E-15)) ;
#89556 = DIRECTION('ref_axis',(0.,2.10827844793964E-15,-1.)) ;
#89557 = DIRECTION('center_axis',(0.,0.,-1.)) ;
#89558 = DIRECTION('ref_axis',(-1.,0.,0.)) ;
#89559 = DIRECTION('center_axis',(-6.77626357803439E-17,-6.7762635780344E-17,
1.)) ;
#89560 = DIRECTION('ref_axis',(-1.3684555315672E-48,-1.,-6.7762635780344E-17)) ;
#89561 = DIRECTION('center_axis',(0.577350269189625,0.577350269189626,0.577350269189627)) ;
#89562 = DIRECTION('ref_axis',(-9.19305248608458E-17,-0.707106781186548,0.707106781186547)) ;
#89563 = DIRECTION('center_axis',(0.577350269189625,0.577350269189626,0.577350269189627)) ;
#89564 = DIRECTION('ref_axis',(-9.19305248608458E-17,-0.707106781186548,0.707106781186547)) ;
#89565 = DIRECTION('center_axis',(0.,1.,0.)) ;
#89566 = DIRECTION('ref_axis',(1.,0.,0.)) ;
#89567 = DIRECTION('center_axis',(-0.577350269189624,-0.577350269189627,0.577350269189626)) ;
#89568 = DIRECTION('ref_axis',(-1.46369207068818E-16,0.707106781186547,0.707106781186548)) ;
#89569 = DIRECTION('center_axis',(0.,0.,-1.)) ;
#89570 = DIRECTION('ref_axis',(-1.,0.,0.)) ;
#89571 = DIRECTION('center_axis',(0.,0.,1.)) ;
#89572 = DIRECTION('ref_axis',(-1.,1.0842021724855E-15,0.)) ;
#89573 = DIRECTION('center_axis',(0.,0.,-1.)) ;
#89574 = DIRECTION('ref_axis',(-1.,0.,0.)) ;
#89575 = DIRECTION('center_axis',(-0.577350269189625,-0.577350269189626,0.577350269189627)) ;
#89576 = DIRECTION('ref_axis',(-1.51735478582867E-16,-0.707106781186548,-0.707106781186547)) ;
#89577 = DIRECTION('center_axis',(0.577350269189625,0.577350269189626,-0.577350269189627)) ;
#89578 = DIRECTION('ref_axis',(-8.00734514747286E-15,-0.707106781186544,-0.707106781186551)) ;
#89579 = DIRECTION('center_axis',(0.,0.,1.)) ;
#89580 = DIRECTION('ref_axis',(1.,0.,0.)) ;
#89581 = DIRECTION('center_axis',(0.,-1.,0.)) ;
#89582 = DIRECTION('ref_axis',(0.,0.,-1.)) ;
#89583 = DIRECTION('center_axis',(9.85638338623186E-18,1.,0.)) ;
#89584 = DIRECTION('ref_axis',(-1.,9.85638338623186E-18,0.)) ;
#89585 = DIRECTION('center_axis',(0.,-1.,0.)) ;
#89586 = DIRECTION('ref_axis',(0.,0.,-1.)) ;
#89587 = DIRECTION('center_axis',(0.,1.,0.)) ;
#89588 = DIRECTION('ref_axis',(1.,0.,0.)) ;
#89589 = DIRECTION('center_axis',(-1.,0.,0.)) ;
#89590 = DIRECTION('ref_axis',(0.,0.,1.)) ;
#89591 = DIRECTION('center_axis',(1.,-9.85638338623186E-18,0.)) ;
#89592 = DIRECTION('ref_axis',(9.85638338623186E-18,1.,0.)) ;
#89593 = DIRECTION('center_axis',(-1.,0.,0.)) ;
#89594 = DIRECTION('ref_axis',(0.,0.,1.)) ;
#89595 = DIRECTION('center_axis',(0.,1.,0.)) ;
#89596 = DIRECTION('ref_axis',(1.,0.,0.)) ;
#89597 = DIRECTION('center_axis',(0.,1.,0.)) ;
#89598 = DIRECTION('ref_axis',(0.,0.,1.)) ;
#89599 = DIRECTION('center_axis',(-9.85638338623186E-18,-1.,0.)) ;
#89600 = DIRECTION('ref_axis',(1.,-9.85638338623186E-18,0.)) ;
#89601 = DIRECTION('center_axis',(0.,1.,0.)) ;
#89602 = DIRECTION('ref_axis',(0.,0.,1.)) ;
#89603 = DIRECTION('center_axis',(0.,0.,1.)) ;
#89604 = DIRECTION('ref_axis',(1.,0.,0.)) ;
#89605 = DIRECTION('center_axis',(0.,0.,1.)) ;
#89606 = DIRECTION('ref_axis',(1.,0.,0.)) ;
#89607 = DIRECTION('center_axis',(0.,-1.,0.)) ;
#89608 = DIRECTION('ref_axis',(0.,0.,-1.)) ;
#89609 = DIRECTION('center_axis',(-9.85638338623186E-18,-1.,0.)) ;
#89610 = DIRECTION('ref_axis',(1.,-9.85638338623186E-18,0.)) ;
#89611 = DIRECTION('center_axis',(0.,-1.,0.)) ;
#89612 = DIRECTION('ref_axis',(0.,0.,-1.)) ;
#89613 = DIRECTION('center_axis',(0.,1.,0.)) ;
#89614 = DIRECTION('ref_axis',(1.,0.,0.)) ;
#89615 = DIRECTION('center_axis',(1.,-7.66646708341686E-16,0.)) ;
#89616 = DIRECTION('ref_axis',(7.66646708341686E-16,1.,0.)) ;
#89617 = DIRECTION('center_axis',(1.,-9.85638338623186E-18,0.)) ;
#89618 = DIRECTION('ref_axis',(9.85638338623186E-18,1.,0.)) ;
#89619 = DIRECTION('center_axis',(1.,0.,0.)) ;
#89620 = DIRECTION('ref_axis',(0.,0.,-1.)) ;
#89621 = DIRECTION('center_axis',(0.,1.,0.)) ;
#89622 = DIRECTION('ref_axis',(1.,0.,0.)) ;
#89623 = DIRECTION('center_axis',(0.,1.,0.)) ;
#89624 = DIRECTION('ref_axis',(0.,0.,1.)) ;
#89625 = DIRECTION('center_axis',(-9.85638338623186E-18,-1.,0.)) ;
#89626 = DIRECTION('ref_axis',(1.,-9.85638338623186E-18,0.)) ;
#89627 = DIRECTION('center_axis',(0.,1.,0.)) ;
#89628 = DIRECTION('ref_axis',(0.,0.,1.)) ;
#89629 = DIRECTION('center_axis',(0.,0.,1.)) ;
#89630 = DIRECTION('ref_axis',(1.,0.,0.)) ;
#89631 = DIRECTION('center_axis',(-1.,-1.95511867169517E-16,0.)) ;
#89632 = DIRECTION('ref_axis',(1.95511867169517E-16,-1.,0.)) ;
#89633 = DIRECTION('center_axis',(1.,0.,0.)) ;
#89634 = DIRECTION('ref_axis',(0.,0.,-1.)) ;
#89635 = DIRECTION('center_axis',(0.,1.,0.)) ;
#89636 = DIRECTION('ref_axis',(1.,0.,0.)) ;
#89637 = DIRECTION('center_axis',(-2.29994012502506E-15,-1.,0.)) ;
#89638 = DIRECTION('ref_axis',(1.,-2.29994012502506E-15,0.)) ;
#89639 = DIRECTION('center_axis',(-1.95511867169517E-16,1.,0.)) ;
#89640 = DIRECTION('ref_axis',(-1.,-1.95511867169517E-16,0.)) ;
#89641 = DIRECTION('center_axis',(0.,-1.,0.)) ;
#89642 = DIRECTION('ref_axis',(0.,0.,-1.)) ;
#89643 = DIRECTION('center_axis',(0.,1.,0.)) ;
#89644 = DIRECTION('ref_axis',(1.,0.,0.)) ;
#89645 = DIRECTION('center_axis',(-1.,0.,0.)) ;
#89646 = DIRECTION('ref_axis',(0.,0.,1.)) ;
#89647 = DIRECTION('center_axis',(1.,-1.06642836637918E-16,0.)) ;
#89648 = DIRECTION('ref_axis',(1.06642836637918E-16,1.,0.)) ;
#89649 = DIRECTION('center_axis',(1.,1.95511867169517E-16,0.)) ;
#89650 = DIRECTION('ref_axis',(-1.95511867169517E-16,1.,0.)) ;
#89651 = DIRECTION('center_axis',(1.,0.,0.)) ;
#89652 = DIRECTION('ref_axis',(0.,0.,-1.)) ;
#89653 = DIRECTION('center_axis',(0.,1.,0.)) ;
#89654 = DIRECTION('ref_axis',(1.,0.,0.)) ;
#89655 = DIRECTION('center_axis',(2.29994012502506E-15,-1.,0.)) ;
#89656 = DIRECTION('ref_axis',(1.,2.29994012502506E-15,0.)) ;
#89657 = DIRECTION('center_axis',(-1.95511867169517E-16,1.,0.)) ;
#89658 = DIRECTION('ref_axis',(-1.,-1.95511867169517E-16,0.)) ;
#89659 = DIRECTION('center_axis',(0.,-1.,0.)) ;
#89660 = DIRECTION('ref_axis',(0.,0.,-1.)) ;
#89661 = DIRECTION('center_axis',(-1.,1.06642836637918E-16,0.)) ;
#89662 = DIRECTION('ref_axis',(-1.06642836637918E-16,-1.,0.)) ;
#89663 = DIRECTION('center_axis',(1.,0.,0.)) ;
#89664 = DIRECTION('ref_axis',(0.,0.,-1.)) ;
#89665 = DIRECTION('center_axis',(0.,1.,0.)) ;
#89666 = DIRECTION('ref_axis',(1.,0.,0.)) ;
#89667 = DIRECTION('center_axis',(-1.,-1.53063836115601E-16,0.)) ;
#89668 = DIRECTION('ref_axis',(1.53063836115601E-16,-1.,0.)) ;
#89669 = DIRECTION('',(0.,0.,1.)) ;
#89670 = DIRECTION('',(-1.53063836115601E-16,1.,-1.020425574104E-16)) ;
#89671 = DIRECTION('',(0.,0.,-1.)) ;
#89672 = DIRECTION('',(1.53063836115601E-16,-1.,5.10212787052002E-17)) ;
#89673 = DIRECTION('',(0.,0.,1.)) ;
#89674 = DIRECTION('',(-1.53063836115601E-16,1.,-1.30104260698261E-16)) ;
#89675 = DIRECTION('center_axis',(-1.,-1.53063836115601E-16,0.)) ;
#89676 = DIRECTION('ref_axis',(1.53063836115601E-16,-1.,0.)) ;
#89677 = DIRECTION('',(0.,0.,1.)) ;
#89678 = DIRECTION('center_axis',(-1.,-1.53063836115601E-16,0.)) ;
#89679 = DIRECTION('ref_axis',(1.53063836115601E-16,-1.,0.)) ;
#89680 = DIRECTION('',(1.53063836115601E-16,-1.,-1.30104260698261E-16)) ;
#89681 = DIRECTION('center_axis',(-1.,-1.53063836115601E-16,0.)) ;
#89682 = DIRECTION('ref_axis',(1.53063836115601E-16,-1.,0.)) ;
#89683 = DIRECTION('',(0.,0.,1.)) ;
#89684 = DIRECTION('',(-1.53063836115601E-16,1.,-1.020425574104E-16)) ;
#89685 = DIRECTION('',(0.,0.,-1.)) ;
#89686 = DIRECTION('',(1.53063836115601E-16,-1.,5.10212787052002E-17)) ;
#89687 = DIRECTION('',(0.,0.,1.)) ;
#89688 = DIRECTION('',(-1.53063836115601E-16,1.,-1.30104260698261E-16)) ;
#89689 = DIRECTION('center_axis',(-1.,-1.53063836115601E-16,0.)) ;
#89690 = DIRECTION('ref_axis',(1.53063836115601E-16,-1.,0.)) ;
#89691 = DIRECTION('',(0.,0.,1.)) ;
#89692 = DIRECTION('center_axis',(-1.,-1.53063836115601E-16,0.)) ;
#89693 = DIRECTION('ref_axis',(1.53063836115601E-16,-1.,0.)) ;
#89694 = DIRECTION('',(1.53063836115601E-16,-1.,-1.30104260698261E-16)) ;
#89695 = DIRECTION('center_axis',(-1.,-1.53063836115601E-16,0.)) ;
#89696 = DIRECTION('ref_axis',(1.53063836115601E-16,-1.,0.)) ;
#89697 = DIRECTION('',(0.,0.,1.)) ;
#89698 = DIRECTION('',(-1.53063836115601E-16,1.,-1.020425574104E-16)) ;
#89699 = DIRECTION('',(0.,0.,-1.)) ;
#89700 = DIRECTION('',(1.53063836115601E-16,-1.,5.10212787052002E-17)) ;
#89701 = DIRECTION('',(0.,0.,1.)) ;
#89702 = DIRECTION('',(-1.53063836115601E-16,1.,-1.30104260698261E-16)) ;
#89703 = DIRECTION('center_axis',(-1.,-1.53063836115601E-16,0.)) ;
#89704 = DIRECTION('ref_axis',(1.53063836115601E-16,-1.,0.)) ;
#89705 = DIRECTION('',(0.,0.,1.)) ;
#89706 = DIRECTION('center_axis',(-1.,-1.53063836115601E-16,0.)) ;
#89707 = DIRECTION('ref_axis',(1.53063836115601E-16,-1.,0.)) ;
#89708 = DIRECTION('',(1.53063836115601E-16,-1.,-1.30104260698261E-16)) ;
#89709 = DIRECTION('center_axis',(-1.,-1.53063836115601E-16,0.)) ;
#89710 = DIRECTION('ref_axis',(1.53063836115601E-16,-1.,0.)) ;
#89711 = DIRECTION('',(0.,0.,1.)) ;
#89712 = DIRECTION('',(-1.53063836115601E-16,1.,-1.020425574104E-16)) ;
#89713 = DIRECTION('',(0.,0.,-1.)) ;
#89714 = DIRECTION('',(1.53063836115601E-16,-1.,5.10212787052002E-17)) ;
#89715 = DIRECTION('',(0.,0.,1.)) ;
#89716 = DIRECTION('',(-1.53063836115601E-16,1.,-1.30104260698261E-16)) ;
#89717 = DIRECTION('center_axis',(-1.,-1.53063836115601E-16,0.)) ;
#89718 = DIRECTION('ref_axis',(1.53063836115601E-16,-1.,0.)) ;
#89719 = DIRECTION('',(0.,0.,1.)) ;
#89720 = DIRECTION('center_axis',(-1.,-1.53063836115601E-16,0.)) ;
#89721 = DIRECTION('ref_axis',(1.53063836115601E-16,-1.,0.)) ;
#89722 = DIRECTION('',(1.53063836115601E-16,-1.,-1.30104260698261E-16)) ;
#89723 = DIRECTION('center_axis',(-1.,-1.53063836115601E-16,0.)) ;
#89724 = DIRECTION('ref_axis',(1.53063836115601E-16,-1.,0.)) ;
#89725 = DIRECTION('',(0.,0.,1.)) ;
#89726 = DIRECTION('',(-1.53063836115601E-16,1.,-1.020425574104E-16)) ;
#89727 = DIRECTION('',(0.,0.,-1.)) ;
#89728 = DIRECTION('',(1.53063836115601E-16,-1.,5.10212787052002E-17)) ;
#89729 = DIRECTION('',(0.,0.,1.)) ;
#89730 = DIRECTION('',(-1.53063836115601E-16,1.,-1.30104260698261E-16)) ;
#89731 = DIRECTION('center_axis',(-1.,-1.53063836115601E-16,0.)) ;
#89732 = DIRECTION('ref_axis',(1.53063836115601E-16,-1.,0.)) ;
#89733 = DIRECTION('',(0.,0.,1.)) ;
#89734 = DIRECTION('center_axis',(-1.,-1.53063836115601E-16,0.)) ;
#89735 = DIRECTION('ref_axis',(1.53063836115601E-16,-1.,0.)) ;
#89736 = DIRECTION('',(1.53063836115601E-16,-1.,-1.30104260698261E-16)) ;
#89737 = DIRECTION('center_axis',(-1.,-1.53063836115601E-16,0.)) ;
#89738 = DIRECTION('ref_axis',(1.53063836115601E-16,-1.,0.)) ;
#89739 = DIRECTION('',(0.,0.,1.)) ;
#89740 = DIRECTION('',(-1.53063836115601E-16,1.,-1.020425574104E-16)) ;
#89741 = DIRECTION('',(0.,0.,-1.)) ;
#89742 = DIRECTION('',(1.53063836115601E-16,-1.,5.10212787052002E-17)) ;
#89743 = DIRECTION('',(0.,0.,1.)) ;
#89744 = DIRECTION('',(-1.53063836115601E-16,1.,-1.30104260698261E-16)) ;
#89745 = DIRECTION('center_axis',(-1.,-1.53063836115601E-16,0.)) ;
#89746 = DIRECTION('ref_axis',(1.53063836115601E-16,-1.,0.)) ;
#89747 = DIRECTION('',(0.,0.,1.)) ;
#89748 = DIRECTION('center_axis',(-1.,-1.53063836115601E-16,0.)) ;
#89749 = DIRECTION('ref_axis',(1.53063836115601E-16,-1.,0.)) ;
#89750 = DIRECTION('',(1.53063836115601E-16,-1.,-1.30104260698261E-16)) ;
#89751 = DIRECTION('center_axis',(-1.,-1.53063836115601E-16,0.)) ;
#89752 = DIRECTION('ref_axis',(1.53063836115601E-16,-1.,0.)) ;
#89753 = DIRECTION('',(0.,0.,1.)) ;
#89754 = DIRECTION('',(-1.53063836115601E-16,1.,-1.020425574104E-16)) ;
#89755 = DIRECTION('',(0.,0.,-1.)) ;
#89756 = DIRECTION('',(1.53063836115601E-16,-1.,5.10212787052002E-17)) ;
#89757 = DIRECTION('',(0.,0.,1.)) ;
#89758 = DIRECTION('',(-1.53063836115601E-16,1.,-1.30104260698261E-16)) ;
#89759 = DIRECTION('center_axis',(-1.,-1.53063836115601E-16,0.)) ;
#89760 = DIRECTION('ref_axis',(1.53063836115601E-16,-1.,0.)) ;
#89761 = DIRECTION('',(0.,0.,1.)) ;
#89762 = DIRECTION('center_axis',(-1.,-1.53063836115601E-16,0.)) ;
#89763 = DIRECTION('ref_axis',(1.53063836115601E-16,-1.,0.)) ;
#89764 = DIRECTION('',(1.53063836115601E-16,-1.,-1.30104260698261E-16)) ;
#89765 = DIRECTION('center_axis',(-1.,-1.53063836115601E-16,0.)) ;
#89766 = DIRECTION('ref_axis',(1.53063836115601E-16,-1.,0.)) ;
#89767 = DIRECTION('',(0.,0.,1.)) ;
#89768 = DIRECTION('',(-1.53063836115601E-16,1.,-1.020425574104E-16)) ;
#89769 = DIRECTION('',(0.,0.,-1.)) ;
#89770 = DIRECTION('',(1.53063836115601E-16,-1.,5.10212787052002E-17)) ;
#89771 = DIRECTION('',(0.,0.,1.)) ;
#89772 = DIRECTION('',(-1.53063836115601E-16,1.,-1.30104260698261E-16)) ;
#89773 = DIRECTION('center_axis',(-1.,-1.53063836115601E-16,0.)) ;
#89774 = DIRECTION('ref_axis',(1.53063836115601E-16,-1.,0.)) ;
#89775 = DIRECTION('',(0.,0.,1.)) ;
#89776 = DIRECTION('center_axis',(-1.,-1.53063836115601E-16,0.)) ;
#89777 = DIRECTION('ref_axis',(1.53063836115601E-16,-1.,0.)) ;
#89778 = DIRECTION('',(1.53063836115601E-16,-1.,-1.30104260698261E-16)) ;
#89779 = DIRECTION('center_axis',(-1.,-1.53063836115601E-16,0.)) ;
#89780 = DIRECTION('ref_axis',(1.53063836115601E-16,-1.,0.)) ;
#89781 = DIRECTION('',(0.,0.,1.)) ;
#89782 = DIRECTION('',(-1.53063836115601E-16,1.,-1.020425574104E-16)) ;
#89783 = DIRECTION('',(0.,0.,-1.)) ;
#89784 = DIRECTION('',(1.53063836115601E-16,-1.,5.10212787052002E-17)) ;
#89785 = DIRECTION('',(0.,0.,1.)) ;
#89786 = DIRECTION('',(-1.53063836115601E-16,1.,-1.30104260698261E-16)) ;
#89787 = DIRECTION('center_axis',(-1.,-1.53063836115601E-16,0.)) ;
#89788 = DIRECTION('ref_axis',(1.53063836115601E-16,-1.,0.)) ;
#89789 = DIRECTION('',(0.,0.,1.)) ;
#89790 = DIRECTION('center_axis',(-1.,-1.53063836115601E-16,0.)) ;
#89791 = DIRECTION('ref_axis',(1.53063836115601E-16,-1.,0.)) ;
#89792 = DIRECTION('',(1.53063836115601E-16,-1.,-1.30104260698261E-16)) ;
#89793 = DIRECTION('center_axis',(-1.53063836115601E-16,1.,0.)) ;
#89794 = DIRECTION('ref_axis',(-1.,-1.53063836115601E-16,0.)) ;
#89795 = DIRECTION('',(-1.,-1.53063836115601E-16,2.73691106313441E-48)) ;
#89796 = DIRECTION('',(0.,0.,-1.)) ;
#89797 = DIRECTION('',(1.,1.53063836115601E-16,-1.53236300070382E-33)) ;
#89798 = DIRECTION('',(0.,0.,1.)) ;
#89799 = DIRECTION('center_axis',(1.99142572374599E-32,-1.30104260698261E-16,
-1.)) ;
#89800 = DIRECTION('ref_axis',(0.,1.,-1.30104260698261E-16)) ;
#89801 = DIRECTION('',(-1.,-1.53063836115601E-16,2.73691106313441E-48)) ;
#89802 = DIRECTION('',(1.53063836115601E-16,-1.,1.30104260698261E-16)) ;
#89803 = DIRECTION('',(1.,1.53063836115601E-16,-2.73691106313441E-48)) ;
#89804 = DIRECTION('center_axis',(-1.53063836115601E-16,1.,0.)) ;
#89805 = DIRECTION('ref_axis',(-1.,-1.53063836115601E-16,0.)) ;
#89806 = DIRECTION('',(-1.,-1.53063836115601E-16,-2.73691106313441E-48)) ;
#89807 = DIRECTION('',(0.,0.,-1.)) ;
#89808 = DIRECTION('',(1.,1.53063836115601E-16,-2.73691106313441E-48)) ;
#89809 = DIRECTION('',(0.,0.,1.)) ;
#89810 = DIRECTION('center_axis',(1.99142572374599E-32,-1.30104260698261E-16,
1.)) ;
#89811 = DIRECTION('ref_axis',(0.,-1.,-1.30104260698261E-16)) ;
#89812 = DIRECTION('',(-1.,-1.53063836115601E-16,-2.73691106313441E-48)) ;
#89813 = DIRECTION('',(-1.53063836115601E-16,1.,1.30104260698261E-16)) ;
#89814 = DIRECTION('',(1.,1.53063836115601E-16,2.73691106313441E-48)) ;
#89815 = DIRECTION('',(2.16840434497101E-16,-1.,-1.30104260698261E-16)) ;
#89816 = DIRECTION('center_axis',(-1.53063836115601E-16,1.,0.)) ;
#89817 = DIRECTION('ref_axis',(-1.,-1.53063836115601E-16,0.)) ;
#89818 = DIRECTION('',(-1.,-1.53063836115601E-16,3.06472600140763E-33)) ;
#89819 = DIRECTION('',(0.,0.,-1.)) ;
#89820 = DIRECTION('',(1.,1.53063836115601E-16,2.73691106313441E-48)) ;
#89821 = DIRECTION('',(0.,0.,1.)) ;
#89822 = DIRECTION('center_axis',(-1.53063836115601E-16,1.,0.)) ;
#89823 = DIRECTION('ref_axis',(-1.,-1.53063836115601E-16,0.)) ;
#89824 = DIRECTION('',(-1.,-1.53063836115601E-16,2.73691106313441E-48)) ;
#89825 = DIRECTION('',(0.,0.,-1.)) ;
#89826 = DIRECTION('',(1.,1.53063836115601E-16,-1.53236300070382E-33)) ;
#89827 = DIRECTION('',(0.,0.,1.)) ;
#89828 = DIRECTION('center_axis',(1.99142572374599E-32,-1.30104260698261E-16,
-1.)) ;
#89829 = DIRECTION('ref_axis',(0.,1.,-1.30104260698261E-16)) ;
#89830 = DIRECTION('',(-1.,-1.53063836115601E-16,2.73691106313441E-48)) ;
#89831 = DIRECTION('',(1.53063836115601E-16,-1.,1.30104260698261E-16)) ;
#89832 = DIRECTION('',(1.,1.53063836115601E-16,-2.73691106313441E-48)) ;
#89833 = DIRECTION('center_axis',(-1.53063836115601E-16,1.,0.)) ;
#89834 = DIRECTION('ref_axis',(-1.,-1.53063836115601E-16,0.)) ;
#89835 = DIRECTION('',(-1.,-1.53063836115601E-16,-2.73691106313441E-48)) ;
#89836 = DIRECTION('',(0.,0.,-1.)) ;
#89837 = DIRECTION('',(1.,1.53063836115601E-16,-2.73691106313441E-48)) ;
#89838 = DIRECTION('',(0.,0.,1.)) ;
#89839 = DIRECTION('center_axis',(1.99142572374599E-32,-1.30104260698261E-16,
1.)) ;
#89840 = DIRECTION('ref_axis',(0.,-1.,-1.30104260698261E-16)) ;
#89841 = DIRECTION('',(-1.,-1.53063836115601E-16,-2.73691106313441E-48)) ;
#89842 = DIRECTION('',(-1.53063836115601E-16,1.,1.30104260698261E-16)) ;
#89843 = DIRECTION('',(1.,1.53063836115601E-16,2.73691106313441E-48)) ;
#89844 = DIRECTION('',(2.16840434497101E-16,-1.,-1.30104260698261E-16)) ;
#89845 = DIRECTION('center_axis',(-1.53063836115601E-16,1.,0.)) ;
#89846 = DIRECTION('ref_axis',(-1.,-1.53063836115601E-16,0.)) ;
#89847 = DIRECTION('',(-1.,-1.53063836115601E-16,3.06472600140763E-33)) ;
#89848 = DIRECTION('',(0.,0.,-1.)) ;
#89849 = DIRECTION('',(1.,1.53063836115601E-16,2.73691106313441E-48)) ;
#89850 = DIRECTION('',(0.,0.,1.)) ;
#89851 = DIRECTION('center_axis',(-1.53063836115601E-16,1.,0.)) ;
#89852 = DIRECTION('ref_axis',(-1.,-1.53063836115601E-16,0.)) ;
#89853 = DIRECTION('',(-1.,-1.53063836115601E-16,2.73691106313441E-48)) ;
#89854 = DIRECTION('',(0.,0.,-1.)) ;
#89855 = DIRECTION('',(1.,1.53063836115601E-16,-1.53236300070382E-33)) ;
#89856 = DIRECTION('',(0.,0.,1.)) ;
#89857 = DIRECTION('center_axis',(1.99142572374599E-32,-1.30104260698261E-16,
-1.)) ;
#89858 = DIRECTION('ref_axis',(0.,1.,-1.30104260698261E-16)) ;
#89859 = DIRECTION('',(-1.,-1.53063836115601E-16,2.73691106313441E-48)) ;
#89860 = DIRECTION('',(1.53063836115601E-16,-1.,1.30104260698261E-16)) ;
#89861 = DIRECTION('',(1.,1.53063836115601E-16,-2.73691106313441E-48)) ;
#89862 = DIRECTION('center_axis',(-1.53063836115601E-16,1.,0.)) ;
#89863 = DIRECTION('ref_axis',(-1.,-1.53063836115601E-16,0.)) ;
#89864 = DIRECTION('',(-1.,-1.53063836115601E-16,-2.73691106313441E-48)) ;
#89865 = DIRECTION('',(0.,0.,-1.)) ;
#89866 = DIRECTION('',(1.,1.53063836115601E-16,-2.73691106313441E-48)) ;
#89867 = DIRECTION('',(0.,0.,1.)) ;
#89868 = DIRECTION('center_axis',(1.99142572374599E-32,-1.30104260698261E-16,
1.)) ;
#89869 = DIRECTION('ref_axis',(0.,-1.,-1.30104260698261E-16)) ;
#89870 = DIRECTION('',(-1.,-1.53063836115601E-16,-2.73691106313441E-48)) ;
#89871 = DIRECTION('',(-1.53063836115601E-16,1.,1.30104260698261E-16)) ;
#89872 = DIRECTION('',(1.,1.53063836115601E-16,2.73691106313441E-48)) ;
#89873 = DIRECTION('',(2.16840434497101E-16,-1.,-1.30104260698261E-16)) ;
#89874 = DIRECTION('center_axis',(-1.53063836115601E-16,1.,0.)) ;
#89875 = DIRECTION('ref_axis',(-1.,-1.53063836115601E-16,0.)) ;
#89876 = DIRECTION('',(-1.,-1.53063836115601E-16,3.06472600140763E-33)) ;
#89877 = DIRECTION('',(0.,0.,-1.)) ;
#89878 = DIRECTION('',(1.,1.53063836115601E-16,2.73691106313441E-48)) ;
#89879 = DIRECTION('',(0.,0.,1.)) ;
#89880 = DIRECTION('center_axis',(-1.53063836115601E-16,1.,0.)) ;
#89881 = DIRECTION('ref_axis',(-1.,-1.53063836115601E-16,0.)) ;
#89882 = DIRECTION('',(-1.,-1.53063836115601E-16,2.73691106313441E-48)) ;
#89883 = DIRECTION('',(0.,0.,-1.)) ;
#89884 = DIRECTION('',(1.,1.53063836115601E-16,-1.53236300070382E-33)) ;
#89885 = DIRECTION('',(0.,0.,1.)) ;
#89886 = DIRECTION('center_axis',(1.99142572374599E-32,-1.30104260698261E-16,
-1.)) ;
#89887 = DIRECTION('ref_axis',(0.,1.,-1.30104260698261E-16)) ;
#89888 = DIRECTION('',(-1.,-1.53063836115601E-16,2.73691106313441E-48)) ;
#89889 = DIRECTION('',(1.53063836115601E-16,-1.,1.30104260698261E-16)) ;
#89890 = DIRECTION('',(1.,1.53063836115601E-16,-2.73691106313441E-48)) ;
#89891 = DIRECTION('center_axis',(-1.53063836115601E-16,1.,0.)) ;
#89892 = DIRECTION('ref_axis',(-1.,-1.53063836115601E-16,0.)) ;
#89893 = DIRECTION('',(-1.,-1.53063836115601E-16,-2.73691106313441E-48)) ;
#89894 = DIRECTION('',(0.,0.,-1.)) ;
#89895 = DIRECTION('',(1.,1.53063836115601E-16,-2.73691106313441E-48)) ;
#89896 = DIRECTION('',(0.,0.,1.)) ;
#89897 = DIRECTION('center_axis',(1.99142572374599E-32,-1.30104260698261E-16,
1.)) ;
#89898 = DIRECTION('ref_axis',(0.,-1.,-1.30104260698261E-16)) ;
#89899 = DIRECTION('',(-1.,-1.53063836115601E-16,-2.73691106313441E-48)) ;
#89900 = DIRECTION('',(-1.53063836115601E-16,1.,1.30104260698261E-16)) ;
#89901 = DIRECTION('',(1.,1.53063836115601E-16,2.73691106313441E-48)) ;
#89902 = DIRECTION('',(2.16840434497101E-16,-1.,-1.30104260698261E-16)) ;
#89903 = DIRECTION('center_axis',(-1.53063836115601E-16,1.,0.)) ;
#89904 = DIRECTION('ref_axis',(-1.,-1.53063836115601E-16,0.)) ;
#89905 = DIRECTION('',(-1.,-1.53063836115601E-16,3.06472600140763E-33)) ;
#89906 = DIRECTION('',(0.,0.,-1.)) ;
#89907 = DIRECTION('',(1.,1.53063836115601E-16,2.73691106313441E-48)) ;
#89908 = DIRECTION('',(0.,0.,1.)) ;
#89909 = DIRECTION('center_axis',(-1.53063836115601E-16,1.,0.)) ;
#89910 = DIRECTION('ref_axis',(-1.,-1.53063836115601E-16,0.)) ;
#89911 = DIRECTION('',(-1.,-1.53063836115601E-16,2.73691106313441E-48)) ;
#89912 = DIRECTION('',(0.,0.,-1.)) ;
#89913 = DIRECTION('',(1.,1.53063836115601E-16,-1.53236300070382E-33)) ;
#89914 = DIRECTION('',(0.,0.,1.)) ;
#89915 = DIRECTION('center_axis',(1.99142572374599E-32,-1.30104260698261E-16,
-1.)) ;
#89916 = DIRECTION('ref_axis',(0.,1.,-1.30104260698261E-16)) ;
#89917 = DIRECTION('',(-1.,-1.53063836115601E-16,2.73691106313441E-48)) ;
#89918 = DIRECTION('',(1.53063836115601E-16,-1.,1.30104260698261E-16)) ;
#89919 = DIRECTION('',(1.,1.53063836115601E-16,-2.73691106313441E-48)) ;
#89920 = DIRECTION('center_axis',(-1.53063836115601E-16,1.,0.)) ;
#89921 = DIRECTION('ref_axis',(-1.,-1.53063836115601E-16,0.)) ;
#89922 = DIRECTION('',(-1.,-1.53063836115601E-16,-2.73691106313441E-48)) ;
#89923 = DIRECTION('',(0.,0.,-1.)) ;
#89924 = DIRECTION('',(1.,1.53063836115601E-16,-2.73691106313441E-48)) ;
#89925 = DIRECTION('',(0.,0.,1.)) ;
#89926 = DIRECTION('center_axis',(1.99142572374599E-32,-1.30104260698261E-16,
1.)) ;
#89927 = DIRECTION('ref_axis',(0.,-1.,-1.30104260698261E-16)) ;
#89928 = DIRECTION('',(-1.,-1.53063836115601E-16,-2.73691106313441E-48)) ;
#89929 = DIRECTION('',(-1.53063836115601E-16,1.,1.30104260698261E-16)) ;
#89930 = DIRECTION('',(1.,1.53063836115601E-16,2.73691106313441E-48)) ;
#89931 = DIRECTION('',(2.16840434497101E-16,-1.,-1.30104260698261E-16)) ;
#89932 = DIRECTION('center_axis',(-1.53063836115601E-16,1.,0.)) ;
#89933 = DIRECTION('ref_axis',(-1.,-1.53063836115601E-16,0.)) ;
#89934 = DIRECTION('',(-1.,-1.53063836115601E-16,3.06472600140763E-33)) ;
#89935 = DIRECTION('',(0.,0.,-1.)) ;
#89936 = DIRECTION('',(1.,1.53063836115601E-16,2.73691106313441E-48)) ;
#89937 = DIRECTION('',(0.,0.,1.)) ;
#89938 = DIRECTION('center_axis',(-1.53063836115601E-16,1.,0.)) ;
#89939 = DIRECTION('ref_axis',(-1.,-1.53063836115601E-16,0.)) ;
#89940 = DIRECTION('',(-1.,-1.53063836115601E-16,2.73691106313441E-48)) ;
#89941 = DIRECTION('',(0.,0.,-1.)) ;
#89942 = DIRECTION('',(1.,1.53063836115601E-16,-1.53236300070382E-33)) ;
#89943 = DIRECTION('',(0.,0.,1.)) ;
#89944 = DIRECTION('center_axis',(1.99142572374599E-32,-1.30104260698261E-16,
-1.)) ;
#89945 = DIRECTION('ref_axis',(0.,1.,-1.30104260698261E-16)) ;
#89946 = DIRECTION('',(-1.,-1.53063836115601E-16,2.73691106313441E-48)) ;
#89947 = DIRECTION('',(1.53063836115601E-16,-1.,1.30104260698261E-16)) ;
#89948 = DIRECTION('',(1.,1.53063836115601E-16,-2.73691106313441E-48)) ;
#89949 = DIRECTION('center_axis',(-1.53063836115601E-16,1.,0.)) ;
#89950 = DIRECTION('ref_axis',(-1.,-1.53063836115601E-16,0.)) ;
#89951 = DIRECTION('',(-1.,-1.53063836115601E-16,-2.73691106313441E-48)) ;
#89952 = DIRECTION('',(0.,0.,-1.)) ;
#89953 = DIRECTION('',(1.,1.53063836115601E-16,-2.73691106313441E-48)) ;
#89954 = DIRECTION('',(0.,0.,1.)) ;
#89955 = DIRECTION('center_axis',(1.99142572374599E-32,-1.30104260698261E-16,
1.)) ;
#89956 = DIRECTION('ref_axis',(0.,-1.,-1.30104260698261E-16)) ;
#89957 = DIRECTION('',(-1.,-1.53063836115601E-16,-2.73691106313441E-48)) ;
#89958 = DIRECTION('',(-1.53063836115601E-16,1.,1.30104260698261E-16)) ;
#89959 = DIRECTION('',(1.,1.53063836115601E-16,2.73691106313441E-48)) ;
#89960 = DIRECTION('',(2.16840434497101E-16,-1.,-1.30104260698261E-16)) ;
#89961 = DIRECTION('center_axis',(-1.53063836115601E-16,1.,0.)) ;
#89962 = DIRECTION('ref_axis',(-1.,-1.53063836115601E-16,0.)) ;
#89963 = DIRECTION('',(-1.,-1.53063836115601E-16,3.06472600140763E-33)) ;
#89964 = DIRECTION('',(0.,0.,-1.)) ;
#89965 = DIRECTION('',(1.,1.53063836115601E-16,2.73691106313441E-48)) ;
#89966 = DIRECTION('',(0.,0.,1.)) ;
#89967 = DIRECTION('center_axis',(-1.53063836115601E-16,1.,0.)) ;
#89968 = DIRECTION('ref_axis',(-1.,-1.53063836115601E-16,0.)) ;
#89969 = DIRECTION('',(-1.,-1.53063836115601E-16,2.73691106313441E-48)) ;
#89970 = DIRECTION('',(0.,0.,-1.)) ;
#89971 = DIRECTION('',(1.,1.53063836115601E-16,-1.53236300070382E-33)) ;
#89972 = DIRECTION('',(0.,0.,1.)) ;
#89973 = DIRECTION('center_axis',(1.99142572374599E-32,-1.30104260698261E-16,
-1.)) ;
#89974 = DIRECTION('ref_axis',(0.,1.,-1.30104260698261E-16)) ;
#89975 = DIRECTION('',(-1.,-1.53063836115601E-16,2.73691106313441E-48)) ;
#89976 = DIRECTION('',(1.53063836115601E-16,-1.,1.30104260698261E-16)) ;
#89977 = DIRECTION('',(1.,1.53063836115601E-16,-2.73691106313441E-48)) ;
#89978 = DIRECTION('center_axis',(-1.53063836115601E-16,1.,0.)) ;
#89979 = DIRECTION('ref_axis',(-1.,-1.53063836115601E-16,0.)) ;
#89980 = DIRECTION('',(-1.,-1.53063836115601E-16,-2.73691106313441E-48)) ;
#89981 = DIRECTION('',(0.,0.,-1.)) ;
#89982 = DIRECTION('',(1.,1.53063836115601E-16,-2.73691106313441E-48)) ;
#89983 = DIRECTION('',(0.,0.,1.)) ;
#89984 = DIRECTION('center_axis',(1.99142572374599E-32,-1.30104260698261E-16,
1.)) ;
#89985 = DIRECTION('ref_axis',(0.,-1.,-1.30104260698261E-16)) ;
#89986 = DIRECTION('',(-1.,-1.53063836115601E-16,-2.73691106313441E-48)) ;
#89987 = DIRECTION('',(-1.53063836115601E-16,1.,1.30104260698261E-16)) ;
#89988 = DIRECTION('',(1.,1.53063836115601E-16,2.73691106313441E-48)) ;
#89989 = DIRECTION('',(2.16840434497101E-16,-1.,-1.30104260698261E-16)) ;
#89990 = DIRECTION('center_axis',(-1.53063836115601E-16,1.,0.)) ;
#89991 = DIRECTION('ref_axis',(-1.,-1.53063836115601E-16,0.)) ;
#89992 = DIRECTION('',(-1.,-1.53063836115601E-16,3.06472600140763E-33)) ;
#89993 = DIRECTION('',(0.,0.,-1.)) ;
#89994 = DIRECTION('',(1.,1.53063836115601E-16,2.73691106313441E-48)) ;
#89995 = DIRECTION('',(0.,0.,1.)) ;
#89996 = DIRECTION('center_axis',(-1.53063836115601E-16,1.,0.)) ;
#89997 = DIRECTION('ref_axis',(-1.,-1.53063836115601E-16,0.)) ;
#89998 = DIRECTION('',(-1.,-1.53063836115601E-16,2.73691106313441E-48)) ;
#89999 = DIRECTION('',(0.,0.,-1.)) ;
#90000 = DIRECTION('',(1.,1.53063836115601E-16,-1.53236300070382E-33)) ;
#90001 = DIRECTION('',(0.,0.,1.)) ;
#90002 = DIRECTION('center_axis',(1.99142572374599E-32,-1.30104260698261E-16,
-1.)) ;
#90003 = DIRECTION('ref_axis',(0.,1.,-1.30104260698261E-16)) ;
#90004 = DIRECTION('',(-1.,-1.53063836115601E-16,2.73691106313441E-48)) ;
#90005 = DIRECTION('',(1.53063836115601E-16,-1.,1.30104260698261E-16)) ;
#90006 = DIRECTION('',(1.,1.53063836115601E-16,-2.73691106313441E-48)) ;
#90007 = DIRECTION('center_axis',(-1.53063836115601E-16,1.,0.)) ;
#90008 = DIRECTION('ref_axis',(-1.,-1.53063836115601E-16,0.)) ;
#90009 = DIRECTION('',(-1.,-1.53063836115601E-16,-2.73691106313441E-48)) ;
#90010 = DIRECTION('',(0.,0.,-1.)) ;
#90011 = DIRECTION('',(1.,1.53063836115601E-16,-2.73691106313441E-48)) ;
#90012 = DIRECTION('',(0.,0.,1.)) ;
#90013 = DIRECTION('center_axis',(1.99142572374599E-32,-1.30104260698261E-16,
1.)) ;
#90014 = DIRECTION('ref_axis',(0.,-1.,-1.30104260698261E-16)) ;
#90015 = DIRECTION('',(-1.,-1.53063836115601E-16,-2.73691106313441E-48)) ;
#90016 = DIRECTION('',(-1.53063836115601E-16,1.,1.30104260698261E-16)) ;
#90017 = DIRECTION('',(1.,1.53063836115601E-16,2.73691106313441E-48)) ;
#90018 = DIRECTION('',(2.16840434497101E-16,-1.,-1.30104260698261E-16)) ;
#90019 = DIRECTION('center_axis',(-1.53063836115601E-16,1.,0.)) ;
#90020 = DIRECTION('ref_axis',(-1.,-1.53063836115601E-16,0.)) ;
#90021 = DIRECTION('',(-1.,-1.53063836115601E-16,3.06472600140763E-33)) ;
#90022 = DIRECTION('',(0.,0.,-1.)) ;
#90023 = DIRECTION('',(1.,1.53063836115601E-16,2.73691106313441E-48)) ;
#90024 = DIRECTION('',(0.,0.,1.)) ;
#90025 = DIRECTION('center_axis',(-1.53063836115601E-16,1.,0.)) ;
#90026 = DIRECTION('ref_axis',(-1.,-1.53063836115601E-16,0.)) ;
#90027 = DIRECTION('',(-1.,-1.53063836115601E-16,2.73691106313441E-48)) ;
#90028 = DIRECTION('',(0.,0.,-1.)) ;
#90029 = DIRECTION('',(1.,1.53063836115601E-16,-1.53236300070382E-33)) ;
#90030 = DIRECTION('',(0.,0.,1.)) ;
#90031 = DIRECTION('center_axis',(1.99142572374599E-32,-1.30104260698261E-16,
-1.)) ;
#90032 = DIRECTION('ref_axis',(0.,1.,-1.30104260698261E-16)) ;
#90033 = DIRECTION('',(-1.,-1.53063836115601E-16,2.73691106313441E-48)) ;
#90034 = DIRECTION('',(1.53063836115601E-16,-1.,1.30104260698261E-16)) ;
#90035 = DIRECTION('',(1.,1.53063836115601E-16,-2.73691106313441E-48)) ;
#90036 = DIRECTION('center_axis',(-1.53063836115601E-16,1.,0.)) ;
#90037 = DIRECTION('ref_axis',(-1.,-1.53063836115601E-16,0.)) ;
#90038 = DIRECTION('',(-1.,-1.53063836115601E-16,-2.73691106313441E-48)) ;
#90039 = DIRECTION('',(0.,0.,-1.)) ;
#90040 = DIRECTION('',(1.,1.53063836115601E-16,-2.73691106313441E-48)) ;
#90041 = DIRECTION('',(0.,0.,1.)) ;
#90042 = DIRECTION('center_axis',(1.99142572374599E-32,-1.30104260698261E-16,
1.)) ;
#90043 = DIRECTION('ref_axis',(0.,-1.,-1.30104260698261E-16)) ;
#90044 = DIRECTION('',(-1.,-1.53063836115601E-16,-2.73691106313441E-48)) ;
#90045 = DIRECTION('',(-1.53063836115601E-16,1.,1.30104260698261E-16)) ;
#90046 = DIRECTION('',(1.,1.53063836115601E-16,2.73691106313441E-48)) ;
#90047 = DIRECTION('',(2.16840434497101E-16,-1.,-1.30104260698261E-16)) ;
#90048 = DIRECTION('center_axis',(-1.53063836115601E-16,1.,0.)) ;
#90049 = DIRECTION('ref_axis',(-1.,-1.53063836115601E-16,0.)) ;
#90050 = DIRECTION('',(-1.,-1.53063836115601E-16,3.06472600140763E-33)) ;
#90051 = DIRECTION('',(0.,0.,-1.)) ;
#90052 = DIRECTION('',(1.,1.53063836115601E-16,2.73691106313441E-48)) ;
#90053 = DIRECTION('',(0.,0.,1.)) ;
#90054 = DIRECTION('center_axis',(1.,0.,0.)) ;
#90055 = DIRECTION('ref_axis',(0.,0.,-1.)) ;
#90056 = DIRECTION('',(1.,0.,0.)) ;
#90057 = DIRECTION('center_axis',(1.,0.,0.)) ;
#90058 = DIRECTION('ref_axis',(0.,0.,1.)) ;
#90059 = DIRECTION('',(1.,0.,0.)) ;
#90060 = DIRECTION('center_axis',(-1.,0.,0.)) ;
#90061 = DIRECTION('ref_axis',(0.,0.,-1.)) ;
#90062 = DIRECTION('center_axis',(0.,0.,1.)) ;
#90063 = DIRECTION('ref_axis',(1.,0.,0.)) ;
#90064 = DIRECTION('',(0.,1.,0.)) ;
#90065 = DIRECTION('',(1.,0.,0.)) ;
#90066 = DIRECTION('',(0.,-1.,0.)) ;
#90067 = DIRECTION('center_axis',(1.,0.,0.)) ;
#90068 = DIRECTION('ref_axis',(0.,0.,-1.)) ;
#90069 = DIRECTION('center_axis',(1.,0.,0.)) ;
#90070 = DIRECTION('ref_axis',(0.,0.,1.)) ;
#90071 = DIRECTION('',(1.,0.,0.)) ;
#90072 = DIRECTION('center_axis',(-1.,0.,0.)) ;
#90073 = DIRECTION('ref_axis',(0.,0.,-1.)) ;
#90074 = DIRECTION('center_axis',(0.,-1.,3.99416362155027E-15)) ;
#90075 = DIRECTION('ref_axis',(0.,-3.99416362155027E-15,-1.)) ;
#90076 = DIRECTION('',(0.,3.99416362155027E-15,1.)) ;
#90077 = DIRECTION('',(1.,0.,0.)) ;
#90078 = DIRECTION('',(0.,-3.99416362155027E-15,-1.)) ;
#90079 = DIRECTION('center_axis',(1.,0.,0.)) ;
#90080 = DIRECTION('ref_axis',(0.,0.,-1.)) ;
#90081 = DIRECTION('center_axis',(-1.,0.,0.)) ;
#90082 = DIRECTION('ref_axis',(0.,1.30104260698266E-14,-1.)) ;
#90083 = DIRECTION('',(1.,0.,0.)) ;
#90084 = DIRECTION('center_axis',(1.,0.,0.)) ;
#90085 = DIRECTION('ref_axis',(0.,0.,-1.)) ;
#90086 = DIRECTION('center_axis',(0.,-0.707106781186549,0.707106781186546)) ;
#90087 = DIRECTION('ref_axis',(0.,-0.707106781186546,-0.707106781186549)) ;
#90088 = DIRECTION('',(0.,0.707106781186546,0.707106781186549)) ;
#90089 = DIRECTION('',(1.,0.,0.)) ;
#90090 = DIRECTION('',(0.,-0.707106781186546,-0.707106781186549)) ;
#90091 = DIRECTION('center_axis',(1.,0.,0.)) ;
#90092 = DIRECTION('ref_axis',(0.,0.382683432365084,0.923879532511289)) ;
#90093 = DIRECTION('',(1.,0.,0.)) ;
#90094 = DIRECTION('center_axis',(1.,0.,0.)) ;
#90095 = DIRECTION('ref_axis',(0.,0.,-1.)) ;
#90096 = DIRECTION('center_axis',(0.,1.,0.)) ;
#90097 = DIRECTION('ref_axis',(0.,0.,1.)) ;
#90098 = DIRECTION('',(0.,0.,-1.)) ;
#90099 = DIRECTION('',(0.,0.,1.)) ;
#90100 = DIRECTION('center_axis',(0.,-0.707106781186547,-0.707106781186548)) ;
#90101 = DIRECTION('ref_axis',(0.,0.707106781186548,-0.707106781186547)) ;
#90102 = DIRECTION('',(0.,-0.707106781186548,0.707106781186547)) ;
#90103 = DIRECTION('',(1.,0.,0.)) ;
#90104 = DIRECTION('',(0.,0.707106781186548,-0.707106781186547)) ;
#90105 = DIRECTION('center_axis',(1.,0.,0.)) ;
#90106 = DIRECTION('ref_axis',(0.,0.,-1.)) ;
#90107 = DIRECTION('center_axis',(-1.,0.,0.)) ;
#90108 = DIRECTION('ref_axis',(0.,1.73472347597676E-14,-1.)) ;
#90109 = DIRECTION('',(1.,0.,0.)) ;
#90110 = DIRECTION('center_axis',(1.,0.,0.)) ;
#90111 = DIRECTION('ref_axis',(0.,0.,-1.)) ;
#90112 = DIRECTION('center_axis',(0.,-1.,0.)) ;
#90113 = DIRECTION('ref_axis',(0.,0.,-1.)) ;
#90114 = DIRECTION('',(0.,0.,1.)) ;
#90115 = DIRECTION('',(1.,0.,0.)) ;
#90116 = DIRECTION('',(0.,0.,-1.)) ;
#90117 = DIRECTION('center_axis',(1.,0.,0.)) ;
#90118 = DIRECTION('ref_axis',(0.,0.,-1.)) ;
#90119 = DIRECTION('center_axis',(1.,0.,0.)) ;
#90120 = DIRECTION('ref_axis',(0.,0.,1.)) ;
#90121 = DIRECTION('',(1.,0.,0.)) ;
#90122 = DIRECTION('center_axis',(-1.,0.,0.)) ;
#90123 = DIRECTION('ref_axis',(0.,0.,-1.)) ;
#90124 = DIRECTION('center_axis',(0.,0.,-1.)) ;
#90125 = DIRECTION('ref_axis',(-1.,0.,0.)) ;
#90126 = DIRECTION('',(0.,-1.,0.)) ;
#90127 = DIRECTION('',(1.,0.,0.)) ;
#90128 = DIRECTION('',(0.,1.,0.)) ;
#90129 = DIRECTION('center_axis',(1.,0.,0.)) ;
#90130 = DIRECTION('ref_axis',(0.,0.,-1.)) ;
#90131 = DIRECTION('center_axis',(1.,0.,0.)) ;
#90132 = DIRECTION('ref_axis',(0.,0.,1.)) ;
#90133 = DIRECTION('',(1.,0.,0.)) ;
#90134 = DIRECTION('center_axis',(-1.,0.,0.)) ;
#90135 = DIRECTION('ref_axis',(0.,0.,-1.)) ;
#90136 = DIRECTION('center_axis',(0.,1.,0.)) ;
#90137 = DIRECTION('ref_axis',(0.,0.,1.)) ;
#90138 = DIRECTION('',(0.,0.,-1.)) ;
#90139 = DIRECTION('',(1.,0.,0.)) ;
#90140 = DIRECTION('',(0.,0.,1.)) ;
#90141 = DIRECTION('center_axis',(1.,0.,0.)) ;
#90142 = DIRECTION('ref_axis',(0.,0.,-1.)) ;
#90143 = DIRECTION('center_axis',(-1.,0.,0.)) ;
#90144 = DIRECTION('ref_axis',(0.,1.95156391047385E-14,-1.)) ;
#90145 = DIRECTION('',(1.,0.,0.)) ;
#90146 = DIRECTION('center_axis',(1.,0.,0.)) ;
#90147 = DIRECTION('ref_axis',(0.,0.,-1.)) ;
#90148 = DIRECTION('center_axis',(0.,1.07081696047951E-16,-1.)) ;
#90149 = DIRECTION('ref_axis',(0.,1.,1.07081696047951E-16)) ;
#90150 = DIRECTION('',(0.,-1.,-1.07081696047951E-16)) ;
#90151 = DIRECTION('',(1.,0.,0.)) ;
#90152 = DIRECTION('',(0.,1.,1.07081696047951E-16)) ;
#90153 = DIRECTION('center_axis',(1.,0.,0.)) ;
#90154 = DIRECTION('ref_axis',(0.,0.,-1.)) ;
#90155 = DIRECTION('center_axis',(-1.,0.,0.)) ;
#90156 = DIRECTION('ref_axis',(0.,0.,-1.)) ;
#90157 = DIRECTION('',(1.,0.,0.)) ;
#90158 = DIRECTION('center_axis',(1.,0.,0.)) ;
#90159 = DIRECTION('ref_axis',(0.,0.,-1.)) ;
#90160 = DIRECTION('center_axis',(0.,-1.,0.)) ;
#90161 = DIRECTION('ref_axis',(0.,0.,-1.)) ;
#90162 = DIRECTION('',(0.,0.,1.)) ;
#90163 = DIRECTION('',(1.,0.,0.)) ;
#90164 = DIRECTION('',(0.,0.,-1.)) ;
#90165 = DIRECTION('center_axis',(1.,0.,0.)) ;
#90166 = DIRECTION('ref_axis',(0.,0.,-1.)) ;
#90167 = DIRECTION('center_axis',(-1.,0.,0.)) ;
#90168 = DIRECTION('ref_axis',(0.,3.03576608295933E-14,-1.)) ;
#90169 = DIRECTION('',(1.,0.,0.)) ;
#90170 = DIRECTION('center_axis',(1.,0.,0.)) ;
#90171 = DIRECTION('ref_axis',(0.,0.,-1.)) ;
#90172 = DIRECTION('center_axis',(1.,0.,0.)) ;
#90173 = DIRECTION('ref_axis',(0.,0.,-1.)) ;
#90174 = DIRECTION('center_axis',(1.,0.,0.)) ;
#90175 = DIRECTION('ref_axis',(0.,-7.85535158932895E-16,1.)) ;
#90176 = DIRECTION('',(1.,0.,0.)) ;
#90177 = DIRECTION('center_axis',(-1.,0.,0.)) ;
#90178 = DIRECTION('ref_axis',(0.,-7.85535158932895E-16,-1.)) ;
#90179 = DIRECTION('center_axis',(1.,0.,0.)) ;
#90180 = DIRECTION('ref_axis',(0.,0.,-1.)) ;
#90181 = DIRECTION('center_axis',(-1.,0.,0.)) ;
#90182 = DIRECTION('ref_axis',(0.,3.46944695195352E-14,-1.)) ;
#90183 = DIRECTION('',(1.,0.,0.)) ;
#90184 = DIRECTION('center_axis',(1.,0.,0.)) ;
#90185 = DIRECTION('ref_axis',(0.,0.,-1.)) ;
#90186 = DIRECTION('center_axis',(0.,-1.,0.)) ;
#90187 = DIRECTION('ref_axis',(0.,0.,-1.)) ;
#90188 = DIRECTION('',(0.,0.,1.)) ;
#90189 = DIRECTION('',(1.,0.,0.)) ;
#90190 = DIRECTION('',(0.,0.,-1.)) ;
#90191 = DIRECTION('center_axis',(1.,0.,0.)) ;
#90192 = DIRECTION('ref_axis',(0.,0.,-1.)) ;
#90193 = DIRECTION('center_axis',(-1.,0.,0.)) ;
#90194 = DIRECTION('ref_axis',(0.,0.,-1.)) ;
#90195 = DIRECTION('',(1.,0.,0.)) ;
#90196 = DIRECTION('center_axis',(1.,0.,0.)) ;
#90197 = DIRECTION('ref_axis',(0.,0.,-1.)) ;
#90198 = DIRECTION('center_axis',(0.,-1.07081696047951E-16,1.)) ;
#90199 = DIRECTION('ref_axis',(0.,-1.,-1.07081696047951E-16)) ;
#90200 = DIRECTION('',(0.,1.,1.07081696047951E-16)) ;
#90201 = DIRECTION('',(1.,0.,0.)) ;
#90202 = DIRECTION('',(0.,-1.,-1.07081696047951E-16)) ;
#90203 = DIRECTION('center_axis',(1.,0.,0.)) ;
#90204 = DIRECTION('ref_axis',(0.,0.,-1.)) ;
#90205 = DIRECTION('center_axis',(-1.,0.,0.)) ;
#90206 = DIRECTION('ref_axis',(0.,0.,-1.)) ;
#90207 = DIRECTION('',(1.,0.,0.)) ;
#90208 = DIRECTION('center_axis',(1.,0.,0.)) ;
#90209 = DIRECTION('ref_axis',(0.,0.,-1.)) ;
#90210 = DIRECTION('center_axis',(0.,1.,0.)) ;
#90211 = DIRECTION('ref_axis',(0.,0.,1.)) ;
#90212 = DIRECTION('',(0.,0.,-1.)) ;
#90213 = DIRECTION('',(0.,0.,1.)) ;
#90214 = DIRECTION('center_axis',(-1.,0.,0.)) ;
#90215 = DIRECTION('ref_axis',(0.,0.,1.)) ;
#90216 = DIRECTION('center_axis',(-1.,0.,0.)) ;
#90217 = DIRECTION('ref_axis',(0.,0.,1.)) ;
#90218 = DIRECTION('',(0.,-1.,0.)) ;
#90219 = DIRECTION('center_axis',(-1.,0.,0.)) ;
#90220 = DIRECTION('ref_axis',(0.,0.,1.)) ;
#90221 = DIRECTION('',(0.,0.,1.)) ;
#90222 = DIRECTION('',(0.,-1.,-1.07081696047951E-16)) ;
#90223 = DIRECTION('',(0.,0.,-1.)) ;
#90224 = DIRECTION('center_axis',(-1.,0.,0.)) ;
#90225 = DIRECTION('ref_axis',(0.,0.,1.)) ;
#90226 = DIRECTION('',(0.,0.,-1.)) ;
#90227 = DIRECTION('',(0.,1.,1.07081696047951E-16)) ;
#90228 = DIRECTION('',(0.,0.,1.)) ;
#90229 = DIRECTION('center_axis',(-1.,0.,0.)) ;
#90230 = DIRECTION('ref_axis',(0.,0.,1.)) ;
#90231 = DIRECTION('',(0.,1.,0.)) ;
#90232 = DIRECTION('center_axis',(-1.,0.,0.)) ;
#90233 = DIRECTION('ref_axis',(0.,0.,1.)) ;
#90234 = DIRECTION('',(0.,0.,-1.)) ;
#90235 = DIRECTION('',(0.,0.707106781186548,-0.707106781186547)) ;
#90236 = DIRECTION('',(0.,0.,1.)) ;
#90237 = DIRECTION('',(0.,-0.707106781186546,-0.707106781186549)) ;
#90238 = DIRECTION('',(0.,-3.99416362155027E-15,-1.)) ;
#90239 = DIRECTION('center_axis',(1.,0.,0.)) ;
#90240 = DIRECTION('ref_axis',(0.,0.,-1.)) ;
#90241 = DIRECTION('',(1.,0.,0.)) ;
#90242 = DIRECTION('center_axis',(1.,0.,0.)) ;
#90243 = DIRECTION('ref_axis',(0.,0.,1.)) ;
#90244 = DIRECTION('',(1.,0.,0.)) ;
#90245 = DIRECTION('center_axis',(-1.,0.,0.)) ;
#90246 = DIRECTION('ref_axis',(0.,0.,-1.)) ;
#90247 = DIRECTION('center_axis',(0.,0.,1.)) ;
#90248 = DIRECTION('ref_axis',(1.,0.,0.)) ;
#90249 = DIRECTION('',(0.,1.,0.)) ;
#90250 = DIRECTION('',(1.,0.,0.)) ;
#90251 = DIRECTION('',(0.,-1.,0.)) ;
#90252 = DIRECTION('center_axis',(1.,0.,0.)) ;
#90253 = DIRECTION('ref_axis',(0.,0.,-1.)) ;
#90254 = DIRECTION('center_axis',(1.,0.,0.)) ;
#90255 = DIRECTION('ref_axis',(0.,0.,1.)) ;
#90256 = DIRECTION('',(1.,0.,0.)) ;
#90257 = DIRECTION('center_axis',(-1.,0.,0.)) ;
#90258 = DIRECTION('ref_axis',(0.,0.,-1.)) ;
#90259 = DIRECTION('center_axis',(0.,-1.,3.99416362155027E-15)) ;
#90260 = DIRECTION('ref_axis',(0.,-3.99416362155027E-15,-1.)) ;
#90261 = DIRECTION('',(0.,3.99416362155027E-15,1.)) ;
#90262 = DIRECTION('',(1.,0.,0.)) ;
#90263 = DIRECTION('',(0.,-3.99416362155027E-15,-1.)) ;
#90264 = DIRECTION('center_axis',(1.,0.,0.)) ;
#90265 = DIRECTION('ref_axis',(0.,0.,-1.)) ;
#90266 = DIRECTION('center_axis',(-1.,0.,0.)) ;
#90267 = DIRECTION('ref_axis',(0.,1.30104260698261E-14,-1.)) ;
#90268 = DIRECTION('',(1.,0.,0.)) ;
#90269 = DIRECTION('center_axis',(1.,0.,0.)) ;
#90270 = DIRECTION('ref_axis',(0.,0.,-1.)) ;
#90271 = DIRECTION('center_axis',(0.,-0.707106781186549,0.707106781186546)) ;
#90272 = DIRECTION('ref_axis',(0.,-0.707106781186546,-0.707106781186549)) ;
#90273 = DIRECTION('',(0.,0.707106781186546,0.707106781186549)) ;
#90274 = DIRECTION('',(1.,0.,0.)) ;
#90275 = DIRECTION('',(0.,-0.707106781186546,-0.707106781186549)) ;
#90276 = DIRECTION('center_axis',(1.,0.,0.)) ;
#90277 = DIRECTION('ref_axis',(0.,0.382683432365098,0.923879532511283)) ;
#90278 = DIRECTION('',(1.,0.,0.)) ;
#90279 = DIRECTION('center_axis',(1.,0.,0.)) ;
#90280 = DIRECTION('ref_axis',(0.,0.,-1.)) ;
#90281 = DIRECTION('center_axis',(0.,1.,0.)) ;
#90282 = DIRECTION('ref_axis',(0.,0.,1.)) ;
#90283 = DIRECTION('',(0.,0.,-1.)) ;
#90284 = DIRECTION('',(0.,0.,1.)) ;
#90285 = DIRECTION('center_axis',(0.,-0.707106781186547,-0.707106781186548)) ;
#90286 = DIRECTION('ref_axis',(0.,0.707106781186548,-0.707106781186547)) ;
#90287 = DIRECTION('',(0.,-0.707106781186548,0.707106781186547)) ;
#90288 = DIRECTION('',(1.,0.,0.)) ;
#90289 = DIRECTION('',(0.,0.707106781186548,-0.707106781186547)) ;
#90290 = DIRECTION('center_axis',(1.,0.,0.)) ;
#90291 = DIRECTION('ref_axis',(0.,0.,-1.)) ;
#90292 = DIRECTION('center_axis',(-1.,0.,0.)) ;
#90293 = DIRECTION('ref_axis',(0.,1.73472347597676E-14,-1.)) ;
#90294 = DIRECTION('',(1.,0.,0.)) ;
#90295 = DIRECTION('center_axis',(1.,0.,0.)) ;
#90296 = DIRECTION('ref_axis',(0.,0.,-1.)) ;
#90297 = DIRECTION('center_axis',(0.,-1.,0.)) ;
#90298 = DIRECTION('ref_axis',(0.,0.,-1.)) ;
#90299 = DIRECTION('',(0.,0.,1.)) ;
#90300 = DIRECTION('',(1.,0.,0.)) ;
#90301 = DIRECTION('',(0.,0.,-1.)) ;
#90302 = DIRECTION('center_axis',(1.,0.,0.)) ;
#90303 = DIRECTION('ref_axis',(0.,0.,-1.)) ;
#90304 = DIRECTION('center_axis',(1.,0.,0.)) ;
#90305 = DIRECTION('ref_axis',(0.,0.,1.)) ;
#90306 = DIRECTION('',(1.,0.,0.)) ;
#90307 = DIRECTION('center_axis',(-1.,0.,0.)) ;
#90308 = DIRECTION('ref_axis',(0.,0.,-1.)) ;
#90309 = DIRECTION('center_axis',(0.,0.,-1.)) ;
#90310 = DIRECTION('ref_axis',(-1.,0.,0.)) ;
#90311 = DIRECTION('',(0.,-1.,0.)) ;
#90312 = DIRECTION('',(1.,0.,0.)) ;
#90313 = DIRECTION('',(0.,1.,0.)) ;
#90314 = DIRECTION('center_axis',(1.,0.,0.)) ;
#90315 = DIRECTION('ref_axis',(0.,0.,-1.)) ;
#90316 = DIRECTION('center_axis',(1.,0.,0.)) ;
#90317 = DIRECTION('ref_axis',(0.,0.,1.)) ;
#90318 = DIRECTION('',(1.,0.,0.)) ;
#90319 = DIRECTION('center_axis',(-1.,0.,0.)) ;
#90320 = DIRECTION('ref_axis',(0.,0.,-1.)) ;
#90321 = DIRECTION('center_axis',(0.,1.,0.)) ;
#90322 = DIRECTION('ref_axis',(0.,0.,1.)) ;
#90323 = DIRECTION('',(0.,0.,-1.)) ;
#90324 = DIRECTION('',(1.,0.,0.)) ;
#90325 = DIRECTION('',(0.,0.,1.)) ;
#90326 = DIRECTION('center_axis',(1.,0.,0.)) ;
#90327 = DIRECTION('ref_axis',(0.,0.,-1.)) ;
#90328 = DIRECTION('center_axis',(-1.,0.,0.)) ;
#90329 = DIRECTION('ref_axis',(0.,1.95156391047385E-14,-1.)) ;
#90330 = DIRECTION('',(1.,0.,0.)) ;
#90331 = DIRECTION('center_axis',(1.,0.,0.)) ;
#90332 = DIRECTION('ref_axis',(0.,0.,-1.)) ;
#90333 = DIRECTION('center_axis',(0.,1.07081696047951E-16,-1.)) ;
#90334 = DIRECTION('ref_axis',(0.,1.,1.07081696047951E-16)) ;
#90335 = DIRECTION('',(0.,-1.,-1.07081696047951E-16)) ;
#90336 = DIRECTION('',(1.,0.,0.)) ;
#90337 = DIRECTION('',(0.,1.,1.07081696047951E-16)) ;
#90338 = DIRECTION('center_axis',(1.,0.,0.)) ;
#90339 = DIRECTION('ref_axis',(0.,0.,-1.)) ;
#90340 = DIRECTION('center_axis',(-1.,0.,0.)) ;
#90341 = DIRECTION('ref_axis',(0.,0.,-1.)) ;
#90342 = DIRECTION('',(1.,0.,0.)) ;
#90343 = DIRECTION('center_axis',(1.,0.,0.)) ;
#90344 = DIRECTION('ref_axis',(0.,0.,-1.)) ;
#90345 = DIRECTION('center_axis',(0.,-1.,0.)) ;
#90346 = DIRECTION('ref_axis',(0.,0.,-1.)) ;
#90347 = DIRECTION('',(0.,0.,1.)) ;
#90348 = DIRECTION('',(1.,0.,0.)) ;
#90349 = DIRECTION('',(0.,0.,-1.)) ;
#90350 = DIRECTION('center_axis',(1.,0.,0.)) ;
#90351 = DIRECTION('ref_axis',(0.,0.,-1.)) ;
#90352 = DIRECTION('center_axis',(-1.,0.,0.)) ;
#90353 = DIRECTION('ref_axis',(0.,3.03576608295933E-14,-1.)) ;
#90354 = DIRECTION('',(1.,0.,0.)) ;
#90355 = DIRECTION('center_axis',(1.,0.,0.)) ;
#90356 = DIRECTION('ref_axis',(0.,0.,-1.)) ;
#90357 = DIRECTION('center_axis',(1.,0.,0.)) ;
#90358 = DIRECTION('ref_axis',(0.,0.,-1.)) ;
#90359 = DIRECTION('center_axis',(1.,0.,0.)) ;
#90360 = DIRECTION('ref_axis',(0.,-7.85535158932895E-16,1.)) ;
#90361 = DIRECTION('',(1.,0.,0.)) ;
#90362 = DIRECTION('center_axis',(-1.,0.,0.)) ;
#90363 = DIRECTION('ref_axis',(0.,-7.85535158932895E-16,-1.)) ;
#90364 = DIRECTION('center_axis',(1.,0.,0.)) ;
#90365 = DIRECTION('ref_axis',(0.,0.,-1.)) ;
#90366 = DIRECTION('center_axis',(-1.,0.,0.)) ;
#90367 = DIRECTION('ref_axis',(0.,4.33680868994204E-15,-1.)) ;
#90368 = DIRECTION('',(1.,0.,0.)) ;
#90369 = DIRECTION('center_axis',(1.,0.,0.)) ;
#90370 = DIRECTION('ref_axis',(0.,0.,-1.)) ;
#90371 = DIRECTION('center_axis',(0.,-1.,0.)) ;
#90372 = DIRECTION('ref_axis',(0.,0.,-1.)) ;
#90373 = DIRECTION('',(0.,0.,1.)) ;
#90374 = DIRECTION('',(1.,0.,0.)) ;
#90375 = DIRECTION('',(0.,0.,-1.)) ;
#90376 = DIRECTION('center_axis',(1.,0.,0.)) ;
#90377 = DIRECTION('ref_axis',(0.,0.,-1.)) ;
#90378 = DIRECTION('center_axis',(-1.,0.,0.)) ;
#90379 = DIRECTION('ref_axis',(0.,0.,-1.)) ;
#90380 = DIRECTION('',(1.,0.,0.)) ;
#90381 = DIRECTION('center_axis',(1.,0.,0.)) ;
#90382 = DIRECTION('ref_axis',(0.,0.,-1.)) ;
#90383 = DIRECTION('center_axis',(0.,-1.07081696047951E-16,1.)) ;
#90384 = DIRECTION('ref_axis',(0.,-1.,-1.07081696047951E-16)) ;
#90385 = DIRECTION('',(0.,1.,1.07081696047951E-16)) ;
#90386 = DIRECTION('',(1.,0.,0.)) ;
#90387 = DIRECTION('',(0.,-1.,-1.07081696047951E-16)) ;
#90388 = DIRECTION('center_axis',(1.,0.,0.)) ;
#90389 = DIRECTION('ref_axis',(0.,0.,-1.)) ;
#90390 = DIRECTION('center_axis',(-1.,0.,0.)) ;
#90391 = DIRECTION('ref_axis',(0.,0.,-1.)) ;
#90392 = DIRECTION('',(1.,0.,0.)) ;
#90393 = DIRECTION('center_axis',(1.,0.,0.)) ;
#90394 = DIRECTION('ref_axis',(0.,0.,-1.)) ;
#90395 = DIRECTION('center_axis',(0.,1.,0.)) ;
#90396 = DIRECTION('ref_axis',(0.,0.,1.)) ;
#90397 = DIRECTION('',(0.,0.,-1.)) ;
#90398 = DIRECTION('',(0.,0.,1.)) ;
#90399 = DIRECTION('center_axis',(-1.,0.,0.)) ;
#90400 = DIRECTION('ref_axis',(0.,0.,1.)) ;
#90401 = DIRECTION('center_axis',(-1.,0.,0.)) ;
#90402 = DIRECTION('ref_axis',(0.,0.,1.)) ;
#90403 = DIRECTION('',(0.,-1.,0.)) ;
#90404 = DIRECTION('center_axis',(-1.,0.,0.)) ;
#90405 = DIRECTION('ref_axis',(0.,0.,1.)) ;
#90406 = DIRECTION('',(0.,0.,1.)) ;
#90407 = DIRECTION('',(0.,-1.,-1.07081696047951E-16)) ;
#90408 = DIRECTION('',(0.,0.,-1.)) ;
#90409 = DIRECTION('center_axis',(-1.,0.,0.)) ;
#90410 = DIRECTION('ref_axis',(0.,0.,1.)) ;
#90411 = DIRECTION('',(0.,0.,-1.)) ;
#90412 = DIRECTION('',(0.,1.,1.07081696047951E-16)) ;
#90413 = DIRECTION('',(0.,0.,1.)) ;
#90414 = DIRECTION('center_axis',(-1.,0.,0.)) ;
#90415 = DIRECTION('ref_axis',(0.,0.,1.)) ;
#90416 = DIRECTION('',(0.,1.,0.)) ;
#90417 = DIRECTION('center_axis',(-1.,0.,0.)) ;
#90418 = DIRECTION('ref_axis',(0.,0.,1.)) ;
#90419 = DIRECTION('',(0.,0.,-1.)) ;
#90420 = DIRECTION('',(0.,0.707106781186548,-0.707106781186547)) ;
#90421 = DIRECTION('',(0.,0.,1.)) ;
#90422 = DIRECTION('',(0.,-0.707106781186546,-0.707106781186549)) ;
#90423 = DIRECTION('',(0.,-3.99416362155027E-15,-1.)) ;
#90424 = DIRECTION('center_axis',(1.,0.,0.)) ;
#90425 = DIRECTION('ref_axis',(0.,0.,-1.)) ;
#90426 = DIRECTION('',(1.,0.,0.)) ;
#90427 = DIRECTION('center_axis',(1.,0.,0.)) ;
#90428 = DIRECTION('ref_axis',(0.,0.,1.)) ;
#90429 = DIRECTION('',(1.,0.,0.)) ;
#90430 = DIRECTION('center_axis',(-1.,0.,0.)) ;
#90431 = DIRECTION('ref_axis',(0.,0.,-1.)) ;
#90432 = DIRECTION('center_axis',(0.,0.,1.)) ;
#90433 = DIRECTION('ref_axis',(1.,0.,0.)) ;
#90434 = DIRECTION('',(0.,1.,0.)) ;
#90435 = DIRECTION('',(1.,0.,0.)) ;
#90436 = DIRECTION('',(0.,-1.,0.)) ;
#90437 = DIRECTION('center_axis',(1.,0.,0.)) ;
#90438 = DIRECTION('ref_axis',(0.,0.,-1.)) ;
#90439 = DIRECTION('center_axis',(1.,0.,0.)) ;
#90440 = DIRECTION('ref_axis',(0.,0.,1.)) ;
#90441 = DIRECTION('',(1.,0.,0.)) ;
#90442 = DIRECTION('center_axis',(-1.,0.,0.)) ;
#90443 = DIRECTION('ref_axis',(0.,0.,-1.)) ;
#90444 = DIRECTION('center_axis',(0.,-1.,3.99416362155027E-15)) ;
#90445 = DIRECTION('ref_axis',(0.,-3.99416362155027E-15,-1.)) ;
#90446 = DIRECTION('',(0.,3.99416362155027E-15,1.)) ;
#90447 = DIRECTION('',(1.,0.,0.)) ;
#90448 = DIRECTION('',(0.,-3.99416362155027E-15,-1.)) ;
#90449 = DIRECTION('center_axis',(1.,0.,0.)) ;
#90450 = DIRECTION('ref_axis',(0.,0.,-1.)) ;
#90451 = DIRECTION('center_axis',(-1.,0.,0.)) ;
#90452 = DIRECTION('ref_axis',(0.,1.30104260698261E-14,-1.)) ;
#90453 = DIRECTION('',(1.,0.,0.)) ;
#90454 = DIRECTION('center_axis',(1.,0.,0.)) ;
#90455 = DIRECTION('ref_axis',(0.,0.,-1.)) ;
#90456 = DIRECTION('center_axis',(0.,-0.707106781186549,0.707106781186546)) ;
#90457 = DIRECTION('ref_axis',(0.,-0.707106781186546,-0.707106781186549)) ;
#90458 = DIRECTION('',(0.,0.707106781186546,0.707106781186549)) ;
#90459 = DIRECTION('',(1.,0.,0.)) ;
#90460 = DIRECTION('',(0.,-0.707106781186546,-0.707106781186549)) ;
#90461 = DIRECTION('center_axis',(1.,0.,0.)) ;
#90462 = DIRECTION('ref_axis',(0.,0.382683432365098,0.923879532511283)) ;
#90463 = DIRECTION('',(1.,0.,0.)) ;
#90464 = DIRECTION('center_axis',(1.,0.,0.)) ;
#90465 = DIRECTION('ref_axis',(0.,0.,-1.)) ;
#90466 = DIRECTION('center_axis',(0.,1.,0.)) ;
#90467 = DIRECTION('ref_axis',(0.,0.,1.)) ;
#90468 = DIRECTION('',(0.,0.,-1.)) ;
#90469 = DIRECTION('',(0.,0.,1.)) ;
#90470 = DIRECTION('center_axis',(0.,-0.707106781186547,-0.707106781186548)) ;
#90471 = DIRECTION('ref_axis',(0.,0.707106781186548,-0.707106781186547)) ;
#90472 = DIRECTION('',(0.,-0.707106781186548,0.707106781186547)) ;
#90473 = DIRECTION('',(1.,0.,0.)) ;
#90474 = DIRECTION('',(0.,0.707106781186548,-0.707106781186547)) ;
#90475 = DIRECTION('center_axis',(1.,0.,0.)) ;
#90476 = DIRECTION('ref_axis',(0.,0.,-1.)) ;
#90477 = DIRECTION('center_axis',(-1.,0.,0.)) ;
#90478 = DIRECTION('ref_axis',(0.,-1.73472347597682E-14,-1.)) ;
#90479 = DIRECTION('',(1.,0.,0.)) ;
#90480 = DIRECTION('center_axis',(1.,0.,0.)) ;
#90481 = DIRECTION('ref_axis',(0.,0.,-1.)) ;
#90482 = DIRECTION('center_axis',(0.,-1.,0.)) ;
#90483 = DIRECTION('ref_axis',(0.,0.,-1.)) ;
#90484 = DIRECTION('',(0.,0.,1.)) ;
#90485 = DIRECTION('',(1.,0.,0.)) ;
#90486 = DIRECTION('',(0.,0.,-1.)) ;
#90487 = DIRECTION('center_axis',(1.,0.,0.)) ;
#90488 = DIRECTION('ref_axis',(0.,0.,-1.)) ;
#90489 = DIRECTION('center_axis',(1.,0.,0.)) ;
#90490 = DIRECTION('ref_axis',(0.,0.,1.)) ;
#90491 = DIRECTION('',(1.,0.,0.)) ;
#90492 = DIRECTION('center_axis',(-1.,0.,0.)) ;
#90493 = DIRECTION('ref_axis',(0.,0.,-1.)) ;
#90494 = DIRECTION('center_axis',(0.,0.,-1.)) ;
#90495 = DIRECTION('ref_axis',(-1.,0.,0.)) ;
#90496 = DIRECTION('',(0.,-1.,0.)) ;
#90497 = DIRECTION('',(1.,0.,0.)) ;
#90498 = DIRECTION('',(0.,1.,0.)) ;
#90499 = DIRECTION('center_axis',(1.,0.,0.)) ;
#90500 = DIRECTION('ref_axis',(0.,0.,-1.)) ;
#90501 = DIRECTION('center_axis',(1.,0.,0.)) ;
#90502 = DIRECTION('ref_axis',(0.,0.,1.)) ;
#90503 = DIRECTION('',(1.,0.,0.)) ;
#90504 = DIRECTION('center_axis',(-1.,0.,0.)) ;
#90505 = DIRECTION('ref_axis',(0.,0.,-1.)) ;
#90506 = DIRECTION('center_axis',(0.,1.,0.)) ;
#90507 = DIRECTION('ref_axis',(0.,0.,1.)) ;
#90508 = DIRECTION('',(0.,0.,-1.)) ;
#90509 = DIRECTION('',(1.,0.,0.)) ;
#90510 = DIRECTION('',(0.,0.,1.)) ;
#90511 = DIRECTION('center_axis',(1.,0.,0.)) ;
#90512 = DIRECTION('ref_axis',(0.,0.,-1.)) ;
#90513 = DIRECTION('center_axis',(-1.,0.,0.)) ;
#90514 = DIRECTION('ref_axis',(0.,1.95156391047392E-14,-1.)) ;
#90515 = DIRECTION('',(1.,0.,0.)) ;
#90516 = DIRECTION('center_axis',(1.,0.,0.)) ;
#90517 = DIRECTION('ref_axis',(0.,0.,-1.)) ;
#90518 = DIRECTION('center_axis',(0.,1.07081696047951E-16,-1.)) ;
#90519 = DIRECTION('ref_axis',(0.,1.,1.07081696047951E-16)) ;
#90520 = DIRECTION('',(0.,-1.,-1.07081696047951E-16)) ;
#90521 = DIRECTION('',(1.,0.,0.)) ;
#90522 = DIRECTION('',(0.,1.,1.07081696047951E-16)) ;
#90523 = DIRECTION('center_axis',(1.,0.,0.)) ;
#90524 = DIRECTION('ref_axis',(0.,0.,-1.)) ;
#90525 = DIRECTION('center_axis',(-1.,0.,0.)) ;
#90526 = DIRECTION('ref_axis',(0.,0.,-1.)) ;
#90527 = DIRECTION('',(1.,0.,0.)) ;
#90528 = DIRECTION('center_axis',(1.,0.,0.)) ;
#90529 = DIRECTION('ref_axis',(0.,0.,-1.)) ;
#90530 = DIRECTION('center_axis',(0.,-1.,0.)) ;
#90531 = DIRECTION('ref_axis',(0.,0.,-1.)) ;
#90532 = DIRECTION('',(0.,0.,1.)) ;
#90533 = DIRECTION('',(1.,0.,0.)) ;
#90534 = DIRECTION('',(0.,0.,-1.)) ;
#90535 = DIRECTION('center_axis',(1.,0.,0.)) ;
#90536 = DIRECTION('ref_axis',(0.,0.,-1.)) ;
#90537 = DIRECTION('center_axis',(-1.,0.,0.)) ;
#90538 = DIRECTION('ref_axis',(0.,4.33680868994204E-15,-1.)) ;
#90539 = DIRECTION('',(1.,0.,0.)) ;
#90540 = DIRECTION('center_axis',(1.,0.,0.)) ;
#90541 = DIRECTION('ref_axis',(0.,0.,-1.)) ;
#90542 = DIRECTION('center_axis',(1.,0.,0.)) ;
#90543 = DIRECTION('ref_axis',(0.,0.,-1.)) ;
#90544 = DIRECTION('center_axis',(1.,0.,0.)) ;
#90545 = DIRECTION('ref_axis',(0.,-7.85535158932895E-16,1.)) ;
#90546 = DIRECTION('',(1.,0.,0.)) ;
#90547 = DIRECTION('center_axis',(-1.,0.,0.)) ;
#90548 = DIRECTION('ref_axis',(0.,-7.85535158932895E-16,-1.)) ;
#90549 = DIRECTION('center_axis',(1.,0.,0.)) ;
#90550 = DIRECTION('ref_axis',(0.,0.,-1.)) ;
#90551 = DIRECTION('center_axis',(-1.,0.,0.)) ;
#90552 = DIRECTION('ref_axis',(0.,4.33680868994204E-15,-1.)) ;
#90553 = DIRECTION('',(1.,0.,0.)) ;
#90554 = DIRECTION('center_axis',(1.,0.,0.)) ;
#90555 = DIRECTION('ref_axis',(0.,0.,-1.)) ;
#90556 = DIRECTION('center_axis',(0.,-1.,0.)) ;
#90557 = DIRECTION('ref_axis',(0.,0.,-1.)) ;
#90558 = DIRECTION('',(0.,0.,1.)) ;
#90559 = DIRECTION('',(1.,0.,0.)) ;
#90560 = DIRECTION('',(0.,0.,-1.)) ;
#90561 = DIRECTION('center_axis',(1.,0.,0.)) ;
#90562 = DIRECTION('ref_axis',(0.,0.,-1.)) ;
#90563 = DIRECTION('center_axis',(-1.,0.,0.)) ;
#90564 = DIRECTION('ref_axis',(0.,0.,-1.)) ;
#90565 = DIRECTION('',(1.,0.,0.)) ;
#90566 = DIRECTION('center_axis',(1.,0.,0.)) ;
#90567 = DIRECTION('ref_axis',(0.,0.,-1.)) ;
#90568 = DIRECTION('center_axis',(0.,-1.07081696047951E-16,1.)) ;
#90569 = DIRECTION('ref_axis',(0.,-1.,-1.07081696047951E-16)) ;
#90570 = DIRECTION('',(0.,1.,1.07081696047951E-16)) ;
#90571 = DIRECTION('',(1.,0.,0.)) ;
#90572 = DIRECTION('',(0.,-1.,-1.07081696047951E-16)) ;
#90573 = DIRECTION('center_axis',(1.,0.,0.)) ;
#90574 = DIRECTION('ref_axis',(0.,0.,-1.)) ;
#90575 = DIRECTION('center_axis',(-1.,0.,0.)) ;
#90576 = DIRECTION('ref_axis',(0.,0.,-1.)) ;
#90577 = DIRECTION('',(1.,0.,0.)) ;
#90578 = DIRECTION('center_axis',(1.,0.,0.)) ;
#90579 = DIRECTION('ref_axis',(0.,0.,-1.)) ;
#90580 = DIRECTION('center_axis',(0.,1.,0.)) ;
#90581 = DIRECTION('ref_axis',(0.,0.,1.)) ;
#90582 = DIRECTION('',(0.,0.,-1.)) ;
#90583 = DIRECTION('',(0.,0.,1.)) ;
#90584 = DIRECTION('center_axis',(-1.,0.,0.)) ;
#90585 = DIRECTION('ref_axis',(0.,0.,1.)) ;
#90586 = DIRECTION('center_axis',(-1.,0.,0.)) ;
#90587 = DIRECTION('ref_axis',(0.,0.,1.)) ;
#90588 = DIRECTION('',(0.,-1.,0.)) ;
#90589 = DIRECTION('center_axis',(-1.,0.,0.)) ;
#90590 = DIRECTION('ref_axis',(0.,0.,1.)) ;
#90591 = DIRECTION('',(0.,0.,1.)) ;
#90592 = DIRECTION('',(0.,-1.,-1.07081696047951E-16)) ;
#90593 = DIRECTION('',(0.,0.,-1.)) ;
#90594 = DIRECTION('center_axis',(-1.,0.,0.)) ;
#90595 = DIRECTION('ref_axis',(0.,0.,1.)) ;
#90596 = DIRECTION('',(0.,0.,-1.)) ;
#90597 = DIRECTION('',(0.,1.,1.07081696047951E-16)) ;
#90598 = DIRECTION('',(0.,0.,1.)) ;
#90599 = DIRECTION('center_axis',(-1.,0.,0.)) ;
#90600 = DIRECTION('ref_axis',(0.,0.,1.)) ;
#90601 = DIRECTION('',(0.,1.,0.)) ;
#90602 = DIRECTION('center_axis',(-1.,0.,0.)) ;
#90603 = DIRECTION('ref_axis',(0.,0.,1.)) ;
#90604 = DIRECTION('',(0.,0.,-1.)) ;
#90605 = DIRECTION('',(0.,0.707106781186548,-0.707106781186547)) ;
#90606 = DIRECTION('',(0.,0.,1.)) ;
#90607 = DIRECTION('',(0.,-0.707106781186546,-0.707106781186549)) ;
#90608 = DIRECTION('',(0.,-3.99416362155027E-15,-1.)) ;
#90609 = DIRECTION('center_axis',(1.,0.,0.)) ;
#90610 = DIRECTION('ref_axis',(0.,0.,-1.)) ;
#90611 = DIRECTION('',(1.,0.,0.)) ;
#90612 = DIRECTION('center_axis',(1.,0.,0.)) ;
#90613 = DIRECTION('ref_axis',(0.,0.,1.)) ;
#90614 = DIRECTION('',(1.,0.,0.)) ;
#90615 = DIRECTION('center_axis',(-1.,0.,0.)) ;
#90616 = DIRECTION('ref_axis',(0.,0.,-1.)) ;
#90617 = DIRECTION('center_axis',(0.,0.,1.)) ;
#90618 = DIRECTION('ref_axis',(1.,0.,0.)) ;
#90619 = DIRECTION('',(0.,1.,0.)) ;
#90620 = DIRECTION('',(1.,0.,0.)) ;
#90621 = DIRECTION('',(0.,-1.,0.)) ;
#90622 = DIRECTION('center_axis',(1.,0.,0.)) ;
#90623 = DIRECTION('ref_axis',(0.,0.,-1.)) ;
#90624 = DIRECTION('center_axis',(1.,0.,0.)) ;
#90625 = DIRECTION('ref_axis',(0.,0.,1.)) ;
#90626 = DIRECTION('',(1.,0.,0.)) ;
#90627 = DIRECTION('center_axis',(-1.,0.,0.)) ;
#90628 = DIRECTION('ref_axis',(0.,0.,-1.)) ;
#90629 = DIRECTION('center_axis',(0.,-1.,3.99416362155027E-15)) ;
#90630 = DIRECTION('ref_axis',(0.,-3.99416362155027E-15,-1.)) ;
#90631 = DIRECTION('',(0.,3.99416362155027E-15,1.)) ;
#90632 = DIRECTION('',(1.,0.,0.)) ;
#90633 = DIRECTION('',(0.,-3.99416362155027E-15,-1.)) ;
#90634 = DIRECTION('center_axis',(1.,0.,0.)) ;
#90635 = DIRECTION('ref_axis',(0.,0.,-1.)) ;
#90636 = DIRECTION('center_axis',(-1.,0.,0.)) ;
#90637 = DIRECTION('ref_axis',(0.,1.30104260698261E-14,-1.)) ;
#90638 = DIRECTION('',(1.,0.,0.)) ;
#90639 = DIRECTION('center_axis',(1.,0.,0.)) ;
#90640 = DIRECTION('ref_axis',(0.,0.,-1.)) ;
#90641 = DIRECTION('center_axis',(0.,-0.707106781186549,0.707106781186546)) ;
#90642 = DIRECTION('ref_axis',(0.,-0.707106781186546,-0.707106781186549)) ;
#90643 = DIRECTION('',(0.,0.707106781186546,0.707106781186549)) ;
#90644 = DIRECTION('',(1.,0.,0.)) ;
#90645 = DIRECTION('',(0.,-0.707106781186546,-0.707106781186549)) ;
#90646 = DIRECTION('center_axis',(1.,0.,0.)) ;
#90647 = DIRECTION('ref_axis',(0.,0.382683432365098,0.923879532511283)) ;
#90648 = DIRECTION('',(1.,0.,0.)) ;
#90649 = DIRECTION('center_axis',(1.,0.,0.)) ;
#90650 = DIRECTION('ref_axis',(0.,0.,-1.)) ;
#90651 = DIRECTION('center_axis',(0.,1.,0.)) ;
#90652 = DIRECTION('ref_axis',(0.,0.,1.)) ;
#90653 = DIRECTION('',(0.,0.,-1.)) ;
#90654 = DIRECTION('',(0.,0.,1.)) ;
#90655 = DIRECTION('center_axis',(0.,-0.707106781186547,-0.707106781186548)) ;
#90656 = DIRECTION('ref_axis',(0.,0.707106781186548,-0.707106781186547)) ;
#90657 = DIRECTION('',(0.,-0.707106781186548,0.707106781186547)) ;
#90658 = DIRECTION('',(1.,0.,0.)) ;
#90659 = DIRECTION('',(0.,0.707106781186548,-0.707106781186547)) ;
#90660 = DIRECTION('center_axis',(1.,0.,0.)) ;
#90661 = DIRECTION('ref_axis',(0.,0.,-1.)) ;
#90662 = DIRECTION('center_axis',(-1.,0.,0.)) ;
#90663 = DIRECTION('ref_axis',(0.,-1.73472347597682E-14,-1.)) ;
#90664 = DIRECTION('',(1.,0.,0.)) ;
#90665 = DIRECTION('center_axis',(1.,0.,0.)) ;
#90666 = DIRECTION('ref_axis',(0.,0.,-1.)) ;
#90667 = DIRECTION('center_axis',(0.,-1.,0.)) ;
#90668 = DIRECTION('ref_axis',(0.,0.,-1.)) ;
#90669 = DIRECTION('',(0.,0.,1.)) ;
#90670 = DIRECTION('',(1.,0.,0.)) ;
#90671 = DIRECTION('',(0.,0.,-1.)) ;
#90672 = DIRECTION('center_axis',(1.,0.,0.)) ;
#90673 = DIRECTION('ref_axis',(0.,0.,-1.)) ;
#90674 = DIRECTION('center_axis',(1.,0.,0.)) ;
#90675 = DIRECTION('ref_axis',(0.,0.,1.)) ;
#90676 = DIRECTION('',(1.,0.,0.)) ;
#90677 = DIRECTION('center_axis',(-1.,0.,0.)) ;
#90678 = DIRECTION('ref_axis',(0.,0.,-1.)) ;
#90679 = DIRECTION('center_axis',(0.,0.,-1.)) ;
#90680 = DIRECTION('ref_axis',(-1.,0.,0.)) ;
#90681 = DIRECTION('',(0.,-1.,0.)) ;
#90682 = DIRECTION('',(1.,0.,0.)) ;
#90683 = DIRECTION('',(0.,1.,0.)) ;
#90684 = DIRECTION('center_axis',(1.,0.,0.)) ;
#90685 = DIRECTION('ref_axis',(0.,0.,-1.)) ;
#90686 = DIRECTION('center_axis',(1.,0.,0.)) ;
#90687 = DIRECTION('ref_axis',(0.,0.,1.)) ;
#90688 = DIRECTION('',(1.,0.,0.)) ;
#90689 = DIRECTION('center_axis',(-1.,0.,0.)) ;
#90690 = DIRECTION('ref_axis',(0.,0.,-1.)) ;
#90691 = DIRECTION('center_axis',(0.,1.,0.)) ;
#90692 = DIRECTION('ref_axis',(0.,0.,1.)) ;
#90693 = DIRECTION('',(0.,0.,-1.)) ;
#90694 = DIRECTION('',(1.,0.,0.)) ;
#90695 = DIRECTION('',(0.,0.,1.)) ;
#90696 = DIRECTION('center_axis',(1.,0.,0.)) ;
#90697 = DIRECTION('ref_axis',(0.,0.,-1.)) ;
#90698 = DIRECTION('center_axis',(-1.,0.,0.)) ;
#90699 = DIRECTION('ref_axis',(0.,1.95156391047392E-14,-1.)) ;
#90700 = DIRECTION('',(1.,0.,0.)) ;
#90701 = DIRECTION('center_axis',(1.,0.,0.)) ;
#90702 = DIRECTION('ref_axis',(0.,0.,-1.)) ;
#90703 = DIRECTION('center_axis',(0.,1.07081696047951E-16,-1.)) ;
#90704 = DIRECTION('ref_axis',(0.,1.,1.07081696047951E-16)) ;
#90705 = DIRECTION('',(0.,-1.,-1.07081696047951E-16)) ;
#90706 = DIRECTION('',(1.,0.,0.)) ;
#90707 = DIRECTION('',(0.,1.,1.07081696047951E-16)) ;
#90708 = DIRECTION('center_axis',(1.,0.,0.)) ;
#90709 = DIRECTION('ref_axis',(0.,0.,-1.)) ;
#90710 = DIRECTION('center_axis',(-1.,0.,0.)) ;
#90711 = DIRECTION('ref_axis',(0.,0.,-1.)) ;
#90712 = DIRECTION('',(1.,0.,0.)) ;
#90713 = DIRECTION('center_axis',(1.,0.,0.)) ;
#90714 = DIRECTION('ref_axis',(0.,0.,-1.)) ;
#90715 = DIRECTION('center_axis',(0.,-1.,0.)) ;
#90716 = DIRECTION('ref_axis',(0.,0.,-1.)) ;
#90717 = DIRECTION('',(0.,0.,1.)) ;
#90718 = DIRECTION('',(1.,0.,0.)) ;
#90719 = DIRECTION('',(0.,0.,-1.)) ;
#90720 = DIRECTION('center_axis',(1.,0.,0.)) ;
#90721 = DIRECTION('ref_axis',(0.,0.,-1.)) ;
#90722 = DIRECTION('center_axis',(-1.,0.,0.)) ;
#90723 = DIRECTION('ref_axis',(0.,4.33680868994204E-15,-1.)) ;
#90724 = DIRECTION('',(1.,0.,0.)) ;
#90725 = DIRECTION('center_axis',(1.,0.,0.)) ;
#90726 = DIRECTION('ref_axis',(0.,0.,-1.)) ;
#90727 = DIRECTION('center_axis',(1.,0.,0.)) ;
#90728 = DIRECTION('ref_axis',(0.,0.,-1.)) ;
#90729 = DIRECTION('center_axis',(1.,0.,0.)) ;
#90730 = DIRECTION('ref_axis',(0.,-7.85535158932895E-16,1.)) ;
#90731 = DIRECTION('',(1.,0.,0.)) ;
#90732 = DIRECTION('center_axis',(-1.,0.,0.)) ;
#90733 = DIRECTION('ref_axis',(0.,-7.85535158932895E-16,-1.)) ;
#90734 = DIRECTION('center_axis',(1.,0.,0.)) ;
#90735 = DIRECTION('ref_axis',(0.,0.,-1.)) ;
#90736 = DIRECTION('center_axis',(-1.,0.,0.)) ;
#90737 = DIRECTION('ref_axis',(0.,4.33680868994204E-15,-1.)) ;
#90738 = DIRECTION('',(1.,0.,0.)) ;
#90739 = DIRECTION('center_axis',(1.,0.,0.)) ;
#90740 = DIRECTION('ref_axis',(0.,0.,-1.)) ;
#90741 = DIRECTION('center_axis',(0.,-1.,0.)) ;
#90742 = DIRECTION('ref_axis',(0.,0.,-1.)) ;
#90743 = DIRECTION('',(0.,0.,1.)) ;
#90744 = DIRECTION('',(1.,0.,0.)) ;
#90745 = DIRECTION('',(0.,0.,-1.)) ;
#90746 = DIRECTION('center_axis',(1.,0.,0.)) ;
#90747 = DIRECTION('ref_axis',(0.,0.,-1.)) ;
#90748 = DIRECTION('center_axis',(-1.,0.,0.)) ;
#90749 = DIRECTION('ref_axis',(0.,0.,-1.)) ;
#90750 = DIRECTION('',(1.,0.,0.)) ;
#90751 = DIRECTION('center_axis',(1.,0.,0.)) ;
#90752 = DIRECTION('ref_axis',(0.,0.,-1.)) ;
#90753 = DIRECTION('center_axis',(0.,-1.07081696047951E-16,1.)) ;
#90754 = DIRECTION('ref_axis',(0.,-1.,-1.07081696047951E-16)) ;
#90755 = DIRECTION('',(0.,1.,1.07081696047951E-16)) ;
#90756 = DIRECTION('',(1.,0.,0.)) ;
#90757 = DIRECTION('',(0.,-1.,-1.07081696047951E-16)) ;
#90758 = DIRECTION('center_axis',(1.,0.,0.)) ;
#90759 = DIRECTION('ref_axis',(0.,0.,-1.)) ;
#90760 = DIRECTION('center_axis',(-1.,0.,0.)) ;
#90761 = DIRECTION('ref_axis',(0.,0.,-1.)) ;
#90762 = DIRECTION('',(1.,0.,0.)) ;
#90763 = DIRECTION('center_axis',(1.,0.,0.)) ;
#90764 = DIRECTION('ref_axis',(0.,0.,-1.)) ;
#90765 = DIRECTION('center_axis',(0.,1.,0.)) ;
#90766 = DIRECTION('ref_axis',(0.,0.,1.)) ;
#90767 = DIRECTION('',(0.,0.,-1.)) ;
#90768 = DIRECTION('',(0.,0.,1.)) ;
#90769 = DIRECTION('center_axis',(-1.,0.,0.)) ;
#90770 = DIRECTION('ref_axis',(0.,0.,1.)) ;
#90771 = DIRECTION('center_axis',(-1.,0.,0.)) ;
#90772 = DIRECTION('ref_axis',(0.,0.,1.)) ;
#90773 = DIRECTION('',(0.,-1.,0.)) ;
#90774 = DIRECTION('center_axis',(-1.,0.,0.)) ;
#90775 = DIRECTION('ref_axis',(0.,0.,1.)) ;
#90776 = DIRECTION('',(0.,0.,1.)) ;
#90777 = DIRECTION('',(0.,-1.,-1.07081696047951E-16)) ;
#90778 = DIRECTION('',(0.,0.,-1.)) ;
#90779 = DIRECTION('center_axis',(-1.,0.,0.)) ;
#90780 = DIRECTION('ref_axis',(0.,0.,1.)) ;
#90781 = DIRECTION('',(0.,0.,-1.)) ;
#90782 = DIRECTION('',(0.,1.,1.07081696047951E-16)) ;
#90783 = DIRECTION('',(0.,0.,1.)) ;
#90784 = DIRECTION('center_axis',(-1.,0.,0.)) ;
#90785 = DIRECTION('ref_axis',(0.,0.,1.)) ;
#90786 = DIRECTION('',(0.,1.,0.)) ;
#90787 = DIRECTION('center_axis',(-1.,0.,0.)) ;
#90788 = DIRECTION('ref_axis',(0.,0.,1.)) ;
#90789 = DIRECTION('',(0.,0.,-1.)) ;
#90790 = DIRECTION('',(0.,0.707106781186548,-0.707106781186547)) ;
#90791 = DIRECTION('',(0.,0.,1.)) ;
#90792 = DIRECTION('',(0.,-0.707106781186546,-0.707106781186549)) ;
#90793 = DIRECTION('',(0.,-3.99416362155027E-15,-1.)) ;
#90794 = DIRECTION('center_axis',(1.,0.,0.)) ;
#90795 = DIRECTION('ref_axis',(0.,0.,-1.)) ;
#90796 = DIRECTION('',(1.,0.,0.)) ;
#90797 = DIRECTION('center_axis',(1.,0.,0.)) ;
#90798 = DIRECTION('ref_axis',(0.,0.,1.)) ;
#90799 = DIRECTION('',(1.,0.,0.)) ;
#90800 = DIRECTION('center_axis',(-1.,0.,0.)) ;
#90801 = DIRECTION('ref_axis',(0.,0.,-1.)) ;
#90802 = DIRECTION('center_axis',(0.,0.,1.)) ;
#90803 = DIRECTION('ref_axis',(1.,0.,0.)) ;
#90804 = DIRECTION('',(0.,1.,0.)) ;
#90805 = DIRECTION('',(1.,0.,0.)) ;
#90806 = DIRECTION('',(0.,-1.,0.)) ;
#90807 = DIRECTION('center_axis',(1.,0.,0.)) ;
#90808 = DIRECTION('ref_axis',(0.,0.,-1.)) ;
#90809 = DIRECTION('center_axis',(1.,0.,0.)) ;
#90810 = DIRECTION('ref_axis',(0.,0.,1.)) ;
#90811 = DIRECTION('',(1.,0.,0.)) ;
#90812 = DIRECTION('center_axis',(-1.,0.,0.)) ;
#90813 = DIRECTION('ref_axis',(0.,0.,-1.)) ;
#90814 = DIRECTION('center_axis',(0.,-1.,3.99416362155027E-15)) ;
#90815 = DIRECTION('ref_axis',(0.,-3.99416362155027E-15,-1.)) ;
#90816 = DIRECTION('',(0.,3.99416362155027E-15,1.)) ;
#90817 = DIRECTION('',(1.,0.,0.)) ;
#90818 = DIRECTION('',(0.,-3.99416362155027E-15,-1.)) ;
#90819 = DIRECTION('center_axis',(1.,0.,0.)) ;
#90820 = DIRECTION('ref_axis',(0.,0.,-1.)) ;
#90821 = DIRECTION('center_axis',(-1.,0.,0.)) ;
#90822 = DIRECTION('ref_axis',(0.,1.30104260698261E-14,-1.)) ;
#90823 = DIRECTION('',(1.,0.,0.)) ;
#90824 = DIRECTION('center_axis',(1.,0.,0.)) ;
#90825 = DIRECTION('ref_axis',(0.,0.,-1.)) ;
#90826 = DIRECTION('center_axis',(0.,-0.707106781186549,0.707106781186546)) ;
#90827 = DIRECTION('ref_axis',(0.,-0.707106781186546,-0.707106781186549)) ;
#90828 = DIRECTION('',(0.,0.707106781186546,0.707106781186549)) ;
#90829 = DIRECTION('',(1.,0.,0.)) ;
#90830 = DIRECTION('',(0.,-0.707106781186546,-0.707106781186549)) ;
#90831 = DIRECTION('center_axis',(1.,0.,0.)) ;
#90832 = DIRECTION('ref_axis',(0.,0.38268343236508,0.923879532511291)) ;
#90833 = DIRECTION('',(1.,0.,0.)) ;
#90834 = DIRECTION('center_axis',(1.,0.,0.)) ;
#90835 = DIRECTION('ref_axis',(0.,0.,-1.)) ;
#90836 = DIRECTION('center_axis',(0.,1.,0.)) ;
#90837 = DIRECTION('ref_axis',(0.,0.,1.)) ;
#90838 = DIRECTION('',(0.,0.,-1.)) ;
#90839 = DIRECTION('',(0.,0.,1.)) ;
#90840 = DIRECTION('center_axis',(0.,-0.707106781186547,-0.707106781186548)) ;
#90841 = DIRECTION('ref_axis',(0.,0.707106781186548,-0.707106781186547)) ;
#90842 = DIRECTION('',(0.,-0.707106781186548,0.707106781186547)) ;
#90843 = DIRECTION('',(1.,0.,0.)) ;
#90844 = DIRECTION('',(0.,0.707106781186548,-0.707106781186547)) ;
#90845 = DIRECTION('center_axis',(1.,0.,0.)) ;
#90846 = DIRECTION('ref_axis',(0.,0.,-1.)) ;
#90847 = DIRECTION('center_axis',(-1.,0.,0.)) ;
#90848 = DIRECTION('ref_axis',(0.,-1.73472347597682E-14,-1.)) ;
#90849 = DIRECTION('',(1.,0.,0.)) ;
#90850 = DIRECTION('center_axis',(1.,0.,0.)) ;
#90851 = DIRECTION('ref_axis',(0.,0.,-1.)) ;
#90852 = DIRECTION('center_axis',(0.,-1.,0.)) ;
#90853 = DIRECTION('ref_axis',(0.,0.,-1.)) ;
#90854 = DIRECTION('',(0.,0.,1.)) ;
#90855 = DIRECTION('',(1.,0.,0.)) ;
#90856 = DIRECTION('',(0.,0.,-1.)) ;
#90857 = DIRECTION('center_axis',(1.,0.,0.)) ;
#90858 = DIRECTION('ref_axis',(0.,0.,-1.)) ;
#90859 = DIRECTION('center_axis',(1.,0.,0.)) ;
#90860 = DIRECTION('ref_axis',(0.,0.,1.)) ;
#90861 = DIRECTION('',(1.,0.,0.)) ;
#90862 = DIRECTION('center_axis',(-1.,0.,0.)) ;
#90863 = DIRECTION('ref_axis',(0.,0.,-1.)) ;
#90864 = DIRECTION('center_axis',(0.,0.,-1.)) ;
#90865 = DIRECTION('ref_axis',(-1.,0.,0.)) ;
#90866 = DIRECTION('',(0.,-1.,0.)) ;
#90867 = DIRECTION('',(1.,0.,0.)) ;
#90868 = DIRECTION('',(0.,1.,0.)) ;
#90869 = DIRECTION('center_axis',(1.,0.,0.)) ;
#90870 = DIRECTION('ref_axis',(0.,0.,-1.)) ;
#90871 = DIRECTION('center_axis',(1.,0.,0.)) ;
#90872 = DIRECTION('ref_axis',(0.,0.,1.)) ;
#90873 = DIRECTION('',(1.,0.,0.)) ;
#90874 = DIRECTION('center_axis',(-1.,0.,0.)) ;
#90875 = DIRECTION('ref_axis',(0.,0.,-1.)) ;
#90876 = DIRECTION('center_axis',(0.,1.,0.)) ;
#90877 = DIRECTION('ref_axis',(0.,0.,1.)) ;
#90878 = DIRECTION('',(0.,0.,-1.)) ;
#90879 = DIRECTION('',(1.,0.,0.)) ;
#90880 = DIRECTION('',(0.,0.,1.)) ;
#90881 = DIRECTION('center_axis',(1.,0.,0.)) ;
#90882 = DIRECTION('ref_axis',(0.,0.,-1.)) ;
#90883 = DIRECTION('center_axis',(-1.,0.,0.)) ;
#90884 = DIRECTION('ref_axis',(0.,1.95156391047392E-14,-1.)) ;
#90885 = DIRECTION('',(1.,0.,0.)) ;
#90886 = DIRECTION('center_axis',(1.,0.,0.)) ;
#90887 = DIRECTION('ref_axis',(0.,0.,-1.)) ;
#90888 = DIRECTION('center_axis',(0.,1.07081696047951E-16,-1.)) ;
#90889 = DIRECTION('ref_axis',(0.,1.,1.07081696047951E-16)) ;
#90890 = DIRECTION('',(0.,-1.,-1.07081696047951E-16)) ;
#90891 = DIRECTION('',(1.,0.,0.)) ;
#90892 = DIRECTION('',(0.,1.,1.07081696047951E-16)) ;
#90893 = DIRECTION('center_axis',(1.,0.,0.)) ;
#90894 = DIRECTION('ref_axis',(0.,0.,-1.)) ;
#90895 = DIRECTION('center_axis',(-1.,0.,0.)) ;
#90896 = DIRECTION('ref_axis',(0.,0.,-1.)) ;
#90897 = DIRECTION('',(1.,0.,0.)) ;
#90898 = DIRECTION('center_axis',(1.,0.,0.)) ;
#90899 = DIRECTION('ref_axis',(0.,0.,-1.)) ;
#90900 = DIRECTION('center_axis',(0.,-1.,0.)) ;
#90901 = DIRECTION('ref_axis',(0.,0.,-1.)) ;
#90902 = DIRECTION('',(0.,0.,1.)) ;
#90903 = DIRECTION('',(1.,0.,0.)) ;
#90904 = DIRECTION('',(0.,0.,-1.)) ;
#90905 = DIRECTION('center_axis',(1.,0.,0.)) ;
#90906 = DIRECTION('ref_axis',(0.,0.,-1.)) ;
#90907 = DIRECTION('center_axis',(-1.,0.,0.)) ;
#90908 = DIRECTION('ref_axis',(0.,4.33680868994204E-15,-1.)) ;
#90909 = DIRECTION('',(1.,0.,0.)) ;
#90910 = DIRECTION('center_axis',(1.,0.,0.)) ;
#90911 = DIRECTION('ref_axis',(0.,0.,-1.)) ;
#90912 = DIRECTION('center_axis',(1.,0.,0.)) ;
#90913 = DIRECTION('ref_axis',(0.,0.,-1.)) ;
#90914 = DIRECTION('center_axis',(1.,0.,0.)) ;
#90915 = DIRECTION('ref_axis',(0.,-7.85535158932895E-16,1.)) ;
#90916 = DIRECTION('',(1.,0.,0.)) ;
#90917 = DIRECTION('center_axis',(-1.,0.,0.)) ;
#90918 = DIRECTION('ref_axis',(0.,-7.85535158932895E-16,-1.)) ;
#90919 = DIRECTION('center_axis',(1.,0.,0.)) ;
#90920 = DIRECTION('ref_axis',(0.,0.,-1.)) ;
#90921 = DIRECTION('center_axis',(-1.,0.,0.)) ;
#90922 = DIRECTION('ref_axis',(0.,4.33680868994204E-15,-1.)) ;
#90923 = DIRECTION('',(1.,0.,0.)) ;
#90924 = DIRECTION('center_axis',(1.,0.,0.)) ;
#90925 = DIRECTION('ref_axis',(0.,0.,-1.)) ;
#90926 = DIRECTION('center_axis',(0.,-1.,0.)) ;
#90927 = DIRECTION('ref_axis',(0.,0.,-1.)) ;
#90928 = DIRECTION('',(0.,0.,1.)) ;
#90929 = DIRECTION('',(1.,0.,0.)) ;
#90930 = DIRECTION('',(0.,0.,-1.)) ;
#90931 = DIRECTION('center_axis',(1.,0.,0.)) ;
#90932 = DIRECTION('ref_axis',(0.,0.,-1.)) ;
#90933 = DIRECTION('center_axis',(-1.,0.,0.)) ;
#90934 = DIRECTION('ref_axis',(0.,0.,-1.)) ;
#90935 = DIRECTION('',(1.,0.,0.)) ;
#90936 = DIRECTION('center_axis',(1.,0.,0.)) ;
#90937 = DIRECTION('ref_axis',(0.,0.,-1.)) ;
#90938 = DIRECTION('center_axis',(0.,-1.07081696047951E-16,1.)) ;
#90939 = DIRECTION('ref_axis',(0.,-1.,-1.07081696047951E-16)) ;
#90940 = DIRECTION('',(0.,1.,1.07081696047951E-16)) ;
#90941 = DIRECTION('',(1.,0.,0.)) ;
#90942 = DIRECTION('',(0.,-1.,-1.07081696047951E-16)) ;
#90943 = DIRECTION('center_axis',(1.,0.,0.)) ;
#90944 = DIRECTION('ref_axis',(0.,0.,-1.)) ;
#90945 = DIRECTION('center_axis',(-1.,0.,0.)) ;
#90946 = DIRECTION('ref_axis',(0.,0.,-1.)) ;
#90947 = DIRECTION('',(1.,0.,0.)) ;
#90948 = DIRECTION('center_axis',(1.,0.,0.)) ;
#90949 = DIRECTION('ref_axis',(0.,0.,-1.)) ;
#90950 = DIRECTION('center_axis',(0.,1.,0.)) ;
#90951 = DIRECTION('ref_axis',(0.,0.,1.)) ;
#90952 = DIRECTION('',(0.,0.,-1.)) ;
#90953 = DIRECTION('',(0.,0.,1.)) ;
#90954 = DIRECTION('center_axis',(-1.,0.,0.)) ;
#90955 = DIRECTION('ref_axis',(0.,0.,1.)) ;
#90956 = DIRECTION('center_axis',(-1.,0.,0.)) ;
#90957 = DIRECTION('ref_axis',(0.,0.,1.)) ;
#90958 = DIRECTION('',(0.,-1.,0.)) ;
#90959 = DIRECTION('center_axis',(-1.,0.,0.)) ;
#90960 = DIRECTION('ref_axis',(0.,0.,1.)) ;
#90961 = DIRECTION('',(0.,0.,1.)) ;
#90962 = DIRECTION('',(0.,-1.,-1.07081696047951E-16)) ;
#90963 = DIRECTION('',(0.,0.,-1.)) ;
#90964 = DIRECTION('center_axis',(-1.,0.,0.)) ;
#90965 = DIRECTION('ref_axis',(0.,0.,1.)) ;
#90966 = DIRECTION('',(0.,0.,-1.)) ;
#90967 = DIRECTION('',(0.,1.,1.07081696047951E-16)) ;
#90968 = DIRECTION('',(0.,0.,1.)) ;
#90969 = DIRECTION('center_axis',(-1.,0.,0.)) ;
#90970 = DIRECTION('ref_axis',(0.,0.,1.)) ;
#90971 = DIRECTION('',(0.,1.,0.)) ;
#90972 = DIRECTION('center_axis',(-1.,0.,0.)) ;
#90973 = DIRECTION('ref_axis',(0.,0.,1.)) ;
#90974 = DIRECTION('',(0.,0.,-1.)) ;
#90975 = DIRECTION('',(0.,0.707106781186548,-0.707106781186547)) ;
#90976 = DIRECTION('',(0.,0.,1.)) ;
#90977 = DIRECTION('',(0.,-0.707106781186546,-0.707106781186549)) ;
#90978 = DIRECTION('',(0.,-3.99416362155027E-15,-1.)) ;
#90979 = DIRECTION('center_axis',(1.,0.,0.)) ;
#90980 = DIRECTION('ref_axis',(0.,0.,-1.)) ;
#90981 = DIRECTION('',(1.,0.,0.)) ;
#90982 = DIRECTION('center_axis',(1.,0.,0.)) ;
#90983 = DIRECTION('ref_axis',(0.,0.,1.)) ;
#90984 = DIRECTION('',(1.,0.,0.)) ;
#90985 = DIRECTION('center_axis',(-1.,0.,0.)) ;
#90986 = DIRECTION('ref_axis',(0.,0.,-1.)) ;
#90987 = DIRECTION('center_axis',(0.,0.,1.)) ;
#90988 = DIRECTION('ref_axis',(1.,0.,0.)) ;
#90989 = DIRECTION('',(0.,1.,0.)) ;
#90990 = DIRECTION('',(1.,0.,0.)) ;
#90991 = DIRECTION('',(0.,-1.,0.)) ;
#90992 = DIRECTION('center_axis',(1.,0.,0.)) ;
#90993 = DIRECTION('ref_axis',(0.,0.,-1.)) ;
#90994 = DIRECTION('center_axis',(1.,0.,0.)) ;
#90995 = DIRECTION('ref_axis',(0.,0.,1.)) ;
#90996 = DIRECTION('',(1.,0.,0.)) ;
#90997 = DIRECTION('center_axis',(-1.,0.,0.)) ;
#90998 = DIRECTION('ref_axis',(0.,0.,-1.)) ;
#90999 = DIRECTION('center_axis',(0.,-1.,3.99416362155027E-15)) ;
#91000 = DIRECTION('ref_axis',(0.,-3.99416362155027E-15,-1.)) ;
#91001 = DIRECTION('',(0.,3.99416362155027E-15,1.)) ;
#91002 = DIRECTION('',(1.,0.,0.)) ;
#91003 = DIRECTION('',(0.,-3.99416362155027E-15,-1.)) ;
#91004 = DIRECTION('center_axis',(1.,0.,0.)) ;
#91005 = DIRECTION('ref_axis',(0.,0.,-1.)) ;
#91006 = DIRECTION('center_axis',(-1.,0.,0.)) ;
#91007 = DIRECTION('ref_axis',(0.,1.30104260698261E-14,-1.)) ;
#91008 = DIRECTION('',(1.,0.,0.)) ;
#91009 = DIRECTION('center_axis',(1.,0.,0.)) ;
#91010 = DIRECTION('ref_axis',(0.,0.,-1.)) ;
#91011 = DIRECTION('center_axis',(0.,-0.707106781186549,0.707106781186546)) ;
#91012 = DIRECTION('ref_axis',(0.,-0.707106781186546,-0.707106781186549)) ;
#91013 = DIRECTION('',(0.,0.707106781186546,0.707106781186549)) ;
#91014 = DIRECTION('',(1.,0.,0.)) ;
#91015 = DIRECTION('',(0.,-0.707106781186546,-0.707106781186549)) ;
#91016 = DIRECTION('center_axis',(1.,0.,0.)) ;
#91017 = DIRECTION('ref_axis',(0.,0.382683432365084,0.923879532511289)) ;
#91018 = DIRECTION('',(1.,0.,0.)) ;
#91019 = DIRECTION('center_axis',(1.,0.,0.)) ;
#91020 = DIRECTION('ref_axis',(0.,0.,-1.)) ;
#91021 = DIRECTION('center_axis',(0.,1.,0.)) ;
#91022 = DIRECTION('ref_axis',(0.,0.,1.)) ;
#91023 = DIRECTION('',(0.,0.,-1.)) ;
#91024 = DIRECTION('',(0.,0.,1.)) ;
#91025 = DIRECTION('center_axis',(0.,-0.707106781186547,-0.707106781186548)) ;
#91026 = DIRECTION('ref_axis',(0.,0.707106781186548,-0.707106781186547)) ;
#91027 = DIRECTION('',(0.,-0.707106781186548,0.707106781186547)) ;
#91028 = DIRECTION('',(1.,0.,0.)) ;
#91029 = DIRECTION('',(0.,0.707106781186548,-0.707106781186547)) ;
#91030 = DIRECTION('center_axis',(1.,0.,0.)) ;
#91031 = DIRECTION('ref_axis',(0.,0.,-1.)) ;
#91032 = DIRECTION('center_axis',(-1.,0.,0.)) ;
#91033 = DIRECTION('ref_axis',(0.,-1.73472347597682E-14,-1.)) ;
#91034 = DIRECTION('',(1.,0.,0.)) ;
#91035 = DIRECTION('center_axis',(1.,0.,0.)) ;
#91036 = DIRECTION('ref_axis',(0.,0.,-1.)) ;
#91037 = DIRECTION('center_axis',(0.,-1.,0.)) ;
#91038 = DIRECTION('ref_axis',(0.,0.,-1.)) ;
#91039 = DIRECTION('',(0.,0.,1.)) ;
#91040 = DIRECTION('',(1.,0.,0.)) ;
#91041 = DIRECTION('',(0.,0.,-1.)) ;
#91042 = DIRECTION('center_axis',(1.,0.,0.)) ;
#91043 = DIRECTION('ref_axis',(0.,0.,-1.)) ;
#91044 = DIRECTION('center_axis',(1.,0.,0.)) ;
#91045 = DIRECTION('ref_axis',(0.,0.,1.)) ;
#91046 = DIRECTION('',(1.,0.,0.)) ;
#91047 = DIRECTION('center_axis',(-1.,0.,0.)) ;
#91048 = DIRECTION('ref_axis',(0.,0.,-1.)) ;
#91049 = DIRECTION('center_axis',(0.,0.,-1.)) ;
#91050 = DIRECTION('ref_axis',(-1.,0.,0.)) ;
#91051 = DIRECTION('',(0.,-1.,0.)) ;
#91052 = DIRECTION('',(1.,0.,0.)) ;
#91053 = DIRECTION('',(0.,1.,0.)) ;
#91054 = DIRECTION('center_axis',(1.,0.,0.)) ;
#91055 = DIRECTION('ref_axis',(0.,0.,-1.)) ;
#91056 = DIRECTION('center_axis',(1.,0.,0.)) ;
#91057 = DIRECTION('ref_axis',(0.,0.,1.)) ;
#91058 = DIRECTION('',(1.,0.,0.)) ;
#91059 = DIRECTION('center_axis',(-1.,0.,0.)) ;
#91060 = DIRECTION('ref_axis',(0.,0.,-1.)) ;
#91061 = DIRECTION('center_axis',(0.,1.,0.)) ;
#91062 = DIRECTION('ref_axis',(0.,0.,1.)) ;
#91063 = DIRECTION('',(0.,0.,-1.)) ;
#91064 = DIRECTION('',(1.,0.,0.)) ;
#91065 = DIRECTION('',(0.,0.,1.)) ;
#91066 = DIRECTION('center_axis',(1.,0.,0.)) ;
#91067 = DIRECTION('ref_axis',(0.,0.,-1.)) ;
#91068 = DIRECTION('center_axis',(-1.,0.,0.)) ;
#91069 = DIRECTION('ref_axis',(0.,1.95156391047392E-14,-1.)) ;
#91070 = DIRECTION('',(1.,0.,0.)) ;
#91071 = DIRECTION('center_axis',(1.,0.,0.)) ;
#91072 = DIRECTION('ref_axis',(0.,0.,-1.)) ;
#91073 = DIRECTION('center_axis',(0.,1.07081696047951E-16,-1.)) ;
#91074 = DIRECTION('ref_axis',(0.,1.,1.07081696047951E-16)) ;
#91075 = DIRECTION('',(0.,-1.,-1.07081696047951E-16)) ;
#91076 = DIRECTION('',(1.,0.,0.)) ;
#91077 = DIRECTION('',(0.,1.,1.07081696047951E-16)) ;
#91078 = DIRECTION('center_axis',(1.,0.,0.)) ;
#91079 = DIRECTION('ref_axis',(0.,0.,-1.)) ;
#91080 = DIRECTION('center_axis',(-1.,0.,0.)) ;
#91081 = DIRECTION('ref_axis',(0.,0.,-1.)) ;
#91082 = DIRECTION('',(1.,0.,0.)) ;
#91083 = DIRECTION('center_axis',(1.,0.,0.)) ;
#91084 = DIRECTION('ref_axis',(0.,0.,-1.)) ;
#91085 = DIRECTION('center_axis',(0.,-1.,0.)) ;
#91086 = DIRECTION('ref_axis',(0.,0.,-1.)) ;
#91087 = DIRECTION('',(0.,0.,1.)) ;
#91088 = DIRECTION('',(1.,0.,0.)) ;
#91089 = DIRECTION('',(0.,0.,-1.)) ;
#91090 = DIRECTION('center_axis',(1.,0.,0.)) ;
#91091 = DIRECTION('ref_axis',(0.,0.,-1.)) ;
#91092 = DIRECTION('center_axis',(-1.,0.,0.)) ;
#91093 = DIRECTION('ref_axis',(0.,4.33680868994204E-15,-1.)) ;
#91094 = DIRECTION('',(1.,0.,0.)) ;
#91095 = DIRECTION('center_axis',(1.,0.,0.)) ;
#91096 = DIRECTION('ref_axis',(0.,0.,-1.)) ;
#91097 = DIRECTION('center_axis',(1.,0.,0.)) ;
#91098 = DIRECTION('ref_axis',(0.,0.,-1.)) ;
#91099 = DIRECTION('center_axis',(1.,0.,0.)) ;
#91100 = DIRECTION('ref_axis',(0.,-7.85535158932894E-16,1.)) ;
#91101 = DIRECTION('',(1.,0.,0.)) ;
#91102 = DIRECTION('center_axis',(-1.,0.,0.)) ;
#91103 = DIRECTION('ref_axis',(0.,-7.85535158932895E-16,-1.)) ;
#91104 = DIRECTION('center_axis',(1.,0.,0.)) ;
#91105 = DIRECTION('ref_axis',(0.,0.,-1.)) ;
#91106 = DIRECTION('center_axis',(-1.,0.,0.)) ;
#91107 = DIRECTION('ref_axis',(0.,-8.67361737988409E-15,-1.)) ;
#91108 = DIRECTION('',(1.,0.,0.)) ;
#91109 = DIRECTION('center_axis',(1.,0.,0.)) ;
#91110 = DIRECTION('ref_axis',(0.,0.,-1.)) ;
#91111 = DIRECTION('center_axis',(0.,-1.,0.)) ;
#91112 = DIRECTION('ref_axis',(0.,0.,-1.)) ;
#91113 = DIRECTION('',(0.,0.,1.)) ;
#91114 = DIRECTION('',(1.,0.,0.)) ;
#91115 = DIRECTION('',(0.,0.,-1.)) ;
#91116 = DIRECTION('center_axis',(1.,0.,0.)) ;
#91117 = DIRECTION('ref_axis',(0.,0.,-1.)) ;
#91118 = DIRECTION('center_axis',(-1.,0.,0.)) ;
#91119 = DIRECTION('ref_axis',(0.,0.,-1.)) ;
#91120 = DIRECTION('',(1.,0.,0.)) ;
#91121 = DIRECTION('center_axis',(1.,0.,0.)) ;
#91122 = DIRECTION('ref_axis',(0.,0.,-1.)) ;
#91123 = DIRECTION('center_axis',(0.,-1.07081696047951E-16,1.)) ;
#91124 = DIRECTION('ref_axis',(0.,-1.,-1.07081696047951E-16)) ;
#91125 = DIRECTION('',(0.,1.,1.07081696047951E-16)) ;
#91126 = DIRECTION('',(1.,0.,0.)) ;
#91127 = DIRECTION('',(0.,-1.,-1.07081696047951E-16)) ;
#91128 = DIRECTION('center_axis',(1.,0.,0.)) ;
#91129 = DIRECTION('ref_axis',(0.,0.,-1.)) ;
#91130 = DIRECTION('center_axis',(-1.,0.,0.)) ;
#91131 = DIRECTION('ref_axis',(0.,0.,-1.)) ;
#91132 = DIRECTION('',(1.,0.,0.)) ;
#91133 = DIRECTION('center_axis',(1.,0.,0.)) ;
#91134 = DIRECTION('ref_axis',(0.,0.,-1.)) ;
#91135 = DIRECTION('center_axis',(0.,1.,0.)) ;
#91136 = DIRECTION('ref_axis',(0.,0.,1.)) ;
#91137 = DIRECTION('',(0.,0.,-1.)) ;
#91138 = DIRECTION('',(0.,0.,1.)) ;
#91139 = DIRECTION('center_axis',(-1.,0.,0.)) ;
#91140 = DIRECTION('ref_axis',(0.,0.,1.)) ;
#91141 = DIRECTION('center_axis',(-1.,0.,0.)) ;
#91142 = DIRECTION('ref_axis',(0.,0.,1.)) ;
#91143 = DIRECTION('',(0.,-1.,0.)) ;
#91144 = DIRECTION('center_axis',(-1.,0.,0.)) ;
#91145 = DIRECTION('ref_axis',(0.,0.,1.)) ;
#91146 = DIRECTION('',(0.,0.,1.)) ;
#91147 = DIRECTION('',(0.,-1.,-1.07081696047951E-16)) ;
#91148 = DIRECTION('',(0.,0.,-1.)) ;
#91149 = DIRECTION('center_axis',(-1.,0.,0.)) ;
#91150 = DIRECTION('ref_axis',(0.,0.,1.)) ;
#91151 = DIRECTION('',(0.,0.,-1.)) ;
#91152 = DIRECTION('',(0.,1.,1.07081696047951E-16)) ;
#91153 = DIRECTION('',(0.,0.,1.)) ;
#91154 = DIRECTION('center_axis',(-1.,0.,0.)) ;
#91155 = DIRECTION('ref_axis',(0.,0.,1.)) ;
#91156 = DIRECTION('',(0.,1.,0.)) ;
#91157 = DIRECTION('center_axis',(-1.,0.,0.)) ;
#91158 = DIRECTION('ref_axis',(0.,0.,1.)) ;
#91159 = DIRECTION('',(0.,0.,-1.)) ;
#91160 = DIRECTION('',(0.,0.707106781186548,-0.707106781186547)) ;
#91161 = DIRECTION('',(0.,0.,1.)) ;
#91162 = DIRECTION('',(0.,-0.707106781186546,-0.707106781186549)) ;
#91163 = DIRECTION('',(0.,-3.99416362155027E-15,-1.)) ;
#91164 = DIRECTION('center_axis',(1.,0.,0.)) ;
#91165 = DIRECTION('ref_axis',(0.,0.,-1.)) ;
#91166 = DIRECTION('',(1.,0.,0.)) ;
#91167 = DIRECTION('center_axis',(1.,0.,0.)) ;
#91168 = DIRECTION('ref_axis',(0.,0.,1.)) ;
#91169 = DIRECTION('',(1.,0.,0.)) ;
#91170 = DIRECTION('center_axis',(-1.,0.,0.)) ;
#91171 = DIRECTION('ref_axis',(0.,0.,-1.)) ;
#91172 = DIRECTION('center_axis',(0.,0.,1.)) ;
#91173 = DIRECTION('ref_axis',(1.,0.,0.)) ;
#91174 = DIRECTION('',(0.,1.,0.)) ;
#91175 = DIRECTION('',(1.,0.,0.)) ;
#91176 = DIRECTION('',(0.,-1.,0.)) ;
#91177 = DIRECTION('center_axis',(1.,0.,0.)) ;
#91178 = DIRECTION('ref_axis',(0.,0.,-1.)) ;
#91179 = DIRECTION('center_axis',(1.,0.,0.)) ;
#91180 = DIRECTION('ref_axis',(0.,0.,1.)) ;
#91181 = DIRECTION('',(1.,0.,0.)) ;
#91182 = DIRECTION('center_axis',(-1.,0.,0.)) ;
#91183 = DIRECTION('ref_axis',(0.,0.,-1.)) ;
#91184 = DIRECTION('center_axis',(0.,-1.,3.99416362155027E-15)) ;
#91185 = DIRECTION('ref_axis',(0.,-3.99416362155027E-15,-1.)) ;
#91186 = DIRECTION('',(0.,3.99416362155027E-15,1.)) ;
#91187 = DIRECTION('',(1.,0.,0.)) ;
#91188 = DIRECTION('',(0.,-3.99416362155027E-15,-1.)) ;
#91189 = DIRECTION('center_axis',(1.,0.,0.)) ;
#91190 = DIRECTION('ref_axis',(0.,0.,-1.)) ;
#91191 = DIRECTION('center_axis',(-1.,0.,0.)) ;
#91192 = DIRECTION('ref_axis',(0.,1.30104260698261E-14,-1.)) ;
#91193 = DIRECTION('',(1.,0.,0.)) ;
#91194 = DIRECTION('center_axis',(1.,0.,0.)) ;
#91195 = DIRECTION('ref_axis',(0.,0.,-1.)) ;
#91196 = DIRECTION('center_axis',(0.,-0.707106781186549,0.707106781186546)) ;
#91197 = DIRECTION('ref_axis',(0.,-0.707106781186546,-0.707106781186549)) ;
#91198 = DIRECTION('',(0.,0.707106781186546,0.707106781186549)) ;
#91199 = DIRECTION('',(1.,0.,0.)) ;
#91200 = DIRECTION('',(0.,-0.707106781186546,-0.707106781186549)) ;
#91201 = DIRECTION('center_axis',(1.,0.,0.)) ;
#91202 = DIRECTION('ref_axis',(0.,0.382683432365088,0.923879532511288)) ;
#91203 = DIRECTION('',(1.,0.,0.)) ;
#91204 = DIRECTION('center_axis',(1.,0.,0.)) ;
#91205 = DIRECTION('ref_axis',(0.,0.,-1.)) ;
#91206 = DIRECTION('center_axis',(0.,1.,0.)) ;
#91207 = DIRECTION('ref_axis',(0.,0.,1.)) ;
#91208 = DIRECTION('',(0.,0.,-1.)) ;
#91209 = DIRECTION('',(0.,0.,1.)) ;
#91210 = DIRECTION('center_axis',(0.,-0.707106781186547,-0.707106781186548)) ;
#91211 = DIRECTION('ref_axis',(0.,0.707106781186548,-0.707106781186547)) ;
#91212 = DIRECTION('',(0.,-0.707106781186548,0.707106781186547)) ;
#91213 = DIRECTION('',(1.,0.,0.)) ;
#91214 = DIRECTION('',(0.,0.707106781186548,-0.707106781186547)) ;
#91215 = DIRECTION('center_axis',(1.,0.,0.)) ;
#91216 = DIRECTION('ref_axis',(0.,0.,-1.)) ;
#91217 = DIRECTION('center_axis',(-1.,0.,0.)) ;
#91218 = DIRECTION('ref_axis',(0.,0.,-1.)) ;
#91219 = DIRECTION('',(1.,0.,0.)) ;
#91220 = DIRECTION('center_axis',(1.,0.,0.)) ;
#91221 = DIRECTION('ref_axis',(0.,0.,-1.)) ;
#91222 = DIRECTION('center_axis',(0.,-1.,0.)) ;
#91223 = DIRECTION('ref_axis',(0.,0.,-1.)) ;
#91224 = DIRECTION('',(0.,0.,1.)) ;
#91225 = DIRECTION('',(1.,0.,0.)) ;
#91226 = DIRECTION('',(0.,0.,-1.)) ;
#91227 = DIRECTION('center_axis',(1.,0.,0.)) ;
#91228 = DIRECTION('ref_axis',(0.,0.,-1.)) ;
#91229 = DIRECTION('center_axis',(1.,0.,0.)) ;
#91230 = DIRECTION('ref_axis',(0.,0.,1.)) ;
#91231 = DIRECTION('',(1.,0.,0.)) ;
#91232 = DIRECTION('center_axis',(-1.,0.,0.)) ;
#91233 = DIRECTION('ref_axis',(0.,0.,-1.)) ;
#91234 = DIRECTION('center_axis',(0.,0.,-1.)) ;
#91235 = DIRECTION('ref_axis',(-1.,0.,0.)) ;
#91236 = DIRECTION('',(0.,-1.,0.)) ;
#91237 = DIRECTION('',(1.,0.,0.)) ;
#91238 = DIRECTION('',(0.,1.,0.)) ;
#91239 = DIRECTION('center_axis',(1.,0.,0.)) ;
#91240 = DIRECTION('ref_axis',(0.,0.,-1.)) ;
#91241 = DIRECTION('center_axis',(1.,0.,0.)) ;
#91242 = DIRECTION('ref_axis',(0.,0.,1.)) ;
#91243 = DIRECTION('',(1.,0.,0.)) ;
#91244 = DIRECTION('center_axis',(-1.,0.,0.)) ;
#91245 = DIRECTION('ref_axis',(0.,0.,-1.)) ;
#91246 = DIRECTION('center_axis',(0.,1.,0.)) ;
#91247 = DIRECTION('ref_axis',(0.,0.,1.)) ;
#91248 = DIRECTION('',(0.,0.,-1.)) ;
#91249 = DIRECTION('',(1.,0.,0.)) ;
#91250 = DIRECTION('',(0.,0.,1.)) ;
#91251 = DIRECTION('center_axis',(1.,0.,0.)) ;
#91252 = DIRECTION('ref_axis',(0.,0.,-1.)) ;
#91253 = DIRECTION('center_axis',(-1.,0.,0.)) ;
#91254 = DIRECTION('ref_axis',(0.,1.95156391047392E-14,-1.)) ;
#91255 = DIRECTION('',(1.,0.,0.)) ;
#91256 = DIRECTION('center_axis',(1.,0.,0.)) ;
#91257 = DIRECTION('ref_axis',(0.,0.,-1.)) ;
#91258 = DIRECTION('center_axis',(0.,1.07081696047951E-16,-1.)) ;
#91259 = DIRECTION('ref_axis',(0.,1.,1.07081696047951E-16)) ;
#91260 = DIRECTION('',(0.,-1.,-1.07081696047951E-16)) ;
#91261 = DIRECTION('',(1.,0.,0.)) ;
#91262 = DIRECTION('',(0.,1.,1.07081696047951E-16)) ;
#91263 = DIRECTION('center_axis',(1.,0.,0.)) ;
#91264 = DIRECTION('ref_axis',(0.,0.,-1.)) ;
#91265 = DIRECTION('center_axis',(-1.,0.,0.)) ;
#91266 = DIRECTION('ref_axis',(0.,0.,-1.)) ;
#91267 = DIRECTION('',(1.,0.,0.)) ;
#91268 = DIRECTION('center_axis',(1.,0.,0.)) ;
#91269 = DIRECTION('ref_axis',(0.,0.,-1.)) ;
#91270 = DIRECTION('center_axis',(0.,-1.,0.)) ;
#91271 = DIRECTION('ref_axis',(0.,0.,-1.)) ;
#91272 = DIRECTION('',(0.,0.,1.)) ;
#91273 = DIRECTION('',(1.,0.,0.)) ;
#91274 = DIRECTION('',(0.,0.,-1.)) ;
#91275 = DIRECTION('center_axis',(1.,0.,0.)) ;
#91276 = DIRECTION('ref_axis',(0.,0.,-1.)) ;
#91277 = DIRECTION('center_axis',(-1.,0.,0.)) ;
#91278 = DIRECTION('ref_axis',(0.,-4.33680868994204E-15,-1.)) ;
#91279 = DIRECTION('',(1.,0.,0.)) ;
#91280 = DIRECTION('center_axis',(1.,0.,0.)) ;
#91281 = DIRECTION('ref_axis',(0.,0.,-1.)) ;
#91282 = DIRECTION('center_axis',(1.,0.,0.)) ;
#91283 = DIRECTION('ref_axis',(0.,0.,-1.)) ;
#91284 = DIRECTION('center_axis',(1.,0.,0.)) ;
#91285 = DIRECTION('ref_axis',(0.,-7.85535158932894E-16,1.)) ;
#91286 = DIRECTION('',(1.,0.,0.)) ;
#91287 = DIRECTION('center_axis',(-1.,0.,0.)) ;
#91288 = DIRECTION('ref_axis',(0.,-7.85535158932894E-16,-1.)) ;
#91289 = DIRECTION('center_axis',(1.,0.,0.)) ;
#91290 = DIRECTION('ref_axis',(0.,0.,-1.)) ;
#91291 = DIRECTION('center_axis',(-1.,0.,0.)) ;
#91292 = DIRECTION('ref_axis',(0.,-8.67361737988409E-15,-1.)) ;
#91293 = DIRECTION('',(1.,0.,0.)) ;
#91294 = DIRECTION('center_axis',(1.,0.,0.)) ;
#91295 = DIRECTION('ref_axis',(0.,0.,-1.)) ;
#91296 = DIRECTION('center_axis',(0.,-1.,0.)) ;
#91297 = DIRECTION('ref_axis',(0.,0.,-1.)) ;
#91298 = DIRECTION('',(0.,0.,1.)) ;
#91299 = DIRECTION('',(1.,0.,0.)) ;
#91300 = DIRECTION('',(0.,0.,-1.)) ;
#91301 = DIRECTION('center_axis',(1.,0.,0.)) ;
#91302 = DIRECTION('ref_axis',(0.,0.,-1.)) ;
#91303 = DIRECTION('center_axis',(-1.,0.,0.)) ;
#91304 = DIRECTION('ref_axis',(0.,0.,-1.)) ;
#91305 = DIRECTION('',(1.,0.,0.)) ;
#91306 = DIRECTION('center_axis',(1.,0.,0.)) ;
#91307 = DIRECTION('ref_axis',(0.,0.,-1.)) ;
#91308 = DIRECTION('center_axis',(0.,-1.07081696047951E-16,1.)) ;
#91309 = DIRECTION('ref_axis',(0.,-1.,-1.07081696047951E-16)) ;
#91310 = DIRECTION('',(0.,1.,1.07081696047951E-16)) ;
#91311 = DIRECTION('',(1.,0.,0.)) ;
#91312 = DIRECTION('',(0.,-1.,-1.07081696047951E-16)) ;
#91313 = DIRECTION('center_axis',(1.,0.,0.)) ;
#91314 = DIRECTION('ref_axis',(0.,0.,-1.)) ;
#91315 = DIRECTION('center_axis',(-1.,0.,0.)) ;
#91316 = DIRECTION('ref_axis',(0.,0.,-1.)) ;
#91317 = DIRECTION('',(1.,0.,0.)) ;
#91318 = DIRECTION('center_axis',(1.,0.,0.)) ;
#91319 = DIRECTION('ref_axis',(0.,0.,-1.)) ;
#91320 = DIRECTION('center_axis',(0.,1.,0.)) ;
#91321 = DIRECTION('ref_axis',(0.,0.,1.)) ;
#91322 = DIRECTION('',(0.,0.,-1.)) ;
#91323 = DIRECTION('',(0.,0.,1.)) ;
#91324 = DIRECTION('center_axis',(-1.,0.,0.)) ;
#91325 = DIRECTION('ref_axis',(0.,0.,1.)) ;
#91326 = DIRECTION('center_axis',(-1.,0.,0.)) ;
#91327 = DIRECTION('ref_axis',(0.,0.,1.)) ;
#91328 = DIRECTION('',(0.,-1.,0.)) ;
#91329 = DIRECTION('center_axis',(-1.,0.,0.)) ;
#91330 = DIRECTION('ref_axis',(0.,0.,1.)) ;
#91331 = DIRECTION('',(0.,0.,1.)) ;
#91332 = DIRECTION('',(0.,-1.,-1.07081696047951E-16)) ;
#91333 = DIRECTION('',(0.,0.,-1.)) ;
#91334 = DIRECTION('center_axis',(-1.,0.,0.)) ;
#91335 = DIRECTION('ref_axis',(0.,0.,1.)) ;
#91336 = DIRECTION('',(0.,0.,-1.)) ;
#91337 = DIRECTION('',(0.,1.,1.07081696047951E-16)) ;
#91338 = DIRECTION('',(0.,0.,1.)) ;
#91339 = DIRECTION('center_axis',(-1.,0.,0.)) ;
#91340 = DIRECTION('ref_axis',(0.,0.,1.)) ;
#91341 = DIRECTION('',(0.,1.,0.)) ;
#91342 = DIRECTION('center_axis',(-1.,0.,0.)) ;
#91343 = DIRECTION('ref_axis',(0.,0.,1.)) ;
#91344 = DIRECTION('',(0.,0.,-1.)) ;
#91345 = DIRECTION('',(0.,0.707106781186548,-0.707106781186547)) ;
#91346 = DIRECTION('',(0.,0.,1.)) ;
#91347 = DIRECTION('',(0.,-0.707106781186546,-0.707106781186549)) ;
#91348 = DIRECTION('',(0.,-3.99416362155027E-15,-1.)) ;
#91349 = DIRECTION('center_axis',(1.,0.,0.)) ;
#91350 = DIRECTION('ref_axis',(0.,0.,-1.)) ;
#91351 = DIRECTION('',(1.,0.,0.)) ;
#91352 = DIRECTION('center_axis',(1.,0.,0.)) ;
#91353 = DIRECTION('ref_axis',(0.,0.,1.)) ;
#91354 = DIRECTION('',(1.,0.,0.)) ;
#91355 = DIRECTION('center_axis',(-1.,0.,0.)) ;
#91356 = DIRECTION('ref_axis',(0.,0.,-1.)) ;
#91357 = DIRECTION('center_axis',(0.,0.,1.)) ;
#91358 = DIRECTION('ref_axis',(1.,0.,0.)) ;
#91359 = DIRECTION('',(0.,1.,0.)) ;
#91360 = DIRECTION('',(1.,0.,0.)) ;
#91361 = DIRECTION('',(0.,-1.,0.)) ;
#91362 = DIRECTION('center_axis',(1.,0.,0.)) ;
#91363 = DIRECTION('ref_axis',(0.,0.,-1.)) ;
#91364 = DIRECTION('center_axis',(1.,0.,0.)) ;
#91365 = DIRECTION('ref_axis',(0.,0.,1.)) ;
#91366 = DIRECTION('',(1.,0.,0.)) ;
#91367 = DIRECTION('center_axis',(-1.,0.,0.)) ;
#91368 = DIRECTION('ref_axis',(0.,0.,-1.)) ;
#91369 = DIRECTION('center_axis',(0.,-1.,3.99416362155027E-15)) ;
#91370 = DIRECTION('ref_axis',(0.,-3.99416362155027E-15,-1.)) ;
#91371 = DIRECTION('',(0.,3.99416362155027E-15,1.)) ;
#91372 = DIRECTION('',(1.,0.,0.)) ;
#91373 = DIRECTION('',(0.,-3.99416362155027E-15,-1.)) ;
#91374 = DIRECTION('center_axis',(1.,0.,0.)) ;
#91375 = DIRECTION('ref_axis',(0.,0.,-1.)) ;
#91376 = DIRECTION('center_axis',(-1.,0.,0.)) ;
#91377 = DIRECTION('ref_axis',(0.,0.,-1.)) ;
#91378 = DIRECTION('',(1.,0.,0.)) ;
#91379 = DIRECTION('center_axis',(1.,0.,0.)) ;
#91380 = DIRECTION('ref_axis',(0.,0.,-1.)) ;
#91381 = DIRECTION('center_axis',(0.,-0.707106781186549,0.707106781186546)) ;
#91382 = DIRECTION('ref_axis',(0.,-0.707106781186546,-0.707106781186549)) ;
#91383 = DIRECTION('',(0.,0.707106781186546,0.707106781186549)) ;
#91384 = DIRECTION('',(1.,0.,0.)) ;
#91385 = DIRECTION('',(0.,-0.707106781186546,-0.707106781186549)) ;
#91386 = DIRECTION('center_axis',(1.,0.,0.)) ;
#91387 = DIRECTION('ref_axis',(0.,0.382683432365092,0.923879532511286)) ;
#91388 = DIRECTION('',(1.,0.,0.)) ;
#91389 = DIRECTION('center_axis',(1.,0.,0.)) ;
#91390 = DIRECTION('ref_axis',(0.,0.,-1.)) ;
#91391 = DIRECTION('center_axis',(0.,1.,0.)) ;
#91392 = DIRECTION('ref_axis',(0.,0.,1.)) ;
#91393 = DIRECTION('',(0.,0.,-1.)) ;
#91394 = DIRECTION('',(0.,0.,1.)) ;
#91395 = DIRECTION('center_axis',(0.,-0.707106781186547,-0.707106781186548)) ;
#91396 = DIRECTION('ref_axis',(0.,0.707106781186548,-0.707106781186547)) ;
#91397 = DIRECTION('',(0.,-0.707106781186548,0.707106781186547)) ;
#91398 = DIRECTION('',(1.,0.,0.)) ;
#91399 = DIRECTION('',(0.,0.707106781186548,-0.707106781186547)) ;
#91400 = DIRECTION('center_axis',(1.,0.,0.)) ;
#91401 = DIRECTION('ref_axis',(0.,0.,-1.)) ;
#91402 = DIRECTION('center_axis',(-1.,0.,0.)) ;
#91403 = DIRECTION('ref_axis',(0.,0.,-1.)) ;
#91404 = DIRECTION('',(1.,0.,0.)) ;
#91405 = DIRECTION('center_axis',(1.,0.,0.)) ;
#91406 = DIRECTION('ref_axis',(0.,0.,-1.)) ;
#91407 = DIRECTION('center_axis',(0.,-1.,0.)) ;
#91408 = DIRECTION('ref_axis',(0.,0.,-1.)) ;
#91409 = DIRECTION('',(0.,0.,1.)) ;
#91410 = DIRECTION('',(1.,0.,0.)) ;
#91411 = DIRECTION('',(0.,0.,-1.)) ;
#91412 = DIRECTION('center_axis',(1.,0.,0.)) ;
#91413 = DIRECTION('ref_axis',(0.,0.,-1.)) ;
#91414 = DIRECTION('center_axis',(1.,0.,0.)) ;
#91415 = DIRECTION('ref_axis',(0.,0.,1.)) ;
#91416 = DIRECTION('',(1.,0.,0.)) ;
#91417 = DIRECTION('center_axis',(-1.,0.,0.)) ;
#91418 = DIRECTION('ref_axis',(0.,0.,-1.)) ;
#91419 = DIRECTION('center_axis',(0.,0.,-1.)) ;
#91420 = DIRECTION('ref_axis',(-1.,0.,0.)) ;
#91421 = DIRECTION('',(0.,-1.,0.)) ;
#91422 = DIRECTION('',(1.,0.,0.)) ;
#91423 = DIRECTION('',(0.,1.,0.)) ;
#91424 = DIRECTION('center_axis',(1.,0.,0.)) ;
#91425 = DIRECTION('ref_axis',(0.,0.,-1.)) ;
#91426 = DIRECTION('center_axis',(1.,0.,0.)) ;
#91427 = DIRECTION('ref_axis',(0.,0.,1.)) ;
#91428 = DIRECTION('',(1.,0.,0.)) ;
#91429 = DIRECTION('center_axis',(-1.,0.,0.)) ;
#91430 = DIRECTION('ref_axis',(0.,0.,-1.)) ;
#91431 = DIRECTION('center_axis',(0.,1.,0.)) ;
#91432 = DIRECTION('ref_axis',(0.,0.,1.)) ;
#91433 = DIRECTION('',(0.,0.,-1.)) ;
#91434 = DIRECTION('',(1.,0.,0.)) ;
#91435 = DIRECTION('',(0.,0.,1.)) ;
#91436 = DIRECTION('center_axis',(1.,0.,0.)) ;
#91437 = DIRECTION('ref_axis',(0.,0.,-1.)) ;
#91438 = DIRECTION('center_axis',(-1.,0.,0.)) ;
#91439 = DIRECTION('ref_axis',(0.,1.95156391047392E-14,-1.)) ;
#91440 = DIRECTION('',(1.,0.,0.)) ;
#91441 = DIRECTION('center_axis',(1.,0.,0.)) ;
#91442 = DIRECTION('ref_axis',(0.,0.,-1.)) ;
#91443 = DIRECTION('center_axis',(0.,1.07081696047951E-16,-1.)) ;
#91444 = DIRECTION('ref_axis',(0.,1.,1.07081696047951E-16)) ;
#91445 = DIRECTION('',(0.,-1.,-1.07081696047951E-16)) ;
#91446 = DIRECTION('',(1.,0.,0.)) ;
#91447 = DIRECTION('',(0.,1.,1.07081696047951E-16)) ;
#91448 = DIRECTION('center_axis',(1.,0.,0.)) ;
#91449 = DIRECTION('ref_axis',(0.,0.,-1.)) ;
#91450 = DIRECTION('center_axis',(-1.,0.,0.)) ;
#91451 = DIRECTION('ref_axis',(0.,0.,-1.)) ;
#91452 = DIRECTION('',(1.,0.,0.)) ;
#91453 = DIRECTION('center_axis',(1.,0.,0.)) ;
#91454 = DIRECTION('ref_axis',(0.,0.,-1.)) ;
#91455 = DIRECTION('center_axis',(0.,-1.,0.)) ;
#91456 = DIRECTION('ref_axis',(0.,0.,-1.)) ;
#91457 = DIRECTION('',(0.,0.,1.)) ;
#91458 = DIRECTION('',(1.,0.,0.)) ;
#91459 = DIRECTION('',(0.,0.,-1.)) ;
#91460 = DIRECTION('center_axis',(1.,0.,0.)) ;
#91461 = DIRECTION('ref_axis',(0.,0.,-1.)) ;
#91462 = DIRECTION('center_axis',(-1.,0.,0.)) ;
#91463 = DIRECTION('ref_axis',(0.,-4.33680868994204E-15,-1.)) ;
#91464 = DIRECTION('',(1.,0.,0.)) ;
#91465 = DIRECTION('center_axis',(1.,0.,0.)) ;
#91466 = DIRECTION('ref_axis',(0.,0.,-1.)) ;
#91467 = DIRECTION('center_axis',(1.,0.,0.)) ;
#91468 = DIRECTION('ref_axis',(0.,0.,-1.)) ;
#91469 = DIRECTION('center_axis',(1.,0.,0.)) ;
#91470 = DIRECTION('ref_axis',(0.,-7.85535158932894E-16,1.)) ;
#91471 = DIRECTION('',(1.,0.,0.)) ;
#91472 = DIRECTION('center_axis',(-1.,0.,0.)) ;
#91473 = DIRECTION('ref_axis',(0.,-7.85535158932894E-16,-1.)) ;
#91474 = DIRECTION('center_axis',(1.,0.,0.)) ;
#91475 = DIRECTION('ref_axis',(0.,0.,-1.)) ;
#91476 = DIRECTION('center_axis',(-1.,0.,0.)) ;
#91477 = DIRECTION('ref_axis',(0.,0.,-1.)) ;
#91478 = DIRECTION('',(1.,0.,0.)) ;
#91479 = DIRECTION('center_axis',(1.,0.,0.)) ;
#91480 = DIRECTION('ref_axis',(0.,0.,-1.)) ;
#91481 = DIRECTION('center_axis',(0.,-1.,0.)) ;
#91482 = DIRECTION('ref_axis',(0.,0.,-1.)) ;
#91483 = DIRECTION('',(0.,0.,1.)) ;
#91484 = DIRECTION('',(1.,0.,0.)) ;
#91485 = DIRECTION('',(0.,0.,-1.)) ;
#91486 = DIRECTION('center_axis',(1.,0.,0.)) ;
#91487 = DIRECTION('ref_axis',(0.,0.,-1.)) ;
#91488 = DIRECTION('center_axis',(-1.,0.,0.)) ;
#91489 = DIRECTION('ref_axis',(0.,0.,-1.)) ;
#91490 = DIRECTION('',(1.,0.,0.)) ;
#91491 = DIRECTION('center_axis',(1.,0.,0.)) ;
#91492 = DIRECTION('ref_axis',(0.,0.,-1.)) ;
#91493 = DIRECTION('center_axis',(0.,-1.07081696047951E-16,1.)) ;
#91494 = DIRECTION('ref_axis',(0.,-1.,-1.07081696047951E-16)) ;
#91495 = DIRECTION('',(0.,1.,1.07081696047951E-16)) ;
#91496 = DIRECTION('',(1.,0.,0.)) ;
#91497 = DIRECTION('',(0.,-1.,-1.07081696047951E-16)) ;
#91498 = DIRECTION('center_axis',(1.,0.,0.)) ;
#91499 = DIRECTION('ref_axis',(0.,0.,-1.)) ;
#91500 = DIRECTION('center_axis',(-1.,0.,0.)) ;
#91501 = DIRECTION('ref_axis',(0.,0.,-1.)) ;
#91502 = DIRECTION('',(1.,0.,0.)) ;
#91503 = DIRECTION('center_axis',(1.,0.,0.)) ;
#91504 = DIRECTION('ref_axis',(0.,0.,-1.)) ;
#91505 = DIRECTION('center_axis',(0.,1.,0.)) ;
#91506 = DIRECTION('ref_axis',(0.,0.,1.)) ;
#91507 = DIRECTION('',(0.,0.,-1.)) ;
#91508 = DIRECTION('',(0.,0.,1.)) ;
#91509 = DIRECTION('center_axis',(-1.,0.,0.)) ;
#91510 = DIRECTION('ref_axis',(0.,0.,1.)) ;
#91511 = DIRECTION('center_axis',(-1.,0.,0.)) ;
#91512 = DIRECTION('ref_axis',(0.,0.,1.)) ;
#91513 = DIRECTION('',(0.,-1.,0.)) ;
#91514 = DIRECTION('center_axis',(-1.,0.,0.)) ;
#91515 = DIRECTION('ref_axis',(0.,0.,1.)) ;
#91516 = DIRECTION('',(0.,0.,1.)) ;
#91517 = DIRECTION('',(0.,-1.,-1.07081696047951E-16)) ;
#91518 = DIRECTION('',(0.,0.,-1.)) ;
#91519 = DIRECTION('center_axis',(-1.,0.,0.)) ;
#91520 = DIRECTION('ref_axis',(0.,0.,1.)) ;
#91521 = DIRECTION('',(0.,0.,-1.)) ;
#91522 = DIRECTION('',(0.,1.,1.07081696047951E-16)) ;
#91523 = DIRECTION('',(0.,0.,1.)) ;
#91524 = DIRECTION('center_axis',(-1.,0.,0.)) ;
#91525 = DIRECTION('ref_axis',(0.,0.,1.)) ;
#91526 = DIRECTION('',(0.,1.,0.)) ;
#91527 = DIRECTION('center_axis',(-1.,0.,0.)) ;
#91528 = DIRECTION('ref_axis',(0.,0.,1.)) ;
#91529 = DIRECTION('',(0.,0.,-1.)) ;
#91530 = DIRECTION('',(0.,0.707106781186548,-0.707106781186547)) ;
#91531 = DIRECTION('',(0.,0.,1.)) ;
#91532 = DIRECTION('',(0.,-0.707106781186546,-0.707106781186549)) ;
#91533 = DIRECTION('',(0.,-3.99416362155027E-15,-1.)) ;
#91534 = DIRECTION('center_axis',(1.,0.,0.)) ;
#91535 = DIRECTION('ref_axis',(0.,0.,-1.)) ;
#91536 = DIRECTION('',(1.,0.,0.)) ;
#91537 = DIRECTION('center_axis',(1.,0.,0.)) ;
#91538 = DIRECTION('ref_axis',(0.,0.,1.)) ;
#91539 = DIRECTION('',(1.,0.,0.)) ;
#91540 = DIRECTION('center_axis',(-1.,0.,0.)) ;
#91541 = DIRECTION('ref_axis',(0.,0.,-1.)) ;
#91542 = DIRECTION('center_axis',(0.,0.,1.)) ;
#91543 = DIRECTION('ref_axis',(1.,0.,0.)) ;
#91544 = DIRECTION('',(0.,1.,0.)) ;
#91545 = DIRECTION('',(1.,0.,0.)) ;
#91546 = DIRECTION('',(0.,-1.,0.)) ;
#91547 = DIRECTION('center_axis',(1.,0.,0.)) ;
#91548 = DIRECTION('ref_axis',(0.,0.,-1.)) ;
#91549 = DIRECTION('center_axis',(1.,0.,0.)) ;
#91550 = DIRECTION('ref_axis',(0.,0.,1.)) ;
#91551 = DIRECTION('',(1.,0.,0.)) ;
#91552 = DIRECTION('center_axis',(-1.,0.,0.)) ;
#91553 = DIRECTION('ref_axis',(0.,0.,-1.)) ;
#91554 = DIRECTION('center_axis',(0.,-1.,3.99416362155027E-15)) ;
#91555 = DIRECTION('ref_axis',(0.,-3.99416362155027E-15,-1.)) ;
#91556 = DIRECTION('',(0.,3.99416362155027E-15,1.)) ;
#91557 = DIRECTION('',(1.,0.,0.)) ;
#91558 = DIRECTION('',(0.,-3.99416362155027E-15,-1.)) ;
#91559 = DIRECTION('center_axis',(1.,0.,0.)) ;
#91560 = DIRECTION('ref_axis',(0.,0.,-1.)) ;
#91561 = DIRECTION('center_axis',(-1.,0.,0.)) ;
#91562 = DIRECTION('ref_axis',(0.,0.,-1.)) ;
#91563 = DIRECTION('',(1.,0.,0.)) ;
#91564 = DIRECTION('center_axis',(1.,0.,0.)) ;
#91565 = DIRECTION('ref_axis',(0.,0.,-1.)) ;
#91566 = DIRECTION('center_axis',(0.,-0.707106781186549,0.707106781186546)) ;
#91567 = DIRECTION('ref_axis',(0.,-0.707106781186546,-0.707106781186549)) ;
#91568 = DIRECTION('',(0.,0.707106781186546,0.707106781186549)) ;
#91569 = DIRECTION('',(1.,0.,0.)) ;
#91570 = DIRECTION('',(0.,-0.707106781186546,-0.707106781186549)) ;
#91571 = DIRECTION('center_axis',(1.,0.,0.)) ;
#91572 = DIRECTION('ref_axis',(0.,0.382683432365092,0.923879532511286)) ;
#91573 = DIRECTION('',(1.,0.,0.)) ;
#91574 = DIRECTION('center_axis',(1.,0.,0.)) ;
#91575 = DIRECTION('ref_axis',(0.,0.,-1.)) ;
#91576 = DIRECTION('center_axis',(0.,1.,0.)) ;
#91577 = DIRECTION('ref_axis',(0.,0.,1.)) ;
#91578 = DIRECTION('',(0.,0.,-1.)) ;
#91579 = DIRECTION('',(0.,0.,1.)) ;
#91580 = DIRECTION('center_axis',(0.,-0.707106781186547,-0.707106781186548)) ;
#91581 = DIRECTION('ref_axis',(0.,0.707106781186548,-0.707106781186547)) ;
#91582 = DIRECTION('',(0.,-0.707106781186548,0.707106781186547)) ;
#91583 = DIRECTION('',(1.,0.,0.)) ;
#91584 = DIRECTION('',(0.,0.707106781186548,-0.707106781186547)) ;
#91585 = DIRECTION('center_axis',(1.,0.,0.)) ;
#91586 = DIRECTION('ref_axis',(0.,0.,-1.)) ;
#91587 = DIRECTION('center_axis',(-1.,0.,0.)) ;
#91588 = DIRECTION('ref_axis',(0.,0.,-1.)) ;
#91589 = DIRECTION('',(1.,0.,0.)) ;
#91590 = DIRECTION('center_axis',(1.,0.,0.)) ;
#91591 = DIRECTION('ref_axis',(0.,0.,-1.)) ;
#91592 = DIRECTION('center_axis',(0.,-1.,0.)) ;
#91593 = DIRECTION('ref_axis',(0.,0.,-1.)) ;
#91594 = DIRECTION('',(0.,0.,1.)) ;
#91595 = DIRECTION('',(1.,0.,0.)) ;
#91596 = DIRECTION('',(0.,0.,-1.)) ;
#91597 = DIRECTION('center_axis',(1.,0.,0.)) ;
#91598 = DIRECTION('ref_axis',(0.,0.,-1.)) ;
#91599 = DIRECTION('center_axis',(1.,0.,0.)) ;
#91600 = DIRECTION('ref_axis',(0.,0.,1.)) ;
#91601 = DIRECTION('',(1.,0.,0.)) ;
#91602 = DIRECTION('center_axis',(-1.,0.,0.)) ;
#91603 = DIRECTION('ref_axis',(0.,0.,-1.)) ;
#91604 = DIRECTION('center_axis',(0.,0.,-1.)) ;
#91605 = DIRECTION('ref_axis',(-1.,0.,0.)) ;
#91606 = DIRECTION('',(0.,-1.,0.)) ;
#91607 = DIRECTION('',(1.,0.,0.)) ;
#91608 = DIRECTION('',(0.,1.,0.)) ;
#91609 = DIRECTION('center_axis',(1.,0.,0.)) ;
#91610 = DIRECTION('ref_axis',(0.,0.,-1.)) ;
#91611 = DIRECTION('center_axis',(1.,0.,0.)) ;
#91612 = DIRECTION('ref_axis',(0.,0.,1.)) ;
#91613 = DIRECTION('',(1.,0.,0.)) ;
#91614 = DIRECTION('center_axis',(-1.,0.,0.)) ;
#91615 = DIRECTION('ref_axis',(0.,0.,-1.)) ;
#91616 = DIRECTION('center_axis',(0.,1.,0.)) ;
#91617 = DIRECTION('ref_axis',(0.,0.,1.)) ;
#91618 = DIRECTION('',(0.,0.,-1.)) ;
#91619 = DIRECTION('',(1.,0.,0.)) ;
#91620 = DIRECTION('',(0.,0.,1.)) ;
#91621 = DIRECTION('center_axis',(1.,0.,0.)) ;
#91622 = DIRECTION('ref_axis',(0.,0.,-1.)) ;
#91623 = DIRECTION('center_axis',(-1.,0.,0.)) ;
#91624 = DIRECTION('ref_axis',(0.,1.7347234759768E-14,-1.)) ;
#91625 = DIRECTION('',(1.,0.,0.)) ;
#91626 = DIRECTION('center_axis',(1.,0.,0.)) ;
#91627 = DIRECTION('ref_axis',(0.,0.,-1.)) ;
#91628 = DIRECTION('center_axis',(0.,1.07081696047951E-16,-1.)) ;
#91629 = DIRECTION('ref_axis',(0.,1.,1.07081696047951E-16)) ;
#91630 = DIRECTION('',(0.,-1.,-1.07081696047951E-16)) ;
#91631 = DIRECTION('',(1.,0.,0.)) ;
#91632 = DIRECTION('',(0.,1.,1.07081696047951E-16)) ;
#91633 = DIRECTION('center_axis',(1.,0.,0.)) ;
#91634 = DIRECTION('ref_axis',(0.,0.,-1.)) ;
#91635 = DIRECTION('center_axis',(-1.,0.,0.)) ;
#91636 = DIRECTION('ref_axis',(0.,0.,-1.)) ;
#91637 = DIRECTION('',(1.,0.,0.)) ;
#91638 = DIRECTION('center_axis',(1.,0.,0.)) ;
#91639 = DIRECTION('ref_axis',(0.,0.,-1.)) ;
#91640 = DIRECTION('center_axis',(0.,-1.,0.)) ;
#91641 = DIRECTION('ref_axis',(0.,0.,-1.)) ;
#91642 = DIRECTION('',(0.,0.,1.)) ;
#91643 = DIRECTION('',(1.,0.,0.)) ;
#91644 = DIRECTION('',(0.,0.,-1.)) ;
#91645 = DIRECTION('center_axis',(1.,0.,0.)) ;
#91646 = DIRECTION('ref_axis',(0.,0.,-1.)) ;
#91647 = DIRECTION('center_axis',(-1.,0.,0.)) ;
#91648 = DIRECTION('ref_axis',(0.,0.,-1.)) ;
#91649 = DIRECTION('',(1.,0.,0.)) ;
#91650 = DIRECTION('center_axis',(1.,0.,0.)) ;
#91651 = DIRECTION('ref_axis',(0.,0.,-1.)) ;
#91652 = DIRECTION('center_axis',(1.,0.,0.)) ;
#91653 = DIRECTION('ref_axis',(0.,0.,-1.)) ;
#91654 = DIRECTION('center_axis',(1.,0.,0.)) ;
#91655 = DIRECTION('ref_axis',(0.,-7.85535158932894E-16,1.)) ;
#91656 = DIRECTION('',(1.,0.,0.)) ;
#91657 = DIRECTION('center_axis',(-1.,0.,0.)) ;
#91658 = DIRECTION('ref_axis',(0.,-7.85535158932894E-16,-1.)) ;
#91659 = DIRECTION('center_axis',(1.,0.,0.)) ;
#91660 = DIRECTION('ref_axis',(0.,0.,-1.)) ;
#91661 = DIRECTION('center_axis',(-1.,0.,0.)) ;
#91662 = DIRECTION('ref_axis',(0.,0.,-1.)) ;
#91663 = DIRECTION('',(1.,0.,0.)) ;
#91664 = DIRECTION('center_axis',(1.,0.,0.)) ;
#91665 = DIRECTION('ref_axis',(0.,0.,-1.)) ;
#91666 = DIRECTION('center_axis',(0.,-1.,0.)) ;
#91667 = DIRECTION('ref_axis',(0.,0.,-1.)) ;
#91668 = DIRECTION('',(0.,0.,1.)) ;
#91669 = DIRECTION('',(1.,0.,0.)) ;
#91670 = DIRECTION('',(0.,0.,-1.)) ;
#91671 = DIRECTION('center_axis',(1.,0.,0.)) ;
#91672 = DIRECTION('ref_axis',(0.,0.,-1.)) ;
#91673 = DIRECTION('center_axis',(-1.,0.,0.)) ;
#91674 = DIRECTION('ref_axis',(0.,0.,-1.)) ;
#91675 = DIRECTION('',(1.,0.,0.)) ;
#91676 = DIRECTION('center_axis',(1.,0.,0.)) ;
#91677 = DIRECTION('ref_axis',(0.,0.,-1.)) ;
#91678 = DIRECTION('center_axis',(0.,-1.07081696047951E-16,1.)) ;
#91679 = DIRECTION('ref_axis',(0.,-1.,-1.07081696047951E-16)) ;
#91680 = DIRECTION('',(0.,1.,1.07081696047951E-16)) ;
#91681 = DIRECTION('',(1.,0.,0.)) ;
#91682 = DIRECTION('',(0.,-1.,-1.07081696047951E-16)) ;
#91683 = DIRECTION('center_axis',(1.,0.,0.)) ;
#91684 = DIRECTION('ref_axis',(0.,0.,-1.)) ;
#91685 = DIRECTION('center_axis',(-1.,0.,0.)) ;
#91686 = DIRECTION('ref_axis',(0.,0.,-1.)) ;
#91687 = DIRECTION('',(1.,0.,0.)) ;
#91688 = DIRECTION('center_axis',(1.,0.,0.)) ;
#91689 = DIRECTION('ref_axis',(0.,0.,-1.)) ;
#91690 = DIRECTION('center_axis',(0.,1.,0.)) ;
#91691 = DIRECTION('ref_axis',(0.,0.,1.)) ;
#91692 = DIRECTION('',(0.,0.,-1.)) ;
#91693 = DIRECTION('',(0.,0.,1.)) ;
#91694 = DIRECTION('center_axis',(-1.,0.,0.)) ;
#91695 = DIRECTION('ref_axis',(0.,0.,1.)) ;
#91696 = DIRECTION('center_axis',(-1.,0.,0.)) ;
#91697 = DIRECTION('ref_axis',(0.,0.,1.)) ;
#91698 = DIRECTION('',(0.,-1.,0.)) ;
#91699 = DIRECTION('center_axis',(-1.,0.,0.)) ;
#91700 = DIRECTION('ref_axis',(0.,0.,1.)) ;
#91701 = DIRECTION('',(0.,0.,1.)) ;
#91702 = DIRECTION('',(0.,-1.,-1.07081696047951E-16)) ;
#91703 = DIRECTION('',(0.,0.,-1.)) ;
#91704 = DIRECTION('center_axis',(-1.,0.,0.)) ;
#91705 = DIRECTION('ref_axis',(0.,0.,1.)) ;
#91706 = DIRECTION('',(0.,0.,-1.)) ;
#91707 = DIRECTION('',(0.,1.,1.07081696047951E-16)) ;
#91708 = DIRECTION('',(0.,0.,1.)) ;
#91709 = DIRECTION('center_axis',(-1.,0.,0.)) ;
#91710 = DIRECTION('ref_axis',(0.,0.,1.)) ;
#91711 = DIRECTION('',(0.,1.,0.)) ;
#91712 = DIRECTION('center_axis',(-1.,0.,0.)) ;
#91713 = DIRECTION('ref_axis',(0.,0.,1.)) ;
#91714 = DIRECTION('',(0.,0.,-1.)) ;
#91715 = DIRECTION('',(0.,0.707106781186548,-0.707106781186547)) ;
#91716 = DIRECTION('',(0.,0.,1.)) ;
#91717 = DIRECTION('',(0.,-0.707106781186546,-0.707106781186549)) ;
#91718 = DIRECTION('',(0.,-3.99416362155027E-15,-1.)) ;
#91719 = DIRECTION('center_axis',(1.,0.,0.)) ;
#91720 = DIRECTION('ref_axis',(0.,0.,-1.)) ;
#91721 = DIRECTION('',(0.,-1.,0.)) ;
#91722 = DIRECTION('center_axis',(-1.,0.,0.)) ;
#91723 = DIRECTION('ref_axis',(0.,0.,-1.)) ;
#91724 = DIRECTION('',(0.,0.,-1.)) ;
#91725 = DIRECTION('center_axis',(-1.,0.,0.)) ;
#91726 = DIRECTION('ref_axis',(0.,1.0842021724855E-15,-1.)) ;
#91727 = DIRECTION('',(0.,-1.,0.)) ;
#91728 = DIRECTION('center_axis',(-1.,0.,0.)) ;
#91729 = DIRECTION('ref_axis',(0.,0.,-1.)) ;
#91730 = DIRECTION('',(0.,0.,1.)) ;
#91731 = DIRECTION('center_axis',(-1.,0.,0.)) ;
#91732 = DIRECTION('ref_axis',(0.,0.,-1.)) ;
#91733 = DIRECTION('center_axis',(1.,0.,0.)) ;
#91734 = DIRECTION('ref_axis',(0.,0.,-1.)) ;
#91735 = DIRECTION('',(0.,-1.,0.)) ;
#91736 = DIRECTION('center_axis',(-1.,0.,0.)) ;
#91737 = DIRECTION('ref_axis',(0.,0.,-1.)) ;
#91738 = DIRECTION('',(0.,0.,-1.)) ;
#91739 = DIRECTION('center_axis',(-1.,0.,0.)) ;
#91740 = DIRECTION('ref_axis',(0.,-1.62630325872827E-15,-1.)) ;
#91741 = DIRECTION('',(0.,-1.,0.)) ;
#91742 = DIRECTION('center_axis',(-1.,0.,0.)) ;
#91743 = DIRECTION('ref_axis',(0.,0.,-1.)) ;
#91744 = DIRECTION('',(0.,0.,1.)) ;
#91745 = DIRECTION('center_axis',(-1.,0.,0.)) ;
#91746 = DIRECTION('ref_axis',(0.,0.,-1.)) ;
#91747 = DIRECTION('center_axis',(1.,0.,0.)) ;
#91748 = DIRECTION('ref_axis',(0.,0.,-1.)) ;
#91749 = DIRECTION('',(0.,-1.,0.)) ;
#91750 = DIRECTION('center_axis',(-1.,0.,0.)) ;
#91751 = DIRECTION('ref_axis',(0.,0.,-1.)) ;
#91752 = DIRECTION('',(0.,0.,-1.)) ;
#91753 = DIRECTION('center_axis',(-1.,0.,0.)) ;
#91754 = DIRECTION('ref_axis',(0.,0.,-1.)) ;
#91755 = DIRECTION('',(0.,-1.,0.)) ;
#91756 = DIRECTION('center_axis',(-1.,0.,0.)) ;
#91757 = DIRECTION('ref_axis',(0.,0.,-1.)) ;
#91758 = DIRECTION('',(0.,0.,1.)) ;
#91759 = DIRECTION('center_axis',(-1.,0.,0.)) ;
#91760 = DIRECTION('ref_axis',(0.,0.,-1.)) ;
#91761 = DIRECTION('center_axis',(1.,0.,0.)) ;
#91762 = DIRECTION('ref_axis',(0.,0.,-1.)) ;
#91763 = DIRECTION('',(0.,-1.,0.)) ;
#91764 = DIRECTION('center_axis',(-1.,0.,0.)) ;
#91765 = DIRECTION('ref_axis',(0.,0.,-1.)) ;
#91766 = DIRECTION('',(0.,0.,-1.)) ;
#91767 = DIRECTION('center_axis',(-1.,0.,0.)) ;
#91768 = DIRECTION('ref_axis',(0.,-1.62630325872827E-15,-1.)) ;
#91769 = DIRECTION('',(0.,-1.,0.)) ;
#91770 = DIRECTION('center_axis',(-1.,0.,0.)) ;
#91771 = DIRECTION('ref_axis',(0.,0.,-1.)) ;
#91772 = DIRECTION('',(0.,0.,1.)) ;
#91773 = DIRECTION('center_axis',(-1.,0.,0.)) ;
#91774 = DIRECTION('ref_axis',(0.,0.,-1.)) ;
#91775 = DIRECTION('center_axis',(1.,0.,0.)) ;
#91776 = DIRECTION('ref_axis',(0.,0.,-1.)) ;
#91777 = DIRECTION('',(0.,-1.,0.)) ;
#91778 = DIRECTION('center_axis',(-1.,0.,0.)) ;
#91779 = DIRECTION('ref_axis',(0.,0.,-1.)) ;
#91780 = DIRECTION('',(0.,0.,-1.)) ;
#91781 = DIRECTION('center_axis',(-1.,0.,0.)) ;
#91782 = DIRECTION('ref_axis',(0.,0.,-1.)) ;
#91783 = DIRECTION('',(0.,-1.,0.)) ;
#91784 = DIRECTION('center_axis',(-1.,0.,0.)) ;
#91785 = DIRECTION('ref_axis',(0.,0.,-1.)) ;
#91786 = DIRECTION('',(0.,0.,1.)) ;
#91787 = DIRECTION('center_axis',(-1.,0.,0.)) ;
#91788 = DIRECTION('ref_axis',(0.,0.,-1.)) ;
#91789 = DIRECTION('center_axis',(1.,0.,0.)) ;
#91790 = DIRECTION('ref_axis',(0.,0.,-1.)) ;
#91791 = DIRECTION('',(0.,-1.,0.)) ;
#91792 = DIRECTION('center_axis',(-1.,0.,0.)) ;
#91793 = DIRECTION('ref_axis',(0.,0.,-1.)) ;
#91794 = DIRECTION('',(0.,0.,-1.)) ;
#91795 = DIRECTION('center_axis',(-1.,0.,0.)) ;
#91796 = DIRECTION('ref_axis',(0.,0.,-1.)) ;
#91797 = DIRECTION('',(0.,-1.,0.)) ;
#91798 = DIRECTION('center_axis',(-1.,0.,0.)) ;
#91799 = DIRECTION('ref_axis',(0.,0.,-1.)) ;
#91800 = DIRECTION('',(0.,0.,1.)) ;
#91801 = DIRECTION('center_axis',(-1.,0.,0.)) ;
#91802 = DIRECTION('ref_axis',(0.,0.,-1.)) ;
#91803 = DIRECTION('center_axis',(1.,0.,0.)) ;
#91804 = DIRECTION('ref_axis',(0.,0.,-1.)) ;
#91805 = DIRECTION('',(0.,-1.,0.)) ;
#91806 = DIRECTION('center_axis',(-1.,0.,0.)) ;
#91807 = DIRECTION('ref_axis',(0.,0.,-1.)) ;
#91808 = DIRECTION('',(0.,0.,-1.)) ;
#91809 = DIRECTION('center_axis',(-1.,0.,0.)) ;
#91810 = DIRECTION('ref_axis',(0.,0.,-1.)) ;
#91811 = DIRECTION('',(0.,-1.,0.)) ;
#91812 = DIRECTION('center_axis',(-1.,0.,0.)) ;
#91813 = DIRECTION('ref_axis',(0.,0.,-1.)) ;
#91814 = DIRECTION('',(0.,0.,1.)) ;
#91815 = DIRECTION('center_axis',(-1.,0.,0.)) ;
#91816 = DIRECTION('ref_axis',(0.,0.,-1.)) ;
#91817 = DIRECTION('center_axis',(1.,0.,0.)) ;
#91818 = DIRECTION('ref_axis',(0.,0.,-1.)) ;
#91819 = DIRECTION('',(0.,-1.,0.)) ;
#91820 = DIRECTION('center_axis',(-1.,0.,0.)) ;
#91821 = DIRECTION('ref_axis',(0.,0.,-1.)) ;
#91822 = DIRECTION('',(0.,0.,-1.)) ;
#91823 = DIRECTION('center_axis',(-1.,0.,0.)) ;
#91824 = DIRECTION('ref_axis',(0.,0.,-1.)) ;
#91825 = DIRECTION('',(0.,-1.,0.)) ;
#91826 = DIRECTION('center_axis',(-1.,0.,0.)) ;
#91827 = DIRECTION('ref_axis',(0.,0.,-1.)) ;
#91828 = DIRECTION('',(0.,0.,1.)) ;
#91829 = DIRECTION('center_axis',(-1.,0.,0.)) ;
#91830 = DIRECTION('ref_axis',(0.,0.,-1.)) ;
#91831 = DIRECTION('center_axis',(1.,0.,0.)) ;
#91832 = DIRECTION('ref_axis',(0.,0.,-1.)) ;
#91833 = DIRECTION('',(0.,-1.,0.)) ;
#91834 = DIRECTION('center_axis',(-1.,0.,0.)) ;
#91835 = DIRECTION('ref_axis',(0.,0.,-1.)) ;
#91836 = DIRECTION('',(0.,0.,-1.)) ;
#91837 = DIRECTION('center_axis',(-1.,0.,0.)) ;
#91838 = DIRECTION('ref_axis',(0.,0.,-1.)) ;
#91839 = DIRECTION('',(0.,-1.,0.)) ;
#91840 = DIRECTION('center_axis',(-1.,0.,0.)) ;
#91841 = DIRECTION('ref_axis',(0.,0.,-1.)) ;
#91842 = DIRECTION('',(0.,0.,1.)) ;
#91843 = DIRECTION('center_axis',(-1.,0.,0.)) ;
#91844 = DIRECTION('ref_axis',(0.,0.,-1.)) ;
#91845 = DIRECTION('center_axis',(1.53063836115601E-16,-1.,-1.30104260698261E-16)) ;
#91846 = DIRECTION('ref_axis',(1.,1.53063836115601E-16,1.99142572374599E-32)) ;
#91847 = DIRECTION('center_axis',(0.,1.,0.)) ;
#91848 = DIRECTION('ref_axis',(0.,0.,1.)) ;
#91849 = DIRECTION('center_axis',(0.,-1.,0.)) ;
#91850 = DIRECTION('ref_axis',(0.,0.,-1.)) ;
#91851 = DIRECTION('center_axis',(1.,1.53063836115601E-16,2.73691106313441E-48)) ;
#91852 = DIRECTION('ref_axis',(-1.53063836115601E-16,1.,-4.18922106430579E-64)) ;
#91853 = DIRECTION('center_axis',(-1.,0.,0.)) ;
#91854 = DIRECTION('ref_axis',(0.,0.,1.)) ;
#91855 = DIRECTION('center_axis',(1.,1.53063836115601E-16,0.)) ;
#91856 = DIRECTION('ref_axis',(1.53063836115601E-16,-1.,0.)) ;
#91857 = DIRECTION('center_axis',(0.,1.,0.)) ;
#91858 = DIRECTION('ref_axis',(1.,0.,0.)) ;
#91859 = DIRECTION('center_axis',(0.,1.,0.)) ;
#91860 = DIRECTION('ref_axis',(0.,0.,-1.)) ;
#91861 = DIRECTION('center_axis',(0.,0.,1.)) ;
#91862 = DIRECTION('ref_axis',(-1.,0.,0.)) ;
#91863 = DIRECTION('center_axis',(0.,1.,0.)) ;
#91864 = DIRECTION('ref_axis',(1.,0.,0.)) ;
#91865 = DIRECTION('center_axis',(0.,0.,1.)) ;
#91866 = DIRECTION('ref_axis',(-1.,0.,0.)) ;
#91867 = DIRECTION('center_axis',(1.,1.0842021724855E-15,0.)) ;
#91868 = DIRECTION('ref_axis',(1.0842021724855E-15,-1.,0.)) ;
#91869 = DIRECTION('center_axis',(-1.,-1.53063836115601E-16,0.)) ;
#91870 = DIRECTION('ref_axis',(0.,-1.,0.)) ;
#91871 = DIRECTION('center_axis',(0.,0.,-1.)) ;
#91872 = DIRECTION('ref_axis',(1.,0.,0.)) ;
#91873 = DIRECTION('center_axis',(0.,0.,-1.)) ;
#91874 = DIRECTION('ref_axis',(0.804034447892617,0.594582716366709,0.)) ;
#91875 = DIRECTION('center_axis',(0.,0.,1.)) ;
#91876 = DIRECTION('ref_axis',(1.,0.,0.)) ;
#91877 = DIRECTION('',(0.,0.,-1.)) ;
#91878 = DIRECTION('center_axis',(-2.16840434497101E-16,1.,1.30104260698261E-16)) ;
#91879 = DIRECTION('ref_axis',(1.,2.16840434497101E-16,1.22464679914735E-16)) ;
#91880 = DIRECTION('',(-2.16840434497101E-16,1.,1.30104260698261E-16)) ;
#91881 = DIRECTION('center_axis',(0.,1.,0.)) ;
#91882 = DIRECTION('ref_axis',(0.,0.,1.)) ;
#91883 = DIRECTION('center_axis',(-1.,-1.53063836115601E-16,-2.73691106313441E-48)) ;
#91884 = DIRECTION('ref_axis',(1.53063836115601E-16,-1.,4.18922106430579E-64)) ;
#91885 = DIRECTION('center_axis',(1.,2.16840434497101E-16,0.)) ;
#91886 = DIRECTION('ref_axis',(2.16840434497101E-16,-1.,0.)) ;
#91887 = DIRECTION('center_axis',(0.,0.,1.)) ;
#91888 = DIRECTION('ref_axis',(1.,0.,0.)) ;
#91889 = DIRECTION('center_axis',(-1.25542992828747E-32,1.020425574104E-16,
1.)) ;
#91890 = DIRECTION('ref_axis',(-1.28107280532009E-48,-1.,1.020425574104E-16)) ;
#91891 = DIRECTION('center_axis',(0.,0.,1.)) ;
#91892 = DIRECTION('ref_axis',(1.,0.,0.)) ;
#91893 = DIRECTION('center_axis',(0.,0.,-1.)) ;
#91894 = DIRECTION('ref_axis',(-1.,0.,0.)) ;
#91895 = DIRECTION('center_axis',(1.,1.53063836115601E-16,-2.73691106313441E-48)) ;
#91896 = DIRECTION('ref_axis',(-1.53063836115601E-16,1.,4.18922106430579E-64)) ;
#91897 = DIRECTION('center_axis',(-1.,0.,0.)) ;
#91898 = DIRECTION('ref_axis',(0.,0.,1.)) ;
#91899 = DIRECTION('center_axis',(1.,1.53063836115601E-16,0.)) ;
#91900 = DIRECTION('ref_axis',(1.53063836115601E-16,-1.,0.)) ;
#91901 = DIRECTION('center_axis',(0.,1.,0.)) ;
#91902 = DIRECTION('ref_axis',(1.,0.,0.)) ;
#91903 = DIRECTION('center_axis',(-1.,-2.16840434497101E-16,0.)) ;
#91904 = DIRECTION('ref_axis',(0.,-1.,0.)) ;
#91905 = DIRECTION('center_axis',(0.,0.,-1.)) ;
#91906 = DIRECTION('ref_axis',(1.,0.,0.)) ;
#91907 = DIRECTION('center_axis',(-1.25542992828747E-32,1.020425574104E-16,
1.)) ;
#91908 = DIRECTION('ref_axis',(0.,-1.,0.)) ;
#91909 = DIRECTION('center_axis',(0.,-1.,0.)) ;
#91910 = DIRECTION('ref_axis',(-6.50521303491304E-15,0.,1.)) ;
#91911 = DIRECTION('center_axis',(-1.,0.,0.)) ;
#91912 = DIRECTION('ref_axis',(0.,0.,-1.)) ;
#91913 = DIRECTION('center_axis',(-1.,-1.53063836115601E-16,0.)) ;
#91914 = DIRECTION('ref_axis',(0.,-1.,0.)) ;
#91915 = DIRECTION('center_axis',(0.,-1.,0.)) ;
#91916 = DIRECTION('ref_axis',(0.,0.,1.)) ;
#91917 = DIRECTION('center_axis',(0.,0.,-1.)) ;
#91918 = DIRECTION('ref_axis',(-1.,0.,0.)) ;
#91919 = DIRECTION('center_axis',(-4.33680868994202E-15,0.,-1.)) ;
#91920 = DIRECTION('ref_axis',(-1.,0.,4.33680868994202E-15)) ;
#91921 = DIRECTION('center_axis',(1.,1.53063836115601E-16,-3.06472600140763E-33)) ;
#91922 = DIRECTION('ref_axis',(-1.53063836115601E-16,1.,4.69098718418678E-49)) ;
#91923 = DIRECTION('center_axis',(-1.,0.,0.)) ;
#91924 = DIRECTION('ref_axis',(0.,0.,1.)) ;
#91925 = DIRECTION('center_axis',(-1.53063836115601E-16,1.,-1.020425574104E-16)) ;
#91926 = DIRECTION('ref_axis',(-1.,-1.53063836115601E-16,1.3684555315672E-47)) ;
#91927 = DIRECTION('',(1.53063836115601E-16,-1.,1.020425574104E-16)) ;
#91928 = DIRECTION('center_axis',(0.,-1.,0.)) ;
#91929 = DIRECTION('ref_axis',(0.,0.,-1.)) ;
#91930 = DIRECTION('center_axis',(-1.53063836115601E-16,1.,-1.30104260698261E-16)) ;
#91931 = DIRECTION('ref_axis',(-1.,-1.53063836115601E-16,1.99142572374599E-32)) ;
#91932 = DIRECTION('center_axis',(0.,-1.,0.)) ;
#91933 = DIRECTION('ref_axis',(0.,0.,-1.)) ;
#91934 = DIRECTION('center_axis',(-1.,-1.53063836115601E-16,2.73691106313441E-48)) ;
#91935 = DIRECTION('ref_axis',(1.53063836115601E-16,-1.,-4.18922106430579E-64)) ;
#91936 = DIRECTION('center_axis',(1.,2.16840434497101E-16,0.)) ;
#91937 = DIRECTION('ref_axis',(2.16840434497101E-16,-1.,0.)) ;
#91938 = DIRECTION('center_axis',(-1.,0.,2.168404344971E-15)) ;
#91939 = DIRECTION('ref_axis',(2.168404344971E-15,0.,1.)) ;
#91940 = DIRECTION('center_axis',(-1.,-2.16840434497101E-16,0.)) ;
#91941 = DIRECTION('ref_axis',(0.,-1.,0.)) ;
#91942 = DIRECTION('center_axis',(0.,0.,1.)) ;
#91943 = DIRECTION('ref_axis',(-1.,0.,0.)) ;
#91944 = DIRECTION('center_axis',(0.,1.,0.)) ;
#91945 = DIRECTION('ref_axis',(1.,0.,0.)) ;
#91946 = DIRECTION('center_axis',(0.,1.,0.)) ;
#91947 = DIRECTION('ref_axis',(0.,0.,-1.)) ;
#91948 = DIRECTION('center_axis',(1.,0.,0.)) ;
#91949 = DIRECTION('ref_axis',(0.,-1.,0.)) ;
#91950 = DIRECTION('center_axis',(1.,6.50521303491304E-15,0.)) ;
#91951 = DIRECTION('ref_axis',(-6.50521303491304E-15,1.,0.)) ;
#91952 = DIRECTION('center_axis',(8.67361737988403E-15,1.,0.)) ;
#91953 = DIRECTION('ref_axis',(-1.,8.67361737988403E-15,0.)) ;
#91954 = DIRECTION('center_axis',(1.2303003375722E-16,-1.,1.020425574104E-16)) ;
#91955 = DIRECTION('ref_axis',(1.,1.2303003375722E-16,-1.25542992828747E-32)) ;
#91956 = DIRECTION('center_axis',(0.,1.,0.)) ;
#91957 = DIRECTION('ref_axis',(0.,0.,1.)) ;
#91958 = DIRECTION('center_axis',(0.,1.,0.)) ;
#91959 = DIRECTION('ref_axis',(1.,0.,0.)) ;
#91960 = DIRECTION('center_axis',(1.,1.2303003375722E-16,0.)) ;
#91961 = DIRECTION('ref_axis',(1.2303003375722E-16,-1.,0.)) ;
#91962 = DIRECTION('center_axis',(0.,0.,1.)) ;
#91963 = DIRECTION('ref_axis',(-1.,0.,0.)) ;
#91964 = DIRECTION('center_axis',(0.,1.,0.)) ;
#91965 = DIRECTION('ref_axis',(1.,0.,0.)) ;
#91966 = DIRECTION('center_axis',(0.,0.,-1.)) ;
#91967 = DIRECTION('ref_axis',(1.,0.,0.)) ;
#91968 = DIRECTION('center_axis',(0.,0.,-1.)) ;
#91969 = DIRECTION('ref_axis',(-1.,0.,0.)) ;
#91970 = DIRECTION('center_axis',(0.,0.,1.)) ;
#91971 = DIRECTION('ref_axis',(1.,0.,0.)) ;
#91972 = DIRECTION('center_axis',(-2.16840434497101E-16,1.,-1.020425574104E-16)) ;
#91973 = DIRECTION('ref_axis',(-1.,-2.16840434497101E-16,5.47382212626882E-48)) ;
#91974 = DIRECTION('center_axis',(0.,1.,0.)) ;
#91975 = DIRECTION('ref_axis',(0.,0.,-1.)) ;
#91976 = DIRECTION('center_axis',(1.,0.,1.25542992828747E-32)) ;
#91977 = DIRECTION('ref_axis',(1.25542992828747E-32,0.,-1.)) ;
#91978 = DIRECTION('center_axis',(1.,0.,0.)) ;
#91979 = DIRECTION('ref_axis',(0.,0.,-1.)) ;
#91980 = DIRECTION('center_axis',(-1.,-1.2303003375722E-16,0.)) ;
#91981 = DIRECTION('ref_axis',(0.,-1.,0.)) ;
#91982 = DIRECTION('center_axis',(0.,0.,-1.)) ;
#91983 = DIRECTION('ref_axis',(1.,0.,0.)) ;
#91984 = DIRECTION('center_axis',(0.,0.,-1.)) ;
#91985 = DIRECTION('ref_axis',(-1.,0.,0.)) ;
#91986 = DIRECTION('',(0.,0.,1.)) ;
#91987 = DIRECTION('center_axis',(0.,0.,1.)) ;
#91988 = DIRECTION('ref_axis',(1.,0.,0.)) ;
#91989 = DIRECTION('center_axis',(0.,0.,1.)) ;
#91990 = DIRECTION('ref_axis',(1.,0.,0.)) ;
#91991 = DIRECTION('center_axis',(6.27714964143733E-33,-5.10212787052002E-17,
-1.)) ;
#91992 = DIRECTION('ref_axis',(3.20268201330022E-49,1.,-5.10212787052002E-17)) ;
#91993 = DIRECTION('center_axis',(1.,1.53063836115601E-16,-1.53236300070382E-33)) ;
#91994 = DIRECTION('ref_axis',(-1.53063836115601E-16,1.,2.34549359209339E-49)) ;
#91995 = DIRECTION('center_axis',(-1.,0.,0.)) ;
#91996 = DIRECTION('ref_axis',(0.,0.,1.)) ;
#91997 = DIRECTION('center_axis',(1.,0.,0.)) ;
#91998 = DIRECTION('ref_axis',(0.,0.,-1.)) ;
#91999 = DIRECTION('center_axis',(0.,1.,0.)) ;
#92000 = DIRECTION('ref_axis',(1.,0.,0.)) ;
#92001 = DIRECTION('center_axis',(-4.33680868994202E-15,1.,0.)) ;
#92002 = DIRECTION('ref_axis',(1.,4.33680868994202E-15,0.)) ;
#92003 = DIRECTION('center_axis',(0.,-1.,0.)) ;
#92004 = DIRECTION('ref_axis',(0.,0.,-1.)) ;
#92005 = DIRECTION('center_axis',(0.,0.,-1.)) ;
#92006 = DIRECTION('ref_axis',(1.,0.,0.)) ;
#92007 = DIRECTION('center_axis',(0.,0.,1.)) ;
#92008 = DIRECTION('ref_axis',(1.,0.,0.)) ;
#92009 = DIRECTION('center_axis',(0.,0.,-1.)) ;
#92010 = DIRECTION('ref_axis',(-1.,0.,0.)) ;
#92011 = DIRECTION('center_axis',(0.,1.,0.)) ;
#92012 = DIRECTION('ref_axis',(1.,0.,0.)) ;
#92013 = DIRECTION('center_axis',(1.,1.2303003375722E-16,0.)) ;
#92014 = DIRECTION('ref_axis',(1.2303003375722E-16,-1.,0.)) ;
#92015 = DIRECTION('center_axis',(0.,1.,0.)) ;
#92016 = DIRECTION('ref_axis',(-6.50521303491301E-15,0.,-1.)) ;
#92017 = DIRECTION('center_axis',(6.27714964143733E-33,-5.10212787052002E-17,
-1.)) ;
#92018 = DIRECTION('ref_axis',(0.,1.,0.)) ;
#92019 = DIRECTION('center_axis',(0.,-1.,0.)) ;
#92020 = DIRECTION('ref_axis',(0.,0.,1.)) ;
#92021 = DIRECTION('center_axis',(2.16840434497101E-16,-1.,5.10212787052002E-17)) ;
#92022 = DIRECTION('ref_axis',(1.,2.16840434497101E-16,-5.47382212626882E-48)) ;
#92023 = DIRECTION('center_axis',(0.,1.,0.)) ;
#92024 = DIRECTION('ref_axis',(0.,0.,-1.)) ;
#92025 = DIRECTION('center_axis',(0.,0.,1.)) ;
#92026 = DIRECTION('ref_axis',(1.,0.,0.)) ;
#92027 = DIRECTION('center_axis',(0.,0.,-1.)) ;
#92028 = DIRECTION('ref_axis',(-1.,0.,0.)) ;
#92029 = DIRECTION('center_axis',(-1.,-1.2303003375722E-16,0.)) ;
#92030 = DIRECTION('ref_axis',(0.,-1.,0.)) ;
#92031 = DIRECTION('center_axis',(0.,-1.,0.)) ;
#92032 = DIRECTION('ref_axis',(0.,0.,1.)) ;
#92033 = DIRECTION('center_axis',(1.53063836115601E-16,-1.,5.10212787052002E-17)) ;
#92034 = DIRECTION('ref_axis',(1.,1.53063836115601E-16,-6.84227765783602E-48)) ;
#92035 = DIRECTION('',(-1.53063836115601E-16,1.,-5.10212787052002E-17)) ;
#92036 = DIRECTION('center_axis',(0.,-1.,0.)) ;
#92037 = DIRECTION('ref_axis',(0.,0.,-1.)) ;
#92038 = DIRECTION('center_axis',(-1.,0.,0.)) ;
#92039 = DIRECTION('ref_axis',(0.,0.,-1.)) ;
#92040 = DIRECTION('center_axis',(-1.2303003375722E-16,1.,-5.10212787052002E-17)) ;
#92041 = DIRECTION('ref_axis',(-1.,-1.2303003375722E-16,6.27714964143733E-33)) ;
#92042 = DIRECTION('center_axis',(-8.67361737988403E-15,-1.,0.)) ;
#92043 = DIRECTION('ref_axis',(1.,-8.67361737988403E-15,0.)) ;
#92044 = DIRECTION('center_axis',(1.,0.,6.27714964143733E-33)) ;
#92045 = DIRECTION('ref_axis',(6.27714964143733E-33,0.,-1.)) ;
#92046 = DIRECTION('center_axis',(-1.,0.,-6.50521303491318E-15)) ;
#92047 = DIRECTION('ref_axis',(-6.50521303491318E-15,0.,1.)) ;
#92048 = DIRECTION('center_axis',(1.,0.,0.)) ;
#92049 = DIRECTION('ref_axis',(0.,1.,0.)) ;
#92050 = DIRECTION('center_axis',(0.,0.,-1.)) ;
#92051 = DIRECTION('ref_axis',(-1.,0.,0.)) ;
#92052 = DIRECTION('center_axis',(0.,0.,1.)) ;
#92053 = DIRECTION('ref_axis',(1.,0.,0.)) ;
#92054 = DIRECTION('center_axis',(0.,0.,-1.)) ;
#92055 = DIRECTION('ref_axis',(-1.,0.,0.)) ;
#92056 = DIRECTION('center_axis',(-1.,0.,0.)) ;
#92057 = DIRECTION('ref_axis',(0.,0.,1.)) ;
#92058 = DIRECTION('center_axis',(0.,-1.,0.)) ;
#92059 = DIRECTION('ref_axis',(0.,0.,-1.)) ;
#92060 = DIRECTION('center_axis',(0.,1.,0.)) ;
#92061 = DIRECTION('ref_axis',(0.,0.,1.)) ;
#92062 = DIRECTION('center_axis',(0.,1.,-6.50521303491301E-15)) ;
#92063 = DIRECTION('ref_axis',(0.,6.50521303491301E-15,1.)) ;
#92064 = DIRECTION('center_axis',(0.,-1.,0.)) ;
#92065 = DIRECTION('ref_axis',(0.,0.,-1.)) ;
#92066 = DIRECTION('center_axis',(0.,-1.,0.)) ;
#92067 = DIRECTION('ref_axis',(0.,0.,-1.)) ;
#92068 = DIRECTION('center_axis',(0.,-1.,-1.07081696047951E-16)) ;
#92069 = DIRECTION('ref_axis',(0.,1.07081696047951E-16,-1.)) ;
#92070 = DIRECTION('center_axis',(0.,1.,0.)) ;
#92071 = DIRECTION('ref_axis',(0.,0.,1.)) ;
#92072 = DIRECTION('center_axis',(-1.,0.,0.)) ;
#92073 = DIRECTION('ref_axis',(0.,0.,1.)) ;
#92074 = DIRECTION('center_axis',(0.,0.,1.)) ;
#92075 = DIRECTION('ref_axis',(1.,0.,0.)) ;
#92076 = DIRECTION('center_axis',(0.,1.,0.)) ;
#92077 = DIRECTION('ref_axis',(0.,0.,1.)) ;
#92078 = DIRECTION('center_axis',(0.,0.,-1.)) ;
#92079 = DIRECTION('ref_axis',(-1.,0.,0.)) ;
#92080 = DIRECTION('center_axis',(0.,0.,1.)) ;
#92081 = DIRECTION('ref_axis',(1.,0.,0.)) ;
#92082 = DIRECTION('center_axis',(0.,0.,1.)) ;
#92083 = DIRECTION('ref_axis',(1.,0.,0.)) ;
#92084 = DIRECTION('center_axis',(0.,0.,1.)) ;
#92085 = DIRECTION('ref_axis',(1.,0.,0.)) ;
#92086 = DIRECTION('center_axis',(0.,0.,-1.)) ;
#92087 = DIRECTION('ref_axis',(-1.,0.,0.)) ;
#92088 = DIRECTION('center_axis',(0.,1.,0.)) ;
#92089 = DIRECTION('ref_axis',(0.,0.,1.)) ;
#92090 = DIRECTION('center_axis',(0.,-0.707106781186545,0.70710678118655)) ;
#92091 = DIRECTION('ref_axis',(0.,-0.70710678118655,-0.707106781186545)) ;
#92092 = DIRECTION('center_axis',(0.,1.,0.)) ;
#92093 = DIRECTION('ref_axis',(0.,0.,1.)) ;
#92094 = DIRECTION('center_axis',(0.,-0.514231796959101,-0.857651245551602)) ;
#92095 = DIRECTION('ref_axis',(0.,0.857651245551602,-0.514231796959101)) ;
#92096 = DIRECTION('center_axis',(0.,-0.707106781186548,0.707106781186547)) ;
#92097 = DIRECTION('ref_axis',(0.,-0.707106781186547,-0.707106781186548)) ;
#92098 = DIRECTION('center_axis',(0.,-0.707106781186552,0.707106781186543)) ;
#92099 = DIRECTION('ref_axis',(0.,-0.707106781186543,-0.707106781186552)) ;
#92100 = DIRECTION('center_axis',(-1.,0.,0.)) ;
#92101 = DIRECTION('ref_axis',(0.,0.,1.)) ;
#92102 = DIRECTION('center_axis',(0.,0.514231796959101,-0.857651245551602)) ;
#92103 = DIRECTION('ref_axis',(0.,0.857651245551602,0.514231796959101)) ;
#92104 = DIRECTION('center_axis',(0.,1.,0.)) ;
#92105 = DIRECTION('ref_axis',(0.,0.,1.)) ;
#92106 = DIRECTION('center_axis',(0.,0.,-1.)) ;
#92107 = DIRECTION('ref_axis',(-1.,0.,0.)) ;
#92108 = DIRECTION('center_axis',(0.,1.,0.)) ;
#92109 = DIRECTION('ref_axis',(0.,0.,1.)) ;
#92110 = DIRECTION('center_axis',(0.,0.,-1.)) ;
#92111 = DIRECTION('ref_axis',(-1.,0.,0.)) ;
#92112 = DIRECTION('center_axis',(0.,0.,-1.)) ;
#92113 = DIRECTION('ref_axis',(-1.,0.,0.)) ;
#92114 = DIRECTION('center_axis',(0.,0.,1.)) ;
#92115 = DIRECTION('ref_axis',(1.,0.,0.)) ;
#92116 = DIRECTION('center_axis',(0.,0.,-1.)) ;
#92117 = DIRECTION('ref_axis',(-1.,0.,0.)) ;
#92118 = DIRECTION('center_axis',(0.,1.,0.)) ;
#92119 = DIRECTION('ref_axis',(0.,0.,1.)) ;
#92120 = DIRECTION('center_axis',(0.,-1.,8.67361737988405E-15)) ;
#92121 = DIRECTION('ref_axis',(0.,-8.67361737988405E-15,-1.)) ;
#92122 = DIRECTION('center_axis',(0.,0.707106781186546,0.707106781186549)) ;
#92123 = DIRECTION('ref_axis',(0.,-0.707106781186549,0.707106781186546)) ;
#92124 = DIRECTION('center_axis',(0.,0.707106781186545,0.70710678118655)) ;
#92125 = DIRECTION('ref_axis',(0.,-0.70710678118655,0.707106781186545)) ;
#92126 = DIRECTION('center_axis',(0.,1.,1.07081696047951E-16)) ;
#92127 = DIRECTION('ref_axis',(0.,-1.07081696047951E-16,1.)) ;
#92128 = DIRECTION('center_axis',(0.,-1.,0.)) ;
#92129 = DIRECTION('ref_axis',(0.,0.,-1.)) ;
#92130 = DIRECTION('center_axis',(0.,1.,0.)) ;
#92131 = DIRECTION('ref_axis',(0.,0.,1.)) ;
#92132 = DIRECTION('center_axis',(0.,0.,1.)) ;
#92133 = DIRECTION('ref_axis',(1.,0.,0.)) ;
#92134 = DIRECTION('center_axis',(0.,1.,0.)) ;
#92135 = DIRECTION('ref_axis',(0.,0.,1.)) ;
#92136 = DIRECTION('center_axis',(0.,8.67361737988403E-15,1.)) ;
#92137 = DIRECTION('ref_axis',(0.,-1.,8.67361737988403E-15)) ;
#92138 = DIRECTION('center_axis',(0.,3.99416362155027E-15,1.)) ;
#92139 = DIRECTION('ref_axis',(0.,-1.,3.99416362155027E-15)) ;
#92140 = DIRECTION('center_axis',(0.,0.,1.)) ;
#92141 = DIRECTION('ref_axis',(1.,0.,0.)) ;
#92142 = DIRECTION('center_axis',(0.,0.,-1.)) ;
#92143 = DIRECTION('ref_axis',(-1.,0.,0.)) ;
#92144 = DIRECTION('center_axis',(0.,0.,1.)) ;
#92145 = DIRECTION('ref_axis',(1.,0.,0.)) ;
#92146 = DIRECTION('center_axis',(-1.,0.,0.)) ;
#92147 = DIRECTION('ref_axis',(0.,0.,1.)) ;
#92148 = DIRECTION('center_axis',(0.,1.,0.)) ;
#92149 = DIRECTION('ref_axis',(0.,0.,1.)) ;
#92150 = DIRECTION('center_axis',(-1.,0.,0.)) ;
#92151 = DIRECTION('ref_axis',(0.,0.,1.)) ;
#92152 = DIRECTION('center_axis',(0.,-1.,0.)) ;
#92153 = DIRECTION('ref_axis',(0.,0.,-1.)) ;
#92154 = DIRECTION('center_axis',(0.,1.,0.)) ;
#92155 = DIRECTION('ref_axis',(0.,0.,1.)) ;
#92156 = DIRECTION('center_axis',(0.,-1.,0.)) ;
#92157 = DIRECTION('ref_axis',(0.,0.,-1.)) ;
#92158 = DIRECTION('center_axis',(0.,1.,0.)) ;
#92159 = DIRECTION('ref_axis',(0.,0.,1.)) ;
#92160 = DIRECTION('center_axis',(0.,-1.,0.)) ;
#92161 = DIRECTION('ref_axis',(0.,0.,-1.)) ;
#92162 = DIRECTION('center_axis',(0.,1.,0.)) ;
#92163 = DIRECTION('ref_axis',(0.,0.,-1.)) ;
#92164 = DIRECTION('center_axis',(0.,0.,-1.)) ;
#92165 = DIRECTION('ref_axis',(-1.,0.,0.)) ;
#92166 = DIRECTION('center_axis',(0.,1.,0.)) ;
#92167 = DIRECTION('ref_axis',(0.,0.,-1.)) ;
#92168 = DIRECTION('center_axis',(0.,0.,-1.)) ;
#92169 = DIRECTION('ref_axis',(-1.,0.,0.)) ;
#92170 = DIRECTION('center_axis',(0.,0.,1.)) ;
#92171 = DIRECTION('ref_axis',(1.,0.,0.)) ;
#92172 = DIRECTION('center_axis',(0.,0.,-1.)) ;
#92173 = DIRECTION('ref_axis',(-1.,0.,0.)) ;
#92174 = DIRECTION('center_axis',(0.,0.,-1.)) ;
#92175 = DIRECTION('ref_axis',(-1.,0.,0.)) ;
#92176 = DIRECTION('center_axis',(0.,6.93889390390724E-14,-1.)) ;
#92177 = DIRECTION('ref_axis',(0.,1.,6.93889390390724E-14)) ;
#92178 = DIRECTION('center_axis',(1.,0.,0.)) ;
#92179 = DIRECTION('ref_axis',(0.,0.,-1.)) ;
#92180 = DIRECTION('center_axis',(3.0665868333667E-15,0.707106781186532,-0.707106781186563)) ;
#92181 = DIRECTION('ref_axis',(-5.39294103027656E-31,0.707106781186563,0.707106781186532)) ;
#92182 = DIRECTION('center_axis',(1.,0.,0.)) ;
#92183 = DIRECTION('ref_axis',(0.,0.,-1.)) ;
#92184 = DIRECTION('center_axis',(0.,-1.,0.)) ;
#92185 = DIRECTION('ref_axis',(0.,0.,-1.)) ;
#92186 = DIRECTION('center_axis',(0.,-0.707106781186548,0.707106781186547)) ;
#92187 = DIRECTION('ref_axis',(0.,-0.707106781186547,-0.707106781186548)) ;
#92188 = DIRECTION('center_axis',(0.,-1.,-1.07081696047951E-16)) ;
#92189 = DIRECTION('ref_axis',(0.,1.07081696047951E-16,-1.)) ;
#92190 = DIRECTION('center_axis',(0.,-1.,-8.67361737988379E-15)) ;
#92191 = DIRECTION('ref_axis',(0.,8.67361737988379E-15,-1.)) ;
#92192 = DIRECTION('center_axis',(1.,0.,0.)) ;
#92193 = DIRECTION('ref_axis',(0.,0.,-1.)) ;
#92194 = DIRECTION('center_axis',(0.,0.,1.)) ;
#92195 = DIRECTION('ref_axis',(1.,0.,0.)) ;
#92196 = DIRECTION('center_axis',(0.,0.,-1.)) ;
#92197 = DIRECTION('ref_axis',(-1.,0.,0.)) ;
#92198 = DIRECTION('center_axis',(0.,0.,1.)) ;
#92199 = DIRECTION('ref_axis',(1.,0.,0.)) ;
#92200 = DIRECTION('center_axis',(0.,0.,1.)) ;
#92201 = DIRECTION('ref_axis',(1.,0.,0.)) ;
#92202 = DIRECTION('center_axis',(0.,0.,1.)) ;
#92203 = DIRECTION('ref_axis',(1.,0.,0.)) ;
#92204 = DIRECTION('center_axis',(1.,0.,0.)) ;
#92205 = DIRECTION('ref_axis',(0.,0.382683432365085,0.923879532511289)) ;
#92206 = DIRECTION('center_axis',(-3.0665868333667E-15,-0.707106781186532,
-0.707106781186563)) ;
#92207 = DIRECTION('ref_axis',(-5.39294103027656E-31,0.707106781186563,-0.707106781186532)) ;
#92208 = DIRECTION('center_axis',(1.,0.,0.)) ;
#92209 = DIRECTION('ref_axis',(0.,0.,-1.)) ;
#92210 = DIRECTION('center_axis',(0.,0.514231796959126,0.857651245551587)) ;
#92211 = DIRECTION('ref_axis',(0.,-0.857651245551587,0.514231796959126)) ;
#92212 = DIRECTION('center_axis',(0.,0.707106781186546,0.707106781186549)) ;
#92213 = DIRECTION('ref_axis',(0.,-0.707106781186549,0.707106781186546)) ;
#92214 = DIRECTION('center_axis',(3.06658683336673E-15,-0.707106781186539,
-0.707106781186556)) ;
#92215 = DIRECTION('ref_axis',(1.90456316695698E-29,0.707106781186556,-0.707106781186539)) ;
#92216 = DIRECTION('center_axis',(1.,0.,0.)) ;
#92217 = DIRECTION('ref_axis',(0.,0.,-1.)) ;
#92218 = DIRECTION('center_axis',(0.,-0.514231796959058,0.857651245551628)) ;
#92219 = DIRECTION('ref_axis',(0.,-0.857651245551628,-0.514231796959058)) ;
#92220 = DIRECTION('center_axis',(1.,0.,0.)) ;
#92221 = DIRECTION('ref_axis',(0.,0.,-1.)) ;
#92222 = DIRECTION('center_axis',(0.,0.,-1.)) ;
#92223 = DIRECTION('ref_axis',(-1.,0.,0.)) ;
#92224 = DIRECTION('center_axis',(1.,0.,0.)) ;
#92225 = DIRECTION('ref_axis',(0.,0.,-1.)) ;
#92226 = DIRECTION('center_axis',(0.,0.,1.)) ;
#92227 = DIRECTION('ref_axis',(1.,0.,0.)) ;
#92228 = DIRECTION('center_axis',(0.,3.99416362155027E-15,1.)) ;
#92229 = DIRECTION('ref_axis',(0.,-1.,3.99416362155027E-15)) ;
#92230 = DIRECTION('center_axis',(0.,0.,-1.)) ;
#92231 = DIRECTION('ref_axis',(-1.,0.,0.)) ;
#92232 = DIRECTION('center_axis',(0.,0.,1.)) ;
#92233 = DIRECTION('ref_axis',(1.,0.,0.)) ;
#92234 = DIRECTION('center_axis',(0.,-6.93889390390724E-14,1.)) ;
#92235 = DIRECTION('ref_axis',(0.,-1.,-6.93889390390724E-14)) ;
#92236 = DIRECTION('center_axis',(0.,1.,0.)) ;
#92237 = DIRECTION('ref_axis',(0.,0.,-1.)) ;
#92238 = DIRECTION('center_axis',(0.,-1.,0.)) ;
#92239 = DIRECTION('ref_axis',(0.,0.,-1.)) ;
#92240 = DIRECTION('center_axis',(1.,0.,0.)) ;
#92241 = DIRECTION('ref_axis',(0.,0.,-1.)) ;
#92242 = DIRECTION('center_axis',(0.,1.,0.)) ;
#92243 = DIRECTION('ref_axis',(0.,0.,1.)) ;
#92244 = DIRECTION('center_axis',(0.,1.,0.)) ;
#92245 = DIRECTION('ref_axis',(0.,0.,1.)) ;
#92246 = DIRECTION('center_axis',(0.,-1.,0.)) ;
#92247 = DIRECTION('ref_axis',(0.,0.,-1.)) ;
#92248 = DIRECTION('center_axis',(0.,1.,1.07081696047951E-16)) ;
#92249 = DIRECTION('ref_axis',(0.,-1.07081696047951E-16,1.)) ;
#92250 = DIRECTION('center_axis',(0.,1.,6.50521303491284E-15)) ;
#92251 = DIRECTION('ref_axis',(0.,-6.50521303491284E-15,1.)) ;
#92252 = DIRECTION('center_axis',(0.,1.,0.)) ;
#92253 = DIRECTION('ref_axis',(0.,0.,-1.)) ;
#92254 = DIRECTION('center_axis',(0.,0.,1.)) ;
#92255 = DIRECTION('ref_axis',(1.,0.,0.)) ;
#92256 = DIRECTION('center_axis',(1.,0.,0.)) ;
#92257 = DIRECTION('ref_axis',(0.,0.,-1.)) ;
#92258 = DIRECTION('center_axis',(0.,0.,-1.)) ;
#92259 = DIRECTION('ref_axis',(-1.,0.,0.)) ;
#92260 = DIRECTION('center_axis',(0.,0.,-1.)) ;
#92261 = DIRECTION('ref_axis',(-1.,0.,0.)) ;
#92262 = DIRECTION('center_axis',(0.,-1.,0.)) ;
#92263 = DIRECTION('ref_axis',(0.,0.,-1.)) ;
#92264 = DIRECTION('center_axis',(0.,1.,0.)) ;
#92265 = DIRECTION('ref_axis',(0.,0.,1.)) ;
#92266 = DIRECTION('center_axis',(0.,-1.,0.)) ;
#92267 = DIRECTION('ref_axis',(0.,0.,-1.)) ;
#92268 = DIRECTION('center_axis',(0.,1.,0.)) ;
#92269 = DIRECTION('ref_axis',(0.,0.,-1.)) ;
#92270 = DIRECTION('center_axis',(0.,0.,-1.)) ;
#92271 = DIRECTION('ref_axis',(-1.,0.,0.)) ;
#92272 = DIRECTION('center_axis',(0.,1.,0.)) ;
#92273 = DIRECTION('ref_axis',(0.,0.,-1.)) ;
#92274 = DIRECTION('center_axis',(0.,0.,-1.)) ;
#92275 = DIRECTION('ref_axis',(-1.,0.,0.)) ;
#92276 = DIRECTION('center_axis',(0.,0.,1.)) ;
#92277 = DIRECTION('ref_axis',(1.,0.,0.)) ;
#92278 = DIRECTION('center_axis',(0.,0.,-1.)) ;
#92279 = DIRECTION('ref_axis',(-1.,0.,0.)) ;
#92280 = DIRECTION('center_axis',(0.,0.,-1.)) ;
#92281 = DIRECTION('ref_axis',(-1.,0.,0.)) ;
#92282 = DIRECTION('center_axis',(0.,0.,-1.)) ;
#92283 = DIRECTION('ref_axis',(-1.,0.,0.)) ;
#92284 = DIRECTION('center_axis',(1.,0.,0.)) ;
#92285 = DIRECTION('ref_axis',(0.,0.,-1.)) ;
#92286 = DIRECTION('center_axis',(3.0665868333667E-15,0.707106781186532,-0.707106781186563)) ;
#92287 = DIRECTION('ref_axis',(-5.39294103027656E-31,0.707106781186563,0.707106781186532)) ;
#92288 = DIRECTION('center_axis',(1.,0.,0.)) ;
#92289 = DIRECTION('ref_axis',(0.,0.,-1.)) ;
#92290 = DIRECTION('center_axis',(0.,-1.,0.)) ;
#92291 = DIRECTION('ref_axis',(0.,0.,-1.)) ;
#92292 = DIRECTION('center_axis',(0.,-0.707106781186548,0.707106781186547)) ;
#92293 = DIRECTION('ref_axis',(0.,-0.707106781186547,-0.707106781186548)) ;
#92294 = DIRECTION('center_axis',(0.,-1.,-1.07081696047951E-16)) ;
#92295 = DIRECTION('ref_axis',(0.,1.07081696047951E-16,-1.)) ;
#92296 = DIRECTION('center_axis',(0.,-1.,-8.67361737988379E-15)) ;
#92297 = DIRECTION('ref_axis',(0.,8.67361737988379E-15,-1.)) ;
#92298 = DIRECTION('center_axis',(1.,0.,0.)) ;
#92299 = DIRECTION('ref_axis',(0.,0.,-1.)) ;
#92300 = DIRECTION('center_axis',(0.,0.,1.)) ;
#92301 = DIRECTION('ref_axis',(1.,0.,0.)) ;
#92302 = DIRECTION('center_axis',(0.,0.,-1.)) ;
#92303 = DIRECTION('ref_axis',(-1.,0.,0.)) ;
#92304 = DIRECTION('center_axis',(0.,0.,1.)) ;
#92305 = DIRECTION('ref_axis',(1.,0.,0.)) ;
#92306 = DIRECTION('center_axis',(0.,0.,1.)) ;
#92307 = DIRECTION('ref_axis',(1.,0.,0.)) ;
#92308 = DIRECTION('center_axis',(0.,0.,1.)) ;
#92309 = DIRECTION('ref_axis',(1.,0.,0.)) ;
#92310 = DIRECTION('center_axis',(1.,0.,0.)) ;
#92311 = DIRECTION('ref_axis',(0.,0.382683432365093,0.923879532511286)) ;
#92312 = DIRECTION('center_axis',(6.13317366673366E-15,-0.707106781186563,
-0.707106781186532)) ;
#92313 = DIRECTION('ref_axis',(-1.7381816909424E-29,0.707106781186532,-0.707106781186563)) ;
#92314 = DIRECTION('center_axis',(1.,0.,0.)) ;
#92315 = DIRECTION('ref_axis',(0.,0.,-1.)) ;
#92316 = DIRECTION('center_axis',(0.,0.514231796959126,0.857651245551587)) ;
#92317 = DIRECTION('ref_axis',(0.,-0.857651245551587,0.514231796959126)) ;
#92318 = DIRECTION('center_axis',(0.,0.707106781186546,0.707106781186549)) ;
#92319 = DIRECTION('ref_axis',(0.,-0.707106781186549,0.707106781186546)) ;
#92320 = DIRECTION('center_axis',(3.06658683336673E-15,-0.707106781186539,
-0.707106781186556)) ;
#92321 = DIRECTION('ref_axis',(1.90456316695698E-29,0.707106781186556,-0.707106781186539)) ;
#92322 = DIRECTION('center_axis',(1.,0.,0.)) ;
#92323 = DIRECTION('ref_axis',(0.,0.,-1.)) ;
#92324 = DIRECTION('center_axis',(0.,-0.514231796959091,0.857651245551608)) ;
#92325 = DIRECTION('ref_axis',(0.,-0.857651245551608,-0.514231796959091)) ;
#92326 = DIRECTION('center_axis',(1.,0.,0.)) ;
#92327 = DIRECTION('ref_axis',(0.,0.,-1.)) ;
#92328 = DIRECTION('center_axis',(0.,0.,-1.)) ;
#92329 = DIRECTION('ref_axis',(-1.,0.,0.)) ;
#92330 = DIRECTION('center_axis',(1.,0.,0.)) ;
#92331 = DIRECTION('ref_axis',(0.,0.,-1.)) ;
#92332 = DIRECTION('center_axis',(0.,0.,1.)) ;
#92333 = DIRECTION('ref_axis',(1.,0.,0.)) ;
#92334 = DIRECTION('center_axis',(0.,3.99416362155027E-15,1.)) ;
#92335 = DIRECTION('ref_axis',(0.,-1.,3.99416362155027E-15)) ;
#92336 = DIRECTION('center_axis',(0.,0.,-1.)) ;
#92337 = DIRECTION('ref_axis',(-1.,0.,0.)) ;
#92338 = DIRECTION('center_axis',(0.,0.,1.)) ;
#92339 = DIRECTION('ref_axis',(1.,0.,0.)) ;
#92340 = DIRECTION('center_axis',(0.,0.,1.)) ;
#92341 = DIRECTION('ref_axis',(1.,0.,0.)) ;
#92342 = DIRECTION('center_axis',(0.,1.,0.)) ;
#92343 = DIRECTION('ref_axis',(0.,0.,-1.)) ;
#92344 = DIRECTION('center_axis',(0.,-1.,0.)) ;
#92345 = DIRECTION('ref_axis',(0.,0.,-1.)) ;
#92346 = DIRECTION('center_axis',(1.,0.,0.)) ;
#92347 = DIRECTION('ref_axis',(0.,0.,-1.)) ;
#92348 = DIRECTION('center_axis',(0.,1.,0.)) ;
#92349 = DIRECTION('ref_axis',(0.,0.,1.)) ;
#92350 = DIRECTION('center_axis',(0.,1.,0.)) ;
#92351 = DIRECTION('ref_axis',(0.,0.,1.)) ;
#92352 = DIRECTION('center_axis',(0.,-1.,0.)) ;
#92353 = DIRECTION('ref_axis',(0.,0.,-1.)) ;
#92354 = DIRECTION('center_axis',(0.,1.,1.07081696047951E-16)) ;
#92355 = DIRECTION('ref_axis',(0.,-1.07081696047951E-16,1.)) ;
#92356 = DIRECTION('center_axis',(0.,1.,6.50521303491307E-15)) ;
#92357 = DIRECTION('ref_axis',(0.,-6.50521303491307E-15,1.)) ;
#92358 = DIRECTION('center_axis',(0.,1.,0.)) ;
#92359 = DIRECTION('ref_axis',(0.,0.,-1.)) ;
#92360 = DIRECTION('center_axis',(0.,0.,1.)) ;
#92361 = DIRECTION('ref_axis',(1.,0.,0.)) ;
#92362 = DIRECTION('center_axis',(1.,0.,0.)) ;
#92363 = DIRECTION('ref_axis',(0.,0.,-1.)) ;
#92364 = DIRECTION('center_axis',(0.,0.,-1.)) ;
#92365 = DIRECTION('ref_axis',(-1.,0.,0.)) ;
#92366 = DIRECTION('center_axis',(0.,0.,-1.)) ;
#92367 = DIRECTION('ref_axis',(-1.,0.,0.)) ;
#92368 = DIRECTION('center_axis',(0.,-1.,0.)) ;
#92369 = DIRECTION('ref_axis',(0.,0.,-1.)) ;
#92370 = DIRECTION('center_axis',(0.,1.,0.)) ;
#92371 = DIRECTION('ref_axis',(0.,0.,1.)) ;
#92372 = DIRECTION('center_axis',(0.,-1.,0.)) ;
#92373 = DIRECTION('ref_axis',(0.,0.,-1.)) ;
#92374 = DIRECTION('center_axis',(0.,1.,0.)) ;
#92375 = DIRECTION('ref_axis',(0.,0.,-1.)) ;
#92376 = DIRECTION('center_axis',(0.,0.,-1.)) ;
#92377 = DIRECTION('ref_axis',(-1.,0.,0.)) ;
#92378 = DIRECTION('center_axis',(0.,1.,0.)) ;
#92379 = DIRECTION('ref_axis',(0.,0.,-1.)) ;
#92380 = DIRECTION('center_axis',(0.,0.,-1.)) ;
#92381 = DIRECTION('ref_axis',(-1.,0.,0.)) ;
#92382 = DIRECTION('center_axis',(0.,0.,1.)) ;
#92383 = DIRECTION('ref_axis',(1.,0.,0.)) ;
#92384 = DIRECTION('center_axis',(0.,0.,-1.)) ;
#92385 = DIRECTION('ref_axis',(-1.,0.,0.)) ;
#92386 = DIRECTION('center_axis',(0.,0.,-1.)) ;
#92387 = DIRECTION('ref_axis',(-1.,0.,0.)) ;
#92388 = DIRECTION('center_axis',(0.,0.,-1.)) ;
#92389 = DIRECTION('ref_axis',(-1.,0.,0.)) ;
#92390 = DIRECTION('center_axis',(1.,0.,0.)) ;
#92391 = DIRECTION('ref_axis',(0.,0.,-1.)) ;
#92392 = DIRECTION('center_axis',(-6.13317366673366E-15,0.707106781186563,
-0.707106781186532)) ;
#92393 = DIRECTION('ref_axis',(-1.7381816909424E-29,0.707106781186532,0.707106781186563)) ;
#92394 = DIRECTION('center_axis',(1.,0.,0.)) ;
#92395 = DIRECTION('ref_axis',(0.,0.,-1.)) ;
#92396 = DIRECTION('center_axis',(0.,-1.,0.)) ;
#92397 = DIRECTION('ref_axis',(0.,0.,-1.)) ;
#92398 = DIRECTION('center_axis',(0.,-0.707106781186548,0.707106781186547)) ;
#92399 = DIRECTION('ref_axis',(0.,-0.707106781186547,-0.707106781186548)) ;
#92400 = DIRECTION('center_axis',(0.,-1.,-1.07081696047951E-16)) ;
#92401 = DIRECTION('ref_axis',(0.,1.07081696047951E-16,-1.)) ;
#92402 = DIRECTION('center_axis',(0.,-1.,-8.67361737988409E-15)) ;
#92403 = DIRECTION('ref_axis',(0.,8.67361737988409E-15,-1.)) ;
#92404 = DIRECTION('center_axis',(1.,0.,0.)) ;
#92405 = DIRECTION('ref_axis',(0.,0.,-1.)) ;
#92406 = DIRECTION('center_axis',(0.,0.,1.)) ;
#92407 = DIRECTION('ref_axis',(1.,0.,0.)) ;
#92408 = DIRECTION('center_axis',(0.,0.,-1.)) ;
#92409 = DIRECTION('ref_axis',(-1.,0.,0.)) ;
#92410 = DIRECTION('center_axis',(0.,0.,1.)) ;
#92411 = DIRECTION('ref_axis',(1.,0.,0.)) ;
#92412 = DIRECTION('center_axis',(0.,0.,1.)) ;
#92413 = DIRECTION('ref_axis',(1.,0.,0.)) ;
#92414 = DIRECTION('center_axis',(0.,0.,1.)) ;
#92415 = DIRECTION('ref_axis',(1.,0.,0.)) ;
#92416 = DIRECTION('center_axis',(1.,0.,0.)) ;
#92417 = DIRECTION('ref_axis',(0.,0.382683432365093,0.923879532511286)) ;
#92418 = DIRECTION('center_axis',(6.13317366673366E-15,-0.707106781186563,
-0.707106781186532)) ;
#92419 = DIRECTION('ref_axis',(-1.7381816909424E-29,0.707106781186532,-0.707106781186563)) ;
#92420 = DIRECTION('center_axis',(1.,0.,0.)) ;
#92421 = DIRECTION('ref_axis',(0.,0.,-1.)) ;
#92422 = DIRECTION('center_axis',(0.,0.514231796959093,0.857651245551607)) ;
#92423 = DIRECTION('ref_axis',(0.,-0.857651245551607,0.514231796959093)) ;
#92424 = DIRECTION('center_axis',(0.,0.707106781186546,0.707106781186549)) ;
#92425 = DIRECTION('ref_axis',(0.,-0.707106781186549,0.707106781186546)) ;
#92426 = DIRECTION('center_axis',(3.06658683336673E-15,-0.707106781186539,
-0.707106781186556)) ;
#92427 = DIRECTION('ref_axis',(1.90456316695698E-29,0.707106781186556,-0.707106781186539)) ;
#92428 = DIRECTION('center_axis',(1.,0.,0.)) ;
#92429 = DIRECTION('ref_axis',(0.,0.,-1.)) ;
#92430 = DIRECTION('center_axis',(0.,-0.514231796959091,0.857651245551608)) ;
#92431 = DIRECTION('ref_axis',(0.,-0.857651245551608,-0.514231796959091)) ;
#92432 = DIRECTION('center_axis',(1.,0.,0.)) ;
#92433 = DIRECTION('ref_axis',(0.,0.,-1.)) ;
#92434 = DIRECTION('center_axis',(0.,0.,-1.)) ;
#92435 = DIRECTION('ref_axis',(-1.,0.,0.)) ;
#92436 = DIRECTION('center_axis',(1.,0.,0.)) ;
#92437 = DIRECTION('ref_axis',(0.,0.,-1.)) ;
#92438 = DIRECTION('center_axis',(0.,0.,1.)) ;
#92439 = DIRECTION('ref_axis',(1.,0.,0.)) ;
#92440 = DIRECTION('center_axis',(0.,3.99416362155027E-15,1.)) ;
#92441 = DIRECTION('ref_axis',(0.,-1.,3.99416362155027E-15)) ;
#92442 = DIRECTION('center_axis',(0.,0.,-1.)) ;
#92443 = DIRECTION('ref_axis',(-1.,0.,0.)) ;
#92444 = DIRECTION('center_axis',(0.,0.,1.)) ;
#92445 = DIRECTION('ref_axis',(1.,0.,0.)) ;
#92446 = DIRECTION('center_axis',(0.,0.,1.)) ;
#92447 = DIRECTION('ref_axis',(1.,0.,0.)) ;
#92448 = DIRECTION('center_axis',(0.,1.,0.)) ;
#92449 = DIRECTION('ref_axis',(0.,0.,-1.)) ;
#92450 = DIRECTION('center_axis',(0.,-1.,0.)) ;
#92451 = DIRECTION('ref_axis',(0.,0.,-1.)) ;
#92452 = DIRECTION('center_axis',(1.,0.,0.)) ;
#92453 = DIRECTION('ref_axis',(0.,0.,-1.)) ;
#92454 = DIRECTION('center_axis',(0.,1.,0.)) ;
#92455 = DIRECTION('ref_axis',(0.,0.,1.)) ;
#92456 = DIRECTION('center_axis',(0.,1.,0.)) ;
#92457 = DIRECTION('ref_axis',(0.,0.,1.)) ;
#92458 = DIRECTION('center_axis',(0.,-1.,0.)) ;
#92459 = DIRECTION('ref_axis',(0.,0.,-1.)) ;
#92460 = DIRECTION('center_axis',(0.,1.,1.07081696047951E-16)) ;
#92461 = DIRECTION('ref_axis',(0.,-1.07081696047951E-16,1.)) ;
#92462 = DIRECTION('center_axis',(0.,1.,6.50521303491307E-15)) ;
#92463 = DIRECTION('ref_axis',(0.,-6.50521303491307E-15,1.)) ;
#92464 = DIRECTION('center_axis',(0.,1.,0.)) ;
#92465 = DIRECTION('ref_axis',(0.,0.,-1.)) ;
#92466 = DIRECTION('center_axis',(0.,0.,1.)) ;
#92467 = DIRECTION('ref_axis',(1.,0.,0.)) ;
#92468 = DIRECTION('center_axis',(1.,0.,0.)) ;
#92469 = DIRECTION('ref_axis',(0.,0.,-1.)) ;
#92470 = DIRECTION('center_axis',(0.,0.,-1.)) ;
#92471 = DIRECTION('ref_axis',(-1.,0.,0.)) ;
#92472 = DIRECTION('center_axis',(0.,0.,-1.)) ;
#92473 = DIRECTION('ref_axis',(-1.,0.,0.)) ;
#92474 = DIRECTION('center_axis',(0.,-1.,0.)) ;
#92475 = DIRECTION('ref_axis',(0.,0.,-1.)) ;
#92476 = DIRECTION('center_axis',(0.,1.,0.)) ;
#92477 = DIRECTION('ref_axis',(0.,0.,1.)) ;
#92478 = DIRECTION('center_axis',(0.,-1.,0.)) ;
#92479 = DIRECTION('ref_axis',(0.,0.,-1.)) ;
#92480 = DIRECTION('center_axis',(0.,1.,0.)) ;
#92481 = DIRECTION('ref_axis',(0.,0.,-1.)) ;
#92482 = DIRECTION('center_axis',(0.,0.,-1.)) ;
#92483 = DIRECTION('ref_axis',(-1.,0.,0.)) ;
#92484 = DIRECTION('center_axis',(0.,1.,0.)) ;
#92485 = DIRECTION('ref_axis',(0.,0.,-1.)) ;
#92486 = DIRECTION('center_axis',(0.,0.,-1.)) ;
#92487 = DIRECTION('ref_axis',(-1.,0.,0.)) ;
#92488 = DIRECTION('center_axis',(0.,0.,1.)) ;
#92489 = DIRECTION('ref_axis',(1.,0.,0.)) ;
#92490 = DIRECTION('center_axis',(0.,0.,-1.)) ;
#92491 = DIRECTION('ref_axis',(-1.,0.,0.)) ;
#92492 = DIRECTION('center_axis',(0.,0.,-1.)) ;
#92493 = DIRECTION('ref_axis',(-1.,0.,0.)) ;
#92494 = DIRECTION('center_axis',(0.,0.,-1.)) ;
#92495 = DIRECTION('ref_axis',(-1.,0.,0.)) ;
#92496 = DIRECTION('center_axis',(1.,0.,0.)) ;
#92497 = DIRECTION('ref_axis',(0.,0.,-1.)) ;
#92498 = DIRECTION('center_axis',(-6.13317366673366E-15,0.707106781186563,
-0.707106781186532)) ;
#92499 = DIRECTION('ref_axis',(-1.7381816909424E-29,0.707106781186532,0.707106781186563)) ;
#92500 = DIRECTION('center_axis',(1.,0.,0.)) ;
#92501 = DIRECTION('ref_axis',(0.,0.,-1.)) ;
#92502 = DIRECTION('center_axis',(0.,-1.,0.)) ;
#92503 = DIRECTION('ref_axis',(0.,0.,-1.)) ;
#92504 = DIRECTION('center_axis',(0.,-0.707106781186548,0.707106781186547)) ;
#92505 = DIRECTION('ref_axis',(0.,-0.707106781186547,-0.707106781186548)) ;
#92506 = DIRECTION('center_axis',(0.,-1.,-1.07081696047951E-16)) ;
#92507 = DIRECTION('ref_axis',(0.,1.07081696047951E-16,-1.)) ;
#92508 = DIRECTION('center_axis',(0.,-1.,-8.67361737988409E-15)) ;
#92509 = DIRECTION('ref_axis',(0.,8.67361737988409E-15,-1.)) ;
#92510 = DIRECTION('center_axis',(1.,0.,0.)) ;
#92511 = DIRECTION('ref_axis',(0.,0.,-1.)) ;
#92512 = DIRECTION('center_axis',(0.,0.,1.)) ;
#92513 = DIRECTION('ref_axis',(1.,0.,0.)) ;
#92514 = DIRECTION('center_axis',(0.,0.,-1.)) ;
#92515 = DIRECTION('ref_axis',(-1.,0.,0.)) ;
#92516 = DIRECTION('center_axis',(0.,0.,1.)) ;
#92517 = DIRECTION('ref_axis',(1.,0.,0.)) ;
#92518 = DIRECTION('center_axis',(0.,0.,1.)) ;
#92519 = DIRECTION('ref_axis',(1.,0.,0.)) ;
#92520 = DIRECTION('center_axis',(0.,0.,1.)) ;
#92521 = DIRECTION('ref_axis',(1.,0.,0.)) ;
#92522 = DIRECTION('center_axis',(1.,0.,0.)) ;
#92523 = DIRECTION('ref_axis',(0.,0.382683432365092,0.923879532511286)) ;
#92524 = DIRECTION('center_axis',(6.13317366673366E-15,-0.707106781186563,
-0.707106781186532)) ;
#92525 = DIRECTION('ref_axis',(-1.7381816909424E-29,0.707106781186532,-0.707106781186563)) ;
#92526 = DIRECTION('center_axis',(1.,0.,0.)) ;
#92527 = DIRECTION('ref_axis',(0.,0.,-1.)) ;
#92528 = DIRECTION('center_axis',(0.,0.514231796959093,0.857651245551607)) ;
#92529 = DIRECTION('ref_axis',(0.,-0.857651245551607,0.514231796959093)) ;
#92530 = DIRECTION('center_axis',(0.,0.707106781186546,0.707106781186549)) ;
#92531 = DIRECTION('ref_axis',(0.,-0.707106781186549,0.707106781186546)) ;
#92532 = DIRECTION('center_axis',(3.06658683336673E-15,-0.707106781186539,
-0.707106781186556)) ;
#92533 = DIRECTION('ref_axis',(1.90456316695698E-29,0.707106781186556,-0.707106781186539)) ;
#92534 = DIRECTION('center_axis',(1.,0.,0.)) ;
#92535 = DIRECTION('ref_axis',(0.,0.,-1.)) ;
#92536 = DIRECTION('center_axis',(0.,-0.514231796959091,0.857651245551608)) ;
#92537 = DIRECTION('ref_axis',(0.,-0.857651245551608,-0.514231796959091)) ;
#92538 = DIRECTION('center_axis',(1.,0.,0.)) ;
#92539 = DIRECTION('ref_axis',(0.,0.,-1.)) ;
#92540 = DIRECTION('center_axis',(0.,0.,-1.)) ;
#92541 = DIRECTION('ref_axis',(-1.,0.,0.)) ;
#92542 = DIRECTION('center_axis',(1.,0.,0.)) ;
#92543 = DIRECTION('ref_axis',(0.,0.,-1.)) ;
#92544 = DIRECTION('center_axis',(0.,0.,1.)) ;
#92545 = DIRECTION('ref_axis',(1.,0.,0.)) ;
#92546 = DIRECTION('center_axis',(0.,3.99416362155027E-15,1.)) ;
#92547 = DIRECTION('ref_axis',(0.,-1.,3.99416362155027E-15)) ;
#92548 = DIRECTION('center_axis',(0.,0.,-1.)) ;
#92549 = DIRECTION('ref_axis',(-1.,0.,0.)) ;
#92550 = DIRECTION('center_axis',(0.,0.,1.)) ;
#92551 = DIRECTION('ref_axis',(1.,0.,0.)) ;
#92552 = DIRECTION('center_axis',(0.,0.,1.)) ;
#92553 = DIRECTION('ref_axis',(1.,0.,0.)) ;
#92554 = DIRECTION('center_axis',(0.,1.,0.)) ;
#92555 = DIRECTION('ref_axis',(0.,0.,-1.)) ;
#92556 = DIRECTION('center_axis',(0.,-1.,0.)) ;
#92557 = DIRECTION('ref_axis',(0.,0.,-1.)) ;
#92558 = DIRECTION('center_axis',(1.,0.,0.)) ;
#92559 = DIRECTION('ref_axis',(0.,0.,-1.)) ;
#92560 = DIRECTION('center_axis',(0.,1.,0.)) ;
#92561 = DIRECTION('ref_axis',(0.,0.,1.)) ;
#92562 = DIRECTION('center_axis',(0.,1.,0.)) ;
#92563 = DIRECTION('ref_axis',(0.,0.,1.)) ;
#92564 = DIRECTION('center_axis',(0.,-1.,0.)) ;
#92565 = DIRECTION('ref_axis',(0.,0.,-1.)) ;
#92566 = DIRECTION('center_axis',(0.,1.,1.07081696047951E-16)) ;
#92567 = DIRECTION('ref_axis',(0.,-1.07081696047951E-16,1.)) ;
#92568 = DIRECTION('center_axis',(0.,1.,6.50521303491307E-15)) ;
#92569 = DIRECTION('ref_axis',(0.,-6.50521303491307E-15,1.)) ;
#92570 = DIRECTION('center_axis',(0.,1.,0.)) ;
#92571 = DIRECTION('ref_axis',(0.,0.,-1.)) ;
#92572 = DIRECTION('center_axis',(0.,0.,1.)) ;
#92573 = DIRECTION('ref_axis',(1.,0.,0.)) ;
#92574 = DIRECTION('center_axis',(1.,0.,0.)) ;
#92575 = DIRECTION('ref_axis',(0.,0.,-1.)) ;
#92576 = DIRECTION('center_axis',(0.,0.,-1.)) ;
#92577 = DIRECTION('ref_axis',(-1.,0.,0.)) ;
#92578 = DIRECTION('center_axis',(0.,0.,-1.)) ;
#92579 = DIRECTION('ref_axis',(-1.,0.,0.)) ;
#92580 = DIRECTION('center_axis',(0.,-1.,0.)) ;
#92581 = DIRECTION('ref_axis',(0.,0.,-1.)) ;
#92582 = DIRECTION('center_axis',(0.,1.,0.)) ;
#92583 = DIRECTION('ref_axis',(0.,0.,1.)) ;
#92584 = DIRECTION('center_axis',(0.,-1.,0.)) ;
#92585 = DIRECTION('ref_axis',(0.,0.,-1.)) ;
#92586 = DIRECTION('center_axis',(0.,1.,0.)) ;
#92587 = DIRECTION('ref_axis',(0.,0.,-1.)) ;
#92588 = DIRECTION('center_axis',(0.,0.,-1.)) ;
#92589 = DIRECTION('ref_axis',(-1.,0.,0.)) ;
#92590 = DIRECTION('center_axis',(0.,1.,0.)) ;
#92591 = DIRECTION('ref_axis',(0.,0.,-1.)) ;
#92592 = DIRECTION('center_axis',(0.,0.,-1.)) ;
#92593 = DIRECTION('ref_axis',(-1.,0.,0.)) ;
#92594 = DIRECTION('center_axis',(0.,0.,1.)) ;
#92595 = DIRECTION('ref_axis',(1.,0.,0.)) ;
#92596 = DIRECTION('center_axis',(0.,0.,-1.)) ;
#92597 = DIRECTION('ref_axis',(-1.,0.,0.)) ;
#92598 = DIRECTION('center_axis',(0.,0.,-1.)) ;
#92599 = DIRECTION('ref_axis',(-1.,0.,0.)) ;
#92600 = DIRECTION('center_axis',(0.,0.,-1.)) ;
#92601 = DIRECTION('ref_axis',(-1.,0.,0.)) ;
#92602 = DIRECTION('center_axis',(1.,0.,0.)) ;
#92603 = DIRECTION('ref_axis',(0.,0.,-1.)) ;
#92604 = DIRECTION('center_axis',(-6.13317366673366E-15,0.707106781186563,
-0.707106781186532)) ;
#92605 = DIRECTION('ref_axis',(-1.7381816909424E-29,0.707106781186532,0.707106781186563)) ;
#92606 = DIRECTION('center_axis',(1.,0.,0.)) ;
#92607 = DIRECTION('ref_axis',(0.,0.,-1.)) ;
#92608 = DIRECTION('center_axis',(0.,-1.,0.)) ;
#92609 = DIRECTION('ref_axis',(0.,0.,-1.)) ;
#92610 = DIRECTION('center_axis',(0.,-0.707106781186548,0.707106781186547)) ;
#92611 = DIRECTION('ref_axis',(0.,-0.707106781186547,-0.707106781186548)) ;
#92612 = DIRECTION('center_axis',(0.,-1.,-1.07081696047951E-16)) ;
#92613 = DIRECTION('ref_axis',(0.,1.07081696047951E-16,-1.)) ;
#92614 = DIRECTION('center_axis',(0.,-1.,-8.67361737988409E-15)) ;
#92615 = DIRECTION('ref_axis',(0.,8.67361737988409E-15,-1.)) ;
#92616 = DIRECTION('center_axis',(1.,0.,0.)) ;
#92617 = DIRECTION('ref_axis',(0.,0.,-1.)) ;
#92618 = DIRECTION('center_axis',(0.,0.,1.)) ;
#92619 = DIRECTION('ref_axis',(1.,0.,0.)) ;
#92620 = DIRECTION('center_axis',(0.,0.,-1.)) ;
#92621 = DIRECTION('ref_axis',(-1.,0.,0.)) ;
#92622 = DIRECTION('center_axis',(0.,0.,1.)) ;
#92623 = DIRECTION('ref_axis',(1.,0.,0.)) ;
#92624 = DIRECTION('center_axis',(0.,0.,1.)) ;
#92625 = DIRECTION('ref_axis',(1.,0.,0.)) ;
#92626 = DIRECTION('center_axis',(0.,0.,1.)) ;
#92627 = DIRECTION('ref_axis',(1.,0.,0.)) ;
#92628 = DIRECTION('center_axis',(1.,0.,0.)) ;
#92629 = DIRECTION('ref_axis',(0.,0.382683432365085,0.923879532511289)) ;
#92630 = DIRECTION('center_axis',(6.13317366673366E-15,-0.707106781186563,
-0.707106781186532)) ;
#92631 = DIRECTION('ref_axis',(-1.7381816909424E-29,0.707106781186532,-0.707106781186563)) ;
#92632 = DIRECTION('center_axis',(1.,0.,0.)) ;
#92633 = DIRECTION('ref_axis',(0.,0.,-1.)) ;
#92634 = DIRECTION('center_axis',(0.,0.514231796959093,0.857651245551607)) ;
#92635 = DIRECTION('ref_axis',(0.,-0.857651245551607,0.514231796959093)) ;
#92636 = DIRECTION('center_axis',(0.,0.707106781186546,0.707106781186549)) ;
#92637 = DIRECTION('ref_axis',(0.,-0.707106781186549,0.707106781186546)) ;
#92638 = DIRECTION('center_axis',(3.06658683336673E-15,-0.707106781186539,
-0.707106781186556)) ;
#92639 = DIRECTION('ref_axis',(1.90456316695698E-29,0.707106781186556,-0.707106781186539)) ;
#92640 = DIRECTION('center_axis',(1.,0.,0.)) ;
#92641 = DIRECTION('ref_axis',(0.,0.,-1.)) ;
#92642 = DIRECTION('center_axis',(0.,-0.514231796959091,0.857651245551608)) ;
#92643 = DIRECTION('ref_axis',(0.,-0.857651245551608,-0.514231796959091)) ;
#92644 = DIRECTION('center_axis',(1.,0.,0.)) ;
#92645 = DIRECTION('ref_axis',(0.,0.,-1.)) ;
#92646 = DIRECTION('center_axis',(0.,0.,-1.)) ;
#92647 = DIRECTION('ref_axis',(-1.,0.,0.)) ;
#92648 = DIRECTION('center_axis',(1.,0.,0.)) ;
#92649 = DIRECTION('ref_axis',(0.,0.,-1.)) ;
#92650 = DIRECTION('center_axis',(0.,0.,1.)) ;
#92651 = DIRECTION('ref_axis',(1.,0.,0.)) ;
#92652 = DIRECTION('center_axis',(0.,3.99416362155027E-15,1.)) ;
#92653 = DIRECTION('ref_axis',(0.,-1.,3.99416362155027E-15)) ;
#92654 = DIRECTION('center_axis',(0.,0.,-1.)) ;
#92655 = DIRECTION('ref_axis',(-1.,0.,0.)) ;
#92656 = DIRECTION('center_axis',(0.,0.,1.)) ;
#92657 = DIRECTION('ref_axis',(1.,0.,0.)) ;
#92658 = DIRECTION('center_axis',(0.,0.,1.)) ;
#92659 = DIRECTION('ref_axis',(1.,0.,0.)) ;
#92660 = DIRECTION('center_axis',(0.,1.,0.)) ;
#92661 = DIRECTION('ref_axis',(0.,0.,-1.)) ;
#92662 = DIRECTION('center_axis',(0.,-1.,0.)) ;
#92663 = DIRECTION('ref_axis',(0.,0.,-1.)) ;
#92664 = DIRECTION('center_axis',(1.,0.,0.)) ;
#92665 = DIRECTION('ref_axis',(0.,0.,-1.)) ;
#92666 = DIRECTION('center_axis',(0.,1.,0.)) ;
#92667 = DIRECTION('ref_axis',(0.,0.,1.)) ;
#92668 = DIRECTION('center_axis',(0.,1.,0.)) ;
#92669 = DIRECTION('ref_axis',(0.,0.,1.)) ;
#92670 = DIRECTION('center_axis',(0.,-1.,0.)) ;
#92671 = DIRECTION('ref_axis',(0.,0.,-1.)) ;
#92672 = DIRECTION('center_axis',(0.,1.,1.07081696047951E-16)) ;
#92673 = DIRECTION('ref_axis',(0.,-1.07081696047951E-16,1.)) ;
#92674 = DIRECTION('center_axis',(0.,1.,6.50521303491307E-15)) ;
#92675 = DIRECTION('ref_axis',(0.,-6.50521303491307E-15,1.)) ;
#92676 = DIRECTION('center_axis',(0.,1.,0.)) ;
#92677 = DIRECTION('ref_axis',(0.,0.,-1.)) ;
#92678 = DIRECTION('center_axis',(0.,0.,1.)) ;
#92679 = DIRECTION('ref_axis',(1.,0.,0.)) ;
#92680 = DIRECTION('center_axis',(1.,0.,0.)) ;
#92681 = DIRECTION('ref_axis',(0.,0.,-1.)) ;
#92682 = DIRECTION('center_axis',(0.,0.,-1.)) ;
#92683 = DIRECTION('ref_axis',(-1.,0.,0.)) ;
#92684 = DIRECTION('center_axis',(0.,0.,-1.)) ;
#92685 = DIRECTION('ref_axis',(-1.,0.,0.)) ;
#92686 = DIRECTION('center_axis',(0.,-1.,0.)) ;
#92687 = DIRECTION('ref_axis',(0.,0.,-1.)) ;
#92688 = DIRECTION('center_axis',(0.,1.,0.)) ;
#92689 = DIRECTION('ref_axis',(0.,0.,1.)) ;
#92690 = DIRECTION('center_axis',(0.,-1.,0.)) ;
#92691 = DIRECTION('ref_axis',(0.,0.,-1.)) ;
#92692 = DIRECTION('center_axis',(0.,1.,0.)) ;
#92693 = DIRECTION('ref_axis',(0.,0.,-1.)) ;
#92694 = DIRECTION('center_axis',(0.,0.,-1.)) ;
#92695 = DIRECTION('ref_axis',(-1.,0.,0.)) ;
#92696 = DIRECTION('center_axis',(0.,1.,0.)) ;
#92697 = DIRECTION('ref_axis',(0.,0.,-1.)) ;
#92698 = DIRECTION('center_axis',(0.,0.,-1.)) ;
#92699 = DIRECTION('ref_axis',(-1.,0.,0.)) ;
#92700 = DIRECTION('center_axis',(0.,0.,1.)) ;
#92701 = DIRECTION('ref_axis',(1.,0.,0.)) ;
#92702 = DIRECTION('center_axis',(0.,0.,-1.)) ;
#92703 = DIRECTION('ref_axis',(-1.,0.,0.)) ;
#92704 = DIRECTION('center_axis',(0.,0.,-1.)) ;
#92705 = DIRECTION('ref_axis',(-1.,0.,0.)) ;
#92706 = DIRECTION('center_axis',(0.,0.,-1.)) ;
#92707 = DIRECTION('ref_axis',(-1.,0.,0.)) ;
#92708 = DIRECTION('center_axis',(1.,0.,0.)) ;
#92709 = DIRECTION('ref_axis',(0.,0.,-1.)) ;
#92710 = DIRECTION('center_axis',(-6.13317366673366E-15,0.707106781186563,
-0.707106781186532)) ;
#92711 = DIRECTION('ref_axis',(-1.7381816909424E-29,0.707106781186532,0.707106781186563)) ;
#92712 = DIRECTION('center_axis',(1.,0.,0.)) ;
#92713 = DIRECTION('ref_axis',(0.,0.,-1.)) ;
#92714 = DIRECTION('center_axis',(0.,-1.,0.)) ;
#92715 = DIRECTION('ref_axis',(0.,0.,-1.)) ;
#92716 = DIRECTION('center_axis',(0.,-0.707106781186548,0.707106781186547)) ;
#92717 = DIRECTION('ref_axis',(0.,-0.707106781186547,-0.707106781186548)) ;
#92718 = DIRECTION('center_axis',(0.,-1.,-1.07081696047951E-16)) ;
#92719 = DIRECTION('ref_axis',(0.,1.07081696047951E-16,-1.)) ;
#92720 = DIRECTION('center_axis',(0.,-1.,-8.67361737988409E-15)) ;
#92721 = DIRECTION('ref_axis',(0.,8.67361737988409E-15,-1.)) ;
#92722 = DIRECTION('center_axis',(1.,0.,0.)) ;
#92723 = DIRECTION('ref_axis',(0.,0.,-1.)) ;
#92724 = DIRECTION('center_axis',(0.,0.,1.)) ;
#92725 = DIRECTION('ref_axis',(1.,0.,0.)) ;
#92726 = DIRECTION('center_axis',(0.,0.,-1.)) ;
#92727 = DIRECTION('ref_axis',(-1.,0.,0.)) ;
#92728 = DIRECTION('center_axis',(0.,0.,1.)) ;
#92729 = DIRECTION('ref_axis',(1.,0.,0.)) ;
#92730 = DIRECTION('center_axis',(0.,0.,1.)) ;
#92731 = DIRECTION('ref_axis',(1.,0.,0.)) ;
#92732 = DIRECTION('center_axis',(0.,0.,1.)) ;
#92733 = DIRECTION('ref_axis',(1.,0.,0.)) ;
#92734 = DIRECTION('center_axis',(1.,0.,0.)) ;
#92735 = DIRECTION('ref_axis',(0.,0.382683432365081,0.92387953251129)) ;
#92736 = DIRECTION('center_axis',(0.,-0.707106781186548,-0.707106781186548)) ;
#92737 = DIRECTION('ref_axis',(0.,0.707106781186548,-0.707106781186548)) ;
#92738 = DIRECTION('center_axis',(1.,0.,0.)) ;
#92739 = DIRECTION('ref_axis',(0.,0.,-1.)) ;
#92740 = DIRECTION('center_axis',(0.,0.514231796959093,0.857651245551607)) ;
#92741 = DIRECTION('ref_axis',(0.,-0.857651245551607,0.514231796959093)) ;
#92742 = DIRECTION('center_axis',(0.,0.707106781186546,0.707106781186549)) ;
#92743 = DIRECTION('ref_axis',(0.,-0.707106781186549,0.707106781186546)) ;
#92744 = DIRECTION('center_axis',(0.,-0.707106781186548,-0.707106781186548)) ;
#92745 = DIRECTION('ref_axis',(0.,0.707106781186548,-0.707106781186548)) ;
#92746 = DIRECTION('center_axis',(1.,0.,0.)) ;
#92747 = DIRECTION('ref_axis',(0.,0.,-1.)) ;
#92748 = DIRECTION('center_axis',(0.,-0.514231796959109,0.857651245551597)) ;
#92749 = DIRECTION('ref_axis',(0.,-0.857651245551597,-0.514231796959109)) ;
#92750 = DIRECTION('center_axis',(1.,0.,0.)) ;
#92751 = DIRECTION('ref_axis',(0.,0.,-1.)) ;
#92752 = DIRECTION('center_axis',(0.,0.,-1.)) ;
#92753 = DIRECTION('ref_axis',(-1.,0.,0.)) ;
#92754 = DIRECTION('center_axis',(1.,0.,0.)) ;
#92755 = DIRECTION('ref_axis',(0.,0.,-1.)) ;
#92756 = DIRECTION('center_axis',(0.,0.,1.)) ;
#92757 = DIRECTION('ref_axis',(1.,0.,0.)) ;
#92758 = DIRECTION('center_axis',(0.,3.99416362155027E-15,1.)) ;
#92759 = DIRECTION('ref_axis',(0.,-1.,3.99416362155027E-15)) ;
#92760 = DIRECTION('center_axis',(0.,0.,-1.)) ;
#92761 = DIRECTION('ref_axis',(-1.,0.,0.)) ;
#92762 = DIRECTION('center_axis',(0.,0.,1.)) ;
#92763 = DIRECTION('ref_axis',(1.,0.,0.)) ;
#92764 = DIRECTION('center_axis',(0.,0.,1.)) ;
#92765 = DIRECTION('ref_axis',(1.,0.,0.)) ;
#92766 = DIRECTION('center_axis',(0.,1.,0.)) ;
#92767 = DIRECTION('ref_axis',(0.,0.,-1.)) ;
#92768 = DIRECTION('center_axis',(0.,-1.,0.)) ;
#92769 = DIRECTION('ref_axis',(0.,0.,-1.)) ;
#92770 = DIRECTION('center_axis',(1.,0.,0.)) ;
#92771 = DIRECTION('ref_axis',(0.,0.,-1.)) ;
#92772 = DIRECTION('center_axis',(0.,1.,0.)) ;
#92773 = DIRECTION('ref_axis',(0.,0.,1.)) ;
#92774 = DIRECTION('center_axis',(0.,1.,0.)) ;
#92775 = DIRECTION('ref_axis',(0.,0.,1.)) ;
#92776 = DIRECTION('center_axis',(0.,-1.,0.)) ;
#92777 = DIRECTION('ref_axis',(0.,0.,-1.)) ;
#92778 = DIRECTION('center_axis',(0.,1.,1.07081696047951E-16)) ;
#92779 = DIRECTION('ref_axis',(0.,-1.07081696047951E-16,1.)) ;
#92780 = DIRECTION('center_axis',(0.,1.,6.50521303491307E-15)) ;
#92781 = DIRECTION('ref_axis',(0.,-6.50521303491307E-15,1.)) ;
#92782 = DIRECTION('center_axis',(0.,1.,0.)) ;
#92783 = DIRECTION('ref_axis',(0.,0.,-1.)) ;
#92784 = DIRECTION('center_axis',(0.,0.,1.)) ;
#92785 = DIRECTION('ref_axis',(1.,0.,0.)) ;
#92786 = DIRECTION('center_axis',(1.,0.,0.)) ;
#92787 = DIRECTION('ref_axis',(0.,0.,-1.)) ;
#92788 = DIRECTION('center_axis',(0.,0.,-1.)) ;
#92789 = DIRECTION('ref_axis',(-1.,0.,0.)) ;
#92790 = DIRECTION('center_axis',(0.,0.,-1.)) ;
#92791 = DIRECTION('ref_axis',(-1.,0.,0.)) ;
#92792 = DIRECTION('center_axis',(0.,-1.,0.)) ;
#92793 = DIRECTION('ref_axis',(0.,0.,-1.)) ;
#92794 = DIRECTION('center_axis',(0.,1.,0.)) ;
#92795 = DIRECTION('ref_axis',(0.,0.,1.)) ;
#92796 = DIRECTION('center_axis',(0.,-1.,0.)) ;
#92797 = DIRECTION('ref_axis',(0.,0.,-1.)) ;
#92798 = DIRECTION('center_axis',(0.,1.,0.)) ;
#92799 = DIRECTION('ref_axis',(0.,0.,-1.)) ;
#92800 = DIRECTION('center_axis',(0.,0.,-1.)) ;
#92801 = DIRECTION('ref_axis',(-1.,0.,0.)) ;
#92802 = DIRECTION('center_axis',(0.,1.,0.)) ;
#92803 = DIRECTION('ref_axis',(0.,0.,-1.)) ;
#92804 = DIRECTION('center_axis',(0.,0.,-1.)) ;
#92805 = DIRECTION('ref_axis',(-1.,0.,0.)) ;
#92806 = DIRECTION('center_axis',(0.,0.,1.)) ;
#92807 = DIRECTION('ref_axis',(1.,0.,0.)) ;
#92808 = DIRECTION('center_axis',(0.,0.,-1.)) ;
#92809 = DIRECTION('ref_axis',(-1.,0.,0.)) ;
#92810 = DIRECTION('center_axis',(0.,0.,-1.)) ;
#92811 = DIRECTION('ref_axis',(-1.,0.,0.)) ;
#92812 = DIRECTION('center_axis',(0.,0.,-1.)) ;
#92813 = DIRECTION('ref_axis',(-1.,0.,0.)) ;
#92814 = DIRECTION('center_axis',(1.,0.,0.)) ;
#92815 = DIRECTION('ref_axis',(0.,0.,-1.)) ;
#92816 = DIRECTION('center_axis',(0.,0.707106781186548,-0.707106781186548)) ;
#92817 = DIRECTION('ref_axis',(0.,0.707106781186548,0.707106781186548)) ;
#92818 = DIRECTION('center_axis',(1.,0.,0.)) ;
#92819 = DIRECTION('ref_axis',(0.,0.,-1.)) ;
#92820 = DIRECTION('center_axis',(0.,-1.,0.)) ;
#92821 = DIRECTION('ref_axis',(0.,0.,-1.)) ;
#92822 = DIRECTION('center_axis',(0.,-0.707106781186548,0.707106781186547)) ;
#92823 = DIRECTION('ref_axis',(0.,-0.707106781186547,-0.707106781186548)) ;
#92824 = DIRECTION('center_axis',(0.,-1.,-1.07081696047951E-16)) ;
#92825 = DIRECTION('ref_axis',(0.,1.07081696047951E-16,-1.)) ;
#92826 = DIRECTION('center_axis',(0.,-1.,-8.67361737988409E-15)) ;
#92827 = DIRECTION('ref_axis',(0.,8.67361737988409E-15,-1.)) ;
#92828 = DIRECTION('center_axis',(1.,0.,0.)) ;
#92829 = DIRECTION('ref_axis',(0.,0.,-1.)) ;
#92830 = DIRECTION('center_axis',(0.,0.,1.)) ;
#92831 = DIRECTION('ref_axis',(1.,0.,0.)) ;
#92832 = DIRECTION('center_axis',(0.,0.,-1.)) ;
#92833 = DIRECTION('ref_axis',(-1.,0.,0.)) ;
#92834 = DIRECTION('center_axis',(0.,0.,1.)) ;
#92835 = DIRECTION('ref_axis',(1.,0.,0.)) ;
#92836 = DIRECTION('center_axis',(0.,0.,1.)) ;
#92837 = DIRECTION('ref_axis',(1.,0.,0.)) ;
#92838 = DIRECTION('center_axis',(0.,0.,1.)) ;
#92839 = DIRECTION('ref_axis',(1.,0.,0.)) ;
#92840 = DIRECTION('center_axis',(1.,0.,0.)) ;
#92841 = DIRECTION('ref_axis',(0.,0.382683432365087,0.923879532511288)) ;
#92842 = DIRECTION('center_axis',(0.,-0.707106781186548,-0.707106781186548)) ;
#92843 = DIRECTION('ref_axis',(0.,0.707106781186548,-0.707106781186548)) ;
#92844 = DIRECTION('center_axis',(1.,0.,0.)) ;
#92845 = DIRECTION('ref_axis',(0.,0.,-1.)) ;
#92846 = DIRECTION('center_axis',(0.,0.514231796959109,0.857651245551597)) ;
#92847 = DIRECTION('ref_axis',(0.,-0.857651245551597,0.514231796959109)) ;
#92848 = DIRECTION('center_axis',(0.,0.707106781186546,0.707106781186549)) ;
#92849 = DIRECTION('ref_axis',(0.,-0.707106781186549,0.707106781186546)) ;
#92850 = DIRECTION('center_axis',(0.,-0.707106781186548,-0.707106781186548)) ;
#92851 = DIRECTION('ref_axis',(0.,0.707106781186548,-0.707106781186548)) ;
#92852 = DIRECTION('center_axis',(1.,0.,0.)) ;
#92853 = DIRECTION('ref_axis',(0.,0.,-1.)) ;
#92854 = DIRECTION('center_axis',(0.,-0.514231796959109,0.857651245551597)) ;
#92855 = DIRECTION('ref_axis',(0.,-0.857651245551597,-0.514231796959109)) ;
#92856 = DIRECTION('center_axis',(1.,0.,0.)) ;
#92857 = DIRECTION('ref_axis',(0.,0.,-1.)) ;
#92858 = DIRECTION('center_axis',(0.,0.,-1.)) ;
#92859 = DIRECTION('ref_axis',(-1.,0.,0.)) ;
#92860 = DIRECTION('center_axis',(1.,0.,0.)) ;
#92861 = DIRECTION('ref_axis',(0.,0.,-1.)) ;
#92862 = DIRECTION('center_axis',(0.,0.,1.)) ;
#92863 = DIRECTION('ref_axis',(1.,0.,0.)) ;
#92864 = DIRECTION('center_axis',(0.,3.99416362155027E-15,1.)) ;
#92865 = DIRECTION('ref_axis',(0.,-1.,3.99416362155027E-15)) ;
#92866 = DIRECTION('center_axis',(0.,0.,-1.)) ;
#92867 = DIRECTION('ref_axis',(-1.,0.,0.)) ;
#92868 = DIRECTION('center_axis',(0.,0.,1.)) ;
#92869 = DIRECTION('ref_axis',(1.,0.,0.)) ;
#92870 = DIRECTION('center_axis',(0.,0.,1.)) ;
#92871 = DIRECTION('ref_axis',(1.,0.,0.)) ;
#92872 = DIRECTION('center_axis',(0.,1.,0.)) ;
#92873 = DIRECTION('ref_axis',(0.,0.,-1.)) ;
#92874 = DIRECTION('center_axis',(0.,-1.,0.)) ;
#92875 = DIRECTION('ref_axis',(0.,0.,-1.)) ;
#92876 = DIRECTION('center_axis',(1.,0.,0.)) ;
#92877 = DIRECTION('ref_axis',(0.,0.,-1.)) ;
#92878 = DIRECTION('center_axis',(0.,1.,0.)) ;
#92879 = DIRECTION('ref_axis',(0.,0.,1.)) ;
#92880 = DIRECTION('center_axis',(0.,1.,0.)) ;
#92881 = DIRECTION('ref_axis',(0.,0.,1.)) ;
#92882 = DIRECTION('center_axis',(0.,-1.,0.)) ;
#92883 = DIRECTION('ref_axis',(0.,0.,-1.)) ;
#92884 = DIRECTION('center_axis',(0.,1.,1.07081696047951E-16)) ;
#92885 = DIRECTION('ref_axis',(0.,-1.07081696047951E-16,1.)) ;
#92886 = DIRECTION('center_axis',(0.,1.,6.50521303491307E-15)) ;
#92887 = DIRECTION('ref_axis',(0.,-6.50521303491307E-15,1.)) ;
#92888 = DIRECTION('center_axis',(0.,1.,0.)) ;
#92889 = DIRECTION('ref_axis',(0.,0.,-1.)) ;
#92890 = DIRECTION('center_axis',(0.,0.,1.)) ;
#92891 = DIRECTION('ref_axis',(1.,0.,0.)) ;
#92892 = DIRECTION('center_axis',(1.,0.,0.)) ;
#92893 = DIRECTION('ref_axis',(0.,0.,-1.)) ;
#92894 = DIRECTION('center_axis',(0.,0.,-1.)) ;
#92895 = DIRECTION('ref_axis',(-1.,0.,0.)) ;
#92896 = DIRECTION('center_axis',(0.,0.,-1.)) ;
#92897 = DIRECTION('ref_axis',(-1.,0.,0.)) ;
#92898 = DIRECTION('center_axis',(0.,-1.,0.)) ;
#92899 = DIRECTION('ref_axis',(0.,0.,-1.)) ;
#92900 = DIRECTION('center_axis',(0.,1.,0.)) ;
#92901 = DIRECTION('ref_axis',(0.,0.,1.)) ;
#92902 = DIRECTION('center_axis',(0.,-1.,0.)) ;
#92903 = DIRECTION('ref_axis',(0.,0.,-1.)) ;
#92904 = DIRECTION('center_axis',(0.,1.,0.)) ;
#92905 = DIRECTION('ref_axis',(0.,0.,-1.)) ;
#92906 = DIRECTION('center_axis',(0.,0.,-1.)) ;
#92907 = DIRECTION('ref_axis',(-1.,0.,0.)) ;
#92908 = DIRECTION('center_axis',(0.,1.,0.)) ;
#92909 = DIRECTION('ref_axis',(0.,0.,-1.)) ;
#92910 = DIRECTION('center_axis',(0.,0.,-1.)) ;
#92911 = DIRECTION('ref_axis',(-1.,0.,0.)) ;
#92912 = DIRECTION('center_axis',(0.,0.,1.)) ;
#92913 = DIRECTION('ref_axis',(1.,0.,0.)) ;
#92914 = DIRECTION('center_axis',(0.,0.,-1.)) ;
#92915 = DIRECTION('ref_axis',(-1.,0.,0.)) ;
#92916 = DIRECTION('center_axis',(0.,0.,-1.)) ;
#92917 = DIRECTION('ref_axis',(-1.,0.,0.)) ;
#92918 = DIRECTION('center_axis',(0.,0.,-1.)) ;
#92919 = DIRECTION('ref_axis',(-1.,0.,0.)) ;
#92920 = DIRECTION('center_axis',(1.,0.,0.)) ;
#92921 = DIRECTION('ref_axis',(0.,0.,-1.)) ;
#92922 = DIRECTION('center_axis',(0.,0.707106781186548,-0.707106781186548)) ;
#92923 = DIRECTION('ref_axis',(0.,0.707106781186548,0.707106781186548)) ;
#92924 = DIRECTION('center_axis',(1.,0.,0.)) ;
#92925 = DIRECTION('ref_axis',(0.,0.,-1.)) ;
#92926 = DIRECTION('center_axis',(0.,-1.,0.)) ;
#92927 = DIRECTION('ref_axis',(0.,0.,-1.)) ;
#92928 = DIRECTION('center_axis',(0.,-0.707106781186548,0.707106781186547)) ;
#92929 = DIRECTION('ref_axis',(0.,-0.707106781186547,-0.707106781186548)) ;
#92930 = DIRECTION('center_axis',(0.,-1.,-1.07081696047951E-16)) ;
#92931 = DIRECTION('ref_axis',(0.,1.07081696047951E-16,-1.)) ;
#92932 = DIRECTION('center_axis',(0.,-1.,-8.67361737988409E-15)) ;
#92933 = DIRECTION('ref_axis',(0.,8.67361737988409E-15,-1.)) ;
#92934 = DIRECTION('center_axis',(1.,0.,0.)) ;
#92935 = DIRECTION('ref_axis',(0.,0.,-1.)) ;
#92936 = DIRECTION('center_axis',(0.,0.,1.)) ;
#92937 = DIRECTION('ref_axis',(1.,0.,0.)) ;
#92938 = DIRECTION('center_axis',(0.,0.,-1.)) ;
#92939 = DIRECTION('ref_axis',(-1.,0.,0.)) ;
#92940 = DIRECTION('center_axis',(0.,0.,1.)) ;
#92941 = DIRECTION('ref_axis',(1.,0.,0.)) ;
#92942 = DIRECTION('center_axis',(0.,0.,1.)) ;
#92943 = DIRECTION('ref_axis',(1.,0.,0.)) ;
#92944 = DIRECTION('center_axis',(0.,0.,1.)) ;
#92945 = DIRECTION('ref_axis',(1.,0.,0.)) ;
#92946 = DIRECTION('center_axis',(1.,0.,0.)) ;
#92947 = DIRECTION('ref_axis',(0.,0.382683432365088,0.923879532511288)) ;
#92948 = DIRECTION('center_axis',(0.,-0.707106781186548,-0.707106781186548)) ;
#92949 = DIRECTION('ref_axis',(0.,0.707106781186548,-0.707106781186548)) ;
#92950 = DIRECTION('center_axis',(1.,0.,0.)) ;
#92951 = DIRECTION('ref_axis',(0.,0.,-1.)) ;
#92952 = DIRECTION('center_axis',(0.,0.514231796959109,0.857651245551597)) ;
#92953 = DIRECTION('ref_axis',(0.,-0.857651245551597,0.514231796959109)) ;
#92954 = DIRECTION('center_axis',(0.,0.707106781186546,0.707106781186549)) ;
#92955 = DIRECTION('ref_axis',(0.,-0.707106781186549,0.707106781186546)) ;
#92956 = DIRECTION('center_axis',(0.,-0.707106781186548,-0.707106781186548)) ;
#92957 = DIRECTION('ref_axis',(0.,0.707106781186548,-0.707106781186548)) ;
#92958 = DIRECTION('center_axis',(1.,0.,0.)) ;
#92959 = DIRECTION('ref_axis',(0.,0.,-1.)) ;
#92960 = DIRECTION('center_axis',(0.,-0.514231796959101,0.857651245551602)) ;
#92961 = DIRECTION('ref_axis',(0.,-0.857651245551602,-0.514231796959101)) ;
#92962 = DIRECTION('center_axis',(1.,0.,0.)) ;
#92963 = DIRECTION('ref_axis',(0.,0.,-1.)) ;
#92964 = DIRECTION('center_axis',(0.,8.67361737988405E-15,-1.)) ;
#92965 = DIRECTION('ref_axis',(0.,1.,8.67361737988405E-15)) ;
#92966 = DIRECTION('center_axis',(1.,0.,0.)) ;
#92967 = DIRECTION('ref_axis',(0.,0.,-1.)) ;
#92968 = DIRECTION('center_axis',(0.,0.,1.)) ;
#92969 = DIRECTION('ref_axis',(1.,0.,0.)) ;
#92970 = DIRECTION('center_axis',(0.,3.99416362155027E-15,1.)) ;
#92971 = DIRECTION('ref_axis',(0.,-1.,3.99416362155027E-15)) ;
#92972 = DIRECTION('center_axis',(0.,0.,-1.)) ;
#92973 = DIRECTION('ref_axis',(-1.,0.,0.)) ;
#92974 = DIRECTION('center_axis',(0.,0.,1.)) ;
#92975 = DIRECTION('ref_axis',(1.,0.,0.)) ;
#92976 = DIRECTION('center_axis',(0.,0.,1.)) ;
#92977 = DIRECTION('ref_axis',(1.,0.,0.)) ;
#92978 = DIRECTION('center_axis',(0.,1.,0.)) ;
#92979 = DIRECTION('ref_axis',(0.,0.,-1.)) ;
#92980 = DIRECTION('center_axis',(0.,-1.,0.)) ;
#92981 = DIRECTION('ref_axis',(0.,0.,-1.)) ;
#92982 = DIRECTION('center_axis',(1.,0.,0.)) ;
#92983 = DIRECTION('ref_axis',(0.,0.,-1.)) ;
#92984 = DIRECTION('center_axis',(0.,1.,0.)) ;
#92985 = DIRECTION('ref_axis',(0.,0.,1.)) ;
#92986 = DIRECTION('center_axis',(0.,1.,0.)) ;
#92987 = DIRECTION('ref_axis',(0.,0.,1.)) ;
#92988 = DIRECTION('center_axis',(0.,-1.,0.)) ;
#92989 = DIRECTION('ref_axis',(0.,0.,-1.)) ;
#92990 = DIRECTION('center_axis',(0.,1.,1.07081696047951E-16)) ;
#92991 = DIRECTION('ref_axis',(0.,-1.07081696047951E-16,1.)) ;
#92992 = DIRECTION('center_axis',(0.,1.,6.50521303491301E-15)) ;
#92993 = DIRECTION('ref_axis',(0.,-6.50521303491301E-15,1.)) ;
#92994 = DIRECTION('center_axis',(0.,1.,0.)) ;
#92995 = DIRECTION('ref_axis',(0.,0.,-1.)) ;
#92996 = DIRECTION('center_axis',(0.,0.,1.)) ;
#92997 = DIRECTION('ref_axis',(1.,0.,0.)) ;
#92998 = DIRECTION('center_axis',(1.,0.,0.)) ;
#92999 = DIRECTION('ref_axis',(0.,0.,-1.)) ;
#93000 = DIRECTION('center_axis',(0.,0.,-1.)) ;
#93001 = DIRECTION('ref_axis',(-1.,0.,0.)) ;
#93002 = DIRECTION('center_axis',(0.,0.,-1.)) ;
#93003 = DIRECTION('ref_axis',(-1.,0.,0.)) ;
#93004 = DIRECTION('center_axis',(0.,-1.,0.)) ;
#93005 = DIRECTION('ref_axis',(0.,0.,-1.)) ;
#93006 = DIRECTION('center_axis',(0.,1.,0.)) ;
#93007 = DIRECTION('ref_axis',(0.,0.,1.)) ;
#93008 = DIRECTION('center_axis',(0.,-1.,0.)) ;
#93009 = DIRECTION('ref_axis',(0.,0.,-1.)) ;
#93010 = DIRECTION('center_axis',(0.,1.,0.)) ;
#93011 = DIRECTION('ref_axis',(0.,0.,-1.)) ;
#93012 = DIRECTION('center_axis',(0.,0.,-1.)) ;
#93013 = DIRECTION('ref_axis',(-1.,0.,0.)) ;
#93014 = DIRECTION('center_axis',(0.,1.,0.)) ;
#93015 = DIRECTION('ref_axis',(0.,0.,-1.)) ;
#93016 = DIRECTION('center_axis',(0.,0.,-1.)) ;
#93017 = DIRECTION('ref_axis',(-1.,0.,0.)) ;
#93018 = DIRECTION('center_axis',(0.,0.,1.)) ;
#93019 = DIRECTION('ref_axis',(1.,0.,0.)) ;
#93020 = DIRECTION('center_axis',(0.,0.,-1.)) ;
#93021 = DIRECTION('ref_axis',(-1.,0.,0.)) ;
#93022 = DIRECTION('center_axis',(0.,0.,-1.)) ;
#93023 = DIRECTION('ref_axis',(-1.,0.,0.)) ;
#93024 = DIRECTION('center_axis',(0.,8.67361737988405E-15,-1.)) ;
#93025 = DIRECTION('ref_axis',(0.,1.,8.67361737988405E-15)) ;
#93026 = DIRECTION('center_axis',(1.,0.,0.)) ;
#93027 = DIRECTION('ref_axis',(0.,0.,-1.)) ;
#93028 = DIRECTION('center_axis',(0.,0.707106781186548,-0.707106781186548)) ;
#93029 = DIRECTION('ref_axis',(0.,0.707106781186548,0.707106781186548)) ;
#93030 = DIRECTION('center_axis',(1.,0.,0.)) ;
#93031 = DIRECTION('ref_axis',(0.,0.,-1.)) ;
#93032 = DIRECTION('center_axis',(0.,-1.,0.)) ;
#93033 = DIRECTION('ref_axis',(0.,0.,-1.)) ;
#93034 = DIRECTION('center_axis',(0.,-0.707106781186548,0.707106781186547)) ;
#93035 = DIRECTION('ref_axis',(0.,-0.707106781186547,-0.707106781186548)) ;
#93036 = DIRECTION('center_axis',(0.,-1.,-1.07081696047951E-16)) ;
#93037 = DIRECTION('ref_axis',(0.,1.07081696047951E-16,-1.)) ;
#93038 = DIRECTION('center_axis',(0.,-1.,-8.67361737988401E-15)) ;
#93039 = DIRECTION('ref_axis',(0.,8.67361737988401E-15,-1.)) ;
#93040 = DIRECTION('center_axis',(1.,0.,0.)) ;
#93041 = DIRECTION('ref_axis',(0.,0.,-1.)) ;
#93042 = DIRECTION('center_axis',(0.,0.,1.)) ;
#93043 = DIRECTION('ref_axis',(1.,0.,0.)) ;
#93044 = DIRECTION('center_axis',(0.,0.,-1.)) ;
#93045 = DIRECTION('ref_axis',(-1.,0.,0.)) ;
#93046 = DIRECTION('center_axis',(0.,0.,1.)) ;
#93047 = DIRECTION('ref_axis',(1.,0.,0.)) ;
#93048 = DIRECTION('center_axis',(0.,0.,1.)) ;
#93049 = DIRECTION('ref_axis',(1.,0.,0.)) ;
#93050 = DIRECTION('center_axis',(0.,0.,1.)) ;
#93051 = DIRECTION('ref_axis',(1.,0.,0.)) ;
#93052 = DIRECTION('center_axis',(1.,0.,0.)) ;
#93053 = DIRECTION('ref_axis',(0.,0.38268343236509,0.923879532511287)) ;
#93054 = DIRECTION('center_axis',(0.,-0.70710678118655,-0.707106781186545)) ;
#93055 = DIRECTION('ref_axis',(0.,0.707106781186545,-0.70710678118655)) ;
#93056 = DIRECTION('center_axis',(1.,0.,0.)) ;
#93057 = DIRECTION('ref_axis',(0.,0.,-1.)) ;
#93058 = DIRECTION('center_axis',(0.,0.514231796959101,0.857651245551602)) ;
#93059 = DIRECTION('ref_axis',(0.,-0.857651245551602,0.514231796959101)) ;
#93060 = DIRECTION('center_axis',(0.,0.707106781186546,0.707106781186549)) ;
#93061 = DIRECTION('ref_axis',(0.,-0.707106781186549,0.707106781186546)) ;
#93062 = DIRECTION('center_axis',(1.88079096131567E-29,-0.707106781186545,
-0.70710678118655)) ;
#93063 = DIRECTION('ref_axis',(7.62257770433106E-46,0.70710678118655,-0.707106781186545)) ;
#93064 = DIRECTION('center_axis',(1.,0.,0.)) ;
#93065 = DIRECTION('ref_axis',(0.,0.,-1.)) ;
#93066 = DIRECTION('center_axis',(0.,-0.514231796959101,0.857651245551602)) ;
#93067 = DIRECTION('ref_axis',(0.,-0.857651245551602,-0.514231796959101)) ;
#93068 = DIRECTION('center_axis',(1.,0.,0.)) ;
#93069 = DIRECTION('ref_axis',(0.,0.,-1.)) ;
#93070 = DIRECTION('center_axis',(0.,0.,-1.)) ;
#93071 = DIRECTION('ref_axis',(-1.,0.,0.)) ;
#93072 = DIRECTION('center_axis',(1.,0.,0.)) ;
#93073 = DIRECTION('ref_axis',(0.,0.,-1.)) ;
#93074 = DIRECTION('center_axis',(0.,0.,1.)) ;
#93075 = DIRECTION('ref_axis',(1.,0.,0.)) ;
#93076 = DIRECTION('center_axis',(0.,3.99416362155027E-15,1.)) ;
#93077 = DIRECTION('ref_axis',(0.,-1.,3.99416362155027E-15)) ;
#93078 = DIRECTION('center_axis',(0.,-4.33680868994202E-15,-1.)) ;
#93079 = DIRECTION('ref_axis',(0.,1.,-4.33680868994202E-15)) ;
#93080 = DIRECTION('center_axis',(0.,0.,1.)) ;
#93081 = DIRECTION('ref_axis',(1.,0.,0.)) ;
#93082 = DIRECTION('center_axis',(0.,-4.33680868994202E-15,1.)) ;
#93083 = DIRECTION('ref_axis',(0.,-1.,-4.33680868994202E-15)) ;
#93084 = DIRECTION('center_axis',(0.,1.,0.)) ;
#93085 = DIRECTION('ref_axis',(0.,0.,-1.)) ;
#93086 = DIRECTION('center_axis',(0.,-1.,0.)) ;
#93087 = DIRECTION('ref_axis',(0.,0.,-1.)) ;
#93088 = DIRECTION('center_axis',(1.,0.,0.)) ;
#93089 = DIRECTION('ref_axis',(0.,0.,-1.)) ;
#93090 = DIRECTION('center_axis',(0.,1.,0.)) ;
#93091 = DIRECTION('ref_axis',(0.,0.,1.)) ;
#93092 = DIRECTION('center_axis',(0.,1.,0.)) ;
#93093 = DIRECTION('ref_axis',(0.,0.,1.)) ;
#93094 = DIRECTION('center_axis',(0.,-1.,0.)) ;
#93095 = DIRECTION('ref_axis',(0.,0.,-1.)) ;
#93096 = DIRECTION('center_axis',(0.,1.,1.07081696047951E-16)) ;
#93097 = DIRECTION('ref_axis',(0.,-1.07081696047951E-16,1.)) ;
#93098 = DIRECTION('center_axis',(0.,1.,6.50521303491304E-15)) ;
#93099 = DIRECTION('ref_axis',(0.,-6.50521303491304E-15,1.)) ;
#93100 = DIRECTION('center_axis',(0.,1.,0.)) ;
#93101 = DIRECTION('ref_axis',(0.,0.,-1.)) ;
#93102 = DIRECTION('center_axis',(0.,0.,1.)) ;
#93103 = DIRECTION('ref_axis',(1.,0.,0.)) ;
#93104 = DIRECTION('center_axis',(1.,0.,0.)) ;
#93105 = DIRECTION('ref_axis',(0.,0.,-1.)) ;
#93106 = DIRECTION('center_axis',(0.,0.,-1.)) ;
#93107 = DIRECTION('ref_axis',(-1.,0.,0.)) ;
#93108 = DIRECTION('center_axis',(0.,0.,-1.)) ;
#93109 = DIRECTION('ref_axis',(-1.,0.,0.)) ;
#93110 = DIRECTION('center_axis',(1.53063836115601E-16,-1.,-1.30104260698261E-16)) ;
#93111 = DIRECTION('ref_axis',(1.,1.53063836115601E-16,1.99142572374599E-32)) ;
#93112 = DIRECTION('center_axis',(0.,1.,0.)) ;
#93113 = DIRECTION('ref_axis',(0.,0.,1.)) ;
#93114 = DIRECTION('center_axis',(0.,-1.,0.)) ;
#93115 = DIRECTION('ref_axis',(0.,0.,-1.)) ;
#93116 = DIRECTION('center_axis',(1.,1.53063836115601E-16,2.73691106313441E-48)) ;
#93117 = DIRECTION('ref_axis',(-1.53063836115601E-16,1.,-4.18922106430579E-64)) ;
#93118 = DIRECTION('center_axis',(-1.,0.,0.)) ;
#93119 = DIRECTION('ref_axis',(0.,0.,1.)) ;
#93120 = DIRECTION('center_axis',(1.,1.53063836115601E-16,0.)) ;
#93121 = DIRECTION('ref_axis',(1.53063836115601E-16,-1.,0.)) ;
#93122 = DIRECTION('center_axis',(0.,1.,0.)) ;
#93123 = DIRECTION('ref_axis',(1.,0.,0.)) ;
#93124 = DIRECTION('center_axis',(0.,1.,0.)) ;
#93125 = DIRECTION('ref_axis',(0.,0.,-1.)) ;
#93126 = DIRECTION('center_axis',(0.,0.,1.)) ;
#93127 = DIRECTION('ref_axis',(-1.,0.,0.)) ;
#93128 = DIRECTION('center_axis',(0.,1.,0.)) ;
#93129 = DIRECTION('ref_axis',(1.,0.,0.)) ;
#93130 = DIRECTION('center_axis',(0.,0.,1.)) ;
#93131 = DIRECTION('ref_axis',(-1.,0.,0.)) ;
#93132 = DIRECTION('center_axis',(1.,1.0842021724855E-15,0.)) ;
#93133 = DIRECTION('ref_axis',(1.0842021724855E-15,-1.,0.)) ;
#93134 = DIRECTION('center_axis',(-1.,-1.53063836115601E-16,0.)) ;
#93135 = DIRECTION('ref_axis',(0.,-1.,0.)) ;
#93136 = DIRECTION('center_axis',(0.,0.,-1.)) ;
#93137 = DIRECTION('ref_axis',(1.,0.,0.)) ;
#93138 = DIRECTION('center_axis',(0.,0.,-1.)) ;
#93139 = DIRECTION('ref_axis',(0.804034447892619,0.594582716366707,0.)) ;
#93140 = DIRECTION('center_axis',(0.,0.,1.)) ;
#93141 = DIRECTION('ref_axis',(1.,0.,0.)) ;
#93142 = DIRECTION('',(0.,0.,-1.)) ;
#93143 = DIRECTION('center_axis',(-2.16840434497101E-16,1.,1.30104260698261E-16)) ;
#93144 = DIRECTION('ref_axis',(1.,2.16840434497101E-16,1.22464679914735E-16)) ;
#93145 = DIRECTION('',(-2.16840434497101E-16,1.,1.30104260698261E-16)) ;
#93146 = DIRECTION('center_axis',(0.,1.,0.)) ;
#93147 = DIRECTION('ref_axis',(0.,0.,1.)) ;
#93148 = DIRECTION('center_axis',(-1.,-1.53063836115601E-16,-2.73691106313441E-48)) ;
#93149 = DIRECTION('ref_axis',(1.53063836115601E-16,-1.,4.18922106430579E-64)) ;
#93150 = DIRECTION('center_axis',(1.,2.16840434497101E-16,0.)) ;
#93151 = DIRECTION('ref_axis',(2.16840434497101E-16,-1.,0.)) ;
#93152 = DIRECTION('center_axis',(0.,0.,1.)) ;
#93153 = DIRECTION('ref_axis',(1.,0.,0.)) ;
#93154 = DIRECTION('center_axis',(-1.25542992828747E-32,1.020425574104E-16,
1.)) ;
#93155 = DIRECTION('ref_axis',(-1.28107280532009E-48,-1.,1.020425574104E-16)) ;
#93156 = DIRECTION('center_axis',(0.,0.,1.)) ;
#93157 = DIRECTION('ref_axis',(1.,0.,0.)) ;
#93158 = DIRECTION('center_axis',(0.,0.,-1.)) ;
#93159 = DIRECTION('ref_axis',(-1.,0.,0.)) ;
#93160 = DIRECTION('center_axis',(1.,1.53063836115601E-16,-2.73691106313441E-48)) ;
#93161 = DIRECTION('ref_axis',(-1.53063836115601E-16,1.,4.18922106430579E-64)) ;
#93162 = DIRECTION('center_axis',(-1.,0.,0.)) ;
#93163 = DIRECTION('ref_axis',(0.,0.,1.)) ;
#93164 = DIRECTION('center_axis',(1.,1.53063836115601E-16,0.)) ;
#93165 = DIRECTION('ref_axis',(1.53063836115601E-16,-1.,0.)) ;
#93166 = DIRECTION('center_axis',(0.,1.,0.)) ;
#93167 = DIRECTION('ref_axis',(1.,0.,0.)) ;
#93168 = DIRECTION('center_axis',(-1.,-2.16840434497101E-16,0.)) ;
#93169 = DIRECTION('ref_axis',(0.,-1.,0.)) ;
#93170 = DIRECTION('center_axis',(0.,0.,-1.)) ;
#93171 = DIRECTION('ref_axis',(1.,0.,0.)) ;
#93172 = DIRECTION('center_axis',(-1.25542992828747E-32,1.020425574104E-16,
1.)) ;
#93173 = DIRECTION('ref_axis',(0.,-1.,0.)) ;
#93174 = DIRECTION('center_axis',(0.,-1.,0.)) ;
#93175 = DIRECTION('ref_axis',(-6.50521303491301E-15,0.,1.)) ;
#93176 = DIRECTION('center_axis',(-1.,0.,0.)) ;
#93177 = DIRECTION('ref_axis',(0.,0.,-1.)) ;
#93178 = DIRECTION('center_axis',(-1.,-1.53063836115601E-16,0.)) ;
#93179 = DIRECTION('ref_axis',(0.,-1.,0.)) ;
#93180 = DIRECTION('center_axis',(0.,-1.,0.)) ;
#93181 = DIRECTION('ref_axis',(0.,0.,1.)) ;
#93182 = DIRECTION('center_axis',(0.,0.,-1.)) ;
#93183 = DIRECTION('ref_axis',(-1.,0.,0.)) ;
#93184 = DIRECTION('center_axis',(0.,0.,-1.)) ;
#93185 = DIRECTION('ref_axis',(-1.,0.,0.)) ;
#93186 = DIRECTION('center_axis',(1.,1.53063836115601E-16,-3.06472600140763E-33)) ;
#93187 = DIRECTION('ref_axis',(-1.53063836115601E-16,1.,4.69098718418678E-49)) ;
#93188 = DIRECTION('center_axis',(-1.,0.,0.)) ;
#93189 = DIRECTION('ref_axis',(0.,0.,1.)) ;
#93190 = DIRECTION('center_axis',(-1.53063836115601E-16,1.,-1.020425574104E-16)) ;
#93191 = DIRECTION('ref_axis',(-1.,-1.53063836115601E-16,1.3684555315672E-47)) ;
#93192 = DIRECTION('',(1.53063836115601E-16,-1.,1.020425574104E-16)) ;
#93193 = DIRECTION('center_axis',(0.,-1.,0.)) ;
#93194 = DIRECTION('ref_axis',(0.,0.,-1.)) ;
#93195 = DIRECTION('center_axis',(-1.53063836115601E-16,1.,-1.30104260698261E-16)) ;
#93196 = DIRECTION('ref_axis',(-1.,-1.53063836115601E-16,1.99142572374599E-32)) ;
#93197 = DIRECTION('center_axis',(0.,-1.,0.)) ;
#93198 = DIRECTION('ref_axis',(0.,0.,-1.)) ;
#93199 = DIRECTION('center_axis',(-1.,-1.53063836115601E-16,2.73691106313441E-48)) ;
#93200 = DIRECTION('ref_axis',(1.53063836115601E-16,-1.,-4.18922106430579E-64)) ;
#93201 = DIRECTION('center_axis',(1.,2.16840434497101E-16,0.)) ;
#93202 = DIRECTION('ref_axis',(2.16840434497101E-16,-1.,0.)) ;
#93203 = DIRECTION('center_axis',(-1.,0.,2.16840434497102E-15)) ;
#93204 = DIRECTION('ref_axis',(2.16840434497102E-15,0.,1.)) ;
#93205 = DIRECTION('center_axis',(-1.,-2.16840434497101E-16,0.)) ;
#93206 = DIRECTION('ref_axis',(0.,-1.,0.)) ;
#93207 = DIRECTION('center_axis',(0.,0.,1.)) ;
#93208 = DIRECTION('ref_axis',(-1.,0.,0.)) ;
#93209 = DIRECTION('center_axis',(0.,1.,0.)) ;
#93210 = DIRECTION('ref_axis',(1.,0.,0.)) ;
#93211 = DIRECTION('center_axis',(0.,1.,0.)) ;
#93212 = DIRECTION('ref_axis',(0.,0.,-1.)) ;
#93213 = DIRECTION('center_axis',(1.,0.,0.)) ;
#93214 = DIRECTION('ref_axis',(0.,-1.,0.)) ;
#93215 = DIRECTION('center_axis',(1.,6.50521303491304E-15,0.)) ;
#93216 = DIRECTION('ref_axis',(-6.50521303491304E-15,1.,0.)) ;
#93217 = DIRECTION('center_axis',(8.67361737988403E-15,1.,0.)) ;
#93218 = DIRECTION('ref_axis',(-1.,8.67361737988403E-15,0.)) ;
#93219 = DIRECTION('center_axis',(1.2303003375722E-16,-1.,1.020425574104E-16)) ;
#93220 = DIRECTION('ref_axis',(1.,1.2303003375722E-16,-1.25542992828747E-32)) ;
#93221 = DIRECTION('center_axis',(0.,1.,0.)) ;
#93222 = DIRECTION('ref_axis',(0.,0.,1.)) ;
#93223 = DIRECTION('center_axis',(0.,1.,0.)) ;
#93224 = DIRECTION('ref_axis',(1.,0.,0.)) ;
#93225 = DIRECTION('center_axis',(1.,1.2303003375722E-16,0.)) ;
#93226 = DIRECTION('ref_axis',(1.2303003375722E-16,-1.,0.)) ;
#93227 = DIRECTION('center_axis',(0.,0.,1.)) ;
#93228 = DIRECTION('ref_axis',(-1.,0.,0.)) ;
#93229 = DIRECTION('center_axis',(0.,1.,0.)) ;
#93230 = DIRECTION('ref_axis',(1.,0.,0.)) ;
#93231 = DIRECTION('center_axis',(0.,0.,-1.)) ;
#93232 = DIRECTION('ref_axis',(1.,0.,0.)) ;
#93233 = DIRECTION('center_axis',(0.,0.,-1.)) ;
#93234 = DIRECTION('ref_axis',(-1.,0.,0.)) ;
#93235 = DIRECTION('center_axis',(0.,0.,1.)) ;
#93236 = DIRECTION('ref_axis',(1.,0.,0.)) ;
#93237 = DIRECTION('center_axis',(-2.16840434497101E-16,1.,-1.020425574104E-16)) ;
#93238 = DIRECTION('ref_axis',(-1.,-2.16840434497101E-16,5.47382212626882E-48)) ;
#93239 = DIRECTION('center_axis',(0.,1.,0.)) ;
#93240 = DIRECTION('ref_axis',(0.,0.,-1.)) ;
#93241 = DIRECTION('center_axis',(1.,0.,1.25542992828747E-32)) ;
#93242 = DIRECTION('ref_axis',(1.25542992828747E-32,0.,-1.)) ;
#93243 = DIRECTION('center_axis',(1.,0.,0.)) ;
#93244 = DIRECTION('ref_axis',(0.,0.,-1.)) ;
#93245 = DIRECTION('center_axis',(-1.,-1.2303003375722E-16,0.)) ;
#93246 = DIRECTION('ref_axis',(0.,-1.,0.)) ;
#93247 = DIRECTION('center_axis',(0.,0.,-1.)) ;
#93248 = DIRECTION('ref_axis',(1.,0.,0.)) ;
#93249 = DIRECTION('center_axis',(0.,0.,-1.)) ;
#93250 = DIRECTION('ref_axis',(-1.,0.,0.)) ;
#93251 = DIRECTION('',(0.,0.,1.)) ;
#93252 = DIRECTION('center_axis',(0.,0.,1.)) ;
#93253 = DIRECTION('ref_axis',(1.,0.,0.)) ;
#93254 = DIRECTION('center_axis',(0.,0.,1.)) ;
#93255 = DIRECTION('ref_axis',(1.,0.,0.)) ;
#93256 = DIRECTION('center_axis',(6.27714964143733E-33,-5.10212787052002E-17,
-1.)) ;
#93257 = DIRECTION('ref_axis',(3.20268201330022E-49,1.,-5.10212787052002E-17)) ;
#93258 = DIRECTION('center_axis',(1.,1.53063836115601E-16,-1.53236300070382E-33)) ;
#93259 = DIRECTION('ref_axis',(-1.53063836115601E-16,1.,2.34549359209339E-49)) ;
#93260 = DIRECTION('center_axis',(-1.,0.,0.)) ;
#93261 = DIRECTION('ref_axis',(0.,0.,1.)) ;
#93262 = DIRECTION('center_axis',(1.,0.,0.)) ;
#93263 = DIRECTION('ref_axis',(0.,0.,-1.)) ;
#93264 = DIRECTION('center_axis',(0.,1.,0.)) ;
#93265 = DIRECTION('ref_axis',(1.,0.,0.)) ;
#93266 = DIRECTION('center_axis',(-4.33680868994202E-15,1.,0.)) ;
#93267 = DIRECTION('ref_axis',(1.,4.33680868994202E-15,0.)) ;
#93268 = DIRECTION('center_axis',(0.,-1.,0.)) ;
#93269 = DIRECTION('ref_axis',(0.,0.,-1.)) ;
#93270 = DIRECTION('center_axis',(0.,0.,-1.)) ;
#93271 = DIRECTION('ref_axis',(1.,0.,0.)) ;
#93272 = DIRECTION('center_axis',(0.,0.,1.)) ;
#93273 = DIRECTION('ref_axis',(1.,0.,0.)) ;
#93274 = DIRECTION('center_axis',(0.,0.,-1.)) ;
#93275 = DIRECTION('ref_axis',(-1.,0.,0.)) ;
#93276 = DIRECTION('center_axis',(0.,1.,0.)) ;
#93277 = DIRECTION('ref_axis',(1.,0.,0.)) ;
#93278 = DIRECTION('center_axis',(1.,1.2303003375722E-16,0.)) ;
#93279 = DIRECTION('ref_axis',(1.2303003375722E-16,-1.,0.)) ;
#93280 = DIRECTION('center_axis',(0.,1.,0.)) ;
#93281 = DIRECTION('ref_axis',(-6.50521303491307E-15,0.,-1.)) ;
#93282 = DIRECTION('center_axis',(6.27714964143733E-33,-5.10212787052002E-17,
-1.)) ;
#93283 = DIRECTION('ref_axis',(0.,1.,0.)) ;
#93284 = DIRECTION('center_axis',(0.,-1.,0.)) ;
#93285 = DIRECTION('ref_axis',(0.,0.,1.)) ;
#93286 = DIRECTION('center_axis',(2.16840434497101E-16,-1.,5.10212787052002E-17)) ;
#93287 = DIRECTION('ref_axis',(1.,2.16840434497101E-16,-5.47382212626882E-48)) ;
#93288 = DIRECTION('center_axis',(0.,1.,0.)) ;
#93289 = DIRECTION('ref_axis',(0.,0.,-1.)) ;
#93290 = DIRECTION('center_axis',(0.,0.,1.)) ;
#93291 = DIRECTION('ref_axis',(1.,0.,0.)) ;
#93292 = DIRECTION('center_axis',(0.,0.,-1.)) ;
#93293 = DIRECTION('ref_axis',(-1.,0.,0.)) ;
#93294 = DIRECTION('center_axis',(-1.,-1.2303003375722E-16,0.)) ;
#93295 = DIRECTION('ref_axis',(0.,-1.,0.)) ;
#93296 = DIRECTION('center_axis',(0.,-1.,0.)) ;
#93297 = DIRECTION('ref_axis',(0.,0.,1.)) ;
#93298 = DIRECTION('center_axis',(1.53063836115601E-16,-1.,5.10212787052002E-17)) ;
#93299 = DIRECTION('ref_axis',(1.,1.53063836115601E-16,-6.84227765783602E-48)) ;
#93300 = DIRECTION('',(-1.53063836115601E-16,1.,-5.10212787052002E-17)) ;
#93301 = DIRECTION('center_axis',(0.,-1.,0.)) ;
#93302 = DIRECTION('ref_axis',(0.,0.,-1.)) ;
#93303 = DIRECTION('center_axis',(-1.,0.,0.)) ;
#93304 = DIRECTION('ref_axis',(0.,0.,-1.)) ;
#93305 = DIRECTION('center_axis',(-1.2303003375722E-16,1.,-5.10212787052002E-17)) ;
#93306 = DIRECTION('ref_axis',(-1.,-1.2303003375722E-16,6.27714964143733E-33)) ;
#93307 = DIRECTION('center_axis',(-8.67361737988403E-15,-1.,0.)) ;
#93308 = DIRECTION('ref_axis',(1.,-8.67361737988403E-15,0.)) ;
#93309 = DIRECTION('center_axis',(1.,0.,6.27714964143733E-33)) ;
#93310 = DIRECTION('ref_axis',(6.27714964143733E-33,0.,-1.)) ;
#93311 = DIRECTION('center_axis',(-1.,0.,-6.50521303491318E-15)) ;
#93312 = DIRECTION('ref_axis',(-6.50521303491318E-15,0.,1.)) ;
#93313 = DIRECTION('center_axis',(1.,0.,0.)) ;
#93314 = DIRECTION('ref_axis',(0.,1.,0.)) ;
#93315 = DIRECTION('center_axis',(0.,0.,-1.)) ;
#93316 = DIRECTION('ref_axis',(-1.,0.,0.)) ;
#93317 = DIRECTION('center_axis',(0.,0.,1.)) ;
#93318 = DIRECTION('ref_axis',(1.,0.,0.)) ;
#93319 = DIRECTION('center_axis',(0.,0.,-1.)) ;
#93320 = DIRECTION('ref_axis',(-1.,0.,0.)) ;
#93321 = DIRECTION('center_axis',(-1.,0.,0.)) ;
#93322 = DIRECTION('ref_axis',(0.,0.,1.)) ;
#93323 = DIRECTION('center_axis',(0.,-1.,0.)) ;
#93324 = DIRECTION('ref_axis',(0.,0.,-1.)) ;
#93325 = DIRECTION('center_axis',(0.,1.,0.)) ;
#93326 = DIRECTION('ref_axis',(0.,0.,1.)) ;
#93327 = DIRECTION('center_axis',(0.,1.,-6.50521303491307E-15)) ;
#93328 = DIRECTION('ref_axis',(0.,6.50521303491307E-15,1.)) ;
#93329 = DIRECTION('center_axis',(0.,-1.,0.)) ;
#93330 = DIRECTION('ref_axis',(0.,0.,-1.)) ;
#93331 = DIRECTION('center_axis',(0.,-1.,0.)) ;
#93332 = DIRECTION('ref_axis',(0.,0.,-1.)) ;
#93333 = DIRECTION('center_axis',(0.,-1.,-1.07081696047951E-16)) ;
#93334 = DIRECTION('ref_axis',(0.,1.07081696047951E-16,-1.)) ;
#93335 = DIRECTION('center_axis',(0.,1.,0.)) ;
#93336 = DIRECTION('ref_axis',(0.,0.,1.)) ;
#93337 = DIRECTION('center_axis',(-1.,0.,0.)) ;
#93338 = DIRECTION('ref_axis',(0.,0.,1.)) ;
#93339 = DIRECTION('center_axis',(0.,0.,1.)) ;
#93340 = DIRECTION('ref_axis',(1.,0.,0.)) ;
#93341 = DIRECTION('center_axis',(0.,1.,0.)) ;
#93342 = DIRECTION('ref_axis',(0.,0.,1.)) ;
#93343 = DIRECTION('center_axis',(0.,-1.73472347597681E-14,-1.)) ;
#93344 = DIRECTION('ref_axis',(0.,1.,-1.73472347597681E-14)) ;
#93345 = DIRECTION('center_axis',(0.,0.,1.)) ;
#93346 = DIRECTION('ref_axis',(1.,0.,0.)) ;
#93347 = DIRECTION('center_axis',(0.,0.,1.)) ;
#93348 = DIRECTION('ref_axis',(1.,0.,0.)) ;
#93349 = DIRECTION('center_axis',(0.,0.,1.)) ;
#93350 = DIRECTION('ref_axis',(1.,0.,0.)) ;
#93351 = DIRECTION('center_axis',(0.,0.,-1.)) ;
#93352 = DIRECTION('ref_axis',(-1.,0.,0.)) ;
#93353 = DIRECTION('center_axis',(0.,1.,0.)) ;
#93354 = DIRECTION('ref_axis',(0.,0.,1.)) ;
#93355 = DIRECTION('center_axis',(0.,-0.707106781186545,0.70710678118655)) ;
#93356 = DIRECTION('ref_axis',(0.,-0.70710678118655,-0.707106781186545)) ;
#93357 = DIRECTION('center_axis',(0.,1.,0.)) ;
#93358 = DIRECTION('ref_axis',(0.,0.,1.)) ;
#93359 = DIRECTION('center_axis',(0.,-0.514231796959109,-0.857651245551597)) ;
#93360 = DIRECTION('ref_axis',(0.,0.857651245551597,-0.514231796959109)) ;
#93361 = DIRECTION('center_axis',(0.,-0.707106781186548,0.707106781186547)) ;
#93362 = DIRECTION('ref_axis',(0.,-0.707106781186547,-0.707106781186548)) ;
#93363 = DIRECTION('center_axis',(0.,-0.707106781186548,0.707106781186548)) ;
#93364 = DIRECTION('ref_axis',(0.,-0.707106781186548,-0.707106781186548)) ;
#93365 = DIRECTION('center_axis',(-1.,0.,0.)) ;
#93366 = DIRECTION('ref_axis',(0.,0.,1.)) ;
#93367 = DIRECTION('center_axis',(0.,0.514231796959101,-0.857651245551602)) ;
#93368 = DIRECTION('ref_axis',(0.,0.857651245551602,0.514231796959101)) ;
#93369 = DIRECTION('center_axis',(0.,1.,0.)) ;
#93370 = DIRECTION('ref_axis',(0.,0.,1.)) ;
#93371 = DIRECTION('center_axis',(0.,0.,-1.)) ;
#93372 = DIRECTION('ref_axis',(-1.,0.,0.)) ;
#93373 = DIRECTION('center_axis',(0.,1.,0.)) ;
#93374 = DIRECTION('ref_axis',(0.,0.,1.)) ;
#93375 = DIRECTION('center_axis',(0.,0.,-1.)) ;
#93376 = DIRECTION('ref_axis',(-1.,0.,0.)) ;
#93377 = DIRECTION('center_axis',(0.,0.,-1.)) ;
#93378 = DIRECTION('ref_axis',(-1.,0.,0.)) ;
#93379 = DIRECTION('center_axis',(0.,0.,1.)) ;
#93380 = DIRECTION('ref_axis',(1.,0.,0.)) ;
#93381 = DIRECTION('center_axis',(0.,0.,-1.)) ;
#93382 = DIRECTION('ref_axis',(-1.,0.,0.)) ;
#93383 = DIRECTION('center_axis',(0.,1.,0.)) ;
#93384 = DIRECTION('ref_axis',(0.,0.,1.)) ;
#93385 = DIRECTION('center_axis',(0.,-1.,8.67361737988401E-15)) ;
#93386 = DIRECTION('ref_axis',(0.,-8.67361737988401E-15,-1.)) ;
#93387 = DIRECTION('center_axis',(0.,0.707106781186546,0.707106781186549)) ;
#93388 = DIRECTION('ref_axis',(0.,-0.707106781186549,0.707106781186546)) ;
#93389 = DIRECTION('center_axis',(0.,0.707106781186548,0.707106781186548)) ;
#93390 = DIRECTION('ref_axis',(0.,-0.707106781186548,0.707106781186548)) ;
#93391 = DIRECTION('center_axis',(0.,1.,1.07081696047951E-16)) ;
#93392 = DIRECTION('ref_axis',(0.,-1.07081696047951E-16,1.)) ;
#93393 = DIRECTION('center_axis',(0.,-1.,0.)) ;
#93394 = DIRECTION('ref_axis',(0.,0.,-1.)) ;
#93395 = DIRECTION('center_axis',(0.,1.,0.)) ;
#93396 = DIRECTION('ref_axis',(0.,0.,1.)) ;
#93397 = DIRECTION('center_axis',(0.,-8.67361737988409E-15,1.)) ;
#93398 = DIRECTION('ref_axis',(0.,-1.,-8.67361737988409E-15)) ;
#93399 = DIRECTION('center_axis',(0.,1.,0.)) ;
#93400 = DIRECTION('ref_axis',(0.,0.,1.)) ;
#93401 = DIRECTION('center_axis',(0.,8.67361737988403E-15,1.)) ;
#93402 = DIRECTION('ref_axis',(0.,-1.,8.67361737988403E-15)) ;
#93403 = DIRECTION('center_axis',(0.,3.99416362155027E-15,1.)) ;
#93404 = DIRECTION('ref_axis',(0.,-1.,3.99416362155027E-15)) ;
#93405 = DIRECTION('center_axis',(0.,0.,1.)) ;
#93406 = DIRECTION('ref_axis',(1.,0.,0.)) ;
#93407 = DIRECTION('center_axis',(0.,0.,-1.)) ;
#93408 = DIRECTION('ref_axis',(-1.,0.,0.)) ;
#93409 = DIRECTION('center_axis',(0.,0.,1.)) ;
#93410 = DIRECTION('ref_axis',(1.,0.,0.)) ;
#93411 = DIRECTION('center_axis',(-1.,0.,0.)) ;
#93412 = DIRECTION('ref_axis',(0.,0.,1.)) ;
#93413 = DIRECTION('center_axis',(0.,1.,0.)) ;
#93414 = DIRECTION('ref_axis',(0.,0.,1.)) ;
#93415 = DIRECTION('center_axis',(-1.,0.,0.)) ;
#93416 = DIRECTION('ref_axis',(0.,0.,1.)) ;
#93417 = DIRECTION('center_axis',(0.,-1.,0.)) ;
#93418 = DIRECTION('ref_axis',(0.,0.,-1.)) ;
#93419 = DIRECTION('center_axis',(0.,1.,0.)) ;
#93420 = DIRECTION('ref_axis',(0.,0.,1.)) ;
#93421 = DIRECTION('center_axis',(1.53063836115601E-16,-1.,-1.30104260698261E-16)) ;
#93422 = DIRECTION('ref_axis',(1.,1.53063836115601E-16,1.99142572374599E-32)) ;
#93423 = DIRECTION('center_axis',(0.,1.,0.)) ;
#93424 = DIRECTION('ref_axis',(0.,0.,1.)) ;
#93425 = DIRECTION('center_axis',(0.,-1.,0.)) ;
#93426 = DIRECTION('ref_axis',(0.,0.,-1.)) ;
#93427 = DIRECTION('center_axis',(1.,1.53063836115601E-16,2.73691106313441E-48)) ;
#93428 = DIRECTION('ref_axis',(-1.53063836115601E-16,1.,-4.18922106430579E-64)) ;
#93429 = DIRECTION('center_axis',(-1.,0.,0.)) ;
#93430 = DIRECTION('ref_axis',(0.,0.,1.)) ;
#93431 = DIRECTION('center_axis',(1.,1.53063836115601E-16,0.)) ;
#93432 = DIRECTION('ref_axis',(1.53063836115601E-16,-1.,0.)) ;
#93433 = DIRECTION('center_axis',(0.,1.,0.)) ;
#93434 = DIRECTION('ref_axis',(1.,0.,0.)) ;
#93435 = DIRECTION('center_axis',(0.,1.,0.)) ;
#93436 = DIRECTION('ref_axis',(0.,0.,-1.)) ;
#93437 = DIRECTION('center_axis',(0.,0.,1.)) ;
#93438 = DIRECTION('ref_axis',(-1.,0.,0.)) ;
#93439 = DIRECTION('center_axis',(0.,1.,0.)) ;
#93440 = DIRECTION('ref_axis',(1.,0.,0.)) ;
#93441 = DIRECTION('center_axis',(0.,0.,1.)) ;
#93442 = DIRECTION('ref_axis',(-1.,0.,0.)) ;
#93443 = DIRECTION('center_axis',(1.,1.0842021724855E-15,0.)) ;
#93444 = DIRECTION('ref_axis',(1.0842021724855E-15,-1.,0.)) ;
#93445 = DIRECTION('center_axis',(-1.,-1.53063836115601E-16,0.)) ;
#93446 = DIRECTION('ref_axis',(0.,-1.,0.)) ;
#93447 = DIRECTION('center_axis',(0.,0.,-1.)) ;
#93448 = DIRECTION('ref_axis',(1.,0.,0.)) ;
#93449 = DIRECTION('center_axis',(0.,0.,-1.)) ;
#93450 = DIRECTION('ref_axis',(0.804034447892625,0.594582716366698,0.)) ;
#93451 = DIRECTION('center_axis',(0.,0.,1.)) ;
#93452 = DIRECTION('ref_axis',(1.,0.,0.)) ;
#93453 = DIRECTION('',(0.,0.,-1.)) ;
#93454 = DIRECTION('center_axis',(-2.16840434497101E-16,1.,1.30104260698261E-16)) ;
#93455 = DIRECTION('ref_axis',(1.,2.16840434497101E-16,1.22464679914735E-16)) ;
#93456 = DIRECTION('',(-2.16840434497101E-16,1.,1.30104260698261E-16)) ;
#93457 = DIRECTION('center_axis',(0.,1.,0.)) ;
#93458 = DIRECTION('ref_axis',(0.,0.,1.)) ;
#93459 = DIRECTION('center_axis',(-1.,-1.53063836115601E-16,-2.73691106313441E-48)) ;
#93460 = DIRECTION('ref_axis',(1.53063836115601E-16,-1.,4.18922106430579E-64)) ;
#93461 = DIRECTION('center_axis',(1.,2.16840434497101E-16,0.)) ;
#93462 = DIRECTION('ref_axis',(2.16840434497101E-16,-1.,0.)) ;
#93463 = DIRECTION('center_axis',(0.,0.,1.)) ;
#93464 = DIRECTION('ref_axis',(1.,0.,0.)) ;
#93465 = DIRECTION('center_axis',(-1.25542992828747E-32,1.020425574104E-16,
1.)) ;
#93466 = DIRECTION('ref_axis',(-1.28107280532009E-48,-1.,1.020425574104E-16)) ;
#93467 = DIRECTION('center_axis',(0.,0.,1.)) ;
#93468 = DIRECTION('ref_axis',(1.,0.,0.)) ;
#93469 = DIRECTION('center_axis',(0.,0.,-1.)) ;
#93470 = DIRECTION('ref_axis',(-1.,0.,0.)) ;
#93471 = DIRECTION('center_axis',(1.,1.53063836115601E-16,-2.73691106313441E-48)) ;
#93472 = DIRECTION('ref_axis',(-1.53063836115601E-16,1.,4.18922106430579E-64)) ;
#93473 = DIRECTION('center_axis',(-1.,0.,0.)) ;
#93474 = DIRECTION('ref_axis',(0.,0.,1.)) ;
#93475 = DIRECTION('center_axis',(1.,1.53063836115601E-16,0.)) ;
#93476 = DIRECTION('ref_axis',(1.53063836115601E-16,-1.,0.)) ;
#93477 = DIRECTION('center_axis',(0.,1.,0.)) ;
#93478 = DIRECTION('ref_axis',(1.,0.,0.)) ;
#93479 = DIRECTION('center_axis',(-1.,-2.16840434497101E-16,0.)) ;
#93480 = DIRECTION('ref_axis',(0.,-1.,0.)) ;
#93481 = DIRECTION('center_axis',(0.,0.,-1.)) ;
#93482 = DIRECTION('ref_axis',(1.,0.,0.)) ;
#93483 = DIRECTION('center_axis',(-1.25542992828747E-32,1.020425574104E-16,
1.)) ;
#93484 = DIRECTION('ref_axis',(0.,-1.,0.)) ;
#93485 = DIRECTION('center_axis',(0.,-1.,0.)) ;
#93486 = DIRECTION('ref_axis',(-6.50521303491307E-15,0.,1.)) ;
#93487 = DIRECTION('center_axis',(-1.,0.,0.)) ;
#93488 = DIRECTION('ref_axis',(0.,0.,-1.)) ;
#93489 = DIRECTION('center_axis',(-1.,-1.53063836115601E-16,0.)) ;
#93490 = DIRECTION('ref_axis',(0.,-1.,0.)) ;
#93491 = DIRECTION('center_axis',(0.,-1.,0.)) ;
#93492 = DIRECTION('ref_axis',(0.,0.,1.)) ;
#93493 = DIRECTION('center_axis',(0.,0.,-1.)) ;
#93494 = DIRECTION('ref_axis',(-1.,0.,0.)) ;
#93495 = DIRECTION('center_axis',(0.,0.,-1.)) ;
#93496 = DIRECTION('ref_axis',(-1.,0.,0.)) ;
#93497 = DIRECTION('center_axis',(1.,1.53063836115601E-16,-3.06472600140763E-33)) ;
#93498 = DIRECTION('ref_axis',(-1.53063836115601E-16,1.,4.69098718418678E-49)) ;
#93499 = DIRECTION('center_axis',(-1.,0.,0.)) ;
#93500 = DIRECTION('ref_axis',(0.,0.,1.)) ;
#93501 = DIRECTION('center_axis',(-1.53063836115601E-16,1.,-1.020425574104E-16)) ;
#93502 = DIRECTION('ref_axis',(-1.,-1.53063836115601E-16,1.3684555315672E-47)) ;
#93503 = DIRECTION('',(1.53063836115601E-16,-1.,1.020425574104E-16)) ;
#93504 = DIRECTION('center_axis',(0.,-1.,0.)) ;
#93505 = DIRECTION('ref_axis',(0.,0.,-1.)) ;
#93506 = DIRECTION('center_axis',(-1.53063836115601E-16,1.,-1.30104260698261E-16)) ;
#93507 = DIRECTION('ref_axis',(-1.,-1.53063836115601E-16,1.99142572374599E-32)) ;
#93508 = DIRECTION('center_axis',(0.,-1.,0.)) ;
#93509 = DIRECTION('ref_axis',(0.,0.,-1.)) ;
#93510 = DIRECTION('center_axis',(-1.,-1.53063836115601E-16,2.73691106313441E-48)) ;
#93511 = DIRECTION('ref_axis',(1.53063836115601E-16,-1.,-4.18922106430579E-64)) ;
#93512 = DIRECTION('center_axis',(1.,2.16840434497101E-16,0.)) ;
#93513 = DIRECTION('ref_axis',(2.16840434497101E-16,-1.,0.)) ;
#93514 = DIRECTION('center_axis',(-1.,0.,2.16840434497102E-15)) ;
#93515 = DIRECTION('ref_axis',(2.16840434497102E-15,0.,1.)) ;
#93516 = DIRECTION('center_axis',(-1.,-2.16840434497101E-16,0.)) ;
#93517 = DIRECTION('ref_axis',(0.,-1.,0.)) ;
#93518 = DIRECTION('center_axis',(0.,0.,1.)) ;
#93519 = DIRECTION('ref_axis',(-1.,0.,0.)) ;
#93520 = DIRECTION('center_axis',(0.,1.,0.)) ;
#93521 = DIRECTION('ref_axis',(1.,0.,0.)) ;
#93522 = DIRECTION('center_axis',(0.,1.,0.)) ;
#93523 = DIRECTION('ref_axis',(0.,0.,-1.)) ;
#93524 = DIRECTION('center_axis',(1.,0.,0.)) ;
#93525 = DIRECTION('ref_axis',(0.,-1.,0.)) ;
#93526 = DIRECTION('center_axis',(1.,6.50521303491304E-15,0.)) ;
#93527 = DIRECTION('ref_axis',(-6.50521303491304E-15,1.,0.)) ;
#93528 = DIRECTION('center_axis',(8.67361737988403E-15,1.,0.)) ;
#93529 = DIRECTION('ref_axis',(-1.,8.67361737988403E-15,0.)) ;
#93530 = DIRECTION('center_axis',(1.2303003375722E-16,-1.,1.020425574104E-16)) ;
#93531 = DIRECTION('ref_axis',(1.,1.2303003375722E-16,-1.25542992828747E-32)) ;
#93532 = DIRECTION('center_axis',(0.,1.,0.)) ;
#93533 = DIRECTION('ref_axis',(0.,0.,1.)) ;
#93534 = DIRECTION('center_axis',(0.,1.,0.)) ;
#93535 = DIRECTION('ref_axis',(1.,0.,0.)) ;
#93536 = DIRECTION('center_axis',(1.,1.2303003375722E-16,0.)) ;
#93537 = DIRECTION('ref_axis',(1.2303003375722E-16,-1.,0.)) ;
#93538 = DIRECTION('center_axis',(0.,0.,1.)) ;
#93539 = DIRECTION('ref_axis',(-1.,0.,0.)) ;
#93540 = DIRECTION('center_axis',(0.,1.,0.)) ;
#93541 = DIRECTION('ref_axis',(1.,0.,0.)) ;
#93542 = DIRECTION('center_axis',(0.,0.,-1.)) ;
#93543 = DIRECTION('ref_axis',(1.,0.,0.)) ;
#93544 = DIRECTION('center_axis',(0.,0.,-1.)) ;
#93545 = DIRECTION('ref_axis',(-1.,0.,0.)) ;
#93546 = DIRECTION('center_axis',(0.,0.,1.)) ;
#93547 = DIRECTION('ref_axis',(1.,0.,0.)) ;
#93548 = DIRECTION('center_axis',(-2.16840434497101E-16,1.,-1.020425574104E-16)) ;
#93549 = DIRECTION('ref_axis',(-1.,-2.16840434497101E-16,5.47382212626882E-48)) ;
#93550 = DIRECTION('center_axis',(0.,1.,0.)) ;
#93551 = DIRECTION('ref_axis',(0.,0.,-1.)) ;
#93552 = DIRECTION('center_axis',(1.,0.,1.25542992828747E-32)) ;
#93553 = DIRECTION('ref_axis',(1.25542992828747E-32,0.,-1.)) ;
#93554 = DIRECTION('center_axis',(1.,0.,0.)) ;
#93555 = DIRECTION('ref_axis',(0.,0.,-1.)) ;
#93556 = DIRECTION('center_axis',(-1.,-1.2303003375722E-16,0.)) ;
#93557 = DIRECTION('ref_axis',(0.,-1.,0.)) ;
#93558 = DIRECTION('center_axis',(0.,0.,-1.)) ;
#93559 = DIRECTION('ref_axis',(1.,0.,0.)) ;
#93560 = DIRECTION('center_axis',(0.,0.,-1.)) ;
#93561 = DIRECTION('ref_axis',(-1.,0.,0.)) ;
#93562 = DIRECTION('',(0.,0.,1.)) ;
#93563 = DIRECTION('center_axis',(0.,0.,1.)) ;
#93564 = DIRECTION('ref_axis',(1.,0.,0.)) ;
#93565 = DIRECTION('center_axis',(0.,0.,1.)) ;
#93566 = DIRECTION('ref_axis',(1.,0.,0.)) ;
#93567 = DIRECTION('center_axis',(6.27714964143733E-33,-5.10212787052002E-17,
-1.)) ;
#93568 = DIRECTION('ref_axis',(3.20268201330022E-49,1.,-5.10212787052002E-17)) ;
#93569 = DIRECTION('center_axis',(1.,1.53063836115601E-16,-1.53236300070382E-33)) ;
#93570 = DIRECTION('ref_axis',(-1.53063836115601E-16,1.,2.34549359209339E-49)) ;
#93571 = DIRECTION('center_axis',(-1.,0.,0.)) ;
#93572 = DIRECTION('ref_axis',(0.,0.,1.)) ;
#93573 = DIRECTION('center_axis',(1.,0.,0.)) ;
#93574 = DIRECTION('ref_axis',(0.,0.,-1.)) ;
#93575 = DIRECTION('center_axis',(0.,1.,0.)) ;
#93576 = DIRECTION('ref_axis',(1.,0.,0.)) ;
#93577 = DIRECTION('center_axis',(-4.33680868994202E-15,1.,0.)) ;
#93578 = DIRECTION('ref_axis',(1.,4.33680868994202E-15,0.)) ;
#93579 = DIRECTION('center_axis',(0.,-1.,0.)) ;
#93580 = DIRECTION('ref_axis',(0.,0.,-1.)) ;
#93581 = DIRECTION('center_axis',(0.,0.,-1.)) ;
#93582 = DIRECTION('ref_axis',(1.,0.,0.)) ;
#93583 = DIRECTION('center_axis',(0.,0.,1.)) ;
#93584 = DIRECTION('ref_axis',(1.,0.,0.)) ;
#93585 = DIRECTION('center_axis',(0.,0.,-1.)) ;
#93586 = DIRECTION('ref_axis',(-1.,0.,0.)) ;
#93587 = DIRECTION('center_axis',(0.,1.,0.)) ;
#93588 = DIRECTION('ref_axis',(1.,0.,0.)) ;
#93589 = DIRECTION('center_axis',(1.,1.2303003375722E-16,0.)) ;
#93590 = DIRECTION('ref_axis',(1.2303003375722E-16,-1.,0.)) ;
#93591 = DIRECTION('center_axis',(0.,1.,0.)) ;
#93592 = DIRECTION('ref_axis',(-6.50521303491307E-15,0.,-1.)) ;
#93593 = DIRECTION('center_axis',(6.27714964143733E-33,-5.10212787052002E-17,
-1.)) ;
#93594 = DIRECTION('ref_axis',(0.,1.,0.)) ;
#93595 = DIRECTION('center_axis',(0.,-1.,0.)) ;
#93596 = DIRECTION('ref_axis',(0.,0.,1.)) ;
#93597 = DIRECTION('center_axis',(2.16840434497101E-16,-1.,5.10212787052002E-17)) ;
#93598 = DIRECTION('ref_axis',(1.,2.16840434497101E-16,-5.47382212626882E-48)) ;
#93599 = DIRECTION('center_axis',(0.,1.,0.)) ;
#93600 = DIRECTION('ref_axis',(0.,0.,-1.)) ;
#93601 = DIRECTION('center_axis',(0.,0.,1.)) ;
#93602 = DIRECTION('ref_axis',(1.,0.,0.)) ;
#93603 = DIRECTION('center_axis',(0.,0.,-1.)) ;
#93604 = DIRECTION('ref_axis',(-1.,0.,0.)) ;
#93605 = DIRECTION('center_axis',(-1.,-1.2303003375722E-16,0.)) ;
#93606 = DIRECTION('ref_axis',(0.,-1.,0.)) ;
#93607 = DIRECTION('center_axis',(0.,-1.,0.)) ;
#93608 = DIRECTION('ref_axis',(0.,0.,1.)) ;
#93609 = DIRECTION('center_axis',(1.53063836115601E-16,-1.,5.10212787052002E-17)) ;
#93610 = DIRECTION('ref_axis',(1.,1.53063836115601E-16,-6.84227765783602E-48)) ;
#93611 = DIRECTION('',(-1.53063836115601E-16,1.,-5.10212787052002E-17)) ;
#93612 = DIRECTION('center_axis',(0.,-1.,0.)) ;
#93613 = DIRECTION('ref_axis',(0.,0.,-1.)) ;
#93614 = DIRECTION('center_axis',(-1.,0.,0.)) ;
#93615 = DIRECTION('ref_axis',(0.,0.,-1.)) ;
#93616 = DIRECTION('center_axis',(-1.2303003375722E-16,1.,-5.10212787052002E-17)) ;
#93617 = DIRECTION('ref_axis',(-1.,-1.2303003375722E-16,6.27714964143733E-33)) ;
#93618 = DIRECTION('center_axis',(-8.67361737988403E-15,-1.,0.)) ;
#93619 = DIRECTION('ref_axis',(1.,-8.67361737988403E-15,0.)) ;
#93620 = DIRECTION('center_axis',(1.,0.,6.27714964143733E-33)) ;
#93621 = DIRECTION('ref_axis',(6.27714964143733E-33,0.,-1.)) ;
#93622 = DIRECTION('center_axis',(-1.,0.,-6.50521303491307E-15)) ;
#93623 = DIRECTION('ref_axis',(-6.50521303491307E-15,0.,1.)) ;
#93624 = DIRECTION('center_axis',(1.,0.,0.)) ;
#93625 = DIRECTION('ref_axis',(0.,1.,0.)) ;
#93626 = DIRECTION('center_axis',(0.,0.,-1.)) ;
#93627 = DIRECTION('ref_axis',(-1.,0.,0.)) ;
#93628 = DIRECTION('center_axis',(0.,0.,1.)) ;
#93629 = DIRECTION('ref_axis',(1.,0.,0.)) ;
#93630 = DIRECTION('center_axis',(0.,0.,-1.)) ;
#93631 = DIRECTION('ref_axis',(-1.,0.,0.)) ;
#93632 = DIRECTION('center_axis',(-1.,0.,0.)) ;
#93633 = DIRECTION('ref_axis',(0.,0.,1.)) ;
#93634 = DIRECTION('center_axis',(0.,-1.,0.)) ;
#93635 = DIRECTION('ref_axis',(0.,0.,-1.)) ;
#93636 = DIRECTION('center_axis',(0.,1.,0.)) ;
#93637 = DIRECTION('ref_axis',(0.,0.,1.)) ;
#93638 = DIRECTION('center_axis',(0.,1.,-6.50521303491307E-15)) ;
#93639 = DIRECTION('ref_axis',(0.,6.50521303491307E-15,1.)) ;
#93640 = DIRECTION('center_axis',(0.,-1.,0.)) ;
#93641 = DIRECTION('ref_axis',(0.,0.,-1.)) ;
#93642 = DIRECTION('center_axis',(0.,-1.,0.)) ;
#93643 = DIRECTION('ref_axis',(0.,0.,-1.)) ;
#93644 = DIRECTION('center_axis',(0.,-1.,-1.07081696047951E-16)) ;
#93645 = DIRECTION('ref_axis',(0.,1.07081696047951E-16,-1.)) ;
#93646 = DIRECTION('center_axis',(0.,1.,0.)) ;
#93647 = DIRECTION('ref_axis',(0.,0.,1.)) ;
#93648 = DIRECTION('center_axis',(-1.,0.,0.)) ;
#93649 = DIRECTION('ref_axis',(0.,0.,1.)) ;
#93650 = DIRECTION('center_axis',(0.,0.,1.)) ;
#93651 = DIRECTION('ref_axis',(1.,0.,0.)) ;
#93652 = DIRECTION('center_axis',(0.,1.,0.)) ;
#93653 = DIRECTION('ref_axis',(0.,0.,1.)) ;
#93654 = DIRECTION('center_axis',(0.,-1.73472347597681E-14,-1.)) ;
#93655 = DIRECTION('ref_axis',(0.,1.,-1.73472347597681E-14)) ;
#93656 = DIRECTION('center_axis',(0.,0.,1.)) ;
#93657 = DIRECTION('ref_axis',(1.,0.,0.)) ;
#93658 = DIRECTION('center_axis',(0.,0.,1.)) ;
#93659 = DIRECTION('ref_axis',(1.,0.,0.)) ;
#93660 = DIRECTION('center_axis',(0.,0.,1.)) ;
#93661 = DIRECTION('ref_axis',(1.,0.,0.)) ;
#93662 = DIRECTION('center_axis',(0.,0.,-1.)) ;
#93663 = DIRECTION('ref_axis',(-1.,0.,0.)) ;
#93664 = DIRECTION('center_axis',(0.,1.,0.)) ;
#93665 = DIRECTION('ref_axis',(0.,0.,1.)) ;
#93666 = DIRECTION('center_axis',(0.,-0.707106781186545,0.70710678118655)) ;
#93667 = DIRECTION('ref_axis',(0.,-0.70710678118655,-0.707106781186545)) ;
#93668 = DIRECTION('center_axis',(0.,1.,0.)) ;
#93669 = DIRECTION('ref_axis',(0.,0.,1.)) ;
#93670 = DIRECTION('center_axis',(0.,-0.514231796959109,-0.857651245551597)) ;
#93671 = DIRECTION('ref_axis',(0.,0.857651245551597,-0.514231796959109)) ;
#93672 = DIRECTION('center_axis',(0.,-0.707106781186548,0.707106781186547)) ;
#93673 = DIRECTION('ref_axis',(0.,-0.707106781186547,-0.707106781186548)) ;
#93674 = DIRECTION('center_axis',(0.,-0.707106781186548,0.707106781186548)) ;
#93675 = DIRECTION('ref_axis',(0.,-0.707106781186548,-0.707106781186548)) ;
#93676 = DIRECTION('center_axis',(-1.,0.,0.)) ;
#93677 = DIRECTION('ref_axis',(0.,0.,1.)) ;
#93678 = DIRECTION('center_axis',(-2.23012492569676E-15,0.514231796959107,
-0.857651245551598)) ;
#93679 = DIRECTION('ref_axis',(-5.69910941180089E-30,0.857651245551598,0.514231796959107)) ;
#93680 = DIRECTION('center_axis',(0.,1.,0.)) ;
#93681 = DIRECTION('ref_axis',(0.,0.,1.)) ;
#93682 = DIRECTION('center_axis',(0.,0.,-1.)) ;
#93683 = DIRECTION('ref_axis',(-1.,0.,0.)) ;
#93684 = DIRECTION('center_axis',(0.,1.,0.)) ;
#93685 = DIRECTION('ref_axis',(0.,0.,1.)) ;
#93686 = DIRECTION('center_axis',(0.,0.,-1.)) ;
#93687 = DIRECTION('ref_axis',(-1.,0.,0.)) ;
#93688 = DIRECTION('center_axis',(0.,0.,-1.)) ;
#93689 = DIRECTION('ref_axis',(-1.,0.,0.)) ;
#93690 = DIRECTION('center_axis',(0.,0.,1.)) ;
#93691 = DIRECTION('ref_axis',(1.,0.,0.)) ;
#93692 = DIRECTION('center_axis',(0.,0.,-1.)) ;
#93693 = DIRECTION('ref_axis',(-1.,0.,0.)) ;
#93694 = DIRECTION('center_axis',(0.,1.,0.)) ;
#93695 = DIRECTION('ref_axis',(0.,0.,1.)) ;
#93696 = DIRECTION('center_axis',(0.,-1.,8.67361737988409E-15)) ;
#93697 = DIRECTION('ref_axis',(0.,-8.67361737988409E-15,-1.)) ;
#93698 = DIRECTION('center_axis',(0.,0.707106781186546,0.707106781186549)) ;
#93699 = DIRECTION('ref_axis',(0.,-0.707106781186549,0.707106781186546)) ;
#93700 = DIRECTION('center_axis',(0.,0.707106781186541,0.707106781186554)) ;
#93701 = DIRECTION('ref_axis',(0.,-0.707106781186554,0.707106781186541)) ;
#93702 = DIRECTION('center_axis',(0.,1.,1.07081696047951E-16)) ;
#93703 = DIRECTION('ref_axis',(0.,-1.07081696047951E-16,1.)) ;
#93704 = DIRECTION('center_axis',(0.,-1.,0.)) ;
#93705 = DIRECTION('ref_axis',(0.,0.,-1.)) ;
#93706 = DIRECTION('center_axis',(0.,1.,0.)) ;
#93707 = DIRECTION('ref_axis',(0.,0.,1.)) ;
#93708 = DIRECTION('center_axis',(0.,0.,1.)) ;
#93709 = DIRECTION('ref_axis',(1.,0.,0.)) ;
#93710 = DIRECTION('center_axis',(0.,1.,0.)) ;
#93711 = DIRECTION('ref_axis',(0.,0.,1.)) ;
#93712 = DIRECTION('center_axis',(0.,0.,1.)) ;
#93713 = DIRECTION('ref_axis',(1.,0.,0.)) ;
#93714 = DIRECTION('center_axis',(0.,3.99416362155027E-15,1.)) ;
#93715 = DIRECTION('ref_axis',(0.,-1.,3.99416362155027E-15)) ;
#93716 = DIRECTION('center_axis',(0.,0.,1.)) ;
#93717 = DIRECTION('ref_axis',(1.,0.,0.)) ;
#93718 = DIRECTION('center_axis',(0.,0.,-1.)) ;
#93719 = DIRECTION('ref_axis',(-1.,0.,0.)) ;
#93720 = DIRECTION('center_axis',(0.,0.,1.)) ;
#93721 = DIRECTION('ref_axis',(1.,0.,0.)) ;
#93722 = DIRECTION('center_axis',(-1.,0.,0.)) ;
#93723 = DIRECTION('ref_axis',(0.,0.,1.)) ;
#93724 = DIRECTION('center_axis',(0.,1.,0.)) ;
#93725 = DIRECTION('ref_axis',(0.,0.,1.)) ;
#93726 = DIRECTION('center_axis',(-1.,0.,0.)) ;
#93727 = DIRECTION('ref_axis',(0.,0.,1.)) ;
#93728 = DIRECTION('center_axis',(0.,-1.,0.)) ;
#93729 = DIRECTION('ref_axis',(0.,0.,-1.)) ;
#93730 = DIRECTION('center_axis',(0.,1.,0.)) ;
#93731 = DIRECTION('ref_axis',(0.,0.,1.)) ;
#93732 = DIRECTION('center_axis',(1.53063836115601E-16,-1.,-1.30104260698261E-16)) ;
#93733 = DIRECTION('ref_axis',(1.,1.53063836115601E-16,1.99142572374599E-32)) ;
#93734 = DIRECTION('center_axis',(0.,1.,0.)) ;
#93735 = DIRECTION('ref_axis',(0.,0.,1.)) ;
#93736 = DIRECTION('center_axis',(0.,-1.,0.)) ;
#93737 = DIRECTION('ref_axis',(0.,0.,-1.)) ;
#93738 = DIRECTION('center_axis',(1.,1.53063836115601E-16,2.73691106313441E-48)) ;
#93739 = DIRECTION('ref_axis',(-1.53063836115601E-16,1.,-4.18922106430579E-64)) ;
#93740 = DIRECTION('center_axis',(-1.,0.,0.)) ;
#93741 = DIRECTION('ref_axis',(0.,0.,1.)) ;
#93742 = DIRECTION('center_axis',(1.,1.53063836115601E-16,0.)) ;
#93743 = DIRECTION('ref_axis',(1.53063836115601E-16,-1.,0.)) ;
#93744 = DIRECTION('center_axis',(0.,1.,0.)) ;
#93745 = DIRECTION('ref_axis',(1.,0.,0.)) ;
#93746 = DIRECTION('center_axis',(0.,1.,0.)) ;
#93747 = DIRECTION('ref_axis',(0.,0.,-1.)) ;
#93748 = DIRECTION('center_axis',(0.,0.,1.)) ;
#93749 = DIRECTION('ref_axis',(-1.,0.,0.)) ;
#93750 = DIRECTION('center_axis',(0.,1.,0.)) ;
#93751 = DIRECTION('ref_axis',(1.,0.,0.)) ;
#93752 = DIRECTION('center_axis',(0.,0.,1.)) ;
#93753 = DIRECTION('ref_axis',(-1.,0.,0.)) ;
#93754 = DIRECTION('center_axis',(1.,1.0842021724855E-15,0.)) ;
#93755 = DIRECTION('ref_axis',(1.0842021724855E-15,-1.,0.)) ;
#93756 = DIRECTION('center_axis',(-1.,-1.53063836115601E-16,0.)) ;
#93757 = DIRECTION('ref_axis',(0.,-1.,0.)) ;
#93758 = DIRECTION('center_axis',(0.,0.,-1.)) ;
#93759 = DIRECTION('ref_axis',(1.,0.,0.)) ;
#93760 = DIRECTION('center_axis',(0.,0.,-1.)) ;
#93761 = DIRECTION('ref_axis',(0.804034447892618,0.594582716366708,0.)) ;
#93762 = DIRECTION('center_axis',(0.,0.,1.)) ;
#93763 = DIRECTION('ref_axis',(1.,0.,0.)) ;
#93764 = DIRECTION('',(0.,0.,-1.)) ;
#93765 = DIRECTION('center_axis',(-2.16840434497101E-16,1.,1.30104260698261E-16)) ;
#93766 = DIRECTION('ref_axis',(1.,2.16840434497101E-16,1.22464679914735E-16)) ;
#93767 = DIRECTION('',(-2.16840434497101E-16,1.,1.30104260698261E-16)) ;
#93768 = DIRECTION('center_axis',(0.,1.,0.)) ;
#93769 = DIRECTION('ref_axis',(0.,0.,1.)) ;
#93770 = DIRECTION('center_axis',(-1.,-1.53063836115601E-16,-2.73691106313441E-48)) ;
#93771 = DIRECTION('ref_axis',(1.53063836115601E-16,-1.,4.18922106430579E-64)) ;
#93772 = DIRECTION('center_axis',(1.,2.16840434497101E-16,0.)) ;
#93773 = DIRECTION('ref_axis',(2.16840434497101E-16,-1.,0.)) ;
#93774 = DIRECTION('center_axis',(0.,0.,1.)) ;
#93775 = DIRECTION('ref_axis',(1.,0.,0.)) ;
#93776 = DIRECTION('center_axis',(-1.25542992828747E-32,1.020425574104E-16,
1.)) ;
#93777 = DIRECTION('ref_axis',(-1.28107280532009E-48,-1.,1.020425574104E-16)) ;
#93778 = DIRECTION('center_axis',(0.,0.,1.)) ;
#93779 = DIRECTION('ref_axis',(1.,0.,0.)) ;
#93780 = DIRECTION('center_axis',(0.,0.,-1.)) ;
#93781 = DIRECTION('ref_axis',(-1.,0.,0.)) ;
#93782 = DIRECTION('center_axis',(1.,1.53063836115601E-16,-2.73691106313441E-48)) ;
#93783 = DIRECTION('ref_axis',(-1.53063836115601E-16,1.,4.18922106430579E-64)) ;
#93784 = DIRECTION('center_axis',(-1.,0.,0.)) ;
#93785 = DIRECTION('ref_axis',(0.,0.,1.)) ;
#93786 = DIRECTION('center_axis',(1.,1.53063836115601E-16,0.)) ;
#93787 = DIRECTION('ref_axis',(1.53063836115601E-16,-1.,0.)) ;
#93788 = DIRECTION('center_axis',(0.,1.,0.)) ;
#93789 = DIRECTION('ref_axis',(1.,0.,0.)) ;
#93790 = DIRECTION('center_axis',(-1.,-2.16840434497101E-16,0.)) ;
#93791 = DIRECTION('ref_axis',(0.,-1.,0.)) ;
#93792 = DIRECTION('center_axis',(0.,0.,-1.)) ;
#93793 = DIRECTION('ref_axis',(1.,0.,0.)) ;
#93794 = DIRECTION('center_axis',(-1.25542992828747E-32,1.020425574104E-16,
1.)) ;
#93795 = DIRECTION('ref_axis',(0.,-1.,0.)) ;
#93796 = DIRECTION('center_axis',(0.,-1.,0.)) ;
#93797 = DIRECTION('ref_axis',(-6.50521303491307E-15,0.,1.)) ;
#93798 = DIRECTION('center_axis',(-1.,0.,0.)) ;
#93799 = DIRECTION('ref_axis',(0.,0.,-1.)) ;
#93800 = DIRECTION('center_axis',(-1.,-1.53063836115601E-16,0.)) ;
#93801 = DIRECTION('ref_axis',(0.,-1.,0.)) ;
#93802 = DIRECTION('center_axis',(0.,-1.,0.)) ;
#93803 = DIRECTION('ref_axis',(0.,0.,1.)) ;
#93804 = DIRECTION('center_axis',(0.,0.,-1.)) ;
#93805 = DIRECTION('ref_axis',(-1.,0.,0.)) ;
#93806 = DIRECTION('center_axis',(0.,0.,-1.)) ;
#93807 = DIRECTION('ref_axis',(-1.,0.,0.)) ;
#93808 = DIRECTION('center_axis',(1.,1.53063836115601E-16,-3.06472600140763E-33)) ;
#93809 = DIRECTION('ref_axis',(-1.53063836115601E-16,1.,4.69098718418678E-49)) ;
#93810 = DIRECTION('center_axis',(-1.,0.,0.)) ;
#93811 = DIRECTION('ref_axis',(0.,0.,1.)) ;
#93812 = DIRECTION('center_axis',(-1.53063836115601E-16,1.,-1.020425574104E-16)) ;
#93813 = DIRECTION('ref_axis',(-1.,-1.53063836115601E-16,1.3684555315672E-47)) ;
#93814 = DIRECTION('',(1.53063836115601E-16,-1.,1.020425574104E-16)) ;
#93815 = DIRECTION('center_axis',(0.,-1.,0.)) ;
#93816 = DIRECTION('ref_axis',(0.,0.,-1.)) ;
#93817 = DIRECTION('center_axis',(-1.53063836115601E-16,1.,-1.30104260698261E-16)) ;
#93818 = DIRECTION('ref_axis',(-1.,-1.53063836115601E-16,1.99142572374599E-32)) ;
#93819 = DIRECTION('center_axis',(0.,-1.,0.)) ;
#93820 = DIRECTION('ref_axis',(0.,0.,-1.)) ;
#93821 = DIRECTION('center_axis',(-1.,-1.53063836115601E-16,2.73691106313441E-48)) ;
#93822 = DIRECTION('ref_axis',(1.53063836115601E-16,-1.,-4.18922106430579E-64)) ;
#93823 = DIRECTION('center_axis',(1.,2.16840434497101E-16,0.)) ;
#93824 = DIRECTION('ref_axis',(2.16840434497101E-16,-1.,0.)) ;
#93825 = DIRECTION('center_axis',(-1.,0.,2.16840434497102E-15)) ;
#93826 = DIRECTION('ref_axis',(2.16840434497102E-15,0.,1.)) ;
#93827 = DIRECTION('center_axis',(-1.,-2.16840434497101E-16,0.)) ;
#93828 = DIRECTION('ref_axis',(0.,-1.,0.)) ;
#93829 = DIRECTION('center_axis',(0.,0.,1.)) ;
#93830 = DIRECTION('ref_axis',(-1.,0.,0.)) ;
#93831 = DIRECTION('center_axis',(0.,1.,0.)) ;
#93832 = DIRECTION('ref_axis',(1.,0.,0.)) ;
#93833 = DIRECTION('center_axis',(0.,1.,0.)) ;
#93834 = DIRECTION('ref_axis',(0.,0.,-1.)) ;
#93835 = DIRECTION('center_axis',(1.,0.,0.)) ;
#93836 = DIRECTION('ref_axis',(0.,-1.,0.)) ;
#93837 = DIRECTION('center_axis',(1.,6.50521303491304E-15,0.)) ;
#93838 = DIRECTION('ref_axis',(-6.50521303491304E-15,1.,0.)) ;
#93839 = DIRECTION('center_axis',(8.67361737988403E-15,1.,0.)) ;
#93840 = DIRECTION('ref_axis',(-1.,8.67361737988403E-15,0.)) ;
#93841 = DIRECTION('center_axis',(1.2303003375722E-16,-1.,1.020425574104E-16)) ;
#93842 = DIRECTION('ref_axis',(1.,1.2303003375722E-16,-1.25542992828747E-32)) ;
#93843 = DIRECTION('center_axis',(0.,1.,0.)) ;
#93844 = DIRECTION('ref_axis',(0.,0.,1.)) ;
#93845 = DIRECTION('center_axis',(0.,1.,0.)) ;
#93846 = DIRECTION('ref_axis',(1.,0.,0.)) ;
#93847 = DIRECTION('center_axis',(1.,1.2303003375722E-16,0.)) ;
#93848 = DIRECTION('ref_axis',(1.2303003375722E-16,-1.,0.)) ;
#93849 = DIRECTION('center_axis',(0.,0.,1.)) ;
#93850 = DIRECTION('ref_axis',(-1.,0.,0.)) ;
#93851 = DIRECTION('center_axis',(0.,1.,0.)) ;
#93852 = DIRECTION('ref_axis',(1.,0.,0.)) ;
#93853 = DIRECTION('center_axis',(0.,0.,-1.)) ;
#93854 = DIRECTION('ref_axis',(1.,0.,0.)) ;
#93855 = DIRECTION('center_axis',(0.,0.,-1.)) ;
#93856 = DIRECTION('ref_axis',(-1.,0.,0.)) ;
#93857 = DIRECTION('center_axis',(0.,0.,1.)) ;
#93858 = DIRECTION('ref_axis',(1.,0.,0.)) ;
#93859 = DIRECTION('center_axis',(-2.16840434497101E-16,1.,-1.020425574104E-16)) ;
#93860 = DIRECTION('ref_axis',(-1.,-2.16840434497101E-16,5.47382212626882E-48)) ;
#93861 = DIRECTION('center_axis',(0.,1.,0.)) ;
#93862 = DIRECTION('ref_axis',(0.,0.,-1.)) ;
#93863 = DIRECTION('center_axis',(1.,0.,1.25542992828747E-32)) ;
#93864 = DIRECTION('ref_axis',(1.25542992828747E-32,0.,-1.)) ;
#93865 = DIRECTION('center_axis',(1.,0.,0.)) ;
#93866 = DIRECTION('ref_axis',(0.,0.,-1.)) ;
#93867 = DIRECTION('center_axis',(-1.,-1.2303003375722E-16,0.)) ;
#93868 = DIRECTION('ref_axis',(0.,-1.,0.)) ;
#93869 = DIRECTION('center_axis',(0.,0.,-1.)) ;
#93870 = DIRECTION('ref_axis',(1.,0.,0.)) ;
#93871 = DIRECTION('center_axis',(0.,0.,-1.)) ;
#93872 = DIRECTION('ref_axis',(-1.,0.,0.)) ;
#93873 = DIRECTION('',(0.,0.,1.)) ;
#93874 = DIRECTION('center_axis',(0.,0.,1.)) ;
#93875 = DIRECTION('ref_axis',(1.,0.,0.)) ;
#93876 = DIRECTION('center_axis',(0.,0.,1.)) ;
#93877 = DIRECTION('ref_axis',(1.,0.,0.)) ;
#93878 = DIRECTION('center_axis',(6.27714964143733E-33,-5.10212787052002E-17,
-1.)) ;
#93879 = DIRECTION('ref_axis',(3.20268201330022E-49,1.,-5.10212787052002E-17)) ;
#93880 = DIRECTION('center_axis',(1.,1.53063836115601E-16,-1.53236300070382E-33)) ;
#93881 = DIRECTION('ref_axis',(-1.53063836115601E-16,1.,2.34549359209339E-49)) ;
#93882 = DIRECTION('center_axis',(-1.,0.,0.)) ;
#93883 = DIRECTION('ref_axis',(0.,0.,1.)) ;
#93884 = DIRECTION('center_axis',(1.,0.,0.)) ;
#93885 = DIRECTION('ref_axis',(0.,0.,-1.)) ;
#93886 = DIRECTION('center_axis',(0.,1.,0.)) ;
#93887 = DIRECTION('ref_axis',(1.,0.,0.)) ;
#93888 = DIRECTION('center_axis',(-4.33680868994202E-15,1.,0.)) ;
#93889 = DIRECTION('ref_axis',(1.,4.33680868994202E-15,0.)) ;
#93890 = DIRECTION('center_axis',(0.,-1.,0.)) ;
#93891 = DIRECTION('ref_axis',(0.,0.,-1.)) ;
#93892 = DIRECTION('center_axis',(0.,0.,-1.)) ;
#93893 = DIRECTION('ref_axis',(1.,0.,0.)) ;
#93894 = DIRECTION('center_axis',(0.,0.,1.)) ;
#93895 = DIRECTION('ref_axis',(1.,0.,0.)) ;
#93896 = DIRECTION('center_axis',(0.,0.,-1.)) ;
#93897 = DIRECTION('ref_axis',(-1.,0.,0.)) ;
#93898 = DIRECTION('center_axis',(0.,1.,0.)) ;
#93899 = DIRECTION('ref_axis',(1.,0.,0.)) ;
#93900 = DIRECTION('center_axis',(1.,1.2303003375722E-16,0.)) ;
#93901 = DIRECTION('ref_axis',(1.2303003375722E-16,-1.,0.)) ;
#93902 = DIRECTION('center_axis',(0.,1.,0.)) ;
#93903 = DIRECTION('ref_axis',(-6.50521303491307E-15,0.,-1.)) ;
#93904 = DIRECTION('center_axis',(6.27714964143733E-33,-5.10212787052002E-17,
-1.)) ;
#93905 = DIRECTION('ref_axis',(0.,1.,0.)) ;
#93906 = DIRECTION('center_axis',(0.,-1.,0.)) ;
#93907 = DIRECTION('ref_axis',(0.,0.,1.)) ;
#93908 = DIRECTION('center_axis',(2.16840434497101E-16,-1.,5.10212787052002E-17)) ;
#93909 = DIRECTION('ref_axis',(1.,2.16840434497101E-16,-5.47382212626882E-48)) ;
#93910 = DIRECTION('center_axis',(0.,1.,0.)) ;
#93911 = DIRECTION('ref_axis',(0.,0.,-1.)) ;
#93912 = DIRECTION('center_axis',(0.,0.,1.)) ;
#93913 = DIRECTION('ref_axis',(1.,0.,0.)) ;
#93914 = DIRECTION('center_axis',(0.,0.,-1.)) ;
#93915 = DIRECTION('ref_axis',(-1.,0.,0.)) ;
#93916 = DIRECTION('center_axis',(-1.,-1.2303003375722E-16,0.)) ;
#93917 = DIRECTION('ref_axis',(0.,-1.,0.)) ;
#93918 = DIRECTION('center_axis',(0.,-1.,0.)) ;
#93919 = DIRECTION('ref_axis',(0.,0.,1.)) ;
#93920 = DIRECTION('center_axis',(1.53063836115601E-16,-1.,5.10212787052002E-17)) ;
#93921 = DIRECTION('ref_axis',(1.,1.53063836115601E-16,-6.84227765783602E-48)) ;
#93922 = DIRECTION('',(-1.53063836115601E-16,1.,-5.10212787052002E-17)) ;
#93923 = DIRECTION('center_axis',(0.,-1.,0.)) ;
#93924 = DIRECTION('ref_axis',(0.,0.,-1.)) ;
#93925 = DIRECTION('center_axis',(-1.,0.,0.)) ;
#93926 = DIRECTION('ref_axis',(0.,0.,-1.)) ;
#93927 = DIRECTION('center_axis',(-1.2303003375722E-16,1.,-5.10212787052002E-17)) ;
#93928 = DIRECTION('ref_axis',(-1.,-1.2303003375722E-16,6.27714964143733E-33)) ;
#93929 = DIRECTION('center_axis',(-8.67361737988403E-15,-1.,0.)) ;
#93930 = DIRECTION('ref_axis',(1.,-8.67361737988403E-15,0.)) ;
#93931 = DIRECTION('center_axis',(1.,0.,6.27714964143733E-33)) ;
#93932 = DIRECTION('ref_axis',(6.27714964143733E-33,0.,-1.)) ;
#93933 = DIRECTION('center_axis',(-1.,0.,-6.50521303491307E-15)) ;
#93934 = DIRECTION('ref_axis',(-6.50521303491307E-15,0.,1.)) ;
#93935 = DIRECTION('center_axis',(1.,0.,0.)) ;
#93936 = DIRECTION('ref_axis',(0.,1.,0.)) ;
#93937 = DIRECTION('center_axis',(0.,0.,-1.)) ;
#93938 = DIRECTION('ref_axis',(-1.,0.,0.)) ;
#93939 = DIRECTION('center_axis',(0.,0.,1.)) ;
#93940 = DIRECTION('ref_axis',(1.,0.,0.)) ;
#93941 = DIRECTION('center_axis',(0.,0.,-1.)) ;
#93942 = DIRECTION('ref_axis',(-1.,0.,0.)) ;
#93943 = DIRECTION('center_axis',(-1.,0.,0.)) ;
#93944 = DIRECTION('ref_axis',(0.,0.,1.)) ;
#93945 = DIRECTION('center_axis',(0.,-1.,0.)) ;
#93946 = DIRECTION('ref_axis',(0.,0.,-1.)) ;
#93947 = DIRECTION('center_axis',(0.,1.,0.)) ;
#93948 = DIRECTION('ref_axis',(0.,0.,1.)) ;
#93949 = DIRECTION('center_axis',(0.,1.,-6.50521303491307E-15)) ;
#93950 = DIRECTION('ref_axis',(0.,6.50521303491307E-15,1.)) ;
#93951 = DIRECTION('center_axis',(0.,-1.,0.)) ;
#93952 = DIRECTION('ref_axis',(0.,0.,-1.)) ;
#93953 = DIRECTION('center_axis',(0.,-1.,0.)) ;
#93954 = DIRECTION('ref_axis',(0.,0.,-1.)) ;
#93955 = DIRECTION('center_axis',(0.,-1.,-1.07081696047951E-16)) ;
#93956 = DIRECTION('ref_axis',(0.,1.07081696047951E-16,-1.)) ;
#93957 = DIRECTION('center_axis',(0.,1.,0.)) ;
#93958 = DIRECTION('ref_axis',(0.,0.,1.)) ;
#93959 = DIRECTION('center_axis',(-1.,0.,0.)) ;
#93960 = DIRECTION('ref_axis',(0.,0.,1.)) ;
#93961 = DIRECTION('center_axis',(0.,0.,1.)) ;
#93962 = DIRECTION('ref_axis',(1.,0.,0.)) ;
#93963 = DIRECTION('center_axis',(0.,1.,0.)) ;
#93964 = DIRECTION('ref_axis',(0.,0.,1.)) ;
#93965 = DIRECTION('center_axis',(0.,0.,-1.)) ;
#93966 = DIRECTION('ref_axis',(-1.,0.,0.)) ;
#93967 = DIRECTION('center_axis',(0.,0.,1.)) ;
#93968 = DIRECTION('ref_axis',(1.,0.,0.)) ;
#93969 = DIRECTION('center_axis',(0.,0.,1.)) ;
#93970 = DIRECTION('ref_axis',(1.,0.,0.)) ;
#93971 = DIRECTION('center_axis',(0.,0.,1.)) ;
#93972 = DIRECTION('ref_axis',(1.,0.,0.)) ;
#93973 = DIRECTION('center_axis',(0.,0.,-1.)) ;
#93974 = DIRECTION('ref_axis',(-1.,0.,0.)) ;
#93975 = DIRECTION('center_axis',(0.,1.,0.)) ;
#93976 = DIRECTION('ref_axis',(0.,0.,1.)) ;
#93977 = DIRECTION('center_axis',(0.,-0.707106781186558,0.707106781186537)) ;
#93978 = DIRECTION('ref_axis',(0.,-0.707106781186537,-0.707106781186558)) ;
#93979 = DIRECTION('center_axis',(0.,1.,0.)) ;
#93980 = DIRECTION('ref_axis',(0.,0.,1.)) ;
#93981 = DIRECTION('center_axis',(0.,-0.514231796959093,-0.857651245551607)) ;
#93982 = DIRECTION('ref_axis',(0.,0.857651245551607,-0.514231796959093)) ;
#93983 = DIRECTION('center_axis',(0.,-0.707106781186548,0.707106781186547)) ;
#93984 = DIRECTION('ref_axis',(0.,-0.707106781186547,-0.707106781186548)) ;
#93985 = DIRECTION('center_axis',(0.,-0.70710678118655,0.707106781186545)) ;
#93986 = DIRECTION('ref_axis',(0.,-0.707106781186545,-0.70710678118655)) ;
#93987 = DIRECTION('center_axis',(-1.,0.,0.)) ;
#93988 = DIRECTION('ref_axis',(0.,0.,1.)) ;
#93989 = DIRECTION('center_axis',(-2.23012492569676E-15,0.514231796959107,
-0.857651245551598)) ;
#93990 = DIRECTION('ref_axis',(-5.69910941180089E-30,0.857651245551598,0.514231796959107)) ;
#93991 = DIRECTION('center_axis',(0.,1.,0.)) ;
#93992 = DIRECTION('ref_axis',(0.,0.,1.)) ;
#93993 = DIRECTION('center_axis',(0.,0.,-1.)) ;
#93994 = DIRECTION('ref_axis',(-1.,0.,0.)) ;
#93995 = DIRECTION('center_axis',(0.,1.,0.)) ;
#93996 = DIRECTION('ref_axis',(0.,0.,1.)) ;
#93997 = DIRECTION('center_axis',(0.,0.,-1.)) ;
#93998 = DIRECTION('ref_axis',(-1.,0.,0.)) ;
#93999 = DIRECTION('center_axis',(0.,0.,-1.)) ;
#94000 = DIRECTION('ref_axis',(-1.,0.,0.)) ;
#94001 = DIRECTION('center_axis',(0.,0.,1.)) ;
#94002 = DIRECTION('ref_axis',(1.,0.,0.)) ;
#94003 = DIRECTION('center_axis',(0.,0.,-1.)) ;
#94004 = DIRECTION('ref_axis',(-1.,0.,0.)) ;
#94005 = DIRECTION('center_axis',(0.,1.,0.)) ;
#94006 = DIRECTION('ref_axis',(0.,0.,1.)) ;
#94007 = DIRECTION('center_axis',(0.,-1.,8.67361737988409E-15)) ;
#94008 = DIRECTION('ref_axis',(0.,-8.67361737988409E-15,-1.)) ;
#94009 = DIRECTION('center_axis',(0.,0.707106781186546,0.707106781186549)) ;
#94010 = DIRECTION('ref_axis',(0.,-0.707106781186549,0.707106781186546)) ;
#94011 = DIRECTION('center_axis',(0.,0.707106781186541,0.707106781186554)) ;
#94012 = DIRECTION('ref_axis',(0.,-0.707106781186554,0.707106781186541)) ;
#94013 = DIRECTION('center_axis',(0.,1.,1.07081696047951E-16)) ;
#94014 = DIRECTION('ref_axis',(0.,-1.07081696047951E-16,1.)) ;
#94015 = DIRECTION('center_axis',(0.,-1.,0.)) ;
#94016 = DIRECTION('ref_axis',(0.,0.,-1.)) ;
#94017 = DIRECTION('center_axis',(0.,1.,0.)) ;
#94018 = DIRECTION('ref_axis',(0.,0.,1.)) ;
#94019 = DIRECTION('center_axis',(0.,0.,1.)) ;
#94020 = DIRECTION('ref_axis',(1.,0.,0.)) ;
#94021 = DIRECTION('center_axis',(0.,1.,0.)) ;
#94022 = DIRECTION('ref_axis',(0.,0.,1.)) ;
#94023 = DIRECTION('center_axis',(0.,0.,1.)) ;
#94024 = DIRECTION('ref_axis',(1.,0.,0.)) ;
#94025 = DIRECTION('center_axis',(0.,3.99416362155027E-15,1.)) ;
#94026 = DIRECTION('ref_axis',(0.,-1.,3.99416362155027E-15)) ;
#94027 = DIRECTION('center_axis',(0.,0.,1.)) ;
#94028 = DIRECTION('ref_axis',(1.,0.,0.)) ;
#94029 = DIRECTION('center_axis',(0.,0.,-1.)) ;
#94030 = DIRECTION('ref_axis',(-1.,0.,0.)) ;
#94031 = DIRECTION('center_axis',(0.,0.,1.)) ;
#94032 = DIRECTION('ref_axis',(1.,0.,0.)) ;
#94033 = DIRECTION('center_axis',(-1.,0.,0.)) ;
#94034 = DIRECTION('ref_axis',(0.,0.,1.)) ;
#94035 = DIRECTION('center_axis',(0.,1.,0.)) ;
#94036 = DIRECTION('ref_axis',(0.,0.,1.)) ;
#94037 = DIRECTION('center_axis',(-1.,0.,0.)) ;
#94038 = DIRECTION('ref_axis',(0.,0.,1.)) ;
#94039 = DIRECTION('center_axis',(0.,-1.,0.)) ;
#94040 = DIRECTION('ref_axis',(0.,0.,-1.)) ;
#94041 = DIRECTION('center_axis',(0.,1.,0.)) ;
#94042 = DIRECTION('ref_axis',(0.,0.,1.)) ;
#94043 = DIRECTION('center_axis',(1.53063836115601E-16,-1.,-1.30104260698261E-16)) ;
#94044 = DIRECTION('ref_axis',(1.,1.53063836115601E-16,1.99142572374599E-32)) ;
#94045 = DIRECTION('center_axis',(0.,1.,0.)) ;
#94046 = DIRECTION('ref_axis',(0.,0.,1.)) ;
#94047 = DIRECTION('center_axis',(0.,-1.,0.)) ;
#94048 = DIRECTION('ref_axis',(0.,0.,-1.)) ;
#94049 = DIRECTION('center_axis',(1.,1.53063836115601E-16,2.73691106313441E-48)) ;
#94050 = DIRECTION('ref_axis',(-1.53063836115601E-16,1.,-4.18922106430579E-64)) ;
#94051 = DIRECTION('center_axis',(-1.,0.,0.)) ;
#94052 = DIRECTION('ref_axis',(0.,0.,1.)) ;
#94053 = DIRECTION('center_axis',(1.,1.53063836115601E-16,0.)) ;
#94054 = DIRECTION('ref_axis',(1.53063836115601E-16,-1.,0.)) ;
#94055 = DIRECTION('center_axis',(0.,1.,0.)) ;
#94056 = DIRECTION('ref_axis',(1.,0.,0.)) ;
#94057 = DIRECTION('center_axis',(0.,1.,0.)) ;
#94058 = DIRECTION('ref_axis',(0.,0.,-1.)) ;
#94059 = DIRECTION('center_axis',(0.,0.,1.)) ;
#94060 = DIRECTION('ref_axis',(-1.,0.,0.)) ;
#94061 = DIRECTION('center_axis',(0.,1.,0.)) ;
#94062 = DIRECTION('ref_axis',(1.,0.,0.)) ;
#94063 = DIRECTION('center_axis',(0.,0.,1.)) ;
#94064 = DIRECTION('ref_axis',(-1.,0.,0.)) ;
#94065 = DIRECTION('center_axis',(1.,1.0842021724855E-15,0.)) ;
#94066 = DIRECTION('ref_axis',(1.0842021724855E-15,-1.,0.)) ;
#94067 = DIRECTION('center_axis',(-1.,-1.53063836115601E-16,0.)) ;
#94068 = DIRECTION('ref_axis',(0.,-1.,0.)) ;
#94069 = DIRECTION('center_axis',(0.,0.,-1.)) ;
#94070 = DIRECTION('ref_axis',(1.,0.,0.)) ;
#94071 = DIRECTION('center_axis',(0.,0.,-1.)) ;
#94072 = DIRECTION('ref_axis',(0.804034447892622,0.594582716366702,0.)) ;
#94073 = DIRECTION('center_axis',(0.,0.,1.)) ;
#94074 = DIRECTION('ref_axis',(1.,0.,0.)) ;
#94075 = DIRECTION('',(0.,0.,-1.)) ;
#94076 = DIRECTION('center_axis',(-2.16840434497101E-16,1.,1.30104260698261E-16)) ;
#94077 = DIRECTION('ref_axis',(1.,2.16840434497101E-16,1.22464679914735E-16)) ;
#94078 = DIRECTION('',(-2.16840434497101E-16,1.,1.30104260698261E-16)) ;
#94079 = DIRECTION('center_axis',(0.,1.,0.)) ;
#94080 = DIRECTION('ref_axis',(0.,0.,1.)) ;
#94081 = DIRECTION('center_axis',(-1.,-1.53063836115601E-16,-2.73691106313441E-48)) ;
#94082 = DIRECTION('ref_axis',(1.53063836115601E-16,-1.,4.18922106430579E-64)) ;
#94083 = DIRECTION('center_axis',(1.,2.16840434497101E-16,0.)) ;
#94084 = DIRECTION('ref_axis',(2.16840434497101E-16,-1.,0.)) ;
#94085 = DIRECTION('center_axis',(0.,0.,1.)) ;
#94086 = DIRECTION('ref_axis',(1.,0.,0.)) ;
#94087 = DIRECTION('center_axis',(-1.25542992828747E-32,1.020425574104E-16,
1.)) ;
#94088 = DIRECTION('ref_axis',(-1.28107280532009E-48,-1.,1.020425574104E-16)) ;
#94089 = DIRECTION('center_axis',(0.,0.,1.)) ;
#94090 = DIRECTION('ref_axis',(1.,0.,0.)) ;
#94091 = DIRECTION('center_axis',(0.,0.,-1.)) ;
#94092 = DIRECTION('ref_axis',(-1.,0.,0.)) ;
#94093 = DIRECTION('center_axis',(1.,1.53063836115601E-16,-2.73691106313441E-48)) ;
#94094 = DIRECTION('ref_axis',(-1.53063836115601E-16,1.,4.18922106430579E-64)) ;
#94095 = DIRECTION('center_axis',(-1.,0.,0.)) ;
#94096 = DIRECTION('ref_axis',(0.,0.,1.)) ;
#94097 = DIRECTION('center_axis',(1.,1.53063836115601E-16,0.)) ;
#94098 = DIRECTION('ref_axis',(1.53063836115601E-16,-1.,0.)) ;
#94099 = DIRECTION('center_axis',(0.,1.,0.)) ;
#94100 = DIRECTION('ref_axis',(1.,0.,0.)) ;
#94101 = DIRECTION('center_axis',(-1.,-2.16840434497101E-16,0.)) ;
#94102 = DIRECTION('ref_axis',(0.,-1.,0.)) ;
#94103 = DIRECTION('center_axis',(0.,0.,-1.)) ;
#94104 = DIRECTION('ref_axis',(1.,0.,0.)) ;
#94105 = DIRECTION('center_axis',(-1.25542992828747E-32,1.020425574104E-16,
1.)) ;
#94106 = DIRECTION('ref_axis',(0.,-1.,0.)) ;
#94107 = DIRECTION('center_axis',(0.,-1.,0.)) ;
#94108 = DIRECTION('ref_axis',(-6.50521303491307E-15,0.,1.)) ;
#94109 = DIRECTION('center_axis',(-1.,0.,0.)) ;
#94110 = DIRECTION('ref_axis',(0.,0.,-1.)) ;
#94111 = DIRECTION('center_axis',(-1.,-1.53063836115601E-16,0.)) ;
#94112 = DIRECTION('ref_axis',(0.,-1.,0.)) ;
#94113 = DIRECTION('center_axis',(0.,-1.,0.)) ;
#94114 = DIRECTION('ref_axis',(0.,0.,1.)) ;
#94115 = DIRECTION('center_axis',(0.,0.,-1.)) ;
#94116 = DIRECTION('ref_axis',(-1.,0.,0.)) ;
#94117 = DIRECTION('center_axis',(0.,0.,-1.)) ;
#94118 = DIRECTION('ref_axis',(-1.,0.,0.)) ;
#94119 = DIRECTION('center_axis',(1.,1.53063836115601E-16,-3.06472600140763E-33)) ;
#94120 = DIRECTION('ref_axis',(-1.53063836115601E-16,1.,4.69098718418678E-49)) ;
#94121 = DIRECTION('center_axis',(-1.,0.,0.)) ;
#94122 = DIRECTION('ref_axis',(0.,0.,1.)) ;
#94123 = DIRECTION('center_axis',(-1.53063836115601E-16,1.,-1.020425574104E-16)) ;
#94124 = DIRECTION('ref_axis',(-1.,-1.53063836115601E-16,1.3684555315672E-47)) ;
#94125 = DIRECTION('',(1.53063836115601E-16,-1.,1.020425574104E-16)) ;
#94126 = DIRECTION('center_axis',(0.,-1.,0.)) ;
#94127 = DIRECTION('ref_axis',(0.,0.,-1.)) ;
#94128 = DIRECTION('center_axis',(-1.53063836115601E-16,1.,-1.30104260698261E-16)) ;
#94129 = DIRECTION('ref_axis',(-1.,-1.53063836115601E-16,1.99142572374599E-32)) ;
#94130 = DIRECTION('center_axis',(0.,-1.,0.)) ;
#94131 = DIRECTION('ref_axis',(0.,0.,-1.)) ;
#94132 = DIRECTION('center_axis',(-1.,-1.53063836115601E-16,2.73691106313441E-48)) ;
#94133 = DIRECTION('ref_axis',(1.53063836115601E-16,-1.,-4.18922106430579E-64)) ;
#94134 = DIRECTION('center_axis',(1.,2.16840434497101E-16,0.)) ;
#94135 = DIRECTION('ref_axis',(2.16840434497101E-16,-1.,0.)) ;
#94136 = DIRECTION('center_axis',(-1.,0.,2.16840434497102E-15)) ;
#94137 = DIRECTION('ref_axis',(2.16840434497102E-15,0.,1.)) ;
#94138 = DIRECTION('center_axis',(-1.,-2.16840434497101E-16,0.)) ;
#94139 = DIRECTION('ref_axis',(0.,-1.,0.)) ;
#94140 = DIRECTION('center_axis',(0.,0.,1.)) ;
#94141 = DIRECTION('ref_axis',(-1.,0.,0.)) ;
#94142 = DIRECTION('center_axis',(0.,1.,0.)) ;
#94143 = DIRECTION('ref_axis',(1.,0.,0.)) ;
#94144 = DIRECTION('center_axis',(0.,1.,0.)) ;
#94145 = DIRECTION('ref_axis',(0.,0.,-1.)) ;
#94146 = DIRECTION('center_axis',(1.,0.,0.)) ;
#94147 = DIRECTION('ref_axis',(0.,-1.,0.)) ;
#94148 = DIRECTION('center_axis',(1.,6.50521303491304E-15,0.)) ;
#94149 = DIRECTION('ref_axis',(-6.50521303491304E-15,1.,0.)) ;
#94150 = DIRECTION('center_axis',(8.67361737988403E-15,1.,0.)) ;
#94151 = DIRECTION('ref_axis',(-1.,8.67361737988403E-15,0.)) ;
#94152 = DIRECTION('center_axis',(1.2303003375722E-16,-1.,1.020425574104E-16)) ;
#94153 = DIRECTION('ref_axis',(1.,1.2303003375722E-16,-1.25542992828747E-32)) ;
#94154 = DIRECTION('center_axis',(0.,1.,0.)) ;
#94155 = DIRECTION('ref_axis',(0.,0.,1.)) ;
#94156 = DIRECTION('center_axis',(0.,1.,0.)) ;
#94157 = DIRECTION('ref_axis',(1.,0.,0.)) ;
#94158 = DIRECTION('center_axis',(1.,1.2303003375722E-16,0.)) ;
#94159 = DIRECTION('ref_axis',(1.2303003375722E-16,-1.,0.)) ;
#94160 = DIRECTION('center_axis',(0.,0.,1.)) ;
#94161 = DIRECTION('ref_axis',(-1.,0.,0.)) ;
#94162 = DIRECTION('center_axis',(0.,1.,0.)) ;
#94163 = DIRECTION('ref_axis',(1.,0.,0.)) ;
#94164 = DIRECTION('center_axis',(0.,0.,-1.)) ;
#94165 = DIRECTION('ref_axis',(1.,0.,0.)) ;
#94166 = DIRECTION('center_axis',(0.,0.,-1.)) ;
#94167 = DIRECTION('ref_axis',(-1.,0.,0.)) ;
#94168 = DIRECTION('center_axis',(0.,0.,1.)) ;
#94169 = DIRECTION('ref_axis',(1.,0.,0.)) ;
#94170 = DIRECTION('center_axis',(-2.16840434497101E-16,1.,-1.020425574104E-16)) ;
#94171 = DIRECTION('ref_axis',(-1.,-2.16840434497101E-16,5.47382212626882E-48)) ;
#94172 = DIRECTION('center_axis',(0.,1.,0.)) ;
#94173 = DIRECTION('ref_axis',(0.,0.,-1.)) ;
#94174 = DIRECTION('center_axis',(1.,0.,1.25542992828747E-32)) ;
#94175 = DIRECTION('ref_axis',(1.25542992828747E-32,0.,-1.)) ;
#94176 = DIRECTION('center_axis',(1.,0.,0.)) ;
#94177 = DIRECTION('ref_axis',(0.,0.,-1.)) ;
#94178 = DIRECTION('center_axis',(-1.,-1.2303003375722E-16,0.)) ;
#94179 = DIRECTION('ref_axis',(0.,-1.,0.)) ;
#94180 = DIRECTION('center_axis',(0.,0.,-1.)) ;
#94181 = DIRECTION('ref_axis',(1.,0.,0.)) ;
#94182 = DIRECTION('center_axis',(0.,0.,-1.)) ;
#94183 = DIRECTION('ref_axis',(-1.,0.,0.)) ;
#94184 = DIRECTION('',(0.,0.,1.)) ;
#94185 = DIRECTION('center_axis',(0.,0.,1.)) ;
#94186 = DIRECTION('ref_axis',(1.,0.,0.)) ;
#94187 = DIRECTION('center_axis',(0.,0.,1.)) ;
#94188 = DIRECTION('ref_axis',(1.,0.,0.)) ;
#94189 = DIRECTION('center_axis',(6.27714964143733E-33,-5.10212787052002E-17,
-1.)) ;
#94190 = DIRECTION('ref_axis',(3.20268201330022E-49,1.,-5.10212787052002E-17)) ;
#94191 = DIRECTION('center_axis',(1.,1.53063836115601E-16,-1.53236300070382E-33)) ;
#94192 = DIRECTION('ref_axis',(-1.53063836115601E-16,1.,2.34549359209339E-49)) ;
#94193 = DIRECTION('center_axis',(-1.,0.,0.)) ;
#94194 = DIRECTION('ref_axis',(0.,0.,1.)) ;
#94195 = DIRECTION('center_axis',(1.,0.,0.)) ;
#94196 = DIRECTION('ref_axis',(0.,0.,-1.)) ;
#94197 = DIRECTION('center_axis',(0.,1.,0.)) ;
#94198 = DIRECTION('ref_axis',(1.,0.,0.)) ;
#94199 = DIRECTION('center_axis',(-4.33680868994202E-15,1.,0.)) ;
#94200 = DIRECTION('ref_axis',(1.,4.33680868994202E-15,0.)) ;
#94201 = DIRECTION('center_axis',(0.,-1.,0.)) ;
#94202 = DIRECTION('ref_axis',(0.,0.,-1.)) ;
#94203 = DIRECTION('center_axis',(0.,0.,-1.)) ;
#94204 = DIRECTION('ref_axis',(1.,0.,0.)) ;
#94205 = DIRECTION('center_axis',(0.,0.,1.)) ;
#94206 = DIRECTION('ref_axis',(1.,0.,0.)) ;
#94207 = DIRECTION('center_axis',(0.,0.,-1.)) ;
#94208 = DIRECTION('ref_axis',(-1.,0.,0.)) ;
#94209 = DIRECTION('center_axis',(0.,1.,0.)) ;
#94210 = DIRECTION('ref_axis',(1.,0.,0.)) ;
#94211 = DIRECTION('center_axis',(1.,1.2303003375722E-16,0.)) ;
#94212 = DIRECTION('ref_axis',(1.2303003375722E-16,-1.,0.)) ;
#94213 = DIRECTION('center_axis',(0.,1.,0.)) ;
#94214 = DIRECTION('ref_axis',(-6.50521303491307E-15,0.,-1.)) ;
#94215 = DIRECTION('center_axis',(6.27714964143733E-33,-5.10212787052002E-17,
-1.)) ;
#94216 = DIRECTION('ref_axis',(0.,1.,0.)) ;
#94217 = DIRECTION('center_axis',(0.,-1.,0.)) ;
#94218 = DIRECTION('ref_axis',(0.,0.,1.)) ;
#94219 = DIRECTION('center_axis',(2.16840434497101E-16,-1.,5.10212787052002E-17)) ;
#94220 = DIRECTION('ref_axis',(1.,2.16840434497101E-16,-5.47382212626882E-48)) ;
#94221 = DIRECTION('center_axis',(0.,1.,0.)) ;
#94222 = DIRECTION('ref_axis',(0.,0.,-1.)) ;
#94223 = DIRECTION('center_axis',(0.,0.,1.)) ;
#94224 = DIRECTION('ref_axis',(1.,0.,0.)) ;
#94225 = DIRECTION('center_axis',(0.,0.,-1.)) ;
#94226 = DIRECTION('ref_axis',(-1.,0.,0.)) ;
#94227 = DIRECTION('center_axis',(-1.,-1.2303003375722E-16,0.)) ;
#94228 = DIRECTION('ref_axis',(0.,-1.,0.)) ;
#94229 = DIRECTION('center_axis',(0.,-1.,0.)) ;
#94230 = DIRECTION('ref_axis',(0.,0.,1.)) ;
#94231 = DIRECTION('center_axis',(1.53063836115601E-16,-1.,5.10212787052002E-17)) ;
#94232 = DIRECTION('ref_axis',(1.,1.53063836115601E-16,-6.84227765783602E-48)) ;
#94233 = DIRECTION('',(-1.53063836115601E-16,1.,-5.10212787052002E-17)) ;
#94234 = DIRECTION('center_axis',(0.,-1.,0.)) ;
#94235 = DIRECTION('ref_axis',(0.,0.,-1.)) ;
#94236 = DIRECTION('center_axis',(-1.,0.,0.)) ;
#94237 = DIRECTION('ref_axis',(0.,0.,-1.)) ;
#94238 = DIRECTION('center_axis',(-1.2303003375722E-16,1.,-5.10212787052002E-17)) ;
#94239 = DIRECTION('ref_axis',(-1.,-1.2303003375722E-16,6.27714964143733E-33)) ;
#94240 = DIRECTION('center_axis',(-8.67361737988403E-15,-1.,0.)) ;
#94241 = DIRECTION('ref_axis',(1.,-8.67361737988403E-15,0.)) ;
#94242 = DIRECTION('center_axis',(1.,0.,6.27714964143733E-33)) ;
#94243 = DIRECTION('ref_axis',(6.27714964143733E-33,0.,-1.)) ;
#94244 = DIRECTION('center_axis',(-1.,0.,-6.50521303491307E-15)) ;
#94245 = DIRECTION('ref_axis',(-6.50521303491307E-15,0.,1.)) ;
#94246 = DIRECTION('center_axis',(1.,0.,0.)) ;
#94247 = DIRECTION('ref_axis',(0.,1.,0.)) ;
#94248 = DIRECTION('center_axis',(0.,0.,-1.)) ;
#94249 = DIRECTION('ref_axis',(-1.,0.,0.)) ;
#94250 = DIRECTION('center_axis',(0.,0.,1.)) ;
#94251 = DIRECTION('ref_axis',(1.,0.,0.)) ;
#94252 = DIRECTION('center_axis',(0.,0.,-1.)) ;
#94253 = DIRECTION('ref_axis',(-1.,0.,0.)) ;
#94254 = DIRECTION('center_axis',(-1.,0.,0.)) ;
#94255 = DIRECTION('ref_axis',(0.,0.,1.)) ;
#94256 = DIRECTION('center_axis',(0.,-1.,0.)) ;
#94257 = DIRECTION('ref_axis',(0.,0.,-1.)) ;
#94258 = DIRECTION('center_axis',(0.,1.,0.)) ;
#94259 = DIRECTION('ref_axis',(0.,0.,1.)) ;
#94260 = DIRECTION('center_axis',(0.,1.,-6.50521303491307E-15)) ;
#94261 = DIRECTION('ref_axis',(0.,6.50521303491307E-15,1.)) ;
#94262 = DIRECTION('center_axis',(0.,-1.,0.)) ;
#94263 = DIRECTION('ref_axis',(0.,0.,-1.)) ;
#94264 = DIRECTION('center_axis',(0.,-1.,0.)) ;
#94265 = DIRECTION('ref_axis',(0.,0.,-1.)) ;
#94266 = DIRECTION('center_axis',(0.,-1.,-1.07081696047951E-16)) ;
#94267 = DIRECTION('ref_axis',(0.,1.07081696047951E-16,-1.)) ;
#94268 = DIRECTION('center_axis',(0.,1.,0.)) ;
#94269 = DIRECTION('ref_axis',(0.,0.,1.)) ;
#94270 = DIRECTION('center_axis',(-1.,0.,0.)) ;
#94271 = DIRECTION('ref_axis',(0.,0.,1.)) ;
#94272 = DIRECTION('center_axis',(0.,0.,1.)) ;
#94273 = DIRECTION('ref_axis',(1.,0.,0.)) ;
#94274 = DIRECTION('center_axis',(0.,1.,0.)) ;
#94275 = DIRECTION('ref_axis',(0.,0.,1.)) ;
#94276 = DIRECTION('center_axis',(0.,0.,-1.)) ;
#94277 = DIRECTION('ref_axis',(-1.,0.,0.)) ;
#94278 = DIRECTION('center_axis',(0.,0.,1.)) ;
#94279 = DIRECTION('ref_axis',(1.,0.,0.)) ;
#94280 = DIRECTION('center_axis',(0.,0.,1.)) ;
#94281 = DIRECTION('ref_axis',(1.,0.,0.)) ;
#94282 = DIRECTION('center_axis',(0.,0.,1.)) ;
#94283 = DIRECTION('ref_axis',(1.,0.,0.)) ;
#94284 = DIRECTION('center_axis',(0.,0.,-1.)) ;
#94285 = DIRECTION('ref_axis',(-1.,0.,0.)) ;
#94286 = DIRECTION('center_axis',(0.,1.,0.)) ;
#94287 = DIRECTION('ref_axis',(0.,0.,1.)) ;
#94288 = DIRECTION('center_axis',(0.,-0.707106781186558,0.707106781186537)) ;
#94289 = DIRECTION('ref_axis',(0.,-0.707106781186537,-0.707106781186558)) ;
#94290 = DIRECTION('center_axis',(0.,1.,0.)) ;
#94291 = DIRECTION('ref_axis',(0.,0.,1.)) ;
#94292 = DIRECTION('center_axis',(0.,-0.514231796959093,-0.857651245551607)) ;
#94293 = DIRECTION('ref_axis',(0.,0.857651245551607,-0.514231796959093)) ;
#94294 = DIRECTION('center_axis',(0.,-0.707106781186548,0.707106781186547)) ;
#94295 = DIRECTION('ref_axis',(0.,-0.707106781186547,-0.707106781186548)) ;
#94296 = DIRECTION('center_axis',(0.,-0.707106781186548,0.707106781186548)) ;
#94297 = DIRECTION('ref_axis',(0.,-0.707106781186548,-0.707106781186548)) ;
#94298 = DIRECTION('center_axis',(-1.,0.,0.)) ;
#94299 = DIRECTION('ref_axis',(0.,0.,1.)) ;
#94300 = DIRECTION('center_axis',(0.,0.514231796959095,-0.857651245551606)) ;
#94301 = DIRECTION('ref_axis',(0.,0.857651245551606,0.514231796959095)) ;
#94302 = DIRECTION('center_axis',(0.,1.,0.)) ;
#94303 = DIRECTION('ref_axis',(0.,0.,1.)) ;
#94304 = DIRECTION('center_axis',(0.,0.,-1.)) ;
#94305 = DIRECTION('ref_axis',(-1.,0.,0.)) ;
#94306 = DIRECTION('center_axis',(0.,1.,0.)) ;
#94307 = DIRECTION('ref_axis',(0.,0.,1.)) ;
#94308 = DIRECTION('center_axis',(0.,0.,-1.)) ;
#94309 = DIRECTION('ref_axis',(-1.,0.,0.)) ;
#94310 = DIRECTION('center_axis',(0.,0.,-1.)) ;
#94311 = DIRECTION('ref_axis',(-1.,0.,0.)) ;
#94312 = DIRECTION('center_axis',(0.,0.,1.)) ;
#94313 = DIRECTION('ref_axis',(1.,0.,0.)) ;
#94314 = DIRECTION('center_axis',(0.,0.,-1.)) ;
#94315 = DIRECTION('ref_axis',(-1.,0.,0.)) ;
#94316 = DIRECTION('center_axis',(0.,1.,0.)) ;
#94317 = DIRECTION('ref_axis',(0.,0.,1.)) ;
#94318 = DIRECTION('center_axis',(0.,-1.,8.67361737988409E-15)) ;
#94319 = DIRECTION('ref_axis',(0.,-8.67361737988409E-15,-1.)) ;
#94320 = DIRECTION('center_axis',(0.,0.707106781186546,0.707106781186549)) ;
#94321 = DIRECTION('ref_axis',(0.,-0.707106781186549,0.707106781186546)) ;
#94322 = DIRECTION('center_axis',(0.,0.707106781186537,0.707106781186558)) ;
#94323 = DIRECTION('ref_axis',(0.,-0.707106781186558,0.707106781186537)) ;
#94324 = DIRECTION('center_axis',(0.,1.,1.07081696047951E-16)) ;
#94325 = DIRECTION('ref_axis',(0.,-1.07081696047951E-16,1.)) ;
#94326 = DIRECTION('center_axis',(0.,-1.,0.)) ;
#94327 = DIRECTION('ref_axis',(0.,0.,-1.)) ;
#94328 = DIRECTION('center_axis',(0.,1.,0.)) ;
#94329 = DIRECTION('ref_axis',(0.,0.,1.)) ;
#94330 = DIRECTION('center_axis',(0.,0.,1.)) ;
#94331 = DIRECTION('ref_axis',(1.,0.,0.)) ;
#94332 = DIRECTION('center_axis',(0.,1.,0.)) ;
#94333 = DIRECTION('ref_axis',(0.,0.,1.)) ;
#94334 = DIRECTION('center_axis',(0.,0.,1.)) ;
#94335 = DIRECTION('ref_axis',(1.,0.,0.)) ;
#94336 = DIRECTION('center_axis',(0.,3.99416362155027E-15,1.)) ;
#94337 = DIRECTION('ref_axis',(0.,-1.,3.99416362155027E-15)) ;
#94338 = DIRECTION('center_axis',(0.,0.,1.)) ;
#94339 = DIRECTION('ref_axis',(1.,0.,0.)) ;
#94340 = DIRECTION('center_axis',(0.,0.,-1.)) ;
#94341 = DIRECTION('ref_axis',(-1.,0.,0.)) ;
#94342 = DIRECTION('center_axis',(0.,0.,1.)) ;
#94343 = DIRECTION('ref_axis',(1.,0.,0.)) ;
#94344 = DIRECTION('center_axis',(-1.,0.,0.)) ;
#94345 = DIRECTION('ref_axis',(0.,0.,1.)) ;
#94346 = DIRECTION('center_axis',(0.,1.,0.)) ;
#94347 = DIRECTION('ref_axis',(0.,0.,1.)) ;
#94348 = DIRECTION('center_axis',(-1.,0.,0.)) ;
#94349 = DIRECTION('ref_axis',(0.,0.,1.)) ;
#94350 = DIRECTION('center_axis',(0.,-1.,0.)) ;
#94351 = DIRECTION('ref_axis',(0.,0.,-1.)) ;
#94352 = DIRECTION('center_axis',(0.,1.,0.)) ;
#94353 = DIRECTION('ref_axis',(0.,0.,1.)) ;
#94354 = DIRECTION('center_axis',(1.53063836115601E-16,-1.,-1.30104260698261E-16)) ;
#94355 = DIRECTION('ref_axis',(1.,1.53063836115601E-16,1.99142572374599E-32)) ;
#94356 = DIRECTION('center_axis',(0.,1.,0.)) ;
#94357 = DIRECTION('ref_axis',(0.,0.,1.)) ;
#94358 = DIRECTION('center_axis',(0.,-1.,0.)) ;
#94359 = DIRECTION('ref_axis',(0.,0.,-1.)) ;
#94360 = DIRECTION('center_axis',(1.,1.53063836115601E-16,2.73691106313441E-48)) ;
#94361 = DIRECTION('ref_axis',(-1.53063836115601E-16,1.,-4.18922106430579E-64)) ;
#94362 = DIRECTION('center_axis',(-1.,0.,0.)) ;
#94363 = DIRECTION('ref_axis',(0.,0.,1.)) ;
#94364 = DIRECTION('center_axis',(1.,1.53063836115601E-16,0.)) ;
#94365 = DIRECTION('ref_axis',(1.53063836115601E-16,-1.,0.)) ;
#94366 = DIRECTION('center_axis',(0.,1.,0.)) ;
#94367 = DIRECTION('ref_axis',(1.,0.,0.)) ;
#94368 = DIRECTION('center_axis',(0.,1.,0.)) ;
#94369 = DIRECTION('ref_axis',(0.,0.,-1.)) ;
#94370 = DIRECTION('center_axis',(0.,0.,1.)) ;
#94371 = DIRECTION('ref_axis',(-1.,0.,0.)) ;
#94372 = DIRECTION('center_axis',(0.,1.,0.)) ;
#94373 = DIRECTION('ref_axis',(1.,0.,0.)) ;
#94374 = DIRECTION('center_axis',(0.,0.,1.)) ;
#94375 = DIRECTION('ref_axis',(-1.,0.,0.)) ;
#94376 = DIRECTION('center_axis',(1.,1.0842021724855E-15,0.)) ;
#94377 = DIRECTION('ref_axis',(1.0842021724855E-15,-1.,0.)) ;
#94378 = DIRECTION('center_axis',(-1.,-1.53063836115601E-16,0.)) ;
#94379 = DIRECTION('ref_axis',(0.,-1.,0.)) ;
#94380 = DIRECTION('center_axis',(0.,0.,-1.)) ;
#94381 = DIRECTION('ref_axis',(1.,0.,0.)) ;
#94382 = DIRECTION('center_axis',(0.,0.,-1.)) ;
#94383 = DIRECTION('ref_axis',(0.804034447892617,0.594582716366709,0.)) ;
#94384 = DIRECTION('center_axis',(0.,0.,1.)) ;
#94385 = DIRECTION('ref_axis',(1.,0.,0.)) ;
#94386 = DIRECTION('',(0.,0.,-1.)) ;
#94387 = DIRECTION('center_axis',(-2.16840434497101E-16,1.,1.30104260698261E-16)) ;
#94388 = DIRECTION('ref_axis',(1.,2.16840434497101E-16,1.22464679914735E-16)) ;
#94389 = DIRECTION('',(-2.16840434497101E-16,1.,1.30104260698261E-16)) ;
#94390 = DIRECTION('center_axis',(0.,1.,0.)) ;
#94391 = DIRECTION('ref_axis',(0.,0.,1.)) ;
#94392 = DIRECTION('center_axis',(-1.,-1.53063836115601E-16,-2.73691106313441E-48)) ;
#94393 = DIRECTION('ref_axis',(1.53063836115601E-16,-1.,4.18922106430579E-64)) ;
#94394 = DIRECTION('center_axis',(1.,2.16840434497101E-16,0.)) ;
#94395 = DIRECTION('ref_axis',(2.16840434497101E-16,-1.,0.)) ;
#94396 = DIRECTION('center_axis',(0.,0.,1.)) ;
#94397 = DIRECTION('ref_axis',(1.,0.,0.)) ;
#94398 = DIRECTION('center_axis',(-1.25542992828747E-32,1.020425574104E-16,
1.)) ;
#94399 = DIRECTION('ref_axis',(-1.28107280532009E-48,-1.,1.020425574104E-16)) ;
#94400 = DIRECTION('center_axis',(0.,0.,1.)) ;
#94401 = DIRECTION('ref_axis',(1.,0.,0.)) ;
#94402 = DIRECTION('center_axis',(0.,0.,-1.)) ;
#94403 = DIRECTION('ref_axis',(-1.,0.,0.)) ;
#94404 = DIRECTION('center_axis',(1.,1.53063836115601E-16,-2.73691106313441E-48)) ;
#94405 = DIRECTION('ref_axis',(-1.53063836115601E-16,1.,4.18922106430579E-64)) ;
#94406 = DIRECTION('center_axis',(-1.,0.,0.)) ;
#94407 = DIRECTION('ref_axis',(0.,0.,1.)) ;
#94408 = DIRECTION('center_axis',(1.,1.53063836115601E-16,0.)) ;
#94409 = DIRECTION('ref_axis',(1.53063836115601E-16,-1.,0.)) ;
#94410 = DIRECTION('center_axis',(0.,1.,0.)) ;
#94411 = DIRECTION('ref_axis',(1.,0.,0.)) ;
#94412 = DIRECTION('center_axis',(-1.,-2.16840434497101E-16,0.)) ;
#94413 = DIRECTION('ref_axis',(0.,-1.,0.)) ;
#94414 = DIRECTION('center_axis',(0.,0.,-1.)) ;
#94415 = DIRECTION('ref_axis',(1.,0.,0.)) ;
#94416 = DIRECTION('center_axis',(-1.25542992828747E-32,1.020425574104E-16,
1.)) ;
#94417 = DIRECTION('ref_axis',(0.,-1.,0.)) ;
#94418 = DIRECTION('center_axis',(0.,-1.,0.)) ;
#94419 = DIRECTION('ref_axis',(-6.50521303491307E-15,0.,1.)) ;
#94420 = DIRECTION('center_axis',(-1.,0.,0.)) ;
#94421 = DIRECTION('ref_axis',(0.,0.,-1.)) ;
#94422 = DIRECTION('center_axis',(-1.,-1.53063836115601E-16,0.)) ;
#94423 = DIRECTION('ref_axis',(0.,-1.,0.)) ;
#94424 = DIRECTION('center_axis',(0.,-1.,0.)) ;
#94425 = DIRECTION('ref_axis',(0.,0.,1.)) ;
#94426 = DIRECTION('center_axis',(0.,0.,-1.)) ;
#94427 = DIRECTION('ref_axis',(-1.,0.,0.)) ;
#94428 = DIRECTION('center_axis',(0.,0.,-1.)) ;
#94429 = DIRECTION('ref_axis',(-1.,0.,0.)) ;
#94430 = DIRECTION('center_axis',(1.,1.53063836115601E-16,-3.06472600140763E-33)) ;
#94431 = DIRECTION('ref_axis',(-1.53063836115601E-16,1.,4.69098718418678E-49)) ;
#94432 = DIRECTION('center_axis',(-1.,0.,0.)) ;
#94433 = DIRECTION('ref_axis',(0.,0.,1.)) ;
#94434 = DIRECTION('center_axis',(-1.53063836115601E-16,1.,-1.020425574104E-16)) ;
#94435 = DIRECTION('ref_axis',(-1.,-1.53063836115601E-16,1.3684555315672E-47)) ;
#94436 = DIRECTION('',(1.53063836115601E-16,-1.,1.020425574104E-16)) ;
#94437 = DIRECTION('center_axis',(0.,-1.,0.)) ;
#94438 = DIRECTION('ref_axis',(0.,0.,-1.)) ;
#94439 = DIRECTION('center_axis',(-1.53063836115601E-16,1.,-1.30104260698261E-16)) ;
#94440 = DIRECTION('ref_axis',(-1.,-1.53063836115601E-16,1.99142572374599E-32)) ;
#94441 = DIRECTION('center_axis',(0.,-1.,0.)) ;
#94442 = DIRECTION('ref_axis',(0.,0.,-1.)) ;
#94443 = DIRECTION('center_axis',(-1.,-1.53063836115601E-16,2.73691106313441E-48)) ;
#94444 = DIRECTION('ref_axis',(1.53063836115601E-16,-1.,-4.18922106430579E-64)) ;
#94445 = DIRECTION('center_axis',(1.,2.16840434497101E-16,0.)) ;
#94446 = DIRECTION('ref_axis',(2.16840434497101E-16,-1.,0.)) ;
#94447 = DIRECTION('center_axis',(-1.,0.,2.16840434497102E-15)) ;
#94448 = DIRECTION('ref_axis',(2.16840434497102E-15,0.,1.)) ;
#94449 = DIRECTION('center_axis',(-1.,-2.16840434497101E-16,0.)) ;
#94450 = DIRECTION('ref_axis',(0.,-1.,0.)) ;
#94451 = DIRECTION('center_axis',(0.,0.,1.)) ;
#94452 = DIRECTION('ref_axis',(-1.,0.,0.)) ;
#94453 = DIRECTION('center_axis',(0.,1.,0.)) ;
#94454 = DIRECTION('ref_axis',(1.,0.,0.)) ;
#94455 = DIRECTION('center_axis',(0.,1.,0.)) ;
#94456 = DIRECTION('ref_axis',(0.,0.,-1.)) ;
#94457 = DIRECTION('center_axis',(1.,0.,0.)) ;
#94458 = DIRECTION('ref_axis',(0.,-1.,0.)) ;
#94459 = DIRECTION('center_axis',(1.,6.50521303491304E-15,0.)) ;
#94460 = DIRECTION('ref_axis',(-6.50521303491304E-15,1.,0.)) ;
#94461 = DIRECTION('center_axis',(8.67361737988403E-15,1.,0.)) ;
#94462 = DIRECTION('ref_axis',(-1.,8.67361737988403E-15,0.)) ;
#94463 = DIRECTION('center_axis',(1.2303003375722E-16,-1.,1.020425574104E-16)) ;
#94464 = DIRECTION('ref_axis',(1.,1.2303003375722E-16,-1.25542992828747E-32)) ;
#94465 = DIRECTION('center_axis',(0.,1.,0.)) ;
#94466 = DIRECTION('ref_axis',(0.,0.,1.)) ;
#94467 = DIRECTION('center_axis',(0.,1.,0.)) ;
#94468 = DIRECTION('ref_axis',(1.,0.,0.)) ;
#94469 = DIRECTION('center_axis',(1.,1.2303003375722E-16,0.)) ;
#94470 = DIRECTION('ref_axis',(1.2303003375722E-16,-1.,0.)) ;
#94471 = DIRECTION('center_axis',(0.,0.,1.)) ;
#94472 = DIRECTION('ref_axis',(-1.,0.,0.)) ;
#94473 = DIRECTION('center_axis',(0.,1.,0.)) ;
#94474 = DIRECTION('ref_axis',(1.,0.,0.)) ;
#94475 = DIRECTION('center_axis',(0.,0.,-1.)) ;
#94476 = DIRECTION('ref_axis',(1.,0.,0.)) ;
#94477 = DIRECTION('center_axis',(0.,0.,-1.)) ;
#94478 = DIRECTION('ref_axis',(-1.,0.,0.)) ;
#94479 = DIRECTION('center_axis',(0.,0.,1.)) ;
#94480 = DIRECTION('ref_axis',(1.,0.,0.)) ;
#94481 = DIRECTION('center_axis',(-2.16840434497101E-16,1.,-1.020425574104E-16)) ;
#94482 = DIRECTION('ref_axis',(-1.,-2.16840434497101E-16,5.47382212626882E-48)) ;
#94483 = DIRECTION('center_axis',(0.,1.,0.)) ;
#94484 = DIRECTION('ref_axis',(0.,0.,-1.)) ;
#94485 = DIRECTION('center_axis',(1.,0.,1.25542992828747E-32)) ;
#94486 = DIRECTION('ref_axis',(1.25542992828747E-32,0.,-1.)) ;
#94487 = DIRECTION('center_axis',(1.,0.,0.)) ;
#94488 = DIRECTION('ref_axis',(0.,0.,-1.)) ;
#94489 = DIRECTION('center_axis',(-1.,-1.2303003375722E-16,0.)) ;
#94490 = DIRECTION('ref_axis',(0.,-1.,0.)) ;
#94491 = DIRECTION('center_axis',(0.,0.,-1.)) ;
#94492 = DIRECTION('ref_axis',(1.,0.,0.)) ;
#94493 = DIRECTION('center_axis',(0.,0.,-1.)) ;
#94494 = DIRECTION('ref_axis',(-1.,0.,0.)) ;
#94495 = DIRECTION('',(0.,0.,1.)) ;
#94496 = DIRECTION('center_axis',(0.,0.,1.)) ;
#94497 = DIRECTION('ref_axis',(1.,0.,0.)) ;
#94498 = DIRECTION('center_axis',(0.,0.,1.)) ;
#94499 = DIRECTION('ref_axis',(1.,0.,0.)) ;
#94500 = DIRECTION('center_axis',(6.27714964143733E-33,-5.10212787052002E-17,
-1.)) ;
#94501 = DIRECTION('ref_axis',(3.20268201330022E-49,1.,-5.10212787052002E-17)) ;
#94502 = DIRECTION('center_axis',(1.,1.53063836115601E-16,-1.53236300070382E-33)) ;
#94503 = DIRECTION('ref_axis',(-1.53063836115601E-16,1.,2.34549359209339E-49)) ;
#94504 = DIRECTION('center_axis',(-1.,0.,0.)) ;
#94505 = DIRECTION('ref_axis',(0.,0.,1.)) ;
#94506 = DIRECTION('center_axis',(1.,0.,0.)) ;
#94507 = DIRECTION('ref_axis',(0.,0.,-1.)) ;
#94508 = DIRECTION('center_axis',(0.,1.,0.)) ;
#94509 = DIRECTION('ref_axis',(1.,0.,0.)) ;
#94510 = DIRECTION('center_axis',(-4.33680868994202E-15,1.,0.)) ;
#94511 = DIRECTION('ref_axis',(1.,4.33680868994202E-15,0.)) ;
#94512 = DIRECTION('center_axis',(0.,-1.,0.)) ;
#94513 = DIRECTION('ref_axis',(0.,0.,-1.)) ;
#94514 = DIRECTION('center_axis',(0.,0.,-1.)) ;
#94515 = DIRECTION('ref_axis',(1.,0.,0.)) ;
#94516 = DIRECTION('center_axis',(0.,0.,1.)) ;
#94517 = DIRECTION('ref_axis',(1.,0.,0.)) ;
#94518 = DIRECTION('center_axis',(0.,0.,-1.)) ;
#94519 = DIRECTION('ref_axis',(-1.,0.,0.)) ;
#94520 = DIRECTION('center_axis',(0.,1.,0.)) ;
#94521 = DIRECTION('ref_axis',(1.,0.,0.)) ;
#94522 = DIRECTION('center_axis',(1.,1.2303003375722E-16,0.)) ;
#94523 = DIRECTION('ref_axis',(1.2303003375722E-16,-1.,0.)) ;
#94524 = DIRECTION('center_axis',(0.,1.,0.)) ;
#94525 = DIRECTION('ref_axis',(-6.50521303491307E-15,0.,-1.)) ;
#94526 = DIRECTION('center_axis',(6.27714964143733E-33,-5.10212787052002E-17,
-1.)) ;
#94527 = DIRECTION('ref_axis',(0.,1.,0.)) ;
#94528 = DIRECTION('center_axis',(0.,-1.,0.)) ;
#94529 = DIRECTION('ref_axis',(0.,0.,1.)) ;
#94530 = DIRECTION('center_axis',(2.16840434497101E-16,-1.,5.10212787052002E-17)) ;
#94531 = DIRECTION('ref_axis',(1.,2.16840434497101E-16,-5.47382212626882E-48)) ;
#94532 = DIRECTION('center_axis',(0.,1.,0.)) ;
#94533 = DIRECTION('ref_axis',(0.,0.,-1.)) ;
#94534 = DIRECTION('center_axis',(0.,0.,1.)) ;
#94535 = DIRECTION('ref_axis',(1.,0.,0.)) ;
#94536 = DIRECTION('center_axis',(0.,0.,-1.)) ;
#94537 = DIRECTION('ref_axis',(-1.,0.,0.)) ;
#94538 = DIRECTION('center_axis',(-1.,-1.2303003375722E-16,0.)) ;
#94539 = DIRECTION('ref_axis',(0.,-1.,0.)) ;
#94540 = DIRECTION('center_axis',(0.,-1.,0.)) ;
#94541 = DIRECTION('ref_axis',(0.,0.,1.)) ;
#94542 = DIRECTION('center_axis',(1.53063836115601E-16,-1.,5.10212787052002E-17)) ;
#94543 = DIRECTION('ref_axis',(1.,1.53063836115601E-16,-6.84227765783602E-48)) ;
#94544 = DIRECTION('',(-1.53063836115601E-16,1.,-5.10212787052002E-17)) ;
#94545 = DIRECTION('center_axis',(0.,-1.,0.)) ;
#94546 = DIRECTION('ref_axis',(0.,0.,-1.)) ;
#94547 = DIRECTION('center_axis',(-1.,0.,0.)) ;
#94548 = DIRECTION('ref_axis',(0.,0.,-1.)) ;
#94549 = DIRECTION('center_axis',(-1.2303003375722E-16,1.,-5.10212787052002E-17)) ;
#94550 = DIRECTION('ref_axis',(-1.,-1.2303003375722E-16,6.27714964143733E-33)) ;
#94551 = DIRECTION('center_axis',(-8.67361737988403E-15,-1.,0.)) ;
#94552 = DIRECTION('ref_axis',(1.,-8.67361737988403E-15,0.)) ;
#94553 = DIRECTION('center_axis',(1.,0.,6.27714964143733E-33)) ;
#94554 = DIRECTION('ref_axis',(6.27714964143733E-33,0.,-1.)) ;
#94555 = DIRECTION('center_axis',(-1.,0.,-6.50521303491307E-15)) ;
#94556 = DIRECTION('ref_axis',(-6.50521303491307E-15,0.,1.)) ;
#94557 = DIRECTION('center_axis',(1.,0.,0.)) ;
#94558 = DIRECTION('ref_axis',(0.,1.,0.)) ;
#94559 = DIRECTION('center_axis',(0.,0.,-1.)) ;
#94560 = DIRECTION('ref_axis',(-1.,0.,0.)) ;
#94561 = DIRECTION('center_axis',(0.,0.,1.)) ;
#94562 = DIRECTION('ref_axis',(1.,0.,0.)) ;
#94563 = DIRECTION('center_axis',(0.,0.,-1.)) ;
#94564 = DIRECTION('ref_axis',(-1.,0.,0.)) ;
#94565 = DIRECTION('center_axis',(-1.,0.,0.)) ;
#94566 = DIRECTION('ref_axis',(0.,0.,1.)) ;
#94567 = DIRECTION('center_axis',(0.,-1.,0.)) ;
#94568 = DIRECTION('ref_axis',(0.,0.,-1.)) ;
#94569 = DIRECTION('center_axis',(0.,1.,0.)) ;
#94570 = DIRECTION('ref_axis',(0.,0.,1.)) ;
#94571 = DIRECTION('center_axis',(0.,1.,-6.50521303491307E-15)) ;
#94572 = DIRECTION('ref_axis',(0.,6.50521303491307E-15,1.)) ;
#94573 = DIRECTION('center_axis',(0.,-1.,0.)) ;
#94574 = DIRECTION('ref_axis',(0.,0.,-1.)) ;
#94575 = DIRECTION('center_axis',(0.,-1.,0.)) ;
#94576 = DIRECTION('ref_axis',(0.,0.,-1.)) ;
#94577 = DIRECTION('center_axis',(0.,-1.,-1.07081696047951E-16)) ;
#94578 = DIRECTION('ref_axis',(0.,1.07081696047951E-16,-1.)) ;
#94579 = DIRECTION('center_axis',(0.,1.,0.)) ;
#94580 = DIRECTION('ref_axis',(0.,0.,1.)) ;
#94581 = DIRECTION('center_axis',(-1.,0.,0.)) ;
#94582 = DIRECTION('ref_axis',(0.,0.,1.)) ;
#94583 = DIRECTION('center_axis',(0.,0.,1.)) ;
#94584 = DIRECTION('ref_axis',(1.,0.,0.)) ;
#94585 = DIRECTION('center_axis',(0.,1.,0.)) ;
#94586 = DIRECTION('ref_axis',(0.,0.,1.)) ;
#94587 = DIRECTION('center_axis',(0.,0.,-1.)) ;
#94588 = DIRECTION('ref_axis',(-1.,0.,0.)) ;
#94589 = DIRECTION('center_axis',(0.,0.,1.)) ;
#94590 = DIRECTION('ref_axis',(1.,0.,0.)) ;
#94591 = DIRECTION('center_axis',(0.,0.,1.)) ;
#94592 = DIRECTION('ref_axis',(1.,0.,0.)) ;
#94593 = DIRECTION('center_axis',(0.,0.,1.)) ;
#94594 = DIRECTION('ref_axis',(1.,0.,0.)) ;
#94595 = DIRECTION('center_axis',(0.,0.,-1.)) ;
#94596 = DIRECTION('ref_axis',(-1.,0.,0.)) ;
#94597 = DIRECTION('center_axis',(0.,1.,0.)) ;
#94598 = DIRECTION('ref_axis',(0.,0.,1.)) ;
#94599 = DIRECTION('center_axis',(0.,-0.707106781186558,0.707106781186537)) ;
#94600 = DIRECTION('ref_axis',(0.,-0.707106781186537,-0.707106781186558)) ;
#94601 = DIRECTION('center_axis',(0.,1.,0.)) ;
#94602 = DIRECTION('ref_axis',(0.,0.,1.)) ;
#94603 = DIRECTION('center_axis',(0.,-0.514231796959093,-0.857651245551607)) ;
#94604 = DIRECTION('ref_axis',(0.,0.857651245551607,-0.514231796959093)) ;
#94605 = DIRECTION('center_axis',(0.,-0.707106781186548,0.707106781186547)) ;
#94606 = DIRECTION('ref_axis',(0.,-0.707106781186547,-0.707106781186548)) ;
#94607 = DIRECTION('center_axis',(0.,-0.707106781186548,0.707106781186548)) ;
#94608 = DIRECTION('ref_axis',(0.,-0.707106781186548,-0.707106781186548)) ;
#94609 = DIRECTION('center_axis',(-1.,0.,0.)) ;
#94610 = DIRECTION('ref_axis',(0.,0.,1.)) ;
#94611 = DIRECTION('center_axis',(0.,0.514231796959095,-0.857651245551606)) ;
#94612 = DIRECTION('ref_axis',(0.,0.857651245551606,0.514231796959095)) ;
#94613 = DIRECTION('center_axis',(0.,1.,0.)) ;
#94614 = DIRECTION('ref_axis',(0.,0.,1.)) ;
#94615 = DIRECTION('center_axis',(0.,0.,-1.)) ;
#94616 = DIRECTION('ref_axis',(-1.,0.,0.)) ;
#94617 = DIRECTION('center_axis',(0.,1.,0.)) ;
#94618 = DIRECTION('ref_axis',(0.,0.,1.)) ;
#94619 = DIRECTION('center_axis',(0.,0.,-1.)) ;
#94620 = DIRECTION('ref_axis',(-1.,0.,0.)) ;
#94621 = DIRECTION('center_axis',(0.,0.,-1.)) ;
#94622 = DIRECTION('ref_axis',(-1.,0.,0.)) ;
#94623 = DIRECTION('center_axis',(0.,0.,1.)) ;
#94624 = DIRECTION('ref_axis',(1.,0.,0.)) ;
#94625 = DIRECTION('center_axis',(0.,0.,-1.)) ;
#94626 = DIRECTION('ref_axis',(-1.,0.,0.)) ;
#94627 = DIRECTION('center_axis',(0.,1.,0.)) ;
#94628 = DIRECTION('ref_axis',(0.,0.,1.)) ;
#94629 = DIRECTION('center_axis',(0.,-1.,8.67361737988409E-15)) ;
#94630 = DIRECTION('ref_axis',(0.,-8.67361737988409E-15,-1.)) ;
#94631 = DIRECTION('center_axis',(0.,0.707106781186546,0.707106781186549)) ;
#94632 = DIRECTION('ref_axis',(0.,-0.707106781186549,0.707106781186546)) ;
#94633 = DIRECTION('center_axis',(0.,0.707106781186537,0.707106781186558)) ;
#94634 = DIRECTION('ref_axis',(0.,-0.707106781186558,0.707106781186537)) ;
#94635 = DIRECTION('center_axis',(0.,1.,1.07081696047951E-16)) ;
#94636 = DIRECTION('ref_axis',(0.,-1.07081696047951E-16,1.)) ;
#94637 = DIRECTION('center_axis',(0.,-1.,0.)) ;
#94638 = DIRECTION('ref_axis',(0.,0.,-1.)) ;
#94639 = DIRECTION('center_axis',(0.,1.,0.)) ;
#94640 = DIRECTION('ref_axis',(0.,0.,1.)) ;
#94641 = DIRECTION('center_axis',(0.,0.,1.)) ;
#94642 = DIRECTION('ref_axis',(1.,0.,0.)) ;
#94643 = DIRECTION('center_axis',(0.,1.,0.)) ;
#94644 = DIRECTION('ref_axis',(0.,0.,1.)) ;
#94645 = DIRECTION('center_axis',(0.,0.,1.)) ;
#94646 = DIRECTION('ref_axis',(1.,0.,0.)) ;
#94647 = DIRECTION('center_axis',(0.,3.99416362155027E-15,1.)) ;
#94648 = DIRECTION('ref_axis',(0.,-1.,3.99416362155027E-15)) ;
#94649 = DIRECTION('center_axis',(0.,0.,1.)) ;
#94650 = DIRECTION('ref_axis',(1.,0.,0.)) ;
#94651 = DIRECTION('center_axis',(0.,0.,-1.)) ;
#94652 = DIRECTION('ref_axis',(-1.,0.,0.)) ;
#94653 = DIRECTION('center_axis',(0.,0.,1.)) ;
#94654 = DIRECTION('ref_axis',(1.,0.,0.)) ;
#94655 = DIRECTION('center_axis',(-1.,0.,0.)) ;
#94656 = DIRECTION('ref_axis',(0.,0.,1.)) ;
#94657 = DIRECTION('center_axis',(0.,1.,0.)) ;
#94658 = DIRECTION('ref_axis',(0.,0.,1.)) ;
#94659 = DIRECTION('center_axis',(-1.,0.,0.)) ;
#94660 = DIRECTION('ref_axis',(0.,0.,1.)) ;
#94661 = DIRECTION('center_axis',(0.,-1.,0.)) ;
#94662 = DIRECTION('ref_axis',(0.,0.,-1.)) ;
#94663 = DIRECTION('center_axis',(0.,1.,0.)) ;
#94664 = DIRECTION('ref_axis',(0.,0.,1.)) ;
#94665 = DIRECTION('center_axis',(1.53063836115601E-16,-1.,-1.30104260698261E-16)) ;
#94666 = DIRECTION('ref_axis',(1.,1.53063836115601E-16,1.99142572374599E-32)) ;
#94667 = DIRECTION('center_axis',(0.,1.,0.)) ;
#94668 = DIRECTION('ref_axis',(0.,0.,1.)) ;
#94669 = DIRECTION('center_axis',(0.,-1.,0.)) ;
#94670 = DIRECTION('ref_axis',(0.,0.,-1.)) ;
#94671 = DIRECTION('center_axis',(1.,1.53063836115601E-16,2.73691106313441E-48)) ;
#94672 = DIRECTION('ref_axis',(-1.53063836115601E-16,1.,-4.18922106430579E-64)) ;
#94673 = DIRECTION('center_axis',(-1.,0.,0.)) ;
#94674 = DIRECTION('ref_axis',(0.,0.,1.)) ;
#94675 = DIRECTION('center_axis',(1.,1.53063836115601E-16,0.)) ;
#94676 = DIRECTION('ref_axis',(1.53063836115601E-16,-1.,0.)) ;
#94677 = DIRECTION('center_axis',(0.,1.,0.)) ;
#94678 = DIRECTION('ref_axis',(1.,0.,0.)) ;
#94679 = DIRECTION('center_axis',(0.,1.,0.)) ;
#94680 = DIRECTION('ref_axis',(0.,0.,-1.)) ;
#94681 = DIRECTION('center_axis',(0.,0.,1.)) ;
#94682 = DIRECTION('ref_axis',(-1.,0.,0.)) ;
#94683 = DIRECTION('center_axis',(0.,1.,0.)) ;
#94684 = DIRECTION('ref_axis',(1.,0.,0.)) ;
#94685 = DIRECTION('center_axis',(0.,0.,1.)) ;
#94686 = DIRECTION('ref_axis',(-1.,0.,0.)) ;
#94687 = DIRECTION('center_axis',(1.,1.0842021724855E-15,0.)) ;
#94688 = DIRECTION('ref_axis',(1.0842021724855E-15,-1.,0.)) ;
#94689 = DIRECTION('center_axis',(-1.,-1.53063836115601E-16,0.)) ;
#94690 = DIRECTION('ref_axis',(0.,-1.,0.)) ;
#94691 = DIRECTION('center_axis',(0.,0.,-1.)) ;
#94692 = DIRECTION('ref_axis',(1.,0.,0.)) ;
#94693 = DIRECTION('center_axis',(0.,0.,-1.)) ;
#94694 = DIRECTION('ref_axis',(0.804034447892626,0.594582716366697,0.)) ;
#94695 = DIRECTION('center_axis',(0.,0.,1.)) ;
#94696 = DIRECTION('ref_axis',(1.,0.,0.)) ;
#94697 = DIRECTION('',(0.,0.,-1.)) ;
#94698 = DIRECTION('center_axis',(-2.16840434497101E-16,1.,1.30104260698261E-16)) ;
#94699 = DIRECTION('ref_axis',(1.,2.16840434497101E-16,1.22464679914735E-16)) ;
#94700 = DIRECTION('',(-2.16840434497101E-16,1.,1.30104260698261E-16)) ;
#94701 = DIRECTION('center_axis',(0.,1.,0.)) ;
#94702 = DIRECTION('ref_axis',(0.,0.,1.)) ;
#94703 = DIRECTION('center_axis',(-1.,-1.53063836115601E-16,-2.73691106313441E-48)) ;
#94704 = DIRECTION('ref_axis',(1.53063836115601E-16,-1.,4.18922106430579E-64)) ;
#94705 = DIRECTION('center_axis',(1.,2.16840434497101E-16,0.)) ;
#94706 = DIRECTION('ref_axis',(2.16840434497101E-16,-1.,0.)) ;
#94707 = DIRECTION('center_axis',(0.,0.,1.)) ;
#94708 = DIRECTION('ref_axis',(1.,0.,0.)) ;
#94709 = DIRECTION('center_axis',(-1.25542992828747E-32,1.020425574104E-16,
1.)) ;
#94710 = DIRECTION('ref_axis',(-1.28107280532009E-48,-1.,1.020425574104E-16)) ;
#94711 = DIRECTION('center_axis',(0.,0.,1.)) ;
#94712 = DIRECTION('ref_axis',(1.,0.,0.)) ;
#94713 = DIRECTION('center_axis',(0.,0.,-1.)) ;
#94714 = DIRECTION('ref_axis',(-1.,0.,0.)) ;
#94715 = DIRECTION('center_axis',(1.,1.53063836115601E-16,-2.73691106313441E-48)) ;
#94716 = DIRECTION('ref_axis',(-1.53063836115601E-16,1.,4.18922106430579E-64)) ;
#94717 = DIRECTION('center_axis',(-1.,0.,0.)) ;
#94718 = DIRECTION('ref_axis',(0.,0.,1.)) ;
#94719 = DIRECTION('center_axis',(1.,1.53063836115601E-16,0.)) ;
#94720 = DIRECTION('ref_axis',(1.53063836115601E-16,-1.,0.)) ;
#94721 = DIRECTION('center_axis',(0.,1.,0.)) ;
#94722 = DIRECTION('ref_axis',(1.,0.,0.)) ;
#94723 = DIRECTION('center_axis',(-1.,-2.16840434497101E-16,0.)) ;
#94724 = DIRECTION('ref_axis',(0.,-1.,0.)) ;
#94725 = DIRECTION('center_axis',(0.,0.,-1.)) ;
#94726 = DIRECTION('ref_axis',(1.,0.,0.)) ;
#94727 = DIRECTION('center_axis',(-1.25542992828747E-32,1.020425574104E-16,
1.)) ;
#94728 = DIRECTION('ref_axis',(0.,-1.,0.)) ;
#94729 = DIRECTION('center_axis',(0.,-1.,0.)) ;
#94730 = DIRECTION('ref_axis',(-6.50521303491307E-15,0.,1.)) ;
#94731 = DIRECTION('center_axis',(-1.,0.,0.)) ;
#94732 = DIRECTION('ref_axis',(0.,0.,-1.)) ;
#94733 = DIRECTION('center_axis',(-1.,-1.53063836115601E-16,0.)) ;
#94734 = DIRECTION('ref_axis',(0.,-1.,0.)) ;
#94735 = DIRECTION('center_axis',(0.,-1.,0.)) ;
#94736 = DIRECTION('ref_axis',(0.,0.,1.)) ;
#94737 = DIRECTION('center_axis',(0.,0.,-1.)) ;
#94738 = DIRECTION('ref_axis',(-1.,0.,0.)) ;
#94739 = DIRECTION('center_axis',(0.,0.,-1.)) ;
#94740 = DIRECTION('ref_axis',(-1.,0.,0.)) ;
#94741 = DIRECTION('center_axis',(1.,1.53063836115601E-16,-3.06472600140763E-33)) ;
#94742 = DIRECTION('ref_axis',(-1.53063836115601E-16,1.,4.69098718418678E-49)) ;
#94743 = DIRECTION('center_axis',(-1.,0.,0.)) ;
#94744 = DIRECTION('ref_axis',(0.,0.,1.)) ;
#94745 = DIRECTION('center_axis',(-1.53063836115601E-16,1.,-1.020425574104E-16)) ;
#94746 = DIRECTION('ref_axis',(-1.,-1.53063836115601E-16,1.3684555315672E-47)) ;
#94747 = DIRECTION('',(1.53063836115601E-16,-1.,1.020425574104E-16)) ;
#94748 = DIRECTION('center_axis',(0.,-1.,0.)) ;
#94749 = DIRECTION('ref_axis',(0.,0.,-1.)) ;
#94750 = DIRECTION('center_axis',(-1.53063836115601E-16,1.,-1.30104260698261E-16)) ;
#94751 = DIRECTION('ref_axis',(-1.,-1.53063836115601E-16,1.99142572374599E-32)) ;
#94752 = DIRECTION('center_axis',(0.,-1.,0.)) ;
#94753 = DIRECTION('ref_axis',(0.,0.,-1.)) ;
#94754 = DIRECTION('center_axis',(-1.,-1.53063836115601E-16,2.73691106313441E-48)) ;
#94755 = DIRECTION('ref_axis',(1.53063836115601E-16,-1.,-4.18922106430579E-64)) ;
#94756 = DIRECTION('center_axis',(1.,2.16840434497101E-16,0.)) ;
#94757 = DIRECTION('ref_axis',(2.16840434497101E-16,-1.,0.)) ;
#94758 = DIRECTION('center_axis',(-1.,0.,2.16840434497102E-15)) ;
#94759 = DIRECTION('ref_axis',(2.16840434497102E-15,0.,1.)) ;
#94760 = DIRECTION('center_axis',(-1.,-2.16840434497101E-16,0.)) ;
#94761 = DIRECTION('ref_axis',(0.,-1.,0.)) ;
#94762 = DIRECTION('center_axis',(0.,0.,1.)) ;
#94763 = DIRECTION('ref_axis',(-1.,0.,0.)) ;
#94764 = DIRECTION('center_axis',(0.,1.,0.)) ;
#94765 = DIRECTION('ref_axis',(1.,0.,0.)) ;
#94766 = DIRECTION('center_axis',(0.,1.,0.)) ;
#94767 = DIRECTION('ref_axis',(0.,0.,-1.)) ;
#94768 = DIRECTION('center_axis',(1.,0.,0.)) ;
#94769 = DIRECTION('ref_axis',(0.,-1.,0.)) ;
#94770 = DIRECTION('center_axis',(1.,6.50521303491304E-15,0.)) ;
#94771 = DIRECTION('ref_axis',(-6.50521303491304E-15,1.,0.)) ;
#94772 = DIRECTION('center_axis',(8.67361737988403E-15,1.,0.)) ;
#94773 = DIRECTION('ref_axis',(-1.,8.67361737988403E-15,0.)) ;
#94774 = DIRECTION('center_axis',(1.2303003375722E-16,-1.,1.020425574104E-16)) ;
#94775 = DIRECTION('ref_axis',(1.,1.2303003375722E-16,-1.25542992828747E-32)) ;
#94776 = DIRECTION('center_axis',(0.,1.,0.)) ;
#94777 = DIRECTION('ref_axis',(0.,0.,1.)) ;
#94778 = DIRECTION('center_axis',(0.,1.,0.)) ;
#94779 = DIRECTION('ref_axis',(1.,0.,0.)) ;
#94780 = DIRECTION('center_axis',(1.,1.2303003375722E-16,0.)) ;
#94781 = DIRECTION('ref_axis',(1.2303003375722E-16,-1.,0.)) ;
#94782 = DIRECTION('center_axis',(0.,0.,1.)) ;
#94783 = DIRECTION('ref_axis',(-1.,0.,0.)) ;
#94784 = DIRECTION('center_axis',(0.,1.,0.)) ;
#94785 = DIRECTION('ref_axis',(1.,0.,0.)) ;
#94786 = DIRECTION('center_axis',(0.,0.,-1.)) ;
#94787 = DIRECTION('ref_axis',(1.,0.,0.)) ;
#94788 = DIRECTION('center_axis',(0.,0.,-1.)) ;
#94789 = DIRECTION('ref_axis',(-1.,0.,0.)) ;
#94790 = DIRECTION('center_axis',(0.,0.,1.)) ;
#94791 = DIRECTION('ref_axis',(1.,0.,0.)) ;
#94792 = DIRECTION('center_axis',(-2.16840434497101E-16,1.,-1.020425574104E-16)) ;
#94793 = DIRECTION('ref_axis',(-1.,-2.16840434497101E-16,5.47382212626882E-48)) ;
#94794 = DIRECTION('center_axis',(0.,1.,0.)) ;
#94795 = DIRECTION('ref_axis',(0.,0.,-1.)) ;
#94796 = DIRECTION('center_axis',(1.,0.,1.25542992828747E-32)) ;
#94797 = DIRECTION('ref_axis',(1.25542992828747E-32,0.,-1.)) ;
#94798 = DIRECTION('center_axis',(1.,0.,0.)) ;
#94799 = DIRECTION('ref_axis',(0.,0.,-1.)) ;
#94800 = DIRECTION('center_axis',(-1.,-1.2303003375722E-16,0.)) ;
#94801 = DIRECTION('ref_axis',(0.,-1.,0.)) ;
#94802 = DIRECTION('center_axis',(0.,0.,-1.)) ;
#94803 = DIRECTION('ref_axis',(1.,0.,0.)) ;
#94804 = DIRECTION('center_axis',(0.,0.,-1.)) ;
#94805 = DIRECTION('ref_axis',(-1.,0.,0.)) ;
#94806 = DIRECTION('',(0.,0.,1.)) ;
#94807 = DIRECTION('center_axis',(0.,0.,1.)) ;
#94808 = DIRECTION('ref_axis',(1.,0.,0.)) ;
#94809 = DIRECTION('center_axis',(0.,0.,1.)) ;
#94810 = DIRECTION('ref_axis',(1.,0.,0.)) ;
#94811 = DIRECTION('center_axis',(6.27714964143733E-33,-5.10212787052002E-17,
-1.)) ;
#94812 = DIRECTION('ref_axis',(3.20268201330022E-49,1.,-5.10212787052002E-17)) ;
#94813 = DIRECTION('center_axis',(1.,1.53063836115601E-16,-1.53236300070382E-33)) ;
#94814 = DIRECTION('ref_axis',(-1.53063836115601E-16,1.,2.34549359209339E-49)) ;
#94815 = DIRECTION('center_axis',(-1.,0.,0.)) ;
#94816 = DIRECTION('ref_axis',(0.,0.,1.)) ;
#94817 = DIRECTION('center_axis',(1.,0.,0.)) ;
#94818 = DIRECTION('ref_axis',(0.,0.,-1.)) ;
#94819 = DIRECTION('center_axis',(0.,1.,0.)) ;
#94820 = DIRECTION('ref_axis',(1.,0.,0.)) ;
#94821 = DIRECTION('center_axis',(-4.33680868994202E-15,1.,0.)) ;
#94822 = DIRECTION('ref_axis',(1.,4.33680868994202E-15,0.)) ;
#94823 = DIRECTION('center_axis',(0.,-1.,0.)) ;
#94824 = DIRECTION('ref_axis',(0.,0.,-1.)) ;
#94825 = DIRECTION('center_axis',(0.,0.,-1.)) ;
#94826 = DIRECTION('ref_axis',(1.,0.,0.)) ;
#94827 = DIRECTION('center_axis',(0.,0.,1.)) ;
#94828 = DIRECTION('ref_axis',(1.,0.,0.)) ;
#94829 = DIRECTION('center_axis',(0.,0.,-1.)) ;
#94830 = DIRECTION('ref_axis',(-1.,0.,0.)) ;
#94831 = DIRECTION('center_axis',(0.,1.,0.)) ;
#94832 = DIRECTION('ref_axis',(1.,0.,0.)) ;
#94833 = DIRECTION('center_axis',(1.,1.2303003375722E-16,0.)) ;
#94834 = DIRECTION('ref_axis',(1.2303003375722E-16,-1.,0.)) ;
#94835 = DIRECTION('center_axis',(0.,1.,0.)) ;
#94836 = DIRECTION('ref_axis',(-6.50521303491307E-15,0.,-1.)) ;
#94837 = DIRECTION('center_axis',(6.27714964143733E-33,-5.10212787052002E-17,
-1.)) ;
#94838 = DIRECTION('ref_axis',(0.,1.,0.)) ;
#94839 = DIRECTION('center_axis',(0.,-1.,0.)) ;
#94840 = DIRECTION('ref_axis',(0.,0.,1.)) ;
#94841 = DIRECTION('center_axis',(2.16840434497101E-16,-1.,5.10212787052002E-17)) ;
#94842 = DIRECTION('ref_axis',(1.,2.16840434497101E-16,-5.47382212626882E-48)) ;
#94843 = DIRECTION('center_axis',(0.,1.,0.)) ;
#94844 = DIRECTION('ref_axis',(0.,0.,-1.)) ;
#94845 = DIRECTION('center_axis',(0.,0.,1.)) ;
#94846 = DIRECTION('ref_axis',(1.,0.,0.)) ;
#94847 = DIRECTION('center_axis',(0.,0.,-1.)) ;
#94848 = DIRECTION('ref_axis',(-1.,0.,0.)) ;
#94849 = DIRECTION('center_axis',(-1.,-1.2303003375722E-16,0.)) ;
#94850 = DIRECTION('ref_axis',(0.,-1.,0.)) ;
#94851 = DIRECTION('center_axis',(0.,-1.,0.)) ;
#94852 = DIRECTION('ref_axis',(0.,0.,1.)) ;
#94853 = DIRECTION('center_axis',(1.53063836115601E-16,-1.,5.10212787052002E-17)) ;
#94854 = DIRECTION('ref_axis',(1.,1.53063836115601E-16,-6.84227765783602E-48)) ;
#94855 = DIRECTION('',(-1.53063836115601E-16,1.,-5.10212787052002E-17)) ;
#94856 = DIRECTION('center_axis',(0.,-1.,0.)) ;
#94857 = DIRECTION('ref_axis',(0.,0.,-1.)) ;
#94858 = DIRECTION('center_axis',(-1.,0.,0.)) ;
#94859 = DIRECTION('ref_axis',(0.,0.,-1.)) ;
#94860 = DIRECTION('center_axis',(-1.2303003375722E-16,1.,-5.10212787052002E-17)) ;
#94861 = DIRECTION('ref_axis',(-1.,-1.2303003375722E-16,6.27714964143733E-33)) ;
#94862 = DIRECTION('center_axis',(-8.67361737988403E-15,-1.,0.)) ;
#94863 = DIRECTION('ref_axis',(1.,-8.67361737988403E-15,0.)) ;
#94864 = DIRECTION('center_axis',(1.,0.,6.27714964143733E-33)) ;
#94865 = DIRECTION('ref_axis',(6.27714964143733E-33,0.,-1.)) ;
#94866 = DIRECTION('center_axis',(-1.,0.,-6.50521303491307E-15)) ;
#94867 = DIRECTION('ref_axis',(-6.50521303491307E-15,0.,1.)) ;
#94868 = DIRECTION('center_axis',(1.,0.,0.)) ;
#94869 = DIRECTION('ref_axis',(0.,1.,0.)) ;
#94870 = DIRECTION('center_axis',(0.,0.,-1.)) ;
#94871 = DIRECTION('ref_axis',(-1.,0.,0.)) ;
#94872 = DIRECTION('center_axis',(0.,0.,1.)) ;
#94873 = DIRECTION('ref_axis',(1.,0.,0.)) ;
#94874 = DIRECTION('center_axis',(0.,0.,-1.)) ;
#94875 = DIRECTION('ref_axis',(-1.,0.,0.)) ;
#94876 = DIRECTION('center_axis',(-1.,0.,0.)) ;
#94877 = DIRECTION('ref_axis',(0.,0.,1.)) ;
#94878 = DIRECTION('center_axis',(0.,-1.,0.)) ;
#94879 = DIRECTION('ref_axis',(0.,0.,-1.)) ;
#94880 = DIRECTION('center_axis',(0.,1.,0.)) ;
#94881 = DIRECTION('ref_axis',(0.,0.,1.)) ;
#94882 = DIRECTION('center_axis',(0.,1.,-6.50521303491307E-15)) ;
#94883 = DIRECTION('ref_axis',(0.,6.50521303491307E-15,1.)) ;
#94884 = DIRECTION('center_axis',(0.,-1.,0.)) ;
#94885 = DIRECTION('ref_axis',(0.,0.,-1.)) ;
#94886 = DIRECTION('center_axis',(0.,-1.,0.)) ;
#94887 = DIRECTION('ref_axis',(0.,0.,-1.)) ;
#94888 = DIRECTION('center_axis',(0.,-1.,-1.07081696047951E-16)) ;
#94889 = DIRECTION('ref_axis',(0.,1.07081696047951E-16,-1.)) ;
#94890 = DIRECTION('center_axis',(0.,1.,0.)) ;
#94891 = DIRECTION('ref_axis',(0.,0.,1.)) ;
#94892 = DIRECTION('center_axis',(-1.,0.,0.)) ;
#94893 = DIRECTION('ref_axis',(0.,0.,1.)) ;
#94894 = DIRECTION('center_axis',(0.,0.,1.)) ;
#94895 = DIRECTION('ref_axis',(1.,0.,0.)) ;
#94896 = DIRECTION('center_axis',(0.,1.,0.)) ;
#94897 = DIRECTION('ref_axis',(0.,0.,1.)) ;
#94898 = DIRECTION('center_axis',(0.,0.,-1.)) ;
#94899 = DIRECTION('ref_axis',(-1.,0.,0.)) ;
#94900 = DIRECTION('center_axis',(0.,0.,1.)) ;
#94901 = DIRECTION('ref_axis',(1.,0.,0.)) ;
#94902 = DIRECTION('center_axis',(0.,0.,1.)) ;
#94903 = DIRECTION('ref_axis',(1.,0.,0.)) ;
#94904 = DIRECTION('center_axis',(0.,0.,1.)) ;
#94905 = DIRECTION('ref_axis',(1.,0.,0.)) ;
#94906 = DIRECTION('center_axis',(0.,0.,-1.)) ;
#94907 = DIRECTION('ref_axis',(-1.,0.,0.)) ;
#94908 = DIRECTION('center_axis',(0.,1.,0.)) ;
#94909 = DIRECTION('ref_axis',(0.,0.,1.)) ;
#94910 = DIRECTION('center_axis',(0.,-0.707106781186558,0.707106781186537)) ;
#94911 = DIRECTION('ref_axis',(0.,-0.707106781186537,-0.707106781186558)) ;
#94912 = DIRECTION('center_axis',(0.,1.,0.)) ;
#94913 = DIRECTION('ref_axis',(0.,0.,1.)) ;
#94914 = DIRECTION('center_axis',(0.,-0.514231796959093,-0.857651245551607)) ;
#94915 = DIRECTION('ref_axis',(0.,0.857651245551607,-0.514231796959093)) ;
#94916 = DIRECTION('center_axis',(0.,-0.707106781186548,0.707106781186547)) ;
#94917 = DIRECTION('ref_axis',(0.,-0.707106781186547,-0.707106781186548)) ;
#94918 = DIRECTION('center_axis',(0.,-0.707106781186548,0.707106781186548)) ;
#94919 = DIRECTION('ref_axis',(0.,-0.707106781186548,-0.707106781186548)) ;
#94920 = DIRECTION('center_axis',(-1.,0.,0.)) ;
#94921 = DIRECTION('ref_axis',(0.,0.,1.)) ;
#94922 = DIRECTION('center_axis',(0.,0.514231796959095,-0.857651245551606)) ;
#94923 = DIRECTION('ref_axis',(0.,0.857651245551606,0.514231796959095)) ;
#94924 = DIRECTION('center_axis',(0.,1.,0.)) ;
#94925 = DIRECTION('ref_axis',(0.,0.,1.)) ;
#94926 = DIRECTION('center_axis',(0.,0.,-1.)) ;
#94927 = DIRECTION('ref_axis',(-1.,0.,0.)) ;
#94928 = DIRECTION('center_axis',(0.,1.,0.)) ;
#94929 = DIRECTION('ref_axis',(0.,0.,1.)) ;
#94930 = DIRECTION('center_axis',(0.,0.,-1.)) ;
#94931 = DIRECTION('ref_axis',(-1.,0.,0.)) ;
#94932 = DIRECTION('center_axis',(0.,0.,-1.)) ;
#94933 = DIRECTION('ref_axis',(-1.,0.,0.)) ;
#94934 = DIRECTION('center_axis',(0.,0.,1.)) ;
#94935 = DIRECTION('ref_axis',(1.,0.,0.)) ;
#94936 = DIRECTION('center_axis',(0.,0.,-1.)) ;
#94937 = DIRECTION('ref_axis',(-1.,0.,0.)) ;
#94938 = DIRECTION('center_axis',(0.,1.,0.)) ;
#94939 = DIRECTION('ref_axis',(0.,0.,1.)) ;
#94940 = DIRECTION('center_axis',(0.,-1.,8.67361737988409E-15)) ;
#94941 = DIRECTION('ref_axis',(0.,-8.67361737988409E-15,-1.)) ;
#94942 = DIRECTION('center_axis',(0.,0.707106781186546,0.707106781186549)) ;
#94943 = DIRECTION('ref_axis',(0.,-0.707106781186549,0.707106781186546)) ;
#94944 = DIRECTION('center_axis',(0.,0.707106781186537,0.707106781186558)) ;
#94945 = DIRECTION('ref_axis',(0.,-0.707106781186558,0.707106781186537)) ;
#94946 = DIRECTION('center_axis',(0.,1.,1.07081696047951E-16)) ;
#94947 = DIRECTION('ref_axis',(0.,-1.07081696047951E-16,1.)) ;
#94948 = DIRECTION('center_axis',(0.,-1.,0.)) ;
#94949 = DIRECTION('ref_axis',(0.,0.,-1.)) ;
#94950 = DIRECTION('center_axis',(0.,1.,0.)) ;
#94951 = DIRECTION('ref_axis',(0.,0.,1.)) ;
#94952 = DIRECTION('center_axis',(0.,0.,1.)) ;
#94953 = DIRECTION('ref_axis',(1.,0.,0.)) ;
#94954 = DIRECTION('center_axis',(0.,1.,0.)) ;
#94955 = DIRECTION('ref_axis',(0.,0.,1.)) ;
#94956 = DIRECTION('center_axis',(0.,0.,1.)) ;
#94957 = DIRECTION('ref_axis',(1.,0.,0.)) ;
#94958 = DIRECTION('center_axis',(0.,3.99416362155027E-15,1.)) ;
#94959 = DIRECTION('ref_axis',(0.,-1.,3.99416362155027E-15)) ;
#94960 = DIRECTION('center_axis',(0.,0.,1.)) ;
#94961 = DIRECTION('ref_axis',(1.,0.,0.)) ;
#94962 = DIRECTION('center_axis',(0.,0.,-1.)) ;
#94963 = DIRECTION('ref_axis',(-1.,0.,0.)) ;
#94964 = DIRECTION('center_axis',(0.,0.,1.)) ;
#94965 = DIRECTION('ref_axis',(1.,0.,0.)) ;
#94966 = DIRECTION('center_axis',(-1.,0.,0.)) ;
#94967 = DIRECTION('ref_axis',(0.,0.,1.)) ;
#94968 = DIRECTION('center_axis',(0.,1.,0.)) ;
#94969 = DIRECTION('ref_axis',(0.,0.,1.)) ;
#94970 = DIRECTION('center_axis',(-1.,0.,0.)) ;
#94971 = DIRECTION('ref_axis',(0.,0.,1.)) ;
#94972 = DIRECTION('center_axis',(0.,-1.,0.)) ;
#94973 = DIRECTION('ref_axis',(0.,0.,-1.)) ;
#94974 = DIRECTION('center_axis',(0.,1.,0.)) ;
#94975 = DIRECTION('ref_axis',(0.,0.,1.)) ;
#94976 = DIRECTION('center_axis',(1.53063836115601E-16,-1.,-1.30104260698261E-16)) ;
#94977 = DIRECTION('ref_axis',(1.,1.53063836115601E-16,1.99142572374599E-32)) ;
#94978 = DIRECTION('center_axis',(0.,1.,0.)) ;
#94979 = DIRECTION('ref_axis',(0.,0.,1.)) ;
#94980 = DIRECTION('center_axis',(0.,-1.,0.)) ;
#94981 = DIRECTION('ref_axis',(0.,0.,-1.)) ;
#94982 = DIRECTION('center_axis',(1.,1.53063836115601E-16,2.73691106313441E-48)) ;
#94983 = DIRECTION('ref_axis',(-1.53063836115601E-16,1.,-4.18922106430579E-64)) ;
#94984 = DIRECTION('center_axis',(-1.,0.,0.)) ;
#94985 = DIRECTION('ref_axis',(0.,0.,1.)) ;
#94986 = DIRECTION('center_axis',(1.,1.53063836115601E-16,0.)) ;
#94987 = DIRECTION('ref_axis',(1.53063836115601E-16,-1.,0.)) ;
#94988 = DIRECTION('center_axis',(0.,1.,0.)) ;
#94989 = DIRECTION('ref_axis',(1.,0.,0.)) ;
#94990 = DIRECTION('center_axis',(0.,1.,0.)) ;
#94991 = DIRECTION('ref_axis',(0.,0.,-1.)) ;
#94992 = DIRECTION('center_axis',(0.,0.,1.)) ;
#94993 = DIRECTION('ref_axis',(-1.,0.,0.)) ;
#94994 = DIRECTION('center_axis',(0.,1.,0.)) ;
#94995 = DIRECTION('ref_axis',(1.,0.,0.)) ;
#94996 = DIRECTION('center_axis',(0.,0.,1.)) ;
#94997 = DIRECTION('ref_axis',(-1.,0.,0.)) ;
#94998 = DIRECTION('center_axis',(1.,1.0842021724855E-15,0.)) ;
#94999 = DIRECTION('ref_axis',(1.0842021724855E-15,-1.,0.)) ;
#95000 = DIRECTION('center_axis',(-1.,-1.53063836115601E-16,0.)) ;
#95001 = DIRECTION('ref_axis',(0.,-1.,0.)) ;
#95002 = DIRECTION('center_axis',(0.,0.,-1.)) ;
#95003 = DIRECTION('ref_axis',(1.,0.,0.)) ;
#95004 = DIRECTION('center_axis',(0.,0.,-1.)) ;
#95005 = DIRECTION('ref_axis',(0.804034447892627,0.594582716366695,0.)) ;
#95006 = DIRECTION('center_axis',(0.,0.,1.)) ;
#95007 = DIRECTION('ref_axis',(1.,0.,0.)) ;
#95008 = DIRECTION('',(0.,0.,-1.)) ;
#95009 = DIRECTION('center_axis',(-2.16840434497101E-16,1.,1.30104260698261E-16)) ;
#95010 = DIRECTION('ref_axis',(1.,2.16840434497101E-16,1.22464679914735E-16)) ;
#95011 = DIRECTION('',(-2.16840434497101E-16,1.,1.30104260698261E-16)) ;
#95012 = DIRECTION('center_axis',(0.,1.,0.)) ;
#95013 = DIRECTION('ref_axis',(0.,0.,1.)) ;
#95014 = DIRECTION('center_axis',(-1.,-1.53063836115601E-16,-2.73691106313441E-48)) ;
#95015 = DIRECTION('ref_axis',(1.53063836115601E-16,-1.,4.18922106430579E-64)) ;
#95016 = DIRECTION('center_axis',(1.,2.16840434497101E-16,0.)) ;
#95017 = DIRECTION('ref_axis',(2.16840434497101E-16,-1.,0.)) ;
#95018 = DIRECTION('center_axis',(0.,0.,1.)) ;
#95019 = DIRECTION('ref_axis',(1.,0.,0.)) ;
#95020 = DIRECTION('center_axis',(-1.25542992828747E-32,1.020425574104E-16,
1.)) ;
#95021 = DIRECTION('ref_axis',(-1.28107280532009E-48,-1.,1.020425574104E-16)) ;
#95022 = DIRECTION('center_axis',(0.,0.,1.)) ;
#95023 = DIRECTION('ref_axis',(1.,0.,0.)) ;
#95024 = DIRECTION('center_axis',(0.,0.,-1.)) ;
#95025 = DIRECTION('ref_axis',(-1.,0.,0.)) ;
#95026 = DIRECTION('center_axis',(1.,1.53063836115601E-16,-2.73691106313441E-48)) ;
#95027 = DIRECTION('ref_axis',(-1.53063836115601E-16,1.,4.18922106430579E-64)) ;
#95028 = DIRECTION('center_axis',(-1.,0.,0.)) ;
#95029 = DIRECTION('ref_axis',(0.,0.,1.)) ;
#95030 = DIRECTION('center_axis',(1.,1.53063836115601E-16,0.)) ;
#95031 = DIRECTION('ref_axis',(1.53063836115601E-16,-1.,0.)) ;
#95032 = DIRECTION('center_axis',(0.,1.,0.)) ;
#95033 = DIRECTION('ref_axis',(1.,0.,0.)) ;
#95034 = DIRECTION('center_axis',(-1.,-2.16840434497101E-16,0.)) ;
#95035 = DIRECTION('ref_axis',(0.,-1.,0.)) ;
#95036 = DIRECTION('center_axis',(0.,0.,-1.)) ;
#95037 = DIRECTION('ref_axis',(1.,0.,0.)) ;
#95038 = DIRECTION('center_axis',(-1.25542992828747E-32,1.020425574104E-16,
1.)) ;
#95039 = DIRECTION('ref_axis',(0.,-1.,0.)) ;
#95040 = DIRECTION('center_axis',(0.,-1.,0.)) ;
#95041 = DIRECTION('ref_axis',(-6.50521303491307E-15,0.,1.)) ;
#95042 = DIRECTION('center_axis',(-1.,0.,0.)) ;
#95043 = DIRECTION('ref_axis',(0.,0.,-1.)) ;
#95044 = DIRECTION('center_axis',(-1.,-1.53063836115601E-16,0.)) ;
#95045 = DIRECTION('ref_axis',(0.,-1.,0.)) ;
#95046 = DIRECTION('center_axis',(0.,-1.,0.)) ;
#95047 = DIRECTION('ref_axis',(0.,0.,1.)) ;
#95048 = DIRECTION('center_axis',(0.,0.,-1.)) ;
#95049 = DIRECTION('ref_axis',(-1.,0.,0.)) ;
#95050 = DIRECTION('center_axis',(0.,0.,-1.)) ;
#95051 = DIRECTION('ref_axis',(-1.,0.,0.)) ;
#95052 = DIRECTION('center_axis',(1.,1.53063836115601E-16,-3.06472600140763E-33)) ;
#95053 = DIRECTION('ref_axis',(-1.53063836115601E-16,1.,4.69098718418678E-49)) ;
#95054 = DIRECTION('center_axis',(-1.,0.,0.)) ;
#95055 = DIRECTION('ref_axis',(0.,0.,1.)) ;
#95056 = DIRECTION('center_axis',(-1.53063836115601E-16,1.,-1.020425574104E-16)) ;
#95057 = DIRECTION('ref_axis',(-1.,-1.53063836115601E-16,1.3684555315672E-47)) ;
#95058 = DIRECTION('',(1.53063836115601E-16,-1.,1.020425574104E-16)) ;
#95059 = DIRECTION('center_axis',(0.,-1.,0.)) ;
#95060 = DIRECTION('ref_axis',(0.,0.,-1.)) ;
#95061 = DIRECTION('center_axis',(-1.53063836115601E-16,1.,-1.30104260698261E-16)) ;
#95062 = DIRECTION('ref_axis',(-1.,-1.53063836115601E-16,1.99142572374599E-32)) ;
#95063 = DIRECTION('center_axis',(0.,-1.,0.)) ;
#95064 = DIRECTION('ref_axis',(0.,0.,-1.)) ;
#95065 = DIRECTION('center_axis',(-1.,-1.53063836115601E-16,2.73691106313441E-48)) ;
#95066 = DIRECTION('ref_axis',(1.53063836115601E-16,-1.,-4.18922106430579E-64)) ;
#95067 = DIRECTION('center_axis',(1.,2.16840434497101E-16,0.)) ;
#95068 = DIRECTION('ref_axis',(2.16840434497101E-16,-1.,0.)) ;
#95069 = DIRECTION('center_axis',(-1.,0.,2.16840434497102E-15)) ;
#95070 = DIRECTION('ref_axis',(2.16840434497102E-15,0.,1.)) ;
#95071 = DIRECTION('center_axis',(-1.,-2.16840434497101E-16,0.)) ;
#95072 = DIRECTION('ref_axis',(0.,-1.,0.)) ;
#95073 = DIRECTION('center_axis',(0.,0.,1.)) ;
#95074 = DIRECTION('ref_axis',(-1.,0.,0.)) ;
#95075 = DIRECTION('center_axis',(0.,1.,0.)) ;
#95076 = DIRECTION('ref_axis',(1.,0.,0.)) ;
#95077 = DIRECTION('center_axis',(0.,1.,0.)) ;
#95078 = DIRECTION('ref_axis',(0.,0.,-1.)) ;
#95079 = DIRECTION('center_axis',(1.,0.,0.)) ;
#95080 = DIRECTION('ref_axis',(0.,-1.,0.)) ;
#95081 = DIRECTION('center_axis',(1.,6.50521303491304E-15,0.)) ;
#95082 = DIRECTION('ref_axis',(-6.50521303491304E-15,1.,0.)) ;
#95083 = DIRECTION('center_axis',(8.67361737988403E-15,1.,0.)) ;
#95084 = DIRECTION('ref_axis',(-1.,8.67361737988403E-15,0.)) ;
#95085 = DIRECTION('center_axis',(1.2303003375722E-16,-1.,1.020425574104E-16)) ;
#95086 = DIRECTION('ref_axis',(1.,1.2303003375722E-16,-1.25542992828747E-32)) ;
#95087 = DIRECTION('center_axis',(0.,1.,0.)) ;
#95088 = DIRECTION('ref_axis',(0.,0.,1.)) ;
#95089 = DIRECTION('center_axis',(0.,1.,0.)) ;
#95090 = DIRECTION('ref_axis',(1.,0.,0.)) ;
#95091 = DIRECTION('center_axis',(1.,1.2303003375722E-16,0.)) ;
#95092 = DIRECTION('ref_axis',(1.2303003375722E-16,-1.,0.)) ;
#95093 = DIRECTION('center_axis',(0.,0.,1.)) ;
#95094 = DIRECTION('ref_axis',(-1.,0.,0.)) ;
#95095 = DIRECTION('center_axis',(0.,1.,0.)) ;
#95096 = DIRECTION('ref_axis',(1.,0.,0.)) ;
#95097 = DIRECTION('center_axis',(0.,0.,-1.)) ;
#95098 = DIRECTION('ref_axis',(1.,0.,0.)) ;
#95099 = DIRECTION('center_axis',(0.,0.,-1.)) ;
#95100 = DIRECTION('ref_axis',(-1.,0.,0.)) ;
#95101 = DIRECTION('center_axis',(0.,0.,1.)) ;
#95102 = DIRECTION('ref_axis',(1.,0.,0.)) ;
#95103 = DIRECTION('center_axis',(-2.16840434497101E-16,1.,-1.020425574104E-16)) ;
#95104 = DIRECTION('ref_axis',(-1.,-2.16840434497101E-16,5.47382212626882E-48)) ;
#95105 = DIRECTION('center_axis',(0.,1.,0.)) ;
#95106 = DIRECTION('ref_axis',(0.,0.,-1.)) ;
#95107 = DIRECTION('center_axis',(1.,0.,1.25542992828747E-32)) ;
#95108 = DIRECTION('ref_axis',(1.25542992828747E-32,0.,-1.)) ;
#95109 = DIRECTION('center_axis',(1.,0.,0.)) ;
#95110 = DIRECTION('ref_axis',(0.,0.,-1.)) ;
#95111 = DIRECTION('center_axis',(-1.,-1.2303003375722E-16,0.)) ;
#95112 = DIRECTION('ref_axis',(0.,-1.,0.)) ;
#95113 = DIRECTION('center_axis',(0.,0.,-1.)) ;
#95114 = DIRECTION('ref_axis',(1.,0.,0.)) ;
#95115 = DIRECTION('center_axis',(0.,0.,-1.)) ;
#95116 = DIRECTION('ref_axis',(-1.,0.,0.)) ;
#95117 = DIRECTION('',(0.,0.,1.)) ;
#95118 = DIRECTION('center_axis',(0.,0.,1.)) ;
#95119 = DIRECTION('ref_axis',(1.,0.,0.)) ;
#95120 = DIRECTION('center_axis',(0.,0.,1.)) ;
#95121 = DIRECTION('ref_axis',(1.,0.,0.)) ;
#95122 = DIRECTION('center_axis',(6.27714964143733E-33,-5.10212787052002E-17,
-1.)) ;
#95123 = DIRECTION('ref_axis',(3.20268201330022E-49,1.,-5.10212787052002E-17)) ;
#95124 = DIRECTION('center_axis',(1.,1.53063836115601E-16,-1.53236300070382E-33)) ;
#95125 = DIRECTION('ref_axis',(-1.53063836115601E-16,1.,2.34549359209339E-49)) ;
#95126 = DIRECTION('center_axis',(-1.,0.,0.)) ;
#95127 = DIRECTION('ref_axis',(0.,0.,1.)) ;
#95128 = DIRECTION('center_axis',(1.,0.,0.)) ;
#95129 = DIRECTION('ref_axis',(0.,0.,-1.)) ;
#95130 = DIRECTION('center_axis',(0.,1.,0.)) ;
#95131 = DIRECTION('ref_axis',(1.,0.,0.)) ;
#95132 = DIRECTION('center_axis',(-4.33680868994202E-15,1.,0.)) ;
#95133 = DIRECTION('ref_axis',(1.,4.33680868994202E-15,0.)) ;
#95134 = DIRECTION('center_axis',(0.,-1.,0.)) ;
#95135 = DIRECTION('ref_axis',(0.,0.,-1.)) ;
#95136 = DIRECTION('center_axis',(0.,0.,-1.)) ;
#95137 = DIRECTION('ref_axis',(1.,0.,0.)) ;
#95138 = DIRECTION('center_axis',(0.,0.,1.)) ;
#95139 = DIRECTION('ref_axis',(1.,0.,0.)) ;
#95140 = DIRECTION('center_axis',(0.,0.,-1.)) ;
#95141 = DIRECTION('ref_axis',(-1.,0.,0.)) ;
#95142 = DIRECTION('center_axis',(0.,1.,0.)) ;
#95143 = DIRECTION('ref_axis',(1.,0.,0.)) ;
#95144 = DIRECTION('center_axis',(1.,1.2303003375722E-16,0.)) ;
#95145 = DIRECTION('ref_axis',(1.2303003375722E-16,-1.,0.)) ;
#95146 = DIRECTION('center_axis',(0.,1.,0.)) ;
#95147 = DIRECTION('ref_axis',(-6.50521303491284E-15,0.,-1.)) ;
#95148 = DIRECTION('center_axis',(6.27714964143733E-33,-5.10212787052002E-17,
-1.)) ;
#95149 = DIRECTION('ref_axis',(0.,1.,0.)) ;
#95150 = DIRECTION('center_axis',(0.,-1.,0.)) ;
#95151 = DIRECTION('ref_axis',(0.,0.,1.)) ;
#95152 = DIRECTION('center_axis',(2.16840434497101E-16,-1.,5.10212787052002E-17)) ;
#95153 = DIRECTION('ref_axis',(1.,2.16840434497101E-16,-5.47382212626882E-48)) ;
#95154 = DIRECTION('center_axis',(0.,1.,0.)) ;
#95155 = DIRECTION('ref_axis',(0.,0.,-1.)) ;
#95156 = DIRECTION('center_axis',(0.,0.,1.)) ;
#95157 = DIRECTION('ref_axis',(1.,0.,0.)) ;
#95158 = DIRECTION('center_axis',(0.,0.,-1.)) ;
#95159 = DIRECTION('ref_axis',(-1.,0.,0.)) ;
#95160 = DIRECTION('center_axis',(-1.,-1.2303003375722E-16,0.)) ;
#95161 = DIRECTION('ref_axis',(0.,-1.,0.)) ;
#95162 = DIRECTION('center_axis',(0.,-1.,0.)) ;
#95163 = DIRECTION('ref_axis',(0.,0.,1.)) ;
#95164 = DIRECTION('center_axis',(1.53063836115601E-16,-1.,5.10212787052002E-17)) ;
#95165 = DIRECTION('ref_axis',(1.,1.53063836115601E-16,-6.84227765783602E-48)) ;
#95166 = DIRECTION('',(-1.53063836115601E-16,1.,-5.10212787052002E-17)) ;
#95167 = DIRECTION('center_axis',(0.,-1.,0.)) ;
#95168 = DIRECTION('ref_axis',(0.,0.,-1.)) ;
#95169 = DIRECTION('center_axis',(-1.,0.,0.)) ;
#95170 = DIRECTION('ref_axis',(0.,0.,-1.)) ;
#95171 = DIRECTION('center_axis',(-1.2303003375722E-16,1.,-5.10212787052002E-17)) ;
#95172 = DIRECTION('ref_axis',(-1.,-1.2303003375722E-16,6.27714964143733E-33)) ;
#95173 = DIRECTION('center_axis',(-8.67361737988403E-15,-1.,0.)) ;
#95174 = DIRECTION('ref_axis',(1.,-8.67361737988403E-15,0.)) ;
#95175 = DIRECTION('center_axis',(1.,0.,6.27714964143733E-33)) ;
#95176 = DIRECTION('ref_axis',(6.27714964143733E-33,0.,-1.)) ;
#95177 = DIRECTION('center_axis',(-1.,0.,-6.50521303491284E-15)) ;
#95178 = DIRECTION('ref_axis',(-6.50521303491284E-15,0.,1.)) ;
#95179 = DIRECTION('center_axis',(1.,0.,0.)) ;
#95180 = DIRECTION('ref_axis',(0.,1.,0.)) ;
#95181 = DIRECTION('center_axis',(0.,0.,-1.)) ;
#95182 = DIRECTION('ref_axis',(-1.,0.,0.)) ;
#95183 = DIRECTION('center_axis',(0.,0.,1.)) ;
#95184 = DIRECTION('ref_axis',(1.,0.,0.)) ;
#95185 = DIRECTION('center_axis',(0.,0.,-1.)) ;
#95186 = DIRECTION('ref_axis',(-1.,0.,0.)) ;
#95187 = DIRECTION('center_axis',(-1.,0.,0.)) ;
#95188 = DIRECTION('ref_axis',(0.,0.,1.)) ;
#95189 = DIRECTION('center_axis',(0.,-1.,0.)) ;
#95190 = DIRECTION('ref_axis',(0.,0.,-1.)) ;
#95191 = DIRECTION('center_axis',(0.,1.,0.)) ;
#95192 = DIRECTION('ref_axis',(0.,0.,1.)) ;
#95193 = DIRECTION('center_axis',(0.,1.,-6.50521303491284E-15)) ;
#95194 = DIRECTION('ref_axis',(0.,6.50521303491284E-15,1.)) ;
#95195 = DIRECTION('center_axis',(0.,-1.,0.)) ;
#95196 = DIRECTION('ref_axis',(0.,0.,-1.)) ;
#95197 = DIRECTION('center_axis',(0.,-1.,0.)) ;
#95198 = DIRECTION('ref_axis',(0.,0.,-1.)) ;
#95199 = DIRECTION('center_axis',(0.,-1.,-1.07081696047951E-16)) ;
#95200 = DIRECTION('ref_axis',(0.,1.07081696047951E-16,-1.)) ;
#95201 = DIRECTION('center_axis',(0.,1.,0.)) ;
#95202 = DIRECTION('ref_axis',(0.,0.,1.)) ;
#95203 = DIRECTION('center_axis',(-1.,0.,0.)) ;
#95204 = DIRECTION('ref_axis',(0.,0.,1.)) ;
#95205 = DIRECTION('center_axis',(0.,0.,1.)) ;
#95206 = DIRECTION('ref_axis',(1.,0.,0.)) ;
#95207 = DIRECTION('center_axis',(0.,1.,0.)) ;
#95208 = DIRECTION('ref_axis',(0.,0.,1.)) ;
#95209 = DIRECTION('center_axis',(0.,0.,-1.)) ;
#95210 = DIRECTION('ref_axis',(-1.,0.,0.)) ;
#95211 = DIRECTION('center_axis',(0.,0.,1.)) ;
#95212 = DIRECTION('ref_axis',(1.,0.,0.)) ;
#95213 = DIRECTION('center_axis',(0.,0.,1.)) ;
#95214 = DIRECTION('ref_axis',(1.,0.,0.)) ;
#95215 = DIRECTION('center_axis',(0.,0.,1.)) ;
#95216 = DIRECTION('ref_axis',(1.,0.,0.)) ;
#95217 = DIRECTION('center_axis',(0.,0.,-1.)) ;
#95218 = DIRECTION('ref_axis',(-1.,0.,0.)) ;
#95219 = DIRECTION('center_axis',(0.,1.,0.)) ;
#95220 = DIRECTION('ref_axis',(0.,0.,1.)) ;
#95221 = DIRECTION('center_axis',(0.,-0.707106781186532,0.707106781186563)) ;
#95222 = DIRECTION('ref_axis',(0.,-0.707106781186563,-0.707106781186532)) ;
#95223 = DIRECTION('center_axis',(0.,1.,0.)) ;
#95224 = DIRECTION('ref_axis',(0.,0.,1.)) ;
#95225 = DIRECTION('center_axis',(2.23012492569655E-15,-0.51423179695906,
-0.857651245551627)) ;
#95226 = DIRECTION('ref_axis',(2.6714619735869E-30,0.857651245551626,-0.51423179695906)) ;
#95227 = DIRECTION('center_axis',(0.,-0.707106781186548,0.707106781186547)) ;
#95228 = DIRECTION('ref_axis',(0.,-0.707106781186547,-0.707106781186548)) ;
#95229 = DIRECTION('center_axis',(0.,-0.707106781186541,0.707106781186554)) ;
#95230 = DIRECTION('ref_axis',(0.,-0.707106781186554,-0.707106781186541)) ;
#95231 = DIRECTION('center_axis',(-1.,0.,0.)) ;
#95232 = DIRECTION('ref_axis',(0.,0.,1.)) ;
#95233 = DIRECTION('center_axis',(0.,0.514231796959095,-0.857651245551606)) ;
#95234 = DIRECTION('ref_axis',(0.,0.857651245551606,0.514231796959095)) ;
#95235 = DIRECTION('center_axis',(0.,1.,0.)) ;
#95236 = DIRECTION('ref_axis',(0.,0.,1.)) ;
#95237 = DIRECTION('center_axis',(0.,0.,-1.)) ;
#95238 = DIRECTION('ref_axis',(-1.,0.,0.)) ;
#95239 = DIRECTION('center_axis',(0.,1.,0.)) ;
#95240 = DIRECTION('ref_axis',(0.,0.,1.)) ;
#95241 = DIRECTION('center_axis',(0.,0.,-1.)) ;
#95242 = DIRECTION('ref_axis',(-1.,0.,0.)) ;
#95243 = DIRECTION('center_axis',(0.,0.,-1.)) ;
#95244 = DIRECTION('ref_axis',(-1.,0.,0.)) ;
#95245 = DIRECTION('center_axis',(0.,0.,1.)) ;
#95246 = DIRECTION('ref_axis',(1.,0.,0.)) ;
#95247 = DIRECTION('center_axis',(0.,0.,-1.)) ;
#95248 = DIRECTION('ref_axis',(-1.,0.,0.)) ;
#95249 = DIRECTION('center_axis',(0.,1.,0.)) ;
#95250 = DIRECTION('ref_axis',(0.,0.,1.)) ;
#95251 = DIRECTION('center_axis',(0.,-1.,8.67361737988409E-15)) ;
#95252 = DIRECTION('ref_axis',(0.,-8.67361737988409E-15,-1.)) ;
#95253 = DIRECTION('center_axis',(0.,0.707106781186546,0.707106781186549)) ;
#95254 = DIRECTION('ref_axis',(0.,-0.707106781186549,0.707106781186546)) ;
#95255 = DIRECTION('center_axis',(0.,0.707106781186537,0.707106781186558)) ;
#95256 = DIRECTION('ref_axis',(0.,-0.707106781186558,0.707106781186537)) ;
#95257 = DIRECTION('center_axis',(0.,1.,1.07081696047951E-16)) ;
#95258 = DIRECTION('ref_axis',(0.,-1.07081696047951E-16,1.)) ;
#95259 = DIRECTION('center_axis',(0.,-1.,0.)) ;
#95260 = DIRECTION('ref_axis',(0.,0.,-1.)) ;
#95261 = DIRECTION('center_axis',(0.,1.,0.)) ;
#95262 = DIRECTION('ref_axis',(0.,0.,1.)) ;
#95263 = DIRECTION('center_axis',(0.,0.,1.)) ;
#95264 = DIRECTION('ref_axis',(1.,0.,0.)) ;
#95265 = DIRECTION('center_axis',(0.,1.,0.)) ;
#95266 = DIRECTION('ref_axis',(0.,0.,1.)) ;
#95267 = DIRECTION('center_axis',(0.,0.,1.)) ;
#95268 = DIRECTION('ref_axis',(1.,0.,0.)) ;
#95269 = DIRECTION('center_axis',(0.,3.99416362155027E-15,1.)) ;
#95270 = DIRECTION('ref_axis',(0.,-1.,3.99416362155027E-15)) ;
#95271 = DIRECTION('center_axis',(0.,0.,1.)) ;
#95272 = DIRECTION('ref_axis',(1.,0.,0.)) ;
#95273 = DIRECTION('center_axis',(0.,0.,-1.)) ;
#95274 = DIRECTION('ref_axis',(-1.,0.,0.)) ;
#95275 = DIRECTION('center_axis',(0.,0.,1.)) ;
#95276 = DIRECTION('ref_axis',(1.,0.,0.)) ;
#95277 = DIRECTION('center_axis',(-1.,0.,0.)) ;
#95278 = DIRECTION('ref_axis',(0.,0.,1.)) ;
#95279 = DIRECTION('center_axis',(0.,1.,0.)) ;
#95280 = DIRECTION('ref_axis',(0.,0.,1.)) ;
#95281 = DIRECTION('center_axis',(-1.,0.,0.)) ;
#95282 = DIRECTION('ref_axis',(0.,0.,1.)) ;
#95283 = DIRECTION('center_axis',(0.,-1.,0.)) ;
#95284 = DIRECTION('ref_axis',(0.,0.,-1.)) ;
#95285 = DIRECTION('center_axis',(0.,1.,0.)) ;
#95286 = DIRECTION('ref_axis',(0.,0.,1.)) ;
#95287 = DIRECTION('center_axis',(1.53063836115601E-16,-1.,-1.30104260698261E-16)) ;
#95288 = DIRECTION('ref_axis',(1.,1.53063836115601E-16,1.99142572374599E-32)) ;
#95289 = DIRECTION('center_axis',(0.,1.,0.)) ;
#95290 = DIRECTION('ref_axis',(0.,0.,1.)) ;
#95291 = DIRECTION('center_axis',(0.,-1.,0.)) ;
#95292 = DIRECTION('ref_axis',(0.,0.,-1.)) ;
#95293 = DIRECTION('center_axis',(1.,1.53063836115601E-16,2.73691106313441E-48)) ;
#95294 = DIRECTION('ref_axis',(-1.53063836115601E-16,1.,-4.18922106430579E-64)) ;
#95295 = DIRECTION('center_axis',(-1.,0.,0.)) ;
#95296 = DIRECTION('ref_axis',(0.,0.,1.)) ;
#95297 = DIRECTION('center_axis',(1.,1.53063836115601E-16,0.)) ;
#95298 = DIRECTION('ref_axis',(1.53063836115601E-16,-1.,0.)) ;
#95299 = DIRECTION('center_axis',(0.,1.,0.)) ;
#95300 = DIRECTION('ref_axis',(1.,0.,0.)) ;
#95301 = DIRECTION('center_axis',(0.,1.,0.)) ;
#95302 = DIRECTION('ref_axis',(0.,0.,-1.)) ;
#95303 = DIRECTION('center_axis',(0.,0.,1.)) ;
#95304 = DIRECTION('ref_axis',(-1.,0.,0.)) ;
#95305 = DIRECTION('center_axis',(0.,1.,0.)) ;
#95306 = DIRECTION('ref_axis',(1.,0.,0.)) ;
#95307 = DIRECTION('center_axis',(0.,0.,1.)) ;
#95308 = DIRECTION('ref_axis',(-1.,0.,0.)) ;
#95309 = DIRECTION('center_axis',(1.,1.0842021724855E-15,0.)) ;
#95310 = DIRECTION('ref_axis',(1.0842021724855E-15,-1.,0.)) ;
#95311 = DIRECTION('center_axis',(-1.,-1.53063836115601E-16,0.)) ;
#95312 = DIRECTION('ref_axis',(0.,-1.,0.)) ;
#95313 = DIRECTION('center_axis',(0.,0.,-1.)) ;
#95314 = DIRECTION('ref_axis',(1.,0.,0.)) ;
#95315 = DIRECTION('center_axis',(0.,0.,-1.)) ;
#95316 = DIRECTION('ref_axis',(0.804034447892622,0.594582716366703,0.)) ;
#95317 = DIRECTION('center_axis',(0.,0.,1.)) ;
#95318 = DIRECTION('ref_axis',(1.,0.,0.)) ;
#95319 = DIRECTION('',(0.,0.,-1.)) ;
#95320 = DIRECTION('center_axis',(-2.16840434497101E-16,1.,1.30104260698261E-16)) ;
#95321 = DIRECTION('ref_axis',(1.,2.16840434497101E-16,1.22464679914735E-16)) ;
#95322 = DIRECTION('',(-2.16840434497101E-16,1.,1.30104260698261E-16)) ;
#95323 = DIRECTION('center_axis',(0.,1.,0.)) ;
#95324 = DIRECTION('ref_axis',(0.,0.,1.)) ;
#95325 = DIRECTION('center_axis',(-1.,-1.53063836115601E-16,-2.73691106313441E-48)) ;
#95326 = DIRECTION('ref_axis',(1.53063836115601E-16,-1.,4.18922106430579E-64)) ;
#95327 = DIRECTION('center_axis',(1.,2.16840434497101E-16,0.)) ;
#95328 = DIRECTION('ref_axis',(2.16840434497101E-16,-1.,0.)) ;
#95329 = DIRECTION('center_axis',(0.,0.,1.)) ;
#95330 = DIRECTION('ref_axis',(1.,0.,0.)) ;
#95331 = DIRECTION('center_axis',(-1.25542992828747E-32,1.020425574104E-16,
1.)) ;
#95332 = DIRECTION('ref_axis',(-1.28107280532009E-48,-1.,1.020425574104E-16)) ;
#95333 = DIRECTION('center_axis',(0.,0.,1.)) ;
#95334 = DIRECTION('ref_axis',(1.,0.,0.)) ;
#95335 = DIRECTION('center_axis',(0.,0.,-1.)) ;
#95336 = DIRECTION('ref_axis',(-1.,0.,0.)) ;
#95337 = DIRECTION('center_axis',(1.,1.53063836115601E-16,-2.73691106313441E-48)) ;
#95338 = DIRECTION('ref_axis',(-1.53063836115601E-16,1.,4.18922106430579E-64)) ;
#95339 = DIRECTION('center_axis',(-1.,0.,0.)) ;
#95340 = DIRECTION('ref_axis',(0.,0.,1.)) ;
#95341 = DIRECTION('center_axis',(1.,1.53063836115601E-16,0.)) ;
#95342 = DIRECTION('ref_axis',(1.53063836115601E-16,-1.,0.)) ;
#95343 = DIRECTION('center_axis',(0.,1.,0.)) ;
#95344 = DIRECTION('ref_axis',(1.,0.,0.)) ;
#95345 = DIRECTION('center_axis',(-1.,-2.16840434497101E-16,0.)) ;
#95346 = DIRECTION('ref_axis',(0.,-1.,0.)) ;
#95347 = DIRECTION('center_axis',(0.,0.,-1.)) ;
#95348 = DIRECTION('ref_axis',(1.,0.,0.)) ;
#95349 = DIRECTION('center_axis',(-1.25542992828747E-32,1.020425574104E-16,
1.)) ;
#95350 = DIRECTION('ref_axis',(0.,-1.,0.)) ;
#95351 = DIRECTION('center_axis',(0.,-1.,0.)) ;
#95352 = DIRECTION('ref_axis',(-6.50521303491284E-15,0.,1.)) ;
#95353 = DIRECTION('center_axis',(-1.,0.,0.)) ;
#95354 = DIRECTION('ref_axis',(0.,0.,-1.)) ;
#95355 = DIRECTION('center_axis',(-1.,-1.53063836115601E-16,0.)) ;
#95356 = DIRECTION('ref_axis',(0.,-1.,0.)) ;
#95357 = DIRECTION('center_axis',(0.,-1.,0.)) ;
#95358 = DIRECTION('ref_axis',(0.,0.,1.)) ;
#95359 = DIRECTION('center_axis',(0.,0.,-1.)) ;
#95360 = DIRECTION('ref_axis',(-1.,0.,0.)) ;
#95361 = DIRECTION('center_axis',(0.,0.,-1.)) ;
#95362 = DIRECTION('ref_axis',(-1.,0.,0.)) ;
#95363 = DIRECTION('center_axis',(1.,1.53063836115601E-16,-3.06472600140763E-33)) ;
#95364 = DIRECTION('ref_axis',(-1.53063836115601E-16,1.,4.69098718418678E-49)) ;
#95365 = DIRECTION('center_axis',(-1.,0.,0.)) ;
#95366 = DIRECTION('ref_axis',(0.,0.,1.)) ;
#95367 = DIRECTION('center_axis',(-1.53063836115601E-16,1.,-1.020425574104E-16)) ;
#95368 = DIRECTION('ref_axis',(-1.,-1.53063836115601E-16,1.3684555315672E-47)) ;
#95369 = DIRECTION('',(1.53063836115601E-16,-1.,1.020425574104E-16)) ;
#95370 = DIRECTION('center_axis',(0.,-1.,0.)) ;
#95371 = DIRECTION('ref_axis',(0.,0.,-1.)) ;
#95372 = DIRECTION('center_axis',(-1.53063836115601E-16,1.,-1.30104260698261E-16)) ;
#95373 = DIRECTION('ref_axis',(-1.,-1.53063836115601E-16,1.99142572374599E-32)) ;
#95374 = DIRECTION('center_axis',(0.,-1.,0.)) ;
#95375 = DIRECTION('ref_axis',(0.,0.,-1.)) ;
#95376 = DIRECTION('center_axis',(-1.,-1.53063836115601E-16,2.73691106313441E-48)) ;
#95377 = DIRECTION('ref_axis',(1.53063836115601E-16,-1.,-4.18922106430579E-64)) ;
#95378 = DIRECTION('center_axis',(1.,2.16840434497101E-16,0.)) ;
#95379 = DIRECTION('ref_axis',(2.16840434497101E-16,-1.,0.)) ;
#95380 = DIRECTION('center_axis',(-1.,0.,2.16840434497095E-15)) ;
#95381 = DIRECTION('ref_axis',(2.16840434497095E-15,0.,1.)) ;
#95382 = DIRECTION('center_axis',(-1.,-2.16840434497101E-16,0.)) ;
#95383 = DIRECTION('ref_axis',(0.,-1.,0.)) ;
#95384 = DIRECTION('center_axis',(0.,0.,1.)) ;
#95385 = DIRECTION('ref_axis',(-1.,0.,0.)) ;
#95386 = DIRECTION('center_axis',(0.,1.,0.)) ;
#95387 = DIRECTION('ref_axis',(1.,0.,0.)) ;
#95388 = DIRECTION('center_axis',(0.,1.,0.)) ;
#95389 = DIRECTION('ref_axis',(0.,0.,-1.)) ;
#95390 = DIRECTION('center_axis',(1.,0.,0.)) ;
#95391 = DIRECTION('ref_axis',(0.,-1.,0.)) ;
#95392 = DIRECTION('center_axis',(1.,6.50521303491304E-15,0.)) ;
#95393 = DIRECTION('ref_axis',(-6.50521303491304E-15,1.,0.)) ;
#95394 = DIRECTION('center_axis',(8.67361737988403E-15,1.,0.)) ;
#95395 = DIRECTION('ref_axis',(-1.,8.67361737988403E-15,0.)) ;
#95396 = DIRECTION('center_axis',(1.2303003375722E-16,-1.,1.020425574104E-16)) ;
#95397 = DIRECTION('ref_axis',(1.,1.2303003375722E-16,-1.25542992828747E-32)) ;
#95398 = DIRECTION('center_axis',(0.,1.,0.)) ;
#95399 = DIRECTION('ref_axis',(0.,0.,1.)) ;
#95400 = DIRECTION('center_axis',(0.,1.,0.)) ;
#95401 = DIRECTION('ref_axis',(1.,0.,0.)) ;
#95402 = DIRECTION('center_axis',(1.,1.2303003375722E-16,0.)) ;
#95403 = DIRECTION('ref_axis',(1.2303003375722E-16,-1.,0.)) ;
#95404 = DIRECTION('center_axis',(0.,0.,1.)) ;
#95405 = DIRECTION('ref_axis',(-1.,0.,0.)) ;
#95406 = DIRECTION('center_axis',(0.,1.,0.)) ;
#95407 = DIRECTION('ref_axis',(1.,0.,0.)) ;
#95408 = DIRECTION('center_axis',(0.,0.,-1.)) ;
#95409 = DIRECTION('ref_axis',(1.,0.,0.)) ;
#95410 = DIRECTION('center_axis',(0.,0.,-1.)) ;
#95411 = DIRECTION('ref_axis',(-1.,0.,0.)) ;
#95412 = DIRECTION('center_axis',(0.,0.,1.)) ;
#95413 = DIRECTION('ref_axis',(1.,0.,0.)) ;
#95414 = DIRECTION('center_axis',(-2.16840434497101E-16,1.,-1.020425574104E-16)) ;
#95415 = DIRECTION('ref_axis',(-1.,-2.16840434497101E-16,5.47382212626882E-48)) ;
#95416 = DIRECTION('center_axis',(0.,1.,0.)) ;
#95417 = DIRECTION('ref_axis',(0.,0.,-1.)) ;
#95418 = DIRECTION('center_axis',(1.,0.,1.25542992828747E-32)) ;
#95419 = DIRECTION('ref_axis',(1.25542992828747E-32,0.,-1.)) ;
#95420 = DIRECTION('center_axis',(1.,0.,0.)) ;
#95421 = DIRECTION('ref_axis',(0.,0.,-1.)) ;
#95422 = DIRECTION('center_axis',(-1.,-1.2303003375722E-16,0.)) ;
#95423 = DIRECTION('ref_axis',(0.,-1.,0.)) ;
#95424 = DIRECTION('center_axis',(0.,0.,-1.)) ;
#95425 = DIRECTION('ref_axis',(1.,0.,0.)) ;
#95426 = DIRECTION('center_axis',(0.,0.,-1.)) ;
#95427 = DIRECTION('ref_axis',(-1.,0.,0.)) ;
#95428 = DIRECTION('',(0.,0.,1.)) ;
#95429 = DIRECTION('center_axis',(0.,0.,1.)) ;
#95430 = DIRECTION('ref_axis',(1.,0.,0.)) ;
#95431 = DIRECTION('center_axis',(0.,0.,1.)) ;
#95432 = DIRECTION('ref_axis',(1.,0.,0.)) ;
#95433 = DIRECTION('center_axis',(6.27714964143733E-33,-5.10212787052002E-17,
-1.)) ;
#95434 = DIRECTION('ref_axis',(3.20268201330022E-49,1.,-5.10212787052002E-17)) ;
#95435 = DIRECTION('center_axis',(1.,1.53063836115601E-16,-1.53236300070382E-33)) ;
#95436 = DIRECTION('ref_axis',(-1.53063836115601E-16,1.,2.34549359209339E-49)) ;
#95437 = DIRECTION('center_axis',(-1.,0.,0.)) ;
#95438 = DIRECTION('ref_axis',(0.,0.,1.)) ;
#95439 = DIRECTION('center_axis',(1.,0.,0.)) ;
#95440 = DIRECTION('ref_axis',(0.,0.,-1.)) ;
#95441 = DIRECTION('center_axis',(0.,1.,0.)) ;
#95442 = DIRECTION('ref_axis',(1.,0.,0.)) ;
#95443 = DIRECTION('center_axis',(-4.33680868994202E-15,1.,0.)) ;
#95444 = DIRECTION('ref_axis',(1.,4.33680868994202E-15,0.)) ;
#95445 = DIRECTION('center_axis',(0.,-1.,0.)) ;
#95446 = DIRECTION('ref_axis',(0.,0.,-1.)) ;
#95447 = DIRECTION('center_axis',(0.,0.,-1.)) ;
#95448 = DIRECTION('ref_axis',(1.,0.,0.)) ;
#95449 = DIRECTION('center_axis',(0.,0.,1.)) ;
#95450 = DIRECTION('ref_axis',(1.,0.,0.)) ;
#95451 = DIRECTION('center_axis',(0.,0.,-1.)) ;
#95452 = DIRECTION('ref_axis',(-1.,0.,0.)) ;
#95453 = DIRECTION('center_axis',(0.,1.,0.)) ;
#95454 = DIRECTION('ref_axis',(1.,0.,0.)) ;
#95455 = DIRECTION('center_axis',(1.,1.2303003375722E-16,0.)) ;
#95456 = DIRECTION('ref_axis',(1.2303003375722E-16,-1.,0.)) ;
#95457 = DIRECTION('center_axis',(0.,1.,0.)) ;
#95458 = DIRECTION('ref_axis',(-6.50521303491284E-15,0.,-1.)) ;
#95459 = DIRECTION('center_axis',(6.27714964143733E-33,-5.10212787052002E-17,
-1.)) ;
#95460 = DIRECTION('ref_axis',(0.,1.,0.)) ;
#95461 = DIRECTION('center_axis',(0.,-1.,0.)) ;
#95462 = DIRECTION('ref_axis',(0.,0.,1.)) ;
#95463 = DIRECTION('center_axis',(2.16840434497101E-16,-1.,5.10212787052002E-17)) ;
#95464 = DIRECTION('ref_axis',(1.,2.16840434497101E-16,-5.47382212626882E-48)) ;
#95465 = DIRECTION('center_axis',(0.,1.,0.)) ;
#95466 = DIRECTION('ref_axis',(0.,0.,-1.)) ;
#95467 = DIRECTION('center_axis',(0.,0.,1.)) ;
#95468 = DIRECTION('ref_axis',(1.,0.,0.)) ;
#95469 = DIRECTION('center_axis',(0.,0.,-1.)) ;
#95470 = DIRECTION('ref_axis',(-1.,0.,0.)) ;
#95471 = DIRECTION('center_axis',(-1.,-1.2303003375722E-16,0.)) ;
#95472 = DIRECTION('ref_axis',(0.,-1.,0.)) ;
#95473 = DIRECTION('center_axis',(0.,-1.,0.)) ;
#95474 = DIRECTION('ref_axis',(0.,0.,1.)) ;
#95475 = DIRECTION('center_axis',(1.53063836115601E-16,-1.,5.10212787052002E-17)) ;
#95476 = DIRECTION('ref_axis',(1.,1.53063836115601E-16,-6.84227765783602E-48)) ;
#95477 = DIRECTION('',(-1.53063836115601E-16,1.,-5.10212787052002E-17)) ;
#95478 = DIRECTION('center_axis',(0.,-1.,0.)) ;
#95479 = DIRECTION('ref_axis',(0.,0.,-1.)) ;
#95480 = DIRECTION('center_axis',(-1.,0.,0.)) ;
#95481 = DIRECTION('ref_axis',(0.,0.,-1.)) ;
#95482 = DIRECTION('center_axis',(-1.2303003375722E-16,1.,-5.10212787052002E-17)) ;
#95483 = DIRECTION('ref_axis',(-1.,-1.2303003375722E-16,6.27714964143733E-33)) ;
#95484 = DIRECTION('center_axis',(-8.67361737988403E-15,-1.,0.)) ;
#95485 = DIRECTION('ref_axis',(1.,-8.67361737988403E-15,0.)) ;
#95486 = DIRECTION('center_axis',(1.,0.,6.27714964143733E-33)) ;
#95487 = DIRECTION('ref_axis',(6.27714964143733E-33,0.,-1.)) ;
#95488 = DIRECTION('center_axis',(-1.,0.,-6.50521303491284E-15)) ;
#95489 = DIRECTION('ref_axis',(-6.50521303491284E-15,0.,1.)) ;
#95490 = DIRECTION('center_axis',(1.,0.,0.)) ;
#95491 = DIRECTION('ref_axis',(0.,1.,0.)) ;
#95492 = DIRECTION('center_axis',(0.,0.,-1.)) ;
#95493 = DIRECTION('ref_axis',(-1.,0.,0.)) ;
#95494 = DIRECTION('center_axis',(0.,0.,1.)) ;
#95495 = DIRECTION('ref_axis',(1.,0.,0.)) ;
#95496 = DIRECTION('center_axis',(0.,0.,-1.)) ;
#95497 = DIRECTION('ref_axis',(-1.,0.,0.)) ;
#95498 = DIRECTION('center_axis',(-1.,0.,0.)) ;
#95499 = DIRECTION('ref_axis',(0.,0.,1.)) ;
#95500 = DIRECTION('center_axis',(0.,-1.,0.)) ;
#95501 = DIRECTION('ref_axis',(0.,0.,-1.)) ;
#95502 = DIRECTION('center_axis',(0.,1.,0.)) ;
#95503 = DIRECTION('ref_axis',(0.,0.,1.)) ;
#95504 = DIRECTION('center_axis',(0.,1.,-6.50521303491284E-15)) ;
#95505 = DIRECTION('ref_axis',(0.,6.50521303491284E-15,1.)) ;
#95506 = DIRECTION('center_axis',(0.,-1.,0.)) ;
#95507 = DIRECTION('ref_axis',(0.,0.,-1.)) ;
#95508 = DIRECTION('center_axis',(0.,-1.,0.)) ;
#95509 = DIRECTION('ref_axis',(0.,0.,-1.)) ;
#95510 = DIRECTION('center_axis',(0.,-1.,-1.07081696047951E-16)) ;
#95511 = DIRECTION('ref_axis',(0.,1.07081696047951E-16,-1.)) ;
#95512 = DIRECTION('center_axis',(0.,1.,0.)) ;
#95513 = DIRECTION('ref_axis',(0.,0.,1.)) ;
#95514 = DIRECTION('center_axis',(-1.,0.,0.)) ;
#95515 = DIRECTION('ref_axis',(0.,0.,1.)) ;
#95516 = DIRECTION('center_axis',(0.,0.,1.)) ;
#95517 = DIRECTION('ref_axis',(1.,0.,0.)) ;
#95518 = DIRECTION('center_axis',(0.,1.,0.)) ;
#95519 = DIRECTION('ref_axis',(0.,0.,1.)) ;
#95520 = DIRECTION('center_axis',(0.,0.,-1.)) ;
#95521 = DIRECTION('ref_axis',(-1.,0.,0.)) ;
#95522 = DIRECTION('center_axis',(0.,0.,1.)) ;
#95523 = DIRECTION('ref_axis',(1.,0.,0.)) ;
#95524 = DIRECTION('center_axis',(0.,0.,1.)) ;
#95525 = DIRECTION('ref_axis',(1.,0.,0.)) ;
#95526 = DIRECTION('center_axis',(0.,0.,1.)) ;
#95527 = DIRECTION('ref_axis',(1.,0.,0.)) ;
#95528 = DIRECTION('center_axis',(0.,0.,-1.)) ;
#95529 = DIRECTION('ref_axis',(-1.,0.,0.)) ;
#95530 = DIRECTION('center_axis',(0.,1.,0.)) ;
#95531 = DIRECTION('ref_axis',(0.,0.,1.)) ;
#95532 = DIRECTION('center_axis',(0.,-0.707106781186532,0.707106781186563)) ;
#95533 = DIRECTION('ref_axis',(0.,-0.707106781186563,-0.707106781186532)) ;
#95534 = DIRECTION('center_axis',(0.,1.,0.)) ;
#95535 = DIRECTION('ref_axis',(0.,0.,1.)) ;
#95536 = DIRECTION('center_axis',(2.23012492569655E-15,-0.51423179695906,
-0.857651245551627)) ;
#95537 = DIRECTION('ref_axis',(2.6714619735869E-30,0.857651245551626,-0.51423179695906)) ;
#95538 = DIRECTION('center_axis',(0.,-0.707106781186548,0.707106781186547)) ;
#95539 = DIRECTION('ref_axis',(0.,-0.707106781186547,-0.707106781186548)) ;
#95540 = DIRECTION('center_axis',(0.,-0.707106781186543,0.707106781186552)) ;
#95541 = DIRECTION('ref_axis',(0.,-0.707106781186552,-0.707106781186543)) ;
#95542 = DIRECTION('center_axis',(-1.,0.,0.)) ;
#95543 = DIRECTION('ref_axis',(0.,0.,1.)) ;
#95544 = DIRECTION('center_axis',(-6.69037477709043E-15,0.51423179695912,
-0.85765124555159)) ;
#95545 = DIRECTION('ref_axis',(-4.44487660401203E-29,0.85765124555159,0.51423179695912)) ;
#95546 = DIRECTION('center_axis',(0.,1.,0.)) ;
#95547 = DIRECTION('ref_axis',(0.,0.,1.)) ;
#95548 = DIRECTION('center_axis',(0.,0.,-1.)) ;
#95549 = DIRECTION('ref_axis',(-1.,0.,0.)) ;
#95550 = DIRECTION('center_axis',(0.,1.,0.)) ;
#95551 = DIRECTION('ref_axis',(0.,0.,1.)) ;
#95552 = DIRECTION('center_axis',(0.,0.,-1.)) ;
#95553 = DIRECTION('ref_axis',(-1.,0.,0.)) ;
#95554 = DIRECTION('center_axis',(0.,0.,-1.)) ;
#95555 = DIRECTION('ref_axis',(-1.,0.,0.)) ;
#95556 = DIRECTION('center_axis',(0.,0.,1.)) ;
#95557 = DIRECTION('ref_axis',(1.,0.,0.)) ;
#95558 = DIRECTION('center_axis',(0.,0.,-1.)) ;
#95559 = DIRECTION('ref_axis',(-1.,0.,0.)) ;
#95560 = DIRECTION('center_axis',(0.,1.,0.)) ;
#95561 = DIRECTION('ref_axis',(0.,0.,1.)) ;
#95562 = DIRECTION('center_axis',(0.,-1.,8.67361737988379E-15)) ;
#95563 = DIRECTION('ref_axis',(0.,-8.67361737988379E-15,-1.)) ;
#95564 = DIRECTION('center_axis',(0.,0.707106781186546,0.707106781186549)) ;
#95565 = DIRECTION('ref_axis',(0.,-0.707106781186549,0.707106781186546)) ;
#95566 = DIRECTION('center_axis',(0.,0.707106781186534,0.707106781186561)) ;
#95567 = DIRECTION('ref_axis',(0.,-0.707106781186561,0.707106781186534)) ;
#95568 = DIRECTION('center_axis',(0.,1.,1.07081696047951E-16)) ;
#95569 = DIRECTION('ref_axis',(0.,-1.07081696047951E-16,1.)) ;
#95570 = DIRECTION('center_axis',(0.,-1.,0.)) ;
#95571 = DIRECTION('ref_axis',(0.,0.,-1.)) ;
#95572 = DIRECTION('center_axis',(0.,1.,0.)) ;
#95573 = DIRECTION('ref_axis',(0.,0.,1.)) ;
#95574 = DIRECTION('center_axis',(0.,0.,1.)) ;
#95575 = DIRECTION('ref_axis',(1.,0.,0.)) ;
#95576 = DIRECTION('center_axis',(0.,1.,0.)) ;
#95577 = DIRECTION('ref_axis',(0.,0.,1.)) ;
#95578 = DIRECTION('center_axis',(0.,6.93889390390723E-14,1.)) ;
#95579 = DIRECTION('ref_axis',(0.,-1.,6.93889390390723E-14)) ;
#95580 = DIRECTION('center_axis',(0.,3.99416362155027E-15,1.)) ;
#95581 = DIRECTION('ref_axis',(0.,-1.,3.99416362155027E-15)) ;
#95582 = DIRECTION('center_axis',(0.,0.,1.)) ;
#95583 = DIRECTION('ref_axis',(1.,0.,0.)) ;
#95584 = DIRECTION('center_axis',(0.,0.,-1.)) ;
#95585 = DIRECTION('ref_axis',(-1.,0.,0.)) ;
#95586 = DIRECTION('center_axis',(0.,0.,1.)) ;
#95587 = DIRECTION('ref_axis',(1.,0.,0.)) ;
#95588 = DIRECTION('center_axis',(-1.,0.,0.)) ;
#95589 = DIRECTION('ref_axis',(0.,0.,1.)) ;
#95590 = DIRECTION('center_axis',(0.,1.,0.)) ;
#95591 = DIRECTION('ref_axis',(0.,0.,1.)) ;
#95592 = DIRECTION('center_axis',(-1.,0.,0.)) ;
#95593 = DIRECTION('ref_axis',(0.,0.,1.)) ;
#95594 = DIRECTION('center_axis',(0.,-1.,0.)) ;
#95595 = DIRECTION('ref_axis',(0.,0.,-1.)) ;
#95596 = DIRECTION('center_axis',(0.,1.,0.)) ;
#95597 = DIRECTION('ref_axis',(0.,0.,1.)) ;
#95598 = DIRECTION('center_axis',(1.,-9.85638338623186E-18,0.)) ;
#95599 = DIRECTION('ref_axis',(9.85638338623186E-18,1.,0.)) ;
#95600 = DIRECTION('',(0.,0.,-1.)) ;
#95601 = DIRECTION('',(-9.85638338623186E-18,-1.,0.)) ;
#95602 = DIRECTION('',(0.,0.,1.)) ;
#95603 = DIRECTION('',(9.85638338623186E-18,1.,0.)) ;
#95604 = DIRECTION('center_axis',(0.707106781186548,0.707106781186548,0.)) ;
#95605 = DIRECTION('ref_axis',(-0.707106781186548,0.707106781186548,0.)) ;
#95606 = DIRECTION('',(0.,0.,1.)) ;
#95607 = DIRECTION('',(-0.577350269189625,0.577350269189625,0.577350269189627)) ;
#95608 = DIRECTION('',(0.,0.,-1.)) ;
#95609 = DIRECTION('',(0.577350269189625,-0.577350269189625,0.577350269189627)) ;
#95610 = DIRECTION('center_axis',(0.,1.,0.)) ;
#95611 = DIRECTION('ref_axis',(0.,0.,1.)) ;
#95612 = DIRECTION('',(0.,0.,1.)) ;
#95613 = DIRECTION('',(-1.,0.,-9.8563833862319E-18)) ;
#95614 = DIRECTION('',(0.,0.,-1.)) ;
#95615 = DIRECTION('',(1.,0.,-9.8563833862319E-18)) ;
#95616 = DIRECTION('center_axis',(-0.707106781186548,0.707106781186548,0.)) ;
#95617 = DIRECTION('ref_axis',(-0.707106781186548,-0.707106781186548,0.)) ;
#95618 = DIRECTION('',(0.,0.,1.)) ;
#95619 = DIRECTION('',(-0.577350269189625,-0.577350269189625,-0.577350269189627)) ;
#95620 = DIRECTION('',(0.,0.,-1.)) ;
#95621 = DIRECTION('',(0.577350269189625,0.577350269189625,-0.577350269189627)) ;
#95622 = DIRECTION('center_axis',(-1.,9.85638338623186E-18,0.)) ;
#95623 = DIRECTION('ref_axis',(-9.85638338623186E-18,-1.,0.)) ;
#95624 = DIRECTION('',(0.,0.,-1.)) ;
#95625 = DIRECTION('',(9.85638338623186E-18,1.,0.)) ;
#95626 = DIRECTION('',(0.,0.,-1.)) ;
#95627 = DIRECTION('',(-9.85638338623186E-18,-1.,0.)) ;
#95628 = DIRECTION('center_axis',(0.,0.,1.)) ;
#95629 = DIRECTION('ref_axis',(1.,0.,0.)) ;
#95630 = DIRECTION('',(9.85638338623186E-18,1.,0.)) ;
#95631 = DIRECTION('center_axis',(0.,0.,-1.)) ;
#95632 = DIRECTION('ref_axis',(1.,0.,0.)) ;
#95633 = DIRECTION('center_axis',(0.,0.,1.)) ;
#95634 = DIRECTION('ref_axis',(1.,0.,0.)) ;
#95635 = DIRECTION('',(-9.85638338623186E-18,-1.,0.)) ;
#95636 = DIRECTION('',(1.,-9.85638338623186E-18,0.)) ;
#95637 = DIRECTION('center_axis',(0.,0.,1.)) ;
#95638 = DIRECTION('ref_axis',(1.,0.,0.)) ;
#95639 = DIRECTION('',(9.85638338623186E-18,1.,0.)) ;
#95640 = DIRECTION('center_axis',(0.,0.,-1.)) ;
#95641 = DIRECTION('ref_axis',(1.,0.,0.)) ;
#95642 = DIRECTION('center_axis',(0.,0.,1.)) ;
#95643 = DIRECTION('ref_axis',(1.,0.,0.)) ;
#95644 = DIRECTION('',(-9.85638338623186E-18,-1.,0.)) ;
#95645 = DIRECTION('',(-1.,9.85638338623186E-18,0.)) ;
#95646 = DIRECTION('center_axis',(0.,0.,-1.)) ;
#95647 = DIRECTION('ref_axis',(-1.,0.,0.)) ;
#95648 = DIRECTION('center_axis',(0.,0.,1.)) ;
#95649 = DIRECTION('ref_axis',(1.,0.,0.)) ;
#95650 = DIRECTION('center_axis',(0.,0.,-1.)) ;
#95651 = DIRECTION('ref_axis',(1.,0.,0.)) ;
#95652 = DIRECTION('center_axis',(0.,0.,-1.)) ;
#95653 = DIRECTION('ref_axis',(-1.,0.,0.)) ;
#95654 = DIRECTION('center_axis',(0.,0.,-1.)) ;
#95655 = DIRECTION('ref_axis',(1.,0.,0.)) ;
#95656 = DIRECTION('center_axis',(0.,0.,1.)) ;
#95657 = DIRECTION('ref_axis',(1.,0.,0.)) ;
#95658 = DIRECTION('center_axis',(-0.707106781186548,-0.707106781186547,0.)) ;
#95659 = DIRECTION('ref_axis',(0.707106781186547,-0.707106781186548,0.)) ;
#95660 = DIRECTION('',(0.,0.,1.)) ;
#95661 = DIRECTION('',(0.577350269189625,-0.577350269189626,-0.577350269189626)) ;
#95662 = DIRECTION('',(0.,0.,-1.)) ;
#95663 = DIRECTION('',(-0.577350269189625,0.577350269189626,-0.577350269189626)) ;
#95664 = DIRECTION('center_axis',(1.95511867169517E-16,-1.,0.)) ;
#95665 = DIRECTION('ref_axis',(1.,1.95511867169517E-16,0.)) ;
#95666 = DIRECTION('',(0.,0.,-1.)) ;
#95667 = DIRECTION('',(-1.,-1.95511867169517E-16,0.)) ;
#95668 = DIRECTION('',(1.,1.95511867169517E-16,0.)) ;
#95669 = DIRECTION('center_axis',(1.06642836637918E-16,1.,0.)) ;
#95670 = DIRECTION('ref_axis',(-1.,1.06642836637918E-16,0.)) ;
#95671 = DIRECTION('',(1.,-1.06642836637919E-16,0.)) ;
#95672 = DIRECTION('',(0.,0.,1.)) ;
#95673 = DIRECTION('',(-1.,1.06642836637919E-16,0.)) ;
#95674 = DIRECTION('center_axis',(-0.707106781186548,0.707106781186547,0.)) ;
#95675 = DIRECTION('ref_axis',(-0.707106781186547,-0.707106781186548,0.)) ;
#95676 = DIRECTION('',(0.,0.,1.)) ;
#95677 = DIRECTION('',(-0.577350269189625,-0.577350269189626,0.577350269189627)) ;
#95678 = DIRECTION('',(0.,0.,-1.)) ;
#95679 = DIRECTION('',(0.577350269189625,0.577350269189626,0.577350269189627)) ;
#95680 = DIRECTION('center_axis',(-1.,0.,0.)) ;
#95681 = DIRECTION('ref_axis',(0.,0.,1.)) ;
#95682 = DIRECTION('',(0.,0.,-1.)) ;
#95683 = DIRECTION('',(0.,1.,1.95511867169518E-16)) ;
#95684 = DIRECTION('',(0.,0.,1.)) ;
#95685 = DIRECTION('',(0.,-1.,1.95511867169518E-16)) ;
#95686 = DIRECTION('center_axis',(0.,0.,1.)) ;
#95687 = DIRECTION('ref_axis',(1.,0.,0.)) ;
#95688 = DIRECTION('',(-1.95511867169517E-16,1.,0.)) ;
#95689 = DIRECTION('',(-1.,-1.95511867169517E-16,0.)) ;
#95690 = DIRECTION('',(1.,-1.06642836637919E-16,0.)) ;
#95691 = DIRECTION('center_axis',(0.,0.,1.)) ;
#95692 = DIRECTION('ref_axis',(1.,0.,0.)) ;
#95693 = DIRECTION('',(1.,1.95511867169517E-16,0.)) ;
#95694 = DIRECTION('',(1.95511867169517E-16,-1.,0.)) ;
#95695 = DIRECTION('',(-1.,1.06642836637919E-16,0.)) ;
#95696 = DIRECTION('center_axis',(1.,-9.85638338623186E-18,0.)) ;
#95697 = DIRECTION('ref_axis',(9.85638338623186E-18,1.,0.)) ;
#95698 = DIRECTION('',(0.,0.,-1.)) ;
#95699 = DIRECTION('',(-9.85638338623186E-18,-1.,0.)) ;
#95700 = DIRECTION('',(0.,0.,1.)) ;
#95701 = DIRECTION('',(9.85638338623186E-18,1.,0.)) ;
#95702 = DIRECTION('center_axis',(0.707106781186548,0.707106781186548,0.)) ;
#95703 = DIRECTION('ref_axis',(-0.707106781186548,0.707106781186548,0.)) ;
#95704 = DIRECTION('',(0.,0.,1.)) ;
#95705 = DIRECTION('',(-0.577350269189625,0.577350269189625,0.577350269189627)) ;
#95706 = DIRECTION('',(0.,0.,-1.)) ;
#95707 = DIRECTION('',(0.577350269189625,-0.577350269189625,0.577350269189627)) ;
#95708 = DIRECTION('center_axis',(0.,1.,0.)) ;
#95709 = DIRECTION('ref_axis',(0.,0.,1.)) ;
#95710 = DIRECTION('',(0.,0.,1.)) ;
#95711 = DIRECTION('',(-1.,0.,-9.8563833862319E-18)) ;
#95712 = DIRECTION('',(0.,0.,-1.)) ;
#95713 = DIRECTION('',(1.,0.,-9.8563833862319E-18)) ;
#95714 = DIRECTION('center_axis',(-0.707106781186548,0.707106781186548,0.)) ;
#95715 = DIRECTION('ref_axis',(-0.707106781186548,-0.707106781186548,0.)) ;
#95716 = DIRECTION('',(0.,0.,1.)) ;
#95717 = DIRECTION('',(-0.577350269189625,-0.577350269189625,-0.577350269189627)) ;
#95718 = DIRECTION('',(0.,0.,-1.)) ;
#95719 = DIRECTION('',(0.577350269189625,0.577350269189625,-0.577350269189627)) ;
#95720 = DIRECTION('center_axis',(-1.,9.85638338623186E-18,0.)) ;
#95721 = DIRECTION('ref_axis',(-9.85638338623186E-18,-1.,0.)) ;
#95722 = DIRECTION('',(0.,0.,-1.)) ;
#95723 = DIRECTION('',(9.85638338623186E-18,1.,0.)) ;
#95724 = DIRECTION('',(0.,0.,-1.)) ;
#95725 = DIRECTION('',(-9.85638338623186E-18,-1.,0.)) ;
#95726 = DIRECTION('center_axis',(0.,0.,1.)) ;
#95727 = DIRECTION('ref_axis',(1.,0.,0.)) ;
#95728 = DIRECTION('',(9.85638338623186E-18,1.,0.)) ;
#95729 = DIRECTION('center_axis',(0.,0.,-1.)) ;
#95730 = DIRECTION('ref_axis',(1.,0.,0.)) ;
#95731 = DIRECTION('center_axis',(0.,0.,1.)) ;
#95732 = DIRECTION('ref_axis',(1.,0.,0.)) ;
#95733 = DIRECTION('',(-9.85638338623186E-18,-1.,0.)) ;
#95734 = DIRECTION('',(1.,-9.85638338623186E-18,0.)) ;
#95735 = DIRECTION('center_axis',(0.,0.,1.)) ;
#95736 = DIRECTION('ref_axis',(1.,0.,0.)) ;
#95737 = DIRECTION('',(9.85638338623186E-18,1.,0.)) ;
#95738 = DIRECTION('center_axis',(0.,0.,-1.)) ;
#95739 = DIRECTION('ref_axis',(1.,0.,0.)) ;
#95740 = DIRECTION('center_axis',(0.,0.,1.)) ;
#95741 = DIRECTION('ref_axis',(1.,0.,0.)) ;
#95742 = DIRECTION('',(-9.85638338623186E-18,-1.,0.)) ;
#95743 = DIRECTION('',(-1.,9.85638338623186E-18,0.)) ;
#95744 = DIRECTION('center_axis',(0.,0.,-1.)) ;
#95745 = DIRECTION('ref_axis',(-1.,0.,0.)) ;
#95746 = DIRECTION('center_axis',(0.,0.,1.)) ;
#95747 = DIRECTION('ref_axis',(1.,0.,0.)) ;
#95748 = DIRECTION('center_axis',(0.,0.,-1.)) ;
#95749 = DIRECTION('ref_axis',(1.,0.,0.)) ;
#95750 = DIRECTION('center_axis',(0.,0.,-1.)) ;
#95751 = DIRECTION('ref_axis',(-1.,0.,0.)) ;
#95752 = DIRECTION('center_axis',(0.,0.,-1.)) ;
#95753 = DIRECTION('ref_axis',(1.,0.,0.)) ;
#95754 = DIRECTION('center_axis',(0.,0.,1.)) ;
#95755 = DIRECTION('ref_axis',(1.,0.,0.)) ;
#95756 = DIRECTION('center_axis',(-0.707106781186548,-0.707106781186547,0.)) ;
#95757 = DIRECTION('ref_axis',(0.707106781186547,-0.707106781186548,0.)) ;
#95758 = DIRECTION('',(0.,0.,1.)) ;
#95759 = DIRECTION('',(0.577350269189625,-0.577350269189626,-0.577350269189626)) ;
#95760 = DIRECTION('',(0.,0.,-1.)) ;
#95761 = DIRECTION('',(-0.577350269189625,0.577350269189626,-0.577350269189626)) ;
#95762 = DIRECTION('center_axis',(1.95511867169517E-16,-1.,0.)) ;
#95763 = DIRECTION('ref_axis',(1.,1.95511867169517E-16,0.)) ;
#95764 = DIRECTION('',(0.,0.,-1.)) ;
#95765 = DIRECTION('',(-1.,-1.95511867169517E-16,0.)) ;
#95766 = DIRECTION('',(1.,1.95511867169517E-16,0.)) ;
#95767 = DIRECTION('center_axis',(1.06642836637918E-16,1.,0.)) ;
#95768 = DIRECTION('ref_axis',(-1.,1.06642836637918E-16,0.)) ;
#95769 = DIRECTION('',(1.,-1.06642836637919E-16,0.)) ;
#95770 = DIRECTION('',(0.,0.,1.)) ;
#95771 = DIRECTION('',(-1.,1.06642836637919E-16,0.)) ;
#95772 = DIRECTION('center_axis',(-0.707106781186548,0.707106781186547,0.)) ;
#95773 = DIRECTION('ref_axis',(-0.707106781186547,-0.707106781186548,0.)) ;
#95774 = DIRECTION('',(0.,0.,1.)) ;
#95775 = DIRECTION('',(-0.577350269189625,-0.577350269189626,0.577350269189627)) ;
#95776 = DIRECTION('',(0.,0.,-1.)) ;
#95777 = DIRECTION('',(0.577350269189625,0.577350269189626,0.577350269189627)) ;
#95778 = DIRECTION('center_axis',(-1.,0.,0.)) ;
#95779 = DIRECTION('ref_axis',(0.,0.,1.)) ;
#95780 = DIRECTION('',(0.,0.,-1.)) ;
#95781 = DIRECTION('',(0.,1.,1.95511867169518E-16)) ;
#95782 = DIRECTION('',(0.,0.,1.)) ;
#95783 = DIRECTION('',(0.,-1.,1.95511867169518E-16)) ;
#95784 = DIRECTION('center_axis',(0.,0.,1.)) ;
#95785 = DIRECTION('ref_axis',(1.,0.,0.)) ;
#95786 = DIRECTION('',(-1.95511867169517E-16,1.,0.)) ;
#95787 = DIRECTION('',(-1.,-1.95511867169517E-16,0.)) ;
#95788 = DIRECTION('',(1.,-1.06642836637919E-16,0.)) ;
#95789 = DIRECTION('center_axis',(0.,0.,1.)) ;
#95790 = DIRECTION('ref_axis',(1.,0.,0.)) ;
#95791 = DIRECTION('',(1.,1.95511867169517E-16,0.)) ;
#95792 = DIRECTION('',(1.95511867169517E-16,-1.,0.)) ;
#95793 = DIRECTION('',(-1.,1.06642836637919E-16,0.)) ;
#95794 = DIRECTION('center_axis',(1.,-9.85638338623186E-18,0.)) ;
#95795 = DIRECTION('ref_axis',(9.85638338623186E-18,1.,0.)) ;
#95796 = DIRECTION('',(0.,0.,-1.)) ;
#95797 = DIRECTION('',(-9.85638338623186E-18,-1.,0.)) ;
#95798 = DIRECTION('',(0.,0.,1.)) ;
#95799 = DIRECTION('',(9.85638338623186E-18,1.,0.)) ;
#95800 = DIRECTION('center_axis',(0.707106781186548,0.707106781186548,0.)) ;
#95801 = DIRECTION('ref_axis',(-0.707106781186548,0.707106781186548,0.)) ;
#95802 = DIRECTION('',(0.,0.,1.)) ;
#95803 = DIRECTION('',(-0.577350269189625,0.577350269189625,0.577350269189627)) ;
#95804 = DIRECTION('',(0.,0.,-1.)) ;
#95805 = DIRECTION('',(0.577350269189625,-0.577350269189625,0.577350269189627)) ;
#95806 = DIRECTION('center_axis',(0.,1.,0.)) ;
#95807 = DIRECTION('ref_axis',(0.,0.,1.)) ;
#95808 = DIRECTION('',(0.,0.,1.)) ;
#95809 = DIRECTION('',(-1.,0.,-9.8563833862319E-18)) ;
#95810 = DIRECTION('',(0.,0.,-1.)) ;
#95811 = DIRECTION('',(1.,0.,-9.8563833862319E-18)) ;
#95812 = DIRECTION('center_axis',(-0.707106781186548,0.707106781186548,0.)) ;
#95813 = DIRECTION('ref_axis',(-0.707106781186548,-0.707106781186548,0.)) ;
#95814 = DIRECTION('',(0.,0.,1.)) ;
#95815 = DIRECTION('',(-0.577350269189625,-0.577350269189625,-0.577350269189627)) ;
#95816 = DIRECTION('',(0.,0.,-1.)) ;
#95817 = DIRECTION('',(0.577350269189625,0.577350269189625,-0.577350269189627)) ;
#95818 = DIRECTION('center_axis',(-1.,9.85638338623186E-18,0.)) ;
#95819 = DIRECTION('ref_axis',(-9.85638338623186E-18,-1.,0.)) ;
#95820 = DIRECTION('',(0.,0.,-1.)) ;
#95821 = DIRECTION('',(9.85638338623186E-18,1.,0.)) ;
#95822 = DIRECTION('',(0.,0.,-1.)) ;
#95823 = DIRECTION('',(-9.85638338623186E-18,-1.,0.)) ;
#95824 = DIRECTION('center_axis',(0.,0.,1.)) ;
#95825 = DIRECTION('ref_axis',(1.,0.,0.)) ;
#95826 = DIRECTION('',(9.85638338623186E-18,1.,0.)) ;
#95827 = DIRECTION('center_axis',(0.,0.,-1.)) ;
#95828 = DIRECTION('ref_axis',(1.,0.,0.)) ;
#95829 = DIRECTION('center_axis',(0.,0.,1.)) ;
#95830 = DIRECTION('ref_axis',(1.,0.,0.)) ;
#95831 = DIRECTION('',(-9.85638338623186E-18,-1.,0.)) ;
#95832 = DIRECTION('',(1.,-9.85638338623186E-18,0.)) ;
#95833 = DIRECTION('center_axis',(0.,0.,1.)) ;
#95834 = DIRECTION('ref_axis',(1.,0.,0.)) ;
#95835 = DIRECTION('',(9.85638338623186E-18,1.,0.)) ;
#95836 = DIRECTION('center_axis',(0.,0.,-1.)) ;
#95837 = DIRECTION('ref_axis',(1.,0.,0.)) ;
#95838 = DIRECTION('center_axis',(0.,0.,1.)) ;
#95839 = DIRECTION('ref_axis',(1.,0.,0.)) ;
#95840 = DIRECTION('',(-9.85638338623186E-18,-1.,0.)) ;
#95841 = DIRECTION('',(-1.,9.85638338623186E-18,0.)) ;
#95842 = DIRECTION('center_axis',(0.,0.,-1.)) ;
#95843 = DIRECTION('ref_axis',(-1.,0.,0.)) ;
#95844 = DIRECTION('center_axis',(0.,0.,1.)) ;
#95845 = DIRECTION('ref_axis',(1.,0.,0.)) ;
#95846 = DIRECTION('center_axis',(0.,0.,-1.)) ;
#95847 = DIRECTION('ref_axis',(1.,0.,0.)) ;
#95848 = DIRECTION('center_axis',(0.,0.,-1.)) ;
#95849 = DIRECTION('ref_axis',(-1.,0.,0.)) ;
#95850 = DIRECTION('center_axis',(0.,0.,-1.)) ;
#95851 = DIRECTION('ref_axis',(1.,0.,0.)) ;
#95852 = DIRECTION('center_axis',(0.,0.,1.)) ;
#95853 = DIRECTION('ref_axis',(1.,0.,0.)) ;
#95854 = DIRECTION('center_axis',(-0.707106781186548,-0.707106781186547,0.)) ;
#95855 = DIRECTION('ref_axis',(0.707106781186547,-0.707106781186548,0.)) ;
#95856 = DIRECTION('',(0.,0.,1.)) ;
#95857 = DIRECTION('',(0.577350269189625,-0.577350269189626,-0.577350269189626)) ;
#95858 = DIRECTION('',(0.,0.,-1.)) ;
#95859 = DIRECTION('',(-0.577350269189625,0.577350269189626,-0.577350269189626)) ;
#95860 = DIRECTION('center_axis',(1.95511867169517E-16,-1.,0.)) ;
#95861 = DIRECTION('ref_axis',(1.,1.95511867169517E-16,0.)) ;
#95862 = DIRECTION('',(0.,0.,-1.)) ;
#95863 = DIRECTION('',(-1.,-1.95511867169517E-16,0.)) ;
#95864 = DIRECTION('',(1.,1.95511867169517E-16,0.)) ;
#95865 = DIRECTION('center_axis',(1.06642836637918E-16,1.,0.)) ;
#95866 = DIRECTION('ref_axis',(-1.,1.06642836637918E-16,0.)) ;
#95867 = DIRECTION('',(1.,-1.06642836637919E-16,0.)) ;
#95868 = DIRECTION('',(0.,0.,1.)) ;
#95869 = DIRECTION('',(-1.,1.06642836637919E-16,0.)) ;
#95870 = DIRECTION('center_axis',(-0.707106781186548,0.707106781186547,0.)) ;
#95871 = DIRECTION('ref_axis',(-0.707106781186547,-0.707106781186548,0.)) ;
#95872 = DIRECTION('',(0.,0.,1.)) ;
#95873 = DIRECTION('',(-0.577350269189625,-0.577350269189626,0.577350269189627)) ;
#95874 = DIRECTION('',(0.,0.,-1.)) ;
#95875 = DIRECTION('',(0.577350269189625,0.577350269189626,0.577350269189627)) ;
#95876 = DIRECTION('center_axis',(-1.,0.,0.)) ;
#95877 = DIRECTION('ref_axis',(0.,0.,1.)) ;
#95878 = DIRECTION('',(0.,0.,-1.)) ;
#95879 = DIRECTION('',(0.,1.,1.95511867169518E-16)) ;
#95880 = DIRECTION('',(0.,0.,1.)) ;
#95881 = DIRECTION('',(0.,-1.,1.95511867169518E-16)) ;
#95882 = DIRECTION('center_axis',(0.,0.,1.)) ;
#95883 = DIRECTION('ref_axis',(1.,0.,0.)) ;
#95884 = DIRECTION('',(-1.95511867169517E-16,1.,0.)) ;
#95885 = DIRECTION('',(-1.,-1.95511867169517E-16,0.)) ;
#95886 = DIRECTION('',(1.,-1.06642836637919E-16,0.)) ;
#95887 = DIRECTION('center_axis',(0.,0.,1.)) ;
#95888 = DIRECTION('ref_axis',(1.,0.,0.)) ;
#95889 = DIRECTION('',(1.,1.95511867169517E-16,0.)) ;
#95890 = DIRECTION('',(1.95511867169517E-16,-1.,0.)) ;
#95891 = DIRECTION('',(-1.,1.06642836637919E-16,0.)) ;
#95892 = DIRECTION('center_axis',(1.,-9.85638338623186E-18,0.)) ;
#95893 = DIRECTION('ref_axis',(9.85638338623186E-18,1.,0.)) ;
#95894 = DIRECTION('',(0.,0.,-1.)) ;
#95895 = DIRECTION('',(-9.85638338623186E-18,-1.,0.)) ;
#95896 = DIRECTION('',(0.,0.,1.)) ;
#95897 = DIRECTION('',(9.85638338623186E-18,1.,0.)) ;
#95898 = DIRECTION('center_axis',(0.707106781186548,0.707106781186548,0.)) ;
#95899 = DIRECTION('ref_axis',(-0.707106781186548,0.707106781186548,0.)) ;
#95900 = DIRECTION('',(0.,0.,1.)) ;
#95901 = DIRECTION('',(-0.577350269189625,0.577350269189625,0.577350269189627)) ;
#95902 = DIRECTION('',(0.,0.,-1.)) ;
#95903 = DIRECTION('',(0.577350269189625,-0.577350269189625,0.577350269189627)) ;
#95904 = DIRECTION('center_axis',(0.,1.,0.)) ;
#95905 = DIRECTION('ref_axis',(0.,0.,1.)) ;
#95906 = DIRECTION('',(0.,0.,1.)) ;
#95907 = DIRECTION('',(-1.,0.,-9.8563833862319E-18)) ;
#95908 = DIRECTION('',(0.,0.,-1.)) ;
#95909 = DIRECTION('',(1.,0.,-9.8563833862319E-18)) ;
#95910 = DIRECTION('center_axis',(-0.707106781186548,0.707106781186548,0.)) ;
#95911 = DIRECTION('ref_axis',(-0.707106781186548,-0.707106781186548,0.)) ;
#95912 = DIRECTION('',(0.,0.,1.)) ;
#95913 = DIRECTION('',(-0.577350269189625,-0.577350269189625,-0.577350269189627)) ;
#95914 = DIRECTION('',(0.,0.,-1.)) ;
#95915 = DIRECTION('',(0.577350269189625,0.577350269189625,-0.577350269189627)) ;
#95916 = DIRECTION('center_axis',(-1.,9.85638338623186E-18,0.)) ;
#95917 = DIRECTION('ref_axis',(-9.85638338623186E-18,-1.,0.)) ;
#95918 = DIRECTION('',(0.,0.,-1.)) ;
#95919 = DIRECTION('',(9.85638338623186E-18,1.,0.)) ;
#95920 = DIRECTION('',(0.,0.,-1.)) ;
#95921 = DIRECTION('',(-9.85638338623186E-18,-1.,0.)) ;
#95922 = DIRECTION('center_axis',(0.,0.,1.)) ;
#95923 = DIRECTION('ref_axis',(1.,0.,0.)) ;
#95924 = DIRECTION('',(9.85638338623186E-18,1.,0.)) ;
#95925 = DIRECTION('center_axis',(0.,0.,-1.)) ;
#95926 = DIRECTION('ref_axis',(1.,0.,0.)) ;
#95927 = DIRECTION('center_axis',(0.,0.,1.)) ;
#95928 = DIRECTION('ref_axis',(1.,0.,0.)) ;
#95929 = DIRECTION('',(-9.85638338623186E-18,-1.,0.)) ;
#95930 = DIRECTION('',(1.,-9.85638338623186E-18,0.)) ;
#95931 = DIRECTION('center_axis',(0.,0.,1.)) ;
#95932 = DIRECTION('ref_axis',(1.,0.,0.)) ;
#95933 = DIRECTION('',(9.85638338623186E-18,1.,0.)) ;
#95934 = DIRECTION('center_axis',(0.,0.,-1.)) ;
#95935 = DIRECTION('ref_axis',(1.,0.,0.)) ;
#95936 = DIRECTION('center_axis',(0.,0.,1.)) ;
#95937 = DIRECTION('ref_axis',(1.,0.,0.)) ;
#95938 = DIRECTION('',(-9.85638338623186E-18,-1.,0.)) ;
#95939 = DIRECTION('',(-1.,9.85638338623186E-18,0.)) ;
#95940 = DIRECTION('center_axis',(0.,0.,-1.)) ;
#95941 = DIRECTION('ref_axis',(-1.,0.,0.)) ;
#95942 = DIRECTION('center_axis',(0.,0.,1.)) ;
#95943 = DIRECTION('ref_axis',(1.,0.,0.)) ;
#95944 = DIRECTION('center_axis',(0.,0.,-1.)) ;
#95945 = DIRECTION('ref_axis',(1.,0.,0.)) ;
#95946 = DIRECTION('center_axis',(0.,0.,-1.)) ;
#95947 = DIRECTION('ref_axis',(-1.,0.,0.)) ;
#95948 = DIRECTION('center_axis',(0.,0.,-1.)) ;
#95949 = DIRECTION('ref_axis',(1.,0.,0.)) ;
#95950 = DIRECTION('center_axis',(0.,0.,1.)) ;
#95951 = DIRECTION('ref_axis',(1.,0.,0.)) ;
#95952 = DIRECTION('center_axis',(-0.707106781186548,-0.707106781186547,0.)) ;
#95953 = DIRECTION('ref_axis',(0.707106781186547,-0.707106781186548,0.)) ;
#95954 = DIRECTION('',(0.,0.,1.)) ;
#95955 = DIRECTION('',(0.577350269189625,-0.577350269189626,-0.577350269189626)) ;
#95956 = DIRECTION('',(0.,0.,-1.)) ;
#95957 = DIRECTION('',(-0.577350269189625,0.577350269189626,-0.577350269189626)) ;
#95958 = DIRECTION('center_axis',(1.95511867169517E-16,-1.,0.)) ;
#95959 = DIRECTION('ref_axis',(1.,1.95511867169517E-16,0.)) ;
#95960 = DIRECTION('',(0.,0.,-1.)) ;
#95961 = DIRECTION('',(-1.,-1.95511867169517E-16,0.)) ;
#95962 = DIRECTION('',(1.,1.95511867169517E-16,0.)) ;
#95963 = DIRECTION('center_axis',(1.06642836637918E-16,1.,0.)) ;
#95964 = DIRECTION('ref_axis',(-1.,1.06642836637918E-16,0.)) ;
#95965 = DIRECTION('',(1.,-1.06642836637919E-16,0.)) ;
#95966 = DIRECTION('',(0.,0.,1.)) ;
#95967 = DIRECTION('',(-1.,1.06642836637919E-16,0.)) ;
#95968 = DIRECTION('center_axis',(-0.707106781186548,0.707106781186547,0.)) ;
#95969 = DIRECTION('ref_axis',(-0.707106781186547,-0.707106781186548,0.)) ;
#95970 = DIRECTION('',(0.,0.,1.)) ;
#95971 = DIRECTION('',(-0.577350269189625,-0.577350269189626,0.577350269189627)) ;
#95972 = DIRECTION('',(0.,0.,-1.)) ;
#95973 = DIRECTION('',(0.577350269189625,0.577350269189626,0.577350269189627)) ;
#95974 = DIRECTION('center_axis',(-1.,0.,0.)) ;
#95975 = DIRECTION('ref_axis',(0.,0.,1.)) ;
#95976 = DIRECTION('',(0.,0.,-1.)) ;
#95977 = DIRECTION('',(0.,1.,1.95511867169518E-16)) ;
#95978 = DIRECTION('',(0.,0.,1.)) ;
#95979 = DIRECTION('',(0.,-1.,1.95511867169518E-16)) ;
#95980 = DIRECTION('center_axis',(0.,0.,1.)) ;
#95981 = DIRECTION('ref_axis',(1.,0.,0.)) ;
#95982 = DIRECTION('',(-1.95511867169517E-16,1.,0.)) ;
#95983 = DIRECTION('',(-1.,-1.95511867169517E-16,0.)) ;
#95984 = DIRECTION('',(1.,-1.06642836637919E-16,0.)) ;
#95985 = DIRECTION('center_axis',(0.,0.,1.)) ;
#95986 = DIRECTION('ref_axis',(1.,0.,0.)) ;
#95987 = DIRECTION('',(1.,1.95511867169517E-16,0.)) ;
#95988 = DIRECTION('',(1.95511867169517E-16,-1.,0.)) ;
#95989 = DIRECTION('',(-1.,1.06642836637919E-16,0.)) ;
#95990 = DIRECTION('center_axis',(1.,-9.85638338623186E-18,0.)) ;
#95991 = DIRECTION('ref_axis',(9.85638338623186E-18,1.,0.)) ;
#95992 = DIRECTION('',(0.,0.,-1.)) ;
#95993 = DIRECTION('',(-9.85638338623186E-18,-1.,0.)) ;
#95994 = DIRECTION('',(0.,0.,1.)) ;
#95995 = DIRECTION('',(9.85638338623186E-18,1.,0.)) ;
#95996 = DIRECTION('center_axis',(0.707106781186548,0.707106781186548,0.)) ;
#95997 = DIRECTION('ref_axis',(-0.707106781186548,0.707106781186548,0.)) ;
#95998 = DIRECTION('',(0.,0.,1.)) ;
#95999 = DIRECTION('',(-0.577350269189625,0.577350269189625,0.577350269189627)) ;
#96000 = DIRECTION('',(0.,0.,-1.)) ;
#96001 = DIRECTION('',(0.577350269189625,-0.577350269189625,0.577350269189627)) ;
#96002 = DIRECTION('center_axis',(0.,1.,0.)) ;
#96003 = DIRECTION('ref_axis',(0.,0.,1.)) ;
#96004 = DIRECTION('',(0.,0.,1.)) ;
#96005 = DIRECTION('',(-1.,0.,-9.8563833862319E-18)) ;
#96006 = DIRECTION('',(0.,0.,-1.)) ;
#96007 = DIRECTION('',(1.,0.,-9.8563833862319E-18)) ;
#96008 = DIRECTION('center_axis',(-0.707106781186548,0.707106781186548,0.)) ;
#96009 = DIRECTION('ref_axis',(-0.707106781186548,-0.707106781186548,0.)) ;
#96010 = DIRECTION('',(0.,0.,1.)) ;
#96011 = DIRECTION('',(-0.577350269189625,-0.577350269189625,-0.577350269189627)) ;
#96012 = DIRECTION('',(0.,0.,-1.)) ;
#96013 = DIRECTION('',(0.577350269189625,0.577350269189625,-0.577350269189627)) ;
#96014 = DIRECTION('center_axis',(-1.,9.85638338623186E-18,0.)) ;
#96015 = DIRECTION('ref_axis',(-9.85638338623186E-18,-1.,0.)) ;
#96016 = DIRECTION('',(0.,0.,-1.)) ;
#96017 = DIRECTION('',(9.85638338623186E-18,1.,0.)) ;
#96018 = DIRECTION('',(0.,0.,-1.)) ;
#96019 = DIRECTION('',(-9.85638338623186E-18,-1.,0.)) ;
#96020 = DIRECTION('center_axis',(0.,0.,1.)) ;
#96021 = DIRECTION('ref_axis',(1.,0.,0.)) ;
#96022 = DIRECTION('',(9.85638338623186E-18,1.,0.)) ;
#96023 = DIRECTION('center_axis',(0.,0.,-1.)) ;
#96024 = DIRECTION('ref_axis',(1.,0.,0.)) ;
#96025 = DIRECTION('center_axis',(0.,0.,1.)) ;
#96026 = DIRECTION('ref_axis',(1.,0.,0.)) ;
#96027 = DIRECTION('',(-9.85638338623186E-18,-1.,0.)) ;
#96028 = DIRECTION('',(1.,-9.85638338623186E-18,0.)) ;
#96029 = DIRECTION('center_axis',(0.,0.,1.)) ;
#96030 = DIRECTION('ref_axis',(1.,0.,0.)) ;
#96031 = DIRECTION('',(9.85638338623186E-18,1.,0.)) ;
#96032 = DIRECTION('center_axis',(0.,0.,-1.)) ;
#96033 = DIRECTION('ref_axis',(1.,0.,0.)) ;
#96034 = DIRECTION('center_axis',(0.,0.,1.)) ;
#96035 = DIRECTION('ref_axis',(1.,0.,0.)) ;
#96036 = DIRECTION('',(-9.85638338623186E-18,-1.,0.)) ;
#96037 = DIRECTION('',(-1.,9.85638338623186E-18,0.)) ;
#96038 = DIRECTION('center_axis',(0.,0.,-1.)) ;
#96039 = DIRECTION('ref_axis',(-1.,0.,0.)) ;
#96040 = DIRECTION('center_axis',(0.,0.,1.)) ;
#96041 = DIRECTION('ref_axis',(1.,0.,0.)) ;
#96042 = DIRECTION('center_axis',(0.,0.,-1.)) ;
#96043 = DIRECTION('ref_axis',(1.,0.,0.)) ;
#96044 = DIRECTION('center_axis',(0.,0.,-1.)) ;
#96045 = DIRECTION('ref_axis',(-1.,0.,0.)) ;
#96046 = DIRECTION('center_axis',(0.,0.,-1.)) ;
#96047 = DIRECTION('ref_axis',(1.,0.,0.)) ;
#96048 = DIRECTION('center_axis',(0.,0.,1.)) ;
#96049 = DIRECTION('ref_axis',(1.,0.,0.)) ;
#96050 = DIRECTION('center_axis',(-0.707106781186548,-0.707106781186547,0.)) ;
#96051 = DIRECTION('ref_axis',(0.707106781186547,-0.707106781186548,0.)) ;
#96052 = DIRECTION('',(0.,0.,1.)) ;
#96053 = DIRECTION('',(0.577350269189625,-0.577350269189626,-0.577350269189626)) ;
#96054 = DIRECTION('',(0.,0.,-1.)) ;
#96055 = DIRECTION('',(-0.577350269189625,0.577350269189626,-0.577350269189626)) ;
#96056 = DIRECTION('center_axis',(1.95511867169517E-16,-1.,0.)) ;
#96057 = DIRECTION('ref_axis',(1.,1.95511867169517E-16,0.)) ;
#96058 = DIRECTION('',(0.,0.,-1.)) ;
#96059 = DIRECTION('',(-1.,-1.95511867169517E-16,0.)) ;
#96060 = DIRECTION('',(1.,1.95511867169517E-16,0.)) ;
#96061 = DIRECTION('center_axis',(1.06642836637918E-16,1.,0.)) ;
#96062 = DIRECTION('ref_axis',(-1.,1.06642836637918E-16,0.)) ;
#96063 = DIRECTION('',(1.,-1.06642836637919E-16,0.)) ;
#96064 = DIRECTION('',(0.,0.,1.)) ;
#96065 = DIRECTION('',(-1.,1.06642836637919E-16,0.)) ;
#96066 = DIRECTION('center_axis',(-0.707106781186548,0.707106781186547,0.)) ;
#96067 = DIRECTION('ref_axis',(-0.707106781186547,-0.707106781186548,0.)) ;
#96068 = DIRECTION('',(0.,0.,1.)) ;
#96069 = DIRECTION('',(-0.577350269189625,-0.577350269189626,0.577350269189627)) ;
#96070 = DIRECTION('',(0.,0.,-1.)) ;
#96071 = DIRECTION('',(0.577350269189625,0.577350269189626,0.577350269189627)) ;
#96072 = DIRECTION('center_axis',(-1.,0.,0.)) ;
#96073 = DIRECTION('ref_axis',(0.,0.,1.)) ;
#96074 = DIRECTION('',(0.,0.,-1.)) ;
#96075 = DIRECTION('',(0.,1.,1.95511867169518E-16)) ;
#96076 = DIRECTION('',(0.,0.,1.)) ;
#96077 = DIRECTION('',(0.,-1.,1.95511867169518E-16)) ;
#96078 = DIRECTION('center_axis',(0.,0.,1.)) ;
#96079 = DIRECTION('ref_axis',(1.,0.,0.)) ;
#96080 = DIRECTION('',(-1.95511867169517E-16,1.,0.)) ;
#96081 = DIRECTION('',(-1.,-1.95511867169517E-16,0.)) ;
#96082 = DIRECTION('',(1.,-1.06642836637919E-16,0.)) ;
#96083 = DIRECTION('center_axis',(0.,0.,1.)) ;
#96084 = DIRECTION('ref_axis',(1.,0.,0.)) ;
#96085 = DIRECTION('',(1.,1.95511867169517E-16,0.)) ;
#96086 = DIRECTION('',(1.95511867169517E-16,-1.,0.)) ;
#96087 = DIRECTION('',(-1.,1.06642836637919E-16,0.)) ;
#96088 = DIRECTION('center_axis',(1.,-9.85638338623186E-18,0.)) ;
#96089 = DIRECTION('ref_axis',(9.85638338623186E-18,1.,0.)) ;
#96090 = DIRECTION('',(0.,0.,-1.)) ;
#96091 = DIRECTION('',(-9.85638338623186E-18,-1.,0.)) ;
#96092 = DIRECTION('',(0.,0.,1.)) ;
#96093 = DIRECTION('',(9.85638338623186E-18,1.,0.)) ;
#96094 = DIRECTION('center_axis',(0.707106781186548,0.707106781186548,0.)) ;
#96095 = DIRECTION('ref_axis',(-0.707106781186548,0.707106781186548,0.)) ;
#96096 = DIRECTION('',(0.,0.,1.)) ;
#96097 = DIRECTION('',(-0.577350269189625,0.577350269189625,0.577350269189627)) ;
#96098 = DIRECTION('',(0.,0.,-1.)) ;
#96099 = DIRECTION('',(0.577350269189625,-0.577350269189625,0.577350269189627)) ;
#96100 = DIRECTION('center_axis',(0.,1.,0.)) ;
#96101 = DIRECTION('ref_axis',(0.,0.,1.)) ;
#96102 = DIRECTION('',(0.,0.,1.)) ;
#96103 = DIRECTION('',(-1.,0.,-9.8563833862319E-18)) ;
#96104 = DIRECTION('',(0.,0.,-1.)) ;
#96105 = DIRECTION('',(1.,0.,-9.8563833862319E-18)) ;
#96106 = DIRECTION('center_axis',(-0.707106781186548,0.707106781186548,0.)) ;
#96107 = DIRECTION('ref_axis',(-0.707106781186548,-0.707106781186548,0.)) ;
#96108 = DIRECTION('',(0.,0.,1.)) ;
#96109 = DIRECTION('',(-0.577350269189625,-0.577350269189625,-0.577350269189627)) ;
#96110 = DIRECTION('',(0.,0.,-1.)) ;
#96111 = DIRECTION('',(0.577350269189625,0.577350269189625,-0.577350269189627)) ;
#96112 = DIRECTION('center_axis',(-1.,9.85638338623186E-18,0.)) ;
#96113 = DIRECTION('ref_axis',(-9.85638338623186E-18,-1.,0.)) ;
#96114 = DIRECTION('',(0.,0.,-1.)) ;
#96115 = DIRECTION('',(9.85638338623186E-18,1.,0.)) ;
#96116 = DIRECTION('',(0.,0.,-1.)) ;
#96117 = DIRECTION('',(-9.85638338623186E-18,-1.,0.)) ;
#96118 = DIRECTION('center_axis',(0.,0.,1.)) ;
#96119 = DIRECTION('ref_axis',(1.,0.,0.)) ;
#96120 = DIRECTION('',(9.85638338623186E-18,1.,0.)) ;
#96121 = DIRECTION('center_axis',(0.,0.,-1.)) ;
#96122 = DIRECTION('ref_axis',(1.,0.,0.)) ;
#96123 = DIRECTION('center_axis',(0.,0.,1.)) ;
#96124 = DIRECTION('ref_axis',(1.,0.,0.)) ;
#96125 = DIRECTION('',(-9.85638338623186E-18,-1.,0.)) ;
#96126 = DIRECTION('',(1.,-9.85638338623186E-18,0.)) ;
#96127 = DIRECTION('center_axis',(0.,0.,1.)) ;
#96128 = DIRECTION('ref_axis',(1.,0.,0.)) ;
#96129 = DIRECTION('',(9.85638338623186E-18,1.,0.)) ;
#96130 = DIRECTION('center_axis',(0.,0.,-1.)) ;
#96131 = DIRECTION('ref_axis',(1.,0.,0.)) ;
#96132 = DIRECTION('center_axis',(0.,0.,1.)) ;
#96133 = DIRECTION('ref_axis',(1.,0.,0.)) ;
#96134 = DIRECTION('',(-9.85638338623186E-18,-1.,0.)) ;
#96135 = DIRECTION('',(-1.,9.85638338623186E-18,0.)) ;
#96136 = DIRECTION('center_axis',(0.,0.,-1.)) ;
#96137 = DIRECTION('ref_axis',(-1.,0.,0.)) ;
#96138 = DIRECTION('center_axis',(0.,0.,1.)) ;
#96139 = DIRECTION('ref_axis',(1.,0.,0.)) ;
#96140 = DIRECTION('center_axis',(0.,0.,-1.)) ;
#96141 = DIRECTION('ref_axis',(1.,0.,0.)) ;
#96142 = DIRECTION('center_axis',(0.,0.,-1.)) ;
#96143 = DIRECTION('ref_axis',(-1.,0.,0.)) ;
#96144 = DIRECTION('center_axis',(0.,0.,-1.)) ;
#96145 = DIRECTION('ref_axis',(1.,0.,0.)) ;
#96146 = DIRECTION('center_axis',(0.,0.,1.)) ;
#96147 = DIRECTION('ref_axis',(1.,0.,0.)) ;
#96148 = DIRECTION('center_axis',(-0.707106781186548,-0.707106781186547,0.)) ;
#96149 = DIRECTION('ref_axis',(0.707106781186547,-0.707106781186548,0.)) ;
#96150 = DIRECTION('',(0.,0.,1.)) ;
#96151 = DIRECTION('',(0.577350269189625,-0.577350269189626,-0.577350269189626)) ;
#96152 = DIRECTION('',(0.,0.,-1.)) ;
#96153 = DIRECTION('',(-0.577350269189625,0.577350269189626,-0.577350269189626)) ;
#96154 = DIRECTION('center_axis',(1.95511867169517E-16,-1.,0.)) ;
#96155 = DIRECTION('ref_axis',(1.,1.95511867169517E-16,0.)) ;
#96156 = DIRECTION('',(0.,0.,-1.)) ;
#96157 = DIRECTION('',(-1.,-1.95511867169517E-16,0.)) ;
#96158 = DIRECTION('',(1.,1.95511867169517E-16,0.)) ;
#96159 = DIRECTION('center_axis',(1.06642836637918E-16,1.,0.)) ;
#96160 = DIRECTION('ref_axis',(-1.,1.06642836637918E-16,0.)) ;
#96161 = DIRECTION('',(1.,-1.06642836637919E-16,0.)) ;
#96162 = DIRECTION('',(0.,0.,1.)) ;
#96163 = DIRECTION('',(-1.,1.06642836637919E-16,0.)) ;
#96164 = DIRECTION('center_axis',(-0.707106781186548,0.707106781186547,0.)) ;
#96165 = DIRECTION('ref_axis',(-0.707106781186547,-0.707106781186548,0.)) ;
#96166 = DIRECTION('',(0.,0.,1.)) ;
#96167 = DIRECTION('',(-0.577350269189625,-0.577350269189626,0.577350269189627)) ;
#96168 = DIRECTION('',(0.,0.,-1.)) ;
#96169 = DIRECTION('',(0.577350269189625,0.577350269189626,0.577350269189627)) ;
#96170 = DIRECTION('center_axis',(-1.,0.,0.)) ;
#96171 = DIRECTION('ref_axis',(0.,0.,1.)) ;
#96172 = DIRECTION('',(0.,0.,-1.)) ;
#96173 = DIRECTION('',(0.,1.,1.95511867169518E-16)) ;
#96174 = DIRECTION('',(0.,0.,1.)) ;
#96175 = DIRECTION('',(0.,-1.,1.95511867169518E-16)) ;
#96176 = DIRECTION('center_axis',(0.,0.,1.)) ;
#96177 = DIRECTION('ref_axis',(1.,0.,0.)) ;
#96178 = DIRECTION('',(-1.95511867169517E-16,1.,0.)) ;
#96179 = DIRECTION('',(-1.,-1.95511867169517E-16,0.)) ;
#96180 = DIRECTION('',(1.,-1.06642836637919E-16,0.)) ;
#96181 = DIRECTION('center_axis',(0.,0.,1.)) ;
#96182 = DIRECTION('ref_axis',(1.,0.,0.)) ;
#96183 = DIRECTION('',(1.,1.95511867169517E-16,0.)) ;
#96184 = DIRECTION('',(1.95511867169517E-16,-1.,0.)) ;
#96185 = DIRECTION('',(-1.,1.06642836637919E-16,0.)) ;
#96186 = DIRECTION('center_axis',(1.,-9.85638338623186E-18,0.)) ;
#96187 = DIRECTION('ref_axis',(9.85638338623186E-18,1.,0.)) ;
#96188 = DIRECTION('',(0.,0.,-1.)) ;
#96189 = DIRECTION('',(-9.85638338623186E-18,-1.,0.)) ;
#96190 = DIRECTION('',(0.,0.,1.)) ;
#96191 = DIRECTION('',(9.85638338623186E-18,1.,0.)) ;
#96192 = DIRECTION('center_axis',(0.707106781186548,0.707106781186548,0.)) ;
#96193 = DIRECTION('ref_axis',(-0.707106781186548,0.707106781186548,0.)) ;
#96194 = DIRECTION('',(0.,0.,1.)) ;
#96195 = DIRECTION('',(-0.577350269189625,0.577350269189625,0.577350269189627)) ;
#96196 = DIRECTION('',(0.,0.,-1.)) ;
#96197 = DIRECTION('',(0.577350269189625,-0.577350269189625,0.577350269189627)) ;
#96198 = DIRECTION('center_axis',(0.,1.,0.)) ;
#96199 = DIRECTION('ref_axis',(0.,0.,1.)) ;
#96200 = DIRECTION('',(0.,0.,1.)) ;
#96201 = DIRECTION('',(-1.,0.,-9.8563833862319E-18)) ;
#96202 = DIRECTION('',(0.,0.,-1.)) ;
#96203 = DIRECTION('',(1.,0.,-9.8563833862319E-18)) ;
#96204 = DIRECTION('center_axis',(-0.707106781186548,0.707106781186548,0.)) ;
#96205 = DIRECTION('ref_axis',(-0.707106781186548,-0.707106781186548,0.)) ;
#96206 = DIRECTION('',(0.,0.,1.)) ;
#96207 = DIRECTION('',(-0.577350269189625,-0.577350269189625,-0.577350269189627)) ;
#96208 = DIRECTION('',(0.,0.,-1.)) ;
#96209 = DIRECTION('',(0.577350269189625,0.577350269189625,-0.577350269189627)) ;
#96210 = DIRECTION('center_axis',(-1.,9.85638338623186E-18,0.)) ;
#96211 = DIRECTION('ref_axis',(-9.85638338623186E-18,-1.,0.)) ;
#96212 = DIRECTION('',(0.,0.,-1.)) ;
#96213 = DIRECTION('',(9.85638338623186E-18,1.,0.)) ;
#96214 = DIRECTION('',(0.,0.,-1.)) ;
#96215 = DIRECTION('',(-9.85638338623186E-18,-1.,0.)) ;
#96216 = DIRECTION('center_axis',(0.,0.,1.)) ;
#96217 = DIRECTION('ref_axis',(1.,0.,0.)) ;
#96218 = DIRECTION('',(9.85638338623186E-18,1.,0.)) ;
#96219 = DIRECTION('center_axis',(0.,0.,-1.)) ;
#96220 = DIRECTION('ref_axis',(1.,0.,0.)) ;
#96221 = DIRECTION('center_axis',(0.,0.,1.)) ;
#96222 = DIRECTION('ref_axis',(1.,0.,0.)) ;
#96223 = DIRECTION('',(-9.85638338623186E-18,-1.,0.)) ;
#96224 = DIRECTION('',(1.,-9.85638338623186E-18,0.)) ;
#96225 = DIRECTION('center_axis',(0.,0.,1.)) ;
#96226 = DIRECTION('ref_axis',(1.,0.,0.)) ;
#96227 = DIRECTION('',(9.85638338623186E-18,1.,0.)) ;
#96228 = DIRECTION('center_axis',(0.,0.,-1.)) ;
#96229 = DIRECTION('ref_axis',(1.,0.,0.)) ;
#96230 = DIRECTION('center_axis',(0.,0.,1.)) ;
#96231 = DIRECTION('ref_axis',(1.,0.,0.)) ;
#96232 = DIRECTION('',(-9.85638338623186E-18,-1.,0.)) ;
#96233 = DIRECTION('',(-1.,9.85638338623186E-18,0.)) ;
#96234 = DIRECTION('center_axis',(0.,0.,-1.)) ;
#96235 = DIRECTION('ref_axis',(-1.,0.,0.)) ;
#96236 = DIRECTION('center_axis',(0.,0.,1.)) ;
#96237 = DIRECTION('ref_axis',(1.,0.,0.)) ;
#96238 = DIRECTION('center_axis',(0.,0.,-1.)) ;
#96239 = DIRECTION('ref_axis',(1.,0.,0.)) ;
#96240 = DIRECTION('center_axis',(0.,0.,-1.)) ;
#96241 = DIRECTION('ref_axis',(-1.,0.,0.)) ;
#96242 = DIRECTION('center_axis',(0.,0.,-1.)) ;
#96243 = DIRECTION('ref_axis',(1.,0.,0.)) ;
#96244 = DIRECTION('center_axis',(0.,0.,1.)) ;
#96245 = DIRECTION('ref_axis',(1.,0.,0.)) ;
#96246 = DIRECTION('center_axis',(-0.707106781186548,-0.707106781186547,0.)) ;
#96247 = DIRECTION('ref_axis',(0.707106781186547,-0.707106781186548,0.)) ;
#96248 = DIRECTION('',(0.,0.,1.)) ;
#96249 = DIRECTION('',(0.577350269189625,-0.577350269189626,-0.577350269189626)) ;
#96250 = DIRECTION('',(0.,0.,-1.)) ;
#96251 = DIRECTION('',(-0.577350269189625,0.577350269189626,-0.577350269189626)) ;
#96252 = DIRECTION('center_axis',(1.95511867169517E-16,-1.,0.)) ;
#96253 = DIRECTION('ref_axis',(1.,1.95511867169517E-16,0.)) ;
#96254 = DIRECTION('',(0.,0.,-1.)) ;
#96255 = DIRECTION('',(-1.,-1.95511867169517E-16,0.)) ;
#96256 = DIRECTION('',(1.,1.95511867169517E-16,0.)) ;
#96257 = DIRECTION('center_axis',(1.06642836637918E-16,1.,0.)) ;
#96258 = DIRECTION('ref_axis',(-1.,1.06642836637918E-16,0.)) ;
#96259 = DIRECTION('',(1.,-1.06642836637919E-16,0.)) ;
#96260 = DIRECTION('',(0.,0.,1.)) ;
#96261 = DIRECTION('',(-1.,1.06642836637919E-16,0.)) ;
#96262 = DIRECTION('center_axis',(-0.707106781186548,0.707106781186547,0.)) ;
#96263 = DIRECTION('ref_axis',(-0.707106781186547,-0.707106781186548,0.)) ;
#96264 = DIRECTION('',(0.,0.,1.)) ;
#96265 = DIRECTION('',(-0.577350269189625,-0.577350269189626,0.577350269189627)) ;
#96266 = DIRECTION('',(0.,0.,-1.)) ;
#96267 = DIRECTION('',(0.577350269189625,0.577350269189626,0.577350269189627)) ;
#96268 = DIRECTION('center_axis',(-1.,0.,0.)) ;
#96269 = DIRECTION('ref_axis',(0.,0.,1.)) ;
#96270 = DIRECTION('',(0.,0.,-1.)) ;
#96271 = DIRECTION('',(0.,1.,1.95511867169518E-16)) ;
#96272 = DIRECTION('',(0.,0.,1.)) ;
#96273 = DIRECTION('',(0.,-1.,1.95511867169518E-16)) ;
#96274 = DIRECTION('center_axis',(0.,0.,1.)) ;
#96275 = DIRECTION('ref_axis',(1.,0.,0.)) ;
#96276 = DIRECTION('',(-1.95511867169517E-16,1.,0.)) ;
#96277 = DIRECTION('',(-1.,-1.95511867169517E-16,0.)) ;
#96278 = DIRECTION('',(1.,-1.06642836637919E-16,0.)) ;
#96279 = DIRECTION('center_axis',(0.,0.,1.)) ;
#96280 = DIRECTION('ref_axis',(1.,0.,0.)) ;
#96281 = DIRECTION('',(1.,1.95511867169517E-16,0.)) ;
#96282 = DIRECTION('',(1.95511867169517E-16,-1.,0.)) ;
#96283 = DIRECTION('',(-1.,1.06642836637919E-16,0.)) ;
#96284 = DIRECTION('center_axis',(1.,-9.85638338623186E-18,0.)) ;
#96285 = DIRECTION('ref_axis',(9.85638338623186E-18,1.,0.)) ;
#96286 = DIRECTION('',(0.,0.,-1.)) ;
#96287 = DIRECTION('',(-9.85638338623186E-18,-1.,0.)) ;
#96288 = DIRECTION('',(0.,0.,1.)) ;
#96289 = DIRECTION('',(9.85638338623186E-18,1.,0.)) ;
#96290 = DIRECTION('center_axis',(0.707106781186548,0.707106781186548,0.)) ;
#96291 = DIRECTION('ref_axis',(-0.707106781186548,0.707106781186548,0.)) ;
#96292 = DIRECTION('',(0.,0.,1.)) ;
#96293 = DIRECTION('',(-0.577350269189625,0.577350269189625,0.577350269189627)) ;
#96294 = DIRECTION('',(0.,0.,-1.)) ;
#96295 = DIRECTION('',(0.577350269189625,-0.577350269189625,0.577350269189627)) ;
#96296 = DIRECTION('center_axis',(0.,1.,0.)) ;
#96297 = DIRECTION('ref_axis',(0.,0.,1.)) ;
#96298 = DIRECTION('',(0.,0.,1.)) ;
#96299 = DIRECTION('',(-1.,0.,-9.8563833862319E-18)) ;
#96300 = DIRECTION('',(0.,0.,-1.)) ;
#96301 = DIRECTION('',(1.,0.,-9.8563833862319E-18)) ;
#96302 = DIRECTION('center_axis',(-0.707106781186548,0.707106781186548,0.)) ;
#96303 = DIRECTION('ref_axis',(-0.707106781186548,-0.707106781186548,0.)) ;
#96304 = DIRECTION('',(0.,0.,1.)) ;
#96305 = DIRECTION('',(-0.577350269189625,-0.577350269189625,-0.577350269189627)) ;
#96306 = DIRECTION('',(0.,0.,-1.)) ;
#96307 = DIRECTION('',(0.577350269189625,0.577350269189625,-0.577350269189627)) ;
#96308 = DIRECTION('center_axis',(-1.,9.85638338623186E-18,0.)) ;
#96309 = DIRECTION('ref_axis',(-9.85638338623186E-18,-1.,0.)) ;
#96310 = DIRECTION('',(0.,0.,-1.)) ;
#96311 = DIRECTION('',(9.85638338623186E-18,1.,0.)) ;
#96312 = DIRECTION('',(0.,0.,-1.)) ;
#96313 = DIRECTION('',(-9.85638338623186E-18,-1.,0.)) ;
#96314 = DIRECTION('center_axis',(0.,0.,1.)) ;
#96315 = DIRECTION('ref_axis',(1.,0.,0.)) ;
#96316 = DIRECTION('',(9.85638338623186E-18,1.,0.)) ;
#96317 = DIRECTION('center_axis',(0.,0.,-1.)) ;
#96318 = DIRECTION('ref_axis',(1.,0.,0.)) ;
#96319 = DIRECTION('center_axis',(0.,0.,1.)) ;
#96320 = DIRECTION('ref_axis',(1.,0.,0.)) ;
#96321 = DIRECTION('',(-9.85638338623186E-18,-1.,0.)) ;
#96322 = DIRECTION('',(1.,-9.85638338623186E-18,0.)) ;
#96323 = DIRECTION('center_axis',(0.,0.,1.)) ;
#96324 = DIRECTION('ref_axis',(1.,0.,0.)) ;
#96325 = DIRECTION('',(9.85638338623186E-18,1.,0.)) ;
#96326 = DIRECTION('center_axis',(0.,0.,-1.)) ;
#96327 = DIRECTION('ref_axis',(1.,0.,0.)) ;
#96328 = DIRECTION('center_axis',(0.,0.,1.)) ;
#96329 = DIRECTION('ref_axis',(1.,0.,0.)) ;
#96330 = DIRECTION('',(-9.85638338623186E-18,-1.,0.)) ;
#96331 = DIRECTION('',(-1.,9.85638338623186E-18,0.)) ;
#96332 = DIRECTION('center_axis',(0.,0.,-1.)) ;
#96333 = DIRECTION('ref_axis',(-1.,0.,0.)) ;
#96334 = DIRECTION('center_axis',(0.,0.,1.)) ;
#96335 = DIRECTION('ref_axis',(1.,0.,0.)) ;
#96336 = DIRECTION('center_axis',(0.,0.,-1.)) ;
#96337 = DIRECTION('ref_axis',(1.,0.,0.)) ;
#96338 = DIRECTION('center_axis',(0.,0.,-1.)) ;
#96339 = DIRECTION('ref_axis',(-1.,0.,0.)) ;
#96340 = DIRECTION('center_axis',(0.,0.,-1.)) ;
#96341 = DIRECTION('ref_axis',(1.,0.,0.)) ;
#96342 = DIRECTION('center_axis',(0.,0.,1.)) ;
#96343 = DIRECTION('ref_axis',(1.,0.,0.)) ;
#96344 = DIRECTION('center_axis',(-0.707106781186548,-0.707106781186547,0.)) ;
#96345 = DIRECTION('ref_axis',(0.707106781186547,-0.707106781186548,0.)) ;
#96346 = DIRECTION('',(0.,0.,1.)) ;
#96347 = DIRECTION('',(0.577350269189625,-0.577350269189626,-0.577350269189626)) ;
#96348 = DIRECTION('',(0.,0.,-1.)) ;
#96349 = DIRECTION('',(-0.577350269189625,0.577350269189626,-0.577350269189626)) ;
#96350 = DIRECTION('center_axis',(1.95511867169517E-16,-1.,0.)) ;
#96351 = DIRECTION('ref_axis',(1.,1.95511867169517E-16,0.)) ;
#96352 = DIRECTION('',(0.,0.,-1.)) ;
#96353 = DIRECTION('',(-1.,-1.95511867169517E-16,0.)) ;
#96354 = DIRECTION('',(1.,1.95511867169517E-16,0.)) ;
#96355 = DIRECTION('center_axis',(1.06642836637918E-16,1.,0.)) ;
#96356 = DIRECTION('ref_axis',(-1.,1.06642836637918E-16,0.)) ;
#96357 = DIRECTION('',(1.,-1.06642836637919E-16,0.)) ;
#96358 = DIRECTION('',(0.,0.,1.)) ;
#96359 = DIRECTION('',(-1.,1.06642836637919E-16,0.)) ;
#96360 = DIRECTION('center_axis',(-0.707106781186548,0.707106781186547,0.)) ;
#96361 = DIRECTION('ref_axis',(-0.707106781186547,-0.707106781186548,0.)) ;
#96362 = DIRECTION('',(0.,0.,1.)) ;
#96363 = DIRECTION('',(-0.577350269189625,-0.577350269189626,0.577350269189627)) ;
#96364 = DIRECTION('',(0.,0.,-1.)) ;
#96365 = DIRECTION('',(0.577350269189625,0.577350269189626,0.577350269189627)) ;
#96366 = DIRECTION('center_axis',(-1.,0.,0.)) ;
#96367 = DIRECTION('ref_axis',(0.,0.,1.)) ;
#96368 = DIRECTION('',(0.,0.,-1.)) ;
#96369 = DIRECTION('',(0.,1.,1.95511867169518E-16)) ;
#96370 = DIRECTION('',(0.,0.,1.)) ;
#96371 = DIRECTION('',(0.,-1.,1.95511867169518E-16)) ;
#96372 = DIRECTION('center_axis',(0.,0.,1.)) ;
#96373 = DIRECTION('ref_axis',(1.,0.,0.)) ;
#96374 = DIRECTION('',(-1.95511867169517E-16,1.,0.)) ;
#96375 = DIRECTION('',(-1.,-1.95511867169517E-16,0.)) ;
#96376 = DIRECTION('',(1.,-1.06642836637919E-16,0.)) ;
#96377 = DIRECTION('center_axis',(0.,0.,1.)) ;
#96378 = DIRECTION('ref_axis',(1.,0.,0.)) ;
#96379 = DIRECTION('',(1.,1.95511867169517E-16,0.)) ;
#96380 = DIRECTION('',(1.95511867169517E-16,-1.,0.)) ;
#96381 = DIRECTION('',(-1.,1.06642836637919E-16,0.)) ;
#96382 = DIRECTION('center_axis',(1.,-9.85638338623186E-18,0.)) ;
#96383 = DIRECTION('ref_axis',(9.85638338623186E-18,1.,0.)) ;
#96384 = DIRECTION('',(0.,0.,-1.)) ;
#96385 = DIRECTION('',(-9.85638338623186E-18,-1.,0.)) ;
#96386 = DIRECTION('',(0.,0.,1.)) ;
#96387 = DIRECTION('',(9.85638338623186E-18,1.,0.)) ;
#96388 = DIRECTION('center_axis',(0.707106781186548,0.707106781186548,0.)) ;
#96389 = DIRECTION('ref_axis',(-0.707106781186548,0.707106781186548,0.)) ;
#96390 = DIRECTION('',(0.,0.,1.)) ;
#96391 = DIRECTION('',(-0.577350269189625,0.577350269189625,0.577350269189627)) ;
#96392 = DIRECTION('',(0.,0.,-1.)) ;
#96393 = DIRECTION('',(0.577350269189625,-0.577350269189625,0.577350269189627)) ;
#96394 = DIRECTION('center_axis',(0.,1.,0.)) ;
#96395 = DIRECTION('ref_axis',(0.,0.,1.)) ;
#96396 = DIRECTION('',(0.,0.,1.)) ;
#96397 = DIRECTION('',(-1.,0.,-9.8563833862319E-18)) ;
#96398 = DIRECTION('',(0.,0.,-1.)) ;
#96399 = DIRECTION('',(1.,0.,-9.8563833862319E-18)) ;
#96400 = DIRECTION('center_axis',(-0.707106781186548,0.707106781186548,0.)) ;
#96401 = DIRECTION('ref_axis',(-0.707106781186548,-0.707106781186548,0.)) ;
#96402 = DIRECTION('',(0.,0.,1.)) ;
#96403 = DIRECTION('',(-0.577350269189625,-0.577350269189625,-0.577350269189627)) ;
#96404 = DIRECTION('',(0.,0.,-1.)) ;
#96405 = DIRECTION('',(0.577350269189625,0.577350269189625,-0.577350269189627)) ;
#96406 = DIRECTION('center_axis',(-1.,9.85638338623186E-18,0.)) ;
#96407 = DIRECTION('ref_axis',(-9.85638338623186E-18,-1.,0.)) ;
#96408 = DIRECTION('',(0.,0.,-1.)) ;
#96409 = DIRECTION('',(9.85638338623186E-18,1.,0.)) ;
#96410 = DIRECTION('',(0.,0.,-1.)) ;
#96411 = DIRECTION('',(-9.85638338623186E-18,-1.,0.)) ;
#96412 = DIRECTION('center_axis',(0.,0.,1.)) ;
#96413 = DIRECTION('ref_axis',(1.,0.,0.)) ;
#96414 = DIRECTION('',(9.85638338623186E-18,1.,0.)) ;
#96415 = DIRECTION('center_axis',(0.,0.,-1.)) ;
#96416 = DIRECTION('ref_axis',(1.,0.,0.)) ;
#96417 = DIRECTION('center_axis',(0.,0.,1.)) ;
#96418 = DIRECTION('ref_axis',(1.,0.,0.)) ;
#96419 = DIRECTION('',(-9.85638338623186E-18,-1.,0.)) ;
#96420 = DIRECTION('',(1.,-9.85638338623186E-18,0.)) ;
#96421 = DIRECTION('center_axis',(0.,0.,1.)) ;
#96422 = DIRECTION('ref_axis',(1.,0.,0.)) ;
#96423 = DIRECTION('',(9.85638338623186E-18,1.,0.)) ;
#96424 = DIRECTION('center_axis',(0.,0.,-1.)) ;
#96425 = DIRECTION('ref_axis',(1.,0.,0.)) ;
#96426 = DIRECTION('center_axis',(0.,0.,1.)) ;
#96427 = DIRECTION('ref_axis',(1.,0.,0.)) ;
#96428 = DIRECTION('',(-9.85638338623186E-18,-1.,0.)) ;
#96429 = DIRECTION('',(-1.,9.85638338623186E-18,0.)) ;
#96430 = DIRECTION('center_axis',(0.,0.,-1.)) ;
#96431 = DIRECTION('ref_axis',(-1.,0.,0.)) ;
#96432 = DIRECTION('center_axis',(0.,0.,1.)) ;
#96433 = DIRECTION('ref_axis',(1.,0.,0.)) ;
#96434 = DIRECTION('center_axis',(0.,0.,-1.)) ;
#96435 = DIRECTION('ref_axis',(1.,0.,0.)) ;
#96436 = DIRECTION('center_axis',(0.,0.,-1.)) ;
#96437 = DIRECTION('ref_axis',(-1.,0.,0.)) ;
#96438 = DIRECTION('center_axis',(0.,0.,-1.)) ;
#96439 = DIRECTION('ref_axis',(1.,0.,0.)) ;
#96440 = DIRECTION('center_axis',(0.,0.,1.)) ;
#96441 = DIRECTION('ref_axis',(1.,0.,0.)) ;
#96442 = DIRECTION('center_axis',(-0.707106781186548,-0.707106781186547,0.)) ;
#96443 = DIRECTION('ref_axis',(0.707106781186547,-0.707106781186548,0.)) ;
#96444 = DIRECTION('',(0.,0.,1.)) ;
#96445 = DIRECTION('',(0.577350269189625,-0.577350269189626,-0.577350269189626)) ;
#96446 = DIRECTION('',(0.,0.,-1.)) ;
#96447 = DIRECTION('',(-0.577350269189625,0.577350269189626,-0.577350269189626)) ;
#96448 = DIRECTION('center_axis',(1.95511867169517E-16,-1.,0.)) ;
#96449 = DIRECTION('ref_axis',(1.,1.95511867169517E-16,0.)) ;
#96450 = DIRECTION('',(0.,0.,-1.)) ;
#96451 = DIRECTION('',(-1.,-1.95511867169517E-16,0.)) ;
#96452 = DIRECTION('',(1.,1.95511867169517E-16,0.)) ;
#96453 = DIRECTION('center_axis',(1.06642836637918E-16,1.,0.)) ;
#96454 = DIRECTION('ref_axis',(-1.,1.06642836637918E-16,0.)) ;
#96455 = DIRECTION('',(1.,-1.06642836637919E-16,0.)) ;
#96456 = DIRECTION('',(0.,0.,1.)) ;
#96457 = DIRECTION('',(-1.,1.06642836637919E-16,0.)) ;
#96458 = DIRECTION('center_axis',(-0.707106781186548,0.707106781186547,0.)) ;
#96459 = DIRECTION('ref_axis',(-0.707106781186547,-0.707106781186548,0.)) ;
#96460 = DIRECTION('',(0.,0.,1.)) ;
#96461 = DIRECTION('',(-0.577350269189625,-0.577350269189626,0.577350269189627)) ;
#96462 = DIRECTION('',(0.,0.,-1.)) ;
#96463 = DIRECTION('',(0.577350269189625,0.577350269189626,0.577350269189627)) ;
#96464 = DIRECTION('center_axis',(-1.,0.,0.)) ;
#96465 = DIRECTION('ref_axis',(0.,0.,1.)) ;
#96466 = DIRECTION('',(0.,0.,-1.)) ;
#96467 = DIRECTION('',(0.,1.,1.95511867169518E-16)) ;
#96468 = DIRECTION('',(0.,0.,1.)) ;
#96469 = DIRECTION('',(0.,-1.,1.95511867169518E-16)) ;
#96470 = DIRECTION('center_axis',(0.,0.,1.)) ;
#96471 = DIRECTION('ref_axis',(1.,0.,0.)) ;
#96472 = DIRECTION('',(-1.95511867169517E-16,1.,0.)) ;
#96473 = DIRECTION('',(-1.,-1.95511867169517E-16,0.)) ;
#96474 = DIRECTION('',(1.,-1.06642836637919E-16,0.)) ;
#96475 = DIRECTION('center_axis',(0.,0.,1.)) ;
#96476 = DIRECTION('ref_axis',(1.,0.,0.)) ;
#96477 = DIRECTION('',(1.,1.95511867169517E-16,0.)) ;
#96478 = DIRECTION('',(1.95511867169517E-16,-1.,0.)) ;
#96479 = DIRECTION('',(-1.,1.06642836637919E-16,0.)) ;
#96480 = DIRECTION('center_axis',(6.96951553037899E-18,0.707106781186549,
0.707106781186546)) ;
#96481 = DIRECTION('ref_axis',(-8.6424177776148E-34,-0.707106781186546,0.707106781186549)) ;
#96482 = DIRECTION('',(-0.577350269189625,0.577350269189625,-0.577350269189627)) ;
#96483 = DIRECTION('',(1.,-9.85638338623186E-18,0.)) ;
#96484 = DIRECTION('',(-0.577350269189625,-0.577350269189625,0.577350269189627)) ;
#96485 = DIRECTION('',(-1.,7.70371977754894E-34,9.8563833862319E-18)) ;
#96486 = DIRECTION('center_axis',(6.96951553037899E-18,0.707106781186549,
-0.707106781186546)) ;
#96487 = DIRECTION('ref_axis',(8.6424177776148E-34,0.707106781186546,0.707106781186549)) ;
#96488 = DIRECTION('',(0.577350269189625,0.577350269189625,0.577350269189627)) ;
#96489 = DIRECTION('',(-1.,9.85638338623186E-18,0.)) ;
#96490 = DIRECTION('',(0.577350269189625,-0.577350269189625,-0.577350269189627)) ;
#96491 = DIRECTION('',(1.,-7.70371977754894E-34,9.8563833862319E-18)) ;
#96492 = DIRECTION('center_axis',(6.96951553037899E-18,0.707106781186549,
0.707106781186546)) ;
#96493 = DIRECTION('ref_axis',(-8.6424177776148E-34,-0.707106781186546,0.707106781186549)) ;
#96494 = DIRECTION('',(-0.577350269189625,0.577350269189625,-0.577350269189627)) ;
#96495 = DIRECTION('',(1.,-9.85638338623186E-18,0.)) ;
#96496 = DIRECTION('',(-0.577350269189625,-0.577350269189625,0.577350269189627)) ;
#96497 = DIRECTION('',(-1.,7.70371977754894E-34,9.8563833862319E-18)) ;
#96498 = DIRECTION('center_axis',(6.96951553037899E-18,0.707106781186549,
-0.707106781186546)) ;
#96499 = DIRECTION('ref_axis',(8.6424177776148E-34,0.707106781186546,0.707106781186549)) ;
#96500 = DIRECTION('',(0.577350269189625,0.577350269189625,0.577350269189627)) ;
#96501 = DIRECTION('',(-1.,9.85638338623186E-18,0.)) ;
#96502 = DIRECTION('',(0.577350269189625,-0.577350269189625,-0.577350269189627)) ;
#96503 = DIRECTION('',(1.,-7.70371977754894E-34,9.8563833862319E-18)) ;
#96504 = DIRECTION('center_axis',(6.96951553037899E-18,0.707106781186549,
0.707106781186546)) ;
#96505 = DIRECTION('ref_axis',(-8.6424177776148E-34,-0.707106781186546,0.707106781186549)) ;
#96506 = DIRECTION('',(-0.577350269189625,0.577350269189625,-0.577350269189627)) ;
#96507 = DIRECTION('',(1.,-9.85638338623186E-18,0.)) ;
#96508 = DIRECTION('',(-0.577350269189625,-0.577350269189625,0.577350269189627)) ;
#96509 = DIRECTION('',(-1.,7.70371977754894E-34,9.8563833862319E-18)) ;
#96510 = DIRECTION('center_axis',(6.96951553037899E-18,0.707106781186549,
-0.707106781186546)) ;
#96511 = DIRECTION('ref_axis',(8.6424177776148E-34,0.707106781186546,0.707106781186549)) ;
#96512 = DIRECTION('',(0.577350269189625,0.577350269189625,0.577350269189627)) ;
#96513 = DIRECTION('',(-1.,9.85638338623186E-18,0.)) ;
#96514 = DIRECTION('',(0.577350269189625,-0.577350269189625,-0.577350269189627)) ;
#96515 = DIRECTION('',(1.,-7.70371977754894E-34,9.8563833862319E-18)) ;
#96516 = DIRECTION('center_axis',(6.96951553037899E-18,0.707106781186549,
0.707106781186546)) ;
#96517 = DIRECTION('ref_axis',(-8.6424177776148E-34,-0.707106781186546,0.707106781186549)) ;
#96518 = DIRECTION('',(-0.577350269189625,0.577350269189625,-0.577350269189627)) ;
#96519 = DIRECTION('',(1.,-9.85638338623186E-18,0.)) ;
#96520 = DIRECTION('',(-0.577350269189625,-0.577350269189625,0.577350269189627)) ;
#96521 = DIRECTION('',(-1.,7.70371977754894E-34,9.8563833862319E-18)) ;
#96522 = DIRECTION('center_axis',(6.96951553037899E-18,0.707106781186549,
-0.707106781186546)) ;
#96523 = DIRECTION('ref_axis',(8.6424177776148E-34,0.707106781186546,0.707106781186549)) ;
#96524 = DIRECTION('',(0.577350269189625,0.577350269189625,0.577350269189627)) ;
#96525 = DIRECTION('',(-1.,9.85638338623186E-18,0.)) ;
#96526 = DIRECTION('',(0.577350269189625,-0.577350269189625,-0.577350269189627)) ;
#96527 = DIRECTION('',(1.,-7.70371977754894E-34,9.8563833862319E-18)) ;
#96528 = DIRECTION('center_axis',(6.96951553037899E-18,0.707106781186549,
0.707106781186546)) ;
#96529 = DIRECTION('ref_axis',(-8.6424177776148E-34,-0.707106781186546,0.707106781186549)) ;
#96530 = DIRECTION('',(-0.577350269189625,0.577350269189625,-0.577350269189627)) ;
#96531 = DIRECTION('',(1.,-9.85638338623186E-18,0.)) ;
#96532 = DIRECTION('',(-0.577350269189625,-0.577350269189625,0.577350269189627)) ;
#96533 = DIRECTION('',(-1.,7.70371977754894E-34,9.8563833862319E-18)) ;
#96534 = DIRECTION('center_axis',(6.96951553037899E-18,0.707106781186549,
-0.707106781186546)) ;
#96535 = DIRECTION('ref_axis',(8.6424177776148E-34,0.707106781186546,0.707106781186549)) ;
#96536 = DIRECTION('',(0.577350269189625,0.577350269189625,0.577350269189627)) ;
#96537 = DIRECTION('',(-1.,9.85638338623186E-18,0.)) ;
#96538 = DIRECTION('',(0.577350269189625,-0.577350269189625,-0.577350269189627)) ;
#96539 = DIRECTION('',(1.,-7.70371977754894E-34,9.8563833862319E-18)) ;
#96540 = DIRECTION('center_axis',(6.96951553037899E-18,0.707106781186549,
0.707106781186546)) ;
#96541 = DIRECTION('ref_axis',(-8.6424177776148E-34,-0.707106781186546,0.707106781186549)) ;
#96542 = DIRECTION('',(-0.577350269189625,0.577350269189625,-0.577350269189627)) ;
#96543 = DIRECTION('',(1.,-9.85638338623186E-18,0.)) ;
#96544 = DIRECTION('',(-0.577350269189625,-0.577350269189625,0.577350269189627)) ;
#96545 = DIRECTION('',(-1.,7.70371977754894E-34,9.8563833862319E-18)) ;
#96546 = DIRECTION('center_axis',(6.96951553037899E-18,0.707106781186549,
-0.707106781186546)) ;
#96547 = DIRECTION('ref_axis',(8.6424177776148E-34,0.707106781186546,0.707106781186549)) ;
#96548 = DIRECTION('',(0.577350269189625,0.577350269189625,0.577350269189627)) ;
#96549 = DIRECTION('',(-1.,9.85638338623186E-18,0.)) ;
#96550 = DIRECTION('',(0.577350269189625,-0.577350269189625,-0.577350269189627)) ;
#96551 = DIRECTION('',(1.,-7.70371977754894E-34,9.8563833862319E-18)) ;
#96552 = DIRECTION('center_axis',(6.96951553037899E-18,0.707106781186549,
0.707106781186546)) ;
#96553 = DIRECTION('ref_axis',(-8.6424177776148E-34,-0.707106781186546,0.707106781186549)) ;
#96554 = DIRECTION('',(-0.577350269189625,0.577350269189625,-0.577350269189627)) ;
#96555 = DIRECTION('',(1.,-9.85638338623186E-18,0.)) ;
#96556 = DIRECTION('',(-0.577350269189625,-0.577350269189625,0.577350269189627)) ;
#96557 = DIRECTION('',(-1.,7.70371977754894E-34,9.8563833862319E-18)) ;
#96558 = DIRECTION('center_axis',(6.96951553037899E-18,0.707106781186549,
-0.707106781186546)) ;
#96559 = DIRECTION('ref_axis',(8.6424177776148E-34,0.707106781186546,0.707106781186549)) ;
#96560 = DIRECTION('',(0.577350269189625,0.577350269189625,0.577350269189627)) ;
#96561 = DIRECTION('',(-1.,9.85638338623186E-18,0.)) ;
#96562 = DIRECTION('',(0.577350269189625,-0.577350269189625,-0.577350269189627)) ;
#96563 = DIRECTION('',(1.,-7.70371977754894E-34,9.8563833862319E-18)) ;
#96564 = DIRECTION('center_axis',(6.96951553037899E-18,0.707106781186549,
0.707106781186546)) ;
#96565 = DIRECTION('ref_axis',(-8.6424177776148E-34,-0.707106781186546,0.707106781186549)) ;
#96566 = DIRECTION('',(-0.577350269189625,0.577350269189625,-0.577350269189627)) ;
#96567 = DIRECTION('',(1.,-9.85638338623186E-18,0.)) ;
#96568 = DIRECTION('',(-0.577350269189625,-0.577350269189625,0.577350269189627)) ;
#96569 = DIRECTION('',(-1.,7.70371977754894E-34,9.8563833862319E-18)) ;
#96570 = DIRECTION('center_axis',(6.96951553037899E-18,0.707106781186549,
-0.707106781186546)) ;
#96571 = DIRECTION('ref_axis',(8.6424177776148E-34,0.707106781186546,0.707106781186549)) ;
#96572 = DIRECTION('',(0.577350269189625,0.577350269189625,0.577350269189627)) ;
#96573 = DIRECTION('',(-1.,9.85638338623186E-18,0.)) ;
#96574 = DIRECTION('',(0.577350269189625,-0.577350269189625,-0.577350269189627)) ;
#96575 = DIRECTION('',(1.,-7.70371977754894E-34,9.8563833862319E-18)) ;
#96576 = DIRECTION('center_axis',(6.96951553037899E-18,0.707106781186549,
0.707106781186546)) ;
#96577 = DIRECTION('ref_axis',(-8.6424177776148E-34,-0.707106781186546,0.707106781186549)) ;
#96578 = DIRECTION('',(-0.577350269189625,0.577350269189625,-0.577350269189627)) ;
#96579 = DIRECTION('',(1.,-9.85638338623186E-18,0.)) ;
#96580 = DIRECTION('',(-0.577350269189625,-0.577350269189625,0.577350269189627)) ;
#96581 = DIRECTION('',(-1.,7.70371977754894E-34,9.8563833862319E-18)) ;
#96582 = DIRECTION('center_axis',(6.96951553037899E-18,0.707106781186549,
-0.707106781186546)) ;
#96583 = DIRECTION('ref_axis',(8.6424177776148E-34,0.707106781186546,0.707106781186549)) ;
#96584 = DIRECTION('',(0.577350269189625,0.577350269189625,0.577350269189627)) ;
#96585 = DIRECTION('',(-1.,9.85638338623186E-18,0.)) ;
#96586 = DIRECTION('',(0.577350269189625,-0.577350269189625,-0.577350269189627)) ;
#96587 = DIRECTION('',(1.,-7.70371977754894E-34,9.8563833862319E-18)) ;
#96588 = DIRECTION('center_axis',(-0.707106781186548,-1.38247767078009E-16,
0.707106781186547)) ;
#96589 = DIRECTION('ref_axis',(0.707106781186547,8.815972061965E-34,0.707106781186548)) ;
#96590 = DIRECTION('',(-0.577350269189625,-0.577350269189626,-0.577350269189626)) ;
#96591 = DIRECTION('',(-1.95511867169517E-16,1.,0.)) ;
#96592 = DIRECTION('',(0.577350269189625,-0.577350269189626,0.577350269189626)) ;
#96593 = DIRECTION('',(0.,-1.,-1.95511867169518E-16)) ;
#96594 = DIRECTION('center_axis',(-0.707106781186548,-1.38247767078009E-16,
-0.707106781186547)) ;
#96595 = DIRECTION('ref_axis',(-0.707106781186547,-8.815972061965E-34,0.707106781186548)) ;
#96596 = DIRECTION('',(-0.577350269189625,0.577350269189626,0.577350269189626)) ;
#96597 = DIRECTION('',(1.95511867169517E-16,-1.,0.)) ;
#96598 = DIRECTION('',(0.577350269189625,0.577350269189626,-0.577350269189626)) ;
#96599 = DIRECTION('',(0.,1.,-1.95511867169518E-16)) ;
#96600 = DIRECTION('center_axis',(-0.707106781186548,-1.38247767078009E-16,
0.707106781186547)) ;
#96601 = DIRECTION('ref_axis',(0.707106781186547,8.815972061965E-34,0.707106781186548)) ;
#96602 = DIRECTION('',(-0.577350269189625,-0.577350269189626,-0.577350269189626)) ;
#96603 = DIRECTION('',(-1.95511867169517E-16,1.,0.)) ;
#96604 = DIRECTION('',(0.577350269189625,-0.577350269189626,0.577350269189626)) ;
#96605 = DIRECTION('',(0.,-1.,-1.95511867169518E-16)) ;
#96606 = DIRECTION('center_axis',(-0.707106781186548,-1.38247767078009E-16,
-0.707106781186547)) ;
#96607 = DIRECTION('ref_axis',(-0.707106781186547,-8.815972061965E-34,0.707106781186548)) ;
#96608 = DIRECTION('',(-0.577350269189625,0.577350269189626,0.577350269189626)) ;
#96609 = DIRECTION('',(1.95511867169517E-16,-1.,0.)) ;
#96610 = DIRECTION('',(0.577350269189625,0.577350269189626,-0.577350269189626)) ;
#96611 = DIRECTION('',(0.,1.,-1.95511867169518E-16)) ;
#96612 = DIRECTION('center_axis',(-0.707106781186548,-1.38247767078009E-16,
0.707106781186547)) ;
#96613 = DIRECTION('ref_axis',(0.707106781186547,8.815972061965E-34,0.707106781186548)) ;
#96614 = DIRECTION('',(-0.577350269189625,-0.577350269189626,-0.577350269189626)) ;
#96615 = DIRECTION('',(-1.95511867169517E-16,1.,0.)) ;
#96616 = DIRECTION('',(0.577350269189625,-0.577350269189626,0.577350269189626)) ;
#96617 = DIRECTION('',(0.,-1.,-1.95511867169518E-16)) ;
#96618 = DIRECTION('center_axis',(-0.707106781186548,-1.38247767078009E-16,
-0.707106781186547)) ;
#96619 = DIRECTION('ref_axis',(-0.707106781186547,-8.815972061965E-34,0.707106781186548)) ;
#96620 = DIRECTION('',(-0.577350269189625,0.577350269189626,0.577350269189626)) ;
#96621 = DIRECTION('',(1.95511867169517E-16,-1.,0.)) ;
#96622 = DIRECTION('',(0.577350269189625,0.577350269189626,-0.577350269189626)) ;
#96623 = DIRECTION('',(0.,1.,-1.95511867169518E-16)) ;
#96624 = DIRECTION('center_axis',(-0.707106781186548,-1.38247767078009E-16,
0.707106781186547)) ;
#96625 = DIRECTION('ref_axis',(0.707106781186547,8.815972061965E-34,0.707106781186548)) ;
#96626 = DIRECTION('',(-0.577350269189625,-0.577350269189626,-0.577350269189626)) ;
#96627 = DIRECTION('',(-1.95511867169517E-16,1.,0.)) ;
#96628 = DIRECTION('',(0.577350269189625,-0.577350269189626,0.577350269189626)) ;
#96629 = DIRECTION('',(0.,-1.,-1.95511867169518E-16)) ;
#96630 = DIRECTION('center_axis',(-0.707106781186548,-1.38247767078009E-16,
-0.707106781186547)) ;
#96631 = DIRECTION('ref_axis',(-0.707106781186547,-8.815972061965E-34,0.707106781186548)) ;
#96632 = DIRECTION('',(-0.577350269189625,0.577350269189626,0.577350269189626)) ;
#96633 = DIRECTION('',(1.95511867169517E-16,-1.,0.)) ;
#96634 = DIRECTION('',(0.577350269189625,0.577350269189626,-0.577350269189626)) ;
#96635 = DIRECTION('',(0.,1.,-1.95511867169518E-16)) ;
#96636 = DIRECTION('center_axis',(-0.707106781186548,-1.38247767078009E-16,
0.707106781186547)) ;
#96637 = DIRECTION('ref_axis',(0.707106781186547,8.815972061965E-34,0.707106781186548)) ;
#96638 = DIRECTION('',(-0.577350269189625,-0.577350269189626,-0.577350269189626)) ;
#96639 = DIRECTION('',(-1.95511867169517E-16,1.,0.)) ;
#96640 = DIRECTION('',(0.577350269189625,-0.577350269189626,0.577350269189626)) ;
#96641 = DIRECTION('',(0.,-1.,-1.95511867169518E-16)) ;
#96642 = DIRECTION('center_axis',(-0.707106781186548,-1.38247767078009E-16,
-0.707106781186547)) ;
#96643 = DIRECTION('ref_axis',(-0.707106781186547,-8.815972061965E-34,0.707106781186548)) ;
#96644 = DIRECTION('',(-0.577350269189625,0.577350269189626,0.577350269189626)) ;
#96645 = DIRECTION('',(1.95511867169517E-16,-1.,0.)) ;
#96646 = DIRECTION('',(0.577350269189625,0.577350269189626,-0.577350269189626)) ;
#96647 = DIRECTION('',(0.,1.,-1.95511867169518E-16)) ;
#96648 = DIRECTION('center_axis',(-0.707106781186548,-1.38247767078009E-16,
0.707106781186547)) ;
#96649 = DIRECTION('ref_axis',(0.707106781186547,8.815972061965E-34,0.707106781186548)) ;
#96650 = DIRECTION('',(-0.577350269189625,-0.577350269189626,-0.577350269189626)) ;
#96651 = DIRECTION('',(-1.95511867169517E-16,1.,0.)) ;
#96652 = DIRECTION('',(0.577350269189625,-0.577350269189626,0.577350269189626)) ;
#96653 = DIRECTION('',(0.,-1.,-1.95511867169518E-16)) ;
#96654 = DIRECTION('center_axis',(-0.707106781186548,-1.38247767078009E-16,
-0.707106781186547)) ;
#96655 = DIRECTION('ref_axis',(-0.707106781186547,-8.815972061965E-34,0.707106781186548)) ;
#96656 = DIRECTION('',(-0.577350269189625,0.577350269189626,0.577350269189626)) ;
#96657 = DIRECTION('',(1.95511867169517E-16,-1.,0.)) ;
#96658 = DIRECTION('',(0.577350269189625,0.577350269189626,-0.577350269189626)) ;
#96659 = DIRECTION('',(0.,1.,-1.95511867169518E-16)) ;
#96660 = DIRECTION('center_axis',(-0.707106781186548,-1.38247767078009E-16,
0.707106781186547)) ;
#96661 = DIRECTION('ref_axis',(0.707106781186547,8.815972061965E-34,0.707106781186548)) ;
#96662 = DIRECTION('',(-0.577350269189625,-0.577350269189626,-0.577350269189626)) ;
#96663 = DIRECTION('',(-1.95511867169517E-16,1.,0.)) ;
#96664 = DIRECTION('',(0.577350269189625,-0.577350269189626,0.577350269189626)) ;
#96665 = DIRECTION('',(0.,-1.,-1.95511867169518E-16)) ;
#96666 = DIRECTION('center_axis',(-0.707106781186548,-1.38247767078009E-16,
-0.707106781186547)) ;
#96667 = DIRECTION('ref_axis',(-0.707106781186547,-8.815972061965E-34,0.707106781186548)) ;
#96668 = DIRECTION('',(-0.577350269189625,0.577350269189626,0.577350269189626)) ;
#96669 = DIRECTION('',(1.95511867169517E-16,-1.,0.)) ;
#96670 = DIRECTION('',(0.577350269189625,0.577350269189626,-0.577350269189626)) ;
#96671 = DIRECTION('',(0.,1.,-1.95511867169518E-16)) ;
#96672 = DIRECTION('center_axis',(-0.707106781186548,-1.38247767078009E-16,
0.707106781186547)) ;
#96673 = DIRECTION('ref_axis',(0.707106781186547,8.815972061965E-34,0.707106781186548)) ;
#96674 = DIRECTION('',(-0.577350269189625,-0.577350269189626,-0.577350269189626)) ;
#96675 = DIRECTION('',(-1.95511867169517E-16,1.,0.)) ;
#96676 = DIRECTION('',(0.577350269189625,-0.577350269189626,0.577350269189626)) ;
#96677 = DIRECTION('',(0.,-1.,-1.95511867169518E-16)) ;
#96678 = DIRECTION('center_axis',(-0.707106781186548,-1.38247767078009E-16,
-0.707106781186547)) ;
#96679 = DIRECTION('ref_axis',(-0.707106781186547,-8.815972061965E-34,0.707106781186548)) ;
#96680 = DIRECTION('',(-0.577350269189625,0.577350269189626,0.577350269189626)) ;
#96681 = DIRECTION('',(1.95511867169517E-16,-1.,0.)) ;
#96682 = DIRECTION('',(0.577350269189625,0.577350269189626,-0.577350269189626)) ;
#96683 = DIRECTION('',(0.,1.,-1.95511867169518E-16)) ;
#96684 = DIRECTION('center_axis',(-0.707106781186548,-1.38247767078009E-16,
0.707106781186547)) ;
#96685 = DIRECTION('ref_axis',(0.707106781186547,8.815972061965E-34,0.707106781186548)) ;
#96686 = DIRECTION('',(-0.577350269189625,-0.577350269189626,-0.577350269189626)) ;
#96687 = DIRECTION('',(-1.95511867169517E-16,1.,0.)) ;
#96688 = DIRECTION('',(0.577350269189625,-0.577350269189626,0.577350269189626)) ;
#96689 = DIRECTION('',(0.,-1.,-1.95511867169518E-16)) ;
#96690 = DIRECTION('center_axis',(-0.707106781186548,-1.38247767078009E-16,
-0.707106781186547)) ;
#96691 = DIRECTION('ref_axis',(-0.707106781186547,-8.815972061965E-34,0.707106781186548)) ;
#96692 = DIRECTION('',(-0.577350269189625,0.577350269189626,0.577350269189626)) ;
#96693 = DIRECTION('',(1.95511867169517E-16,-1.,0.)) ;
#96694 = DIRECTION('',(0.577350269189625,0.577350269189626,-0.577350269189626)) ;
#96695 = DIRECTION('',(0.,1.,-1.95511867169518E-16)) ;
#96696 = DIRECTION('center_axis',(0.577350269189625,0.577350269189625,-0.577350269189628)) ;
#96697 = DIRECTION('ref_axis',(-0.70710678118655,2.50449302218608E-16,-0.707106781186546)) ;
#96698 = DIRECTION('center_axis',(-0.577350269189625,-0.577350269189625,0.577350269189628)) ;
#96699 = DIRECTION('ref_axis',(-0.707106781186548,-2.12258087602815E-15,-0.707106781186547)) ;
#96700 = DIRECTION('center_axis',(-0.577350269189622,-0.577350269189626,0.57735026918963)) ;
#96701 = DIRECTION('ref_axis',(4.78608867599257E-17,-0.70710678118655,-0.707106781186545)) ;
#96702 = DIRECTION('center_axis',(0.,0.,-1.)) ;
#96703 = DIRECTION('ref_axis',(-1.,0.,0.)) ;
#96704 = DIRECTION('center_axis',(0.,0.,1.)) ;
#96705 = DIRECTION('ref_axis',(-1.,-8.67361737988404E-15,0.)) ;
#96706 = DIRECTION('center_axis',(0.,0.,-1.)) ;
#96707 = DIRECTION('ref_axis',(-1.,0.,0.)) ;
#96708 = DIRECTION('center_axis',(2.08166817117218E-16,1.,0.)) ;
#96709 = DIRECTION('ref_axis',(1.,0.,0.)) ;
#96710 = DIRECTION('center_axis',(-1.,0.,-4.40821857296472E-15)) ;
#96711 = DIRECTION('ref_axis',(4.40821857296472E-15,0.,-1.)) ;
#96712 = DIRECTION('center_axis',(8.67361737988402E-15,8.67361737988401E-15,
1.)) ;
#96713 = DIRECTION('ref_axis',(-1.,-9.79595207717063E-44,8.67361737988402E-15)) ;
#96714 = DIRECTION('center_axis',(-0.577350269189625,-0.577350269189625,-0.577350269189628)) ;
#96715 = DIRECTION('ref_axis',(-0.70710678118655,2.50449302218608E-16,0.707106781186546)) ;
#96716 = DIRECTION('center_axis',(-0.577350269189625,-0.577350269189625,-0.577350269189628)) ;
#96717 = DIRECTION('ref_axis',(-0.70710678118655,2.22693726602979E-16,0.707106781186546)) ;
#96718 = DIRECTION('center_axis',(-0.577350269189624,-0.577350269189623,-0.577350269189631)) ;
#96719 = DIRECTION('ref_axis',(-0.707106781186552,5.79770761800025E-17,0.707106781186543)) ;
#96720 = DIRECTION('center_axis',(0.,0.,-1.)) ;
#96721 = DIRECTION('ref_axis',(-1.,0.,0.)) ;
#96722 = DIRECTION('center_axis',(-6.1331736667335E-15,0.,1.)) ;
#96723 = DIRECTION('ref_axis',(1.,0.,6.1331736667335E-15)) ;
#96724 = DIRECTION('center_axis',(-1.,0.,9.8563833862319E-18)) ;
#96725 = DIRECTION('ref_axis',(9.8563833862319E-18,0.,1.)) ;
#96726 = DIRECTION('center_axis',(-1.,3.93023287525994E-15,-3.93023287525997E-15)) ;
#96727 = DIRECTION('ref_axis',(-3.93023287525997E-15,2.80259692864963E-44,
1.)) ;
#96728 = DIRECTION('center_axis',(2.08166817117218E-16,1.,0.)) ;
#96729 = DIRECTION('ref_axis',(1.,0.,0.)) ;
#96730 = DIRECTION('center_axis',(-1.,-8.13151629364126E-16,-8.13151629364131E-16)) ;
#96731 = DIRECTION('ref_axis',(8.13151629364131E-16,1.13855500226391E-45,
-1.)) ;
#96732 = DIRECTION('center_axis',(2.08166817117218E-16,1.,0.)) ;
#96733 = DIRECTION('ref_axis',(1.,0.,0.)) ;
#96734 = DIRECTION('center_axis',(-0.577350269189623,0.577350269189622,-0.577350269189633)) ;
#96735 = DIRECTION('ref_axis',(0.707106781186554,7.82055407754491E-16,-0.707106781186541)) ;
#96736 = DIRECTION('center_axis',(-6.1331736667335E-15,0.,1.)) ;
#96737 = DIRECTION('ref_axis',(-1.,0.,-6.1331736667335E-15)) ;
#96738 = DIRECTION('center_axis',(-1.,0.,-9.8563833862319E-18)) ;
#96739 = DIRECTION('ref_axis',(-9.8563833862319E-18,0.,1.)) ;
#96740 = DIRECTION('center_axis',(-1.,0.,-2.10827844793965E-15)) ;
#96741 = DIRECTION('ref_axis',(-2.10827844793965E-15,0.,1.)) ;
#96742 = DIRECTION('center_axis',(0.,0.,-1.)) ;
#96743 = DIRECTION('ref_axis',(-1.,0.,0.)) ;
#96744 = DIRECTION('center_axis',(0.,0.,1.)) ;
#96745 = DIRECTION('ref_axis',(1.,0.,0.)) ;
#96746 = DIRECTION('center_axis',(0.577350269189625,-0.577350269189625,0.577350269189628)) ;
#96747 = DIRECTION('ref_axis',(0.707106781186549,-7.23605167296792E-16,-0.707106781186546)) ;
#96748 = DIRECTION('center_axis',(0.577350269189625,-0.577350269189625,0.577350269189628)) ;
#96749 = DIRECTION('ref_axis',(0.707106781186549,-7.51360742912421E-16,-0.707106781186546)) ;
#96750 = DIRECTION('center_axis',(2.08166817117218E-16,1.,0.)) ;
#96751 = DIRECTION('ref_axis',(1.,0.,0.)) ;
#96752 = DIRECTION('center_axis',(-0.577350269189626,0.577350269189624,0.577350269189628)) ;
#96753 = DIRECTION('ref_axis',(-0.707106781186549,-7.24154524606924E-16,-0.707106781186546)) ;
#96754 = DIRECTION('center_axis',(0.,0.,-1.)) ;
#96755 = DIRECTION('ref_axis',(-1.,0.,0.)) ;
#96756 = DIRECTION('center_axis',(0.,0.,1.)) ;
#96757 = DIRECTION('ref_axis',(-1.,0.,0.)) ;
#96758 = DIRECTION('center_axis',(0.,0.,-1.)) ;
#96759 = DIRECTION('ref_axis',(-1.,0.,0.)) ;
#96760 = DIRECTION('center_axis',(-0.577350269189625,0.577350269189625,0.577350269189628)) ;
#96761 = DIRECTION('ref_axis',(0.70710678118655,2.22693726602979E-16,0.707106781186546)) ;
#96762 = DIRECTION('center_axis',(0.577350269189625,-0.577350269189625,-0.577350269189628)) ;
#96763 = DIRECTION('ref_axis',(0.707106781186549,-8.43215074740835E-16,0.707106781186546)) ;
#96764 = DIRECTION('center_axis',(-0.577350269189625,0.577350269189626,-0.577350269189626)) ;
#96765 = DIRECTION('ref_axis',(6.27941990732594E-17,0.707106781186548,0.707106781186548)) ;
#96766 = DIRECTION('center_axis',(0.577350269189625,-0.577350269189626,0.577350269189626)) ;
#96767 = DIRECTION('ref_axis',(5.0289788758123E-16,0.707106781186548,0.707106781186547)) ;
#96768 = DIRECTION('center_axis',(0.577350269189624,-0.57735026918963,0.577350269189624)) ;
#96769 = DIRECTION('ref_axis',(0.707106781186551,0.707106781186544,6.33763658455854E-16)) ;
#96770 = DIRECTION('center_axis',(0.,0.,-1.)) ;
#96771 = DIRECTION('ref_axis',(-1.,0.,0.)) ;
#96772 = DIRECTION('center_axis',(0.,0.,1.)) ;
#96773 = DIRECTION('ref_axis',(-1.,2.71050543121375E-15,0.)) ;
#96774 = DIRECTION('center_axis',(0.,0.,-1.)) ;
#96775 = DIRECTION('ref_axis',(-1.,0.,0.)) ;
#96776 = DIRECTION('center_axis',(0.,1.,0.)) ;
#96777 = DIRECTION('ref_axis',(1.,0.,0.)) ;
#96778 = DIRECTION('center_axis',(0.,-1.,-3.25824851045217E-15)) ;
#96779 = DIRECTION('ref_axis',(0.,-3.25824851045217E-15,1.)) ;
#96780 = DIRECTION('center_axis',(4.33680868994201E-15,-4.33680868994202E-15,
1.)) ;
#96781 = DIRECTION('ref_axis',(3.0828566215146E-44,1.,4.33680868994202E-15)) ;
#96782 = DIRECTION('center_axis',(0.577350269189625,-0.577350269189626,-0.577350269189626)) ;
#96783 = DIRECTION('ref_axis',(6.27941990732594E-17,0.707106781186548,-0.707106781186548)) ;
#96784 = DIRECTION('center_axis',(0.577350269189625,-0.577350269189626,-0.577350269189626)) ;
#96785 = DIRECTION('ref_axis',(-7.7646791370609E-16,0.707106781186547,-0.707106781186548)) ;
#96786 = DIRECTION('center_axis',(0.577350269189625,-0.577350269189626,-0.577350269189627)) ;
#96787 = DIRECTION('ref_axis',(-3.31150339748933E-16,0.707106781186548,-0.707106781186547)) ;
#96788 = DIRECTION('center_axis',(0.,0.,-1.)) ;
#96789 = DIRECTION('ref_axis',(-1.,0.,0.)) ;
#96790 = DIRECTION('center_axis',(0.,-6.1331736667335E-15,1.)) ;
#96791 = DIRECTION('ref_axis',(0.,-1.,-6.1331736667335E-15)) ;
#96792 = DIRECTION('center_axis',(0.,1.,1.95511867169518E-16)) ;
#96793 = DIRECTION('ref_axis',(0.,-1.95511867169518E-16,1.)) ;
#96794 = DIRECTION('center_axis',(2.71050543121375E-16,-1.,7.93888660359539E-17)) ;
#96795 = DIRECTION('ref_axis',(1.,2.71050543121375E-16,0.)) ;
#96796 = DIRECTION('center_axis',(0.,1.,0.)) ;
#96797 = DIRECTION('ref_axis',(1.,0.,0.)) ;
#96798 = DIRECTION('center_axis',(-1.28749007982653E-15,-1.,1.47915175691195E-15)) ;
#96799 = DIRECTION('ref_axis',(-1.49686561198851E-32,1.47915175691195E-15,
1.)) ;
#96800 = DIRECTION('center_axis',(0.,1.,0.)) ;
#96801 = DIRECTION('ref_axis',(1.,0.,0.)) ;
#96802 = DIRECTION('center_axis',(-0.577350269189624,-0.577350269189626,-0.577350269189628)) ;
#96803 = DIRECTION('ref_axis',(-1.24495925064522E-15,-0.707106781186548,0.707106781186547)) ;
#96804 = DIRECTION('center_axis',(0.,-6.1331736667335E-15,1.)) ;
#96805 = DIRECTION('ref_axis',(0.,1.,6.1331736667335E-15)) ;
#96806 = DIRECTION('center_axis',(0.,1.,-1.95511867169518E-16)) ;
#96807 = DIRECTION('ref_axis',(0.,1.95511867169518E-16,1.)) ;
#96808 = DIRECTION('center_axis',(0.,-1.,-4.59988025005012E-15)) ;
#96809 = DIRECTION('ref_axis',(0.,4.59988025005012E-15,-1.)) ;
#96810 = DIRECTION('center_axis',(0.,0.,-1.)) ;
#96811 = DIRECTION('ref_axis',(-1.,0.,0.)) ;
#96812 = DIRECTION('center_axis',(0.,0.,1.)) ;
#96813 = DIRECTION('ref_axis',(1.,0.,0.)) ;
#96814 = DIRECTION('center_axis',(0.577350269189625,0.577350269189626,0.577350269189627)) ;
#96815 = DIRECTION('ref_axis',(-2.71345386026911E-16,-0.707106781186548,0.707106781186547)) ;
#96816 = DIRECTION('center_axis',(0.577350269189625,0.577350269189626,0.577350269189627)) ;
#96817 = DIRECTION('ref_axis',(-2.71345386026911E-16,-0.707106781186548,0.707106781186547)) ;
#96818 = DIRECTION('center_axis',(0.,1.,0.)) ;
#96819 = DIRECTION('ref_axis',(1.,0.,0.)) ;
#96820 = DIRECTION('center_axis',(-0.577350269189624,-0.577350269189628,0.577350269189625)) ;
#96821 = DIRECTION('ref_axis',(-6.89490688817364E-15,0.707106781186549,0.707106781186546)) ;
#96822 = DIRECTION('center_axis',(0.,0.,-1.)) ;
#96823 = DIRECTION('ref_axis',(-1.,0.,0.)) ;
#96824 = DIRECTION('center_axis',(0.,0.,1.)) ;
#96825 = DIRECTION('ref_axis',(-1.,1.0842021724855E-15,0.)) ;
#96826 = DIRECTION('center_axis',(0.,0.,-1.)) ;
#96827 = DIRECTION('ref_axis',(-1.,0.,0.)) ;
#96828 = DIRECTION('center_axis',(-0.577350269189625,-0.577350269189626,0.577350269189627)) ;
#96829 = DIRECTION('ref_axis',(-2.71345386026911E-16,-0.707106781186548,-0.707106781186547)) ;
#96830 = DIRECTION('center_axis',(0.577350269189625,0.577350269189626,-0.577350269189627)) ;
#96831 = DIRECTION('ref_axis',(-9.76085677604559E-15,-0.707106781186543,-0.707106781186552)) ;
#96832 = DIRECTION('center_axis',(0.577350269189625,0.577350269189625,-0.577350269189628)) ;
#96833 = DIRECTION('ref_axis',(-0.707106781186549,-7.23605167296792E-16,-0.707106781186546)) ;
#96834 = DIRECTION('center_axis',(-0.577350269189625,-0.577350269189625,0.577350269189628)) ;
#96835 = DIRECTION('ref_axis',(-0.707106781186542,-1.47047746496289E-14,-0.707106781186553)) ;
#96836 = DIRECTION('center_axis',(-0.577350269189629,-0.577350269189624,0.577350269189624)) ;
#96837 = DIRECTION('ref_axis',(0.707106781186545,-9.59471324968973E-16,0.70710678118655)) ;
#96838 = DIRECTION('center_axis',(0.,0.,-1.)) ;
#96839 = DIRECTION('ref_axis',(-1.,0.,0.)) ;
#96840 = DIRECTION('center_axis',(0.,0.,1.)) ;
#96841 = DIRECTION('ref_axis',(-1.,0.,0.)) ;
#96842 = DIRECTION('center_axis',(0.,0.,-1.)) ;
#96843 = DIRECTION('ref_axis',(-1.,0.,0.)) ;
#96844 = DIRECTION('center_axis',(2.08166817117218E-16,1.,0.)) ;
#96845 = DIRECTION('ref_axis',(1.,0.,0.)) ;
#96846 = DIRECTION('center_axis',(-1.,0.,-5.94151198964807E-15)) ;
#96847 = DIRECTION('ref_axis',(5.94151198964807E-15,0.,-1.)) ;
#96848 = DIRECTION('center_axis',(0.,0.,1.)) ;
#96849 = DIRECTION('ref_axis',(-1.,0.,0.)) ;
#96850 = DIRECTION('center_axis',(-0.577350269189625,-0.577350269189625,-0.577350269189628)) ;
#96851 = DIRECTION('ref_axis',(-0.707106781186549,-7.23605167296792E-16,0.707106781186546)) ;
#96852 = DIRECTION('center_axis',(-0.577350269189625,-0.577350269189625,-0.577350269189628)) ;
#96853 = DIRECTION('ref_axis',(-0.707106781186549,-7.51360742912421E-16,0.707106781186546)) ;
#96854 = DIRECTION('center_axis',(-0.577350269189629,-0.577350269189628,-0.577350269189621)) ;
#96855 = DIRECTION('ref_axis',(0.707106781186547,-0.707106781186548,-9.25270248417546E-17)) ;
#96856 = DIRECTION('center_axis',(0.,0.,-1.)) ;
#96857 = DIRECTION('ref_axis',(-1.,0.,0.)) ;
#96858 = DIRECTION('center_axis',(1.2266347333467E-14,0.,1.)) ;
#96859 = DIRECTION('ref_axis',(1.,0.,-1.2266347333467E-14)) ;
#96860 = DIRECTION('center_axis',(-1.,0.,9.8563833862319E-18)) ;
#96861 = DIRECTION('ref_axis',(9.8563833862319E-18,0.,1.)) ;
#96862 = DIRECTION('center_axis',(-1.,1.62630325872825E-15,-1.62630325872825E-15)) ;
#96863 = DIRECTION('ref_axis',(-1.62630325872825E-15,0.,1.)) ;
#96864 = DIRECTION('center_axis',(2.08166817117218E-16,1.,0.)) ;
#96865 = DIRECTION('ref_axis',(1.,0.,0.)) ;
#96866 = DIRECTION('center_axis',(-1.,1.35525271560688E-16,1.35525271560688E-16)) ;
#96867 = DIRECTION('ref_axis',(-1.35525271560688E-16,0.,-1.)) ;
#96868 = DIRECTION('center_axis',(2.08166817117218E-16,1.,0.)) ;
#96869 = DIRECTION('ref_axis',(1.,0.,0.)) ;
#96870 = DIRECTION('center_axis',(-0.577350269189628,0.577350269189628,-0.577350269189621)) ;
#96871 = DIRECTION('ref_axis',(0.707106781186547,0.707106781186548,5.83290435273539E-16)) ;
#96872 = DIRECTION('center_axis',(1.2266347333467E-14,0.,1.)) ;
#96873 = DIRECTION('ref_axis',(-1.,0.,1.2266347333467E-14)) ;
#96874 = DIRECTION('center_axis',(-1.,0.,-9.8563833862319E-18)) ;
#96875 = DIRECTION('ref_axis',(-9.8563833862319E-18,0.,1.)) ;
#96876 = DIRECTION('center_axis',(-1.,0.,9.58308385427108E-16)) ;
#96877 = DIRECTION('ref_axis',(9.58308385427108E-16,0.,1.)) ;
#96878 = DIRECTION('center_axis',(0.,0.,-1.)) ;
#96879 = DIRECTION('ref_axis',(-1.,0.,0.)) ;
#96880 = DIRECTION('center_axis',(-8.67361737988402E-15,8.67361737988401E-15,
1.)) ;
#96881 = DIRECTION('ref_axis',(1.,-9.79595207717063E-44,8.67361737988402E-15)) ;
#96882 = DIRECTION('center_axis',(0.577350269189625,-0.577350269189625,0.577350269189628)) ;
#96883 = DIRECTION('ref_axis',(0.707106781186549,-7.23605167296792E-16,-0.707106781186546)) ;
#96884 = DIRECTION('center_axis',(0.577350269189625,-0.577350269189625,0.577350269189628)) ;
#96885 = DIRECTION('ref_axis',(0.707106781186549,-7.51360742912421E-16,-0.707106781186546)) ;
#96886 = DIRECTION('center_axis',(2.08166817117218E-16,1.,0.)) ;
#96887 = DIRECTION('ref_axis',(1.,0.,0.)) ;
#96888 = DIRECTION('center_axis',(-0.577350269189631,0.577350269189623,0.577350269189623)) ;
#96889 = DIRECTION('ref_axis',(-0.707106781186542,1.43689139429453E-15,-0.707106781186553)) ;
#96890 = DIRECTION('center_axis',(0.,0.,-1.)) ;
#96891 = DIRECTION('ref_axis',(-1.,0.,0.)) ;
#96892 = DIRECTION('center_axis',(0.,0.,1.)) ;
#96893 = DIRECTION('ref_axis',(-1.,0.,0.)) ;
#96894 = DIRECTION('center_axis',(0.,0.,-1.)) ;
#96895 = DIRECTION('ref_axis',(-1.,0.,0.)) ;
#96896 = DIRECTION('center_axis',(-0.577350269189625,0.577350269189625,0.577350269189628)) ;
#96897 = DIRECTION('ref_axis',(0.707106781186549,-7.51360742912421E-16,0.707106781186546)) ;
#96898 = DIRECTION('center_axis',(0.577350269189625,-0.577350269189625,-0.577350269189628)) ;
#96899 = DIRECTION('ref_axis',(0.707106781186549,-8.43215074740835E-16,0.707106781186546)) ;
#96900 = DIRECTION('center_axis',(-0.577350269189625,0.577350269189626,-0.577350269189626)) ;
#96901 = DIRECTION('ref_axis',(6.27941990732594E-17,0.707106781186548,0.707106781186548)) ;
#96902 = DIRECTION('center_axis',(0.577350269189625,-0.577350269189626,0.577350269189626)) ;
#96903 = DIRECTION('ref_axis',(-4.12932450763554E-14,0.707106781186527,0.707106781186568)) ;
#96904 = DIRECTION('center_axis',(0.577350269189626,-0.577350269189626,0.577350269189626)) ;
#96905 = DIRECTION('ref_axis',(0.707106781186548,0.707106781186547,-6.70219100485003E-16)) ;
#96906 = DIRECTION('center_axis',(0.,0.,-1.)) ;
#96907 = DIRECTION('ref_axis',(-1.,0.,0.)) ;
#96908 = DIRECTION('center_axis',(0.,0.,1.)) ;
#96909 = DIRECTION('ref_axis',(-1.,0.,0.)) ;
#96910 = DIRECTION('center_axis',(0.,0.,-1.)) ;
#96911 = DIRECTION('ref_axis',(-1.,0.,0.)) ;
#96912 = DIRECTION('center_axis',(0.,1.,0.)) ;
#96913 = DIRECTION('ref_axis',(1.,0.,0.)) ;
#96914 = DIRECTION('center_axis',(0.,-1.,-1.05413922396982E-14)) ;
#96915 = DIRECTION('ref_axis',(0.,-1.05413922396982E-14,1.)) ;
#96916 = DIRECTION('center_axis',(-8.67361737988401E-15,8.67361737988403E-15,
1.)) ;
#96917 = DIRECTION('ref_axis',(-4.48415508583941E-44,1.,-8.67361737988403E-15)) ;
#96918 = DIRECTION('center_axis',(0.577350269189625,-0.577350269189626,-0.577350269189626)) ;
#96919 = DIRECTION('ref_axis',(6.27941990732594E-17,0.707106781186548,-0.707106781186548)) ;
#96920 = DIRECTION('center_axis',(0.577350269189625,-0.577350269189626,-0.577350269189626)) ;
#96921 = DIRECTION('ref_axis',(-7.7646791370609E-16,0.707106781186547,-0.707106781186548)) ;
#96922 = DIRECTION('center_axis',(0.577350269189627,-0.577350269189628,-0.577350269189622)) ;
#96923 = DIRECTION('ref_axis',(0.707106781186548,0.707106781186547,-7.93962717014541E-17)) ;
#96924 = DIRECTION('center_axis',(0.,0.,-1.)) ;
#96925 = DIRECTION('ref_axis',(-1.,0.,0.)) ;
#96926 = DIRECTION('center_axis',(0.,1.2266347333467E-14,1.)) ;
#96927 = DIRECTION('ref_axis',(0.,-1.,1.2266347333467E-14)) ;
#96928 = DIRECTION('center_axis',(0.,1.,1.95511867169518E-16)) ;
#96929 = DIRECTION('ref_axis',(0.,-1.95511867169518E-16,1.)) ;
#96930 = DIRECTION('center_axis',(-1.42301535138722E-15,-1.,-1.61467702847264E-15)) ;
#96931 = DIRECTION('ref_axis',(-1.65443041324959E-32,1.61467702847264E-15,
-1.)) ;
#96932 = DIRECTION('center_axis',(0.,1.,0.)) ;
#96933 = DIRECTION('ref_axis',(1.,0.,0.)) ;
#96934 = DIRECTION('center_axis',(3.72694496791891E-15,-1.,-3.53528329083349E-15)) ;
#96935 = DIRECTION('ref_axis',(-1.,-3.72694496791891E-15,0.)) ;
#96936 = DIRECTION('center_axis',(0.,1.,0.)) ;
#96937 = DIRECTION('ref_axis',(1.,0.,0.)) ;
#96938 = DIRECTION('center_axis',(-0.577350269189623,-0.577350269189624,-0.577350269189631)) ;
#96939 = DIRECTION('ref_axis',(1.89964573407132E-15,-0.707106781186553,0.707106781186542)) ;
#96940 = DIRECTION('center_axis',(0.,-1.2266347333467E-14,1.)) ;
#96941 = DIRECTION('ref_axis',(0.,1.,1.2266347333467E-14)) ;
#96942 = DIRECTION('center_axis',(0.,1.,-1.95511867169518E-16)) ;
#96943 = DIRECTION('ref_axis',(0.,1.95511867169518E-16,1.)) ;
#96944 = DIRECTION('center_axis',(0.,-1.,-7.66646708341686E-16)) ;
#96945 = DIRECTION('ref_axis',(0.,7.66646708341686E-16,-1.)) ;
#96946 = DIRECTION('center_axis',(0.,0.,-1.)) ;
#96947 = DIRECTION('ref_axis',(-1.,0.,0.)) ;
#96948 = DIRECTION('center_axis',(0.,0.,1.)) ;
#96949 = DIRECTION('ref_axis',(1.,0.,0.)) ;
#96950 = DIRECTION('center_axis',(0.577350269189625,0.577350269189626,0.577350269189627)) ;
#96951 = DIRECTION('ref_axis',(-2.71345386026911E-16,-0.707106781186548,0.707106781186547)) ;
#96952 = DIRECTION('center_axis',(0.577350269189625,0.577350269189626,0.577350269189627)) ;
#96953 = DIRECTION('ref_axis',(-2.71345386026911E-16,-0.707106781186548,0.707106781186547)) ;
#96954 = DIRECTION('center_axis',(0.,1.,0.)) ;
#96955 = DIRECTION('ref_axis',(1.,0.,0.)) ;
#96956 = DIRECTION('center_axis',(-0.577350269189625,-0.577350269189627,0.577350269189625)) ;
#96957 = DIRECTION('ref_axis',(4.24759239037863E-16,0.707106781186546,0.707106781186549)) ;
#96958 = DIRECTION('center_axis',(0.,0.,-1.)) ;
#96959 = DIRECTION('ref_axis',(-1.,0.,0.)) ;
#96960 = DIRECTION('center_axis',(0.,0.,1.)) ;
#96961 = DIRECTION('ref_axis',(-1.,1.0842021724855E-15,0.)) ;
#96962 = DIRECTION('center_axis',(0.,0.,-1.)) ;
#96963 = DIRECTION('ref_axis',(-1.,0.,0.)) ;
#96964 = DIRECTION('center_axis',(-0.577350269189625,-0.577350269189626,0.577350269189627)) ;
#96965 = DIRECTION('ref_axis',(-2.71345386026911E-16,-0.707106781186548,-0.707106781186547)) ;
#96966 = DIRECTION('center_axis',(0.577350269189625,0.577350269189626,-0.577350269189627)) ;
#96967 = DIRECTION('ref_axis',(-8.1269550549169E-15,-0.707106781186544,-0.707106781186551)) ;
#96968 = DIRECTION('center_axis',(0.577350269189625,0.577350269189625,-0.577350269189628)) ;
#96969 = DIRECTION('ref_axis',(-0.707106781186549,-7.23605167296792E-16,-0.707106781186546)) ;
#96970 = DIRECTION('center_axis',(-0.577350269189625,-0.577350269189625,0.577350269189628)) ;
#96971 = DIRECTION('ref_axis',(-0.707106781186545,-8.33999502129868E-15,-0.70710678118655)) ;
#96972 = DIRECTION('center_axis',(-0.577350269189627,-0.577350269189625,0.577350269189625)) ;
#96973 = DIRECTION('ref_axis',(0.707106781186546,1.26631399429469E-16,0.707106781186549)) ;
#96974 = DIRECTION('center_axis',(0.,0.,-1.)) ;
#96975 = DIRECTION('ref_axis',(-1.,0.,0.)) ;
#96976 = DIRECTION('center_axis',(0.,0.,1.)) ;
#96977 = DIRECTION('ref_axis',(-1.,0.,0.)) ;
#96978 = DIRECTION('center_axis',(0.,0.,-1.)) ;
#96979 = DIRECTION('ref_axis',(-1.,0.,0.)) ;
#96980 = DIRECTION('center_axis',(2.08166817117218E-16,1.,0.)) ;
#96981 = DIRECTION('ref_axis',(1.,0.,0.)) ;
#96982 = DIRECTION('center_axis',(-1.,0.,9.58308385427108E-16)) ;
#96983 = DIRECTION('ref_axis',(-9.58308385427108E-16,0.,-1.)) ;
#96984 = DIRECTION('center_axis',(0.,0.,1.)) ;
#96985 = DIRECTION('ref_axis',(-1.,0.,0.)) ;
#96986 = DIRECTION('center_axis',(-0.577350269189625,-0.577350269189625,-0.577350269189628)) ;
#96987 = DIRECTION('ref_axis',(-0.707106781186549,-7.23605167296792E-16,0.707106781186546)) ;
#96988 = DIRECTION('center_axis',(-0.577350269189625,-0.577350269189625,-0.577350269189628)) ;
#96989 = DIRECTION('ref_axis',(-0.707106781186549,-7.51360742912421E-16,0.707106781186546)) ;
#96990 = DIRECTION('center_axis',(-0.577350269189633,-0.577350269189632,-0.577350269189612)) ;
#96991 = DIRECTION('ref_axis',(0.707106781186547,-0.707106781186548,-7.39398349810839E-17)) ;
#96992 = DIRECTION('center_axis',(0.,0.,-1.)) ;
#96993 = DIRECTION('ref_axis',(-1.,0.,0.)) ;
#96994 = DIRECTION('center_axis',(2.4532694666934E-14,0.,1.)) ;
#96995 = DIRECTION('ref_axis',(1.,0.,-2.4532694666934E-14)) ;
#96996 = DIRECTION('center_axis',(-1.,0.,9.8563833862319E-18)) ;
#96997 = DIRECTION('ref_axis',(9.8563833862319E-18,0.,1.)) ;
#96998 = DIRECTION('center_axis',(-1.,-8.40256683676264E-15,8.40256683676264E-15)) ;
#96999 = DIRECTION('ref_axis',(8.40256683676264E-15,-6.05360936588321E-43,
1.)) ;
#97000 = DIRECTION('center_axis',(2.08166817117218E-16,1.,0.)) ;
#97001 = DIRECTION('ref_axis',(1.,0.,0.)) ;
#97002 = DIRECTION('center_axis',(-1.,4.9466724119651E-15,4.9466724119651E-15)) ;
#97003 = DIRECTION('ref_axis',(-4.9466724119651E-15,-2.12997366577372E-43,
-1.)) ;
#97004 = DIRECTION('center_axis',(2.08166817117218E-16,1.,0.)) ;
#97005 = DIRECTION('ref_axis',(1.,0.,0.)) ;
#97006 = DIRECTION('center_axis',(-0.577350269189629,0.577350269189628,-0.577350269189621)) ;
#97007 = DIRECTION('ref_axis',(0.707106781186547,0.707106781186548,-3.27220711197328E-17)) ;
#97008 = DIRECTION('center_axis',(0.,0.,1.)) ;
#97009 = DIRECTION('ref_axis',(-1.,0.,0.)) ;
#97010 = DIRECTION('center_axis',(-1.,0.,-9.8563833862319E-18)) ;
#97011 = DIRECTION('ref_axis',(-9.8563833862319E-18,0.,1.)) ;
#97012 = DIRECTION('center_axis',(-1.,0.,-1.05413922396982E-14)) ;
#97013 = DIRECTION('ref_axis',(-1.05413922396982E-14,0.,1.)) ;
#97014 = DIRECTION('center_axis',(0.,0.,-1.)) ;
#97015 = DIRECTION('ref_axis',(-1.,0.,0.)) ;
#97016 = DIRECTION('center_axis',(0.,0.,1.)) ;
#97017 = DIRECTION('ref_axis',(1.,0.,0.)) ;
#97018 = DIRECTION('center_axis',(0.577350269189625,-0.577350269189625,0.577350269189628)) ;
#97019 = DIRECTION('ref_axis',(0.707106781186549,-7.23605167296792E-16,-0.707106781186546)) ;
#97020 = DIRECTION('center_axis',(0.577350269189625,-0.577350269189625,0.577350269189628)) ;
#97021 = DIRECTION('ref_axis',(0.707106781186549,-7.51360742912421E-16,-0.707106781186546)) ;
#97022 = DIRECTION('center_axis',(2.08166817117218E-16,1.,0.)) ;
#97023 = DIRECTION('ref_axis',(1.,0.,0.)) ;
#97024 = DIRECTION('center_axis',(-0.577350269189631,0.577350269189623,0.577350269189623)) ;
#97025 = DIRECTION('ref_axis',(-0.707106781186544,-2.28159610212341E-15,-0.707106781186551)) ;
#97026 = DIRECTION('center_axis',(0.,0.,-1.)) ;
#97027 = DIRECTION('ref_axis',(-1.,0.,0.)) ;
#97028 = DIRECTION('center_axis',(0.,0.,1.)) ;
#97029 = DIRECTION('ref_axis',(-1.,0.,0.)) ;
#97030 = DIRECTION('center_axis',(0.,0.,-1.)) ;
#97031 = DIRECTION('ref_axis',(-1.,0.,0.)) ;
#97032 = DIRECTION('center_axis',(-0.577350269189625,0.577350269189625,0.577350269189628)) ;
#97033 = DIRECTION('ref_axis',(0.707106781186549,-7.51360742912421E-16,0.707106781186546)) ;
#97034 = DIRECTION('center_axis',(0.577350269189625,-0.577350269189625,-0.577350269189628)) ;
#97035 = DIRECTION('ref_axis',(0.707106781186548,-2.12258087602815E-15,0.707106781186547)) ;
#97036 = DIRECTION('center_axis',(-0.577350269189625,0.577350269189626,-0.577350269189626)) ;
#97037 = DIRECTION('ref_axis',(6.27941990732594E-17,0.707106781186548,0.707106781186548)) ;
#97038 = DIRECTION('center_axis',(0.577350269189625,-0.577350269189626,0.577350269189626)) ;
#97039 = DIRECTION('ref_axis',(-2.74316855014674E-14,0.707106781186534,0.707106781186561)) ;
#97040 = DIRECTION('center_axis',(0.577350269189617,-0.577350269189643,0.577350269189617)) ;
#97041 = DIRECTION('ref_axis',(0.707106781186564,0.707106781186531,-7.69284786604672E-16)) ;
#97042 = DIRECTION('center_axis',(0.,0.,-1.)) ;
#97043 = DIRECTION('ref_axis',(-1.,0.,0.)) ;
#97044 = DIRECTION('center_axis',(0.,0.,1.)) ;
#97045 = DIRECTION('ref_axis',(-1.,0.,0.)) ;
#97046 = DIRECTION('center_axis',(0.,0.,-1.)) ;
#97047 = DIRECTION('ref_axis',(-1.,0.,0.)) ;
#97048 = DIRECTION('center_axis',(0.,1.,0.)) ;
#97049 = DIRECTION('ref_axis',(1.,0.,0.)) ;
#97050 = DIRECTION('center_axis',(0.,-1.,-1.39913024272358E-14)) ;
#97051 = DIRECTION('ref_axis',(0.,-1.39913024272358E-14,1.)) ;
#97052 = DIRECTION('center_axis',(1.7347234759768E-14,-1.73472347597681E-14,
1.)) ;
#97053 = DIRECTION('ref_axis',(-1.79366203433577E-43,1.,1.73472347597681E-14)) ;
#97054 = DIRECTION('center_axis',(0.577350269189625,-0.577350269189626,-0.577350269189626)) ;
#97055 = DIRECTION('ref_axis',(6.27941990732594E-17,0.707106781186548,-0.707106781186548)) ;
#97056 = DIRECTION('center_axis',(0.577350269189625,-0.577350269189626,-0.577350269189626)) ;
#97057 = DIRECTION('ref_axis',(-7.7646791370609E-16,0.707106781186547,-0.707106781186548)) ;
#97058 = DIRECTION('center_axis',(0.577350269189636,-0.577350269189637,-0.577350269189605)) ;
#97059 = DIRECTION('ref_axis',(0.707106781186548,0.707106781186547,-1.89650892222054E-16)) ;
#97060 = DIRECTION('center_axis',(0.,0.,-1.)) ;
#97061 = DIRECTION('ref_axis',(-1.,0.,0.)) ;
#97062 = DIRECTION('center_axis',(0.,2.4532694666934E-14,1.)) ;
#97063 = DIRECTION('ref_axis',(0.,-1.,2.4532694666934E-14)) ;
#97064 = DIRECTION('center_axis',(0.,1.,1.95511867169518E-16)) ;
#97065 = DIRECTION('ref_axis',(0.,-1.95511867169518E-16,1.)) ;
#97066 = DIRECTION('center_axis',(1.21972744404619E-15,-1.,1.02806576696077E-15)) ;
#97067 = DIRECTION('ref_axis',(1.,1.21972744404619E-15,0.)) ;
#97068 = DIRECTION('center_axis',(0.,1.,0.)) ;
#97069 = DIRECTION('ref_axis',(1.,0.,0.)) ;
#97070 = DIRECTION('center_axis',(-1.41623908780917E-14,-1.,1.43540525551772E-14)) ;
#97071 = DIRECTION('ref_axis',(-1.64655217322172E-31,1.43540525551772E-14,
1.)) ;
#97072 = DIRECTION('center_axis',(0.,1.,0.)) ;
#97073 = DIRECTION('ref_axis',(1.,0.,0.)) ;
#97074 = DIRECTION('center_axis',(-0.577350269189625,-0.577350269189626,-0.577350269189626)) ;
#97075 = DIRECTION('ref_axis',(4.43092933859209E-16,-0.707106781186548,0.707106781186547)) ;
#97076 = DIRECTION('center_axis',(0.,0.,1.)) ;
#97077 = DIRECTION('ref_axis',(-1.,8.87690528722505E-15,0.)) ;
#97078 = DIRECTION('center_axis',(0.,1.,-1.95511867169518E-16)) ;
#97079 = DIRECTION('ref_axis',(0.,1.95511867169518E-16,1.)) ;
#97080 = DIRECTION('center_axis',(0.,-1.,-2.17536003491953E-14)) ;
#97081 = DIRECTION('ref_axis',(0.,2.17536003491953E-14,-1.)) ;
#97082 = DIRECTION('center_axis',(0.,0.,-1.)) ;
#97083 = DIRECTION('ref_axis',(-1.,0.,0.)) ;
#97084 = DIRECTION('center_axis',(-1.7347234759768E-14,-1.73472347597681E-14,
1.)) ;
#97085 = DIRECTION('ref_axis',(-8.96831017167883E-44,-1.,-1.73472347597681E-14)) ;
#97086 = DIRECTION('center_axis',(0.577350269189625,0.577350269189626,0.577350269189627)) ;
#97087 = DIRECTION('ref_axis',(-2.71345386026911E-16,-0.707106781186548,0.707106781186547)) ;
#97088 = DIRECTION('center_axis',(0.577350269189625,0.577350269189626,0.577350269189627)) ;
#97089 = DIRECTION('ref_axis',(-2.71345386026911E-16,-0.707106781186548,0.707106781186547)) ;
#97090 = DIRECTION('center_axis',(0.,1.,0.)) ;
#97091 = DIRECTION('ref_axis',(1.,0.,0.)) ;
#97092 = DIRECTION('center_axis',(-0.577350269189615,-0.577350269189648,0.577350269189615)) ;
#97093 = DIRECTION('ref_axis',(-7.65039491896549E-15,0.707106781186531,0.707106781186564)) ;
#97094 = DIRECTION('center_axis',(0.,0.,-1.)) ;
#97095 = DIRECTION('ref_axis',(-1.,0.,0.)) ;
#97096 = DIRECTION('center_axis',(0.,0.,1.)) ;
#97097 = DIRECTION('ref_axis',(-1.,1.0842021724855E-15,0.)) ;
#97098 = DIRECTION('center_axis',(0.,0.,-1.)) ;
#97099 = DIRECTION('ref_axis',(-1.,0.,0.)) ;
#97100 = DIRECTION('center_axis',(-0.577350269189625,-0.577350269189626,0.577350269189627)) ;
#97101 = DIRECTION('ref_axis',(-2.71345386026911E-16,-0.707106781186548,-0.707106781186547)) ;
#97102 = DIRECTION('center_axis',(0.577350269189625,0.577350269189626,-0.577350269189627)) ;
#97103 = DIRECTION('ref_axis',(1.27552458785726E-14,-0.707106781186554,-0.707106781186541)) ;
#97104 = DIRECTION('center_axis',(0.577350269189625,0.577350269189625,-0.577350269189628)) ;
#97105 = DIRECTION('ref_axis',(-0.707106781186549,-7.23605167296792E-16,-0.707106781186546)) ;
#97106 = DIRECTION('center_axis',(-0.577350269189625,-0.577350269189625,0.577350269189628)) ;
#97107 = DIRECTION('ref_axis',(-0.707106781186545,-8.28019006757666E-15,-0.70710678118655)) ;
#97108 = DIRECTION('center_axis',(-0.577350269189628,-0.577350269189625,0.577350269189625)) ;
#97109 = DIRECTION('ref_axis',(0.707106781186546,1.58001979428239E-16,0.707106781186549)) ;
#97110 = DIRECTION('center_axis',(0.,0.,-1.)) ;
#97111 = DIRECTION('ref_axis',(-1.,0.,0.)) ;
#97112 = DIRECTION('center_axis',(0.,0.,1.)) ;
#97113 = DIRECTION('ref_axis',(-1.,-8.67361737988404E-15,0.)) ;
#97114 = DIRECTION('center_axis',(0.,0.,-1.)) ;
#97115 = DIRECTION('ref_axis',(-1.,0.,0.)) ;
#97116 = DIRECTION('center_axis',(2.08166817117218E-16,1.,0.)) ;
#97117 = DIRECTION('ref_axis',(1.,0.,0.)) ;
#97118 = DIRECTION('center_axis',(-1.,0.,-4.40821857296469E-15)) ;
#97119 = DIRECTION('ref_axis',(4.40821857296469E-15,0.,-1.)) ;
#97120 = DIRECTION('center_axis',(0.,0.,1.)) ;
#97121 = DIRECTION('ref_axis',(-1.,0.,0.)) ;
#97122 = DIRECTION('center_axis',(-0.577350269189625,-0.577350269189625,-0.577350269189628)) ;
#97123 = DIRECTION('ref_axis',(-0.707106781186549,-7.23605167296792E-16,0.707106781186546)) ;
#97124 = DIRECTION('center_axis',(-0.577350269189625,-0.577350269189625,-0.577350269189628)) ;
#97125 = DIRECTION('ref_axis',(-0.707106781186549,-7.51360742912421E-16,0.707106781186546)) ;
#97126 = DIRECTION('center_axis',(-0.577350269189624,-0.577350269189624,-0.57735026918963)) ;
#97127 = DIRECTION('ref_axis',(-0.70710678118655,-1.90469774984546E-15,0.707106781186545)) ;
#97128 = DIRECTION('center_axis',(0.,0.,-1.)) ;
#97129 = DIRECTION('ref_axis',(-1.,0.,0.)) ;
#97130 = DIRECTION('center_axis',(0.,0.,1.)) ;
#97131 = DIRECTION('ref_axis',(1.,0.,0.)) ;
#97132 = DIRECTION('center_axis',(-1.,0.,9.8563833862319E-18)) ;
#97133 = DIRECTION('ref_axis',(9.8563833862319E-18,0.,1.)) ;
#97134 = DIRECTION('center_axis',(-1.,3.93023287525994E-15,-3.93023287525994E-15)) ;
#97135 = DIRECTION('ref_axis',(-3.93023287525994E-15,-1.34524652575182E-43,
1.)) ;
#97136 = DIRECTION('center_axis',(2.08166817117218E-16,1.,0.)) ;
#97137 = DIRECTION('ref_axis',(1.,0.,0.)) ;
#97138 = DIRECTION('center_axis',(-1.,-4.33680868994201E-15,-4.33680868994201E-15)) ;
#97139 = DIRECTION('ref_axis',(4.33680868994201E-15,-1.59748024933029E-43,
-1.)) ;
#97140 = DIRECTION('center_axis',(2.08166817117218E-16,1.,0.)) ;
#97141 = DIRECTION('ref_axis',(1.,0.,0.)) ;
#97142 = DIRECTION('center_axis',(-0.577350269189625,0.577350269189624,-0.577350269189628)) ;
#97143 = DIRECTION('ref_axis',(0.707106781186549,-6.77492742903108E-16,-0.707106781186546)) ;
#97144 = DIRECTION('center_axis',(0.,0.,1.)) ;
#97145 = DIRECTION('ref_axis',(-1.,0.,0.)) ;
#97146 = DIRECTION('center_axis',(-1.,0.,-9.8563833862319E-18)) ;
#97147 = DIRECTION('ref_axis',(-9.8563833862319E-18,0.,1.)) ;
#97148 = DIRECTION('center_axis',(-1.,0.,-9.00809882301481E-15)) ;
#97149 = DIRECTION('ref_axis',(-9.00809882301481E-15,0.,1.)) ;
#97150 = DIRECTION('center_axis',(0.,0.,-1.)) ;
#97151 = DIRECTION('ref_axis',(-1.,0.,0.)) ;
#97152 = DIRECTION('center_axis',(0.,0.,1.)) ;
#97153 = DIRECTION('ref_axis',(1.,0.,0.)) ;
#97154 = DIRECTION('center_axis',(0.577350269189625,-0.577350269189625,0.577350269189628)) ;
#97155 = DIRECTION('ref_axis',(0.707106781186549,-7.23605167296792E-16,-0.707106781186546)) ;
#97156 = DIRECTION('center_axis',(0.577350269189625,-0.577350269189625,0.577350269189628)) ;
#97157 = DIRECTION('ref_axis',(0.707106781186549,-7.51360742912421E-16,-0.707106781186546)) ;
#97158 = DIRECTION('center_axis',(2.08166817117218E-16,1.,0.)) ;
#97159 = DIRECTION('ref_axis',(1.,0.,0.)) ;
#97160 = DIRECTION('center_axis',(-0.57735026918963,0.577350269189624,0.577350269189624)) ;
#97161 = DIRECTION('ref_axis',(-0.707106781186544,-8.1317851962192E-16,-0.707106781186551)) ;
#97162 = DIRECTION('center_axis',(0.,0.,-1.)) ;
#97163 = DIRECTION('ref_axis',(-1.,0.,0.)) ;
#97164 = DIRECTION('center_axis',(0.,0.,1.)) ;
#97165 = DIRECTION('ref_axis',(-1.,0.,0.)) ;
#97166 = DIRECTION('center_axis',(0.,0.,-1.)) ;
#97167 = DIRECTION('ref_axis',(-1.,0.,0.)) ;
#97168 = DIRECTION('center_axis',(-0.577350269189625,0.577350269189625,0.577350269189628)) ;
#97169 = DIRECTION('ref_axis',(0.707106781186549,-7.51360742912421E-16,0.707106781186546)) ;
#97170 = DIRECTION('center_axis',(0.577350269189625,-0.577350269189625,-0.577350269189628)) ;
#97171 = DIRECTION('ref_axis',(0.707106781186545,-8.51940988246475E-15,0.70710678118655)) ;
#97172 = DIRECTION('center_axis',(-0.577350269189625,0.577350269189626,-0.577350269189626)) ;
#97173 = DIRECTION('ref_axis',(6.27941990732594E-17,0.707106781186548,0.707106781186548)) ;
#97174 = DIRECTION('center_axis',(0.577350269189625,-0.577350269189626,0.577350269189626)) ;
#97175 = DIRECTION('ref_axis',(-6.96183268087023E-15,0.707106781186544,0.707106781186551)) ;
#97176 = DIRECTION('center_axis',(0.577350269189619,-0.57735026918964,0.577350269189619)) ;
#97177 = DIRECTION('ref_axis',(0.70710678118656,0.707106781186535,9.56388759536482E-16)) ;
#97178 = DIRECTION('center_axis',(0.,0.,-1.)) ;
#97179 = DIRECTION('ref_axis',(-1.,0.,0.)) ;
#97180 = DIRECTION('center_axis',(0.,0.,1.)) ;
#97181 = DIRECTION('ref_axis',(-1.,0.,0.)) ;
#97182 = DIRECTION('center_axis',(0.,0.,-1.)) ;
#97183 = DIRECTION('ref_axis',(-1.,0.,0.)) ;
#97184 = DIRECTION('center_axis',(0.,1.,0.)) ;
#97185 = DIRECTION('ref_axis',(1.,0.,0.)) ;
#97186 = DIRECTION('center_axis',(0.,-1.,-5.94151198964807E-15)) ;
#97187 = DIRECTION('ref_axis',(0.,-5.94151198964807E-15,1.)) ;
#97188 = DIRECTION('center_axis',(1.7347234759768E-14,-1.73472347597681E-14,
1.)) ;
#97189 = DIRECTION('ref_axis',(-1.79366203433577E-43,1.,1.73472347597681E-14)) ;
#97190 = DIRECTION('center_axis',(0.577350269189625,-0.577350269189626,-0.577350269189626)) ;
#97191 = DIRECTION('ref_axis',(6.27941990732594E-17,0.707106781186548,-0.707106781186548)) ;
#97192 = DIRECTION('center_axis',(0.577350269189625,-0.577350269189626,-0.577350269189626)) ;
#97193 = DIRECTION('ref_axis',(3.83287980137187E-16,0.707106781186548,-0.707106781186547)) ;
#97194 = DIRECTION('center_axis',(0.57735026918963,-0.577350269189631,-0.577350269189617)) ;
#97195 = DIRECTION('ref_axis',(0.707106781186548,0.707106781186547,-9.21608659434825E-17)) ;
#97196 = DIRECTION('center_axis',(0.,0.,-1.)) ;
#97197 = DIRECTION('ref_axis',(-1.,0.,0.)) ;
#97198 = DIRECTION('center_axis',(0.,0.,1.)) ;
#97199 = DIRECTION('ref_axis',(1.,0.,0.)) ;
#97200 = DIRECTION('center_axis',(0.,1.,1.95511867169518E-16)) ;
#97201 = DIRECTION('ref_axis',(0.,-1.95511867169518E-16,1.)) ;
#97202 = DIRECTION('center_axis',(1.15196480826585E-15,-1.,9.60303131180424E-16)) ;
#97203 = DIRECTION('ref_axis',(1.,1.15196480826585E-15,0.)) ;
#97204 = DIRECTION('center_axis',(0.,1.,0.)) ;
#97205 = DIRECTION('ref_axis',(1.,0.,0.)) ;
#97206 = DIRECTION('center_axis',(-7.5216525716181E-15,-1.,7.71331424870352E-15)) ;
#97207 = DIRECTION('ref_axis',(-8.74484647013228E-32,7.71331424870352E-15,
1.)) ;
#97208 = DIRECTION('center_axis',(0.,1.,0.)) ;
#97209 = DIRECTION('ref_axis',(1.,0.,0.)) ;
#97210 = DIRECTION('center_axis',(-0.577350269189626,-0.577350269189627,-0.577350269189625)) ;
#97211 = DIRECTION('ref_axis',(-0.707106781186548,0.707106781186547,-9.19305248608458E-17)) ;
#97212 = DIRECTION('center_axis',(0.,0.,1.)) ;
#97213 = DIRECTION('ref_axis',(-1.,1.76182853028894E-15,0.)) ;
#97214 = DIRECTION('center_axis',(0.,1.,-1.95511867169518E-16)) ;
#97215 = DIRECTION('ref_axis',(0.,1.95511867169518E-16,1.)) ;
#97216 = DIRECTION('center_axis',(0.,-1.,-7.95395959904499E-15)) ;
#97217 = DIRECTION('ref_axis',(0.,7.95395959904499E-15,-1.)) ;
#97218 = DIRECTION('center_axis',(0.,0.,-1.)) ;
#97219 = DIRECTION('ref_axis',(-1.,0.,0.)) ;
#97220 = DIRECTION('center_axis',(0.,0.,1.)) ;
#97221 = DIRECTION('ref_axis',(1.,0.,0.)) ;
#97222 = DIRECTION('center_axis',(0.577350269189625,0.577350269189626,0.577350269189627)) ;
#97223 = DIRECTION('ref_axis',(-2.71345386026911E-16,-0.707106781186548,0.707106781186547)) ;
#97224 = DIRECTION('center_axis',(0.577350269189625,0.577350269189626,0.577350269189627)) ;
#97225 = DIRECTION('ref_axis',(-2.71345386026911E-16,-0.707106781186548,0.707106781186547)) ;
#97226 = DIRECTION('center_axis',(0.,1.,0.)) ;
#97227 = DIRECTION('ref_axis',(1.,0.,0.)) ;
#97228 = DIRECTION('center_axis',(-0.577350269189622,-0.577350269189633,0.577350269189622)) ;
#97229 = DIRECTION('ref_axis',(-1.42949951585321E-15,0.707106781186542,0.707106781186553)) ;
#97230 = DIRECTION('center_axis',(0.,0.,-1.)) ;
#97231 = DIRECTION('ref_axis',(-1.,0.,0.)) ;
#97232 = DIRECTION('center_axis',(0.,0.,1.)) ;
#97233 = DIRECTION('ref_axis',(-1.,1.0842021724855E-15,0.)) ;
#97234 = DIRECTION('center_axis',(0.,0.,-1.)) ;
#97235 = DIRECTION('ref_axis',(-1.,0.,0.)) ;
#97236 = DIRECTION('center_axis',(-0.577350269189625,-0.577350269189626,0.577350269189627)) ;
#97237 = DIRECTION('ref_axis',(-2.71345386026911E-16,-0.707106781186548,-0.707106781186547)) ;
#97238 = DIRECTION('center_axis',(0.577350269189625,0.577350269189626,-0.577350269189627)) ;
#97239 = DIRECTION('ref_axis',(-2.71345386026911E-16,-0.707106781186548,-0.707106781186547)) ;
#97240 = DIRECTION('center_axis',(0.577350269189625,0.577350269189625,-0.577350269189628)) ;
#97241 = DIRECTION('ref_axis',(-0.707106781186552,5.19478420936363E-15,-0.707106781186543)) ;
#97242 = DIRECTION('center_axis',(-0.577350269189625,-0.577350269189625,0.577350269189628)) ;
#97243 = DIRECTION('ref_axis',(-0.707106781186566,3.31891725521342E-14,-0.707106781186529)) ;
#97244 = DIRECTION('center_axis',(-0.577350269189652,-0.577350269189606,0.57735026918962)) ;
#97245 = DIRECTION('ref_axis',(0.707106781186528,-3.96520952299298E-16,0.707106781186567)) ;
#97246 = DIRECTION('center_axis',(0.,0.,-1.)) ;
#97247 = DIRECTION('ref_axis',(-1.,0.,0.)) ;
#97248 = DIRECTION('center_axis',(0.,0.,1.)) ;
#97249 = DIRECTION('ref_axis',(-1.,-8.67361737988404E-15,0.)) ;
#97250 = DIRECTION('center_axis',(0.,0.,-1.)) ;
#97251 = DIRECTION('ref_axis',(-1.,0.,0.)) ;
#97252 = DIRECTION('center_axis',(2.08166817117218E-16,1.,0.)) ;
#97253 = DIRECTION('ref_axis',(1.,0.,0.)) ;
#97254 = DIRECTION('center_axis',(-1.,0.,-1.66745659064321E-14)) ;
#97255 = DIRECTION('ref_axis',(1.66745659064321E-14,2.60208521396523E-14,
-1.)) ;
#97256 = DIRECTION('center_axis',(-3.46944695195361E-14,-3.4694469519536E-14,
1.)) ;
#97257 = DIRECTION('ref_axis',(-1.,-1.68611237719883E-42,-3.46944695195361E-14)) ;
#97258 = DIRECTION('center_axis',(-0.577350269189625,-0.577350269189625,-0.577350269189628)) ;
#97259 = DIRECTION('ref_axis',(-0.707106781186552,5.19478420936363E-15,0.707106781186543)) ;
#97260 = DIRECTION('center_axis',(-0.577350269189625,-0.577350269189625,-0.577350269189628)) ;
#97261 = DIRECTION('ref_axis',(-0.707106781186552,5.1349792556416E-15,0.707106781186543)) ;
#97262 = DIRECTION('center_axis',(-0.577350269189626,-0.577350269189626,-0.577350269189626)) ;
#97263 = DIRECTION('ref_axis',(0.707106781186547,-0.707106781186548,6.36902276417946E-16)) ;
#97264 = DIRECTION('center_axis',(0.,0.,-1.)) ;
#97265 = DIRECTION('ref_axis',(-1.,0.,0.)) ;
#97266 = DIRECTION('center_axis',(0.,0.,1.)) ;
#97267 = DIRECTION('ref_axis',(1.,0.,0.)) ;
#97268 = DIRECTION('center_axis',(-1.,0.,9.8563833862319E-18)) ;
#97269 = DIRECTION('ref_axis',(9.8563833862319E-18,0.,1.)) ;
#97270 = DIRECTION('center_axis',(-1.,8.87690528722497E-15,-8.87690528722518E-15)) ;
#97271 = DIRECTION('ref_axis',(-8.87690528722518E-15,4.48415508583942E-43,
1.)) ;
#97272 = DIRECTION('center_axis',(2.08166817117218E-16,1.,0.)) ;
#97273 = DIRECTION('ref_axis',(1.,0.,0.)) ;
#97274 = DIRECTION('center_axis',(-1.,8.53809210832325E-15,8.53809210832346E-15)) ;
#97275 = DIRECTION('ref_axis',(-8.53809210832339E-15,8.67361737988409E-15,
-1.)) ;
#97276 = DIRECTION('center_axis',(2.08166817117218E-16,1.,0.)) ;
#97277 = DIRECTION('ref_axis',(1.,0.,0.)) ;
#97278 = DIRECTION('center_axis',(-0.577350269189622,0.577350269189621,-0.577350269189634)) ;
#97279 = DIRECTION('ref_axis',(0.707106781186563,1.66970714627838E-14,-0.707106781186532)) ;
#97280 = DIRECTION('center_axis',(0.,0.,1.)) ;
#97281 = DIRECTION('ref_axis',(-1.,0.,0.)) ;
#97282 = DIRECTION('center_axis',(-1.,0.,-9.8563833862319E-18)) ;
#97283 = DIRECTION('ref_axis',(-9.8563833862319E-18,0.,1.)) ;
#97284 = DIRECTION('center_axis',(-1.,0.,-1.34163173959798E-15)) ;
#97285 = DIRECTION('ref_axis',(-1.34163173959798E-15,0.,1.)) ;
#97286 = DIRECTION('center_axis',(0.,0.,-1.)) ;
#97287 = DIRECTION('ref_axis',(-1.,0.,0.)) ;
#97288 = DIRECTION('center_axis',(-3.46944695195361E-14,3.4694469519536E-14,
1.)) ;
#97289 = DIRECTION('ref_axis',(1.,-1.68611237719883E-42,3.46944695195361E-14)) ;
#97290 = DIRECTION('center_axis',(0.577350269189625,-0.577350269189625,0.577350269189628)) ;
#97291 = DIRECTION('ref_axis',(0.707106781186552,5.19478420936363E-15,-0.707106781186543)) ;
#97292 = DIRECTION('center_axis',(0.577350269189625,-0.577350269189625,0.577350269189628)) ;
#97293 = DIRECTION('ref_axis',(0.707106781186552,5.1349792556416E-15,-0.707106781186543)) ;
#97294 = DIRECTION('center_axis',(2.08166817117218E-16,1.,0.)) ;
#97295 = DIRECTION('ref_axis',(1.,0.,0.)) ;
#97296 = DIRECTION('center_axis',(-0.577350269189646,0.577350269189609,0.577350269189623)) ;
#97297 = DIRECTION('ref_axis',(-0.707106781186529,8.66006384940495E-15,-0.707106781186566)) ;
#97298 = DIRECTION('center_axis',(0.,0.,-1.)) ;
#97299 = DIRECTION('ref_axis',(-1.,0.,0.)) ;
#97300 = DIRECTION('center_axis',(0.,0.,1.)) ;
#97301 = DIRECTION('ref_axis',(-1.,0.,0.)) ;
#97302 = DIRECTION('center_axis',(0.,0.,-1.)) ;
#97303 = DIRECTION('ref_axis',(-1.,0.,0.)) ;
#97304 = DIRECTION('center_axis',(-0.577350269189625,0.577350269189625,0.577350269189628)) ;
#97305 = DIRECTION('ref_axis',(0.707106781186552,5.1349792556416E-15,0.707106781186543)) ;
#97306 = DIRECTION('center_axis',(0.577350269189625,-0.577350269189625,-0.577350269189628)) ;
#97307 = DIRECTION('ref_axis',(0.707106781186559,1.92955635991398E-14,0.707106781186536)) ;
#97308 = DIRECTION('center_axis',(-0.577350269189625,0.577350269189626,-0.577350269189626)) ;
#97309 = DIRECTION('ref_axis',(5.20172641667636E-15,0.70710678118655,0.707106781186545)) ;
#97310 = DIRECTION('center_axis',(0.577350269189625,-0.577350269189626,0.577350269189626)) ;
#97311 = DIRECTION('ref_axis',(1.27903606950626E-14,0.707106781186554,0.707106781186541)) ;
#97312 = DIRECTION('center_axis',(0.577350269189636,-0.577350269189592,0.57735026918965)) ;
#97313 = DIRECTION('ref_axis',(0.707106781186558,3.40611850366138E-15,-0.707106781186537)) ;
#97314 = DIRECTION('center_axis',(0.,0.,-1.)) ;
#97315 = DIRECTION('ref_axis',(-1.,0.,0.)) ;
#97316 = DIRECTION('center_axis',(0.,0.,1.)) ;
#97317 = DIRECTION('ref_axis',(-1.,1.57209315010398E-14,0.)) ;
#97318 = DIRECTION('center_axis',(0.,0.,-1.)) ;
#97319 = DIRECTION('ref_axis',(-1.,0.,0.)) ;
#97320 = DIRECTION('center_axis',(0.,1.,0.)) ;
#97321 = DIRECTION('ref_axis',(1.,0.,0.)) ;
#97322 = DIRECTION('center_axis',(0.,-1.,7.76229792195976E-15)) ;
#97323 = DIRECTION('ref_axis',(3.46944695195364E-14,7.76229792195976E-15,
1.)) ;
#97324 = DIRECTION('center_axis',(-3.46944695195361E-14,3.46944695195361E-14,
1.)) ;
#97325 = DIRECTION('ref_axis',(-7.17464813734306E-43,1.,-3.46944695195361E-14)) ;
#97326 = DIRECTION('center_axis',(0.577350269189625,-0.577350269189626,-0.577350269189626)) ;
#97327 = DIRECTION('ref_axis',(5.20172641667636E-15,0.70710678118655,-0.707106781186545)) ;
#97328 = DIRECTION('center_axis',(0.577350269189625,-0.577350269189626,-0.577350269189626)) ;
#97329 = DIRECTION('ref_axis',(5.11416588733871E-15,0.70710678118655,-0.707106781186545)) ;
#97330 = DIRECTION('center_axis',(0.577350269189624,-0.577350269189625,-0.577350269189629)) ;
#97331 = DIRECTION('ref_axis',(4.29556475679742E-15,0.707106781186552,-0.707106781186543)) ;
#97332 = DIRECTION('center_axis',(0.,0.,-1.)) ;
#97333 = DIRECTION('ref_axis',(-1.,0.,0.)) ;
#97334 = DIRECTION('center_axis',(0.,0.,1.)) ;
#97335 = DIRECTION('ref_axis',(1.,0.,0.)) ;
#97336 = DIRECTION('center_axis',(0.,1.,1.95511867169518E-16)) ;
#97337 = DIRECTION('ref_axis',(0.,-1.95511867169518E-16,1.)) ;
#97338 = DIRECTION('center_axis',(-7.65717784317885E-15,-1.,-7.84883952026447E-15)) ;
#97339 = DIRECTION('ref_axis',(-8.90241127119925E-32,7.84883952026447E-15,
-1.)) ;
#97340 = DIRECTION('center_axis',(0.,1.,0.)) ;
#97341 = DIRECTION('ref_axis',(1.,0.,0.)) ;
#97342 = DIRECTION('center_axis',(-1.28749007982652E-15,-1.,1.47915175691198E-15)) ;
#97343 = DIRECTION('ref_axis',(3.46944695195364E-14,1.47915175691194E-15,
1.)) ;
#97344 = DIRECTION('center_axis',(0.,1.,0.)) ;
#97345 = DIRECTION('ref_axis',(1.,0.,0.)) ;
#97346 = DIRECTION('center_axis',(-0.577350269189619,-0.577350269189621,-0.577350269189638)) ;
#97347 = DIRECTION('ref_axis',(1.66660234080318E-14,-0.707106781186566,0.707106781186529)) ;
#97348 = DIRECTION('center_axis',(0.,0.,1.)) ;
#97349 = DIRECTION('ref_axis',(-1.,-3.52365706057788E-15,0.)) ;
#97350 = DIRECTION('center_axis',(0.,1.,-1.95511867169518E-16)) ;
#97351 = DIRECTION('ref_axis',(0.,1.95511867169518E-16,1.)) ;
#97352 = DIRECTION('center_axis',(0.,-1.,3.06658683336682E-15)) ;
#97353 = DIRECTION('ref_axis',(0.,-3.06658683336682E-15,-1.)) ;
#97354 = DIRECTION('center_axis',(0.,0.,-1.)) ;
#97355 = DIRECTION('ref_axis',(-1.,0.,0.)) ;
#97356 = DIRECTION('center_axis',(-3.4694469519536E-14,-3.46944695195361E-14,
1.)) ;
#97357 = DIRECTION('ref_axis',(-8.96831017167883E-43,-1.,-3.46944695195361E-14)) ;
#97358 = DIRECTION('center_axis',(0.577350269189625,0.577350269189626,0.577350269189627)) ;
#97359 = DIRECTION('ref_axis',(5.35231302451417E-15,-0.707106781186551,0.707106781186544)) ;
#97360 = DIRECTION('center_axis',(0.577350269189625,0.577350269189626,0.577350269189627)) ;
#97361 = DIRECTION('ref_axis',(5.35231302451417E-15,-0.707106781186551,0.707106781186544)) ;
#97362 = DIRECTION('center_axis',(0.,1.,0.)) ;
#97363 = DIRECTION('ref_axis',(1.,0.,0.)) ;
#97364 = DIRECTION('center_axis',(-0.577350269189609,-0.577350269189646,0.577350269189623)) ;
#97365 = DIRECTION('ref_axis',(8.91337114590872E-15,0.707106781186529,0.707106781186566)) ;
#97366 = DIRECTION('center_axis',(0.,0.,-1.)) ;
#97367 = DIRECTION('ref_axis',(-1.,0.,0.)) ;
#97368 = DIRECTION('center_axis',(0.,0.,1.)) ;
#97369 = DIRECTION('ref_axis',(-1.,1.0842021724855E-15,0.)) ;
#97370 = DIRECTION('center_axis',(0.,0.,-1.)) ;
#97371 = DIRECTION('ref_axis',(-1.,0.,0.)) ;
#97372 = DIRECTION('center_axis',(-0.577350269189625,-0.577350269189626,0.577350269189627)) ;
#97373 = DIRECTION('ref_axis',(5.35231302451417E-15,-0.707106781186551,-0.707106781186544)) ;
#97374 = DIRECTION('center_axis',(0.577350269189625,0.577350269189626,-0.577350269189627)) ;
#97375 = DIRECTION('ref_axis',(-6.40836823623517E-14,-0.707106781186516,-0.707106781186579)) ;
#97376 = DIRECTION('center_axis',(0.577350269189625,0.577350269189625,-0.577350269189628)) ;
#97377 = DIRECTION('ref_axis',(-0.707106781186552,5.19478420936363E-15,-0.707106781186543)) ;
#97378 = DIRECTION('center_axis',(-0.577350269189625,-0.577350269189625,0.577350269189628)) ;
#97379 = DIRECTION('ref_axis',(-0.707106781186566,3.31891725521342E-14,-0.707106781186529)) ;
#97380 = DIRECTION('center_axis',(-0.577350269189652,-0.577350269189606,0.57735026918962)) ;
#97381 = DIRECTION('ref_axis',(0.707106781186528,-3.96520952299298E-16,0.707106781186567)) ;
#97382 = DIRECTION('center_axis',(0.,0.,-1.)) ;
#97383 = DIRECTION('ref_axis',(-1.,0.,0.)) ;
#97384 = DIRECTION('center_axis',(0.,0.,1.)) ;
#97385 = DIRECTION('ref_axis',(-1.,-8.67361737988404E-15,0.)) ;
#97386 = DIRECTION('center_axis',(0.,0.,-1.)) ;
#97387 = DIRECTION('ref_axis',(-1.,0.,0.)) ;
#97388 = DIRECTION('center_axis',(2.08166817117218E-16,1.,0.)) ;
#97389 = DIRECTION('ref_axis',(1.,0.,0.)) ;
#97390 = DIRECTION('center_axis',(-1.,0.,-1.66745659064321E-14)) ;
#97391 = DIRECTION('ref_axis',(1.66745659064321E-14,2.60208521396523E-14,
-1.)) ;
#97392 = DIRECTION('center_axis',(-3.46944695195361E-14,-3.4694469519536E-14,
1.)) ;
#97393 = DIRECTION('ref_axis',(-1.,-1.68611237719883E-42,-3.46944695195361E-14)) ;
#97394 = DIRECTION('center_axis',(-0.577350269189625,-0.577350269189625,-0.577350269189628)) ;
#97395 = DIRECTION('ref_axis',(-0.707106781186552,5.19478420936363E-15,0.707106781186543)) ;
#97396 = DIRECTION('center_axis',(-0.577350269189625,-0.577350269189625,-0.577350269189628)) ;
#97397 = DIRECTION('ref_axis',(-0.707106781186552,5.1349792556416E-15,0.707106781186543)) ;
#97398 = DIRECTION('center_axis',(-0.577350269189626,-0.577350269189626,-0.577350269189626)) ;
#97399 = DIRECTION('ref_axis',(0.707106781186547,-0.707106781186548,6.36902276417946E-16)) ;
#97400 = DIRECTION('center_axis',(0.,0.,-1.)) ;
#97401 = DIRECTION('ref_axis',(-1.,0.,0.)) ;
#97402 = DIRECTION('center_axis',(0.,0.,1.)) ;
#97403 = DIRECTION('ref_axis',(1.,0.,0.)) ;
#97404 = DIRECTION('center_axis',(-1.,0.,9.8563833862319E-18)) ;
#97405 = DIRECTION('ref_axis',(9.8563833862319E-18,0.,1.)) ;
#97406 = DIRECTION('center_axis',(-1.,8.87690528722497E-15,-8.87690528722518E-15)) ;
#97407 = DIRECTION('ref_axis',(-8.87690528722518E-15,4.48415508583942E-43,
1.)) ;
#97408 = DIRECTION('center_axis',(2.08166817117218E-16,1.,0.)) ;
#97409 = DIRECTION('ref_axis',(1.,0.,0.)) ;
#97410 = DIRECTION('center_axis',(-1.,8.53809210832325E-15,8.53809210832346E-15)) ;
#97411 = DIRECTION('ref_axis',(-8.53809210832339E-15,8.67361737988409E-15,
-1.)) ;
#97412 = DIRECTION('center_axis',(2.08166817117218E-16,1.,0.)) ;
#97413 = DIRECTION('ref_axis',(1.,0.,0.)) ;
#97414 = DIRECTION('center_axis',(-0.577350269189622,0.577350269189621,-0.577350269189634)) ;
#97415 = DIRECTION('ref_axis',(0.707106781186563,1.66970714627838E-14,-0.707106781186532)) ;
#97416 = DIRECTION('center_axis',(0.,0.,1.)) ;
#97417 = DIRECTION('ref_axis',(-1.,0.,0.)) ;
#97418 = DIRECTION('center_axis',(-1.,0.,-9.8563833862319E-18)) ;
#97419 = DIRECTION('ref_axis',(-9.8563833862319E-18,0.,1.)) ;
#97420 = DIRECTION('center_axis',(-1.,0.,-1.34163173959798E-15)) ;
#97421 = DIRECTION('ref_axis',(-1.34163173959798E-15,0.,1.)) ;
#97422 = DIRECTION('center_axis',(0.,0.,-1.)) ;
#97423 = DIRECTION('ref_axis',(-1.,0.,0.)) ;
#97424 = DIRECTION('center_axis',(-3.46944695195361E-14,3.4694469519536E-14,
1.)) ;
#97425 = DIRECTION('ref_axis',(1.,-1.68611237719883E-42,3.46944695195361E-14)) ;
#97426 = DIRECTION('center_axis',(0.577350269189625,-0.577350269189625,0.577350269189628)) ;
#97427 = DIRECTION('ref_axis',(0.707106781186552,5.19478420936363E-15,-0.707106781186543)) ;
#97428 = DIRECTION('center_axis',(0.577350269189625,-0.577350269189625,0.577350269189628)) ;
#97429 = DIRECTION('ref_axis',(0.707106781186552,5.1349792556416E-15,-0.707106781186543)) ;
#97430 = DIRECTION('center_axis',(2.08166817117218E-16,1.,0.)) ;
#97431 = DIRECTION('ref_axis',(1.,0.,0.)) ;
#97432 = DIRECTION('center_axis',(-0.577350269189646,0.577350269189609,0.577350269189623)) ;
#97433 = DIRECTION('ref_axis',(-0.707106781186529,8.66006384940495E-15,-0.707106781186566)) ;
#97434 = DIRECTION('center_axis',(0.,0.,-1.)) ;
#97435 = DIRECTION('ref_axis',(-1.,0.,0.)) ;
#97436 = DIRECTION('center_axis',(0.,0.,1.)) ;
#97437 = DIRECTION('ref_axis',(-1.,0.,0.)) ;
#97438 = DIRECTION('center_axis',(0.,0.,-1.)) ;
#97439 = DIRECTION('ref_axis',(-1.,0.,0.)) ;
#97440 = DIRECTION('center_axis',(-0.577350269189625,0.577350269189625,0.577350269189628)) ;
#97441 = DIRECTION('ref_axis',(0.707106781186552,5.1349792556416E-15,0.707106781186543)) ;
#97442 = DIRECTION('center_axis',(0.577350269189625,-0.577350269189625,-0.577350269189628)) ;
#97443 = DIRECTION('ref_axis',(0.707106781186559,1.92955635991398E-14,0.707106781186536)) ;
#97444 = DIRECTION('center_axis',(-0.577350269189625,0.577350269189626,-0.577350269189626)) ;
#97445 = DIRECTION('ref_axis',(5.20172641667636E-15,0.70710678118655,0.707106781186545)) ;
#97446 = DIRECTION('center_axis',(0.577350269189625,-0.577350269189626,0.577350269189626)) ;
#97447 = DIRECTION('ref_axis',(1.27903606950626E-14,0.707106781186554,0.707106781186541)) ;
#97448 = DIRECTION('center_axis',(0.577350269189636,-0.577350269189592,0.57735026918965)) ;
#97449 = DIRECTION('ref_axis',(0.707106781186558,3.40611850366138E-15,-0.707106781186537)) ;
#97450 = DIRECTION('center_axis',(0.,0.,-1.)) ;
#97451 = DIRECTION('ref_axis',(-1.,0.,0.)) ;
#97452 = DIRECTION('center_axis',(0.,0.,1.)) ;
#97453 = DIRECTION('ref_axis',(-1.,1.57209315010398E-14,0.)) ;
#97454 = DIRECTION('center_axis',(0.,0.,-1.)) ;
#97455 = DIRECTION('ref_axis',(-1.,0.,0.)) ;
#97456 = DIRECTION('center_axis',(0.,1.,0.)) ;
#97457 = DIRECTION('ref_axis',(1.,0.,0.)) ;
#97458 = DIRECTION('center_axis',(0.,-1.,7.76229792195976E-15)) ;
#97459 = DIRECTION('ref_axis',(3.46944695195364E-14,7.76229792195976E-15,
1.)) ;
#97460 = DIRECTION('center_axis',(-3.46944695195361E-14,3.46944695195361E-14,
1.)) ;
#97461 = DIRECTION('ref_axis',(-7.17464813734306E-43,1.,-3.46944695195361E-14)) ;
#97462 = DIRECTION('center_axis',(0.577350269189625,-0.577350269189626,-0.577350269189626)) ;
#97463 = DIRECTION('ref_axis',(5.20172641667636E-15,0.70710678118655,-0.707106781186545)) ;
#97464 = DIRECTION('center_axis',(0.577350269189625,-0.577350269189626,-0.577350269189626)) ;
#97465 = DIRECTION('ref_axis',(5.11416588733871E-15,0.70710678118655,-0.707106781186545)) ;
#97466 = DIRECTION('center_axis',(0.577350269189624,-0.577350269189625,-0.577350269189629)) ;
#97467 = DIRECTION('ref_axis',(4.29556475679742E-15,0.707106781186552,-0.707106781186543)) ;
#97468 = DIRECTION('center_axis',(0.,0.,-1.)) ;
#97469 = DIRECTION('ref_axis',(-1.,0.,0.)) ;
#97470 = DIRECTION('center_axis',(0.,0.,1.)) ;
#97471 = DIRECTION('ref_axis',(1.,0.,0.)) ;
#97472 = DIRECTION('center_axis',(0.,1.,1.95511867169518E-16)) ;
#97473 = DIRECTION('ref_axis',(0.,-1.95511867169518E-16,1.)) ;
#97474 = DIRECTION('center_axis',(-7.65717784317885E-15,-1.,-7.84883952026447E-15)) ;
#97475 = DIRECTION('ref_axis',(-8.90241127119925E-32,7.84883952026447E-15,
-1.)) ;
#97476 = DIRECTION('center_axis',(0.,1.,0.)) ;
#97477 = DIRECTION('ref_axis',(1.,0.,0.)) ;
#97478 = DIRECTION('center_axis',(-1.28749007982652E-15,-1.,1.47915175691198E-15)) ;
#97479 = DIRECTION('ref_axis',(3.46944695195364E-14,1.47915175691194E-15,
1.)) ;
#97480 = DIRECTION('center_axis',(0.,1.,0.)) ;
#97481 = DIRECTION('ref_axis',(1.,0.,0.)) ;
#97482 = DIRECTION('center_axis',(-0.577350269189619,-0.577350269189621,-0.577350269189638)) ;
#97483 = DIRECTION('ref_axis',(1.66660234080318E-14,-0.707106781186566,0.707106781186529)) ;
#97484 = DIRECTION('center_axis',(0.,0.,1.)) ;
#97485 = DIRECTION('ref_axis',(-1.,-3.52365706057788E-15,0.)) ;
#97486 = DIRECTION('center_axis',(0.,1.,-1.95511867169518E-16)) ;
#97487 = DIRECTION('ref_axis',(0.,1.95511867169518E-16,1.)) ;
#97488 = DIRECTION('center_axis',(0.,-1.,3.06658683336682E-15)) ;
#97489 = DIRECTION('ref_axis',(0.,-3.06658683336682E-15,-1.)) ;
#97490 = DIRECTION('center_axis',(0.,0.,-1.)) ;
#97491 = DIRECTION('ref_axis',(-1.,0.,0.)) ;
#97492 = DIRECTION('center_axis',(-3.4694469519536E-14,-3.46944695195361E-14,
1.)) ;
#97493 = DIRECTION('ref_axis',(-8.96831017167883E-43,-1.,-3.46944695195361E-14)) ;
#97494 = DIRECTION('center_axis',(0.577350269189625,0.577350269189626,0.577350269189627)) ;
#97495 = DIRECTION('ref_axis',(5.35231302451417E-15,-0.707106781186551,0.707106781186544)) ;
#97496 = DIRECTION('center_axis',(0.577350269189625,0.577350269189626,0.577350269189627)) ;
#97497 = DIRECTION('ref_axis',(5.35231302451417E-15,-0.707106781186551,0.707106781186544)) ;
#97498 = DIRECTION('center_axis',(0.,1.,0.)) ;
#97499 = DIRECTION('ref_axis',(1.,0.,0.)) ;
#97500 = DIRECTION('center_axis',(-0.577350269189609,-0.577350269189646,0.577350269189623)) ;
#97501 = DIRECTION('ref_axis',(8.91337114590872E-15,0.707106781186529,0.707106781186566)) ;
#97502 = DIRECTION('center_axis',(0.,0.,-1.)) ;
#97503 = DIRECTION('ref_axis',(-1.,0.,0.)) ;
#97504 = DIRECTION('center_axis',(0.,0.,1.)) ;
#97505 = DIRECTION('ref_axis',(-1.,1.0842021724855E-15,0.)) ;
#97506 = DIRECTION('center_axis',(0.,0.,-1.)) ;
#97507 = DIRECTION('ref_axis',(-1.,0.,0.)) ;
#97508 = DIRECTION('center_axis',(-0.577350269189625,-0.577350269189626,0.577350269189627)) ;
#97509 = DIRECTION('ref_axis',(5.35231302451417E-15,-0.707106781186551,-0.707106781186544)) ;
#97510 = DIRECTION('center_axis',(0.577350269189625,0.577350269189626,-0.577350269189627)) ;
#97511 = DIRECTION('ref_axis',(-6.40836823623517E-14,-0.707106781186516,-0.707106781186579)) ;
#97512 = DIRECTION('center_axis',(0.577350269189625,0.577350269189625,-0.577350269189628)) ;
#97513 = DIRECTION('ref_axis',(-0.707106781186552,5.19478420936363E-15,-0.707106781186543)) ;
#97514 = DIRECTION('center_axis',(-0.577350269189625,-0.577350269189625,0.577350269189628)) ;
#97515 = DIRECTION('ref_axis',(-0.707106781186566,3.31891725521342E-14,-0.707106781186529)) ;
#97516 = DIRECTION('center_axis',(-0.577350269189652,-0.577350269189606,0.57735026918962)) ;
#97517 = DIRECTION('ref_axis',(0.707106781186528,-3.96520952299298E-16,0.707106781186567)) ;
#97518 = DIRECTION('center_axis',(0.,0.,-1.)) ;
#97519 = DIRECTION('ref_axis',(-1.,0.,0.)) ;
#97520 = DIRECTION('center_axis',(0.,0.,1.)) ;
#97521 = DIRECTION('ref_axis',(-1.,-8.67361737988404E-15,0.)) ;
#97522 = DIRECTION('center_axis',(0.,0.,-1.)) ;
#97523 = DIRECTION('ref_axis',(-1.,0.,0.)) ;
#97524 = DIRECTION('center_axis',(2.08166817117218E-16,1.,0.)) ;
#97525 = DIRECTION('ref_axis',(1.,0.,0.)) ;
#97526 = DIRECTION('center_axis',(-1.,0.,-1.66745659064321E-14)) ;
#97527 = DIRECTION('ref_axis',(1.66745659064321E-14,2.60208521396523E-14,
-1.)) ;
#97528 = DIRECTION('center_axis',(-3.46944695195361E-14,-3.4694469519536E-14,
1.)) ;
#97529 = DIRECTION('ref_axis',(-1.,-1.68611237719883E-42,-3.46944695195361E-14)) ;
#97530 = DIRECTION('center_axis',(-0.577350269189625,-0.577350269189625,-0.577350269189628)) ;
#97531 = DIRECTION('ref_axis',(-0.707106781186552,5.19478420936363E-15,0.707106781186543)) ;
#97532 = DIRECTION('center_axis',(-0.577350269189625,-0.577350269189625,-0.577350269189628)) ;
#97533 = DIRECTION('ref_axis',(-0.707106781186552,5.1349792556416E-15,0.707106781186543)) ;
#97534 = DIRECTION('center_axis',(-0.577350269189626,-0.577350269189626,-0.577350269189626)) ;
#97535 = DIRECTION('ref_axis',(0.707106781186547,-0.707106781186548,6.36902276417946E-16)) ;
#97536 = DIRECTION('center_axis',(0.,0.,-1.)) ;
#97537 = DIRECTION('ref_axis',(-1.,0.,0.)) ;
#97538 = DIRECTION('center_axis',(0.,0.,1.)) ;
#97539 = DIRECTION('ref_axis',(1.,0.,0.)) ;
#97540 = DIRECTION('center_axis',(-1.,0.,9.8563833862319E-18)) ;
#97541 = DIRECTION('ref_axis',(9.8563833862319E-18,0.,1.)) ;
#97542 = DIRECTION('center_axis',(-1.,8.87690528722497E-15,-8.87690528722518E-15)) ;
#97543 = DIRECTION('ref_axis',(-8.87690528722518E-15,4.48415508583942E-43,
1.)) ;
#97544 = DIRECTION('center_axis',(2.08166817117218E-16,1.,0.)) ;
#97545 = DIRECTION('ref_axis',(1.,0.,0.)) ;
#97546 = DIRECTION('center_axis',(-1.,8.53809210832325E-15,8.53809210832346E-15)) ;
#97547 = DIRECTION('ref_axis',(-8.53809210832339E-15,8.67361737988409E-15,
-1.)) ;
#97548 = DIRECTION('center_axis',(2.08166817117218E-16,1.,0.)) ;
#97549 = DIRECTION('ref_axis',(1.,0.,0.)) ;
#97550 = DIRECTION('center_axis',(-0.577350269189622,0.577350269189621,-0.577350269189634)) ;
#97551 = DIRECTION('ref_axis',(0.707106781186563,1.66970714627838E-14,-0.707106781186532)) ;
#97552 = DIRECTION('center_axis',(0.,0.,1.)) ;
#97553 = DIRECTION('ref_axis',(-1.,0.,0.)) ;
#97554 = DIRECTION('center_axis',(-1.,0.,-9.8563833862319E-18)) ;
#97555 = DIRECTION('ref_axis',(-9.8563833862319E-18,0.,1.)) ;
#97556 = DIRECTION('center_axis',(-1.,0.,-1.34163173959798E-15)) ;
#97557 = DIRECTION('ref_axis',(-1.34163173959798E-15,0.,1.)) ;
#97558 = DIRECTION('center_axis',(0.,0.,-1.)) ;
#97559 = DIRECTION('ref_axis',(-1.,0.,0.)) ;
#97560 = DIRECTION('center_axis',(-3.46944695195361E-14,3.4694469519536E-14,
1.)) ;
#97561 = DIRECTION('ref_axis',(1.,-1.68611237719883E-42,3.46944695195361E-14)) ;
#97562 = DIRECTION('center_axis',(0.577350269189625,-0.577350269189625,0.577350269189628)) ;
#97563 = DIRECTION('ref_axis',(0.707106781186552,5.19478420936363E-15,-0.707106781186543)) ;
#97564 = DIRECTION('center_axis',(0.577350269189625,-0.577350269189625,0.577350269189628)) ;
#97565 = DIRECTION('ref_axis',(0.707106781186552,5.1349792556416E-15,-0.707106781186543)) ;
#97566 = DIRECTION('center_axis',(2.08166817117218E-16,1.,0.)) ;
#97567 = DIRECTION('ref_axis',(1.,0.,0.)) ;
#97568 = DIRECTION('center_axis',(-0.577350269189646,0.577350269189609,0.577350269189623)) ;
#97569 = DIRECTION('ref_axis',(-0.707106781186529,8.66006384940495E-15,-0.707106781186566)) ;
#97570 = DIRECTION('center_axis',(0.,0.,-1.)) ;
#97571 = DIRECTION('ref_axis',(-1.,0.,0.)) ;
#97572 = DIRECTION('center_axis',(0.,0.,1.)) ;
#97573 = DIRECTION('ref_axis',(-1.,0.,0.)) ;
#97574 = DIRECTION('center_axis',(0.,0.,-1.)) ;
#97575 = DIRECTION('ref_axis',(-1.,0.,0.)) ;
#97576 = DIRECTION('center_axis',(-0.577350269189625,0.577350269189625,0.577350269189628)) ;
#97577 = DIRECTION('ref_axis',(0.707106781186552,5.1349792556416E-15,0.707106781186543)) ;
#97578 = DIRECTION('center_axis',(0.577350269189625,-0.577350269189625,-0.577350269189628)) ;
#97579 = DIRECTION('ref_axis',(0.707106781186559,1.92955635991398E-14,0.707106781186536)) ;
#97580 = DIRECTION('center_axis',(-0.577350269189625,0.577350269189626,-0.577350269189626)) ;
#97581 = DIRECTION('ref_axis',(5.20172641667636E-15,0.70710678118655,0.707106781186545)) ;
#97582 = DIRECTION('center_axis',(0.577350269189625,-0.577350269189626,0.577350269189626)) ;
#97583 = DIRECTION('ref_axis',(1.27903606950626E-14,0.707106781186554,0.707106781186541)) ;
#97584 = DIRECTION('center_axis',(0.577350269189636,-0.577350269189592,0.57735026918965)) ;
#97585 = DIRECTION('ref_axis',(0.707106781186558,3.40611850366138E-15,-0.707106781186537)) ;
#97586 = DIRECTION('center_axis',(0.,0.,-1.)) ;
#97587 = DIRECTION('ref_axis',(-1.,0.,0.)) ;
#97588 = DIRECTION('center_axis',(0.,0.,1.)) ;
#97589 = DIRECTION('ref_axis',(-1.,1.57209315010398E-14,0.)) ;
#97590 = DIRECTION('center_axis',(0.,0.,-1.)) ;
#97591 = DIRECTION('ref_axis',(-1.,0.,0.)) ;
#97592 = DIRECTION('center_axis',(0.,1.,0.)) ;
#97593 = DIRECTION('ref_axis',(1.,0.,0.)) ;
#97594 = DIRECTION('center_axis',(0.,-1.,7.76229792195976E-15)) ;
#97595 = DIRECTION('ref_axis',(3.46944695195364E-14,7.76229792195976E-15,
1.)) ;
#97596 = DIRECTION('center_axis',(-3.46944695195361E-14,3.46944695195361E-14,
1.)) ;
#97597 = DIRECTION('ref_axis',(-7.17464813734306E-43,1.,-3.46944695195361E-14)) ;
#97598 = DIRECTION('center_axis',(0.577350269189625,-0.577350269189626,-0.577350269189626)) ;
#97599 = DIRECTION('ref_axis',(5.20172641667636E-15,0.70710678118655,-0.707106781186545)) ;
#97600 = DIRECTION('center_axis',(0.577350269189625,-0.577350269189626,-0.577350269189626)) ;
#97601 = DIRECTION('ref_axis',(5.11416588733871E-15,0.70710678118655,-0.707106781186545)) ;
#97602 = DIRECTION('center_axis',(0.577350269189624,-0.577350269189625,-0.577350269189629)) ;
#97603 = DIRECTION('ref_axis',(4.29556475679742E-15,0.707106781186552,-0.707106781186543)) ;
#97604 = DIRECTION('center_axis',(0.,0.,-1.)) ;
#97605 = DIRECTION('ref_axis',(-1.,0.,0.)) ;
#97606 = DIRECTION('center_axis',(0.,0.,1.)) ;
#97607 = DIRECTION('ref_axis',(1.,0.,0.)) ;
#97608 = DIRECTION('center_axis',(0.,1.,1.95511867169518E-16)) ;
#97609 = DIRECTION('ref_axis',(0.,-1.95511867169518E-16,1.)) ;
#97610 = DIRECTION('center_axis',(-7.65717784317885E-15,-1.,-7.84883952026447E-15)) ;
#97611 = DIRECTION('ref_axis',(-8.90241127119925E-32,7.84883952026447E-15,
-1.)) ;
#97612 = DIRECTION('center_axis',(0.,1.,0.)) ;
#97613 = DIRECTION('ref_axis',(1.,0.,0.)) ;
#97614 = DIRECTION('center_axis',(-1.28749007982652E-15,-1.,1.47915175691198E-15)) ;
#97615 = DIRECTION('ref_axis',(3.46944695195364E-14,1.47915175691194E-15,
1.)) ;
#97616 = DIRECTION('center_axis',(0.,1.,0.)) ;
#97617 = DIRECTION('ref_axis',(1.,0.,0.)) ;
#97618 = DIRECTION('center_axis',(-0.577350269189619,-0.577350269189621,-0.577350269189638)) ;
#97619 = DIRECTION('ref_axis',(1.66660234080318E-14,-0.707106781186566,0.707106781186529)) ;
#97620 = DIRECTION('center_axis',(0.,0.,1.)) ;
#97621 = DIRECTION('ref_axis',(-1.,-3.52365706057788E-15,0.)) ;
#97622 = DIRECTION('center_axis',(0.,1.,-1.95511867169518E-16)) ;
#97623 = DIRECTION('ref_axis',(0.,1.95511867169518E-16,1.)) ;
#97624 = DIRECTION('center_axis',(0.,-1.,3.06658683336682E-15)) ;
#97625 = DIRECTION('ref_axis',(0.,-3.06658683336682E-15,-1.)) ;
#97626 = DIRECTION('center_axis',(0.,0.,-1.)) ;
#97627 = DIRECTION('ref_axis',(-1.,0.,0.)) ;
#97628 = DIRECTION('center_axis',(-3.4694469519536E-14,-3.46944695195361E-14,
1.)) ;
#97629 = DIRECTION('ref_axis',(-8.96831017167883E-43,-1.,-3.46944695195361E-14)) ;
#97630 = DIRECTION('center_axis',(0.577350269189625,0.577350269189626,0.577350269189627)) ;
#97631 = DIRECTION('ref_axis',(5.35231302451417E-15,-0.707106781186551,0.707106781186544)) ;
#97632 = DIRECTION('center_axis',(0.577350269189625,0.577350269189626,0.577350269189627)) ;
#97633 = DIRECTION('ref_axis',(5.35231302451417E-15,-0.707106781186551,0.707106781186544)) ;
#97634 = DIRECTION('center_axis',(0.,1.,0.)) ;
#97635 = DIRECTION('ref_axis',(1.,0.,0.)) ;
#97636 = DIRECTION('center_axis',(-0.577350269189609,-0.577350269189646,0.577350269189623)) ;
#97637 = DIRECTION('ref_axis',(8.91337114590872E-15,0.707106781186529,0.707106781186566)) ;
#97638 = DIRECTION('center_axis',(0.,0.,-1.)) ;
#97639 = DIRECTION('ref_axis',(-1.,0.,0.)) ;
#97640 = DIRECTION('center_axis',(0.,0.,1.)) ;
#97641 = DIRECTION('ref_axis',(-1.,1.0842021724855E-15,0.)) ;
#97642 = DIRECTION('center_axis',(0.,0.,-1.)) ;
#97643 = DIRECTION('ref_axis',(-1.,0.,0.)) ;
#97644 = DIRECTION('center_axis',(-0.577350269189625,-0.577350269189626,0.577350269189627)) ;
#97645 = DIRECTION('ref_axis',(5.35231302451417E-15,-0.707106781186551,-0.707106781186544)) ;
#97646 = DIRECTION('center_axis',(0.577350269189625,0.577350269189626,-0.577350269189627)) ;
#97647 = DIRECTION('ref_axis',(-6.40836823623517E-14,-0.707106781186516,-0.707106781186579)) ;
#97648 = DIRECTION('center_axis',(0.577350269189625,0.577350269189625,-0.577350269189628)) ;
#97649 = DIRECTION('ref_axis',(-0.707106781186552,5.19478420936363E-15,-0.707106781186543)) ;
#97650 = DIRECTION('center_axis',(-0.577350269189625,-0.577350269189625,0.577350269189628)) ;
#97651 = DIRECTION('ref_axis',(-0.707106781186566,3.31891725521342E-14,-0.707106781186529)) ;
#97652 = DIRECTION('center_axis',(-0.577350269189652,-0.577350269189606,0.57735026918962)) ;
#97653 = DIRECTION('ref_axis',(0.707106781186528,-3.96520952299298E-16,0.707106781186567)) ;
#97654 = DIRECTION('center_axis',(0.,0.,-1.)) ;
#97655 = DIRECTION('ref_axis',(-1.,0.,0.)) ;
#97656 = DIRECTION('center_axis',(0.,0.,1.)) ;
#97657 = DIRECTION('ref_axis',(-1.,-8.67361737988404E-15,0.)) ;
#97658 = DIRECTION('center_axis',(0.,0.,-1.)) ;
#97659 = DIRECTION('ref_axis',(-1.,0.,0.)) ;
#97660 = DIRECTION('center_axis',(2.08166817117218E-16,1.,0.)) ;
#97661 = DIRECTION('ref_axis',(1.,0.,0.)) ;
#97662 = DIRECTION('center_axis',(-1.,0.,-1.66745659064321E-14)) ;
#97663 = DIRECTION('ref_axis',(1.66745659064321E-14,2.60208521396523E-14,
-1.)) ;
#97664 = DIRECTION('center_axis',(-3.46944695195361E-14,-3.4694469519536E-14,
1.)) ;
#97665 = DIRECTION('ref_axis',(-1.,-1.68611237719883E-42,-3.46944695195361E-14)) ;
#97666 = DIRECTION('center_axis',(-0.577350269189625,-0.577350269189625,-0.577350269189628)) ;
#97667 = DIRECTION('ref_axis',(-0.707106781186552,5.19478420936363E-15,0.707106781186543)) ;
#97668 = DIRECTION('center_axis',(-0.577350269189625,-0.577350269189625,-0.577350269189628)) ;
#97669 = DIRECTION('ref_axis',(-0.707106781186552,5.1349792556416E-15,0.707106781186543)) ;
#97670 = DIRECTION('center_axis',(-0.577350269189626,-0.577350269189626,-0.577350269189626)) ;
#97671 = DIRECTION('ref_axis',(0.707106781186547,-0.707106781186548,6.36902276417946E-16)) ;
#97672 = DIRECTION('center_axis',(0.,0.,-1.)) ;
#97673 = DIRECTION('ref_axis',(-1.,0.,0.)) ;
#97674 = DIRECTION('center_axis',(0.,0.,1.)) ;
#97675 = DIRECTION('ref_axis',(1.,0.,0.)) ;
#97676 = DIRECTION('center_axis',(-1.,0.,9.8563833862319E-18)) ;
#97677 = DIRECTION('ref_axis',(9.8563833862319E-18,0.,1.)) ;
#97678 = DIRECTION('center_axis',(-1.,8.87690528722497E-15,-8.87690528722518E-15)) ;
#97679 = DIRECTION('ref_axis',(-8.87690528722518E-15,4.48415508583942E-43,
1.)) ;
#97680 = DIRECTION('center_axis',(2.08166817117218E-16,1.,0.)) ;
#97681 = DIRECTION('ref_axis',(1.,0.,0.)) ;
#97682 = DIRECTION('center_axis',(-1.,8.53809210832325E-15,8.53809210832346E-15)) ;
#97683 = DIRECTION('ref_axis',(-8.53809210832339E-15,8.67361737988409E-15,
-1.)) ;
#97684 = DIRECTION('center_axis',(2.08166817117218E-16,1.,0.)) ;
#97685 = DIRECTION('ref_axis',(1.,0.,0.)) ;
#97686 = DIRECTION('center_axis',(-0.577350269189622,0.577350269189621,-0.577350269189634)) ;
#97687 = DIRECTION('ref_axis',(0.707106781186563,1.66970714627838E-14,-0.707106781186532)) ;
#97688 = DIRECTION('center_axis',(0.,0.,1.)) ;
#97689 = DIRECTION('ref_axis',(-1.,0.,0.)) ;
#97690 = DIRECTION('center_axis',(-1.,0.,-9.8563833862319E-18)) ;
#97691 = DIRECTION('ref_axis',(-9.8563833862319E-18,0.,1.)) ;
#97692 = DIRECTION('center_axis',(-1.,0.,-1.34163173959798E-15)) ;
#97693 = DIRECTION('ref_axis',(-1.34163173959798E-15,0.,1.)) ;
#97694 = DIRECTION('center_axis',(0.,0.,-1.)) ;
#97695 = DIRECTION('ref_axis',(-1.,0.,0.)) ;
#97696 = DIRECTION('center_axis',(-3.46944695195361E-14,3.4694469519536E-14,
1.)) ;
#97697 = DIRECTION('ref_axis',(1.,-1.68611237719883E-42,3.46944695195361E-14)) ;
#97698 = DIRECTION('center_axis',(0.577350269189625,-0.577350269189625,0.577350269189628)) ;
#97699 = DIRECTION('ref_axis',(0.707106781186552,5.19478420936363E-15,-0.707106781186543)) ;
#97700 = DIRECTION('center_axis',(0.577350269189625,-0.577350269189625,0.577350269189628)) ;
#97701 = DIRECTION('ref_axis',(0.707106781186552,5.1349792556416E-15,-0.707106781186543)) ;
#97702 = DIRECTION('center_axis',(2.08166817117218E-16,1.,0.)) ;
#97703 = DIRECTION('ref_axis',(1.,0.,0.)) ;
#97704 = DIRECTION('center_axis',(-0.577350269189646,0.577350269189609,0.577350269189623)) ;
#97705 = DIRECTION('ref_axis',(-0.707106781186529,8.66006384940495E-15,-0.707106781186566)) ;
#97706 = DIRECTION('center_axis',(0.,0.,-1.)) ;
#97707 = DIRECTION('ref_axis',(-1.,0.,0.)) ;
#97708 = DIRECTION('center_axis',(0.,0.,1.)) ;
#97709 = DIRECTION('ref_axis',(-1.,0.,0.)) ;
#97710 = DIRECTION('center_axis',(0.,0.,-1.)) ;
#97711 = DIRECTION('ref_axis',(-1.,0.,0.)) ;
#97712 = DIRECTION('center_axis',(-0.577350269189625,0.577350269189625,0.577350269189628)) ;
#97713 = DIRECTION('ref_axis',(0.707106781186552,5.1349792556416E-15,0.707106781186543)) ;
#97714 = DIRECTION('center_axis',(0.577350269189625,-0.577350269189625,-0.577350269189628)) ;
#97715 = DIRECTION('ref_axis',(0.707106781186559,1.92955635991398E-14,0.707106781186536)) ;
#97716 = DIRECTION('center_axis',(-0.577350269189625,0.577350269189626,-0.577350269189626)) ;
#97717 = DIRECTION('ref_axis',(5.20172641667636E-15,0.70710678118655,0.707106781186545)) ;
#97718 = DIRECTION('center_axis',(0.577350269189625,-0.577350269189626,0.577350269189626)) ;
#97719 = DIRECTION('ref_axis',(1.27903606950626E-14,0.707106781186554,0.707106781186541)) ;
#97720 = DIRECTION('center_axis',(0.577350269189636,-0.577350269189592,0.57735026918965)) ;
#97721 = DIRECTION('ref_axis',(0.707106781186558,3.40611850366138E-15,-0.707106781186537)) ;
#97722 = DIRECTION('center_axis',(0.,0.,-1.)) ;
#97723 = DIRECTION('ref_axis',(-1.,0.,0.)) ;
#97724 = DIRECTION('center_axis',(0.,0.,1.)) ;
#97725 = DIRECTION('ref_axis',(-1.,1.57209315010398E-14,0.)) ;
#97726 = DIRECTION('center_axis',(0.,0.,-1.)) ;
#97727 = DIRECTION('ref_axis',(-1.,0.,0.)) ;
#97728 = DIRECTION('center_axis',(0.,1.,0.)) ;
#97729 = DIRECTION('ref_axis',(1.,0.,0.)) ;
#97730 = DIRECTION('center_axis',(0.,-1.,7.76229792195976E-15)) ;
#97731 = DIRECTION('ref_axis',(3.46944695195364E-14,7.76229792195976E-15,
1.)) ;
#97732 = DIRECTION('center_axis',(-3.46944695195361E-14,3.46944695195361E-14,
1.)) ;
#97733 = DIRECTION('ref_axis',(-7.17464813734306E-43,1.,-3.46944695195361E-14)) ;
#97734 = DIRECTION('center_axis',(0.577350269189625,-0.577350269189626,-0.577350269189626)) ;
#97735 = DIRECTION('ref_axis',(5.20172641667636E-15,0.70710678118655,-0.707106781186545)) ;
#97736 = DIRECTION('center_axis',(0.577350269189625,-0.577350269189626,-0.577350269189626)) ;
#97737 = DIRECTION('ref_axis',(5.11416588733871E-15,0.70710678118655,-0.707106781186545)) ;
#97738 = DIRECTION('center_axis',(0.577350269189624,-0.577350269189625,-0.577350269189629)) ;
#97739 = DIRECTION('ref_axis',(4.29556475679742E-15,0.707106781186552,-0.707106781186543)) ;
#97740 = DIRECTION('center_axis',(0.,0.,-1.)) ;
#97741 = DIRECTION('ref_axis',(-1.,0.,0.)) ;
#97742 = DIRECTION('center_axis',(0.,0.,1.)) ;
#97743 = DIRECTION('ref_axis',(1.,0.,0.)) ;
#97744 = DIRECTION('center_axis',(0.,1.,1.95511867169518E-16)) ;
#97745 = DIRECTION('ref_axis',(0.,-1.95511867169518E-16,1.)) ;
#97746 = DIRECTION('center_axis',(-7.65717784317885E-15,-1.,-7.84883952026447E-15)) ;
#97747 = DIRECTION('ref_axis',(-8.90241127119925E-32,7.84883952026447E-15,
-1.)) ;
#97748 = DIRECTION('center_axis',(0.,1.,0.)) ;
#97749 = DIRECTION('ref_axis',(1.,0.,0.)) ;
#97750 = DIRECTION('center_axis',(-1.28749007982652E-15,-1.,1.47915175691198E-15)) ;
#97751 = DIRECTION('ref_axis',(3.46944695195364E-14,1.47915175691194E-15,
1.)) ;
#97752 = DIRECTION('center_axis',(0.,1.,0.)) ;
#97753 = DIRECTION('ref_axis',(1.,0.,0.)) ;
#97754 = DIRECTION('center_axis',(-0.577350269189619,-0.577350269189621,-0.577350269189638)) ;
#97755 = DIRECTION('ref_axis',(1.66660234080318E-14,-0.707106781186566,0.707106781186529)) ;
#97756 = DIRECTION('center_axis',(0.,0.,1.)) ;
#97757 = DIRECTION('ref_axis',(-1.,-3.52365706057788E-15,0.)) ;
#97758 = DIRECTION('center_axis',(0.,1.,-1.95511867169518E-16)) ;
#97759 = DIRECTION('ref_axis',(0.,1.95511867169518E-16,1.)) ;
#97760 = DIRECTION('center_axis',(0.,-1.,3.06658683336682E-15)) ;
#97761 = DIRECTION('ref_axis',(0.,-3.06658683336682E-15,-1.)) ;
#97762 = DIRECTION('center_axis',(0.,0.,-1.)) ;
#97763 = DIRECTION('ref_axis',(-1.,0.,0.)) ;
#97764 = DIRECTION('center_axis',(-3.4694469519536E-14,-3.46944695195361E-14,
1.)) ;
#97765 = DIRECTION('ref_axis',(-8.96831017167883E-43,-1.,-3.46944695195361E-14)) ;
#97766 = DIRECTION('center_axis',(0.577350269189625,0.577350269189626,0.577350269189627)) ;
#97767 = DIRECTION('ref_axis',(5.35231302451417E-15,-0.707106781186551,0.707106781186544)) ;
#97768 = DIRECTION('center_axis',(0.577350269189625,0.577350269189626,0.577350269189627)) ;
#97769 = DIRECTION('ref_axis',(5.35231302451417E-15,-0.707106781186551,0.707106781186544)) ;
#97770 = DIRECTION('center_axis',(0.,1.,0.)) ;
#97771 = DIRECTION('ref_axis',(1.,0.,0.)) ;
#97772 = DIRECTION('center_axis',(-0.577350269189609,-0.577350269189646,0.577350269189623)) ;
#97773 = DIRECTION('ref_axis',(8.91337114590872E-15,0.707106781186529,0.707106781186566)) ;
#97774 = DIRECTION('center_axis',(0.,0.,-1.)) ;
#97775 = DIRECTION('ref_axis',(-1.,0.,0.)) ;
#97776 = DIRECTION('center_axis',(0.,0.,1.)) ;
#97777 = DIRECTION('ref_axis',(-1.,1.0842021724855E-15,0.)) ;
#97778 = DIRECTION('center_axis',(0.,0.,-1.)) ;
#97779 = DIRECTION('ref_axis',(-1.,0.,0.)) ;
#97780 = DIRECTION('center_axis',(-0.577350269189625,-0.577350269189626,0.577350269189627)) ;
#97781 = DIRECTION('ref_axis',(5.35231302451417E-15,-0.707106781186551,-0.707106781186544)) ;
#97782 = DIRECTION('center_axis',(0.577350269189625,0.577350269189626,-0.577350269189627)) ;
#97783 = DIRECTION('ref_axis',(-6.40836823623517E-14,-0.707106781186516,-0.707106781186579)) ;
#97784 = DIRECTION('center_axis',(0.577350269189625,0.577350269189625,-0.577350269189628)) ;
#97785 = DIRECTION('ref_axis',(-0.707106781186552,5.19478420936363E-15,-0.707106781186543)) ;
#97786 = DIRECTION('center_axis',(-0.577350269189625,-0.577350269189625,0.577350269189628)) ;
#97787 = DIRECTION('ref_axis',(-0.707106781186562,2.56048320762387E-14,-0.707106781186533)) ;
#97788 = DIRECTION('center_axis',(-0.577350269189542,-0.577350269189661,0.577350269189675)) ;
#97789 = DIRECTION('ref_axis',(3.44881489367205E-15,-0.707106781186558,-0.707106781186537)) ;
#97790 = DIRECTION('center_axis',(0.,0.,-1.)) ;
#97791 = DIRECTION('ref_axis',(-1.,0.,0.)) ;
#97792 = DIRECTION('center_axis',(0.,0.,1.)) ;
#97793 = DIRECTION('ref_axis',(-1.,-8.67361737988404E-15,0.)) ;
#97794 = DIRECTION('center_axis',(0.,0.,-1.)) ;
#97795 = DIRECTION('ref_axis',(-1.,0.,0.)) ;
#97796 = DIRECTION('center_axis',(2.08166817117218E-16,1.,0.)) ;
#97797 = DIRECTION('ref_axis',(1.,0.,0.)) ;
#97798 = DIRECTION('center_axis',(-1.,0.,9.05601424228639E-14)) ;
#97799 = DIRECTION('ref_axis',(-9.05601424228639E-14,0.,-1.)) ;
#97800 = DIRECTION('center_axis',(6.93889390390722E-14,6.93889390390721E-14,
1.)) ;
#97801 = DIRECTION('ref_axis',(-1.,-6.3534872372487E-42,6.93889390390722E-14)) ;
#97802 = DIRECTION('center_axis',(-0.577350269189625,-0.577350269189625,-0.577350269189628)) ;
#97803 = DIRECTION('ref_axis',(-0.707106781186552,5.19478420936363E-15,0.707106781186543)) ;
#97804 = DIRECTION('center_axis',(-0.577350269189625,-0.577350269189625,-0.577350269189628)) ;
#97805 = DIRECTION('ref_axis',(-0.707106781186552,5.1349792556416E-15,0.707106781186543)) ;
#97806 = DIRECTION('center_axis',(-0.577350269189609,-0.577350269189608,-0.57735026918966)) ;
#97807 = DIRECTION('ref_axis',(-0.707106781186576,-5.08171669240118E-15,0.707106781186519)) ;
#97808 = DIRECTION('center_axis',(0.,0.,-1.)) ;
#97809 = DIRECTION('ref_axis',(-1.,0.,0.)) ;
#97810 = DIRECTION('center_axis',(0.,0.,1.)) ;
#97811 = DIRECTION('ref_axis',(1.,0.,0.)) ;
#97812 = DIRECTION('center_axis',(-1.,0.,9.8563833862319E-18)) ;
#97813 = DIRECTION('ref_axis',(9.8563833862319E-18,0.,1.)) ;
#97814 = DIRECTION('center_axis',(-1.,1.31459513413869E-14,-1.31459513413873E-14)) ;
#97815 = DIRECTION('ref_axis',(-1.31459513413873E-14,1.17484863248993E-41,
1.)) ;
#97816 = DIRECTION('center_axis',(2.08166817117218E-16,1.,0.)) ;
#97817 = DIRECTION('ref_axis',(1.,0.,0.)) ;
#97818 = DIRECTION('center_axis',(-1.,-1.77538105744504E-14,-1.77538105744508E-14)) ;
#97819 = DIRECTION('ref_axis',(1.77538105744506E-14,8.67361737988379E-15,
-1.)) ;
#97820 = DIRECTION('center_axis',(2.08166817117218E-16,1.,0.)) ;
#97821 = DIRECTION('ref_axis',(1.,0.,0.)) ;
#97822 = DIRECTION('center_axis',(-0.577350269189595,0.577350269189594,-0.577350269189688)) ;
#97823 = DIRECTION('ref_axis',(0.707106781186627,4.55186387217293E-14,-0.707106781186468)) ;
#97824 = DIRECTION('center_axis',(-9.81307786677359E-14,0.,1.)) ;
#97825 = DIRECTION('ref_axis',(-1.,0.,-9.81307786677359E-14)) ;
#97826 = DIRECTION('center_axis',(-1.,0.,-9.8563833862319E-18)) ;
#97827 = DIRECTION('ref_axis',(-9.8563833862319E-18,0.,1.)) ;
#97828 = DIRECTION('center_axis',(-1.,0.,8.71102322353262E-14)) ;
#97829 = DIRECTION('ref_axis',(8.71102322353262E-14,0.,1.)) ;
#97830 = DIRECTION('center_axis',(0.,0.,-1.)) ;
#97831 = DIRECTION('ref_axis',(-1.,0.,0.)) ;
#97832 = DIRECTION('center_axis',(6.93889390390722E-14,-6.93889390390721E-14,
1.)) ;
#97833 = DIRECTION('ref_axis',(1.,-6.3534872372487E-42,-6.93889390390722E-14)) ;
#97834 = DIRECTION('center_axis',(0.577350269189625,-0.577350269189625,0.577350269189628)) ;
#97835 = DIRECTION('ref_axis',(0.707106781186552,5.19478420936363E-15,-0.707106781186543)) ;
#97836 = DIRECTION('center_axis',(0.577350269189625,-0.577350269189625,0.577350269189628)) ;
#97837 = DIRECTION('ref_axis',(0.707106781186552,5.1349792556416E-15,-0.707106781186543)) ;
#97838 = DIRECTION('center_axis',(2.08166817117218E-16,1.,0.)) ;
#97839 = DIRECTION('ref_axis',(1.,0.,0.)) ;
#97840 = DIRECTION('center_axis',(-0.577350269189538,0.577350269189662,0.577350269189676)) ;
#97841 = DIRECTION('ref_axis',(1.74300544639431E-14,0.707106781186565,-0.70710678118653)) ;
#97842 = DIRECTION('center_axis',(0.,0.,-1.)) ;
#97843 = DIRECTION('ref_axis',(-1.,0.,0.)) ;
#97844 = DIRECTION('center_axis',(0.,0.,1.)) ;
#97845 = DIRECTION('ref_axis',(-1.,0.,0.)) ;
#97846 = DIRECTION('center_axis',(0.,0.,-1.)) ;
#97847 = DIRECTION('ref_axis',(-1.,0.,0.)) ;
#97848 = DIRECTION('center_axis',(-0.577350269189625,0.577350269189625,0.577350269189628)) ;
#97849 = DIRECTION('ref_axis',(0.707106781186552,5.1349792556416E-15,0.707106781186543)) ;
#97850 = DIRECTION('center_axis',(0.577350269189625,-0.577350269189625,-0.577350269189628)) ;
#97851 = DIRECTION('ref_axis',(0.707106781186562,2.5899563042358E-14,0.707106781186533)) ;
#97852 = DIRECTION('center_axis',(-0.577350269189625,0.577350269189626,-0.577350269189626)) ;
#97853 = DIRECTION('ref_axis',(5.20172641667636E-15,0.70710678118655,0.707106781186545)) ;
#97854 = DIRECTION('center_axis',(0.577350269189625,-0.577350269189626,0.577350269189626)) ;
#97855 = DIRECTION('ref_axis',(4.10196750502305E-14,0.707106781186568,0.707106781186527)) ;
#97856 = DIRECTION('center_axis',(0.577350269189612,-0.57735026918964,0.577350269189626)) ;
#97857 = DIRECTION('ref_axis',(-8.27428663398926E-15,-0.707106781186543,-0.707106781186552)) ;
#97858 = DIRECTION('center_axis',(0.,0.,-1.)) ;
#97859 = DIRECTION('ref_axis',(-1.,0.,0.)) ;
#97860 = DIRECTION('center_axis',(0.,0.,1.)) ;
#97861 = DIRECTION('ref_axis',(-1.,1.35525271560688E-14,0.)) ;
#97862 = DIRECTION('center_axis',(0.,0.,-1.)) ;
#97863 = DIRECTION('ref_axis',(-1.,0.,0.)) ;
#97864 = DIRECTION('center_axis',(0.,1.,0.)) ;
#97865 = DIRECTION('ref_axis',(1.,0.,0.)) ;
#97866 = DIRECTION('center_axis',(0.,-1.,1.13080389480401E-14)) ;
#97867 = DIRECTION('ref_axis',(1.12757025938489E-13,1.13080389480401E-14,
1.)) ;
#97868 = DIRECTION('center_axis',(0.,0.,1.)) ;
#97869 = DIRECTION('ref_axis',(-1.,0.,0.)) ;
#97870 = DIRECTION('center_axis',(0.577350269189625,-0.577350269189626,-0.577350269189626)) ;
#97871 = DIRECTION('ref_axis',(5.20172641667636E-15,0.70710678118655,-0.707106781186545)) ;
#97872 = DIRECTION('center_axis',(0.577350269189625,-0.577350269189626,-0.577350269189626)) ;
#97873 = DIRECTION('ref_axis',(5.11416588733871E-15,0.70710678118655,-0.707106781186545)) ;
#97874 = DIRECTION('center_axis',(0.577350269189618,-0.577350269189619,-0.57735026918964)) ;
#97875 = DIRECTION('ref_axis',(1.15945863464918E-15,0.707106781186561,-0.707106781186534)) ;
#97876 = DIRECTION('center_axis',(0.,0.,-1.)) ;
#97877 = DIRECTION('ref_axis',(-1.,0.,0.)) ;
#97878 = DIRECTION('center_axis',(0.,0.,1.)) ;
#97879 = DIRECTION('ref_axis',(1.,0.,0.)) ;
#97880 = DIRECTION('center_axis',(0.,1.,1.95511867169518E-16)) ;
#97881 = DIRECTION('ref_axis',(0.,-1.95511867169518E-16,1.)) ;
#97882 = DIRECTION('center_axis',(4.26226979058352E-14,-1.,4.24310362287508E-14)) ;
#97883 = DIRECTION('ref_axis',(1.,4.26226979058352E-14,4.69939452995971E-41)) ;
#97884 = DIRECTION('center_axis',(0.,1.,0.)) ;
#97885 = DIRECTION('ref_axis',(1.,0.,0.)) ;
#97886 = DIRECTION('center_axis',(-1.00288700954911E-14,-1.,1.02205317725767E-14)) ;
#97887 = DIRECTION('ref_axis',(3.46944695195352E-14,1.02205317725764E-14,
1.)) ;
#97888 = DIRECTION('center_axis',(0.,1.,0.)) ;
#97889 = DIRECTION('ref_axis',(1.,0.,0.)) ;
#97890 = DIRECTION('center_axis',(-0.577350269189659,-0.57735026918966,-0.577350269189558)) ;
#97891 = DIRECTION('ref_axis',(-0.707106781186543,0.707106781186552,-1.03102727271032E-14)) ;
#97892 = DIRECTION('center_axis',(0.,9.8130778667736E-14,1.)) ;
#97893 = DIRECTION('ref_axis',(-8.67361737988403E-15,1.,-9.8130778667736E-14)) ;
#97894 = DIRECTION('center_axis',(0.,1.,-1.95511867169518E-16)) ;
#97895 = DIRECTION('ref_axis',(0.,1.95511867169518E-16,1.)) ;
#97896 = DIRECTION('center_axis',(0.,-1.,9.83224403448236E-14)) ;
#97897 = DIRECTION('ref_axis',(0.,-9.83224403448236E-14,-1.)) ;
#97898 = DIRECTION('center_axis',(0.,0.,-1.)) ;
#97899 = DIRECTION('ref_axis',(-1.,0.,0.)) ;
#97900 = DIRECTION('center_axis',(0.,0.,1.)) ;
#97901 = DIRECTION('ref_axis',(1.,0.,0.)) ;
#97902 = DIRECTION('center_axis',(0.577350269189625,0.577350269189626,0.577350269189627)) ;
#97903 = DIRECTION('ref_axis',(5.35231302451417E-15,-0.707106781186551,0.707106781186544)) ;
#97904 = DIRECTION('center_axis',(0.577350269189625,0.577350269189626,0.577350269189627)) ;
#97905 = DIRECTION('ref_axis',(5.35231302451417E-15,-0.707106781186551,0.707106781186544)) ;
#97906 = DIRECTION('center_axis',(0.,1.,0.)) ;
#97907 = DIRECTION('ref_axis',(1.,0.,0.)) ;
#97908 = DIRECTION('center_axis',(-0.57735026918964,-0.577350269189583,0.577350269189654)) ;
#97909 = DIRECTION('ref_axis',(-0.707106781186567,2.1970613508967E-14,-0.707106781186528)) ;
#97910 = DIRECTION('center_axis',(0.,0.,-1.)) ;
#97911 = DIRECTION('ref_axis',(-1.,0.,0.)) ;
#97912 = DIRECTION('center_axis',(0.,0.,1.)) ;
#97913 = DIRECTION('ref_axis',(-1.,1.0842021724855E-15,0.)) ;
#97914 = DIRECTION('center_axis',(0.,0.,-1.)) ;
#97915 = DIRECTION('ref_axis',(-1.,0.,0.)) ;
#97916 = DIRECTION('center_axis',(-0.577350269189625,-0.577350269189626,0.577350269189627)) ;
#97917 = DIRECTION('ref_axis',(5.35231302451417E-15,-0.707106781186551,-0.707106781186544)) ;
#97918 = DIRECTION('center_axis',(0.577350269189625,0.577350269189626,-0.577350269189627)) ;
#97919 = DIRECTION('ref_axis',(4.8009187113684E-14,-0.707106781186572,-0.707106781186523)) ;
#97920 = DIRECTION('center_axis',(0.,0.,1.)) ;
#97921 = DIRECTION('ref_axis',(1.,0.,0.)) ;
#97922 = DIRECTION('center_axis',(0.,-1.,0.)) ;
#97923 = DIRECTION('ref_axis',(0.,0.,-1.)) ;
#97924 = DIRECTION('center_axis',(9.85638338623186E-18,1.,0.)) ;
#97925 = DIRECTION('ref_axis',(-1.,9.85638338623186E-18,0.)) ;
#97926 = DIRECTION('center_axis',(0.,-1.,0.)) ;
#97927 = DIRECTION('ref_axis',(0.,0.,-1.)) ;
#97928 = DIRECTION('center_axis',(0.,1.,0.)) ;
#97929 = DIRECTION('ref_axis',(1.,0.,0.)) ;
#97930 = DIRECTION('center_axis',(-1.,-7.66646708341686E-16,0.)) ;
#97931 = DIRECTION('ref_axis',(7.66646708341686E-16,-1.,0.)) ;
#97932 = DIRECTION('center_axis',(1.,-9.85638338623186E-18,0.)) ;
#97933 = DIRECTION('ref_axis',(9.85638338623186E-18,1.,0.)) ;
#97934 = DIRECTION('center_axis',(-1.,0.,0.)) ;
#97935 = DIRECTION('ref_axis',(0.,0.,1.)) ;
#97936 = DIRECTION('center_axis',(0.,1.,0.)) ;
#97937 = DIRECTION('ref_axis',(1.,0.,0.)) ;
#97938 = DIRECTION('center_axis',(0.,1.,0.)) ;
#97939 = DIRECTION('ref_axis',(0.,0.,1.)) ;
#97940 = DIRECTION('center_axis',(-9.85638338623186E-18,-1.,0.)) ;
#97941 = DIRECTION('ref_axis',(1.,-9.85638338623186E-18,0.)) ;
#97942 = DIRECTION('center_axis',(0.,1.,0.)) ;
#97943 = DIRECTION('ref_axis',(0.,0.,1.)) ;
#97944 = DIRECTION('center_axis',(0.,0.,1.)) ;
#97945 = DIRECTION('ref_axis',(1.,0.,0.)) ;
#97946 = DIRECTION('center_axis',(0.,0.,1.)) ;
#97947 = DIRECTION('ref_axis',(1.,0.,0.)) ;
#97948 = DIRECTION('center_axis',(0.,-1.,0.)) ;
#97949 = DIRECTION('ref_axis',(0.,0.,-1.)) ;
#97950 = DIRECTION('center_axis',(-9.85638338623186E-18,-1.,0.)) ;
#97951 = DIRECTION('ref_axis',(1.,-9.85638338623186E-18,0.)) ;
#97952 = DIRECTION('center_axis',(0.,-1.,0.)) ;
#97953 = DIRECTION('ref_axis',(0.,0.,-1.)) ;
#97954 = DIRECTION('center_axis',(0.,1.,0.)) ;
#97955 = DIRECTION('ref_axis',(1.,0.,0.)) ;
#97956 = DIRECTION('center_axis',(1.,-3.06658683336674E-15,0.)) ;
#97957 = DIRECTION('ref_axis',(3.06658683336674E-15,1.,0.)) ;
#97958 = DIRECTION('center_axis',(1.,-9.85638338623186E-18,0.)) ;
#97959 = DIRECTION('ref_axis',(9.85638338623186E-18,1.,0.)) ;
#97960 = DIRECTION('center_axis',(1.,0.,0.)) ;
#97961 = DIRECTION('ref_axis',(0.,0.,-1.)) ;
#97962 = DIRECTION('center_axis',(0.,1.,0.)) ;
#97963 = DIRECTION('ref_axis',(1.,0.,0.)) ;
#97964 = DIRECTION('center_axis',(0.,1.,0.)) ;
#97965 = DIRECTION('ref_axis',(0.,0.,1.)) ;
#97966 = DIRECTION('center_axis',(-9.85638338623186E-18,-1.,0.)) ;
#97967 = DIRECTION('ref_axis',(1.,-9.85638338623186E-18,0.)) ;
#97968 = DIRECTION('center_axis',(0.,1.,0.)) ;
#97969 = DIRECTION('ref_axis',(0.,0.,1.)) ;
#97970 = DIRECTION('center_axis',(0.,0.,1.)) ;
#97971 = DIRECTION('ref_axis',(1.,0.,0.)) ;
#97972 = DIRECTION('center_axis',(-1.,-1.95511867169517E-16,0.)) ;
#97973 = DIRECTION('ref_axis',(1.95511867169517E-16,-1.,0.)) ;
#97974 = DIRECTION('center_axis',(1.,0.,0.)) ;
#97975 = DIRECTION('ref_axis',(0.,0.,-1.)) ;
#97976 = DIRECTION('center_axis',(0.,1.,0.)) ;
#97977 = DIRECTION('ref_axis',(1.,0.,0.)) ;
#97978 = DIRECTION('center_axis',(7.66646708341686E-16,-1.,0.)) ;
#97979 = DIRECTION('ref_axis',(1.,7.66646708341686E-16,0.)) ;
#97980 = DIRECTION('center_axis',(-1.95511867169517E-16,1.,0.)) ;
#97981 = DIRECTION('ref_axis',(-1.,-1.95511867169517E-16,0.)) ;
#97982 = DIRECTION('center_axis',(0.,-1.,0.)) ;
#97983 = DIRECTION('ref_axis',(0.,0.,-1.)) ;
#97984 = DIRECTION('center_axis',(0.,1.,0.)) ;
#97985 = DIRECTION('ref_axis',(1.,0.,0.)) ;
#97986 = DIRECTION('center_axis',(-1.,0.,0.)) ;
#97987 = DIRECTION('ref_axis',(0.,0.,1.)) ;
#97988 = DIRECTION('center_axis',(1.,-1.06642836637918E-16,0.)) ;
#97989 = DIRECTION('ref_axis',(1.06642836637918E-16,1.,0.)) ;
#97990 = DIRECTION('center_axis',(1.,1.95511867169517E-16,0.)) ;
#97991 = DIRECTION('ref_axis',(-1.95511867169517E-16,1.,0.)) ;
#97992 = DIRECTION('center_axis',(1.,0.,0.)) ;
#97993 = DIRECTION('ref_axis',(0.,0.,-1.)) ;
#97994 = DIRECTION('center_axis',(0.,1.,0.)) ;
#97995 = DIRECTION('ref_axis',(1.,0.,0.)) ;
#97996 = DIRECTION('center_axis',(2.29994012502506E-15,-1.,0.)) ;
#97997 = DIRECTION('ref_axis',(1.,2.29994012502506E-15,0.)) ;
#97998 = DIRECTION('center_axis',(-1.95511867169517E-16,1.,0.)) ;
#97999 = DIRECTION('ref_axis',(-1.,-1.95511867169517E-16,0.)) ;
#98000 = DIRECTION('center_axis',(0.,-1.,0.)) ;
#98001 = DIRECTION('ref_axis',(0.,0.,-1.)) ;
#98002 = DIRECTION('center_axis',(-1.,1.06642836637918E-16,0.)) ;
#98003 = DIRECTION('ref_axis',(-1.06642836637918E-16,-1.,0.)) ;
#98004 = DIRECTION('center_axis',(1.,0.,0.)) ;
#98005 = DIRECTION('ref_axis',(0.,0.,-1.)) ;
#98006 = DIRECTION('center_axis',(0.,1.,0.)) ;
#98007 = DIRECTION('ref_axis',(1.,0.,0.)) ;
#98008 = DIRECTION('center_axis',(0.,0.,1.)) ;
#98009 = DIRECTION('ref_axis',(1.,0.,0.)) ;
#98010 = DIRECTION('center_axis',(0.,-1.,0.)) ;
#98011 = DIRECTION('ref_axis',(0.,0.,-1.)) ;
#98012 = DIRECTION('center_axis',(9.85638338623186E-18,1.,0.)) ;
#98013 = DIRECTION('ref_axis',(-1.,9.85638338623186E-18,0.)) ;
#98014 = DIRECTION('center_axis',(0.,-1.,0.)) ;
#98015 = DIRECTION('ref_axis',(0.,0.,-1.)) ;
#98016 = DIRECTION('center_axis',(0.,1.,0.)) ;
#98017 = DIRECTION('ref_axis',(1.,0.,0.)) ;
#98018 = DIRECTION('center_axis',(-1.,-1.14997006251252E-14,0.)) ;
#98019 = DIRECTION('ref_axis',(1.14997006251252E-14,-1.,0.)) ;
#98020 = DIRECTION('center_axis',(1.,-9.85638338623186E-18,0.)) ;
#98021 = DIRECTION('ref_axis',(9.85638338623186E-18,1.,0.)) ;
#98022 = DIRECTION('center_axis',(-1.,0.,0.)) ;
#98023 = DIRECTION('ref_axis',(0.,0.,1.)) ;
#98024 = DIRECTION('center_axis',(0.,1.,0.)) ;
#98025 = DIRECTION('ref_axis',(1.,0.,0.)) ;
#98026 = DIRECTION('center_axis',(0.,1.,0.)) ;
#98027 = DIRECTION('ref_axis',(0.,0.,1.)) ;
#98028 = DIRECTION('center_axis',(-9.85638338623186E-18,-1.,0.)) ;
#98029 = DIRECTION('ref_axis',(1.,-9.85638338623186E-18,0.)) ;
#98030 = DIRECTION('center_axis',(0.,1.,0.)) ;
#98031 = DIRECTION('ref_axis',(0.,0.,1.)) ;
#98032 = DIRECTION('center_axis',(0.,0.,1.)) ;
#98033 = DIRECTION('ref_axis',(1.,0.,0.)) ;
#98034 = DIRECTION('center_axis',(0.,0.,1.)) ;
#98035 = DIRECTION('ref_axis',(1.,0.,0.)) ;
#98036 = DIRECTION('center_axis',(0.,-1.,0.)) ;
#98037 = DIRECTION('ref_axis',(0.,0.,-1.)) ;
#98038 = DIRECTION('center_axis',(-9.85638338623186E-18,-1.,0.)) ;
#98039 = DIRECTION('ref_axis',(1.,-9.85638338623186E-18,0.)) ;
#98040 = DIRECTION('center_axis',(0.,-1.,0.)) ;
#98041 = DIRECTION('ref_axis',(0.,0.,-1.)) ;
#98042 = DIRECTION('center_axis',(0.,1.,0.)) ;
#98043 = DIRECTION('ref_axis',(1.,0.,0.)) ;
#98044 = DIRECTION('center_axis',(1.,3.83323354170843E-15,0.)) ;
#98045 = DIRECTION('ref_axis',(-3.83323354170843E-15,1.,0.)) ;
#98046 = DIRECTION('center_axis',(1.,-9.85638338623186E-18,0.)) ;
#98047 = DIRECTION('ref_axis',(9.85638338623186E-18,1.,0.)) ;
#98048 = DIRECTION('center_axis',(1.,0.,0.)) ;
#98049 = DIRECTION('ref_axis',(0.,0.,-1.)) ;
#98050 = DIRECTION('center_axis',(0.,1.,0.)) ;
#98051 = DIRECTION('ref_axis',(1.,0.,0.)) ;
#98052 = DIRECTION('center_axis',(0.,1.,0.)) ;
#98053 = DIRECTION('ref_axis',(0.,0.,1.)) ;
#98054 = DIRECTION('center_axis',(-9.85638338623186E-18,-1.,0.)) ;
#98055 = DIRECTION('ref_axis',(1.,-9.85638338623186E-18,0.)) ;
#98056 = DIRECTION('center_axis',(0.,1.,0.)) ;
#98057 = DIRECTION('ref_axis',(0.,0.,1.)) ;
#98058 = DIRECTION('center_axis',(0.,0.,1.)) ;
#98059 = DIRECTION('ref_axis',(1.,0.,0.)) ;
#98060 = DIRECTION('center_axis',(-1.,-1.95511867169517E-16,0.)) ;
#98061 = DIRECTION('ref_axis',(1.95511867169517E-16,-1.,0.)) ;
#98062 = DIRECTION('center_axis',(1.,0.,0.)) ;
#98063 = DIRECTION('ref_axis',(0.,0.,-1.)) ;
#98064 = DIRECTION('center_axis',(0.,1.,0.)) ;
#98065 = DIRECTION('ref_axis',(1.,0.,0.)) ;
#98066 = DIRECTION('center_axis',(4.59988025005012E-15,-1.,0.)) ;
#98067 = DIRECTION('ref_axis',(1.,4.59988025005012E-15,0.)) ;
#98068 = DIRECTION('center_axis',(-1.95511867169517E-16,1.,0.)) ;
#98069 = DIRECTION('ref_axis',(-1.,-1.95511867169517E-16,0.)) ;
#98070 = DIRECTION('center_axis',(0.,-1.,0.)) ;
#98071 = DIRECTION('ref_axis',(0.,0.,-1.)) ;
#98072 = DIRECTION('center_axis',(0.,1.,0.)) ;
#98073 = DIRECTION('ref_axis',(1.,0.,0.)) ;
#98074 = DIRECTION('center_axis',(-1.,0.,0.)) ;
#98075 = DIRECTION('ref_axis',(0.,0.,1.)) ;
#98076 = DIRECTION('center_axis',(1.,-1.06642836637918E-16,0.)) ;
#98077 = DIRECTION('ref_axis',(1.06642836637918E-16,1.,0.)) ;
#98078 = DIRECTION('center_axis',(1.,1.95511867169517E-16,0.)) ;
#98079 = DIRECTION('ref_axis',(-1.95511867169517E-16,1.,0.)) ;
#98080 = DIRECTION('center_axis',(1.,0.,0.)) ;
#98081 = DIRECTION('ref_axis',(0.,0.,-1.)) ;
#98082 = DIRECTION('center_axis',(0.,1.,0.)) ;
#98083 = DIRECTION('ref_axis',(1.,0.,0.)) ;
#98084 = DIRECTION('center_axis',(-1.53329341668337E-15,-1.,0.)) ;
#98085 = DIRECTION('ref_axis',(1.,-1.53329341668337E-15,0.)) ;
#98086 = DIRECTION('center_axis',(-1.95511867169517E-16,1.,0.)) ;
#98087 = DIRECTION('ref_axis',(-1.,-1.95511867169517E-16,0.)) ;
#98088 = DIRECTION('center_axis',(0.,-1.,0.)) ;
#98089 = DIRECTION('ref_axis',(0.,0.,-1.)) ;
#98090 = DIRECTION('center_axis',(-1.,1.06642836637918E-16,0.)) ;
#98091 = DIRECTION('ref_axis',(-1.06642836637918E-16,-1.,0.)) ;
#98092 = DIRECTION('center_axis',(1.,0.,0.)) ;
#98093 = DIRECTION('ref_axis',(0.,0.,-1.)) ;
#98094 = DIRECTION('center_axis',(0.,1.,0.)) ;
#98095 = DIRECTION('ref_axis',(1.,0.,0.)) ;
#98096 = DIRECTION('center_axis',(0.,0.,1.)) ;
#98097 = DIRECTION('ref_axis',(1.,0.,0.)) ;
#98098 = DIRECTION('center_axis',(0.,-1.,0.)) ;
#98099 = DIRECTION('ref_axis',(0.,0.,-1.)) ;
#98100 = DIRECTION('center_axis',(9.85638338623186E-18,1.,0.)) ;
#98101 = DIRECTION('ref_axis',(-1.,9.85638338623186E-18,0.)) ;
#98102 = DIRECTION('center_axis',(0.,-1.,0.)) ;
#98103 = DIRECTION('ref_axis',(0.,0.,-1.)) ;
#98104 = DIRECTION('center_axis',(0.,1.,0.)) ;
#98105 = DIRECTION('ref_axis',(1.,0.,0.)) ;
#98106 = DIRECTION('center_axis',(-1.,-2.29994012502506E-15,0.)) ;
#98107 = DIRECTION('ref_axis',(2.29994012502506E-15,-1.,0.)) ;
#98108 = DIRECTION('center_axis',(1.,-9.85638338623186E-18,0.)) ;
#98109 = DIRECTION('ref_axis',(9.85638338623186E-18,1.,0.)) ;
#98110 = DIRECTION('center_axis',(-1.,0.,0.)) ;
#98111 = DIRECTION('ref_axis',(0.,0.,1.)) ;
#98112 = DIRECTION('center_axis',(0.,1.,0.)) ;
#98113 = DIRECTION('ref_axis',(1.,0.,0.)) ;
#98114 = DIRECTION('center_axis',(0.,1.,0.)) ;
#98115 = DIRECTION('ref_axis',(0.,0.,1.)) ;
#98116 = DIRECTION('center_axis',(-9.85638338623186E-18,-1.,0.)) ;
#98117 = DIRECTION('ref_axis',(1.,-9.85638338623186E-18,0.)) ;
#98118 = DIRECTION('center_axis',(0.,1.,0.)) ;
#98119 = DIRECTION('ref_axis',(0.,0.,1.)) ;
#98120 = DIRECTION('center_axis',(0.,0.,1.)) ;
#98121 = DIRECTION('ref_axis',(1.,0.,0.)) ;
#98122 = DIRECTION('center_axis',(0.,0.,1.)) ;
#98123 = DIRECTION('ref_axis',(1.,0.,0.)) ;
#98124 = DIRECTION('center_axis',(0.,-1.,0.)) ;
#98125 = DIRECTION('ref_axis',(0.,0.,-1.)) ;
#98126 = DIRECTION('center_axis',(-9.85638338623186E-18,-1.,0.)) ;
#98127 = DIRECTION('ref_axis',(1.,-9.85638338623186E-18,0.)) ;
#98128 = DIRECTION('center_axis',(0.,-1.,0.)) ;
#98129 = DIRECTION('ref_axis',(0.,0.,-1.)) ;
#98130 = DIRECTION('center_axis',(0.,1.,0.)) ;
#98131 = DIRECTION('ref_axis',(1.,0.,0.)) ;
#98132 = DIRECTION('center_axis',(1.,-7.66646708341686E-15,0.)) ;
#98133 = DIRECTION('ref_axis',(7.66646708341686E-15,1.,0.)) ;
#98134 = DIRECTION('center_axis',(1.,-9.85638338623186E-18,0.)) ;
#98135 = DIRECTION('ref_axis',(9.85638338623186E-18,1.,0.)) ;
#98136 = DIRECTION('center_axis',(1.,0.,0.)) ;
#98137 = DIRECTION('ref_axis',(0.,0.,-1.)) ;
#98138 = DIRECTION('center_axis',(0.,1.,0.)) ;
#98139 = DIRECTION('ref_axis',(1.,0.,0.)) ;
#98140 = DIRECTION('center_axis',(0.,1.,0.)) ;
#98141 = DIRECTION('ref_axis',(0.,0.,1.)) ;
#98142 = DIRECTION('center_axis',(-9.85638338623186E-18,-1.,0.)) ;
#98143 = DIRECTION('ref_axis',(1.,-9.85638338623186E-18,0.)) ;
#98144 = DIRECTION('center_axis',(0.,1.,0.)) ;
#98145 = DIRECTION('ref_axis',(0.,0.,1.)) ;
#98146 = DIRECTION('center_axis',(0.,0.,1.)) ;
#98147 = DIRECTION('ref_axis',(1.,0.,0.)) ;
#98148 = DIRECTION('center_axis',(-1.,-1.95511867169517E-16,0.)) ;
#98149 = DIRECTION('ref_axis',(1.95511867169517E-16,-1.,0.)) ;
#98150 = DIRECTION('center_axis',(1.,0.,0.)) ;
#98151 = DIRECTION('ref_axis',(0.,0.,-1.)) ;
#98152 = DIRECTION('center_axis',(0.,1.,0.)) ;
#98153 = DIRECTION('ref_axis',(1.,0.,0.)) ;
#98154 = DIRECTION('center_axis',(9.9664072084418E-15,-1.,0.)) ;
#98155 = DIRECTION('ref_axis',(1.,9.9664072084418E-15,0.)) ;
#98156 = DIRECTION('center_axis',(-1.95511867169517E-16,1.,0.)) ;
#98157 = DIRECTION('ref_axis',(-1.,-1.95511867169517E-16,0.)) ;
#98158 = DIRECTION('center_axis',(0.,-1.,0.)) ;
#98159 = DIRECTION('ref_axis',(0.,0.,-1.)) ;
#98160 = DIRECTION('center_axis',(0.,1.,0.)) ;
#98161 = DIRECTION('ref_axis',(1.,0.,0.)) ;
#98162 = DIRECTION('center_axis',(-1.,0.,0.)) ;
#98163 = DIRECTION('ref_axis',(0.,0.,1.)) ;
#98164 = DIRECTION('center_axis',(1.,-1.06642836637918E-16,0.)) ;
#98165 = DIRECTION('ref_axis',(1.06642836637918E-16,1.,0.)) ;
#98166 = DIRECTION('center_axis',(1.,1.95511867169517E-16,0.)) ;
#98167 = DIRECTION('ref_axis',(-1.95511867169517E-16,1.,0.)) ;
#98168 = DIRECTION('center_axis',(1.,0.,0.)) ;
#98169 = DIRECTION('ref_axis',(0.,0.,-1.)) ;
#98170 = DIRECTION('center_axis',(0.,1.,0.)) ;
#98171 = DIRECTION('ref_axis',(1.,0.,0.)) ;
#98172 = DIRECTION('center_axis',(6.89982037507517E-15,-1.,0.)) ;
#98173 = DIRECTION('ref_axis',(1.,6.89982037507517E-15,0.)) ;
#98174 = DIRECTION('center_axis',(-1.95511867169517E-16,1.,0.)) ;
#98175 = DIRECTION('ref_axis',(-1.,-1.95511867169517E-16,0.)) ;
#98176 = DIRECTION('center_axis',(0.,-1.,0.)) ;
#98177 = DIRECTION('ref_axis',(0.,0.,-1.)) ;
#98178 = DIRECTION('center_axis',(-1.,1.06642836637918E-16,0.)) ;
#98179 = DIRECTION('ref_axis',(-1.06642836637918E-16,-1.,0.)) ;
#98180 = DIRECTION('center_axis',(1.,0.,0.)) ;
#98181 = DIRECTION('ref_axis',(0.,0.,-1.)) ;
#98182 = DIRECTION('center_axis',(0.,1.,0.)) ;
#98183 = DIRECTION('ref_axis',(1.,0.,0.)) ;
#98184 = DIRECTION('center_axis',(0.,0.,1.)) ;
#98185 = DIRECTION('ref_axis',(1.,0.,0.)) ;
#98186 = DIRECTION('center_axis',(0.,-1.,0.)) ;
#98187 = DIRECTION('ref_axis',(0.,0.,-1.)) ;
#98188 = DIRECTION('center_axis',(9.85638338623186E-18,1.,0.)) ;
#98189 = DIRECTION('ref_axis',(-1.,9.85638338623186E-18,0.)) ;
#98190 = DIRECTION('center_axis',(0.,-1.,0.)) ;
#98191 = DIRECTION('ref_axis',(0.,0.,-1.)) ;
#98192 = DIRECTION('center_axis',(0.,1.,0.)) ;
#98193 = DIRECTION('ref_axis',(1.,0.,0.)) ;
#98194 = DIRECTION('center_axis',(-1.,0.,0.)) ;
#98195 = DIRECTION('ref_axis',(0.,0.,1.)) ;
#98196 = DIRECTION('center_axis',(1.,-9.85638338623186E-18,0.)) ;
#98197 = DIRECTION('ref_axis',(9.85638338623186E-18,1.,0.)) ;
#98198 = DIRECTION('center_axis',(-1.,0.,0.)) ;
#98199 = DIRECTION('ref_axis',(0.,0.,1.)) ;
#98200 = DIRECTION('center_axis',(0.,1.,0.)) ;
#98201 = DIRECTION('ref_axis',(1.,0.,0.)) ;
#98202 = DIRECTION('center_axis',(0.,1.,0.)) ;
#98203 = DIRECTION('ref_axis',(0.,0.,1.)) ;
#98204 = DIRECTION('center_axis',(-9.85638338623186E-18,-1.,0.)) ;
#98205 = DIRECTION('ref_axis',(1.,-9.85638338623186E-18,0.)) ;
#98206 = DIRECTION('center_axis',(0.,1.,0.)) ;
#98207 = DIRECTION('ref_axis',(0.,0.,1.)) ;
#98208 = DIRECTION('center_axis',(0.,0.,1.)) ;
#98209 = DIRECTION('ref_axis',(1.,0.,0.)) ;
#98210 = DIRECTION('center_axis',(0.,0.,1.)) ;
#98211 = DIRECTION('ref_axis',(1.,0.,0.)) ;
#98212 = DIRECTION('center_axis',(0.,-1.,0.)) ;
#98213 = DIRECTION('ref_axis',(0.,0.,-1.)) ;
#98214 = DIRECTION('center_axis',(-9.85638338623186E-18,-1.,0.)) ;
#98215 = DIRECTION('ref_axis',(1.,-9.85638338623186E-18,0.)) ;
#98216 = DIRECTION('center_axis',(0.,-1.,0.)) ;
#98217 = DIRECTION('ref_axis',(0.,0.,-1.)) ;
#98218 = DIRECTION('center_axis',(0.,1.,0.)) ;
#98219 = DIRECTION('ref_axis',(1.,0.,0.)) ;
#98220 = DIRECTION('center_axis',(1.,-9.19976050010023E-15,0.)) ;
#98221 = DIRECTION('ref_axis',(9.19976050010023E-15,1.,0.)) ;
#98222 = DIRECTION('center_axis',(1.,-9.85638338623186E-18,0.)) ;
#98223 = DIRECTION('ref_axis',(9.85638338623186E-18,1.,0.)) ;
#98224 = DIRECTION('center_axis',(1.,0.,0.)) ;
#98225 = DIRECTION('ref_axis',(0.,0.,-1.)) ;
#98226 = DIRECTION('center_axis',(0.,1.,0.)) ;
#98227 = DIRECTION('ref_axis',(1.,0.,0.)) ;
#98228 = DIRECTION('center_axis',(0.,1.,0.)) ;
#98229 = DIRECTION('ref_axis',(0.,0.,1.)) ;
#98230 = DIRECTION('center_axis',(-9.85638338623186E-18,-1.,0.)) ;
#98231 = DIRECTION('ref_axis',(1.,-9.85638338623186E-18,0.)) ;
#98232 = DIRECTION('center_axis',(0.,1.,0.)) ;
#98233 = DIRECTION('ref_axis',(0.,0.,1.)) ;
#98234 = DIRECTION('center_axis',(0.,0.,1.)) ;
#98235 = DIRECTION('ref_axis',(1.,0.,0.)) ;
#98236 = DIRECTION('center_axis',(-1.,-1.95511867169517E-16,0.)) ;
#98237 = DIRECTION('ref_axis',(1.95511867169517E-16,-1.,0.)) ;
#98238 = DIRECTION('center_axis',(1.,0.,0.)) ;
#98239 = DIRECTION('ref_axis',(0.,0.,-1.)) ;
#98240 = DIRECTION('center_axis',(0.,1.,0.)) ;
#98241 = DIRECTION('ref_axis',(1.,0.,0.)) ;
#98242 = DIRECTION('center_axis',(-1.53329341668337E-15,-1.,0.)) ;
#98243 = DIRECTION('ref_axis',(1.,-1.53329341668337E-15,0.)) ;
#98244 = DIRECTION('center_axis',(-1.95511867169517E-16,1.,0.)) ;
#98245 = DIRECTION('ref_axis',(-1.,-1.95511867169517E-16,0.)) ;
#98246 = DIRECTION('center_axis',(0.,-1.,0.)) ;
#98247 = DIRECTION('ref_axis',(0.,0.,-1.)) ;
#98248 = DIRECTION('center_axis',(0.,1.,0.)) ;
#98249 = DIRECTION('ref_axis',(1.,0.,0.)) ;
#98250 = DIRECTION('center_axis',(-1.,0.,0.)) ;
#98251 = DIRECTION('ref_axis',(0.,0.,1.)) ;
#98252 = DIRECTION('center_axis',(1.,-1.06642836637918E-16,0.)) ;
#98253 = DIRECTION('ref_axis',(1.06642836637918E-16,1.,0.)) ;
#98254 = DIRECTION('center_axis',(1.,1.95511867169517E-16,0.)) ;
#98255 = DIRECTION('ref_axis',(-1.95511867169517E-16,1.,0.)) ;
#98256 = DIRECTION('center_axis',(1.,0.,0.)) ;
#98257 = DIRECTION('ref_axis',(0.,0.,-1.)) ;
#98258 = DIRECTION('center_axis',(0.,1.,0.)) ;
#98259 = DIRECTION('ref_axis',(1.,0.,0.)) ;
#98260 = DIRECTION('center_axis',(-3.06658683336674E-15,-1.,0.)) ;
#98261 = DIRECTION('ref_axis',(1.,-3.06658683336674E-15,0.)) ;
#98262 = DIRECTION('center_axis',(-1.95511867169517E-16,1.,0.)) ;
#98263 = DIRECTION('ref_axis',(-1.,-1.95511867169517E-16,0.)) ;
#98264 = DIRECTION('center_axis',(0.,-1.,0.)) ;
#98265 = DIRECTION('ref_axis',(0.,0.,-1.)) ;
#98266 = DIRECTION('center_axis',(-1.,1.06642836637918E-16,0.)) ;
#98267 = DIRECTION('ref_axis',(-1.06642836637918E-16,-1.,0.)) ;
#98268 = DIRECTION('center_axis',(1.,0.,0.)) ;
#98269 = DIRECTION('ref_axis',(0.,0.,-1.)) ;
#98270 = DIRECTION('center_axis',(0.,1.,0.)) ;
#98271 = DIRECTION('ref_axis',(1.,0.,0.)) ;
#98272 = DIRECTION('center_axis',(0.,0.,1.)) ;
#98273 = DIRECTION('ref_axis',(1.,0.,0.)) ;
#98274 = DIRECTION('center_axis',(0.,-1.,0.)) ;
#98275 = DIRECTION('ref_axis',(0.,0.,-1.)) ;
#98276 = DIRECTION('center_axis',(9.85638338623186E-18,1.,0.)) ;
#98277 = DIRECTION('ref_axis',(-1.,9.85638338623186E-18,0.)) ;
#98278 = DIRECTION('center_axis',(0.,-1.,0.)) ;
#98279 = DIRECTION('ref_axis',(0.,0.,-1.)) ;
#98280 = DIRECTION('center_axis',(0.,1.,0.)) ;
#98281 = DIRECTION('ref_axis',(1.,0.,0.)) ;
#98282 = DIRECTION('center_axis',(-1.,4.59988025005012E-15,0.)) ;
#98283 = DIRECTION('ref_axis',(-4.59988025005012E-15,-1.,0.)) ;
#98284 = DIRECTION('center_axis',(1.,-9.85638338623186E-18,0.)) ;
#98285 = DIRECTION('ref_axis',(9.85638338623186E-18,1.,0.)) ;
#98286 = DIRECTION('center_axis',(-1.,0.,0.)) ;
#98287 = DIRECTION('ref_axis',(0.,0.,1.)) ;
#98288 = DIRECTION('center_axis',(0.,1.,0.)) ;
#98289 = DIRECTION('ref_axis',(1.,0.,0.)) ;
#98290 = DIRECTION('center_axis',(0.,1.,0.)) ;
#98291 = DIRECTION('ref_axis',(0.,0.,1.)) ;
#98292 = DIRECTION('center_axis',(-9.85638338623186E-18,-1.,0.)) ;
#98293 = DIRECTION('ref_axis',(1.,-9.85638338623186E-18,0.)) ;
#98294 = DIRECTION('center_axis',(0.,1.,0.)) ;
#98295 = DIRECTION('ref_axis',(0.,0.,1.)) ;
#98296 = DIRECTION('center_axis',(0.,0.,1.)) ;
#98297 = DIRECTION('ref_axis',(1.,0.,0.)) ;
#98298 = DIRECTION('center_axis',(0.,0.,1.)) ;
#98299 = DIRECTION('ref_axis',(1.,0.,0.)) ;
#98300 = DIRECTION('center_axis',(0.,-1.,0.)) ;
#98301 = DIRECTION('ref_axis',(0.,0.,-1.)) ;
#98302 = DIRECTION('center_axis',(-9.85638338623186E-18,-1.,0.)) ;
#98303 = DIRECTION('ref_axis',(1.,-9.85638338623186E-18,0.)) ;
#98304 = DIRECTION('center_axis',(0.,-1.,0.)) ;
#98305 = DIRECTION('ref_axis',(0.,0.,-1.)) ;
#98306 = DIRECTION('center_axis',(0.,1.,0.)) ;
#98307 = DIRECTION('ref_axis',(1.,0.,0.)) ;
#98308 = DIRECTION('center_axis',(1.,-6.13317366673349E-15,0.)) ;
#98309 = DIRECTION('ref_axis',(6.13317366673349E-15,1.,0.)) ;
#98310 = DIRECTION('center_axis',(1.,-9.85638338623186E-18,0.)) ;
#98311 = DIRECTION('ref_axis',(9.85638338623186E-18,1.,0.)) ;
#98312 = DIRECTION('center_axis',(1.,0.,0.)) ;
#98313 = DIRECTION('ref_axis',(0.,0.,-1.)) ;
#98314 = DIRECTION('center_axis',(0.,1.,0.)) ;
#98315 = DIRECTION('ref_axis',(1.,0.,0.)) ;
#98316 = DIRECTION('center_axis',(0.,1.,0.)) ;
#98317 = DIRECTION('ref_axis',(0.,0.,1.)) ;
#98318 = DIRECTION('center_axis',(-9.85638338623186E-18,-1.,0.)) ;
#98319 = DIRECTION('ref_axis',(1.,-9.85638338623186E-18,0.)) ;
#98320 = DIRECTION('center_axis',(0.,1.,0.)) ;
#98321 = DIRECTION('ref_axis',(0.,0.,1.)) ;
#98322 = DIRECTION('center_axis',(0.,0.,1.)) ;
#98323 = DIRECTION('ref_axis',(1.,0.,0.)) ;
#98324 = DIRECTION('center_axis',(-1.,-1.95511867169517E-16,0.)) ;
#98325 = DIRECTION('ref_axis',(1.95511867169517E-16,-1.,0.)) ;
#98326 = DIRECTION('center_axis',(1.,0.,0.)) ;
#98327 = DIRECTION('ref_axis',(0.,0.,-1.)) ;
#98328 = DIRECTION('center_axis',(0.,1.,0.)) ;
#98329 = DIRECTION('ref_axis',(1.,0.,0.)) ;
#98330 = DIRECTION('center_axis',(1.22663473334668E-14,-1.,0.)) ;
#98331 = DIRECTION('ref_axis',(1.,1.22663473334668E-14,0.)) ;
#98332 = DIRECTION('center_axis',(-1.95511867169517E-16,1.,0.)) ;
#98333 = DIRECTION('ref_axis',(-1.,-1.95511867169517E-16,0.)) ;
#98334 = DIRECTION('center_axis',(0.,-1.,0.)) ;
#98335 = DIRECTION('ref_axis',(0.,0.,-1.)) ;
#98336 = DIRECTION('center_axis',(0.,1.,0.)) ;
#98337 = DIRECTION('ref_axis',(1.,0.,0.)) ;
#98338 = DIRECTION('center_axis',(-1.,0.,0.)) ;
#98339 = DIRECTION('ref_axis',(0.,0.,1.)) ;
#98340 = DIRECTION('center_axis',(1.,-1.06642836637918E-16,0.)) ;
#98341 = DIRECTION('ref_axis',(1.06642836637918E-16,1.,0.)) ;
#98342 = DIRECTION('center_axis',(1.,1.95511867169517E-16,0.)) ;
#98343 = DIRECTION('ref_axis',(-1.95511867169517E-16,1.,0.)) ;
#98344 = DIRECTION('center_axis',(1.,0.,0.)) ;
#98345 = DIRECTION('ref_axis',(0.,0.,-1.)) ;
#98346 = DIRECTION('center_axis',(0.,1.,0.)) ;
#98347 = DIRECTION('ref_axis',(1.,0.,0.)) ;
#98348 = DIRECTION('center_axis',(-8.43311379175855E-15,-1.,0.)) ;
#98349 = DIRECTION('ref_axis',(1.,-8.43311379175855E-15,0.)) ;
#98350 = DIRECTION('center_axis',(-1.95511867169517E-16,1.,0.)) ;
#98351 = DIRECTION('ref_axis',(-1.,-1.95511867169517E-16,0.)) ;
#98352 = DIRECTION('center_axis',(0.,-1.,0.)) ;
#98353 = DIRECTION('ref_axis',(0.,0.,-1.)) ;
#98354 = DIRECTION('center_axis',(-1.,1.06642836637918E-16,0.)) ;
#98355 = DIRECTION('ref_axis',(-1.06642836637918E-16,-1.,0.)) ;
#98356 = DIRECTION('center_axis',(1.,0.,0.)) ;
#98357 = DIRECTION('ref_axis',(0.,0.,-1.)) ;
#98358 = DIRECTION('center_axis',(0.,1.,0.)) ;
#98359 = DIRECTION('ref_axis',(1.,0.,0.)) ;
#98360 = DIRECTION('center_axis',(0.,0.,1.)) ;
#98361 = DIRECTION('ref_axis',(1.,0.,0.)) ;
#98362 = DIRECTION('center_axis',(0.,-1.,0.)) ;
#98363 = DIRECTION('ref_axis',(0.,0.,-1.)) ;
#98364 = DIRECTION('center_axis',(9.85638338623186E-18,1.,0.)) ;
#98365 = DIRECTION('ref_axis',(-1.,9.85638338623186E-18,0.)) ;
#98366 = DIRECTION('center_axis',(0.,-1.,0.)) ;
#98367 = DIRECTION('ref_axis',(0.,0.,-1.)) ;
#98368 = DIRECTION('center_axis',(0.,1.,0.)) ;
#98369 = DIRECTION('ref_axis',(1.,0.,0.)) ;
#98370 = DIRECTION('center_axis',(-1.,4.59988025005012E-15,0.)) ;
#98371 = DIRECTION('ref_axis',(-4.59988025005012E-15,-1.,0.)) ;
#98372 = DIRECTION('center_axis',(1.,-9.85638338623186E-18,0.)) ;
#98373 = DIRECTION('ref_axis',(9.85638338623186E-18,1.,0.)) ;
#98374 = DIRECTION('center_axis',(-1.,0.,0.)) ;
#98375 = DIRECTION('ref_axis',(0.,0.,1.)) ;
#98376 = DIRECTION('center_axis',(0.,1.,0.)) ;
#98377 = DIRECTION('ref_axis',(1.,0.,0.)) ;
#98378 = DIRECTION('center_axis',(0.,1.,0.)) ;
#98379 = DIRECTION('ref_axis',(0.,0.,1.)) ;
#98380 = DIRECTION('center_axis',(-9.85638338623186E-18,-1.,0.)) ;
#98381 = DIRECTION('ref_axis',(1.,-9.85638338623186E-18,0.)) ;
#98382 = DIRECTION('center_axis',(0.,1.,0.)) ;
#98383 = DIRECTION('ref_axis',(0.,0.,1.)) ;
#98384 = DIRECTION('center_axis',(0.,0.,1.)) ;
#98385 = DIRECTION('ref_axis',(1.,0.,0.)) ;
#98386 = DIRECTION('center_axis',(0.,0.,1.)) ;
#98387 = DIRECTION('ref_axis',(1.,0.,0.)) ;
#98388 = DIRECTION('center_axis',(0.,-1.,0.)) ;
#98389 = DIRECTION('ref_axis',(0.,0.,-1.)) ;
#98390 = DIRECTION('center_axis',(-9.85638338623186E-18,-1.,0.)) ;
#98391 = DIRECTION('ref_axis',(1.,-9.85638338623186E-18,0.)) ;
#98392 = DIRECTION('center_axis',(0.,-1.,0.)) ;
#98393 = DIRECTION('ref_axis',(0.,0.,-1.)) ;
#98394 = DIRECTION('center_axis',(0.,1.,0.)) ;
#98395 = DIRECTION('ref_axis',(1.,0.,0.)) ;
#98396 = DIRECTION('center_axis',(1.,-6.13317366673349E-15,0.)) ;
#98397 = DIRECTION('ref_axis',(6.13317366673349E-15,1.,0.)) ;
#98398 = DIRECTION('center_axis',(1.,-9.85638338623186E-18,0.)) ;
#98399 = DIRECTION('ref_axis',(9.85638338623186E-18,1.,0.)) ;
#98400 = DIRECTION('center_axis',(1.,0.,0.)) ;
#98401 = DIRECTION('ref_axis',(0.,0.,-1.)) ;
#98402 = DIRECTION('center_axis',(0.,1.,0.)) ;
#98403 = DIRECTION('ref_axis',(1.,0.,0.)) ;
#98404 = DIRECTION('center_axis',(0.,1.,0.)) ;
#98405 = DIRECTION('ref_axis',(0.,0.,1.)) ;
#98406 = DIRECTION('center_axis',(-9.85638338623186E-18,-1.,0.)) ;
#98407 = DIRECTION('ref_axis',(1.,-9.85638338623186E-18,0.)) ;
#98408 = DIRECTION('center_axis',(0.,1.,0.)) ;
#98409 = DIRECTION('ref_axis',(0.,0.,1.)) ;
#98410 = DIRECTION('center_axis',(0.,0.,1.)) ;
#98411 = DIRECTION('ref_axis',(1.,0.,0.)) ;
#98412 = DIRECTION('center_axis',(-1.,-1.95511867169517E-16,0.)) ;
#98413 = DIRECTION('ref_axis',(1.95511867169517E-16,-1.,0.)) ;
#98414 = DIRECTION('center_axis',(1.,0.,0.)) ;
#98415 = DIRECTION('ref_axis',(0.,0.,-1.)) ;
#98416 = DIRECTION('center_axis',(0.,1.,0.)) ;
#98417 = DIRECTION('ref_axis',(1.,0.,0.)) ;
#98418 = DIRECTION('center_axis',(1.22663473334668E-14,-1.,0.)) ;
#98419 = DIRECTION('ref_axis',(1.,1.22663473334668E-14,0.)) ;
#98420 = DIRECTION('center_axis',(-1.95511867169517E-16,1.,0.)) ;
#98421 = DIRECTION('ref_axis',(-1.,-1.95511867169517E-16,0.)) ;
#98422 = DIRECTION('center_axis',(0.,-1.,0.)) ;
#98423 = DIRECTION('ref_axis',(0.,0.,-1.)) ;
#98424 = DIRECTION('center_axis',(0.,1.,0.)) ;
#98425 = DIRECTION('ref_axis',(1.,0.,0.)) ;
#98426 = DIRECTION('center_axis',(-1.,0.,0.)) ;
#98427 = DIRECTION('ref_axis',(0.,0.,1.)) ;
#98428 = DIRECTION('center_axis',(1.,-1.06642836637918E-16,0.)) ;
#98429 = DIRECTION('ref_axis',(1.06642836637918E-16,1.,0.)) ;
#98430 = DIRECTION('center_axis',(1.,1.95511867169517E-16,0.)) ;
#98431 = DIRECTION('ref_axis',(-1.95511867169517E-16,1.,0.)) ;
#98432 = DIRECTION('center_axis',(1.,0.,0.)) ;
#98433 = DIRECTION('ref_axis',(0.,0.,-1.)) ;
#98434 = DIRECTION('center_axis',(0.,1.,0.)) ;
#98435 = DIRECTION('ref_axis',(1.,0.,0.)) ;
#98436 = DIRECTION('center_axis',(-8.43311379175855E-15,-1.,0.)) ;
#98437 = DIRECTION('ref_axis',(1.,-8.43311379175855E-15,0.)) ;
#98438 = DIRECTION('center_axis',(-1.95511867169517E-16,1.,0.)) ;
#98439 = DIRECTION('ref_axis',(-1.,-1.95511867169517E-16,0.)) ;
#98440 = DIRECTION('center_axis',(0.,-1.,0.)) ;
#98441 = DIRECTION('ref_axis',(0.,0.,-1.)) ;
#98442 = DIRECTION('center_axis',(-1.,1.06642836637918E-16,0.)) ;
#98443 = DIRECTION('ref_axis',(-1.06642836637918E-16,-1.,0.)) ;
#98444 = DIRECTION('center_axis',(1.,0.,0.)) ;
#98445 = DIRECTION('ref_axis',(0.,0.,-1.)) ;
#98446 = DIRECTION('center_axis',(0.,1.,0.)) ;
#98447 = DIRECTION('ref_axis',(1.,0.,0.)) ;
#98448 = DIRECTION('center_axis',(0.,0.,1.)) ;
#98449 = DIRECTION('ref_axis',(1.,0.,0.)) ;
#98450 = DIRECTION('center_axis',(0.,-1.,0.)) ;
#98451 = DIRECTION('ref_axis',(0.,0.,-1.)) ;
#98452 = DIRECTION('center_axis',(9.85638338623186E-18,1.,0.)) ;
#98453 = DIRECTION('ref_axis',(-1.,9.85638338623186E-18,0.)) ;
#98454 = DIRECTION('center_axis',(0.,-1.,0.)) ;
#98455 = DIRECTION('ref_axis',(0.,0.,-1.)) ;
#98456 = DIRECTION('center_axis',(0.,1.,0.)) ;
#98457 = DIRECTION('ref_axis',(1.,0.,0.)) ;
#98458 = DIRECTION('center_axis',(-1.,4.59988025005012E-15,0.)) ;
#98459 = DIRECTION('ref_axis',(-4.59988025005012E-15,-1.,0.)) ;
#98460 = DIRECTION('center_axis',(1.,-9.85638338623186E-18,0.)) ;
#98461 = DIRECTION('ref_axis',(9.85638338623186E-18,1.,0.)) ;
#98462 = DIRECTION('center_axis',(-1.,0.,0.)) ;
#98463 = DIRECTION('ref_axis',(0.,0.,1.)) ;
#98464 = DIRECTION('center_axis',(0.,1.,0.)) ;
#98465 = DIRECTION('ref_axis',(1.,0.,0.)) ;
#98466 = DIRECTION('center_axis',(0.,1.,0.)) ;
#98467 = DIRECTION('ref_axis',(0.,0.,1.)) ;
#98468 = DIRECTION('center_axis',(-9.85638338623186E-18,-1.,0.)) ;
#98469 = DIRECTION('ref_axis',(1.,-9.85638338623186E-18,0.)) ;
#98470 = DIRECTION('center_axis',(0.,1.,0.)) ;
#98471 = DIRECTION('ref_axis',(0.,0.,1.)) ;
#98472 = DIRECTION('center_axis',(0.,0.,1.)) ;
#98473 = DIRECTION('ref_axis',(1.,0.,0.)) ;
#98474 = DIRECTION('center_axis',(0.,0.,1.)) ;
#98475 = DIRECTION('ref_axis',(1.,0.,0.)) ;
#98476 = DIRECTION('center_axis',(0.,-1.,0.)) ;
#98477 = DIRECTION('ref_axis',(0.,0.,-1.)) ;
#98478 = DIRECTION('center_axis',(-9.85638338623186E-18,-1.,0.)) ;
#98479 = DIRECTION('ref_axis',(1.,-9.85638338623186E-18,0.)) ;
#98480 = DIRECTION('center_axis',(0.,-1.,0.)) ;
#98481 = DIRECTION('ref_axis',(0.,0.,-1.)) ;
#98482 = DIRECTION('center_axis',(0.,1.,0.)) ;
#98483 = DIRECTION('ref_axis',(1.,0.,0.)) ;
#98484 = DIRECTION('center_axis',(1.,-6.13317366673349E-15,0.)) ;
#98485 = DIRECTION('ref_axis',(6.13317366673349E-15,1.,0.)) ;
#98486 = DIRECTION('center_axis',(1.,-9.85638338623186E-18,0.)) ;
#98487 = DIRECTION('ref_axis',(9.85638338623186E-18,1.,0.)) ;
#98488 = DIRECTION('center_axis',(1.,0.,0.)) ;
#98489 = DIRECTION('ref_axis',(0.,0.,-1.)) ;
#98490 = DIRECTION('center_axis',(0.,1.,0.)) ;
#98491 = DIRECTION('ref_axis',(1.,0.,0.)) ;
#98492 = DIRECTION('center_axis',(0.,1.,0.)) ;
#98493 = DIRECTION('ref_axis',(0.,0.,1.)) ;
#98494 = DIRECTION('center_axis',(-9.85638338623186E-18,-1.,0.)) ;
#98495 = DIRECTION('ref_axis',(1.,-9.85638338623186E-18,0.)) ;
#98496 = DIRECTION('center_axis',(0.,1.,0.)) ;
#98497 = DIRECTION('ref_axis',(0.,0.,1.)) ;
#98498 = DIRECTION('center_axis',(0.,0.,1.)) ;
#98499 = DIRECTION('ref_axis',(1.,0.,0.)) ;
#98500 = DIRECTION('center_axis',(-1.,-1.95511867169517E-16,0.)) ;
#98501 = DIRECTION('ref_axis',(1.95511867169517E-16,-1.,0.)) ;
#98502 = DIRECTION('center_axis',(1.,0.,0.)) ;
#98503 = DIRECTION('ref_axis',(0.,0.,-1.)) ;
#98504 = DIRECTION('center_axis',(0.,1.,0.)) ;
#98505 = DIRECTION('ref_axis',(1.,0.,0.)) ;
#98506 = DIRECTION('center_axis',(1.22663473334668E-14,-1.,0.)) ;
#98507 = DIRECTION('ref_axis',(1.,1.22663473334668E-14,0.)) ;
#98508 = DIRECTION('center_axis',(-1.95511867169517E-16,1.,0.)) ;
#98509 = DIRECTION('ref_axis',(-1.,-1.95511867169517E-16,0.)) ;
#98510 = DIRECTION('center_axis',(0.,-1.,0.)) ;
#98511 = DIRECTION('ref_axis',(0.,0.,-1.)) ;
#98512 = DIRECTION('center_axis',(0.,1.,0.)) ;
#98513 = DIRECTION('ref_axis',(1.,0.,0.)) ;
#98514 = DIRECTION('center_axis',(-1.,0.,0.)) ;
#98515 = DIRECTION('ref_axis',(0.,0.,1.)) ;
#98516 = DIRECTION('center_axis',(1.,-1.06642836637918E-16,0.)) ;
#98517 = DIRECTION('ref_axis',(1.06642836637918E-16,1.,0.)) ;
#98518 = DIRECTION('center_axis',(1.,1.95511867169517E-16,0.)) ;
#98519 = DIRECTION('ref_axis',(-1.95511867169517E-16,1.,0.)) ;
#98520 = DIRECTION('center_axis',(1.,0.,0.)) ;
#98521 = DIRECTION('ref_axis',(0.,0.,-1.)) ;
#98522 = DIRECTION('center_axis',(0.,1.,0.)) ;
#98523 = DIRECTION('ref_axis',(1.,0.,0.)) ;
#98524 = DIRECTION('center_axis',(-8.43311379175855E-15,-1.,0.)) ;
#98525 = DIRECTION('ref_axis',(1.,-8.43311379175855E-15,0.)) ;
#98526 = DIRECTION('center_axis',(-1.95511867169517E-16,1.,0.)) ;
#98527 = DIRECTION('ref_axis',(-1.,-1.95511867169517E-16,0.)) ;
#98528 = DIRECTION('center_axis',(0.,-1.,0.)) ;
#98529 = DIRECTION('ref_axis',(0.,0.,-1.)) ;
#98530 = DIRECTION('center_axis',(-1.,1.06642836637918E-16,0.)) ;
#98531 = DIRECTION('ref_axis',(-1.06642836637918E-16,-1.,0.)) ;
#98532 = DIRECTION('center_axis',(1.,0.,0.)) ;
#98533 = DIRECTION('ref_axis',(0.,0.,-1.)) ;
#98534 = DIRECTION('center_axis',(0.,1.,0.)) ;
#98535 = DIRECTION('ref_axis',(1.,0.,0.)) ;
#98536 = DIRECTION('center_axis',(0.,0.,1.)) ;
#98537 = DIRECTION('ref_axis',(1.,0.,0.)) ;
#98538 = DIRECTION('center_axis',(0.,-1.,0.)) ;
#98539 = DIRECTION('ref_axis',(0.,0.,-1.)) ;
#98540 = DIRECTION('center_axis',(9.85638338623186E-18,1.,0.)) ;
#98541 = DIRECTION('ref_axis',(-1.,9.85638338623186E-18,0.)) ;
#98542 = DIRECTION('center_axis',(0.,-1.,0.)) ;
#98543 = DIRECTION('ref_axis',(0.,0.,-1.)) ;
#98544 = DIRECTION('center_axis',(0.,1.,0.)) ;
#98545 = DIRECTION('ref_axis',(1.,0.,0.)) ;
#98546 = DIRECTION('center_axis',(-1.,4.59988025005012E-15,0.)) ;
#98547 = DIRECTION('ref_axis',(-4.59988025005012E-15,-1.,0.)) ;
#98548 = DIRECTION('center_axis',(1.,-9.85638338623186E-18,0.)) ;
#98549 = DIRECTION('ref_axis',(9.85638338623186E-18,1.,0.)) ;
#98550 = DIRECTION('center_axis',(-1.,0.,0.)) ;
#98551 = DIRECTION('ref_axis',(0.,0.,1.)) ;
#98552 = DIRECTION('center_axis',(0.,1.,0.)) ;
#98553 = DIRECTION('ref_axis',(1.,0.,0.)) ;
#98554 = DIRECTION('center_axis',(0.,1.,0.)) ;
#98555 = DIRECTION('ref_axis',(0.,0.,1.)) ;
#98556 = DIRECTION('center_axis',(-9.85638338623186E-18,-1.,0.)) ;
#98557 = DIRECTION('ref_axis',(1.,-9.85638338623186E-18,0.)) ;
#98558 = DIRECTION('center_axis',(0.,1.,0.)) ;
#98559 = DIRECTION('ref_axis',(0.,0.,1.)) ;
#98560 = DIRECTION('center_axis',(0.,0.,1.)) ;
#98561 = DIRECTION('ref_axis',(1.,0.,0.)) ;
#98562 = DIRECTION('center_axis',(0.,0.,1.)) ;
#98563 = DIRECTION('ref_axis',(1.,0.,0.)) ;
#98564 = DIRECTION('center_axis',(0.,-1.,0.)) ;
#98565 = DIRECTION('ref_axis',(0.,0.,-1.)) ;
#98566 = DIRECTION('center_axis',(-9.85638338623186E-18,-1.,0.)) ;
#98567 = DIRECTION('ref_axis',(1.,-9.85638338623186E-18,0.)) ;
#98568 = DIRECTION('center_axis',(0.,-1.,0.)) ;
#98569 = DIRECTION('ref_axis',(0.,0.,-1.)) ;
#98570 = DIRECTION('center_axis',(0.,1.,0.)) ;
#98571 = DIRECTION('ref_axis',(1.,0.,0.)) ;
#98572 = DIRECTION('center_axis',(1.,-6.13317366673349E-15,0.)) ;
#98573 = DIRECTION('ref_axis',(6.13317366673349E-15,1.,0.)) ;
#98574 = DIRECTION('center_axis',(1.,-9.85638338623186E-18,0.)) ;
#98575 = DIRECTION('ref_axis',(9.85638338623186E-18,1.,0.)) ;
#98576 = DIRECTION('center_axis',(1.,0.,0.)) ;
#98577 = DIRECTION('ref_axis',(0.,0.,-1.)) ;
#98578 = DIRECTION('center_axis',(0.,1.,0.)) ;
#98579 = DIRECTION('ref_axis',(1.,0.,0.)) ;
#98580 = DIRECTION('center_axis',(0.,1.,0.)) ;
#98581 = DIRECTION('ref_axis',(0.,0.,1.)) ;
#98582 = DIRECTION('center_axis',(-9.85638338623186E-18,-1.,0.)) ;
#98583 = DIRECTION('ref_axis',(1.,-9.85638338623186E-18,0.)) ;
#98584 = DIRECTION('center_axis',(0.,1.,0.)) ;
#98585 = DIRECTION('ref_axis',(0.,0.,1.)) ;
#98586 = DIRECTION('center_axis',(0.,0.,1.)) ;
#98587 = DIRECTION('ref_axis',(1.,0.,0.)) ;
#98588 = DIRECTION('center_axis',(-1.,-1.95511867169517E-16,0.)) ;
#98589 = DIRECTION('ref_axis',(1.95511867169517E-16,-1.,0.)) ;
#98590 = DIRECTION('center_axis',(1.,0.,0.)) ;
#98591 = DIRECTION('ref_axis',(0.,0.,-1.)) ;
#98592 = DIRECTION('center_axis',(0.,1.,0.)) ;
#98593 = DIRECTION('ref_axis',(1.,0.,0.)) ;
#98594 = DIRECTION('center_axis',(1.22663473334668E-14,-1.,0.)) ;
#98595 = DIRECTION('ref_axis',(1.,1.22663473334668E-14,0.)) ;
#98596 = DIRECTION('center_axis',(-1.95511867169517E-16,1.,0.)) ;
#98597 = DIRECTION('ref_axis',(-1.,-1.95511867169517E-16,0.)) ;
#98598 = DIRECTION('center_axis',(0.,-1.,0.)) ;
#98599 = DIRECTION('ref_axis',(0.,0.,-1.)) ;
#98600 = DIRECTION('center_axis',(0.,1.,0.)) ;
#98601 = DIRECTION('ref_axis',(1.,0.,0.)) ;
#98602 = DIRECTION('center_axis',(-1.,0.,0.)) ;
#98603 = DIRECTION('ref_axis',(0.,0.,1.)) ;
#98604 = DIRECTION('center_axis',(1.,-1.06642836637918E-16,0.)) ;
#98605 = DIRECTION('ref_axis',(1.06642836637918E-16,1.,0.)) ;
#98606 = DIRECTION('center_axis',(1.,1.95511867169517E-16,0.)) ;
#98607 = DIRECTION('ref_axis',(-1.95511867169517E-16,1.,0.)) ;
#98608 = DIRECTION('center_axis',(1.,0.,0.)) ;
#98609 = DIRECTION('ref_axis',(0.,0.,-1.)) ;
#98610 = DIRECTION('center_axis',(0.,1.,0.)) ;
#98611 = DIRECTION('ref_axis',(1.,0.,0.)) ;
#98612 = DIRECTION('center_axis',(-8.43311379175855E-15,-1.,0.)) ;
#98613 = DIRECTION('ref_axis',(1.,-8.43311379175855E-15,0.)) ;
#98614 = DIRECTION('center_axis',(-1.95511867169517E-16,1.,0.)) ;
#98615 = DIRECTION('ref_axis',(-1.,-1.95511867169517E-16,0.)) ;
#98616 = DIRECTION('center_axis',(0.,-1.,0.)) ;
#98617 = DIRECTION('ref_axis',(0.,0.,-1.)) ;
#98618 = DIRECTION('center_axis',(-1.,1.06642836637918E-16,0.)) ;
#98619 = DIRECTION('ref_axis',(-1.06642836637918E-16,-1.,0.)) ;
#98620 = DIRECTION('center_axis',(1.,0.,0.)) ;
#98621 = DIRECTION('ref_axis',(0.,0.,-1.)) ;
#98622 = DIRECTION('center_axis',(0.,1.,0.)) ;
#98623 = DIRECTION('ref_axis',(1.,0.,0.)) ;
#98624 = DIRECTION('center_axis',(0.,0.,1.)) ;
#98625 = DIRECTION('ref_axis',(1.,0.,0.)) ;
#98626 = DIRECTION('center_axis',(0.,-1.,0.)) ;
#98627 = DIRECTION('ref_axis',(0.,0.,-1.)) ;
#98628 = DIRECTION('center_axis',(9.85638338623186E-18,1.,0.)) ;
#98629 = DIRECTION('ref_axis',(-1.,9.85638338623186E-18,0.)) ;
#98630 = DIRECTION('center_axis',(0.,-1.,0.)) ;
#98631 = DIRECTION('ref_axis',(0.,0.,-1.)) ;
#98632 = DIRECTION('center_axis',(0.,1.,0.)) ;
#98633 = DIRECTION('ref_axis',(1.,0.,0.)) ;
#98634 = DIRECTION('center_axis',(-1.,1.83995210002007E-14,0.)) ;
#98635 = DIRECTION('ref_axis',(-1.83995210002007E-14,-1.,0.)) ;
#98636 = DIRECTION('center_axis',(1.,-9.85638338623186E-18,0.)) ;
#98637 = DIRECTION('ref_axis',(9.85638338623186E-18,1.,0.)) ;
#98638 = DIRECTION('center_axis',(-1.,0.,0.)) ;
#98639 = DIRECTION('ref_axis',(0.,0.,1.)) ;
#98640 = DIRECTION('center_axis',(0.,1.,0.)) ;
#98641 = DIRECTION('ref_axis',(1.,0.,0.)) ;
#98642 = DIRECTION('center_axis',(0.,1.,0.)) ;
#98643 = DIRECTION('ref_axis',(0.,0.,1.)) ;
#98644 = DIRECTION('center_axis',(-9.85638338623186E-18,-1.,0.)) ;
#98645 = DIRECTION('ref_axis',(1.,-9.85638338623186E-18,0.)) ;
#98646 = DIRECTION('center_axis',(0.,1.,0.)) ;
#98647 = DIRECTION('ref_axis',(0.,0.,1.)) ;
#98648 = DIRECTION('center_axis',(0.,0.,1.)) ;
#98649 = DIRECTION('ref_axis',(1.,0.,0.)) ;
#98650 = DIRECTION('center_axis',(0.,0.,1.)) ;
#98651 = DIRECTION('ref_axis',(1.,0.,0.)) ;
#98652 = DIRECTION('center_axis',(0.,-1.,0.)) ;
#98653 = DIRECTION('ref_axis',(0.,0.,-1.)) ;
#98654 = DIRECTION('center_axis',(-9.85638338623186E-18,-1.,0.)) ;
#98655 = DIRECTION('ref_axis',(1.,-9.85638338623186E-18,0.)) ;
#98656 = DIRECTION('center_axis',(0.,-1.,0.)) ;
#98657 = DIRECTION('ref_axis',(0.,0.,-1.)) ;
#98658 = DIRECTION('center_axis',(0.,1.,0.)) ;
#98659 = DIRECTION('ref_axis',(1.,0.,0.)) ;
#98660 = DIRECTION('center_axis',(1.,2.22327545419092E-14,0.)) ;
#98661 = DIRECTION('ref_axis',(-2.22327545419092E-14,1.,0.)) ;
#98662 = DIRECTION('center_axis',(1.,-9.85638338623186E-18,0.)) ;
#98663 = DIRECTION('ref_axis',(9.85638338623186E-18,1.,0.)) ;
#98664 = DIRECTION('center_axis',(1.,0.,0.)) ;
#98665 = DIRECTION('ref_axis',(0.,0.,-1.)) ;
#98666 = DIRECTION('center_axis',(0.,1.,0.)) ;
#98667 = DIRECTION('ref_axis',(1.,0.,0.)) ;
#98668 = DIRECTION('center_axis',(0.,1.,0.)) ;
#98669 = DIRECTION('ref_axis',(0.,0.,1.)) ;
#98670 = DIRECTION('center_axis',(-9.85638338623186E-18,-1.,0.)) ;
#98671 = DIRECTION('ref_axis',(1.,-9.85638338623186E-18,0.)) ;
#98672 = DIRECTION('center_axis',(0.,1.,0.)) ;
#98673 = DIRECTION('ref_axis',(0.,0.,1.)) ;
#98674 = DIRECTION('center_axis',(0.,0.,1.)) ;
#98675 = DIRECTION('ref_axis',(1.,0.,0.)) ;
#98676 = DIRECTION('center_axis',(-1.,-1.95511867169517E-16,0.)) ;
#98677 = DIRECTION('ref_axis',(1.95511867169517E-16,-1.,0.)) ;
#98678 = DIRECTION('center_axis',(1.,0.,0.)) ;
#98679 = DIRECTION('ref_axis',(0.,0.,-1.)) ;
#98680 = DIRECTION('center_axis',(0.,1.,0.)) ;
#98681 = DIRECTION('ref_axis',(1.,0.,0.)) ;
#98682 = DIRECTION('center_axis',(-1.83995210002007E-14,-1.,0.)) ;
#98683 = DIRECTION('ref_axis',(1.,-1.83995210002007E-14,0.)) ;
#98684 = DIRECTION('center_axis',(-1.95511867169517E-16,1.,0.)) ;
#98685 = DIRECTION('ref_axis',(-1.,-1.95511867169517E-16,0.)) ;
#98686 = DIRECTION('center_axis',(0.,-1.,0.)) ;
#98687 = DIRECTION('ref_axis',(0.,0.,-1.)) ;
#98688 = DIRECTION('center_axis',(0.,1.,0.)) ;
#98689 = DIRECTION('ref_axis',(1.,0.,0.)) ;
#98690 = DIRECTION('center_axis',(-1.,0.,0.)) ;
#98691 = DIRECTION('ref_axis',(0.,0.,1.)) ;
#98692 = DIRECTION('center_axis',(1.,-1.06642836637918E-16,0.)) ;
#98693 = DIRECTION('ref_axis',(1.06642836637918E-16,1.,0.)) ;
#98694 = DIRECTION('center_axis',(1.,1.95511867169517E-16,0.)) ;
#98695 = DIRECTION('ref_axis',(-1.95511867169517E-16,1.,0.)) ;
#98696 = DIRECTION('center_axis',(1.,0.,0.)) ;
#98697 = DIRECTION('ref_axis',(0.,0.,-1.)) ;
#98698 = DIRECTION('center_axis',(0.,1.,0.)) ;
#98699 = DIRECTION('ref_axis',(1.,0.,0.)) ;
#98700 = DIRECTION('center_axis',(2.68326347919587E-14,-1.,0.)) ;
#98701 = DIRECTION('ref_axis',(1.,2.68326347919587E-14,0.)) ;
#98702 = DIRECTION('center_axis',(-1.95511867169517E-16,1.,0.)) ;
#98703 = DIRECTION('ref_axis',(-1.,-1.95511867169517E-16,0.)) ;
#98704 = DIRECTION('center_axis',(0.,-1.,0.)) ;
#98705 = DIRECTION('ref_axis',(0.,0.,-1.)) ;
#98706 = DIRECTION('center_axis',(-1.,1.06642836637918E-16,0.)) ;
#98707 = DIRECTION('ref_axis',(-1.06642836637918E-16,-1.,0.)) ;
#98708 = DIRECTION('center_axis',(1.,0.,0.)) ;
#98709 = DIRECTION('ref_axis',(0.,0.,-1.)) ;
#98710 = DIRECTION('center_axis',(0.,1.,0.)) ;
#98711 = DIRECTION('ref_axis',(1.,0.,0.)) ;
#98712 = DIRECTION('axis',(0.,0.,1.)) ;
#98713 = DIRECTION('refdir',(1.,0.,0.)) ;
#98714 = DIRECTION('center_axis',(0.,-1.,0.)) ;
#98715 = DIRECTION('ref_axis',(1.,0.,2.2577126443575E-16)) ;
#98716 = DIRECTION('',(0.,1.,0.)) ;
#98717 = DIRECTION('',(2.50091441307106E-5,0.999999996725694,7.6962037204612E-5)) ;
#98718 = DIRECTION('center_axis',(0.,-1.,0.)) ;
#98719 = DIRECTION('ref_axis',(1.,0.,2.2577126443575E-16)) ;
#98720 = DIRECTION('',(0.,1.,0.)) ;
#98721 = DIRECTION('center_axis',(0.,-1.,0.)) ;
#98722 = DIRECTION('ref_axis',(1.,0.,2.2577126443575E-16)) ;
#98723 = DIRECTION('',(0.,1.,0.)) ;
#98724 = DIRECTION('center_axis',(0.,-1.,0.)) ;
#98725 = DIRECTION('ref_axis',(1.,0.,2.2577126443575E-16)) ;
#98726 = DIRECTION('',(0.,1.,0.)) ;
#98727 = DIRECTION('center_axis',(0.,-1.,0.)) ;
#98728 = DIRECTION('ref_axis',(1.,0.,2.2577126443575E-16)) ;
#98729 = DIRECTION('',(0.,1.,0.)) ;
#98730 = DIRECTION('center_axis',(0.,-1.,0.)) ;
#98731 = DIRECTION('ref_axis',(1.,0.,2.2577126443575E-16)) ;
#98732 = DIRECTION('',(0.,1.,0.)) ;
#98733 = DIRECTION('center_axis',(0.,-1.,0.)) ;
#98734 = DIRECTION('ref_axis',(1.,0.,2.2577126443575E-16)) ;
#98735 = DIRECTION('',(0.,1.,0.)) ;
#98736 = DIRECTION('center_axis',(0.,-1.,0.)) ;
#98737 = DIRECTION('ref_axis',(1.,0.,2.2577126443575E-16)) ;
#98738 = DIRECTION('',(0.,1.,0.)) ;
#98739 = DIRECTION('center_axis',(0.,-1.,0.)) ;
#98740 = DIRECTION('ref_axis',(1.,0.,2.2577126443575E-16)) ;
#98741 = DIRECTION('',(0.,1.,0.)) ;
#98742 = DIRECTION('center_axis',(0.,-1.,0.)) ;
#98743 = DIRECTION('ref_axis',(1.,0.,2.2577126443575E-16)) ;
#98744 = DIRECTION('',(0.,1.,0.)) ;
#98745 = DIRECTION('center_axis',(0.,1.,0.)) ;
#98746 = DIRECTION('ref_axis',(0.,0.,1.)) ;
#98747 = DIRECTION('',(0.,-1.,0.)) ;
#98748 = DIRECTION('center_axis',(0.,1.,0.)) ;
#98749 = DIRECTION('ref_axis',(0.,0.,-1.)) ;
#98750 = DIRECTION('center_axis',(0.,1.,0.)) ;
#98751 = DIRECTION('ref_axis',(0.,0.,1.)) ;
#98752 = DIRECTION('',(0.,-1.,0.)) ;
#98753 = DIRECTION('center_axis',(0.,1.,0.)) ;
#98754 = DIRECTION('ref_axis',(0.,0.,1.)) ;
#98755 = DIRECTION('',(0.,-1.,0.)) ;
#98756 = DIRECTION('center_axis',(0.,1.,0.)) ;
#98757 = DIRECTION('ref_axis',(0.,0.,1.)) ;
#98758 = DIRECTION('',(0.,-1.,0.)) ;
#98759 = DIRECTION('center_axis',(0.,1.,0.)) ;
#98760 = DIRECTION('ref_axis',(0.,0.,1.)) ;
#98761 = DIRECTION('',(0.,-1.,0.)) ;
#98762 = DIRECTION('center_axis',(0.,1.,0.)) ;
#98763 = DIRECTION('ref_axis',(0.,0.,1.)) ;
#98764 = DIRECTION('',(0.,-1.,0.)) ;
#98765 = DIRECTION('center_axis',(0.,1.,0.)) ;
#98766 = DIRECTION('ref_axis',(0.,0.,1.)) ;
#98767 = DIRECTION('',(0.,-1.,0.)) ;
#98768 = DIRECTION('center_axis',(0.,1.,0.)) ;
#98769 = DIRECTION('ref_axis',(0.,0.,1.)) ;
#98770 = DIRECTION('',(0.,-1.,0.)) ;
#98771 = DIRECTION('center_axis',(0.,1.,0.)) ;
#98772 = DIRECTION('ref_axis',(0.,0.,1.)) ;
#98773 = DIRECTION('center_axis',(0.,-1.,0.)) ;
#98774 = DIRECTION('ref_axis',(0.,0.,1.)) ;
#98775 = DIRECTION('',(0.,-1.,0.)) ;
#98776 = DIRECTION('center_axis',(-0.475489515607485,0.866028065754805,0.15461277396241)) ;
#98777 = DIRECTION('ref_axis',(-0.823582125550541,-0.499995389303733,0.26780047264458)) ;
#98778 = DIRECTION('',(-6.95778281854898E-9,-1.,-5.25180768870477E-9)) ;
#98779 = DIRECTION('center_axis',(-0.475585457889948,-0.866022400932201,0.154349192829876)) ;
#98780 = DIRECTION('ref_axis',(-0.823726751681711,0.500005201056575,0.267336936243893)) ;
#98781 = DIRECTION('',(0.,-1.,0.)) ;
#98782 = DIRECTION('center_axis',(0.,1.,0.)) ;
#98783 = DIRECTION('ref_axis',(0.,0.,1.)) ;
#98784 = DIRECTION('center_axis',(0.,-1.,0.)) ;
#98785 = DIRECTION('ref_axis',(1.,0.,2.2577126443575E-16)) ;
#98786 = DIRECTION('center_axis',(-1.42478674527368E-13,-1.,-3.7508514743183E-14)) ;
#98787 = DIRECTION('ref_axis',(0.798195139400692,-1.36320876135353E-13,0.602398970315447)) ;
#98788 = DIRECTION('center_axis',(0.,1.,0.)) ;
#98789 = DIRECTION('ref_axis',(0.,0.,1.)) ;
#98790 = DIRECTION('center_axis',(0.,1.,0.)) ;
#98791 = DIRECTION('ref_axis',(0.,0.,1.)) ;
#98792 = DIRECTION('',(-8.6595605623549E-17,0.70710678118655,-0.707106781186545)) ;
#98793 = DIRECTION('center_axis',(0.,1.,0.)) ;
#98794 = DIRECTION('ref_axis',(0.,0.,1.)) ;
#98795 = DIRECTION('center_axis',(0.,1.,0.)) ;
#98796 = DIRECTION('ref_axis',(0.,0.,1.)) ;
#98797 = DIRECTION('center_axis',(0.,1.,0.)) ;
#98798 = DIRECTION('ref_axis',(0.,0.,1.)) ;
#98799 = DIRECTION('',(0.,1.,0.)) ;
#98800 = DIRECTION('center_axis',(0.,1.,0.)) ;
#98801 = DIRECTION('ref_axis',(0.,0.,1.)) ;
#98802 = DIRECTION('',(-1.04972719113862E-16,0.515038074910058,-0.85716730070211)) ;
#98803 = DIRECTION('center_axis',(0.,1.,0.)) ;
#98804 = DIRECTION('ref_axis',(0.,0.,1.)) ;
#98805 = DIRECTION('center_axis',(0.,1.,0.)) ;
#98806 = DIRECTION('ref_axis',(0.,0.,1.)) ;
#98807 = DIRECTION('center_axis',(1.,0.,-1.22464679914735E-16)) ;
#98808 = DIRECTION('ref_axis',(-1.22464679914735E-16,0.,-1.)) ;
#98809 = DIRECTION('center_axis',(0.,1.,0.)) ;
#98810 = DIRECTION('ref_axis',(0.,0.,1.)) ;
#98811 = DIRECTION('',(8.65956056235491E-17,-0.707106781186549,0.707106781186546)) ;
#98812 = DIRECTION('center_axis',(0.,-1.,0.)) ;
#98813 = DIRECTION('ref_axis',(0.,0.,-1.)) ;
#98814 = DIRECTION('center_axis',(0.,-1.,0.)) ;
#98815 = DIRECTION('ref_axis',(0.,0.,-1.)) ;
#98816 = DIRECTION('',(0.,-1.,0.)) ;
#98817 = DIRECTION('center_axis',(0.,-1.,0.)) ;
#98818 = DIRECTION('ref_axis',(8.88178419700125E-16,0.,1.)) ;
#98819 = DIRECTION('',(0.,1.,0.)) ;
#98820 = DIRECTION('center_axis',(0.,1.,0.)) ;
#98821 = DIRECTION('ref_axis',(0.,0.,1.)) ;
#98822 = DIRECTION('center_axis',(0.,-1.,0.)) ;
#98823 = DIRECTION('ref_axis',(0.,0.,-1.)) ;
#98824 = DIRECTION('',(0.,1.,0.)) ;
#98825 = DIRECTION('center_axis',(0.,1.,0.)) ;
#98826 = DIRECTION('ref_axis',(0.,0.,1.)) ;
#98827 = DIRECTION('',(0.,-1.,0.)) ;
#98828 = DIRECTION('center_axis',(0.,-1.,0.)) ;
#98829 = DIRECTION('ref_axis',(1.4210854715202E-14,0.,1.)) ;
#98830 = DIRECTION('center_axis',(0.,-1.,0.)) ;
#98831 = DIRECTION('ref_axis',(0.,0.,-1.)) ;
#98832 = DIRECTION('',(0.,-1.,0.)) ;
#98833 = DIRECTION('center_axis',(0.,-1.,0.)) ;
#98834 = DIRECTION('ref_axis',(0.,0.,1.)) ;
#98835 = DIRECTION('',(0.,1.,0.)) ;
#98836 = DIRECTION('center_axis',(0.,1.,0.)) ;
#98837 = DIRECTION('ref_axis',(0.,0.,1.)) ;
#98838 = DIRECTION('center_axis',(0.,-1.,0.)) ;
#98839 = DIRECTION('ref_axis',(0.,0.,-1.)) ;
#98840 = DIRECTION('',(0.,-1.,0.)) ;
#98841 = DIRECTION('center_axis',(0.,-1.,0.)) ;
#98842 = DIRECTION('ref_axis',(0.,0.,1.)) ;
#98843 = DIRECTION('',(0.,1.,0.)) ;
#98844 = DIRECTION('center_axis',(0.,1.,0.)) ;
#98845 = DIRECTION('ref_axis',(0.,0.,1.)) ;
#98846 = DIRECTION('center_axis',(0.,-1.,0.)) ;
#98847 = DIRECTION('ref_axis',(0.,0.,-1.)) ;
#98848 = DIRECTION('',(0.,-1.,0.)) ;
#98849 = DIRECTION('center_axis',(0.,-1.,0.)) ;
#98850 = DIRECTION('ref_axis',(0.,0.,1.)) ;
#98851 = DIRECTION('',(0.,1.,0.)) ;
#98852 = DIRECTION('center_axis',(0.,1.,0.)) ;
#98853 = DIRECTION('ref_axis',(0.,0.,1.)) ;
#98854 = DIRECTION('center_axis',(0.,-1.,0.)) ;
#98855 = DIRECTION('ref_axis',(0.,0.,-1.)) ;
#98856 = DIRECTION('',(0.,-1.,0.)) ;
#98857 = DIRECTION('center_axis',(0.,-1.,0.)) ;
#98858 = DIRECTION('ref_axis',(0.,0.,1.)) ;
#98859 = DIRECTION('',(0.,1.,0.)) ;
#98860 = DIRECTION('center_axis',(0.,1.,0.)) ;
#98861 = DIRECTION('ref_axis',(0.,0.,1.)) ;
#98862 = DIRECTION('center_axis',(0.,1.,0.)) ;
#98863 = DIRECTION('ref_axis',(0.,0.,1.)) ;
#98864 = DIRECTION('center_axis',(0.,-1.,0.)) ;
#98865 = DIRECTION('ref_axis',(1.77635683940025E-15,0.,1.)) ;
#98866 = DIRECTION('center_axis',(0.,1.,0.)) ;
#98867 = DIRECTION('ref_axis',(0.,0.,1.)) ;
#98868 = DIRECTION('center_axis',(0.,-1.,0.)) ;
#98869 = DIRECTION('ref_axis',(-3.5527136788005E-15,0.,1.)) ;
#98870 = DIRECTION('center_axis',(0.,1.,0.)) ;
#98871 = DIRECTION('ref_axis',(0.,0.,1.)) ;
#98872 = DIRECTION('center_axis',(0.,-1.,0.)) ;
#98873 = DIRECTION('ref_axis',(0.,0.,1.)) ;
#98874 = DIRECTION('center_axis',(0.,1.,0.)) ;
#98875 = DIRECTION('ref_axis',(0.,0.,1.)) ;
#98876 = DIRECTION('center_axis',(0.,-1.,0.)) ;
#98877 = DIRECTION('ref_axis',(0.,0.,1.)) ;
#98878 = DIRECTION('center_axis',(0.,1.,0.)) ;
#98879 = DIRECTION('ref_axis',(0.,0.,1.)) ;
#98880 = DIRECTION('center_axis',(0.,-1.,0.)) ;
#98881 = DIRECTION('ref_axis',(1.77635683940025E-15,0.,1.)) ;
#98882 = DIRECTION('center_axis',(0.,1.,0.)) ;
#98883 = DIRECTION('ref_axis',(0.,0.,1.)) ;
#98884 = DIRECTION('center_axis',(0.,-1.,0.)) ;
#98885 = DIRECTION('ref_axis',(0.,0.,1.)) ;
#98886 = DIRECTION('center_axis',(0.,-1.,0.)) ;
#98887 = DIRECTION('ref_axis',(0.,0.,-1.)) ;
#98888 = DIRECTION('center_axis',(0.,1.,0.)) ;
#98889 = DIRECTION('ref_axis',(0.,0.,1.)) ;
#98890 = DIRECTION('center_axis',(0.,-1.,0.)) ;
#98891 = DIRECTION('ref_axis',(0.,0.,-1.)) ;
#98892 = DIRECTION('center_axis',(0.,1.,0.)) ;
#98893 = DIRECTION('ref_axis',(0.,0.,1.)) ;
#98894 = DIRECTION('center_axis',(0.,-1.,0.)) ;
#98895 = DIRECTION('ref_axis',(0.,0.,-1.)) ;
#98896 = DIRECTION('center_axis',(0.,1.,0.)) ;
#98897 = DIRECTION('ref_axis',(0.,0.,1.)) ;
#98898 = DIRECTION('center_axis',(0.,-1.,0.)) ;
#98899 = DIRECTION('ref_axis',(0.,0.,-1.)) ;
#98900 = DIRECTION('center_axis',(0.,1.,0.)) ;
#98901 = DIRECTION('ref_axis',(0.,0.,1.)) ;
#98902 = DIRECTION('center_axis',(0.,-1.,0.)) ;
#98903 = DIRECTION('ref_axis',(0.,0.,-1.)) ;
#98904 = DIRECTION('center_axis',(0.,1.,0.)) ;
#98905 = DIRECTION('ref_axis',(0.,0.,1.)) ;
#98906 = DIRECTION('center_axis',(0.,-1.,0.)) ;
#98907 = DIRECTION('ref_axis',(0.,0.,-1.)) ;
#98908 = DIRECTION('center_axis',(0.,1.,0.)) ;
#98909 = DIRECTION('ref_axis',(0.,0.,1.)) ;
#98910 = DIRECTION('center_axis',(0.,1.,0.)) ;
#98911 = DIRECTION('ref_axis',(0.,0.,1.)) ;
#98912 = DIRECTION('center_axis',(0.,1.,0.)) ;
#98913 = DIRECTION('ref_axis',(0.,0.,1.)) ;
#98914 = DIRECTION('center_axis',(0.,-1.,0.)) ;
#98915 = DIRECTION('ref_axis',(0.,0.,-1.)) ;
#98916 = DIRECTION('center_axis',(0.866025403784438,0.,-0.5)) ;
#98917 = DIRECTION('ref_axis',(-0.5,0.,-0.866025403784438)) ;
#98918 = DIRECTION('center_axis',(-1.66923844304129E-16,0.,-1.)) ;
#98919 = DIRECTION('ref_axis',(-1.,0.,1.66923844304129E-16)) ;
#98920 = DIRECTION('center_axis',(-0.866025403784439,0.,-0.5)) ;
#98921 = DIRECTION('ref_axis',(-0.5,0.,0.866025403784439)) ;
#98922 = DIRECTION('center_axis',(-0.866025403784439,0.,0.5)) ;
#98923 = DIRECTION('ref_axis',(0.5,0.,0.866025403784439)) ;
#98924 = DIRECTION('center_axis',(0.,0.,1.)) ;
#98925 = DIRECTION('ref_axis',(1.,0.,0.)) ;
#98926 = DIRECTION('center_axis',(0.866025403784439,0.,0.5)) ;
#98927 = DIRECTION('ref_axis',(0.5,0.,-0.866025403784439)) ;
#98928 = DIRECTION('',(-0.823666160229971,0.500005191429812,0.267523578465998)) ;
#98929 = DIRECTION('center_axis',(0.820330601492067,0.506050349255751,-0.266403356348595)) ;
#98930 = DIRECTION('ref_axis',(0.462747539860455,-0.861076590521797,-0.210741119880419)) ;
#98931 = DIRECTION('center_axis',(-0.475585457889948,-0.866022400932201,0.154349192829876)) ;
#98932 = DIRECTION('ref_axis',(0.876526377919256,-0.48135382912339,1.20637155219922E-16)) ;
#98933 = DIRECTION('',(0.308961791614634,-0.000161847349230684,0.951074437217041)) ;
#98934 = DIRECTION('center_axis',(-0.951074449673282,4.99476165283064E-9,
0.308961795661963)) ;
#98935 = DIRECTION('ref_axis',(0.308961795661963,-8.41182830767154E-26,0.951074449673282)) ;
#98936 = DIRECTION('',(0.308961791614634,-0.000161847349230685,0.951074437217041)) ;
#98937 = DIRECTION('center_axis',(-0.475489515607485,0.866028065754805,0.15461277396241)) ;
#98938 = DIRECTION('ref_axis',(-0.87656867565068,-0.481276798597245,1.5659813065563E-16)) ;
#98939 = DIRECTION('axis',(0.,0.,1.)) ;
#98940 = DIRECTION('refdir',(1.,0.,0.)) ;
#98941 = DIRECTION('center_axis',(-1.,0.,0.)) ;
#98942 = DIRECTION('ref_axis',(0.,0.,1.)) ;
#98943 = DIRECTION('',(-0.309016994374945,-1.16470831848909E-16,-0.951056516295154)) ;
#98944 = DIRECTION('center_axis',(-1.,0.,0.)) ;
#98945 = DIRECTION('ref_axis',(0.,0.,1.)) ;
#98946 = DIRECTION('center_axis',(-1.,0.,0.)) ;
#98947 = DIRECTION('ref_axis',(0.,0.,1.)) ;
#98948 = DIRECTION('center_axis',(-1.,0.,0.)) ;
#98949 = DIRECTION('ref_axis',(0.,0.,1.)) ;
#98950 = DIRECTION('center_axis',(-1.,0.,0.)) ;
#98951 = DIRECTION('ref_axis',(0.,0.,1.)) ;
#98952 = DIRECTION('center_axis',(-1.,0.,0.)) ;
#98953 = DIRECTION('ref_axis',(0.,0.,1.)) ;
#98954 = DIRECTION('center_axis',(-1.,0.,0.)) ;
#98955 = DIRECTION('ref_axis',(0.,0.,1.)) ;
#98956 = DIRECTION('center_axis',(-1.,0.,0.)) ;
#98957 = DIRECTION('ref_axis',(0.,0.,1.)) ;
#98958 = DIRECTION('center_axis',(-1.,0.,0.)) ;
#98959 = DIRECTION('ref_axis',(0.,0.,1.)) ;
#98960 = DIRECTION('center_axis',(-1.,0.,0.)) ;
#98961 = DIRECTION('ref_axis',(0.,0.,1.)) ;
#98962 = DIRECTION('center_axis',(-1.,0.,0.)) ;
#98963 = DIRECTION('ref_axis',(0.,0.,1.)) ;
#98964 = DIRECTION('center_axis',(-1.,0.,0.)) ;
#98965 = DIRECTION('ref_axis',(0.,0.,1.)) ;
#98966 = DIRECTION('center_axis',(-1.,0.,0.)) ;
#98967 = DIRECTION('ref_axis',(0.,0.,1.)) ;
#98968 = DIRECTION('center_axis',(-1.,0.,0.)) ;
#98969 = DIRECTION('ref_axis',(0.,0.,1.)) ;
#98970 = DIRECTION('center_axis',(-1.,0.,0.)) ;
#98971 = DIRECTION('ref_axis',(0.,0.,1.)) ;
#98972 = DIRECTION('center_axis',(-1.,0.,0.)) ;
#98973 = DIRECTION('ref_axis',(0.,0.,1.)) ;
#98974 = DIRECTION('center_axis',(-1.,0.,0.)) ;
#98975 = DIRECTION('ref_axis',(0.,0.,1.)) ;
#98976 = DIRECTION('center_axis',(-1.,0.,0.)) ;
#98977 = DIRECTION('ref_axis',(0.,0.,1.)) ;
#98978 = DIRECTION('center_axis',(-1.,0.,0.)) ;
#98979 = DIRECTION('ref_axis',(0.,0.,1.)) ;
#98980 = DIRECTION('center_axis',(-0.446197753347441,5.43259321731477E-15,
-0.89493439139844)) ;
#98981 = DIRECTION('ref_axis',(0.89493439139844,8.82040419595591E-13,-0.446197753347441)) ;
#98982 = DIRECTION('center_axis',(-1.,0.,0.)) ;
#98983 = DIRECTION('ref_axis',(0.,0.,1.)) ;
#98984 = DIRECTION('center_axis',(-1.,0.,0.)) ;
#98985 = DIRECTION('ref_axis',(0.,0.,1.)) ;
#98986 = DIRECTION('center_axis',(0.,1.,-1.22464679914735E-16)) ;
#98987 = DIRECTION('ref_axis',(0.,-1.22464679914735E-16,-1.)) ;
#98988 = DIRECTION('center_axis',(1.,0.,0.)) ;
#98989 = DIRECTION('ref_axis',(0.,0.,1.)) ;
#98990 = DIRECTION('center_axis',(-1.,0.,0.)) ;
#98991 = DIRECTION('ref_axis',(0.,0.,1.)) ;
#98992 = DIRECTION('center_axis',(-1.,0.,0.)) ;
#98993 = DIRECTION('ref_axis',(0.,0.,1.)) ;
#98994 = DIRECTION('center_axis',(0.,-1.,1.22464679914735E-16)) ;
#98995 = DIRECTION('ref_axis',(0.,-1.22464679914735E-16,-1.)) ;
#98996 = DIRECTION('center_axis',(-1.,0.,0.)) ;
#98997 = DIRECTION('ref_axis',(0.,0.,1.)) ;
#98998 = DIRECTION('center_axis',(-1.,0.,0.)) ;
#98999 = DIRECTION('ref_axis',(0.,0.,1.)) ;
#99000 = DIRECTION('',(1.,0.,0.)) ;
#99001 = DIRECTION('center_axis',(-1.,0.,0.)) ;
#99002 = DIRECTION('ref_axis',(0.,0.,1.)) ;
#99003 = DIRECTION('center_axis',(-1.,0.,0.)) ;
#99004 = DIRECTION('ref_axis',(0.,0.,1.)) ;
#99005 = DIRECTION('',(1.,0.,0.)) ;
#99006 = DIRECTION('center_axis',(-1.,0.,0.)) ;
#99007 = DIRECTION('ref_axis',(0.,0.,1.)) ;
#99008 = DIRECTION('center_axis',(0.,1.83697019872103E-16,-1.)) ;
#99009 = DIRECTION('ref_axis',(0.,1.,1.22464679914735E-16)) ;
#99010 = DIRECTION('center_axis',(0.446197753347436,0.894934391398443,0.)) ;
#99011 = DIRECTION('ref_axis',(-0.894934391398443,0.446197753347436,0.)) ;
#99012 = DIRECTION('center_axis',(7.80261272178311E-17,1.54157131018989E-16,
-1.)) ;
#99013 = DIRECTION('ref_axis',(-1.52269221131066E-34,1.,1.54157131018989E-16)) ;
#99014 = DIRECTION('center_axis',(-1.,0.,0.)) ;
#99015 = DIRECTION('ref_axis',(0.,0.,-1.)) ;
#99016 = DIRECTION('center_axis',(0.,-1.,-3.49148133884313E-15)) ;
#99017 = DIRECTION('ref_axis',(0.,3.49148133884313E-15,-1.)) ;
#99018 = DIRECTION('center_axis',(0.446197753347436,-3.1246467270566E-15,
0.894934391398443)) ;
#99019 = DIRECTION('ref_axis',(0.894934391398443,-2.08468151695124E-30,-0.446197753347436)) ;
#99020 = DIRECTION('center_axis',(7.80261272178311E-17,1.,3.64563846986212E-15)) ;
#99021 = DIRECTION('ref_axis',(-2.78985116612342E-34,-3.64563846986212E-15,
1.)) ;
#99022 = DIRECTION('center_axis',(-1.,0.,0.)) ;
#99023 = DIRECTION('ref_axis',(0.,0.,-1.)) ;
#99024 = DIRECTION('center_axis',(7.80261272178311E-17,1.54157131018989E-16,
-1.)) ;
#99025 = DIRECTION('ref_axis',(-1.52269221131066E-34,1.,1.54157131018989E-16)) ;
#99026 = DIRECTION('center_axis',(0.446197753347436,-0.894934391398443,0.)) ;
#99027 = DIRECTION('ref_axis',(0.894934391398443,0.446197753347436,0.)) ;
#99028 = DIRECTION('center_axis',(0.,0.,1.)) ;
#99029 = DIRECTION('ref_axis',(1.,0.,0.)) ;
#99030 = DIRECTION('center_axis',(-1.,0.,0.)) ;
#99031 = DIRECTION('ref_axis',(0.,0.,-1.)) ;
#99032 = DIRECTION('center_axis',(7.80261272178311E-17,1.,3.64563846986212E-15)) ;
#99033 = DIRECTION('ref_axis',(-2.78985116612342E-34,-3.64563846986212E-15,
1.)) ;
#99034 = DIRECTION('center_axis',(0.446197753347436,3.1246467270566E-15,-0.894934391398443)) ;
#99035 = DIRECTION('ref_axis',(-0.894934391398443,4.22434834092767E-32,-0.446197753347436)) ;
#99036 = DIRECTION('center_axis',(0.,-1.,-3.49148133884313E-15)) ;
#99037 = DIRECTION('ref_axis',(0.,3.49148133884313E-15,-1.)) ;
#99038 = DIRECTION('center_axis',(-1.,0.,0.)) ;
#99039 = DIRECTION('ref_axis',(0.,-4.44089209850063E-15,-1.)) ;
#99040 = DIRECTION('center_axis',(0.,0.,1.)) ;
#99041 = DIRECTION('ref_axis',(1.,0.,0.)) ;
#99042 = DIRECTION('center_axis',(0.,0.,1.)) ;
#99043 = DIRECTION('ref_axis',(1.,0.,0.)) ;
#99044 = DIRECTION('',(0.,1.,0.)) ;
#99045 = DIRECTION('',(0.894934391398443,-0.446197753347436,0.)) ;
#99046 = DIRECTION('center_axis',(0.,0.,1.)) ;
#99047 = DIRECTION('ref_axis',(1.,0.,0.)) ;
#99048 = DIRECTION('',(0.,1.,0.)) ;
#99049 = DIRECTION('',(0.894934391398442,0.446197753347436,-2.77225660396053E-17)) ;
#99050 = DIRECTION('center_axis',(7.8026127217831E-17,1.54157131018989E-16,
-1.)) ;
#99051 = DIRECTION('ref_axis',(0.,1.,1.54157131018989E-16)) ;
#99052 = DIRECTION('',(0.,-1.,-1.54157131018989E-16)) ;
#99053 = DIRECTION('',(0.894934391398442,-0.446197753347436,5.54451320792105E-17)) ;
#99054 = DIRECTION('center_axis',(7.8026127217831E-17,1.54157131018989E-16,
-1.)) ;
#99055 = DIRECTION('ref_axis',(0.,1.,1.54157131018989E-16)) ;
#99056 = DIRECTION('',(0.,-1.,-1.54157131018989E-16)) ;
#99057 = DIRECTION('',(0.894934391398443,0.446197753347436,1.38612830198026E-16)) ;
#99058 = DIRECTION('center_axis',(0.446197753347436,0.894934391398443,0.)) ;
#99059 = DIRECTION('ref_axis',(-0.894934391398443,0.446197753347436,0.)) ;
#99060 = DIRECTION('center_axis',(-0.446197753347433,-0.894934391398444,0.)) ;
#99061 = DIRECTION('ref_axis',(0.894934391398444,-0.446197753347433,-4.12152110262257E-18)) ;
#99062 = DIRECTION('',(0.,0.,-1.)) ;
#99063 = DIRECTION('',(0.,0.,-1.)) ;
#99064 = DIRECTION('center_axis',(0.446197753347436,-0.894934391398443,0.)) ;
#99065 = DIRECTION('ref_axis',(0.894934391398443,0.446197753347436,0.)) ;
#99066 = DIRECTION('center_axis',(-0.446197753347435,0.894934391398443,1.76637751103157E-16)) ;
#99067 = DIRECTION('ref_axis',(0.894934391398443,0.446197753347435,4.30154570777946E-16)) ;
#99068 = DIRECTION('',(0.,-2.93027614185272E-16,1.)) ;
#99069 = DIRECTION('',(0.,-2.93027614185272E-16,1.)) ;
#99070 = DIRECTION('center_axis',(-1.,0.,0.)) ;
#99071 = DIRECTION('ref_axis',(0.,0.,1.)) ;
#99072 = DIRECTION('',(0.,1.,3.49148133884313E-15)) ;
#99073 = DIRECTION('',(0.,3.64563846986212E-15,-1.)) ;
#99074 = DIRECTION('center_axis',(-1.,0.,0.)) ;
#99075 = DIRECTION('ref_axis',(0.,0.,1.)) ;
#99076 = DIRECTION('center_axis',(-1.,0.,0.)) ;
#99077 = DIRECTION('ref_axis',(0.,0.,1.)) ;
#99078 = DIRECTION('center_axis',(-1.,0.,0.)) ;
#99079 = DIRECTION('ref_axis',(0.,0.,1.)) ;
#99080 = DIRECTION('',(0.,3.64563846986212E-15,-1.)) ;
#99081 = DIRECTION('',(0.,-1.,-3.78450895302841E-15)) ;
#99082 = DIRECTION('center_axis',(-1.,0.,0.)) ;
#99083 = DIRECTION('ref_axis',(0.,0.,1.)) ;
#99084 = DIRECTION('',(0.,-1.,-3.78450895302841E-15)) ;
#99085 = DIRECTION('',(0.,-3.49148133884313E-15,1.)) ;
#99086 = DIRECTION('center_axis',(-1.,0.,0.)) ;
#99087 = DIRECTION('ref_axis',(0.,0.,1.)) ;
#99088 = DIRECTION('center_axis',(-1.,0.,0.)) ;
#99089 = DIRECTION('ref_axis',(0.,0.,1.)) ;
#99090 = DIRECTION('center_axis',(0.,-1.,-3.49148133884313E-15)) ;
#99091 = DIRECTION('ref_axis',(1.,0.,0.)) ;
#99092 = DIRECTION('',(0.,-3.49148133884313E-15,1.)) ;
#99093 = DIRECTION('',(0.894934391398443,1.5578911292463E-15,-0.446197753347436)) ;
#99094 = DIRECTION('center_axis',(7.8026127217831E-17,1.,3.64563846986212E-15)) ;
#99095 = DIRECTION('ref_axis',(-3.38151074872755E-48,-3.64563846986212E-15,
1.)) ;
#99096 = DIRECTION('',(0.894934391398442,1.50244599716709E-15,-0.446197753347436)) ;
#99097 = DIRECTION('center_axis',(0.446197753347436,-3.1246467270566E-15,
0.894934391398443)) ;
#99098 = DIRECTION('ref_axis',(-0.894934391398443,-1.5578911292463E-15,0.446197753347436)) ;
#99099 = DIRECTION('',(0.,1.,3.49148133884313E-15)) ;
#99100 = DIRECTION('center_axis',(0.446197753347436,3.1246467270566E-15,-0.894934391398443)) ;
#99101 = DIRECTION('ref_axis',(0.894934391398443,-1.5578911292463E-15,0.446197753347436)) ;
#99102 = DIRECTION('center_axis',(-0.446197753347437,-3.00284176875363E-15,
0.894934391398442)) ;
#99103 = DIRECTION('ref_axis',(0.894934391398442,4.02859800883856E-16,0.446197753347437)) ;
#99104 = DIRECTION('',(0.894934391398442,-1.5301685632067E-15,0.446197753347436)) ;
#99105 = DIRECTION('',(0.894934391398443,-1.69650395944433E-15,0.446197753347436)) ;
#99106 = DIRECTION('center_axis',(0.,-1.,-3.49148133884313E-15)) ;
#99107 = DIRECTION('ref_axis',(1.,0.,0.)) ;
#99108 = DIRECTION('center_axis',(7.8026127217831E-17,1.,3.64563846986212E-15)) ;
#99109 = DIRECTION('ref_axis',(-3.38151074872755E-48,-3.64563846986212E-15,
1.)) ;
#99110 = DIRECTION('center_axis',(-1.,0.,0.)) ;
#99111 = DIRECTION('ref_axis',(0.,0.,1.)) ;
#99112 = DIRECTION('center_axis',(1.,0.,0.)) ;
#99113 = DIRECTION('ref_axis',(0.,0.,-1.)) ;
#99114 = DIRECTION('center_axis',(-1.,0.,0.)) ;
#99115 = DIRECTION('ref_axis',(0.,0.,1.)) ;
#99116 = DIRECTION('center_axis',(-1.,0.,0.)) ;
#99117 = DIRECTION('ref_axis',(0.,0.,1.)) ;
#99118 = DIRECTION('center_axis',(-1.,0.,0.)) ;
#99119 = DIRECTION('ref_axis',(0.,0.,1.)) ;
#99120 = DIRECTION('center_axis',(-1.,0.,0.)) ;
#99121 = DIRECTION('ref_axis',(0.,0.,1.)) ;
#99122 = DIRECTION('center_axis',(-1.,0.,0.)) ;
#99123 = DIRECTION('ref_axis',(0.,3.67517835871524E-15,-1.)) ;
#99124 = DIRECTION('center_axis',(-1.,0.,0.)) ;
#99125 = DIRECTION('ref_axis',(0.,0.,1.)) ;
#99126 = DIRECTION('center_axis',(-1.,0.,0.)) ;
#99127 = DIRECTION('ref_axis',(0.,0.,1.)) ;
#99128 = DIRECTION('center_axis',(-1.,0.,0.)) ;
#99129 = DIRECTION('ref_axis',(0.,0.,1.)) ;
#99130 = DIRECTION('',(0.,0.,1.)) ;
#99131 = DIRECTION('',(1.,0.,0.)) ;
#99132 = DIRECTION('',(0.,0.,1.)) ;
#99133 = DIRECTION('',(1.,0.,0.)) ;
#99134 = DIRECTION('',(0.,0.,1.)) ;
#99135 = DIRECTION('',(1.,0.,0.)) ;
#99136 = DIRECTION('',(-3.63825924986263E-15,1.,-5.55111512312577E-17)) ;
#99137 = DIRECTION('',(4.09137426284976E-17,5.55111512312579E-17,1.)) ;
#99138 = DIRECTION('',(0.,0.,1.)) ;
#99139 = DIRECTION('',(1.,0.,0.)) ;
#99140 = DIRECTION('',(-5.55111512312578E-17,1.50043247445456E-16,-1.)) ;
#99141 = DIRECTION('',(3.13759758499951E-17,-1.,-1.50043247445456E-16)) ;
#99142 = DIRECTION('',(0.,0.,1.)) ;
#99143 = DIRECTION('',(1.,0.,0.)) ;
#99144 = DIRECTION('',(3.33066907387547E-16,1.4539153497531E-16,-1.)) ;
#99145 = DIRECTION('',(4.6642992146974E-17,-1.,-1.4539153497531E-16)) ;
#99146 = CARTESIAN_POINT('',(0.,0.,0.)) ;
#99147 = CARTESIAN_POINT('',(0.,0.,0.)) ;
#99148 = CARTESIAN_POINT('Origin',(53.4,-9.74999999999999,-35.5)) ;
#99149 = CARTESIAN_POINT('',(53.4,-11.35,-35.5)) ;
#99150 = CARTESIAN_POINT('',(53.4,-8.14999999999999,-35.5)) ;
#99151 = CARTESIAN_POINT('Origin',(53.4,-9.74999999999999,-35.5)) ;
#99152 = CARTESIAN_POINT('Origin',(53.4,-9.74999999999999,-35.5)) ;
#99153 = CARTESIAN_POINT('',(53.25,-8.,-35.5)) ;
#99154 = CARTESIAN_POINT('Origin',(53.4,-7.99999999999999,-35.5)) ;
#99155 = CARTESIAN_POINT('Origin',(53.25,-9.74999999999999,-35.5)) ;
#99156 = CARTESIAN_POINT('Origin',(53.85,-9.74999999999999,-35.5)) ;
#99157 = CARTESIAN_POINT('',(54.,-7.99999999999999,-35.5)) ;
#99158 = CARTESIAN_POINT('Origin',(54.,-9.74999999999999,-35.5)) ;
#99159 = CARTESIAN_POINT('',(53.85,-8.14999999999999,-35.5)) ;
#99160 = CARTESIAN_POINT('Origin',(53.85,-7.99999999999999,-35.5)) ;
#99161 = CARTESIAN_POINT('',(53.8500000000001,-11.35,-35.5)) ;
#99162 = CARTESIAN_POINT('Origin',(53.85,-9.74999999999999,-35.5)) ;
#99163 = CARTESIAN_POINT('Origin',(53.85,-9.74999999999999,-35.5)) ;
#99164 = CARTESIAN_POINT('Origin',(43.,-0.162132034355965,-34.25)) ;
#99165 = CARTESIAN_POINT('',(43.,-0.0560660171779847,-35.793933982822)) ;
#99166 = CARTESIAN_POINT('',(43.,-0.0560660171779853,-32.706066017178)) ;
#99167 = CARTESIAN_POINT('Origin',(43.,-0.056066017177985,-34.25)) ;
#99168 = CARTESIAN_POINT('Origin',(43.,-0.056066017177985,-34.25)) ;
#99169 = CARTESIAN_POINT('',(43.,-0.162132034355965,-32.75)) ;
#99170 = CARTESIAN_POINT('Origin',(43.,-0.162132034355965,-32.6)) ;
#99171 = CARTESIAN_POINT('',(43.,-0.162132034355965,-35.75)) ;
#99172 = CARTESIAN_POINT('Origin',(43.,-0.162132034355965,-34.25)) ;
#99173 = CARTESIAN_POINT('Origin',(43.,-0.162132034355965,-34.25)) ;
#99174 = CARTESIAN_POINT('Origin',(43.,-0.600000000000015,-34.25)) ;
#99175 = CARTESIAN_POINT('',(43.,-0.750000000000015,-35.9)) ;
#99176 = CARTESIAN_POINT('Origin',(43.,-0.750000000000015,-34.25)) ;
#99177 = CARTESIAN_POINT('',(43.,-0.600000000000015,-35.75)) ;
#99178 = CARTESIAN_POINT('Origin',(43.,-0.600000000000015,-35.9)) ;
#99179 = CARTESIAN_POINT('Origin',(43.,-0.600000000000015,-34.25)) ;
#99180 = CARTESIAN_POINT('Origin',(43.,-0.162132034355978,34.25)) ;
#99181 = CARTESIAN_POINT('',(43.,-0.0560660171779973,32.706066017178)) ;
#99182 = CARTESIAN_POINT('',(43.,-0.0560660171779978,35.793933982822)) ;
#99183 = CARTESIAN_POINT('Origin',(43.,-0.0560660171779975,34.25)) ;
#99184 = CARTESIAN_POINT('Origin',(43.,-0.0560660171779975,34.25)) ;
#99185 = CARTESIAN_POINT('',(43.,-0.162132034355978,35.75)) ;
#99186 = CARTESIAN_POINT('Origin',(43.,-0.162132034355978,35.9)) ;
#99187 = CARTESIAN_POINT('',(43.,-0.162132034355977,32.75)) ;
#99188 = CARTESIAN_POINT('Origin',(43.,-0.162132034355978,34.25)) ;
#99189 = CARTESIAN_POINT('Origin',(43.,-0.162132034355978,34.25)) ;
#99190 = CARTESIAN_POINT('Origin',(43.,-0.600000000000027,34.25)) ;
#99191 = CARTESIAN_POINT('',(43.,-0.750000000000027,32.6)) ;
#99192 = CARTESIAN_POINT('Origin',(43.,-0.750000000000027,34.25)) ;
#99193 = CARTESIAN_POINT('',(43.,-0.600000000000027,32.75)) ;
#99194 = CARTESIAN_POINT('Origin',(43.,-0.600000000000027,32.6)) ;
#99195 = CARTESIAN_POINT('Origin',(43.,-0.600000000000027,34.25)) ;
#99196 = CARTESIAN_POINT('Origin',(43.,-6.29162293061953E-15,34.25)) ;
#99197 = CARTESIAN_POINT('',(43.,-5.82322967106645E-15,32.65)) ;
#99198 = CARTESIAN_POINT('',(43.,-5.99770769882417E-15,32.65)) ;
#99199 = CARTESIAN_POINT('Origin',(43.,-6.29162293061953E-15,34.25)) ;
#99200 = CARTESIAN_POINT('Origin',(43.,-6.29162293061953E-15,34.25)) ;
#99201 = CARTESIAN_POINT('',(43.,-6.01607740081138E-15,32.75)) ;
#99202 = CARTESIAN_POINT('Origin',(43.,6.29162293061953E-15,-34.25)) ;
#99203 = CARTESIAN_POINT('',(43.,6.76001619017261E-15,-35.85)) ;
#99204 = CARTESIAN_POINT('',(43.,6.5855381624149E-15,-35.85)) ;
#99205 = CARTESIAN_POINT('Origin',(43.,6.29162293061953E-15,-34.25)) ;
#99206 = CARTESIAN_POINT('Origin',(43.,6.29162293061953E-15,-34.25)) ;
#99207 = CARTESIAN_POINT('',(43.,6.56716846042768E-15,-35.75)) ;
#99208 = CARTESIAN_POINT('Origin',(-2.00100000000009,-9.7500000000002,-35.5)) ;
#99209 = CARTESIAN_POINT('',(-2.00100000000008,-11.3500000000002,-35.5)) ;
#99210 = CARTESIAN_POINT('Origin',(54.,1.9709024278469E-13,3.63163086615829E-29)) ;
#99211 = CARTESIAN_POINT('',(54.,-1.74999999999999,38.25)) ;
#99212 = CARTESIAN_POINT('',(54.,-1.74999999999999,39.85)) ;
#99213 = CARTESIAN_POINT('',(54.,-1.74999999999999,38.25)) ;
#99214 = CARTESIAN_POINT('',(54.0000000000001,-19.6,39.85)) ;
#99215 = CARTESIAN_POINT('',(54.,1.9709024278469E-13,39.85)) ;
#99216 = CARTESIAN_POINT('',(54.0000000000001,-19.6,-39.85)) ;
#99217 = CARTESIAN_POINT('',(54.0000000000001,-19.6,-3.55561622265573E-15)) ;
#99218 = CARTESIAN_POINT('',(54.,-1.74999999999998,-39.85)) ;
#99219 = CARTESIAN_POINT('',(54.,-1.74999999999998,-39.85)) ;
#99220 = CARTESIAN_POINT('',(54.,-1.74999999999998,-38.25)) ;
#99221 = CARTESIAN_POINT('',(54.,-1.74999999999998,-38.25)) ;
#99222 = CARTESIAN_POINT('',(54.,-1.74999999999998,-3.17465734165687E-16)) ;
#99223 = CARTESIAN_POINT('',(54.,-4.39999999999999,-32.65)) ;
#99224 = CARTESIAN_POINT('',(54.,-4.09999999999999,-32.35)) ;
#99225 = CARTESIAN_POINT('Origin',(54.,-4.39999999999999,-32.35)) ;
#99226 = CARTESIAN_POINT('',(54.0000000000001,-14.1,-32.65)) ;
#99227 = CARTESIAN_POINT('',(54.,1.9709024278469E-13,-32.65)) ;
#99228 = CARTESIAN_POINT('',(54.0000000000001,-14.4,-32.35)) ;
#99229 = CARTESIAN_POINT('Origin',(54.0000000000001,-14.1,-32.35)) ;
#99230 = CARTESIAN_POINT('',(54.0000000000001,-14.4,33.85)) ;
#99231 = CARTESIAN_POINT('',(54.0000000000001,-14.4,3.63163086615829E-29)) ;
#99232 = CARTESIAN_POINT('',(54.0000000000001,-14.1,34.15)) ;
#99233 = CARTESIAN_POINT('Origin',(54.0000000000001,-14.1,33.85)) ;
#99234 = CARTESIAN_POINT('',(54.,-4.39999999999999,34.15)) ;
#99235 = CARTESIAN_POINT('',(54.,1.9709024278469E-13,34.15)) ;
#99236 = CARTESIAN_POINT('',(54.,-4.09999999999999,33.85)) ;
#99237 = CARTESIAN_POINT('Origin',(54.,-4.39999999999999,33.85)) ;
#99238 = CARTESIAN_POINT('',(54.,-4.09999999999999,3.63163086615829E-29)) ;
#99239 = CARTESIAN_POINT('Origin',(53.25,1.94471631780558E-13,3.58301353414727E-29)) ;
#99240 = CARTESIAN_POINT('',(53.2500000000001,-19.6,-39.85)) ;
#99241 = CARTESIAN_POINT('',(53.2500000000001,-19.6,39.85)) ;
#99242 = CARTESIAN_POINT('',(53.2500000000001,-19.6,40.)) ;
#99243 = CARTESIAN_POINT('',(53.25,-1.75,39.85)) ;
#99244 = CARTESIAN_POINT('',(53.25,-1.75,39.85)) ;
#99245 = CARTESIAN_POINT('',(53.25,-1.75,38.25)) ;
#99246 = CARTESIAN_POINT('',(53.25,-1.75,38.25)) ;
#99247 = CARTESIAN_POINT('',(53.25,-1.74999999999998,-38.25)) ;
#99248 = CARTESIAN_POINT('',(53.25,-1.74999999999998,-38.25)) ;
#99249 = CARTESIAN_POINT('',(53.25,-1.74999999999998,-39.85)) ;
#99250 = CARTESIAN_POINT('',(53.25,-1.74999999999998,-38.25)) ;
#99251 = CARTESIAN_POINT('',(53.25,2.25195512010636E-13,-39.85)) ;
#99252 = CARTESIAN_POINT('',(53.2500000000001,-14.1,-32.65)) ;
#99253 = CARTESIAN_POINT('',(53.2500000000001,-14.4,-32.35)) ;
#99254 = CARTESIAN_POINT('Origin',(53.2500000000001,-14.1,-32.35)) ;
#99255 = CARTESIAN_POINT('',(53.25,-4.4,-32.65)) ;
#99256 = CARTESIAN_POINT('',(53.25,-4.25,-32.65)) ;
#99257 = CARTESIAN_POINT('',(53.25,-4.1,-32.35)) ;
#99258 = CARTESIAN_POINT('Origin',(53.25,-4.4,-32.35)) ;
#99259 = CARTESIAN_POINT('',(53.25,-4.1,33.85)) ;
#99260 = CARTESIAN_POINT('',(53.25,-4.1,34.)) ;
#99261 = CARTESIAN_POINT('',(53.25,-4.4,34.15)) ;
#99262 = CARTESIAN_POINT('Origin',(53.25,-4.4,33.85)) ;
#99263 = CARTESIAN_POINT('',(53.2500000000001,-14.1,34.15)) ;
#99264 = CARTESIAN_POINT('',(53.2500000000001,-14.2500000000002,34.15)) ;
#99265 = CARTESIAN_POINT('',(53.2500000000001,-14.4,33.85)) ;
#99266 = CARTESIAN_POINT('Origin',(53.2500000000001,-14.1,33.85)) ;
#99267 = CARTESIAN_POINT('',(53.2500000000001,-14.4,-32.5)) ;
#99268 = CARTESIAN_POINT('Origin',(53.25,-6.93889390390723E-15,-40.)) ;
#99269 = CARTESIAN_POINT('',(0.149999999999965,-4.6,-40.)) ;
#99270 = CARTESIAN_POINT('',(-0.150000000000035,-4.9,-40.)) ;
#99271 = CARTESIAN_POINT('Origin',(-0.150000000000035,-4.6,-40.)) ;
#99272 = CARTESIAN_POINT('',(0.149999999999963,-1.75,-40.)) ;
#99273 = CARTESIAN_POINT('',(0.149999999999965,-1.75000000000001,-40.)) ;
#99274 = CARTESIAN_POINT('',(52.25,-1.74999999999999,-40.)) ;
#99275 = CARTESIAN_POINT('',(53.25,-1.75,-40.)) ;
#99276 = CARTESIAN_POINT('',(53.,-1.75,-40.)) ;
#99277 = CARTESIAN_POINT('',(53.25,-1.75,-40.)) ;
#99278 = CARTESIAN_POINT('',(53.0000000000001,-19.6,-40.)) ;
#99279 = CARTESIAN_POINT('',(53.,-7.81264669430658E-15,-40.)) ;
#99280 = CARTESIAN_POINT('',(0.149999999999965,-19.6,-40.)) ;
#99281 = CARTESIAN_POINT('',(53.25,-19.6,-40.)) ;
#99282 = CARTESIAN_POINT('',(0.149999999999965,-6.90000000000001,-40.)) ;
#99283 = CARTESIAN_POINT('',(0.149999999999965,-6.75000000000001,-40.)) ;
#99284 = CARTESIAN_POINT('',(-0.150000000000035,-6.60000000000001,-40.)) ;
#99285 = CARTESIAN_POINT('Origin',(-0.150000000000035,-6.90000000000001,-40.)) ;
#99286 = CARTESIAN_POINT('',(-1.85000000000003,-6.60000000000001,-40.)) ;
#99287 = CARTESIAN_POINT('',(-2.00000000000004,-6.60000000000001,-40.)) ;
#99288 = CARTESIAN_POINT('',(-1.85000000000003,-4.9,-40.)) ;
#99289 = CARTESIAN_POINT('',(-1.85000000000003,-4.75000000000001,-40.)) ;
#99290 = CARTESIAN_POINT('',(-2.77555756156289E-14,-4.9,-40.)) ;
#99291 = CARTESIAN_POINT('',(19.1,-2.90000000000002,-40.)) ;
#99292 = CARTESIAN_POINT('',(19.4,-2.60000000000002,-40.)) ;
#99293 = CARTESIAN_POINT('Origin',(19.4,-2.90000000000002,-40.)) ;
#99294 = CARTESIAN_POINT('',(19.1,-13.1,-40.)) ;
#99295 = CARTESIAN_POINT('',(19.1,-13.25,-40.)) ;
#99296 = CARTESIAN_POINT('',(19.4,-13.4,-40.)) ;
#99297 = CARTESIAN_POINT('Origin',(19.4,-13.1,-40.)) ;
#99298 = CARTESIAN_POINT('',(38.1,-13.4,-40.)) ;
#99299 = CARTESIAN_POINT('',(38.25,-13.4,-40.)) ;
#99300 = CARTESIAN_POINT('',(38.4,-13.1,-40.)) ;
#99301 = CARTESIAN_POINT('Origin',(38.1,-13.1,-40.)) ;
#99302 = CARTESIAN_POINT('',(38.4,-2.90000000000002,-40.)) ;
#99303 = CARTESIAN_POINT('',(38.4,-2.75000000000002,-40.)) ;
#99304 = CARTESIAN_POINT('',(38.1,-2.60000000000002,-40.)) ;
#99305 = CARTESIAN_POINT('Origin',(38.1,-2.90000000000002,-40.)) ;
#99306 = CARTESIAN_POINT('',(19.25,-2.60000000000002,-40.)) ;
#99307 = CARTESIAN_POINT('',(7.34999999999997,-5.40000000000002,-40.)) ;
#99308 = CARTESIAN_POINT('',(7.64999999999997,-5.10000000000002,-40.)) ;
#99309 = CARTESIAN_POINT('Origin',(7.64999999999997,-5.40000000000002,-40.)) ;
#99310 = CARTESIAN_POINT('',(7.34999999999996,-15.1,-40.)) ;
#99311 = CARTESIAN_POINT('',(7.34999999999996,-15.25,-40.)) ;
#99312 = CARTESIAN_POINT('',(7.64999999999996,-15.4,-40.)) ;
#99313 = CARTESIAN_POINT('Origin',(7.64999999999996,-15.1,-40.)) ;
#99314 = CARTESIAN_POINT('',(10.35,-15.4,-40.)) ;
#99315 = CARTESIAN_POINT('',(10.5,-15.4,-40.)) ;
#99316 = CARTESIAN_POINT('',(10.65,-15.1,-40.)) ;
#99317 = CARTESIAN_POINT('Origin',(10.35,-15.1,-40.)) ;
#99318 = CARTESIAN_POINT('',(10.65,-5.40000000000002,-40.)) ;
#99319 = CARTESIAN_POINT('',(10.65,-5.25000000000002,-40.)) ;
#99320 = CARTESIAN_POINT('',(10.35,-5.10000000000002,-40.)) ;
#99321 = CARTESIAN_POINT('Origin',(10.35,-5.40000000000002,-40.)) ;
#99322 = CARTESIAN_POINT('',(7.49999999999997,-5.10000000000002,-40.)) ;
#99323 = CARTESIAN_POINT('',(16.65,-15.1000000000001,-40.)) ;
#99324 = CARTESIAN_POINT('',(16.35,-15.4000000000001,-40.)) ;
#99325 = CARTESIAN_POINT('Origin',(16.35,-15.1000000000001,-40.)) ;
#99326 = CARTESIAN_POINT('',(16.65,-5.40000000000006,-40.)) ;
#99327 = CARTESIAN_POINT('',(16.65,-5.25000000000006,-40.)) ;
#99328 = CARTESIAN_POINT('',(16.35,-5.10000000000006,-40.)) ;
#99329 = CARTESIAN_POINT('Origin',(16.35,-5.40000000000006,-40.)) ;
#99330 = CARTESIAN_POINT('',(13.65,-5.10000000000006,-40.)) ;
#99331 = CARTESIAN_POINT('',(13.5,-5.10000000000006,-40.)) ;
#99332 = CARTESIAN_POINT('',(13.35,-5.40000000000006,-40.)) ;
#99333 = CARTESIAN_POINT('Origin',(13.65,-5.40000000000006,-40.)) ;
#99334 = CARTESIAN_POINT('',(13.35,-15.1000000000001,-40.)) ;
#99335 = CARTESIAN_POINT('',(13.35,-15.2500000000001,-40.)) ;
#99336 = CARTESIAN_POINT('',(13.65,-15.4000000000001,-40.)) ;
#99337 = CARTESIAN_POINT('Origin',(13.65,-15.1000000000001,-40.)) ;
#99338 = CARTESIAN_POINT('',(16.5,-15.4000000000001,-40.)) ;
#99339 = CARTESIAN_POINT('',(46.65,-15.1000000000003,-40.)) ;
#99340 = CARTESIAN_POINT('',(46.35,-15.4000000000003,-40.)) ;
#99341 = CARTESIAN_POINT('Origin',(46.35,-15.1000000000003,-40.)) ;
#99342 = CARTESIAN_POINT('',(46.65,-5.40000000000027,-40.)) ;
#99343 = CARTESIAN_POINT('',(46.65,-5.25000000000027,-40.)) ;
#99344 = CARTESIAN_POINT('',(46.35,-5.10000000000027,-40.)) ;
#99345 = CARTESIAN_POINT('Origin',(46.35,-5.40000000000027,-40.)) ;
#99346 = CARTESIAN_POINT('',(43.65,-5.10000000000027,-40.)) ;
#99347 = CARTESIAN_POINT('',(43.5,-5.10000000000027,-40.)) ;
#99348 = CARTESIAN_POINT('',(43.35,-5.40000000000027,-40.)) ;
#99349 = CARTESIAN_POINT('Origin',(43.65,-5.40000000000027,-40.)) ;
#99350 = CARTESIAN_POINT('',(43.35,-15.1000000000003,-40.)) ;
#99351 = CARTESIAN_POINT('',(43.35,-15.2500000000003,-40.)) ;
#99352 = CARTESIAN_POINT('',(43.65,-15.4000000000003,-40.)) ;
#99353 = CARTESIAN_POINT('Origin',(43.65,-15.1000000000003,-40.)) ;
#99354 = CARTESIAN_POINT('',(46.5,-15.4000000000003,-40.)) ;
#99355 = CARTESIAN_POINT('Origin',(53.25,-6.93889390390723E-15,-39.25)) ;
#99356 = CARTESIAN_POINT('',(52.25,-1.74999999999999,-39.25)) ;
#99357 = CARTESIAN_POINT('',(0.149999999999963,-1.75,-39.25)) ;
#99358 = CARTESIAN_POINT('',(53.25,-1.75,-39.25)) ;
#99359 = CARTESIAN_POINT('',(0.149999999999963,-4.6,-39.25)) ;
#99360 = CARTESIAN_POINT('',(0.149999999999963,-6.93889390390723E-15,-39.25)) ;
#99361 = CARTESIAN_POINT('',(-0.150000000000035,-4.9,-39.25)) ;
#99362 = CARTESIAN_POINT('Origin',(-0.150000000000035,-4.6,-39.25)) ;
#99363 = CARTESIAN_POINT('',(-1.85000000000003,-4.9,-39.25)) ;
#99364 = CARTESIAN_POINT('',(53.25,-4.9,-39.25)) ;
#99365 = CARTESIAN_POINT('',(-1.85000000000003,-6.60000000000001,-39.25)) ;
#99366 = CARTESIAN_POINT('',(-1.85000000000003,-1.88868018446975E-14,-39.25)) ;
#99367 = CARTESIAN_POINT('',(-0.150000000000035,-6.60000000000001,-39.25)) ;
#99368 = CARTESIAN_POINT('',(53.25,-6.60000000000001,-39.25)) ;
#99369 = CARTESIAN_POINT('',(0.149999999999963,-6.90000000000001,-39.25)) ;
#99370 = CARTESIAN_POINT('Origin',(-0.150000000000035,-6.90000000000001,-39.25)) ;
#99371 = CARTESIAN_POINT('',(0.149999999999963,-19.6,-39.25)) ;
#99372 = CARTESIAN_POINT('',(0.149999999999963,-6.93889390390723E-15,-39.25)) ;
#99373 = CARTESIAN_POINT('',(53.0000000000001,-19.6,-39.25)) ;
#99374 = CARTESIAN_POINT('',(53.15,-19.6,-39.25)) ;
#99375 = CARTESIAN_POINT('',(53.,-1.75,-39.25)) ;
#99376 = CARTESIAN_POINT('',(53.,-1.75,-39.25)) ;
#99377 = CARTESIAN_POINT('',(53.25,-1.75,-39.25)) ;
#99378 = CARTESIAN_POINT('',(19.1,-13.1,-39.25)) ;
#99379 = CARTESIAN_POINT('',(19.4,-13.4,-39.25)) ;
#99380 = CARTESIAN_POINT('Origin',(19.4,-13.1,-39.25)) ;
#99381 = CARTESIAN_POINT('',(19.1,-2.90000000000002,-39.25)) ;
#99382 = CARTESIAN_POINT('',(19.1,-6.93889390390723E-15,-39.25)) ;
#99383 = CARTESIAN_POINT('',(19.4,-2.60000000000002,-39.25)) ;
#99384 = CARTESIAN_POINT('Origin',(19.4,-2.90000000000002,-39.25)) ;
#99385 = CARTESIAN_POINT('',(38.1,-2.60000000000002,-39.25)) ;
#99386 = CARTESIAN_POINT('',(53.25,-2.60000000000002,-39.25)) ;
#99387 = CARTESIAN_POINT('',(38.4,-2.90000000000002,-39.25)) ;
#99388 = CARTESIAN_POINT('Origin',(38.1,-2.90000000000002,-39.25)) ;
#99389 = CARTESIAN_POINT('',(38.4,-13.1,-39.25)) ;
#99390 = CARTESIAN_POINT('',(38.4,-6.93889390390723E-15,-39.25)) ;
#99391 = CARTESIAN_POINT('',(38.1,-13.4,-39.25)) ;
#99392 = CARTESIAN_POINT('Origin',(38.1,-13.1,-39.25)) ;
#99393 = CARTESIAN_POINT('',(53.25,-13.4,-39.25)) ;
#99394 = CARTESIAN_POINT('',(7.34999999999996,-15.1,-39.25)) ;
#99395 = CARTESIAN_POINT('',(7.64999999999996,-15.4,-39.25)) ;
#99396 = CARTESIAN_POINT('Origin',(7.64999999999996,-15.1,-39.25)) ;
#99397 = CARTESIAN_POINT('',(7.34999999999997,-5.40000000000002,-39.25)) ;
#99398 = CARTESIAN_POINT('',(7.34999999999997,-2.95770352654046E-15,-39.25)) ;
#99399 = CARTESIAN_POINT('',(7.64999999999997,-5.10000000000002,-39.25)) ;
#99400 = CARTESIAN_POINT('Origin',(7.64999999999997,-5.40000000000002,-39.25)) ;
#99401 = CARTESIAN_POINT('',(10.35,-5.10000000000002,-39.25)) ;
#99402 = CARTESIAN_POINT('',(53.25,-5.10000000000002,-39.25)) ;
#99403 = CARTESIAN_POINT('',(10.65,-5.40000000000002,-39.25)) ;
#99404 = CARTESIAN_POINT('Origin',(10.35,-5.40000000000002,-39.25)) ;
#99405 = CARTESIAN_POINT('',(10.65,-15.1,-39.25)) ;
#99406 = CARTESIAN_POINT('',(10.65,4.51028103753969E-16,-39.25)) ;
#99407 = CARTESIAN_POINT('',(10.35,-15.4,-39.25)) ;
#99408 = CARTESIAN_POINT('Origin',(10.35,-15.1,-39.25)) ;
#99409 = CARTESIAN_POINT('',(53.25,-15.4,-39.25)) ;
#99410 = CARTESIAN_POINT('',(16.65,-5.40000000000006,-39.25)) ;
#99411 = CARTESIAN_POINT('',(16.35,-5.10000000000006,-39.25)) ;
#99412 = CARTESIAN_POINT('Origin',(16.35,-5.40000000000006,-39.25)) ;
#99413 = CARTESIAN_POINT('',(16.65,-15.1000000000001,-39.25)) ;
#99414 = CARTESIAN_POINT('',(16.65,5.759281940243E-15,-39.25)) ;
#99415 = CARTESIAN_POINT('',(16.35,-15.4000000000001,-39.25)) ;
#99416 = CARTESIAN_POINT('Origin',(16.35,-15.1000000000001,-39.25)) ;
#99417 = CARTESIAN_POINT('',(13.65,-15.4000000000001,-39.25)) ;
#99418 = CARTESIAN_POINT('',(53.25,-15.4000000000001,-39.25)) ;
#99419 = CARTESIAN_POINT('',(13.35,-15.1000000000001,-39.25)) ;
#99420 = CARTESIAN_POINT('Origin',(13.65,-15.1000000000001,-39.25)) ;
#99421 = CARTESIAN_POINT('',(13.35,-5.40000000000006,-39.25)) ;
#99422 = CARTESIAN_POINT('',(13.35,-1.73472347597685E-17,-39.25)) ;
#99423 = CARTESIAN_POINT('',(13.65,-5.10000000000006,-39.25)) ;
#99424 = CARTESIAN_POINT('Origin',(13.65,-5.40000000000006,-39.25)) ;
#99425 = CARTESIAN_POINT('',(53.25,-5.10000000000006,-39.25)) ;
#99426 = CARTESIAN_POINT('',(46.65,-5.40000000000027,-39.25)) ;
#99427 = CARTESIAN_POINT('',(46.35,-5.10000000000027,-39.25)) ;
#99428 = CARTESIAN_POINT('Origin',(46.35,-5.40000000000027,-39.25)) ;
#99429 = CARTESIAN_POINT('',(46.65,-15.1000000000003,-39.25)) ;
#99430 = CARTESIAN_POINT('',(46.65,-2.35922392732846E-15,-39.25)) ;
#99431 = CARTESIAN_POINT('',(46.35,-15.4000000000003,-39.25)) ;
#99432 = CARTESIAN_POINT('Origin',(46.35,-15.1000000000003,-39.25)) ;
#99433 = CARTESIAN_POINT('',(43.65,-15.4000000000003,-39.25)) ;
#99434 = CARTESIAN_POINT('',(53.25,-15.4000000000003,-39.25)) ;
#99435 = CARTESIAN_POINT('',(43.35,-15.1000000000003,-39.25)) ;
#99436 = CARTESIAN_POINT('Origin',(43.65,-15.1000000000003,-39.25)) ;
#99437 = CARTESIAN_POINT('',(43.35,-5.40000000000027,-39.25)) ;
#99438 = CARTESIAN_POINT('',(43.35,-6.93889390390723E-15,-39.25)) ;
#99439 = CARTESIAN_POINT('',(43.65,-5.10000000000027,-39.25)) ;
#99440 = CARTESIAN_POINT('Origin',(43.65,-5.40000000000027,-39.25)) ;
#99441 = CARTESIAN_POINT('',(53.25,-5.10000000000027,-39.25)) ;
#99442 = CARTESIAN_POINT('Origin',(53.25,-19.75,40.)) ;
#99443 = CARTESIAN_POINT('',(52.25,-1.75,40.)) ;
#99444 = CARTESIAN_POINT('',(0.14999999999997,-1.75000000000002,40.)) ;
#99445 = CARTESIAN_POINT('',(53.25,-1.75000000000002,40.)) ;
#99446 = CARTESIAN_POINT('',(0.149999999999972,-4.60000000000001,40.)) ;
#99447 = CARTESIAN_POINT('',(0.14999999999997,-19.75,40.)) ;
#99448 = CARTESIAN_POINT('',(-0.150000000000028,-4.90000000000001,40.)) ;
#99449 = CARTESIAN_POINT('Origin',(-0.150000000000028,-4.60000000000001,40.)) ;
#99450 = CARTESIAN_POINT('',(-1.85000000000004,-4.90000000000001,40.)) ;
#99451 = CARTESIAN_POINT('',(53.25,-4.90000000000001,40.)) ;
#99452 = CARTESIAN_POINT('',(-1.85000000000003,-6.60000000000001,40.)) ;
#99453 = CARTESIAN_POINT('',(-1.85000000000003,-19.75,40.)) ;
#99454 = CARTESIAN_POINT('',(-0.150000000000028,-6.60000000000001,40.)) ;
#99455 = CARTESIAN_POINT('',(53.25,-6.60000000000001,40.)) ;
#99456 = CARTESIAN_POINT('',(0.149999999999972,-6.90000000000001,40.)) ;
#99457 = CARTESIAN_POINT('Origin',(-0.150000000000028,-6.90000000000001,40.)) ;
#99458 = CARTESIAN_POINT('',(0.149999999999972,-19.6,40.)) ;
#99459 = CARTESIAN_POINT('',(0.14999999999997,-19.75,40.)) ;
#99460 = CARTESIAN_POINT('',(53.,-19.6,40.)) ;
#99461 = CARTESIAN_POINT('',(53.25,-19.6,40.)) ;
#99462 = CARTESIAN_POINT('',(53.,-1.75000000000002,40.)) ;
#99463 = CARTESIAN_POINT('',(53.,-1.75000000000002,40.)) ;
#99464 = CARTESIAN_POINT('',(53.25,-1.75000000000002,40.)) ;
#99465 = CARTESIAN_POINT('',(10.65,-5.40000000000002,40.)) ;
#99466 = CARTESIAN_POINT('',(10.35,-5.10000000000002,40.)) ;
#99467 = CARTESIAN_POINT('Origin',(10.35,-5.40000000000002,40.)) ;
#99468 = CARTESIAN_POINT('',(10.65,-15.1,40.)) ;
#99469 = CARTESIAN_POINT('',(10.65,-15.25,40.)) ;
#99470 = CARTESIAN_POINT('',(10.35,-15.4,40.)) ;
#99471 = CARTESIAN_POINT('Origin',(10.35,-15.1,40.)) ;
#99472 = CARTESIAN_POINT('',(7.64999999999997,-15.4,40.)) ;
#99473 = CARTESIAN_POINT('',(7.49999999999997,-15.4,40.)) ;
#99474 = CARTESIAN_POINT('',(7.34999999999997,-15.1,40.)) ;
#99475 = CARTESIAN_POINT('Origin',(7.64999999999997,-15.1,40.)) ;
#99476 = CARTESIAN_POINT('',(7.34999999999996,-5.40000000000002,40.)) ;
#99477 = CARTESIAN_POINT('',(7.34999999999996,-5.25000000000002,40.)) ;
#99478 = CARTESIAN_POINT('',(7.64999999999996,-5.10000000000002,40.)) ;
#99479 = CARTESIAN_POINT('Origin',(7.64999999999996,-5.40000000000002,40.)) ;
#99480 = CARTESIAN_POINT('',(10.5,-5.10000000000002,40.)) ;
#99481 = CARTESIAN_POINT('',(22.65,-5.40000000000002,40.)) ;
#99482 = CARTESIAN_POINT('',(22.35,-5.10000000000002,40.)) ;
#99483 = CARTESIAN_POINT('Origin',(22.35,-5.40000000000002,40.)) ;
#99484 = CARTESIAN_POINT('',(22.65,-15.1,40.)) ;
#99485 = CARTESIAN_POINT('',(22.65,-15.25,40.)) ;
#99486 = CARTESIAN_POINT('',(22.35,-15.4,40.)) ;
#99487 = CARTESIAN_POINT('Origin',(22.35,-15.1,40.)) ;
#99488 = CARTESIAN_POINT('',(19.65,-15.4,40.)) ;
#99489 = CARTESIAN_POINT('',(19.5,-15.4,40.)) ;
#99490 = CARTESIAN_POINT('',(19.35,-15.1,40.)) ;
#99491 = CARTESIAN_POINT('Origin',(19.65,-15.1,40.)) ;
#99492 = CARTESIAN_POINT('',(19.35,-5.40000000000002,40.)) ;
#99493 = CARTESIAN_POINT('',(19.35,-5.25000000000002,40.)) ;
#99494 = CARTESIAN_POINT('',(19.65,-5.10000000000002,40.)) ;
#99495 = CARTESIAN_POINT('Origin',(19.65,-5.40000000000002,40.)) ;
#99496 = CARTESIAN_POINT('',(22.5,-5.10000000000002,40.)) ;
#99497 = CARTESIAN_POINT('',(34.65,-5.40000000000002,40.)) ;
#99498 = CARTESIAN_POINT('',(34.35,-5.10000000000002,40.)) ;
#99499 = CARTESIAN_POINT('Origin',(34.35,-5.40000000000002,40.)) ;
#99500 = CARTESIAN_POINT('',(34.65,-15.1,40.)) ;
#99501 = CARTESIAN_POINT('',(34.65,-15.25,40.)) ;
#99502 = CARTESIAN_POINT('',(34.35,-15.4,40.)) ;
#99503 = CARTESIAN_POINT('Origin',(34.35,-15.1,40.)) ;
#99504 = CARTESIAN_POINT('',(31.65,-15.4,40.)) ;
#99505 = CARTESIAN_POINT('',(31.5,-15.4,40.)) ;
#99506 = CARTESIAN_POINT('',(31.35,-15.1,40.)) ;
#99507 = CARTESIAN_POINT('Origin',(31.65,-15.1,40.)) ;
#99508 = CARTESIAN_POINT('',(31.35,-5.40000000000002,40.)) ;
#99509 = CARTESIAN_POINT('',(31.35,-5.25000000000002,40.)) ;
#99510 = CARTESIAN_POINT('',(31.65,-5.10000000000002,40.)) ;
#99511 = CARTESIAN_POINT('Origin',(31.65,-5.40000000000002,40.)) ;
#99512 = CARTESIAN_POINT('',(34.5,-5.10000000000002,40.)) ;
#99513 = CARTESIAN_POINT('',(46.65,-5.40000000000002,40.)) ;
#99514 = CARTESIAN_POINT('',(46.35,-5.10000000000002,40.)) ;
#99515 = CARTESIAN_POINT('Origin',(46.35,-5.40000000000002,40.)) ;
#99516 = CARTESIAN_POINT('',(46.65,-15.1,40.)) ;
#99517 = CARTESIAN_POINT('',(46.65,-15.25,40.)) ;
#99518 = CARTESIAN_POINT('',(46.35,-15.4,40.)) ;
#99519 = CARTESIAN_POINT('Origin',(46.35,-15.1,40.)) ;
#99520 = CARTESIAN_POINT('',(43.65,-15.4,40.)) ;
#99521 = CARTESIAN_POINT('',(43.5,-15.4,40.)) ;
#99522 = CARTESIAN_POINT('',(43.35,-15.1,40.)) ;
#99523 = CARTESIAN_POINT('Origin',(43.65,-15.1,40.)) ;
#99524 = CARTESIAN_POINT('',(43.35,-5.40000000000002,40.)) ;
#99525 = CARTESIAN_POINT('',(43.35,-5.25000000000002,40.)) ;
#99526 = CARTESIAN_POINT('',(43.65,-5.10000000000002,40.)) ;
#99527 = CARTESIAN_POINT('Origin',(43.65,-5.40000000000002,40.)) ;
#99528 = CARTESIAN_POINT('',(46.5,-5.10000000000002,40.)) ;
#99529 = CARTESIAN_POINT('',(40.65,-5.40000000000002,40.)) ;
#99530 = CARTESIAN_POINT('',(40.35,-5.10000000000002,40.)) ;
#99531 = CARTESIAN_POINT('Origin',(40.35,-5.40000000000002,40.)) ;
#99532 = CARTESIAN_POINT('',(40.65,-15.1,40.)) ;
#99533 = CARTESIAN_POINT('',(40.65,-15.25,40.)) ;
#99534 = CARTESIAN_POINT('',(40.35,-15.4,40.)) ;
#99535 = CARTESIAN_POINT('Origin',(40.35,-15.1,40.)) ;
#99536 = CARTESIAN_POINT('',(37.65,-15.4,40.)) ;
#99537 = CARTESIAN_POINT('',(37.5,-15.4,40.)) ;
#99538 = CARTESIAN_POINT('',(37.35,-15.1,40.)) ;
#99539 = CARTESIAN_POINT('Origin',(37.65,-15.1,40.)) ;
#99540 = CARTESIAN_POINT('',(37.35,-5.40000000000002,40.)) ;
#99541 = CARTESIAN_POINT('',(37.35,-5.25000000000002,40.)) ;
#99542 = CARTESIAN_POINT('',(37.65,-5.10000000000002,40.)) ;
#99543 = CARTESIAN_POINT('Origin',(37.65,-5.40000000000002,40.)) ;
#99544 = CARTESIAN_POINT('',(40.5,-5.10000000000002,40.)) ;
#99545 = CARTESIAN_POINT('',(28.65,-5.40000000000002,40.)) ;
#99546 = CARTESIAN_POINT('',(28.35,-5.10000000000002,40.)) ;
#99547 = CARTESIAN_POINT('Origin',(28.35,-5.40000000000002,40.)) ;
#99548 = CARTESIAN_POINT('',(28.65,-15.1,40.)) ;
#99549 = CARTESIAN_POINT('',(28.65,-15.25,40.)) ;
#99550 = CARTESIAN_POINT('',(28.35,-15.4,40.)) ;
#99551 = CARTESIAN_POINT('Origin',(28.35,-15.1,40.)) ;
#99552 = CARTESIAN_POINT('',(25.65,-15.4,40.)) ;
#99553 = CARTESIAN_POINT('',(25.5,-15.4,40.)) ;
#99554 = CARTESIAN_POINT('',(25.35,-15.1,40.)) ;
#99555 = CARTESIAN_POINT('Origin',(25.65,-15.1,40.)) ;
#99556 = CARTESIAN_POINT('',(25.35,-5.40000000000002,40.)) ;
#99557 = CARTESIAN_POINT('',(25.35,-5.25000000000002,40.)) ;
#99558 = CARTESIAN_POINT('',(25.65,-5.10000000000002,40.)) ;
#99559 = CARTESIAN_POINT('Origin',(25.65,-5.40000000000002,40.)) ;
#99560 = CARTESIAN_POINT('',(28.5,-5.10000000000002,40.)) ;
#99561 = CARTESIAN_POINT('',(13.35,-15.1,40.)) ;
#99562 = CARTESIAN_POINT('',(13.65,-15.4,40.)) ;
#99563 = CARTESIAN_POINT('Origin',(13.65,-15.1,40.)) ;
#99564 = CARTESIAN_POINT('',(13.35,-5.40000000000002,40.)) ;
#99565 = CARTESIAN_POINT('',(13.35,-5.25000000000002,40.)) ;
#99566 = CARTESIAN_POINT('',(13.65,-5.10000000000002,40.)) ;
#99567 = CARTESIAN_POINT('Origin',(13.65,-5.40000000000002,40.)) ;
#99568 = CARTESIAN_POINT('',(16.35,-5.10000000000002,40.)) ;
#99569 = CARTESIAN_POINT('',(16.5,-5.10000000000002,40.)) ;
#99570 = CARTESIAN_POINT('',(16.65,-5.40000000000002,40.)) ;
#99571 = CARTESIAN_POINT('Origin',(16.35,-5.40000000000002,40.)) ;
#99572 = CARTESIAN_POINT('',(16.65,-15.1,40.)) ;
#99573 = CARTESIAN_POINT('',(16.65,-15.25,40.)) ;
#99574 = CARTESIAN_POINT('',(16.35,-15.4,40.)) ;
#99575 = CARTESIAN_POINT('Origin',(16.35,-15.1,40.)) ;
#99576 = CARTESIAN_POINT('',(13.5,-15.4,40.)) ;
#99577 = CARTESIAN_POINT('Origin',(53.25,-19.75,39.25)) ;
#99578 = CARTESIAN_POINT('',(0.14999999999997,-4.60000000000001,39.25)) ;
#99579 = CARTESIAN_POINT('',(-0.150000000000028,-4.90000000000001,39.25)) ;
#99580 = CARTESIAN_POINT('Origin',(-0.150000000000028,-4.60000000000001,39.25)) ;
#99581 = CARTESIAN_POINT('',(0.14999999999997,-1.75000000000002,39.25)) ;
#99582 = CARTESIAN_POINT('',(0.14999999999997,-1.75000000000001,39.25)) ;
#99583 = CARTESIAN_POINT('',(52.25,-1.75000000000001,39.25)) ;
#99584 = CARTESIAN_POINT('',(53.25,-1.75000000000002,39.25)) ;
#99585 = CARTESIAN_POINT('',(53.,-1.75000000000002,39.25)) ;
#99586 = CARTESIAN_POINT('',(53.25,-1.75000000000002,39.25)) ;
#99587 = CARTESIAN_POINT('',(53.,-19.6,39.25)) ;
#99588 = CARTESIAN_POINT('',(53.,-19.75,39.25)) ;
#99589 = CARTESIAN_POINT('',(0.14999999999997,-19.6,39.25)) ;
#99590 = CARTESIAN_POINT('',(-3.46944695195361E-14,-19.6,39.25)) ;
#99591 = CARTESIAN_POINT('',(0.14999999999997,-6.90000000000001,39.25)) ;
#99592 = CARTESIAN_POINT('',(0.14999999999997,-6.75000000000001,39.25)) ;
#99593 = CARTESIAN_POINT('',(-0.150000000000028,-6.60000000000001,39.25)) ;
#99594 = CARTESIAN_POINT('Origin',(-0.150000000000028,-6.90000000000001,39.25)) ;
#99595 = CARTESIAN_POINT('',(-1.85000000000003,-6.60000000000001,39.25)) ;
#99596 = CARTESIAN_POINT('',(-2.00000000000003,-6.60000000000001,39.25)) ;
#99597 = CARTESIAN_POINT('',(-1.85000000000003,-4.90000000000001,39.25)) ;
#99598 = CARTESIAN_POINT('',(-1.85000000000003,-4.75000000000002,39.25)) ;
#99599 = CARTESIAN_POINT('',(-2.77555756156289E-14,-4.90000000000001,39.25)) ;
#99600 = CARTESIAN_POINT('',(10.65,-15.1,39.25)) ;
#99601 = CARTESIAN_POINT('',(10.35,-15.4,39.25)) ;
#99602 = CARTESIAN_POINT('Origin',(10.35,-15.1,39.25)) ;
#99603 = CARTESIAN_POINT('',(10.65,-5.40000000000002,39.25)) ;
#99604 = CARTESIAN_POINT('',(10.65,-19.75,39.25)) ;
#99605 = CARTESIAN_POINT('',(10.35,-5.10000000000002,39.25)) ;
#99606 = CARTESIAN_POINT('Origin',(10.35,-5.40000000000002,39.25)) ;
#99607 = CARTESIAN_POINT('',(7.64999999999996,-5.10000000000002,39.25)) ;
#99608 = CARTESIAN_POINT('',(53.25,-5.10000000000002,39.25)) ;
#99609 = CARTESIAN_POINT('',(7.34999999999996,-5.40000000000002,39.25)) ;
#99610 = CARTESIAN_POINT('Origin',(7.64999999999996,-5.40000000000002,39.25)) ;
#99611 = CARTESIAN_POINT('',(7.34999999999997,-15.1,39.25)) ;
#99612 = CARTESIAN_POINT('',(7.34999999999997,-19.75,39.25)) ;
#99613 = CARTESIAN_POINT('',(7.64999999999997,-15.4,39.25)) ;
#99614 = CARTESIAN_POINT('Origin',(7.64999999999997,-15.1,39.25)) ;
#99615 = CARTESIAN_POINT('',(53.25,-15.4,39.25)) ;
#99616 = CARTESIAN_POINT('',(22.65,-15.1,39.25)) ;
#99617 = CARTESIAN_POINT('',(22.35,-15.4,39.25)) ;
#99618 = CARTESIAN_POINT('Origin',(22.35,-15.1,39.25)) ;
#99619 = CARTESIAN_POINT('',(22.65,-5.40000000000002,39.25)) ;
#99620 = CARTESIAN_POINT('',(22.65,-19.75,39.25)) ;
#99621 = CARTESIAN_POINT('',(22.35,-5.10000000000002,39.25)) ;
#99622 = CARTESIAN_POINT('Origin',(22.35,-5.40000000000002,39.25)) ;
#99623 = CARTESIAN_POINT('',(19.65,-5.10000000000002,39.25)) ;
#99624 = CARTESIAN_POINT('',(53.25,-5.10000000000002,39.25)) ;
#99625 = CARTESIAN_POINT('',(19.35,-5.40000000000002,39.25)) ;
#99626 = CARTESIAN_POINT('Origin',(19.65,-5.40000000000002,39.25)) ;
#99627 = CARTESIAN_POINT('',(19.35,-15.1,39.25)) ;
#99628 = CARTESIAN_POINT('',(19.35,-19.75,39.25)) ;
#99629 = CARTESIAN_POINT('',(19.65,-15.4,39.25)) ;
#99630 = CARTESIAN_POINT('Origin',(19.65,-15.1,39.25)) ;
#99631 = CARTESIAN_POINT('',(53.25,-15.4,39.25)) ;
#99632 = CARTESIAN_POINT('',(34.65,-15.1,39.25)) ;
#99633 = CARTESIAN_POINT('',(34.35,-15.4,39.25)) ;
#99634 = CARTESIAN_POINT('Origin',(34.35,-15.1,39.25)) ;
#99635 = CARTESIAN_POINT('',(34.65,-5.40000000000002,39.25)) ;
#99636 = CARTESIAN_POINT('',(34.65,-19.75,39.25)) ;
#99637 = CARTESIAN_POINT('',(34.35,-5.10000000000002,39.25)) ;
#99638 = CARTESIAN_POINT('Origin',(34.35,-5.40000000000002,39.25)) ;
#99639 = CARTESIAN_POINT('',(31.65,-5.10000000000002,39.25)) ;
#99640 = CARTESIAN_POINT('',(53.25,-5.10000000000002,39.25)) ;
#99641 = CARTESIAN_POINT('',(31.35,-5.40000000000002,39.25)) ;
#99642 = CARTESIAN_POINT('Origin',(31.65,-5.40000000000002,39.25)) ;
#99643 = CARTESIAN_POINT('',(31.35,-15.1,39.25)) ;
#99644 = CARTESIAN_POINT('',(31.35,-19.75,39.25)) ;
#99645 = CARTESIAN_POINT('',(31.65,-15.4,39.25)) ;
#99646 = CARTESIAN_POINT('Origin',(31.65,-15.1,39.25)) ;
#99647 = CARTESIAN_POINT('',(53.25,-15.4,39.25)) ;
#99648 = CARTESIAN_POINT('',(46.65,-15.1,39.25)) ;
#99649 = CARTESIAN_POINT('',(46.35,-15.4,39.25)) ;
#99650 = CARTESIAN_POINT('Origin',(46.35,-15.1,39.25)) ;
#99651 = CARTESIAN_POINT('',(46.65,-5.40000000000002,39.25)) ;
#99652 = CARTESIAN_POINT('',(46.65,-19.75,39.25)) ;
#99653 = CARTESIAN_POINT('',(46.35,-5.10000000000002,39.25)) ;
#99654 = CARTESIAN_POINT('Origin',(46.35,-5.40000000000002,39.25)) ;
#99655 = CARTESIAN_POINT('',(43.65,-5.10000000000002,39.25)) ;
#99656 = CARTESIAN_POINT('',(53.25,-5.10000000000002,39.25)) ;
#99657 = CARTESIAN_POINT('',(43.35,-5.40000000000002,39.25)) ;
#99658 = CARTESIAN_POINT('Origin',(43.65,-5.40000000000002,39.25)) ;
#99659 = CARTESIAN_POINT('',(43.35,-15.1,39.25)) ;
#99660 = CARTESIAN_POINT('',(43.35,-19.75,39.25)) ;
#99661 = CARTESIAN_POINT('',(43.65,-15.4,39.25)) ;
#99662 = CARTESIAN_POINT('Origin',(43.65,-15.1,39.25)) ;
#99663 = CARTESIAN_POINT('',(53.25,-15.4,39.25)) ;
#99664 = CARTESIAN_POINT('',(40.65,-15.1,39.25)) ;
#99665 = CARTESIAN_POINT('',(40.35,-15.4,39.25)) ;
#99666 = CARTESIAN_POINT('Origin',(40.35,-15.1,39.25)) ;
#99667 = CARTESIAN_POINT('',(40.65,-5.40000000000002,39.25)) ;
#99668 = CARTESIAN_POINT('',(40.65,-19.75,39.25)) ;
#99669 = CARTESIAN_POINT('',(40.35,-5.10000000000002,39.25)) ;
#99670 = CARTESIAN_POINT('Origin',(40.35,-5.40000000000002,39.25)) ;
#99671 = CARTESIAN_POINT('',(37.65,-5.10000000000002,39.25)) ;
#99672 = CARTESIAN_POINT('',(53.25,-5.10000000000002,39.25)) ;
#99673 = CARTESIAN_POINT('',(37.35,-5.40000000000002,39.25)) ;
#99674 = CARTESIAN_POINT('Origin',(37.65,-5.40000000000002,39.25)) ;
#99675 = CARTESIAN_POINT('',(37.35,-15.1,39.25)) ;
#99676 = CARTESIAN_POINT('',(37.35,-19.75,39.25)) ;
#99677 = CARTESIAN_POINT('',(37.65,-15.4,39.25)) ;
#99678 = CARTESIAN_POINT('Origin',(37.65,-15.1,39.25)) ;
#99679 = CARTESIAN_POINT('',(53.25,-15.4,39.25)) ;
#99680 = CARTESIAN_POINT('',(28.65,-15.1,39.25)) ;
#99681 = CARTESIAN_POINT('',(28.35,-15.4,39.25)) ;
#99682 = CARTESIAN_POINT('Origin',(28.35,-15.1,39.25)) ;
#99683 = CARTESIAN_POINT('',(28.65,-5.40000000000002,39.25)) ;
#99684 = CARTESIAN_POINT('',(28.65,-19.75,39.25)) ;
#99685 = CARTESIAN_POINT('',(28.35,-5.10000000000002,39.25)) ;
#99686 = CARTESIAN_POINT('Origin',(28.35,-5.40000000000002,39.25)) ;
#99687 = CARTESIAN_POINT('',(25.65,-5.10000000000002,39.25)) ;
#99688 = CARTESIAN_POINT('',(53.25,-5.10000000000002,39.25)) ;
#99689 = CARTESIAN_POINT('',(25.35,-5.40000000000002,39.25)) ;
#99690 = CARTESIAN_POINT('Origin',(25.65,-5.40000000000002,39.25)) ;
#99691 = CARTESIAN_POINT('',(25.35,-15.1,39.25)) ;
#99692 = CARTESIAN_POINT('',(25.35,-19.75,39.25)) ;
#99693 = CARTESIAN_POINT('',(25.65,-15.4,39.25)) ;
#99694 = CARTESIAN_POINT('Origin',(25.65,-15.1,39.25)) ;
#99695 = CARTESIAN_POINT('',(53.25,-15.4,39.25)) ;
#99696 = CARTESIAN_POINT('',(13.35,-5.40000000000002,39.25)) ;
#99697 = CARTESIAN_POINT('',(13.65,-5.10000000000002,39.25)) ;
#99698 = CARTESIAN_POINT('Origin',(13.65,-5.40000000000002,39.25)) ;
#99699 = CARTESIAN_POINT('',(13.35,-15.1,39.25)) ;
#99700 = CARTESIAN_POINT('',(13.35,-19.75,39.25)) ;
#99701 = CARTESIAN_POINT('',(13.65,-15.4,39.25)) ;
#99702 = CARTESIAN_POINT('Origin',(13.65,-15.1,39.25)) ;
#99703 = CARTESIAN_POINT('',(16.35,-15.4,39.25)) ;
#99704 = CARTESIAN_POINT('',(53.25,-15.4,39.25)) ;
#99705 = CARTESIAN_POINT('',(16.65,-15.1,39.25)) ;
#99706 = CARTESIAN_POINT('Origin',(16.35,-15.1,39.25)) ;
#99707 = CARTESIAN_POINT('',(16.65,-5.40000000000002,39.25)) ;
#99708 = CARTESIAN_POINT('',(16.65,-19.75,39.25)) ;
#99709 = CARTESIAN_POINT('',(16.35,-5.10000000000002,39.25)) ;
#99710 = CARTESIAN_POINT('Origin',(16.35,-5.40000000000002,39.25)) ;
#99711 = CARTESIAN_POINT('',(53.25,-5.10000000000002,39.25)) ;
#99712 = CARTESIAN_POINT('Origin',(53.25,-2.77555756156289E-14,40.)) ;
#99713 = CARTESIAN_POINT('',(0.149999999999965,-2.30070076519351E-14,14.15)) ;
#99714 = CARTESIAN_POINT('',(-0.150000000000035,-2.29518985459734E-14,13.85)) ;
#99715 = CARTESIAN_POINT('Origin',(-0.150000000000035,-2.30121911110048E-14,
14.15)) ;
#99716 = CARTESIAN_POINT('',(0.149999999999963,-2.77555756156289E-14,38.25)) ;
#99717 = CARTESIAN_POINT('',(0.149999999999963,-2.77555756156289E-14,40.)) ;
#99718 = CARTESIAN_POINT('',(52.25,1.95156391047391E-15,38.25)) ;
#99719 = CARTESIAN_POINT('',(53.25,-2.77555756156289E-14,38.25)) ;
#99720 = CARTESIAN_POINT('',(52.25,-1.38777878078145E-14,-38.25)) ;
#99721 = CARTESIAN_POINT('',(52.25,-1.38777878078145E-14,38.25)) ;
#99722 = CARTESIAN_POINT('',(0.149999999999963,-1.38777878078145E-14,-38.25)) ;
#99723 = CARTESIAN_POINT('',(53.25,-1.38777878078145E-14,-38.25)) ;
#99724 = CARTESIAN_POINT('',(0.149999999999965,-1.78083819895545E-14,-14.15)) ;
#99725 = CARTESIAN_POINT('',(0.149999999999963,-2.77555756156289E-14,40.)) ;
#99726 = CARTESIAN_POINT('',(-0.150000000000035,-1.78634910955162E-14,-13.85)) ;
#99727 = CARTESIAN_POINT('Origin',(-0.150000000000035,-1.78080206830744E-14,
-14.15)) ;
#99728 = CARTESIAN_POINT('',(-1.85000000000004,-1.78634910955162E-14,-13.85)) ;
#99729 = CARTESIAN_POINT('',(53.25,-1.78634910955162E-14,-13.85)) ;
#99730 = CARTESIAN_POINT('',(-1.85000000000004,-2.29518985459734E-14,13.85)) ;
#99731 = CARTESIAN_POINT('',(-1.85000000000004,-2.77555756156289E-14,40.)) ;
#99732 = CARTESIAN_POINT('',(53.25,-2.29518985459734E-14,13.85)) ;
#99733 = CARTESIAN_POINT('Origin',(53.25,-0.750000000000028,40.)) ;
#99734 = CARTESIAN_POINT('',(52.25,-0.749999999999998,38.25)) ;
#99735 = CARTESIAN_POINT('',(0.149999999999963,-0.750000000000028,38.25)) ;
#99736 = CARTESIAN_POINT('',(53.25,-0.750000000000028,38.25)) ;
#99737 = CARTESIAN_POINT('',(0.149999999999963,-0.750000000000024,14.15)) ;
#99738 = CARTESIAN_POINT('',(0.149999999999963,-0.750000000000024,14.)) ;
#99739 = CARTESIAN_POINT('',(-0.150000000000035,-0.750000000000024,13.85)) ;
#99740 = CARTESIAN_POINT('Origin',(-0.150000000000035,-0.750000000000024,
14.15)) ;
#99741 = CARTESIAN_POINT('',(-1.85000000000004,-0.750000000000024,13.85)) ;
#99742 = CARTESIAN_POINT('',(-2.00000000000004,-0.750000000000024,13.85)) ;
#99743 = CARTESIAN_POINT('',(-1.85000000000004,-0.750000000000019,-13.85)) ;
#99744 = CARTESIAN_POINT('',(-1.85000000000004,-0.750000000000019,-14.)) ;
#99745 = CARTESIAN_POINT('',(-0.150000000000035,-0.750000000000019,-13.85)) ;
#99746 = CARTESIAN_POINT('',(-4.85722573273506E-14,-0.750000000000019,-13.85)) ;
#99747 = CARTESIAN_POINT('',(0.149999999999963,-0.750000000000018,-14.15)) ;
#99748 = CARTESIAN_POINT('Origin',(-0.150000000000035,-0.750000000000018,
-14.15)) ;
#99749 = CARTESIAN_POINT('',(0.149999999999963,-0.750000000000015,-38.25)) ;
#99750 = CARTESIAN_POINT('',(0.149999999999963,-0.750000000000014,-38.25)) ;
#99751 = CARTESIAN_POINT('',(52.25,-0.750000000000014,-38.25)) ;
#99752 = CARTESIAN_POINT('',(53.25,-0.750000000000015,-38.25)) ;
#99753 = CARTESIAN_POINT('',(52.25,-0.750000000000015,38.25)) ;
#99754 = CARTESIAN_POINT('Origin',(-3.46944695195361E-14,-1.75,-39.25)) ;
#99755 = CARTESIAN_POINT('',(-3.46944695195361E-14,-0.150000000000013,-38.25)) ;
#99756 = CARTESIAN_POINT('',(-3.46944695195361E-14,-0.600000000000014,-38.25)) ;
#99757 = CARTESIAN_POINT('',(-3.46944695195361E-14,0.,-38.25)) ;
#99758 = CARTESIAN_POINT('',(-3.46944695195361E-14,-0.600000000000019,-14.15)) ;
#99759 = CARTESIAN_POINT('',(-3.46944695195361E-14,-0.600000000000019,-14.)) ;
#99760 = CARTESIAN_POINT('',(-3.46944695195361E-14,-0.150000000000018,-14.15)) ;
#99761 = CARTESIAN_POINT('',(-3.46944695195361E-14,-1.38777878078145E-14,
-14.15)) ;
#99762 = CARTESIAN_POINT('',(-3.46944695195361E-14,-0.150000000000013,-39.25)) ;
#99763 = CARTESIAN_POINT('Origin',(-3.46944695195361E-14,-1.75,-39.25)) ;
#99764 = CARTESIAN_POINT('',(-3.46944695195361E-14,-0.150000000000023,14.15)) ;
#99765 = CARTESIAN_POINT('',(-3.46944695195361E-14,-0.600000000000024,14.15)) ;
#99766 = CARTESIAN_POINT('',(-3.46944695195361E-14,-0.750000000000015,14.15)) ;
#99767 = CARTESIAN_POINT('',(-3.46944695195361E-14,-0.600000000000028,38.25)) ;
#99768 = CARTESIAN_POINT('',(-3.46944695195361E-14,-0.600000000000028,38.25)) ;
#99769 = CARTESIAN_POINT('',(-3.46944695195361E-14,-0.150000000000027,38.25)) ;
#99770 = CARTESIAN_POINT('',(-3.46944695195361E-14,-0.750000000000015,38.25)) ;
#99771 = CARTESIAN_POINT('',(-3.46944695195361E-14,-0.150000000000013,-39.25)) ;
#99772 = CARTESIAN_POINT('Origin',(-2.00000000000004,-0.750000000000028,14.)) ;
#99773 = CARTESIAN_POINT('',(-2.00000000000004,-0.600000000000019,-13.85)) ;
#99774 = CARTESIAN_POINT('',(-2.00000000000004,-0.600000000000024,13.85)) ;
#99775 = CARTESIAN_POINT('',(-2.00000000000004,-0.600000000000024,14.)) ;
#99776 = CARTESIAN_POINT('',(-2.00000000000004,-0.150000000000023,13.85)) ;
#99777 = CARTESIAN_POINT('',(-2.00000000000004,-0.750000000000028,13.85)) ;
#99778 = CARTESIAN_POINT('',(-2.00000000000004,-0.150000000000018,-13.85)) ;
#99779 = CARTESIAN_POINT('',(-2.00000000000004,-0.150000000000023,14.)) ;
#99780 = CARTESIAN_POINT('',(-2.00000000000004,-0.750000000000023,-13.85)) ;
#99781 = CARTESIAN_POINT('Origin',(-4.85722573273506E-14,-0.750000000000015,
-14.)) ;
#99782 = CARTESIAN_POINT('',(-0.150000000000035,-0.600000000000019,-14.)) ;
#99783 = CARTESIAN_POINT('',(-1.85000000000004,-0.600000000000019,-14.)) ;
#99784 = CARTESIAN_POINT('',(-2.00000000000005,-0.600000000000019,-14.)) ;
#99785 = CARTESIAN_POINT('',(-1.85000000000004,-0.150000000000018,-14.)) ;
#99786 = CARTESIAN_POINT('',(-1.85000000000004,-0.750000000000015,-14.)) ;
#99787 = CARTESIAN_POINT('',(-0.150000000000035,-0.150000000000018,-14.)) ;
#99788 = CARTESIAN_POINT('',(-4.85722573273506E-14,-0.150000000000018,-14.)) ;
#99789 = CARTESIAN_POINT('',(-0.150000000000035,-0.750000000000008,-14.)) ;
#99790 = CARTESIAN_POINT('Origin',(-3.46944695195361E-14,-0.750000000000015,
14.)) ;
#99791 = CARTESIAN_POINT('',(-1.85000000000004,-0.600000000000024,14.)) ;
#99792 = CARTESIAN_POINT('',(-0.150000000000035,-0.600000000000024,14.)) ;
#99793 = CARTESIAN_POINT('',(-3.46944695195361E-14,-0.600000000000024,14.)) ;
#99794 = CARTESIAN_POINT('',(-0.150000000000035,-0.150000000000023,14.)) ;
#99795 = CARTESIAN_POINT('',(-0.150000000000035,-1.38502332548336E-14,14.)) ;
#99796 = CARTESIAN_POINT('',(-1.85000000000004,-0.150000000000023,14.)) ;
#99797 = CARTESIAN_POINT('',(-3.46944695195361E-14,-0.150000000000023,14.)) ;
#99798 = CARTESIAN_POINT('',(-1.85000000000004,-0.750000000000015,14.)) ;
#99799 = CARTESIAN_POINT('Origin',(-3.46944695195361E-14,-1.75000000000002,
38.25)) ;
#99800 = CARTESIAN_POINT('',(-3.46944695195361E-14,-1.75000000000001,39.4)) ;
#99801 = CARTESIAN_POINT('Origin',(-3.46944695195361E-14,-1.75000000000003,
38.25)) ;
#99802 = CARTESIAN_POINT('',(-3.46944695195361E-14,-1.75000000000001,39.85)) ;
#99803 = CARTESIAN_POINT('',(-3.46944695195361E-14,-1.75000000000001,40.)) ;
#99804 = CARTESIAN_POINT('Origin',(-3.46944695195361E-14,-1.75000000000003,
38.25)) ;
#99805 = CARTESIAN_POINT('Origin',(52.25,-1.75000000000002,38.25)) ;
#99806 = CARTESIAN_POINT('Origin',(52.25,-1.75000000000002,38.25)) ;
#99807 = CARTESIAN_POINT('',(52.25,-0.750000000000015,38.25)) ;
#99808 = CARTESIAN_POINT('Origin',(52.25,-1.75000000000002,38.25)) ;
#99809 = CARTESIAN_POINT('',(52.25,-1.75000000000001,40.)) ;
#99810 = CARTESIAN_POINT('Origin',(-26.1749993327458,-1.75000000000003,38.25)) ;
#99811 = CARTESIAN_POINT('Origin',(0.149999999999966,-1.75000000000003,38.25)) ;
#99812 = CARTESIAN_POINT('Origin',(-26.1749993327458,-1.75000000000003,38.25)) ;
#99813 = CARTESIAN_POINT('Origin',(0.149999999999966,-1.75000000000003,38.25)) ;
#99814 = CARTESIAN_POINT('Origin',(53.25,-19.75,39.25)) ;
#99815 = CARTESIAN_POINT('',(0.149999999999972,-19.75,39.85)) ;
#99816 = CARTESIAN_POINT('',(0.149999999999972,-19.75,39.4)) ;
#99817 = CARTESIAN_POINT('',(0.14999999999997,-19.75,39.25)) ;
#99818 = CARTESIAN_POINT('',(53.,-19.75,39.4)) ;
#99819 = CARTESIAN_POINT('',(53.15,-19.75,39.4)) ;
#99820 = CARTESIAN_POINT('',(53.,-19.75,39.85)) ;
#99821 = CARTESIAN_POINT('',(53.,-19.75,40.)) ;
#99822 = CARTESIAN_POINT('',(53.25,-19.75,39.85)) ;
#99823 = CARTESIAN_POINT('Origin',(-2.77555756156289E-14,-0.750000000000015,
38.25)) ;
#99824 = CARTESIAN_POINT('',(-2.77555756156289E-14,-6.90000000000001,39.4)) ;
#99825 = CARTESIAN_POINT('',(-2.77555756156289E-14,-19.6,39.4)) ;
#99826 = CARTESIAN_POINT('',(-2.77555756156289E-14,-19.75,39.4)) ;
#99827 = CARTESIAN_POINT('',(-2.77555756156289E-14,-19.6,39.85)) ;
#99828 = CARTESIAN_POINT('',(-2.77555756156289E-14,-19.6,38.25)) ;
#99829 = CARTESIAN_POINT('',(-2.77555756156289E-14,-6.90000000000001,39.85)) ;
#99830 = CARTESIAN_POINT('',(-2.77555756156289E-14,-0.750000000000015,39.85)) ;
#99831 = CARTESIAN_POINT('',(-2.77555756156289E-14,-6.90000000000001,39.25)) ;
#99832 = CARTESIAN_POINT('Origin',(-2.77555756156289E-14,-6.75000000000001,
39.25)) ;
#99833 = CARTESIAN_POINT('',(-1.85000000000003,-6.75000000000001,39.4)) ;
#99834 = CARTESIAN_POINT('',(-0.150000000000028,-6.75000000000001,39.4)) ;
#99835 = CARTESIAN_POINT('',(-2.77555756156289E-14,-6.75000000000001,39.4)) ;
#99836 = CARTESIAN_POINT('',(-0.150000000000028,-6.75000000000001,39.85)) ;
#99837 = CARTESIAN_POINT('',(-0.150000000000028,-6.75000000000001,40.)) ;
#99838 = CARTESIAN_POINT('',(-1.85000000000003,-6.75000000000001,39.85)) ;
#99839 = CARTESIAN_POINT('',(-2.77555756156289E-14,-6.75000000000001,39.85)) ;
#99840 = CARTESIAN_POINT('',(-1.85000000000003,-6.75000000000001,39.25)) ;
#99841 = CARTESIAN_POINT('Origin',(-2.00000000000003,-4.75000000000002,39.25)) ;
#99842 = CARTESIAN_POINT('',(-2.00000000000003,-4.90000000000001,39.4)) ;
#99843 = CARTESIAN_POINT('',(-2.00000000000003,-6.60000000000001,39.4)) ;
#99844 = CARTESIAN_POINT('',(-2.00000000000003,-6.75000000000002,39.4)) ;
#99845 = CARTESIAN_POINT('',(-2.00000000000003,-6.60000000000001,39.85)) ;
#99846 = CARTESIAN_POINT('',(-2.00000000000003,-6.60000000000001,39.25)) ;
#99847 = CARTESIAN_POINT('',(-2.00000000000003,-4.90000000000001,39.85)) ;
#99848 = CARTESIAN_POINT('',(-2.00000000000003,-4.75000000000002,39.85)) ;
#99849 = CARTESIAN_POINT('',(-2.00000000000003,-4.90000000000001,39.25)) ;
#99850 = CARTESIAN_POINT('Origin',(-2.77555756156289E-14,-4.75000000000001,
39.25)) ;
#99851 = CARTESIAN_POINT('',(-0.150000000000028,-4.75000000000001,39.4)) ;
#99852 = CARTESIAN_POINT('',(-1.85000000000003,-4.75000000000001,39.4)) ;
#99853 = CARTESIAN_POINT('',(-2.00000000000003,-4.75000000000001,39.4)) ;
#99854 = CARTESIAN_POINT('',(-1.85000000000003,-4.75000000000001,39.85)) ;
#99855 = CARTESIAN_POINT('',(-1.85000000000003,-4.75000000000001,39.25)) ;
#99856 = CARTESIAN_POINT('',(-0.150000000000028,-4.75000000000001,39.85)) ;
#99857 = CARTESIAN_POINT('',(-2.77555756156289E-14,-4.75000000000001,39.85)) ;
#99858 = CARTESIAN_POINT('',(-0.150000000000028,-4.75000000000001,39.25)) ;
#99859 = CARTESIAN_POINT('Origin',(53.1499999999998,56.3581964958473,39.25)) ;
#99860 = CARTESIAN_POINT('',(53.15,-1.90000000000001,39.85)) ;
#99861 = CARTESIAN_POINT('',(53.15,-19.6,39.85)) ;
#99862 = CARTESIAN_POINT('',(53.15,-19.75,39.85)) ;
#99863 = CARTESIAN_POINT('',(53.15,-19.6,39.4)) ;
#99864 = CARTESIAN_POINT('',(53.15,-19.6,39.25)) ;
#99865 = CARTESIAN_POINT('',(53.15,-1.90000000000001,39.4)) ;
#99866 = CARTESIAN_POINT('',(53.1499999999998,56.3581964958473,39.4)) ;
#99867 = CARTESIAN_POINT('',(53.15,-1.90000000000001,40.)) ;
#99868 = CARTESIAN_POINT('Origin',(-2.77555756156289E-14,-0.750000000000015,
38.25)) ;
#99869 = CARTESIAN_POINT('',(-2.77555756156289E-14,-4.60000000000001,39.4)) ;
#99870 = CARTESIAN_POINT('',(-2.77555756156289E-14,-4.75000000000001,39.4)) ;
#99871 = CARTESIAN_POINT('',(-2.77555756156289E-14,-4.60000000000001,39.85)) ;
#99872 = CARTESIAN_POINT('',(-2.77555756156289E-14,-4.60000000000001,40.)) ;
#99873 = CARTESIAN_POINT('',(-2.77555756156289E-14,-0.750000000000015,39.85)) ;
#99874 = CARTESIAN_POINT('Origin',(-3.46944695195361E-14,-1.75000000000002,
7.18201007936591E-15)) ;
#99875 = CARTESIAN_POINT('',(53.,-1.75000000000001,39.25)) ;
#99876 = CARTESIAN_POINT('Origin',(54.,-1.74999999999998,-40.)) ;
#99877 = CARTESIAN_POINT('',(53.85,-1.89999999999998,-40.)) ;
#99878 = CARTESIAN_POINT('',(53.8500000000001,-19.6,-40.)) ;
#99879 = CARTESIAN_POINT('',(53.8500000000001,-19.75,-40.)) ;
#99880 = CARTESIAN_POINT('',(53.4000000000001,-19.6,-40.)) ;
#99881 = CARTESIAN_POINT('',(53.2500000000001,-19.6,-40.)) ;
#99882 = CARTESIAN_POINT('',(53.4,-1.89999999999998,-40.)) ;
#99883 = CARTESIAN_POINT('',(53.4,-1.74999999999998,-40.)) ;
#99884 = CARTESIAN_POINT('',(54.,-1.89999999999998,-40.)) ;
#99885 = CARTESIAN_POINT('Origin',(54.0000000000001,-19.75,-38.25)) ;
#99886 = CARTESIAN_POINT('',(53.8500000000001,-19.75,-39.85)) ;
#99887 = CARTESIAN_POINT('',(53.8500000000001,-19.75,39.85)) ;
#99888 = CARTESIAN_POINT('',(53.8500000000001,-19.75,-38.25)) ;
#99889 = CARTESIAN_POINT('',(53.4000000000001,-19.75,39.85)) ;
#99890 = CARTESIAN_POINT('',(54.0000000000001,-19.75,39.85)) ;
#99891 = CARTESIAN_POINT('',(53.4000000000001,-19.75,-39.85)) ;
#99892 = CARTESIAN_POINT('',(53.4000000000001,-19.75,-40.)) ;
#99893 = CARTESIAN_POINT('',(54.0000000000001,-19.75,-39.85)) ;
#99894 = CARTESIAN_POINT('Origin',(54.,-1.74999999999999,40.)) ;
#99895 = CARTESIAN_POINT('',(53.8500000000001,-19.6,40.)) ;
#99896 = CARTESIAN_POINT('',(53.85,-1.89999999999999,40.)) ;
#99897 = CARTESIAN_POINT('',(53.85,-1.74999999999999,40.)) ;
#99898 = CARTESIAN_POINT('',(53.4,-1.9,40.)) ;
#99899 = CARTESIAN_POINT('',(54.,-1.89999999999999,40.)) ;
#99900 = CARTESIAN_POINT('',(53.4000000000001,-19.6,40.)) ;
#99901 = CARTESIAN_POINT('',(53.4000000000001,-19.75,40.)) ;
#99902 = CARTESIAN_POINT('',(54.0000000000001,-19.6,40.)) ;
#99903 = CARTESIAN_POINT('Origin',(54.,-1.74999999999999,38.25)) ;
#99904 = CARTESIAN_POINT('',(54.,-1.74999999999999,39.85)) ;
#99905 = CARTESIAN_POINT('',(53.25,-1.74999999999999,38.25)) ;
#99906 = CARTESIAN_POINT('Origin',(54.,-1.74999999999998,-38.25)) ;
#99907 = CARTESIAN_POINT('',(54.,-1.74999999999998,-39.85)) ;
#99908 = CARTESIAN_POINT('',(53.25,-1.74999999999998,-38.25)) ;
#99909 = CARTESIAN_POINT('Origin',(52.25,-1.74999999999998,-38.25)) ;
#99910 = CARTESIAN_POINT('Origin',(52.25,-1.74999999999998,-38.25)) ;
#99911 = CARTESIAN_POINT('',(52.25,-0.750000000000001,-38.25)) ;
#99912 = CARTESIAN_POINT('Origin',(52.25,-1.74999999999998,-38.25)) ;
#99913 = CARTESIAN_POINT('Origin',(52.25,-1.75,38.25)) ;
#99914 = CARTESIAN_POINT('Origin',(52.25,-1.75,38.25)) ;
#99915 = CARTESIAN_POINT('Origin',(52.25,-1.75,38.25)) ;
#99916 = CARTESIAN_POINT('Origin',(52.25,-1.74999999999998,-76.5341585842897)) ;
#99917 = CARTESIAN_POINT('Origin',(52.25,-1.74999999999998,-76.5341585842897)) ;
#99918 = CARTESIAN_POINT('Origin',(-2.77555756156289E-14,-1.75000000000001,
-38.25)) ;
#99919 = CARTESIAN_POINT('',(-3.46944695195361E-14,-1.74999999999999,-39.4)) ;
#99920 = CARTESIAN_POINT('',(-3.46944695195361E-14,-1.74999999999999,-39.85)) ;
#99921 = CARTESIAN_POINT('',(-3.46944695195361E-14,-1.74999999999999,-39.25)) ;
#99922 = CARTESIAN_POINT('Origin',(-2.77555756156289E-14,-1.75000000000001,
-38.25)) ;
#99923 = CARTESIAN_POINT('Origin',(-2.77555756156289E-14,-1.75000000000001,
-38.25)) ;
#99924 = CARTESIAN_POINT('Origin',(52.25,-1.75000000000001,-38.25)) ;
#99925 = CARTESIAN_POINT('Origin',(52.25,-1.75000000000001,-38.25)) ;
#99926 = CARTESIAN_POINT('',(52.25,-1.74999999999999,-39.25)) ;
#99927 = CARTESIAN_POINT('Origin',(52.25,-1.75000000000001,-38.25)) ;
#99928 = CARTESIAN_POINT('Origin',(78.4249993327457,-1.75000000000001,-38.25)) ;
#99929 = CARTESIAN_POINT('Origin',(0.14999999999997,-1.75000000000001,-38.25)) ;
#99930 = CARTESIAN_POINT('Origin',(78.4249993327457,-1.75000000000001,-38.25)) ;
#99931 = CARTESIAN_POINT('Origin',(0.14999999999997,-1.75000000000001,-38.25)) ;
#99932 = CARTESIAN_POINT('Origin',(-2.77555756156289E-14,-4.75,-39.25)) ;
#99933 = CARTESIAN_POINT('',(-1.85000000000003,-4.75,-39.4)) ;
#99934 = CARTESIAN_POINT('',(-0.150000000000035,-4.75,-39.4)) ;
#99935 = CARTESIAN_POINT('',(-2.77555756156289E-14,-4.75,-39.4)) ;
#99936 = CARTESIAN_POINT('',(-0.150000000000035,-4.75,-39.85)) ;
#99937 = CARTESIAN_POINT('',(-0.150000000000035,-4.75,-40.)) ;
#99938 = CARTESIAN_POINT('',(-1.85000000000003,-4.75,-39.85)) ;
#99939 = CARTESIAN_POINT('',(-2.00000000000003,-4.75,-39.85)) ;
#99940 = CARTESIAN_POINT('',(-1.85000000000003,-4.75,-39.25)) ;
#99941 = CARTESIAN_POINT('Origin',(-2.00000000000003,-4.75000000000001,-39.25)) ;
#99942 = CARTESIAN_POINT('',(-2.00000000000003,-6.60000000000001,-39.4)) ;
#99943 = CARTESIAN_POINT('',(-2.00000000000003,-4.9,-39.4)) ;
#99944 = CARTESIAN_POINT('',(-2.00000000000003,-4.75000000000001,-39.4)) ;
#99945 = CARTESIAN_POINT('',(-2.00000000000003,-4.9,-39.85)) ;
#99946 = CARTESIAN_POINT('',(-2.00000000000003,-4.9,-39.25)) ;
#99947 = CARTESIAN_POINT('',(-2.00000000000003,-6.60000000000001,-39.85)) ;
#99948 = CARTESIAN_POINT('',(-2.00000000000003,-6.75000000000001,-39.85)) ;
#99949 = CARTESIAN_POINT('',(-2.00000000000003,-6.60000000000001,-39.25)) ;
#99950 = CARTESIAN_POINT('Origin',(-3.46944695195361E-14,-6.75000000000001,
-39.25)) ;
#99951 = CARTESIAN_POINT('',(-0.150000000000035,-6.75000000000001,-39.4)) ;
#99952 = CARTESIAN_POINT('',(-1.85000000000003,-6.75000000000001,-39.4)) ;
#99953 = CARTESIAN_POINT('',(-3.46944695195361E-14,-6.75000000000001,-39.4)) ;
#99954 = CARTESIAN_POINT('',(-1.85000000000003,-6.75000000000001,-39.85)) ;
#99955 = CARTESIAN_POINT('',(-1.85000000000003,-6.75000000000001,-39.25)) ;
#99956 = CARTESIAN_POINT('',(-0.150000000000035,-6.75000000000001,-39.85)) ;
#99957 = CARTESIAN_POINT('',(-3.46944695195361E-14,-6.75000000000001,-39.85)) ;
#99958 = CARTESIAN_POINT('',(-0.150000000000035,-6.75000000000001,-39.25)) ;
#99959 = CARTESIAN_POINT('Origin',(-3.46944695195361E-14,-1.74999999999999,
-38.25)) ;
#99960 = CARTESIAN_POINT('',(-3.46944695195361E-14,-19.6,-39.4)) ;
#99961 = CARTESIAN_POINT('',(-3.46944695195361E-14,-6.90000000000001,-39.4)) ;
#99962 = CARTESIAN_POINT('',(-3.46944695195361E-14,-1.74999999999999,-39.4)) ;
#99963 = CARTESIAN_POINT('',(-3.46944695195361E-14,-6.90000000000001,-39.85)) ;
#99964 = CARTESIAN_POINT('',(-3.46944695195361E-14,-6.90000000000001,-40.)) ;
#99965 = CARTESIAN_POINT('',(-3.46944695195361E-14,-19.6,-39.85)) ;
#99966 = CARTESIAN_POINT('',(-3.46944695195361E-14,-19.75,-39.85)) ;
#99967 = CARTESIAN_POINT('',(-3.46944695195361E-14,-19.6,-39.25)) ;
#99968 = CARTESIAN_POINT('Origin',(53.25,-19.75,-40.)) ;
#99969 = CARTESIAN_POINT('',(53.0000000000001,-19.75,-39.4)) ;
#99970 = CARTESIAN_POINT('',(0.149999999999965,-19.75,-39.4)) ;
#99971 = CARTESIAN_POINT('',(-2.77555756156289E-14,-19.75,-39.4)) ;
#99972 = CARTESIAN_POINT('',(0.149999999999965,-19.75,-39.85)) ;
#99973 = CARTESIAN_POINT('',(0.149999999999965,-19.75,-40.)) ;
#99974 = CARTESIAN_POINT('',(53.0000000000001,-19.75,-39.85)) ;
#99975 = CARTESIAN_POINT('',(53.25,-19.75,-39.85)) ;
#99976 = CARTESIAN_POINT('',(53.0000000000001,-19.75,-40.)) ;
#99977 = CARTESIAN_POINT('Origin',(53.1499999999998,56.3581964958473,-39.25)) ;
#99978 = CARTESIAN_POINT('',(53.1500000000001,-19.6,-39.4)) ;
#99979 = CARTESIAN_POINT('',(53.1500000000001,-19.6,-39.85)) ;
#99980 = CARTESIAN_POINT('',(53.1500000000001,-19.6,-39.25)) ;
#99981 = CARTESIAN_POINT('',(53.15,-1.89999999999998,-39.85)) ;
#99982 = CARTESIAN_POINT('',(53.1499999999998,56.3581964958473,-39.85)) ;
#99983 = CARTESIAN_POINT('',(53.15,-1.89999999999998,-39.4)) ;
#99984 = CARTESIAN_POINT('',(53.15,-1.89999999999999,-39.25)) ;
#99985 = CARTESIAN_POINT('',(53.1500000000001,-19.75,-39.4)) ;
#99986 = CARTESIAN_POINT('Origin',(-3.46944695195361E-14,-1.75000000000002,
-1.38777878078145E-14)) ;
#99987 = CARTESIAN_POINT('',(53.,-1.75000000000002,-1.38777878078145E-14)) ;
#99988 = CARTESIAN_POINT('Origin',(-3.46944695195361E-14,-1.74999999999999,
-38.25)) ;
#99989 = CARTESIAN_POINT('',(-3.46944695195361E-14,-4.6,-39.85)) ;
#99990 = CARTESIAN_POINT('',(-3.46944695195361E-14,-4.6,-39.4)) ;
#99991 = CARTESIAN_POINT('',(-3.46944695195361E-14,-4.6,-39.25)) ;
#99992 = CARTESIAN_POINT('',(-3.46944695195361E-14,-1.74999999999999,-39.4)) ;
#99993 = CARTESIAN_POINT('',(-3.46944695195361E-14,-4.75,-39.85)) ;
#99994 = CARTESIAN_POINT('Origin',(43.5,-15.25,-40.001)) ;
#99995 = CARTESIAN_POINT('',(43.65,-15.25,39.85)) ;
#99996 = CARTESIAN_POINT('',(46.35,-15.25,39.85)) ;
#99997 = CARTESIAN_POINT('',(46.5,-15.25,39.85)) ;
#99998 = CARTESIAN_POINT('',(46.35,-15.25,39.4)) ;
#99999 = CARTESIAN_POINT('',(46.35,-15.25,39.25)) ;
#100000 = CARTESIAN_POINT('',(43.65,-15.25,39.4)) ;
#100001 = CARTESIAN_POINT('',(43.5,-15.25,39.4)) ;
#100002 = CARTESIAN_POINT('',(43.65,-15.25,40.)) ;
#100003 = CARTESIAN_POINT('Origin',(43.5,-5.25000000000002,-40.001)) ;
#100004 = CARTESIAN_POINT('',(43.5,-5.40000000000002,39.85)) ;
#100005 = CARTESIAN_POINT('',(43.5,-15.1,39.85)) ;
#100006 = CARTESIAN_POINT('',(43.5,-15.25,39.85)) ;
#100007 = CARTESIAN_POINT('',(43.5,-15.1,39.4)) ;
#100008 = CARTESIAN_POINT('',(43.5,-15.1,39.25)) ;
#100009 = CARTESIAN_POINT('',(43.5,-5.40000000000002,39.4)) ;
#100010 = CARTESIAN_POINT('',(43.5,-5.25000000000002,39.4)) ;
#100011 = CARTESIAN_POINT('',(43.5,-5.40000000000002,40.)) ;
#100012 = CARTESIAN_POINT('Origin',(43.5,-5.25000000000002,-40.001)) ;
#100013 = CARTESIAN_POINT('',(43.65,-5.25000000000002,39.4)) ;
#100014 = CARTESIAN_POINT('',(46.35,-5.25000000000002,39.4)) ;
#100015 = CARTESIAN_POINT('',(43.5,-5.25000000000002,39.4)) ;
#100016 = CARTESIAN_POINT('',(46.35,-5.25000000000002,39.85)) ;
#100017 = CARTESIAN_POINT('',(46.35,-5.25000000000002,40.)) ;
#100018 = CARTESIAN_POINT('',(43.65,-5.25000000000002,39.85)) ;
#100019 = CARTESIAN_POINT('',(43.5,-5.25000000000002,39.85)) ;
#100020 = CARTESIAN_POINT('',(43.65,-5.25000000000002,39.25)) ;
#100021 = CARTESIAN_POINT('Origin',(46.5,-5.25000000000002,-40.001)) ;
#100022 = CARTESIAN_POINT('',(46.5,-15.1,39.85)) ;
#100023 = CARTESIAN_POINT('',(46.5,-5.40000000000002,39.85)) ;
#100024 = CARTESIAN_POINT('',(46.5,-5.25000000000002,39.85)) ;
#100025 = CARTESIAN_POINT('',(46.5,-5.40000000000002,39.4)) ;
#100026 = CARTESIAN_POINT('',(46.5,-5.40000000000002,39.25)) ;
#100027 = CARTESIAN_POINT('',(46.5,-15.1,39.4)) ;
#100028 = CARTESIAN_POINT('',(46.5,-5.25000000000002,39.4)) ;
#100029 = CARTESIAN_POINT('',(46.5,-15.1,40.)) ;
#100030 = CARTESIAN_POINT('Origin',(37.5,-15.25,-40.001)) ;
#100031 = CARTESIAN_POINT('',(37.65,-15.25,39.85)) ;
#100032 = CARTESIAN_POINT('',(40.35,-15.25,39.85)) ;
#100033 = CARTESIAN_POINT('',(40.5,-15.25,39.85)) ;
#100034 = CARTESIAN_POINT('',(40.35,-15.25,39.4)) ;
#100035 = CARTESIAN_POINT('',(40.35,-15.25,39.25)) ;
#100036 = CARTESIAN_POINT('',(37.65,-15.25,39.4)) ;
#100037 = CARTESIAN_POINT('',(37.5,-15.25,39.4)) ;
#100038 = CARTESIAN_POINT('',(37.65,-15.25,40.)) ;
#100039 = CARTESIAN_POINT('Origin',(37.5,-5.25000000000002,-40.001)) ;
#100040 = CARTESIAN_POINT('',(37.5,-5.40000000000002,39.85)) ;
#100041 = CARTESIAN_POINT('',(37.5,-15.1,39.85)) ;
#100042 = CARTESIAN_POINT('',(37.5,-15.25,39.85)) ;
#100043 = CARTESIAN_POINT('',(37.5,-15.1,39.4)) ;
#100044 = CARTESIAN_POINT('',(37.5,-15.1,39.25)) ;
#100045 = CARTESIAN_POINT('',(37.5,-5.40000000000002,39.4)) ;
#100046 = CARTESIAN_POINT('',(37.5,-5.25000000000002,39.4)) ;
#100047 = CARTESIAN_POINT('',(37.5,-5.40000000000002,40.)) ;
#100048 = CARTESIAN_POINT('Origin',(37.5,-5.25000000000002,-40.001)) ;
#100049 = CARTESIAN_POINT('',(37.65,-5.25000000000002,39.4)) ;
#100050 = CARTESIAN_POINT('',(40.35,-5.25000000000002,39.4)) ;
#100051 = CARTESIAN_POINT('',(37.5,-5.25000000000002,39.4)) ;
#100052 = CARTESIAN_POINT('',(40.35,-5.25000000000002,39.85)) ;
#100053 = CARTESIAN_POINT('',(40.35,-5.25000000000002,40.)) ;
#100054 = CARTESIAN_POINT('',(37.65,-5.25000000000002,39.85)) ;
#100055 = CARTESIAN_POINT('',(37.5,-5.25000000000002,39.85)) ;
#100056 = CARTESIAN_POINT('',(37.65,-5.25000000000002,39.25)) ;
#100057 = CARTESIAN_POINT('Origin',(40.5,-5.25000000000002,-40.001)) ;
#100058 = CARTESIAN_POINT('',(40.5,-15.1,39.85)) ;
#100059 = CARTESIAN_POINT('',(40.5,-5.40000000000002,39.85)) ;
#100060 = CARTESIAN_POINT('',(40.5,-5.25000000000002,39.85)) ;
#100061 = CARTESIAN_POINT('',(40.5,-5.40000000000002,39.4)) ;
#100062 = CARTESIAN_POINT('',(40.5,-5.40000000000002,39.25)) ;
#100063 = CARTESIAN_POINT('',(40.5,-15.1,39.4)) ;
#100064 = CARTESIAN_POINT('',(40.5,-5.25000000000002,39.4)) ;
#100065 = CARTESIAN_POINT('',(40.5,-15.1,40.)) ;
#100066 = CARTESIAN_POINT('Origin',(31.5,-15.25,-40.001)) ;
#100067 = CARTESIAN_POINT('',(31.65,-15.25,39.85)) ;
#100068 = CARTESIAN_POINT('',(34.35,-15.25,39.85)) ;
#100069 = CARTESIAN_POINT('',(34.5,-15.25,39.85)) ;
#100070 = CARTESIAN_POINT('',(34.35,-15.25,39.4)) ;
#100071 = CARTESIAN_POINT('',(34.35,-15.25,39.25)) ;
#100072 = CARTESIAN_POINT('',(31.65,-15.25,39.4)) ;
#100073 = CARTESIAN_POINT('',(31.5,-15.25,39.4)) ;
#100074 = CARTESIAN_POINT('',(31.65,-15.25,40.)) ;
#100075 = CARTESIAN_POINT('Origin',(31.5,-5.25000000000002,-40.001)) ;
#100076 = CARTESIAN_POINT('',(31.5,-5.40000000000002,39.85)) ;
#100077 = CARTESIAN_POINT('',(31.5,-15.1,39.85)) ;
#100078 = CARTESIAN_POINT('',(31.5,-15.25,39.85)) ;
#100079 = CARTESIAN_POINT('',(31.5,-15.1,39.4)) ;
#100080 = CARTESIAN_POINT('',(31.5,-15.1,39.25)) ;
#100081 = CARTESIAN_POINT('',(31.5,-5.40000000000002,39.4)) ;
#100082 = CARTESIAN_POINT('',(31.5,-5.25000000000002,39.4)) ;
#100083 = CARTESIAN_POINT('',(31.5,-5.40000000000002,40.)) ;
#100084 = CARTESIAN_POINT('Origin',(31.5,-5.25000000000002,-40.001)) ;
#100085 = CARTESIAN_POINT('',(31.65,-5.25000000000002,39.4)) ;
#100086 = CARTESIAN_POINT('',(34.35,-5.25000000000002,39.4)) ;
#100087 = CARTESIAN_POINT('',(31.5,-5.25000000000002,39.4)) ;
#100088 = CARTESIAN_POINT('',(34.35,-5.25000000000002,39.85)) ;
#100089 = CARTESIAN_POINT('',(34.35,-5.25000000000002,40.)) ;
#100090 = CARTESIAN_POINT('',(31.65,-5.25000000000002,39.85)) ;
#100091 = CARTESIAN_POINT('',(31.5,-5.25000000000002,39.85)) ;
#100092 = CARTESIAN_POINT('',(31.65,-5.25000000000002,39.25)) ;
#100093 = CARTESIAN_POINT('Origin',(34.5,-5.25000000000002,-40.001)) ;
#100094 = CARTESIAN_POINT('',(34.5,-15.1,39.85)) ;
#100095 = CARTESIAN_POINT('',(34.5,-5.40000000000002,39.85)) ;
#100096 = CARTESIAN_POINT('',(34.5,-5.25000000000002,39.85)) ;
#100097 = CARTESIAN_POINT('',(34.5,-5.40000000000002,39.4)) ;
#100098 = CARTESIAN_POINT('',(34.5,-5.40000000000002,39.25)) ;
#100099 = CARTESIAN_POINT('',(34.5,-15.1,39.4)) ;
#100100 = CARTESIAN_POINT('',(34.5,-5.25000000000002,39.4)) ;
#100101 = CARTESIAN_POINT('',(34.5,-15.1,40.)) ;
#100102 = CARTESIAN_POINT('Origin',(25.5,-15.25,-40.001)) ;
#100103 = CARTESIAN_POINT('',(25.65,-15.25,39.85)) ;
#100104 = CARTESIAN_POINT('',(28.35,-15.25,39.85)) ;
#100105 = CARTESIAN_POINT('',(28.5,-15.25,39.85)) ;
#100106 = CARTESIAN_POINT('',(28.35,-15.25,39.4)) ;
#100107 = CARTESIAN_POINT('',(28.35,-15.25,39.25)) ;
#100108 = CARTESIAN_POINT('',(25.65,-15.25,39.4)) ;
#100109 = CARTESIAN_POINT('',(25.5,-15.25,39.4)) ;
#100110 = CARTESIAN_POINT('',(25.65,-15.25,40.)) ;
#100111 = CARTESIAN_POINT('Origin',(25.5,-5.25000000000002,-40.001)) ;
#100112 = CARTESIAN_POINT('',(25.5,-5.40000000000002,39.85)) ;
#100113 = CARTESIAN_POINT('',(25.5,-15.1,39.85)) ;
#100114 = CARTESIAN_POINT('',(25.5,-15.25,39.85)) ;
#100115 = CARTESIAN_POINT('',(25.5,-15.1,39.4)) ;
#100116 = CARTESIAN_POINT('',(25.5,-15.1,39.25)) ;
#100117 = CARTESIAN_POINT('',(25.5,-5.40000000000002,39.4)) ;
#100118 = CARTESIAN_POINT('',(25.5,-5.25000000000002,39.4)) ;
#100119 = CARTESIAN_POINT('',(25.5,-5.40000000000002,40.)) ;
#100120 = CARTESIAN_POINT('Origin',(25.5,-5.25000000000002,-40.001)) ;
#100121 = CARTESIAN_POINT('',(25.65,-5.25000000000002,39.4)) ;
#100122 = CARTESIAN_POINT('',(28.35,-5.25000000000002,39.4)) ;
#100123 = CARTESIAN_POINT('',(25.5,-5.25000000000002,39.4)) ;
#100124 = CARTESIAN_POINT('',(28.35,-5.25000000000002,39.85)) ;
#100125 = CARTESIAN_POINT('',(28.35,-5.25000000000002,40.)) ;
#100126 = CARTESIAN_POINT('',(25.65,-5.25000000000002,39.85)) ;
#100127 = CARTESIAN_POINT('',(25.5,-5.25000000000002,39.85)) ;
#100128 = CARTESIAN_POINT('',(25.65,-5.25000000000002,39.25)) ;
#100129 = CARTESIAN_POINT('Origin',(28.5,-5.25000000000002,-40.001)) ;
#100130 = CARTESIAN_POINT('',(28.5,-15.1,39.85)) ;
#100131 = CARTESIAN_POINT('',(28.5,-5.40000000000002,39.85)) ;
#100132 = CARTESIAN_POINT('',(28.5,-5.25000000000002,39.85)) ;
#100133 = CARTESIAN_POINT('',(28.5,-5.40000000000002,39.4)) ;
#100134 = CARTESIAN_POINT('',(28.5,-5.40000000000002,39.25)) ;
#100135 = CARTESIAN_POINT('',(28.5,-15.1,39.4)) ;
#100136 = CARTESIAN_POINT('',(28.5,-5.25000000000002,39.4)) ;
#100137 = CARTESIAN_POINT('',(28.5,-15.1,40.)) ;
#100138 = CARTESIAN_POINT('Origin',(19.5,-15.25,-40.001)) ;
#100139 = CARTESIAN_POINT('',(19.65,-15.25,39.85)) ;
#100140 = CARTESIAN_POINT('',(22.35,-15.25,39.85)) ;
#100141 = CARTESIAN_POINT('',(22.5,-15.25,39.85)) ;
#100142 = CARTESIAN_POINT('',(22.35,-15.25,39.4)) ;
#100143 = CARTESIAN_POINT('',(22.35,-15.25,39.25)) ;
#100144 = CARTESIAN_POINT('',(19.65,-15.25,39.4)) ;
#100145 = CARTESIAN_POINT('',(19.5,-15.25,39.4)) ;
#100146 = CARTESIAN_POINT('',(19.65,-15.25,40.)) ;
#100147 = CARTESIAN_POINT('Origin',(19.5,-5.25000000000002,-40.001)) ;
#100148 = CARTESIAN_POINT('',(19.5,-5.40000000000002,39.85)) ;
#100149 = CARTESIAN_POINT('',(19.5,-15.1,39.85)) ;
#100150 = CARTESIAN_POINT('',(19.5,-15.25,39.85)) ;
#100151 = CARTESIAN_POINT('',(19.5,-15.1,39.4)) ;
#100152 = CARTESIAN_POINT('',(19.5,-15.1,39.25)) ;
#100153 = CARTESIAN_POINT('',(19.5,-5.40000000000002,39.4)) ;
#100154 = CARTESIAN_POINT('',(19.5,-5.25000000000002,39.4)) ;
#100155 = CARTESIAN_POINT('',(19.5,-5.40000000000002,40.)) ;
#100156 = CARTESIAN_POINT('Origin',(19.5,-5.25000000000002,-40.001)) ;
#100157 = CARTESIAN_POINT('',(19.65,-5.25000000000002,39.4)) ;
#100158 = CARTESIAN_POINT('',(22.35,-5.25000000000002,39.4)) ;
#100159 = CARTESIAN_POINT('',(19.5,-5.25000000000002,39.4)) ;
#100160 = CARTESIAN_POINT('',(22.35,-5.25000000000002,39.85)) ;
#100161 = CARTESIAN_POINT('',(22.35,-5.25000000000002,40.)) ;
#100162 = CARTESIAN_POINT('',(19.65,-5.25000000000002,39.85)) ;
#100163 = CARTESIAN_POINT('',(19.5,-5.25000000000002,39.85)) ;
#100164 = CARTESIAN_POINT('',(19.65,-5.25000000000002,39.25)) ;
#100165 = CARTESIAN_POINT('Origin',(22.5,-5.25000000000002,-40.001)) ;
#100166 = CARTESIAN_POINT('',(22.5,-15.1,39.85)) ;
#100167 = CARTESIAN_POINT('',(22.5,-5.40000000000002,39.85)) ;
#100168 = CARTESIAN_POINT('',(22.5,-5.25000000000002,39.85)) ;
#100169 = CARTESIAN_POINT('',(22.5,-5.40000000000002,39.4)) ;
#100170 = CARTESIAN_POINT('',(22.5,-5.40000000000002,39.25)) ;
#100171 = CARTESIAN_POINT('',(22.5,-15.1,39.4)) ;
#100172 = CARTESIAN_POINT('',(22.5,-5.25000000000002,39.4)) ;
#100173 = CARTESIAN_POINT('',(22.5,-15.1,40.)) ;
#100174 = CARTESIAN_POINT('Origin',(13.5,-15.25,-40.001)) ;
#100175 = CARTESIAN_POINT('',(16.35,-15.25,39.4)) ;
#100176 = CARTESIAN_POINT('',(13.65,-15.25,39.4)) ;
#100177 = CARTESIAN_POINT('',(13.5,-15.25,39.4)) ;
#100178 = CARTESIAN_POINT('',(13.65,-15.25,39.85)) ;
#100179 = CARTESIAN_POINT('',(13.65,-15.25,40.)) ;
#100180 = CARTESIAN_POINT('',(16.35,-15.25,39.85)) ;
#100181 = CARTESIAN_POINT('',(16.5,-15.25,39.85)) ;
#100182 = CARTESIAN_POINT('',(16.35,-15.25,39.25)) ;
#100183 = CARTESIAN_POINT('Origin',(13.5,-5.25000000000002,-40.001)) ;
#100184 = CARTESIAN_POINT('',(13.5,-5.40000000000002,39.85)) ;
#100185 = CARTESIAN_POINT('',(13.5,-15.1,39.85)) ;
#100186 = CARTESIAN_POINT('',(13.5,-15.25,39.85)) ;
#100187 = CARTESIAN_POINT('',(13.5,-15.1,39.4)) ;
#100188 = CARTESIAN_POINT('',(13.5,-15.1,39.25)) ;
#100189 = CARTESIAN_POINT('',(13.5,-5.40000000000002,39.4)) ;
#100190 = CARTESIAN_POINT('',(13.5,-5.25000000000002,39.4)) ;
#100191 = CARTESIAN_POINT('',(13.5,-5.40000000000002,40.)) ;
#100192 = CARTESIAN_POINT('Origin',(13.5,-5.25000000000002,-40.001)) ;
#100193 = CARTESIAN_POINT('',(16.35,-5.25000000000002,39.85)) ;
#100194 = CARTESIAN_POINT('',(13.65,-5.25000000000002,39.85)) ;
#100195 = CARTESIAN_POINT('',(13.5,-5.25000000000002,39.85)) ;
#100196 = CARTESIAN_POINT('',(13.65,-5.25000000000002,39.4)) ;
#100197 = CARTESIAN_POINT('',(13.65,-5.25000000000002,39.25)) ;
#100198 = CARTESIAN_POINT('',(16.35,-5.25000000000002,39.4)) ;
#100199 = CARTESIAN_POINT('',(13.5,-5.25000000000002,39.4)) ;
#100200 = CARTESIAN_POINT('',(16.35,-5.25000000000002,40.)) ;
#100201 = CARTESIAN_POINT('Origin',(16.5,-5.25000000000002,-40.001)) ;
#100202 = CARTESIAN_POINT('',(16.5,-15.1,39.85)) ;
#100203 = CARTESIAN_POINT('',(16.5,-5.40000000000002,39.85)) ;
#100204 = CARTESIAN_POINT('',(16.5,-5.25000000000002,39.85)) ;
#100205 = CARTESIAN_POINT('',(16.5,-5.40000000000002,39.4)) ;
#100206 = CARTESIAN_POINT('',(16.5,-5.40000000000002,39.25)) ;
#100207 = CARTESIAN_POINT('',(16.5,-15.1,39.4)) ;
#100208 = CARTESIAN_POINT('',(16.5,-5.25000000000002,39.4)) ;
#100209 = CARTESIAN_POINT('',(16.5,-15.1,40.)) ;
#100210 = CARTESIAN_POINT('Origin',(10.5,-5.25000000000002,-40.001)) ;
#100211 = CARTESIAN_POINT('',(10.5,-15.1,39.85)) ;
#100212 = CARTESIAN_POINT('',(10.5,-5.40000000000002,39.85)) ;
#100213 = CARTESIAN_POINT('',(10.5,-5.25000000000002,39.85)) ;
#100214 = CARTESIAN_POINT('',(10.5,-5.40000000000002,39.4)) ;
#100215 = CARTESIAN_POINT('',(10.5,-5.40000000000002,39.25)) ;
#100216 = CARTESIAN_POINT('',(10.5,-15.1,39.4)) ;
#100217 = CARTESIAN_POINT('',(10.5,-5.25000000000002,39.4)) ;
#100218 = CARTESIAN_POINT('',(10.5,-15.1,40.)) ;
#100219 = CARTESIAN_POINT('Origin',(7.49999999999997,-15.25,-40.001)) ;
#100220 = CARTESIAN_POINT('',(7.64999999999997,-15.25,39.85)) ;
#100221 = CARTESIAN_POINT('',(10.35,-15.25,39.85)) ;
#100222 = CARTESIAN_POINT('',(10.5,-15.25,39.85)) ;
#100223 = CARTESIAN_POINT('',(10.35,-15.25,39.4)) ;
#100224 = CARTESIAN_POINT('',(10.35,-15.25,39.25)) ;
#100225 = CARTESIAN_POINT('',(7.64999999999997,-15.25,39.4)) ;
#100226 = CARTESIAN_POINT('',(7.49999999999997,-15.25,39.4)) ;
#100227 = CARTESIAN_POINT('',(7.64999999999997,-15.25,40.)) ;
#100228 = CARTESIAN_POINT('Origin',(7.49999999999996,-5.25000000000002,-40.001)) ;
#100229 = CARTESIAN_POINT('',(7.49999999999996,-5.40000000000002,39.85)) ;
#100230 = CARTESIAN_POINT('',(7.49999999999997,-15.1,39.85)) ;
#100231 = CARTESIAN_POINT('',(7.49999999999997,-15.25,39.85)) ;
#100232 = CARTESIAN_POINT('',(7.49999999999997,-15.1,39.4)) ;
#100233 = CARTESIAN_POINT('',(7.49999999999997,-15.1,39.25)) ;
#100234 = CARTESIAN_POINT('',(7.49999999999996,-5.40000000000002,39.4)) ;
#100235 = CARTESIAN_POINT('',(7.49999999999996,-5.25000000000002,39.4)) ;
#100236 = CARTESIAN_POINT('',(7.49999999999996,-5.40000000000002,40.)) ;
#100237 = CARTESIAN_POINT('Origin',(7.49999999999996,-5.25000000000002,-40.001)) ;
#100238 = CARTESIAN_POINT('',(7.64999999999996,-5.25000000000002,39.4)) ;
#100239 = CARTESIAN_POINT('',(10.35,-5.25000000000002,39.4)) ;
#100240 = CARTESIAN_POINT('',(7.49999999999996,-5.25000000000002,39.4)) ;
#100241 = CARTESIAN_POINT('',(10.35,-5.25000000000002,39.85)) ;
#100242 = CARTESIAN_POINT('',(10.35,-5.25000000000002,40.)) ;
#100243 = CARTESIAN_POINT('',(7.64999999999996,-5.25000000000002,39.85)) ;
#100244 = CARTESIAN_POINT('',(7.49999999999996,-5.25000000000002,39.85)) ;
#100245 = CARTESIAN_POINT('',(7.64999999999996,-5.25000000000002,39.25)) ;
#100246 = CARTESIAN_POINT('Origin',(46.5,-15.2500000000003,40.001)) ;
#100247 = CARTESIAN_POINT('',(43.65,-15.2500000000003,-39.4)) ;
#100248 = CARTESIAN_POINT('',(46.35,-15.2500000000003,-39.4)) ;
#100249 = CARTESIAN_POINT('',(46.5,-15.2500000000003,-39.4)) ;
#100250 = CARTESIAN_POINT('',(46.35,-15.2500000000003,-39.85)) ;
#100251 = CARTESIAN_POINT('',(46.35,-15.2500000000003,-40.)) ;
#100252 = CARTESIAN_POINT('',(43.65,-15.2500000000003,-39.85)) ;
#100253 = CARTESIAN_POINT('',(43.5,-15.2500000000003,-39.85)) ;
#100254 = CARTESIAN_POINT('',(43.65,-15.2500000000003,-39.25)) ;
#100255 = CARTESIAN_POINT('Origin',(46.5,-5.25000000000033,40.001)) ;
#100256 = CARTESIAN_POINT('',(46.5,-5.40000000000027,-39.85)) ;
#100257 = CARTESIAN_POINT('',(46.5,-15.1000000000003,-39.85)) ;
#100258 = CARTESIAN_POINT('',(46.5,-15.2500000000003,-39.85)) ;
#100259 = CARTESIAN_POINT('',(46.5,-15.1000000000003,-39.4)) ;
#100260 = CARTESIAN_POINT('',(46.5,-15.1000000000003,-39.25)) ;
#100261 = CARTESIAN_POINT('',(46.5,-5.40000000000027,-39.4)) ;
#100262 = CARTESIAN_POINT('',(46.5,-5.25000000000027,-39.4)) ;
#100263 = CARTESIAN_POINT('',(46.5,-5.40000000000027,-40.)) ;
#100264 = CARTESIAN_POINT('Origin',(46.5,-5.25000000000033,40.001)) ;
#100265 = CARTESIAN_POINT('',(43.65,-5.25000000000027,-39.85)) ;
#100266 = CARTESIAN_POINT('',(46.35,-5.25000000000027,-39.85)) ;
#100267 = CARTESIAN_POINT('',(46.5,-5.25000000000027,-39.85)) ;
#100268 = CARTESIAN_POINT('',(46.35,-5.25000000000027,-39.4)) ;
#100269 = CARTESIAN_POINT('',(46.35,-5.25000000000027,-39.25)) ;
#100270 = CARTESIAN_POINT('',(43.65,-5.25000000000027,-39.4)) ;
#100271 = CARTESIAN_POINT('',(46.5,-5.25000000000027,-39.4)) ;
#100272 = CARTESIAN_POINT('',(43.65,-5.25000000000027,-40.)) ;
#100273 = CARTESIAN_POINT('Origin',(43.5,-5.25000000000033,40.001)) ;
#100274 = CARTESIAN_POINT('',(43.5,-15.1000000000003,-39.85)) ;
#100275 = CARTESIAN_POINT('',(43.5,-5.40000000000027,-39.85)) ;
#100276 = CARTESIAN_POINT('',(43.5,-5.25000000000027,-39.85)) ;
#100277 = CARTESIAN_POINT('',(43.5,-5.40000000000027,-39.4)) ;
#100278 = CARTESIAN_POINT('',(43.5,-5.40000000000027,-39.25)) ;
#100279 = CARTESIAN_POINT('',(43.5,-15.1000000000003,-39.4)) ;
#100280 = CARTESIAN_POINT('',(43.5,-5.25000000000027,-39.4)) ;
#100281 = CARTESIAN_POINT('',(43.5,-15.1000000000003,-40.)) ;
#100282 = CARTESIAN_POINT('Origin',(38.25,-2.75000000000007,40.001)) ;
#100283 = CARTESIAN_POINT('',(38.1,-2.75000000000002,-39.4)) ;
#100284 = CARTESIAN_POINT('',(19.4,-2.75000000000002,-39.4)) ;
#100285 = CARTESIAN_POINT('',(38.25,-2.75000000000002,-39.4)) ;
#100286 = CARTESIAN_POINT('',(19.4,-2.75000000000002,-39.85)) ;
#100287 = CARTESIAN_POINT('',(19.4,-2.75000000000002,-40.)) ;
#100288 = CARTESIAN_POINT('',(38.1,-2.75000000000002,-39.85)) ;
#100289 = CARTESIAN_POINT('',(38.25,-2.75000000000002,-39.85)) ;
#100290 = CARTESIAN_POINT('',(38.1,-2.75000000000002,-39.25)) ;
#100291 = CARTESIAN_POINT('Origin',(38.25,-2.75000000000007,40.001)) ;
#100292 = CARTESIAN_POINT('',(38.25,-2.90000000000002,-39.85)) ;
#100293 = CARTESIAN_POINT('',(38.25,-13.1,-39.85)) ;
#100294 = CARTESIAN_POINT('',(38.25,-13.25,-39.85)) ;
#100295 = CARTESIAN_POINT('',(38.25,-13.1,-39.4)) ;
#100296 = CARTESIAN_POINT('',(38.25,-13.1,-39.25)) ;
#100297 = CARTESIAN_POINT('',(38.25,-2.90000000000002,-39.4)) ;
#100298 = CARTESIAN_POINT('',(38.25,-2.75000000000002,-39.4)) ;
#100299 = CARTESIAN_POINT('',(38.25,-2.90000000000002,-40.)) ;
#100300 = CARTESIAN_POINT('Origin',(38.25,-13.2500000000001,40.001)) ;
#100301 = CARTESIAN_POINT('',(38.1,-13.25,-39.85)) ;
#100302 = CARTESIAN_POINT('',(19.4,-13.25,-39.85)) ;
#100303 = CARTESIAN_POINT('',(19.25,-13.25,-39.85)) ;
#100304 = CARTESIAN_POINT('',(19.4,-13.25,-39.4)) ;
#100305 = CARTESIAN_POINT('',(19.4,-13.25,-39.25)) ;
#100306 = CARTESIAN_POINT('',(38.1,-13.25,-39.4)) ;
#100307 = CARTESIAN_POINT('',(38.25,-13.25,-39.4)) ;
#100308 = CARTESIAN_POINT('',(38.1,-13.25,-40.)) ;
#100309 = CARTESIAN_POINT('Origin',(19.25,-2.75000000000007,40.001)) ;
#100310 = CARTESIAN_POINT('',(19.25,-13.1,-39.85)) ;
#100311 = CARTESIAN_POINT('',(19.25,-2.90000000000002,-39.85)) ;
#100312 = CARTESIAN_POINT('',(19.25,-2.75000000000002,-39.85)) ;
#100313 = CARTESIAN_POINT('',(19.25,-2.90000000000002,-39.4)) ;
#100314 = CARTESIAN_POINT('',(19.25,-2.90000000000002,-39.25)) ;
#100315 = CARTESIAN_POINT('',(19.25,-13.1,-39.4)) ;
#100316 = CARTESIAN_POINT('',(19.25,-2.75000000000002,-39.4)) ;
#100317 = CARTESIAN_POINT('',(19.25,-13.1,-40.)) ;
#100318 = CARTESIAN_POINT('Origin',(16.5,-15.2500000000001,40.001)) ;
#100319 = CARTESIAN_POINT('',(13.65,-15.2500000000001,-39.4)) ;
#100320 = CARTESIAN_POINT('',(16.35,-15.2500000000001,-39.4)) ;
#100321 = CARTESIAN_POINT('',(16.5,-15.2500000000001,-39.4)) ;
#100322 = CARTESIAN_POINT('',(16.35,-15.2500000000001,-39.85)) ;
#100323 = CARTESIAN_POINT('',(16.35,-15.2500000000001,-40.)) ;
#100324 = CARTESIAN_POINT('',(13.65,-15.2500000000001,-39.85)) ;
#100325 = CARTESIAN_POINT('',(13.5,-15.2500000000001,-39.85)) ;
#100326 = CARTESIAN_POINT('',(13.65,-15.2500000000001,-39.25)) ;
#100327 = CARTESIAN_POINT('Origin',(16.5,-5.25000000000011,40.001)) ;
#100328 = CARTESIAN_POINT('',(16.5,-5.40000000000006,-39.85)) ;
#100329 = CARTESIAN_POINT('',(16.5,-15.1000000000001,-39.85)) ;
#100330 = CARTESIAN_POINT('',(16.5,-15.2500000000001,-39.85)) ;
#100331 = CARTESIAN_POINT('',(16.5,-15.1000000000001,-39.4)) ;
#100332 = CARTESIAN_POINT('',(16.5,-15.1000000000001,-39.25)) ;
#100333 = CARTESIAN_POINT('',(16.5,-5.40000000000006,-39.4)) ;
#100334 = CARTESIAN_POINT('',(16.5,-5.25000000000006,-39.4)) ;
#100335 = CARTESIAN_POINT('',(16.5,-5.40000000000006,-40.)) ;
#100336 = CARTESIAN_POINT('Origin',(16.5,-5.25000000000011,40.001)) ;
#100337 = CARTESIAN_POINT('',(13.65,-5.25000000000006,-39.85)) ;
#100338 = CARTESIAN_POINT('',(16.35,-5.25000000000006,-39.85)) ;
#100339 = CARTESIAN_POINT('',(16.5,-5.25000000000006,-39.85)) ;
#100340 = CARTESIAN_POINT('',(16.35,-5.25000000000006,-39.4)) ;
#100341 = CARTESIAN_POINT('',(16.35,-5.25000000000006,-39.25)) ;
#100342 = CARTESIAN_POINT('',(13.65,-5.25000000000006,-39.4)) ;
#100343 = CARTESIAN_POINT('',(16.5,-5.25000000000006,-39.4)) ;
#100344 = CARTESIAN_POINT('',(13.65,-5.25000000000006,-40.)) ;
#100345 = CARTESIAN_POINT('Origin',(13.5,-5.25000000000011,40.001)) ;
#100346 = CARTESIAN_POINT('',(13.5,-15.1000000000001,-39.85)) ;
#100347 = CARTESIAN_POINT('',(13.5,-5.40000000000006,-39.85)) ;
#100348 = CARTESIAN_POINT('',(13.5,-5.25000000000006,-39.85)) ;
#100349 = CARTESIAN_POINT('',(13.5,-5.40000000000006,-39.4)) ;
#100350 = CARTESIAN_POINT('',(13.5,-5.40000000000006,-39.25)) ;
#100351 = CARTESIAN_POINT('',(13.5,-15.1000000000001,-39.4)) ;
#100352 = CARTESIAN_POINT('',(13.5,-5.25000000000006,-39.4)) ;
#100353 = CARTESIAN_POINT('',(13.5,-15.1000000000001,-40.)) ;
#100354 = CARTESIAN_POINT('Origin',(7.49999999999997,-5.25000000000007,40.001)) ;
#100355 = CARTESIAN_POINT('',(7.49999999999996,-15.1,-39.85)) ;
#100356 = CARTESIAN_POINT('',(7.49999999999997,-5.40000000000002,-39.85)) ;
#100357 = CARTESIAN_POINT('',(7.49999999999997,-5.25000000000002,-39.85)) ;
#100358 = CARTESIAN_POINT('',(7.49999999999997,-5.40000000000002,-39.4)) ;
#100359 = CARTESIAN_POINT('',(7.49999999999997,-5.40000000000002,-39.25)) ;
#100360 = CARTESIAN_POINT('',(7.49999999999996,-15.1,-39.4)) ;
#100361 = CARTESIAN_POINT('',(7.49999999999997,-5.25000000000002,-39.4)) ;
#100362 = CARTESIAN_POINT('',(7.49999999999996,-15.1,-40.)) ;
#100363 = CARTESIAN_POINT('Origin',(10.5,-15.2500000000001,40.001)) ;
#100364 = CARTESIAN_POINT('',(10.35,-15.25,-39.85)) ;
#100365 = CARTESIAN_POINT('',(7.64999999999996,-15.25,-39.85)) ;
#100366 = CARTESIAN_POINT('',(7.49999999999996,-15.25,-39.85)) ;
#100367 = CARTESIAN_POINT('',(7.64999999999996,-15.25,-39.4)) ;
#100368 = CARTESIAN_POINT('',(7.64999999999996,-15.25,-39.25)) ;
#100369 = CARTESIAN_POINT('',(10.35,-15.25,-39.4)) ;
#100370 = CARTESIAN_POINT('',(10.5,-15.25,-39.4)) ;
#100371 = CARTESIAN_POINT('',(10.35,-15.25,-40.)) ;
#100372 = CARTESIAN_POINT('Origin',(10.5,-5.25000000000007,40.001)) ;
#100373 = CARTESIAN_POINT('',(10.5,-5.40000000000002,-39.85)) ;
#100374 = CARTESIAN_POINT('',(10.5,-15.1,-39.85)) ;
#100375 = CARTESIAN_POINT('',(10.5,-15.25,-39.85)) ;
#100376 = CARTESIAN_POINT('',(10.5,-15.1,-39.4)) ;
#100377 = CARTESIAN_POINT('',(10.5,-15.1,-39.25)) ;
#100378 = CARTESIAN_POINT('',(10.5,-5.40000000000002,-39.4)) ;
#100379 = CARTESIAN_POINT('',(10.5,-5.25000000000002,-39.4)) ;
#100380 = CARTESIAN_POINT('',(10.5,-5.40000000000002,-40.)) ;
#100381 = CARTESIAN_POINT('Origin',(10.5,-5.25000000000007,40.001)) ;
#100382 = CARTESIAN_POINT('',(10.35,-5.25000000000002,-39.4)) ;
#100383 = CARTESIAN_POINT('',(7.64999999999997,-5.25000000000002,-39.4)) ;
#100384 = CARTESIAN_POINT('',(10.5,-5.25000000000002,-39.4)) ;
#100385 = CARTESIAN_POINT('',(7.64999999999997,-5.25000000000002,-39.85)) ;
#100386 = CARTESIAN_POINT('',(7.64999999999997,-5.25000000000002,-40.)) ;
#100387 = CARTESIAN_POINT('',(10.35,-5.25000000000002,-39.85)) ;
#100388 = CARTESIAN_POINT('',(10.5,-5.25000000000002,-39.85)) ;
#100389 = CARTESIAN_POINT('',(10.35,-5.25000000000002,-39.25)) ;
#100390 = CARTESIAN_POINT('Origin',(-2.00100000000011,-4.2500000000002,-32.5)) ;
#100391 = CARTESIAN_POINT('',(53.85,-4.39999999999999,-32.5)) ;
#100392 = CARTESIAN_POINT('',(53.4,-4.4,-32.5)) ;
#100393 = CARTESIAN_POINT('',(53.25,-4.4,-32.5)) ;
#100394 = CARTESIAN_POINT('',(53.4,-14.1,-32.5)) ;
#100395 = CARTESIAN_POINT('',(53.4,-14.25,-32.5)) ;
#100396 = CARTESIAN_POINT('',(53.8500000000001,-14.1,-32.5)) ;
#100397 = CARTESIAN_POINT('',(54.0000000000001,-14.1,-32.5)) ;
#100398 = CARTESIAN_POINT('',(53.85,-4.24999999999999,-32.5)) ;
#100399 = CARTESIAN_POINT('Origin',(-2.00100000000007,-14.2500000000002,34.)) ;
#100400 = CARTESIAN_POINT('',(53.8500000000001,-14.25,33.85)) ;
#100401 = CARTESIAN_POINT('',(53.8500000000001,-14.25,-32.35)) ;
#100402 = CARTESIAN_POINT('',(53.8500000000001,-14.25,34.)) ;
#100403 = CARTESIAN_POINT('',(53.4,-14.25,-32.35)) ;
#100404 = CARTESIAN_POINT('',(53.2500000000001,-14.25,-32.35)) ;
#100405 = CARTESIAN_POINT('',(53.4,-14.25,33.85)) ;
#100406 = CARTESIAN_POINT('',(53.4,-14.25,34.)) ;
#100407 = CARTESIAN_POINT('',(54.0000000000001,-14.25,33.85)) ;
#100408 = CARTESIAN_POINT('Origin',(-2.00100000000011,-4.2500000000002,34.)) ;
#100409 = CARTESIAN_POINT('',(53.8500000000001,-14.1,34.)) ;
#100410 = CARTESIAN_POINT('',(53.4,-14.1,34.)) ;
#100411 = CARTESIAN_POINT('',(53.2500000000001,-14.1,34.)) ;
#100412 = CARTESIAN_POINT('',(53.4,-4.4,34.)) ;
#100413 = CARTESIAN_POINT('',(53.4,-4.25,34.)) ;
#100414 = CARTESIAN_POINT('',(53.85,-4.4,34.)) ;
#100415 = CARTESIAN_POINT('',(54.,-4.39999999999999,34.)) ;
#100416 = CARTESIAN_POINT('',(53.85,-4.24999999999999,34.)) ;
#100417 = CARTESIAN_POINT('Origin',(-2.00100000000011,-4.2500000000002,34.)) ;
#100418 = CARTESIAN_POINT('',(53.4,-4.25,33.85)) ;
#100419 = CARTESIAN_POINT('',(53.4,-4.25,-32.35)) ;
#100420 = CARTESIAN_POINT('',(53.4,-4.25,-32.5)) ;
#100421 = CARTESIAN_POINT('',(53.85,-4.24999999999999,-32.35)) ;
#100422 = CARTESIAN_POINT('',(54.,-4.24999999999999,-32.35)) ;
#100423 = CARTESIAN_POINT('',(53.85,-4.24999999999999,33.85)) ;
#100424 = CARTESIAN_POINT('',(53.85,-4.24999999999999,34.)) ;
#100425 = CARTESIAN_POINT('',(53.25,-4.25,33.85)) ;
#100426 = CARTESIAN_POINT('Origin',(53.,-7.91804761436593E-15,-39.85)) ;
#100427 = CARTESIAN_POINT('Origin',(53.0000000000001,-19.6,-39.85)) ;
#100428 = CARTESIAN_POINT('Origin',(53.0000000000001,-1.89999999999994,-39.8500000000001)) ;
#100429 = CARTESIAN_POINT('Origin',(53.,-1.89999999999999,-39.25)) ;
#100430 = CARTESIAN_POINT('Origin',(52.9999999999994,-1.90000000000071,-39.4000000000007)) ;
#100431 = CARTESIAN_POINT('Origin',(53.0000000000001,-19.6,-39.85)) ;
#100432 = CARTESIAN_POINT('Origin',(53.0000000000001,-19.6,-39.85)) ;
#100433 = CARTESIAN_POINT('Origin',(53.0000000000001,-19.6,-39.85)) ;
#100434 = CARTESIAN_POINT('Origin',(52.9999999999998,56.3581964958473,-39.4)) ;
#100435 = CARTESIAN_POINT('Origin',(53.0000000000001,-19.6,-39.4)) ;
#100436 = CARTESIAN_POINT('Origin',(53.0000000000001,-19.6,-40.)) ;
#100437 = CARTESIAN_POINT('Origin',(53.0000000000001,-19.6,-39.4)) ;
#100438 = CARTESIAN_POINT('Origin',(53.25,-19.6,-39.85)) ;
#100439 = CARTESIAN_POINT('Origin',(0.149999999999965,-19.6,-39.85)) ;
#100440 = CARTESIAN_POINT('Origin',(53.0000000000001,-19.6,-39.4)) ;
#100441 = CARTESIAN_POINT('Origin',(53.0000000000001,-19.6,-39.4)) ;
#100442 = CARTESIAN_POINT('Origin',(0.149999999999965,-19.6,-39.85)) ;
#100443 = CARTESIAN_POINT('Origin',(0.149999999999965,-19.6,-39.85)) ;
#100444 = CARTESIAN_POINT('Origin',(0.149999999999965,-19.6,-39.85)) ;
#100445 = CARTESIAN_POINT('Origin',(53.25,-19.6,-39.4)) ;
#100446 = CARTESIAN_POINT('Origin',(0.149999999999965,-19.6,-39.4)) ;
#100447 = CARTESIAN_POINT('Origin',(0.149999999999965,-19.6,-38.25)) ;
#100448 = CARTESIAN_POINT('Origin',(0.149999999999965,-19.6,-39.4)) ;
#100449 = CARTESIAN_POINT('Origin',(0.149999999999965,-1.74999999999999,-39.85)) ;
#100450 = CARTESIAN_POINT('Origin',(0.149999999999965,-6.90000000000001,-39.85)) ;
#100451 = CARTESIAN_POINT('Origin',(0.149999999999965,-19.6,-39.4)) ;
#100452 = CARTESIAN_POINT('Origin',(0.149999999999963,-19.6,-39.4)) ;
#100453 = CARTESIAN_POINT('Origin',(-0.150000000000035,-6.90000000000001,
-39.85)) ;
#100454 = CARTESIAN_POINT('Origin',(-0.150000000000035,-6.90000000000001,
-39.85)) ;
#100455 = CARTESIAN_POINT('Origin',(-0.150000000000035,-6.60000000000001,
-39.85)) ;
#100456 = CARTESIAN_POINT('Origin',(0.149999999999963,-6.83349298384788E-15,
-39.4)) ;
#100457 = CARTESIAN_POINT('Origin',(0.149999999999965,-6.90000000000001,-39.4)) ;
#100458 = CARTESIAN_POINT('Origin',(-0.150000000000035,-6.90000000000001,
-38.25)) ;
#100459 = CARTESIAN_POINT('Origin',(-0.150000000000035,-6.90000000000001,
-39.4)) ;
#100460 = CARTESIAN_POINT('Origin',(-3.46944695195361E-14,-6.60000000000001,
-39.85)) ;
#100461 = CARTESIAN_POINT('Origin',(-1.85000000000003,-6.60000000000001,-39.85)) ;
#100462 = CARTESIAN_POINT('Origin',(-0.150000000000035,-6.90000000000001,
-39.4)) ;
#100463 = CARTESIAN_POINT('Origin',(-0.150000000000035,-6.60000000000001,
-39.4)) ;
#100464 = CARTESIAN_POINT('Origin',(-1.85000000000003,-6.60000000000001,-39.85)) ;
#100465 = CARTESIAN_POINT('Origin',(-1.85000000000003,-6.60000000000001,-39.85)) ;
#100466 = CARTESIAN_POINT('Origin',(-1.85000000000003,-6.60000000000001,-39.85)) ;
#100467 = CARTESIAN_POINT('Origin',(53.25,-6.60000000000001,-39.4)) ;
#100468 = CARTESIAN_POINT('Origin',(-1.85000000000003,-6.60000000000001,-39.4)) ;
#100469 = CARTESIAN_POINT('Origin',(-1.85000000000003,-6.60000000000001,-39.25)) ;
#100470 = CARTESIAN_POINT('Origin',(-1.85000000000003,-6.60000000000001,-39.4)) ;
#100471 = CARTESIAN_POINT('Origin',(-1.85000000000003,-4.75000000000001,-39.85)) ;
#100472 = CARTESIAN_POINT('Origin',(-1.85000000000003,-4.9,-39.85)) ;
#100473 = CARTESIAN_POINT('Origin',(-1.85000000000003,-6.60000000000001,-39.4)) ;
#100474 = CARTESIAN_POINT('Origin',(-1.85000000000003,-6.60000000000001,-39.4)) ;
#100475 = CARTESIAN_POINT('Origin',(-1.85000000000003,-4.9,-39.85)) ;
#100476 = CARTESIAN_POINT('Origin',(-1.85000000000003,-4.9,-39.85)) ;
#100477 = CARTESIAN_POINT('Origin',(-1.85000000000003,-4.9,-39.85)) ;
#100478 = CARTESIAN_POINT('Origin',(-1.85000000000003,-1.87814009246381E-14,
-39.4)) ;
#100479 = CARTESIAN_POINT('Origin',(-1.85000000000003,-4.9,-39.4)) ;
#100480 = CARTESIAN_POINT('Origin',(-1.85000000000003,-4.9,-39.25)) ;
#100481 = CARTESIAN_POINT('Origin',(-1.85000000000003,-4.9,-39.4)) ;
#100482 = CARTESIAN_POINT('Origin',(-2.77555756156289E-14,-4.9,-39.85)) ;
#100483 = CARTESIAN_POINT('Origin',(-0.150000000000035,-4.9,-39.85)) ;
#100484 = CARTESIAN_POINT('Origin',(52.9999999999998,56.3581964958473,39.85)) ;
#100485 = CARTESIAN_POINT('Origin',(52.9999999999998,-1.90000000000013,39.8499999999999)) ;
#100486 = CARTESIAN_POINT('Origin',(53.,-19.6,39.85)) ;
#100487 = CARTESIAN_POINT('Origin',(-1.85000000000003,-4.9,-39.4)) ;
#100488 = CARTESIAN_POINT('Origin',(-1.85000000000003,-4.9,-39.4)) ;
#100489 = CARTESIAN_POINT('Origin',(-0.150000000000035,-4.6,-39.85)) ;
#100490 = CARTESIAN_POINT('Origin',(-0.150000000000035,-4.6,-39.85)) ;
#100491 = CARTESIAN_POINT('Origin',(0.149999999999965,-4.6,-39.85)) ;
#100492 = CARTESIAN_POINT('Origin',(53.,-19.6,39.85)) ;
#100493 = CARTESIAN_POINT('Origin',(53.,-19.6,39.85)) ;
#100494 = CARTESIAN_POINT('Origin',(53.,-19.6,39.85)) ;
#100495 = CARTESIAN_POINT('Origin',(53.,-1.90000000000001,39.25)) ;
#100496 = CARTESIAN_POINT('Origin',(52.9999999999997,-1.90000000000036,39.4000000000004)) ;
#100497 = CARTESIAN_POINT('Origin',(53.25,-4.9,-39.4)) ;
#100498 = CARTESIAN_POINT('Origin',(-0.150000000000035,-4.9,-39.4)) ;
#100499 = CARTESIAN_POINT('Origin',(-0.150000000000035,-4.6,-39.25)) ;
#100500 = CARTESIAN_POINT('Origin',(-0.150000000000035,-4.6,-39.4)) ;
#100501 = CARTESIAN_POINT('Origin',(0.149999999999965,-1.74999999999999,-39.85)) ;
#100502 = CARTESIAN_POINT('Origin',(0.149999999999965,-1.75,-39.85)) ;
#100503 = CARTESIAN_POINT('Origin',(53.25,-19.6,39.85)) ;
#100504 = CARTESIAN_POINT('Origin',(0.149999999999972,-19.6,39.85)) ;
#100505 = CARTESIAN_POINT('Origin',(53.,-19.6,39.25)) ;
#100506 = CARTESIAN_POINT('Origin',(53.,-19.6,39.4)) ;
#100507 = CARTESIAN_POINT('Origin',(53.,-19.75,39.4)) ;
#100508 = CARTESIAN_POINT('Origin',(53.,-19.6,39.4)) ;
#100509 = CARTESIAN_POINT('Origin',(-0.150000000000035,-4.6,-39.4)) ;
#100510 = CARTESIAN_POINT('Origin',(0.149999999999963,-4.6,-39.4)) ;
#100511 = CARTESIAN_POINT('Origin',(0.14999999999997,-1.75000000000001,-38.25)) ;
#100512 = CARTESIAN_POINT('Origin',(0.15000000000005,-0.150000000000014,-38.25)) ;
#100513 = CARTESIAN_POINT('Origin',(0.149999999999972,-19.6,39.85)) ;
#100514 = CARTESIAN_POINT('Origin',(0.149999999999972,-19.6,39.85)) ;
#100515 = CARTESIAN_POINT('Origin',(0.149999999999972,-19.6,39.85)) ;
#100516 = CARTESIAN_POINT('Origin',(53.,-19.6,39.4)) ;
#100517 = CARTESIAN_POINT('Origin',(53.,-19.6,39.4)) ;
#100518 = CARTESIAN_POINT('Origin',(0.149999999999963,-6.83349298384788E-15,
-39.4)) ;
#100519 = CARTESIAN_POINT('Origin',(0.149999999999965,-1.74999999999999,-39.4)) ;
#100520 = CARTESIAN_POINT('Origin',(0.149999999999965,-0.150000000000013,
-39.25)) ;
#100521 = CARTESIAN_POINT('Origin',(0.149999999999965,-0.150000000000018,
-14.15)) ;
#100522 = CARTESIAN_POINT('Origin',(0.149999999999972,-0.750000000000015,
39.85)) ;
#100523 = CARTESIAN_POINT('Origin',(0.149999999999972,-6.90000000000001,39.85)) ;
#100524 = CARTESIAN_POINT('Origin',(0.149999999999972,-19.6,38.25)) ;
#100525 = CARTESIAN_POINT('Origin',(0.149999999999972,-19.6,39.4)) ;
#100526 = CARTESIAN_POINT('Origin',(53.25,-19.6,39.4)) ;
#100527 = CARTESIAN_POINT('Origin',(0.14999999999997,-19.6,39.4)) ;
#100528 = CARTESIAN_POINT('Origin',(0.14999999999997,-1.75000000000001,-38.25)) ;
#100529 = CARTESIAN_POINT('Origin',(0.150000000000031,-0.600000000000014,
-38.25)) ;
#100530 = CARTESIAN_POINT('Origin',(-0.150000000000035,-0.150000000000018,
-14.15)) ;
#100531 = CARTESIAN_POINT('Origin',(-0.150000000000035,-0.150000000000018,
-14.15)) ;
#100532 = CARTESIAN_POINT('Origin',(-0.150000000000035,-0.150000000000018,
-13.85)) ;
#100533 = CARTESIAN_POINT('Origin',(-0.150000000000028,-6.90000000000001,
39.85)) ;
#100534 = CARTESIAN_POINT('Origin',(-0.150000000000028,-6.60000000000001,
39.85)) ;
#100535 = CARTESIAN_POINT('Origin',(-0.150000000000028,-6.90000000000001,
39.85)) ;
#100536 = CARTESIAN_POINT('Origin',(0.149999999999972,-19.6,39.4)) ;
#100537 = CARTESIAN_POINT('Origin',(0.149999999999972,-19.6,39.4)) ;
#100538 = CARTESIAN_POINT('Origin',(0.149999999999963,-0.600000000000029,
40.)) ;
#100539 = CARTESIAN_POINT('Origin',(0.149999999999965,-0.600000000000019,
-14.15)) ;
#100540 = CARTESIAN_POINT('Origin',(-0.150000000000035,-1.75000000000001,
-14.15)) ;
#100541 = CARTESIAN_POINT('Origin',(-0.150000000000035,-0.600000000000019,
-14.15)) ;
#100542 = CARTESIAN_POINT('Origin',(53.25,-0.150000000000018,-13.85)) ;
#100543 = CARTESIAN_POINT('Origin',(-1.85000000000004,-0.150000000000018,
-13.85)) ;
#100544 = CARTESIAN_POINT('Origin',(53.25,-6.60000000000001,39.85)) ;
#100545 = CARTESIAN_POINT('Origin',(-1.85000000000003,-6.60000000000001,39.85)) ;
#100546 = CARTESIAN_POINT('Origin',(-0.150000000000028,-6.90000000000001,
39.25)) ;
#100547 = CARTESIAN_POINT('Origin',(-0.150000000000028,-6.90000000000001,
39.4)) ;
#100548 = CARTESIAN_POINT('Origin',(0.14999999999997,-19.75,39.4)) ;
#100549 = CARTESIAN_POINT('Origin',(0.14999999999997,-6.90000000000001,39.4)) ;
#100550 = CARTESIAN_POINT('Origin',(-0.150000000000035,-0.600000000000019,
-14.15)) ;
#100551 = CARTESIAN_POINT('Origin',(-0.150000000000035,-0.600000000000019,
-13.85)) ;
#100552 = CARTESIAN_POINT('Origin',(-1.85000000000004,-0.150000000000018,
-13.85)) ;
#100553 = CARTESIAN_POINT('Origin',(-1.85000000000004,-0.150000000000018,
-13.85)) ;
#100554 = CARTESIAN_POINT('Origin',(-1.85000000000004,-0.150000000000018,
-13.85)) ;
#100555 = CARTESIAN_POINT('Origin',(-1.85000000000003,-6.60000000000001,39.85)) ;
#100556 = CARTESIAN_POINT('Origin',(-1.85000000000003,-6.60000000000001,39.85)) ;
#100557 = CARTESIAN_POINT('Origin',(-1.85000000000003,-6.60000000000001,39.85)) ;
#100558 = CARTESIAN_POINT('Origin',(-0.150000000000028,-6.90000000000001,
39.4)) ;
#100559 = CARTESIAN_POINT('Origin',(-0.150000000000028,-6.60000000000001,
39.4)) ;
#100560 = CARTESIAN_POINT('Origin',(-4.85722573273506E-14,-0.600000000000019,
-13.85)) ;
#100561 = CARTESIAN_POINT('Origin',(-1.85000000000004,-0.600000000000019,
-13.85)) ;
#100562 = CARTESIAN_POINT('Origin',(-1.85000000000004,-0.750000000000015,
-13.85)) ;
#100563 = CARTESIAN_POINT('Origin',(-1.85000000000004,-0.600000000000019,
-13.85)) ;
#100564 = CARTESIAN_POINT('Origin',(-1.85000000000004,-0.150000000000028,
40.)) ;
#100565 = CARTESIAN_POINT('Origin',(-1.85000000000004,-0.150000000000023,
13.85)) ;
#100566 = CARTESIAN_POINT('Origin',(-1.85000000000003,-19.75,39.85)) ;
#100567 = CARTESIAN_POINT('Origin',(-1.85000000000003,-4.90000000000001,39.85)) ;
#100568 = CARTESIAN_POINT('Origin',(-1.85000000000003,-6.60000000000001,39.25)) ;
#100569 = CARTESIAN_POINT('Origin',(-1.85000000000003,-6.60000000000001,39.4)) ;
#100570 = CARTESIAN_POINT('Origin',(-2.77555756156289E-14,-6.60000000000001,
39.4)) ;
#100571 = CARTESIAN_POINT('Origin',(-1.85000000000003,-6.60000000000001,39.4)) ;
#100572 = CARTESIAN_POINT('Origin',(-1.85000000000004,-0.600000000000019,
-13.85)) ;
#100573 = CARTESIAN_POINT('Origin',(-1.85000000000004,-0.600000000000019,
-13.85)) ;
#100574 = CARTESIAN_POINT('Origin',(-1.85000000000004,-0.150000000000023,
13.85)) ;
#100575 = CARTESIAN_POINT('Origin',(-1.85000000000004,-0.150000000000023,
13.85)) ;
#100576 = CARTESIAN_POINT('Origin',(-1.85000000000004,-0.150000000000023,
13.85)) ;
#100577 = CARTESIAN_POINT('Origin',(0.149999999999966,-1.75000000000003,38.25)) ;
#100578 = CARTESIAN_POINT('Origin',(0.149999999999966,-1.75000000000002,39.85)) ;
#100579 = CARTESIAN_POINT('Origin',(0.149999999999965,-0.150000000000029,
38.25)) ;
#100580 = CARTESIAN_POINT('Origin',(-1.85000000000003,-4.90000000000001,39.85)) ;
#100581 = CARTESIAN_POINT('Origin',(-1.85000000000003,-4.90000000000001,39.85)) ;
#100582 = CARTESIAN_POINT('Origin',(-1.85000000000004,-4.90000000000001,39.85)) ;
#100583 = CARTESIAN_POINT('Origin',(-1.85000000000003,-6.60000000000001,39.4)) ;
#100584 = CARTESIAN_POINT('Origin',(-1.85000000000003,-6.60000000000001,39.4)) ;
#100585 = CARTESIAN_POINT('Origin',(-1.85000000000004,-0.600000000000024,
14.)) ;
#100586 = CARTESIAN_POINT('Origin',(-1.85000000000004,-0.600000000000024,
13.85)) ;
#100587 = CARTESIAN_POINT('Origin',(-1.85000000000004,-0.750000000000028,
13.85)) ;
#100588 = CARTESIAN_POINT('Origin',(-1.85000000000004,-0.600000000000024,
13.85)) ;
#100589 = CARTESIAN_POINT('Origin',(53.25,-0.150000000000023,13.85)) ;
#100590 = CARTESIAN_POINT('Origin',(-0.150000000000035,-0.150000000000023,
13.85)) ;
#100591 = CARTESIAN_POINT('Origin',(0.149999999999965,-0.150000000000013,
-39.25)) ;
#100592 = CARTESIAN_POINT('Origin',(0.149999999999965,-0.150000000000023,
14.15)) ;
#100593 = CARTESIAN_POINT('Origin',(0.149999999999972,-0.750000000000015,
39.85)) ;
#100594 = CARTESIAN_POINT('Origin',(0.149999999999972,-4.60000000000001,39.85)) ;
#100595 = CARTESIAN_POINT('Origin',(53.25,-4.90000000000001,39.85)) ;
#100596 = CARTESIAN_POINT('Origin',(-0.150000000000028,-4.90000000000001,
39.85)) ;
#100597 = CARTESIAN_POINT('Origin',(-1.85000000000003,-4.90000000000001,39.25)) ;
#100598 = CARTESIAN_POINT('Origin',(-1.85000000000003,-4.90000000000001,39.4)) ;
#100599 = CARTESIAN_POINT('Origin',(-1.85000000000003,-4.75000000000002,39.4)) ;
#100600 = CARTESIAN_POINT('Origin',(-1.85000000000003,-4.90000000000001,39.4)) ;
#100601 = CARTESIAN_POINT('Origin',(-1.85000000000004,-0.600000000000024,
13.85)) ;
#100602 = CARTESIAN_POINT('Origin',(-1.85000000000004,-0.600000000000024,
13.85)) ;
#100603 = CARTESIAN_POINT('Origin',(-0.150000000000035,-0.150000000000023,
14.15)) ;
#100604 = CARTESIAN_POINT('Origin',(-0.150000000000035,-0.150000000000023,
14.15)) ;
#100605 = CARTESIAN_POINT('Origin',(-0.150000000000028,-4.60000000000001,
39.85)) ;
#100606 = CARTESIAN_POINT('Origin',(-0.150000000000028,-4.60000000000001,
39.85)) ;
#100607 = CARTESIAN_POINT('Origin',(-1.85000000000003,-4.90000000000001,39.4)) ;
#100608 = CARTESIAN_POINT('Origin',(-1.85000000000003,-4.90000000000001,39.4)) ;
#100609 = CARTESIAN_POINT('Origin',(-3.46944695195361E-14,-0.600000000000024,
13.85)) ;
#100610 = CARTESIAN_POINT('Origin',(-0.150000000000035,-0.600000000000024,
13.85)) ;
#100611 = CARTESIAN_POINT('Origin',(-0.150000000000035,-0.750000000000015,
14.15)) ;
#100612 = CARTESIAN_POINT('Origin',(-0.150000000000035,-0.600000000000024,
14.15)) ;
#100613 = CARTESIAN_POINT('Origin',(-0.150000000000028,-4.60000000000001,
38.25)) ;
#100614 = CARTESIAN_POINT('Origin',(-0.150000000000028,-4.60000000000001,
39.4)) ;
#100615 = CARTESIAN_POINT('Origin',(-2.77555756156289E-14,-4.90000000000001,
39.4)) ;
#100616 = CARTESIAN_POINT('Origin',(-0.150000000000028,-4.90000000000001,
39.4)) ;
#100617 = CARTESIAN_POINT('Origin',(-0.150000000000035,-0.600000000000024,
14.15)) ;
#100618 = CARTESIAN_POINT('Origin',(0.149999999999963,-0.600000000000024,
14.15)) ;
#100619 = CARTESIAN_POINT('Origin',(-0.150000000000028,-4.60000000000001,
39.4)) ;
#100620 = CARTESIAN_POINT('Origin',(0.149999999999972,-4.60000000000001,39.4)) ;
#100621 = CARTESIAN_POINT('Origin',(0.149999999999963,-0.600000000000029,
40.)) ;
#100622 = CARTESIAN_POINT('Origin',(0.149999999999965,-0.600000000000028,
38.25)) ;
#100623 = CARTESIAN_POINT('Origin',(0.14999999999997,-19.75,39.4)) ;
#100624 = CARTESIAN_POINT('Origin',(0.14999999999997,-1.75000000000002,39.4)) ;
#100625 = CARTESIAN_POINT('Origin',(0.149999999999966,-1.75000000000003,38.25)) ;
#100626 = CARTESIAN_POINT('Origin',(10.5,-5.10000000000002,-39.85)) ;
#100627 = CARTESIAN_POINT('Origin',(7.64999999999997,-5.10000000000002,-39.85)) ;
#100628 = CARTESIAN_POINT('Origin',(10.35,-5.10000000000002,-39.85)) ;
#100629 = CARTESIAN_POINT('Origin',(7.64999999999997,-5.40000000000002,-39.85)) ;
#100630 = CARTESIAN_POINT('Origin',(7.64999999999997,-5.40000000000002,-39.85)) ;
#100631 = CARTESIAN_POINT('Origin',(7.34999999999997,-5.40000000000002,-39.85)) ;
#100632 = CARTESIAN_POINT('Origin',(10.35,-5.40000000000002,-39.85)) ;
#100633 = CARTESIAN_POINT('Origin',(10.65,-5.40000000000002,-39.85)) ;
#100634 = CARTESIAN_POINT('Origin',(10.35,-5.40000000000002,-39.85)) ;
#100635 = CARTESIAN_POINT('Origin',(7.64999999999997,-5.40000000000007,40.001)) ;
#100636 = CARTESIAN_POINT('Origin',(7.64999999999997,-5.40000000000002,-39.4)) ;
#100637 = CARTESIAN_POINT('Origin',(7.34999999999997,-5.25000000000002,-39.85)) ;
#100638 = CARTESIAN_POINT('Origin',(7.34999999999996,-15.1,-39.85)) ;
#100639 = CARTESIAN_POINT('Origin',(10.5,-15.4,-39.85)) ;
#100640 = CARTESIAN_POINT('Origin',(10.35,-15.4,-39.85)) ;
#100641 = CARTESIAN_POINT('Origin',(7.64999999999996,-15.4,-39.85)) ;
#100642 = CARTESIAN_POINT('Origin',(10.65,-5.25000000000002,-39.85)) ;
#100643 = CARTESIAN_POINT('Origin',(10.65,-15.1,-39.85)) ;
#100644 = CARTESIAN_POINT('Origin',(10.35,-5.40000000000007,40.001)) ;
#100645 = CARTESIAN_POINT('Origin',(10.35,-5.40000000000002,-39.4)) ;
#100646 = CARTESIAN_POINT('Origin',(10.5,-5.10000000000002,-39.4)) ;
#100647 = CARTESIAN_POINT('Origin',(10.35,-5.10000000000002,-39.4)) ;
#100648 = CARTESIAN_POINT('Origin',(7.64999999999997,-5.10000000000002,-39.4)) ;
#100649 = CARTESIAN_POINT('Origin',(7.64999999999997,-5.40000000000002,-39.4)) ;
#100650 = CARTESIAN_POINT('Origin',(7.34999999999997,-5.40000000000002,-39.4)) ;
#100651 = CARTESIAN_POINT('Origin',(7.64999999999996,-15.1,-39.85)) ;
#100652 = CARTESIAN_POINT('Origin',(7.64999999999996,-15.1,-39.85)) ;
#100653 = CARTESIAN_POINT('Origin',(10.35,-15.1,-39.85)) ;
#100654 = CARTESIAN_POINT('Origin',(10.35,-15.1,-39.85)) ;
#100655 = CARTESIAN_POINT('Origin',(10.35,-5.40000000000002,-39.4)) ;
#100656 = CARTESIAN_POINT('Origin',(10.65,-5.40000000000002,-39.4)) ;
#100657 = CARTESIAN_POINT('Origin',(7.34999999999997,-5.25000000000002,-39.4)) ;
#100658 = CARTESIAN_POINT('Origin',(7.34999999999996,-15.1,-39.4)) ;
#100659 = CARTESIAN_POINT('Origin',(7.64999999999996,-15.1000000000001,40.001)) ;
#100660 = CARTESIAN_POINT('Origin',(7.64999999999996,-15.1,-39.4)) ;
#100661 = CARTESIAN_POINT('Origin',(10.35,-15.1000000000001,40.001)) ;
#100662 = CARTESIAN_POINT('Origin',(10.35,-15.1,-39.4)) ;
#100663 = CARTESIAN_POINT('Origin',(10.65,-5.25000000000002,-39.4)) ;
#100664 = CARTESIAN_POINT('Origin',(10.65,-15.1,-39.4)) ;
#100665 = CARTESIAN_POINT('Origin',(7.64999999999996,-15.1,-39.4)) ;
#100666 = CARTESIAN_POINT('Origin',(7.64999999999996,-15.4,-39.4)) ;
#100667 = CARTESIAN_POINT('Origin',(10.35,-15.1,-39.4)) ;
#100668 = CARTESIAN_POINT('Origin',(10.35,-15.4,-39.4)) ;
#100669 = CARTESIAN_POINT('Origin',(10.5,-15.4,-39.4)) ;
#100670 = CARTESIAN_POINT('Origin',(16.5,-15.4000000000001,-39.85)) ;
#100671 = CARTESIAN_POINT('Origin',(16.35,-15.4000000000001,-39.85)) ;
#100672 = CARTESIAN_POINT('Origin',(13.65,-15.4000000000001,-39.85)) ;
#100673 = CARTESIAN_POINT('Origin',(16.35,-15.1000000000001,-39.85)) ;
#100674 = CARTESIAN_POINT('Origin',(16.35,-15.1000000000001,-39.85)) ;
#100675 = CARTESIAN_POINT('Origin',(16.65,-15.1000000000001,-39.85)) ;
#100676 = CARTESIAN_POINT('Origin',(13.65,-15.1000000000001,-39.85)) ;
#100677 = CARTESIAN_POINT('Origin',(13.35,-15.1000000000001,-39.85)) ;
#100678 = CARTESIAN_POINT('Origin',(13.65,-15.1000000000001,-39.85)) ;
#100679 = CARTESIAN_POINT('Origin',(16.35,-15.1000000000001,40.001)) ;
#100680 = CARTESIAN_POINT('Origin',(16.35,-15.1000000000001,-39.4)) ;
#100681 = CARTESIAN_POINT('Origin',(16.65,-5.25000000000006,-39.85)) ;
#100682 = CARTESIAN_POINT('Origin',(16.65,-5.40000000000006,-39.85)) ;
#100683 = CARTESIAN_POINT('Origin',(16.5,-5.10000000000006,-39.85)) ;
#100684 = CARTESIAN_POINT('Origin',(13.65,-5.10000000000006,-39.85)) ;
#100685 = CARTESIAN_POINT('Origin',(16.35,-5.10000000000006,-39.85)) ;
#100686 = CARTESIAN_POINT('Origin',(13.35,-5.25000000000006,-39.85)) ;
#100687 = CARTESIAN_POINT('Origin',(13.35,-5.40000000000006,-39.85)) ;
#100688 = CARTESIAN_POINT('Origin',(13.65,-15.1000000000001,40.001)) ;
#100689 = CARTESIAN_POINT('Origin',(13.65,-15.1000000000001,-39.4)) ;
#100690 = CARTESIAN_POINT('Origin',(16.5,-15.4000000000001,-39.4)) ;
#100691 = CARTESIAN_POINT('Origin',(13.65,-15.4000000000001,-39.4)) ;
#100692 = CARTESIAN_POINT('Origin',(16.35,-15.4000000000001,-39.4)) ;
#100693 = CARTESIAN_POINT('Origin',(16.35,-15.1000000000001,-39.4)) ;
#100694 = CARTESIAN_POINT('Origin',(16.65,-15.1000000000001,-39.4)) ;
#100695 = CARTESIAN_POINT('Origin',(16.35,-5.40000000000006,-39.85)) ;
#100696 = CARTESIAN_POINT('Origin',(16.35,-5.40000000000006,-39.85)) ;
#100697 = CARTESIAN_POINT('Origin',(13.65,-5.40000000000006,-39.85)) ;
#100698 = CARTESIAN_POINT('Origin',(13.65,-5.40000000000006,-39.85)) ;
#100699 = CARTESIAN_POINT('Origin',(13.65,-15.1000000000001,-39.4)) ;
#100700 = CARTESIAN_POINT('Origin',(13.35,-15.1000000000001,-39.4)) ;
#100701 = CARTESIAN_POINT('Origin',(16.65,-5.25000000000006,-39.4)) ;
#100702 = CARTESIAN_POINT('Origin',(16.65,-5.40000000000006,-39.4)) ;
#100703 = CARTESIAN_POINT('Origin',(16.35,-5.40000000000011,40.001)) ;
#100704 = CARTESIAN_POINT('Origin',(16.35,-5.40000000000006,-39.4)) ;
#100705 = CARTESIAN_POINT('Origin',(13.65,-5.40000000000011,40.001)) ;
#100706 = CARTESIAN_POINT('Origin',(13.65,-5.40000000000006,-39.4)) ;
#100707 = CARTESIAN_POINT('Origin',(13.35,-5.25000000000006,-39.4)) ;
#100708 = CARTESIAN_POINT('Origin',(13.35,-5.40000000000006,-39.4)) ;
#100709 = CARTESIAN_POINT('Origin',(16.35,-5.40000000000006,-39.4)) ;
#100710 = CARTESIAN_POINT('Origin',(16.35,-5.10000000000006,-39.4)) ;
#100711 = CARTESIAN_POINT('Origin',(13.65,-5.40000000000006,-39.4)) ;
#100712 = CARTESIAN_POINT('Origin',(13.65,-5.10000000000006,-39.4)) ;
#100713 = CARTESIAN_POINT('Origin',(16.5,-5.10000000000006,-39.4)) ;
#100714 = CARTESIAN_POINT('Origin',(38.25,-2.60000000000002,-39.85)) ;
#100715 = CARTESIAN_POINT('Origin',(19.4,-2.60000000000002,-39.85)) ;
#100716 = CARTESIAN_POINT('Origin',(38.1,-2.60000000000002,-39.85)) ;
#100717 = CARTESIAN_POINT('Origin',(19.4,-2.90000000000002,-39.85)) ;
#100718 = CARTESIAN_POINT('Origin',(19.4,-2.90000000000002,-39.85)) ;
#100719 = CARTESIAN_POINT('Origin',(19.1,-2.90000000000002,-39.85)) ;
#100720 = CARTESIAN_POINT('Origin',(38.1,-2.90000000000002,-39.85)) ;
#100721 = CARTESIAN_POINT('Origin',(38.4,-2.90000000000002,-39.85)) ;
#100722 = CARTESIAN_POINT('Origin',(38.1,-2.90000000000002,-39.85)) ;
#100723 = CARTESIAN_POINT('Origin',(19.4,-2.90000000000007,40.001)) ;
#100724 = CARTESIAN_POINT('Origin',(19.4,-2.90000000000002,-39.4)) ;
#100725 = CARTESIAN_POINT('Origin',(19.1,-2.75000000000002,-39.85)) ;
#100726 = CARTESIAN_POINT('Origin',(19.1,-13.1,-39.85)) ;
#100727 = CARTESIAN_POINT('Origin',(38.25,-13.4,-39.85)) ;
#100728 = CARTESIAN_POINT('Origin',(38.1,-13.4,-39.85)) ;
#100729 = CARTESIAN_POINT('Origin',(19.4,-13.4,-39.85)) ;
#100730 = CARTESIAN_POINT('Origin',(38.4,-2.75000000000002,-39.85)) ;
#100731 = CARTESIAN_POINT('Origin',(38.4,-13.1,-39.85)) ;
#100732 = CARTESIAN_POINT('Origin',(38.1,-2.90000000000007,40.001)) ;
#100733 = CARTESIAN_POINT('Origin',(38.1,-2.90000000000002,-39.4)) ;
#100734 = CARTESIAN_POINT('Origin',(38.25,-2.60000000000002,-39.4)) ;
#100735 = CARTESIAN_POINT('Origin',(38.1,-2.60000000000002,-39.4)) ;
#100736 = CARTESIAN_POINT('Origin',(19.4,-2.60000000000002,-39.4)) ;
#100737 = CARTESIAN_POINT('Origin',(19.4,-2.90000000000002,-39.4)) ;
#100738 = CARTESIAN_POINT('Origin',(19.1,-2.90000000000002,-39.4)) ;
#100739 = CARTESIAN_POINT('Origin',(19.4,-13.1,-39.85)) ;
#100740 = CARTESIAN_POINT('Origin',(19.4,-13.1,-39.85)) ;
#100741 = CARTESIAN_POINT('Origin',(38.1,-13.1,-39.85)) ;
#100742 = CARTESIAN_POINT('Origin',(38.1,-13.1,-39.85)) ;
#100743 = CARTESIAN_POINT('Origin',(38.1,-2.90000000000002,-39.4)) ;
#100744 = CARTESIAN_POINT('Origin',(38.4,-2.90000000000002,-39.4)) ;
#100745 = CARTESIAN_POINT('Origin',(19.1,-2.75000000000002,-39.4)) ;
#100746 = CARTESIAN_POINT('Origin',(19.1,-13.1,-39.4)) ;
#100747 = CARTESIAN_POINT('Origin',(19.4,-13.1000000000001,40.001)) ;
#100748 = CARTESIAN_POINT('Origin',(19.4,-13.1,-39.4)) ;
#100749 = CARTESIAN_POINT('Origin',(38.1,-13.1000000000001,40.001)) ;
#100750 = CARTESIAN_POINT('Origin',(38.1,-13.1,-39.4)) ;
#100751 = CARTESIAN_POINT('Origin',(38.4,-2.75000000000002,-39.4)) ;
#100752 = CARTESIAN_POINT('Origin',(38.4,-13.1,-39.4)) ;
#100753 = CARTESIAN_POINT('Origin',(19.4,-13.1,-39.4)) ;
#100754 = CARTESIAN_POINT('Origin',(19.4,-13.4,-39.4)) ;
#100755 = CARTESIAN_POINT('Origin',(38.1,-13.1,-39.4)) ;
#100756 = CARTESIAN_POINT('Origin',(38.1,-13.4,-39.4)) ;
#100757 = CARTESIAN_POINT('Origin',(38.25,-13.4,-39.4)) ;
#100758 = CARTESIAN_POINT('Origin',(46.5,-15.4000000000003,-39.85)) ;
#100759 = CARTESIAN_POINT('Origin',(46.35,-15.4000000000003,-39.85)) ;
#100760 = CARTESIAN_POINT('Origin',(43.65,-15.4000000000003,-39.85)) ;
#100761 = CARTESIAN_POINT('Origin',(46.35,-15.1000000000003,-39.85)) ;
#100762 = CARTESIAN_POINT('Origin',(46.35,-15.1000000000003,-39.85)) ;
#100763 = CARTESIAN_POINT('Origin',(46.65,-15.1000000000003,-39.85)) ;
#100764 = CARTESIAN_POINT('Origin',(43.65,-15.1000000000003,-39.85)) ;
#100765 = CARTESIAN_POINT('Origin',(43.35,-15.1000000000003,-39.85)) ;
#100766 = CARTESIAN_POINT('Origin',(43.65,-15.1000000000003,-39.85)) ;
#100767 = CARTESIAN_POINT('Origin',(46.35,-15.1000000000003,40.001)) ;
#100768 = CARTESIAN_POINT('Origin',(46.35,-15.1000000000003,-39.4)) ;
#100769 = CARTESIAN_POINT('Origin',(46.65,-5.25000000000027,-39.85)) ;
#100770 = CARTESIAN_POINT('Origin',(46.65,-5.40000000000027,-39.85)) ;
#100771 = CARTESIAN_POINT('Origin',(46.5,-5.10000000000027,-39.85)) ;
#100772 = CARTESIAN_POINT('Origin',(43.65,-5.10000000000027,-39.85)) ;
#100773 = CARTESIAN_POINT('Origin',(46.35,-5.10000000000027,-39.85)) ;
#100774 = CARTESIAN_POINT('Origin',(43.35,-5.25000000000027,-39.85)) ;
#100775 = CARTESIAN_POINT('Origin',(43.35,-5.40000000000027,-39.85)) ;
#100776 = CARTESIAN_POINT('Origin',(43.65,-15.1000000000003,40.001)) ;
#100777 = CARTESIAN_POINT('Origin',(43.65,-15.1000000000003,-39.4)) ;
#100778 = CARTESIAN_POINT('Origin',(46.5,-15.4000000000003,-39.4)) ;
#100779 = CARTESIAN_POINT('Origin',(43.65,-15.4000000000003,-39.4)) ;
#100780 = CARTESIAN_POINT('Origin',(46.35,-15.4000000000003,-39.4)) ;
#100781 = CARTESIAN_POINT('Origin',(46.35,-15.1000000000003,-39.4)) ;
#100782 = CARTESIAN_POINT('Origin',(46.65,-15.1000000000003,-39.4)) ;
#100783 = CARTESIAN_POINT('Origin',(46.35,-5.40000000000027,-39.85)) ;
#100784 = CARTESIAN_POINT('Origin',(46.35,-5.40000000000027,-39.85)) ;
#100785 = CARTESIAN_POINT('Origin',(43.65,-5.40000000000027,-39.85)) ;
#100786 = CARTESIAN_POINT('Origin',(43.65,-5.40000000000027,-39.85)) ;
#100787 = CARTESIAN_POINT('Origin',(43.65,-15.1000000000003,-39.4)) ;
#100788 = CARTESIAN_POINT('Origin',(43.35,-15.1000000000003,-39.4)) ;
#100789 = CARTESIAN_POINT('Origin',(46.65,-5.25000000000027,-39.4)) ;
#100790 = CARTESIAN_POINT('Origin',(46.65,-5.40000000000027,-39.4)) ;
#100791 = CARTESIAN_POINT('Origin',(46.35,-5.40000000000032,40.001)) ;
#100792 = CARTESIAN_POINT('Origin',(46.35,-5.40000000000027,-39.4)) ;
#100793 = CARTESIAN_POINT('Origin',(43.65,-5.40000000000032,40.001)) ;
#100794 = CARTESIAN_POINT('Origin',(43.65,-5.40000000000027,-39.4)) ;
#100795 = CARTESIAN_POINT('Origin',(43.35,-5.25000000000027,-39.4)) ;
#100796 = CARTESIAN_POINT('Origin',(43.35,-5.40000000000027,-39.4)) ;
#100797 = CARTESIAN_POINT('Origin',(46.35,-5.40000000000027,-39.4)) ;
#100798 = CARTESIAN_POINT('Origin',(46.35,-5.10000000000027,-39.4)) ;
#100799 = CARTESIAN_POINT('Origin',(43.65,-5.40000000000027,-39.4)) ;
#100800 = CARTESIAN_POINT('Origin',(43.65,-5.10000000000027,-39.4)) ;
#100801 = CARTESIAN_POINT('Origin',(46.5,-5.10000000000027,-39.4)) ;
#100802 = CARTESIAN_POINT('Origin',(53.8500000000001,-14.4,34.)) ;
#100803 = CARTESIAN_POINT('Origin',(53.8500000000001,-14.4,33.85)) ;
#100804 = CARTESIAN_POINT('Origin',(53.8500000000001,-14.4,-32.35)) ;
#100805 = CARTESIAN_POINT('Origin',(53.8500000000001,-14.1,-32.35)) ;
#100806 = CARTESIAN_POINT('Origin',(53.8500000000001,-14.1,-32.65)) ;
#100807 = CARTESIAN_POINT('Origin',(53.8500000000001,-14.1,-32.35)) ;
#100808 = CARTESIAN_POINT('Origin',(53.8500000000001,-14.1,33.85)) ;
#100809 = CARTESIAN_POINT('Origin',(53.8500000000001,-14.1,33.85)) ;
#100810 = CARTESIAN_POINT('Origin',(53.8500000000001,-14.1,34.15)) ;
#100811 = CARTESIAN_POINT('Origin',(53.85,-4.24999999999999,-32.65)) ;
#100812 = CARTESIAN_POINT('Origin',(53.85,-4.39999999999999,-32.65)) ;
#100813 = CARTESIAN_POINT('Origin',(-2.00100000000007,-14.1000000000002,-32.35)) ;
#100814 = CARTESIAN_POINT('Origin',(53.4,-14.1,-32.35)) ;
#100815 = CARTESIAN_POINT('Origin',(53.4,-14.4,3.59310653001811E-29)) ;
#100816 = CARTESIAN_POINT('Origin',(53.4,-14.4,33.85)) ;
#100817 = CARTESIAN_POINT('Origin',(53.4,-14.4,-32.35)) ;
#100818 = CARTESIAN_POINT('Origin',(-2.00100000000007,-14.1000000000002,33.85)) ;
#100819 = CARTESIAN_POINT('Origin',(53.4,-14.1,33.85)) ;
#100820 = CARTESIAN_POINT('Origin',(53.85,-4.24999999999999,34.15)) ;
#100821 = CARTESIAN_POINT('Origin',(53.85,-4.4,34.15)) ;
#100822 = CARTESIAN_POINT('Origin',(53.85,-4.1,34.)) ;
#100823 = CARTESIAN_POINT('Origin',(53.85,-4.1,-32.35)) ;
#100824 = CARTESIAN_POINT('Origin',(53.85,-4.1,33.85)) ;
#100825 = CARTESIAN_POINT('Origin',(53.85,-4.4,-32.35)) ;
#100826 = CARTESIAN_POINT('Origin',(53.85,-4.4,-32.35)) ;
#100827 = CARTESIAN_POINT('Origin',(53.4,-14.1,-32.35)) ;
#100828 = CARTESIAN_POINT('Origin',(53.4,-14.1,-32.65)) ;
#100829 = CARTESIAN_POINT('Origin',(53.4,-14.1,33.85)) ;
#100830 = CARTESIAN_POINT('Origin',(53.4,-14.1,34.15)) ;
#100831 = CARTESIAN_POINT('Origin',(53.85,-4.4,33.85)) ;
#100832 = CARTESIAN_POINT('Origin',(53.85,-4.4,33.85)) ;
#100833 = CARTESIAN_POINT('Origin',(-2.00100000000011,-4.4000000000002,-32.35)) ;
#100834 = CARTESIAN_POINT('Origin',(53.4,-4.4,-32.35)) ;
#100835 = CARTESIAN_POINT('Origin',(53.4,1.95019439194024E-13,-32.65)) ;
#100836 = CARTESIAN_POINT('Origin',(53.4,-4.4,-32.65)) ;
#100837 = CARTESIAN_POINT('Origin',(53.4,1.95019439194024E-13,34.15)) ;
#100838 = CARTESIAN_POINT('Origin',(53.4,-4.4,34.15)) ;
#100839 = CARTESIAN_POINT('Origin',(-2.00100000000011,-4.4000000000002,33.85)) ;
#100840 = CARTESIAN_POINT('Origin',(53.4,-4.4,33.85)) ;
#100841 = CARTESIAN_POINT('Origin',(53.4,-4.4,-32.35)) ;
#100842 = CARTESIAN_POINT('Origin',(53.4,-4.1,-32.35)) ;
#100843 = CARTESIAN_POINT('Origin',(53.4,-4.4,33.85)) ;
#100844 = CARTESIAN_POINT('Origin',(53.4,-4.1,33.85)) ;
#100845 = CARTESIAN_POINT('Origin',(53.4,-4.1,3.59310653001811E-29)) ;
#100846 = CARTESIAN_POINT('Origin',(43.5,-5.10000000000002,39.85)) ;
#100847 = CARTESIAN_POINT('Origin',(46.35,-5.10000000000002,39.85)) ;
#100848 = CARTESIAN_POINT('Origin',(43.65,-5.10000000000002,39.85)) ;
#100849 = CARTESIAN_POINT('Origin',(46.35,-5.40000000000002,39.85)) ;
#100850 = CARTESIAN_POINT('Origin',(46.35,-5.40000000000002,39.85)) ;
#100851 = CARTESIAN_POINT('Origin',(46.65,-5.40000000000002,39.85)) ;
#100852 = CARTESIAN_POINT('Origin',(43.65,-5.40000000000002,39.85)) ;
#100853 = CARTESIAN_POINT('Origin',(43.35,-5.40000000000002,39.85)) ;
#100854 = CARTESIAN_POINT('Origin',(43.65,-5.40000000000002,39.85)) ;
#100855 = CARTESIAN_POINT('Origin',(46.35,-5.40000000000002,-40.001)) ;
#100856 = CARTESIAN_POINT('Origin',(46.35,-5.40000000000002,39.4)) ;
#100857 = CARTESIAN_POINT('Origin',(46.65,-5.25000000000002,39.85)) ;
#100858 = CARTESIAN_POINT('Origin',(46.65,-15.1,39.85)) ;
#100859 = CARTESIAN_POINT('Origin',(43.5,-15.4,39.85)) ;
#100860 = CARTESIAN_POINT('Origin',(43.65,-15.4,39.85)) ;
#100861 = CARTESIAN_POINT('Origin',(46.35,-15.4,39.85)) ;
#100862 = CARTESIAN_POINT('Origin',(43.35,-5.25000000000002,39.85)) ;
#100863 = CARTESIAN_POINT('Origin',(43.35,-15.1,39.85)) ;
#100864 = CARTESIAN_POINT('Origin',(43.65,-5.40000000000002,-40.001)) ;
#100865 = CARTESIAN_POINT('Origin',(43.65,-5.40000000000002,39.4)) ;
#100866 = CARTESIAN_POINT('Origin',(43.5,-5.10000000000002,39.4)) ;
#100867 = CARTESIAN_POINT('Origin',(43.65,-5.10000000000002,39.4)) ;
#100868 = CARTESIAN_POINT('Origin',(46.35,-5.10000000000002,39.4)) ;
#100869 = CARTESIAN_POINT('Origin',(46.35,-5.40000000000002,39.4)) ;
#100870 = CARTESIAN_POINT('Origin',(46.65,-5.40000000000002,39.4)) ;
#100871 = CARTESIAN_POINT('Origin',(46.35,-15.1,39.85)) ;
#100872 = CARTESIAN_POINT('Origin',(46.35,-15.1,39.85)) ;
#100873 = CARTESIAN_POINT('Origin',(43.65,-15.1,39.85)) ;
#100874 = CARTESIAN_POINT('Origin',(43.65,-15.1,39.85)) ;
#100875 = CARTESIAN_POINT('Origin',(43.65,-5.40000000000002,39.4)) ;
#100876 = CARTESIAN_POINT('Origin',(43.35,-5.40000000000002,39.4)) ;
#100877 = CARTESIAN_POINT('Origin',(46.65,-5.25000000000002,39.4)) ;
#100878 = CARTESIAN_POINT('Origin',(46.65,-15.1,39.4)) ;
#100879 = CARTESIAN_POINT('Origin',(46.35,-15.1,-40.001)) ;
#100880 = CARTESIAN_POINT('Origin',(46.35,-15.1,39.4)) ;
#100881 = CARTESIAN_POINT('Origin',(43.65,-15.1,-40.001)) ;
#100882 = CARTESIAN_POINT('Origin',(43.65,-15.1,39.4)) ;
#100883 = CARTESIAN_POINT('Origin',(43.35,-5.25000000000002,39.4)) ;
#100884 = CARTESIAN_POINT('Origin',(43.35,-15.1,39.4)) ;
#100885 = CARTESIAN_POINT('Origin',(46.35,-15.1,39.4)) ;
#100886 = CARTESIAN_POINT('Origin',(46.35,-15.4,39.4)) ;
#100887 = CARTESIAN_POINT('Origin',(43.65,-15.1,39.4)) ;
#100888 = CARTESIAN_POINT('Origin',(43.65,-15.4,39.4)) ;
#100889 = CARTESIAN_POINT('Origin',(43.5,-15.4,39.4)) ;
#100890 = CARTESIAN_POINT('Origin',(37.5,-5.10000000000002,39.85)) ;
#100891 = CARTESIAN_POINT('Origin',(40.35,-5.10000000000002,39.85)) ;
#100892 = CARTESIAN_POINT('Origin',(37.65,-5.10000000000002,39.85)) ;
#100893 = CARTESIAN_POINT('Origin',(40.35,-5.40000000000002,39.85)) ;
#100894 = CARTESIAN_POINT('Origin',(40.35,-5.40000000000002,39.85)) ;
#100895 = CARTESIAN_POINT('Origin',(40.65,-5.40000000000002,39.85)) ;
#100896 = CARTESIAN_POINT('Origin',(37.65,-5.40000000000002,39.85)) ;
#100897 = CARTESIAN_POINT('Origin',(37.35,-5.40000000000002,39.85)) ;
#100898 = CARTESIAN_POINT('Origin',(37.65,-5.40000000000002,39.85)) ;
#100899 = CARTESIAN_POINT('Origin',(40.35,-5.40000000000002,-40.001)) ;
#100900 = CARTESIAN_POINT('Origin',(40.35,-5.40000000000002,39.4)) ;
#100901 = CARTESIAN_POINT('Origin',(40.65,-5.25000000000002,39.85)) ;
#100902 = CARTESIAN_POINT('Origin',(40.65,-15.1,39.85)) ;
#100903 = CARTESIAN_POINT('Origin',(37.5,-15.4,39.85)) ;
#100904 = CARTESIAN_POINT('Origin',(37.65,-15.4,39.85)) ;
#100905 = CARTESIAN_POINT('Origin',(40.35,-15.4,39.85)) ;
#100906 = CARTESIAN_POINT('Origin',(37.35,-5.25000000000002,39.85)) ;
#100907 = CARTESIAN_POINT('Origin',(37.35,-15.1,39.85)) ;
#100908 = CARTESIAN_POINT('Origin',(37.65,-5.40000000000002,-40.001)) ;
#100909 = CARTESIAN_POINT('Origin',(37.65,-5.40000000000002,39.4)) ;
#100910 = CARTESIAN_POINT('Origin',(37.5,-5.10000000000002,39.4)) ;
#100911 = CARTESIAN_POINT('Origin',(37.65,-5.10000000000002,39.4)) ;
#100912 = CARTESIAN_POINT('Origin',(40.35,-5.10000000000002,39.4)) ;
#100913 = CARTESIAN_POINT('Origin',(40.35,-5.40000000000002,39.4)) ;
#100914 = CARTESIAN_POINT('Origin',(40.65,-5.40000000000002,39.4)) ;
#100915 = CARTESIAN_POINT('Origin',(40.35,-15.1,39.85)) ;
#100916 = CARTESIAN_POINT('Origin',(40.35,-15.1,39.85)) ;
#100917 = CARTESIAN_POINT('Origin',(37.65,-15.1,39.85)) ;
#100918 = CARTESIAN_POINT('Origin',(37.65,-15.1,39.85)) ;
#100919 = CARTESIAN_POINT('Origin',(37.65,-5.40000000000002,39.4)) ;
#100920 = CARTESIAN_POINT('Origin',(37.35,-5.40000000000002,39.4)) ;
#100921 = CARTESIAN_POINT('Origin',(40.65,-5.25000000000002,39.4)) ;
#100922 = CARTESIAN_POINT('Origin',(40.65,-15.1,39.4)) ;
#100923 = CARTESIAN_POINT('Origin',(40.35,-15.1,-40.001)) ;
#100924 = CARTESIAN_POINT('Origin',(40.35,-15.1,39.4)) ;
#100925 = CARTESIAN_POINT('Origin',(37.65,-15.1,-40.001)) ;
#100926 = CARTESIAN_POINT('Origin',(37.65,-15.1,39.4)) ;
#100927 = CARTESIAN_POINT('Origin',(37.35,-5.25000000000002,39.4)) ;
#100928 = CARTESIAN_POINT('Origin',(37.35,-15.1,39.4)) ;
#100929 = CARTESIAN_POINT('Origin',(40.35,-15.1,39.4)) ;
#100930 = CARTESIAN_POINT('Origin',(40.35,-15.4,39.4)) ;
#100931 = CARTESIAN_POINT('Origin',(37.65,-15.1,39.4)) ;
#100932 = CARTESIAN_POINT('Origin',(37.65,-15.4,39.4)) ;
#100933 = CARTESIAN_POINT('Origin',(37.5,-15.4,39.4)) ;
#100934 = CARTESIAN_POINT('Origin',(31.5,-5.10000000000002,39.85)) ;
#100935 = CARTESIAN_POINT('Origin',(34.35,-5.10000000000002,39.85)) ;
#100936 = CARTESIAN_POINT('Origin',(31.65,-5.10000000000002,39.85)) ;
#100937 = CARTESIAN_POINT('Origin',(34.35,-5.40000000000002,39.85)) ;
#100938 = CARTESIAN_POINT('Origin',(34.35,-5.40000000000002,39.85)) ;
#100939 = CARTESIAN_POINT('Origin',(34.65,-5.40000000000002,39.85)) ;
#100940 = CARTESIAN_POINT('Origin',(31.65,-5.40000000000002,39.85)) ;
#100941 = CARTESIAN_POINT('Origin',(31.35,-5.40000000000002,39.85)) ;
#100942 = CARTESIAN_POINT('Origin',(31.65,-5.40000000000002,39.85)) ;
#100943 = CARTESIAN_POINT('Origin',(34.35,-5.40000000000002,-40.001)) ;
#100944 = CARTESIAN_POINT('Origin',(34.35,-5.40000000000002,39.4)) ;
#100945 = CARTESIAN_POINT('Origin',(34.65,-5.25000000000002,39.85)) ;
#100946 = CARTESIAN_POINT('Origin',(34.65,-15.1,39.85)) ;
#100947 = CARTESIAN_POINT('Origin',(31.5,-15.4,39.85)) ;
#100948 = CARTESIAN_POINT('Origin',(31.65,-15.4,39.85)) ;
#100949 = CARTESIAN_POINT('Origin',(34.35,-15.4,39.85)) ;
#100950 = CARTESIAN_POINT('Origin',(31.35,-5.25000000000002,39.85)) ;
#100951 = CARTESIAN_POINT('Origin',(31.35,-15.1,39.85)) ;
#100952 = CARTESIAN_POINT('Origin',(31.65,-5.40000000000002,-40.001)) ;
#100953 = CARTESIAN_POINT('Origin',(31.65,-5.40000000000002,39.4)) ;
#100954 = CARTESIAN_POINT('Origin',(31.5,-5.10000000000002,39.4)) ;
#100955 = CARTESIAN_POINT('Origin',(31.65,-5.10000000000002,39.4)) ;
#100956 = CARTESIAN_POINT('Origin',(34.35,-5.10000000000002,39.4)) ;
#100957 = CARTESIAN_POINT('Origin',(34.35,-5.40000000000002,39.4)) ;
#100958 = CARTESIAN_POINT('Origin',(34.65,-5.40000000000002,39.4)) ;
#100959 = CARTESIAN_POINT('Origin',(34.35,-15.1,39.85)) ;
#100960 = CARTESIAN_POINT('Origin',(34.35,-15.1,39.85)) ;
#100961 = CARTESIAN_POINT('Origin',(31.65,-15.1,39.85)) ;
#100962 = CARTESIAN_POINT('Origin',(31.65,-15.1,39.85)) ;
#100963 = CARTESIAN_POINT('Origin',(31.65,-5.40000000000002,39.4)) ;
#100964 = CARTESIAN_POINT('Origin',(31.35,-5.40000000000002,39.4)) ;
#100965 = CARTESIAN_POINT('Origin',(34.65,-5.25000000000002,39.4)) ;
#100966 = CARTESIAN_POINT('Origin',(34.65,-15.1,39.4)) ;
#100967 = CARTESIAN_POINT('Origin',(34.35,-15.1,-40.001)) ;
#100968 = CARTESIAN_POINT('Origin',(34.35,-15.1,39.4)) ;
#100969 = CARTESIAN_POINT('Origin',(31.65,-15.1,-40.001)) ;
#100970 = CARTESIAN_POINT('Origin',(31.65,-15.1,39.4)) ;
#100971 = CARTESIAN_POINT('Origin',(31.35,-5.25000000000002,39.4)) ;
#100972 = CARTESIAN_POINT('Origin',(31.35,-15.1,39.4)) ;
#100973 = CARTESIAN_POINT('Origin',(34.35,-15.1,39.4)) ;
#100974 = CARTESIAN_POINT('Origin',(34.35,-15.4,39.4)) ;
#100975 = CARTESIAN_POINT('Origin',(31.65,-15.1,39.4)) ;
#100976 = CARTESIAN_POINT('Origin',(31.65,-15.4,39.4)) ;
#100977 = CARTESIAN_POINT('Origin',(31.5,-15.4,39.4)) ;
#100978 = CARTESIAN_POINT('Origin',(25.5,-5.10000000000002,39.85)) ;
#100979 = CARTESIAN_POINT('Origin',(28.35,-5.10000000000002,39.85)) ;
#100980 = CARTESIAN_POINT('Origin',(25.65,-5.10000000000002,39.85)) ;
#100981 = CARTESIAN_POINT('Origin',(28.35,-5.40000000000002,39.85)) ;
#100982 = CARTESIAN_POINT('Origin',(28.35,-5.40000000000002,39.85)) ;
#100983 = CARTESIAN_POINT('Origin',(28.65,-5.40000000000002,39.85)) ;
#100984 = CARTESIAN_POINT('Origin',(25.65,-5.40000000000002,39.85)) ;
#100985 = CARTESIAN_POINT('Origin',(25.35,-5.40000000000002,39.85)) ;
#100986 = CARTESIAN_POINT('Origin',(25.65,-5.40000000000002,39.85)) ;
#100987 = CARTESIAN_POINT('Origin',(28.35,-5.40000000000002,-40.001)) ;
#100988 = CARTESIAN_POINT('Origin',(28.35,-5.40000000000002,39.4)) ;
#100989 = CARTESIAN_POINT('Origin',(28.65,-5.25000000000002,39.85)) ;
#100990 = CARTESIAN_POINT('Origin',(28.65,-15.1,39.85)) ;
#100991 = CARTESIAN_POINT('Origin',(25.5,-15.4,39.85)) ;
#100992 = CARTESIAN_POINT('Origin',(25.65,-15.4,39.85)) ;
#100993 = CARTESIAN_POINT('Origin',(28.35,-15.4,39.85)) ;
#100994 = CARTESIAN_POINT('Origin',(25.35,-5.25000000000002,39.85)) ;
#100995 = CARTESIAN_POINT('Origin',(25.35,-15.1,39.85)) ;
#100996 = CARTESIAN_POINT('Origin',(25.65,-5.40000000000002,-40.001)) ;
#100997 = CARTESIAN_POINT('Origin',(25.65,-5.40000000000002,39.4)) ;
#100998 = CARTESIAN_POINT('Origin',(25.5,-5.10000000000002,39.4)) ;
#100999 = CARTESIAN_POINT('Origin',(25.65,-5.10000000000002,39.4)) ;
#101000 = CARTESIAN_POINT('Origin',(28.35,-5.10000000000002,39.4)) ;
#101001 = CARTESIAN_POINT('Origin',(28.35,-5.40000000000002,39.4)) ;
#101002 = CARTESIAN_POINT('Origin',(28.65,-5.40000000000002,39.4)) ;
#101003 = CARTESIAN_POINT('Origin',(28.35,-15.1,39.85)) ;
#101004 = CARTESIAN_POINT('Origin',(28.35,-15.1,39.85)) ;
#101005 = CARTESIAN_POINT('Origin',(25.65,-15.1,39.85)) ;
#101006 = CARTESIAN_POINT('Origin',(25.65,-15.1,39.85)) ;
#101007 = CARTESIAN_POINT('Origin',(25.65,-5.40000000000002,39.4)) ;
#101008 = CARTESIAN_POINT('Origin',(25.35,-5.40000000000002,39.4)) ;
#101009 = CARTESIAN_POINT('Origin',(28.65,-5.25000000000002,39.4)) ;
#101010 = CARTESIAN_POINT('Origin',(28.65,-15.1,39.4)) ;
#101011 = CARTESIAN_POINT('Origin',(28.35,-15.1,-40.001)) ;
#101012 = CARTESIAN_POINT('Origin',(28.35,-15.1,39.4)) ;
#101013 = CARTESIAN_POINT('Origin',(25.65,-15.1,-40.001)) ;
#101014 = CARTESIAN_POINT('Origin',(25.65,-15.1,39.4)) ;
#101015 = CARTESIAN_POINT('Origin',(25.35,-5.25000000000002,39.4)) ;
#101016 = CARTESIAN_POINT('Origin',(25.35,-15.1,39.4)) ;
#101017 = CARTESIAN_POINT('Origin',(28.35,-15.1,39.4)) ;
#101018 = CARTESIAN_POINT('Origin',(28.35,-15.4,39.4)) ;
#101019 = CARTESIAN_POINT('Origin',(25.65,-15.1,39.4)) ;
#101020 = CARTESIAN_POINT('Origin',(25.65,-15.4,39.4)) ;
#101021 = CARTESIAN_POINT('Origin',(25.5,-15.4,39.4)) ;
#101022 = CARTESIAN_POINT('Origin',(19.5,-5.10000000000002,39.85)) ;
#101023 = CARTESIAN_POINT('Origin',(22.35,-5.10000000000002,39.85)) ;
#101024 = CARTESIAN_POINT('Origin',(19.65,-5.10000000000002,39.85)) ;
#101025 = CARTESIAN_POINT('Origin',(22.35,-5.40000000000002,39.85)) ;
#101026 = CARTESIAN_POINT('Origin',(22.35,-5.40000000000002,39.85)) ;
#101027 = CARTESIAN_POINT('Origin',(22.65,-5.40000000000002,39.85)) ;
#101028 = CARTESIAN_POINT('Origin',(19.65,-5.40000000000002,39.85)) ;
#101029 = CARTESIAN_POINT('Origin',(19.35,-5.40000000000002,39.85)) ;
#101030 = CARTESIAN_POINT('Origin',(19.65,-5.40000000000002,39.85)) ;
#101031 = CARTESIAN_POINT('Origin',(22.35,-5.40000000000002,-40.001)) ;
#101032 = CARTESIAN_POINT('Origin',(22.35,-5.40000000000002,39.4)) ;
#101033 = CARTESIAN_POINT('Origin',(22.65,-5.25000000000002,39.85)) ;
#101034 = CARTESIAN_POINT('Origin',(22.65,-15.1,39.85)) ;
#101035 = CARTESIAN_POINT('Origin',(19.5,-15.4,39.85)) ;
#101036 = CARTESIAN_POINT('Origin',(19.65,-15.4,39.85)) ;
#101037 = CARTESIAN_POINT('Origin',(22.35,-15.4,39.85)) ;
#101038 = CARTESIAN_POINT('Origin',(19.35,-5.25000000000002,39.85)) ;
#101039 = CARTESIAN_POINT('Origin',(19.35,-15.1,39.85)) ;
#101040 = CARTESIAN_POINT('Origin',(19.65,-5.40000000000002,-40.001)) ;
#101041 = CARTESIAN_POINT('Origin',(19.65,-5.40000000000002,39.4)) ;
#101042 = CARTESIAN_POINT('Origin',(19.5,-5.10000000000002,39.4)) ;
#101043 = CARTESIAN_POINT('Origin',(19.65,-5.10000000000002,39.4)) ;
#101044 = CARTESIAN_POINT('Origin',(22.35,-5.10000000000002,39.4)) ;
#101045 = CARTESIAN_POINT('Origin',(22.35,-5.40000000000002,39.4)) ;
#101046 = CARTESIAN_POINT('Origin',(22.65,-5.40000000000002,39.4)) ;
#101047 = CARTESIAN_POINT('Origin',(22.35,-15.1,39.85)) ;
#101048 = CARTESIAN_POINT('Origin',(22.35,-15.1,39.85)) ;
#101049 = CARTESIAN_POINT('Origin',(19.65,-15.1,39.85)) ;
#101050 = CARTESIAN_POINT('Origin',(19.65,-15.1,39.85)) ;
#101051 = CARTESIAN_POINT('Origin',(19.65,-5.40000000000002,39.4)) ;
#101052 = CARTESIAN_POINT('Origin',(19.35,-5.40000000000002,39.4)) ;
#101053 = CARTESIAN_POINT('Origin',(22.65,-5.25000000000002,39.4)) ;
#101054 = CARTESIAN_POINT('Origin',(22.65,-15.1,39.4)) ;
#101055 = CARTESIAN_POINT('Origin',(22.35,-15.1,-40.001)) ;
#101056 = CARTESIAN_POINT('Origin',(22.35,-15.1,39.4)) ;
#101057 = CARTESIAN_POINT('Origin',(19.65,-15.1,-40.001)) ;
#101058 = CARTESIAN_POINT('Origin',(19.65,-15.1,39.4)) ;
#101059 = CARTESIAN_POINT('Origin',(19.35,-5.25000000000002,39.4)) ;
#101060 = CARTESIAN_POINT('Origin',(19.35,-15.1,39.4)) ;
#101061 = CARTESIAN_POINT('Origin',(22.35,-15.1,39.4)) ;
#101062 = CARTESIAN_POINT('Origin',(22.35,-15.4,39.4)) ;
#101063 = CARTESIAN_POINT('Origin',(19.65,-15.1,39.4)) ;
#101064 = CARTESIAN_POINT('Origin',(19.65,-15.4,39.4)) ;
#101065 = CARTESIAN_POINT('Origin',(19.5,-15.4,39.4)) ;
#101066 = CARTESIAN_POINT('Origin',(13.5,-15.4,39.85)) ;
#101067 = CARTESIAN_POINT('Origin',(13.65,-15.4,39.85)) ;
#101068 = CARTESIAN_POINT('Origin',(16.35,-15.4,39.85)) ;
#101069 = CARTESIAN_POINT('Origin',(13.65,-15.1,39.85)) ;
#101070 = CARTESIAN_POINT('Origin',(13.65,-15.1,39.85)) ;
#101071 = CARTESIAN_POINT('Origin',(13.35,-15.1,39.85)) ;
#101072 = CARTESIAN_POINT('Origin',(16.35,-15.1,39.85)) ;
#101073 = CARTESIAN_POINT('Origin',(16.65,-15.1,39.85)) ;
#101074 = CARTESIAN_POINT('Origin',(16.35,-15.1,39.85)) ;
#101075 = CARTESIAN_POINT('Origin',(13.65,-15.1,-40.001)) ;
#101076 = CARTESIAN_POINT('Origin',(13.65,-15.1,39.4)) ;
#101077 = CARTESIAN_POINT('Origin',(13.35,-5.25000000000002,39.85)) ;
#101078 = CARTESIAN_POINT('Origin',(13.35,-5.40000000000002,39.85)) ;
#101079 = CARTESIAN_POINT('Origin',(13.5,-5.10000000000002,39.85)) ;
#101080 = CARTESIAN_POINT('Origin',(16.35,-5.10000000000002,39.85)) ;
#101081 = CARTESIAN_POINT('Origin',(13.65,-5.10000000000002,39.85)) ;
#101082 = CARTESIAN_POINT('Origin',(16.65,-5.25000000000002,39.85)) ;
#101083 = CARTESIAN_POINT('Origin',(16.65,-5.40000000000002,39.85)) ;
#101084 = CARTESIAN_POINT('Origin',(16.35,-15.1,-40.001)) ;
#101085 = CARTESIAN_POINT('Origin',(16.35,-15.1,39.4)) ;
#101086 = CARTESIAN_POINT('Origin',(13.5,-15.4,39.4)) ;
#101087 = CARTESIAN_POINT('Origin',(16.35,-15.4,39.4)) ;
#101088 = CARTESIAN_POINT('Origin',(13.65,-15.4,39.4)) ;
#101089 = CARTESIAN_POINT('Origin',(13.65,-15.1,39.4)) ;
#101090 = CARTESIAN_POINT('Origin',(13.35,-15.1,39.4)) ;
#101091 = CARTESIAN_POINT('Origin',(13.65,-5.40000000000002,39.85)) ;
#101092 = CARTESIAN_POINT('Origin',(13.65,-5.40000000000002,39.85)) ;
#101093 = CARTESIAN_POINT('Origin',(16.35,-5.40000000000002,39.85)) ;
#101094 = CARTESIAN_POINT('Origin',(16.35,-5.40000000000002,39.85)) ;
#101095 = CARTESIAN_POINT('Origin',(16.35,-15.1,39.4)) ;
#101096 = CARTESIAN_POINT('Origin',(16.65,-15.1,39.4)) ;
#101097 = CARTESIAN_POINT('Origin',(13.35,-5.25000000000002,39.4)) ;
#101098 = CARTESIAN_POINT('Origin',(13.35,-5.40000000000002,39.4)) ;
#101099 = CARTESIAN_POINT('Origin',(13.65,-5.40000000000002,-40.001)) ;
#101100 = CARTESIAN_POINT('Origin',(13.65,-5.40000000000002,39.4)) ;
#101101 = CARTESIAN_POINT('Origin',(16.35,-5.40000000000002,-40.001)) ;
#101102 = CARTESIAN_POINT('Origin',(16.35,-5.40000000000002,39.4)) ;
#101103 = CARTESIAN_POINT('Origin',(16.65,-5.25000000000002,39.4)) ;
#101104 = CARTESIAN_POINT('Origin',(16.65,-5.40000000000002,39.4)) ;
#101105 = CARTESIAN_POINT('Origin',(13.65,-5.40000000000002,39.4)) ;
#101106 = CARTESIAN_POINT('Origin',(13.65,-5.10000000000002,39.4)) ;
#101107 = CARTESIAN_POINT('Origin',(16.35,-5.40000000000002,39.4)) ;
#101108 = CARTESIAN_POINT('Origin',(16.35,-5.10000000000002,39.4)) ;
#101109 = CARTESIAN_POINT('Origin',(13.5,-5.10000000000002,39.4)) ;
#101110 = CARTESIAN_POINT('Origin',(7.49999999999996,-5.10000000000002,39.85)) ;
#101111 = CARTESIAN_POINT('Origin',(10.35,-5.10000000000002,39.85)) ;
#101112 = CARTESIAN_POINT('Origin',(7.64999999999996,-5.10000000000002,39.85)) ;
#101113 = CARTESIAN_POINT('Origin',(10.35,-5.40000000000002,39.85)) ;
#101114 = CARTESIAN_POINT('Origin',(10.35,-5.40000000000002,39.85)) ;
#101115 = CARTESIAN_POINT('Origin',(10.65,-5.40000000000002,39.85)) ;
#101116 = CARTESIAN_POINT('Origin',(7.64999999999996,-5.40000000000002,39.85)) ;
#101117 = CARTESIAN_POINT('Origin',(7.34999999999996,-5.40000000000002,39.85)) ;
#101118 = CARTESIAN_POINT('Origin',(7.64999999999996,-5.40000000000002,39.85)) ;
#101119 = CARTESIAN_POINT('Origin',(10.35,-5.40000000000002,-40.001)) ;
#101120 = CARTESIAN_POINT('Origin',(10.35,-5.40000000000002,39.4)) ;
#101121 = CARTESIAN_POINT('Origin',(10.65,-5.25000000000002,39.85)) ;
#101122 = CARTESIAN_POINT('Origin',(10.65,-15.1,39.85)) ;
#101123 = CARTESIAN_POINT('Origin',(7.49999999999997,-15.4,39.85)) ;
#101124 = CARTESIAN_POINT('Origin',(7.64999999999997,-15.4,39.85)) ;
#101125 = CARTESIAN_POINT('Origin',(10.35,-15.4,39.85)) ;
#101126 = CARTESIAN_POINT('Origin',(7.34999999999996,-5.25000000000002,39.85)) ;
#101127 = CARTESIAN_POINT('Origin',(7.34999999999997,-15.1,39.85)) ;
#101128 = CARTESIAN_POINT('Origin',(7.64999999999996,-5.40000000000002,-40.001)) ;
#101129 = CARTESIAN_POINT('Origin',(7.64999999999996,-5.40000000000002,39.4)) ;
#101130 = CARTESIAN_POINT('Origin',(7.49999999999996,-5.10000000000002,39.4)) ;
#101131 = CARTESIAN_POINT('Origin',(7.64999999999996,-5.10000000000002,39.4)) ;
#101132 = CARTESIAN_POINT('Origin',(10.35,-5.10000000000002,39.4)) ;
#101133 = CARTESIAN_POINT('Origin',(10.35,-5.40000000000002,39.4)) ;
#101134 = CARTESIAN_POINT('Origin',(10.65,-5.40000000000002,39.4)) ;
#101135 = CARTESIAN_POINT('Origin',(10.35,-15.1,39.85)) ;
#101136 = CARTESIAN_POINT('Origin',(10.35,-15.1,39.85)) ;
#101137 = CARTESIAN_POINT('Origin',(7.64999999999997,-15.1,39.85)) ;
#101138 = CARTESIAN_POINT('Origin',(7.64999999999997,-15.1,39.85)) ;
#101139 = CARTESIAN_POINT('Origin',(7.64999999999996,-5.40000000000002,39.4)) ;
#101140 = CARTESIAN_POINT('Origin',(7.34999999999996,-5.40000000000002,39.4)) ;
#101141 = CARTESIAN_POINT('Origin',(10.65,-5.25000000000002,39.4)) ;
#101142 = CARTESIAN_POINT('Origin',(10.65,-15.1,39.4)) ;
#101143 = CARTESIAN_POINT('Origin',(10.35,-15.1,-40.001)) ;
#101144 = CARTESIAN_POINT('Origin',(10.35,-15.1,39.4)) ;
#101145 = CARTESIAN_POINT('Origin',(7.64999999999997,-15.1,-40.001)) ;
#101146 = CARTESIAN_POINT('Origin',(7.64999999999997,-15.1,39.4)) ;
#101147 = CARTESIAN_POINT('Origin',(7.34999999999996,-5.25000000000002,39.4)) ;
#101148 = CARTESIAN_POINT('Origin',(7.34999999999997,-15.1,39.4)) ;
#101149 = CARTESIAN_POINT('Origin',(10.35,-15.1,39.4)) ;
#101150 = CARTESIAN_POINT('Origin',(10.35,-15.4,39.4)) ;
#101151 = CARTESIAN_POINT('Origin',(7.64999999999997,-15.1,39.4)) ;
#101152 = CARTESIAN_POINT('Origin',(7.64999999999997,-15.4,39.4)) ;
#101153 = CARTESIAN_POINT('Origin',(7.49999999999997,-15.4,39.4)) ;
#101154 = CARTESIAN_POINT('Origin',(53.4,-1.75,39.85)) ;
#101155 = CARTESIAN_POINT('Origin',(53.4000000000002,-1.90000000000016,39.8499999999998)) ;
#101156 = CARTESIAN_POINT('Origin',(53.4000000000001,-19.6,39.85)) ;
#101157 = CARTESIAN_POINT('Origin',(53.4,2.25743319424102E-13,-39.85)) ;
#101158 = CARTESIAN_POINT('Origin',(53.4000000000001,-19.6,-39.85)) ;
#101159 = CARTESIAN_POINT('Origin',(53.4,-1.89999999999994,-39.8500000000001)) ;
#101160 = CARTESIAN_POINT('Origin',(53.4000000000001,-19.6,-38.25)) ;
#101161 = CARTESIAN_POINT('Origin',(53.4000000000001,-19.6,39.85)) ;
#101162 = CARTESIAN_POINT('Origin',(53.4000000000001,-19.6,-39.85)) ;
#101163 = CARTESIAN_POINT('Origin',(53.4000000000001,-19.6,39.85)) ;
#101164 = CARTESIAN_POINT('Origin',(53.4000000000001,-19.6,39.85)) ;
#101165 = CARTESIAN_POINT('Origin',(54.,-1.89999999999999,39.85)) ;
#101166 = CARTESIAN_POINT('Origin',(53.8500000000008,-1.89999999999927,39.8500000000007)) ;
#101167 = CARTESIAN_POINT('Origin',(54.,-1.89999999999998,-39.85)) ;
#101168 = CARTESIAN_POINT('Origin',(53.85,-1.9,-39.85)) ;
#101169 = CARTESIAN_POINT('Origin',(53.4000000000001,-19.6,-39.85)) ;
#101170 = CARTESIAN_POINT('Origin',(53.4000000000001,-19.6,-39.85)) ;
#101171 = CARTESIAN_POINT('Origin',(54.0000000000001,-19.6,39.85)) ;
#101172 = CARTESIAN_POINT('Origin',(53.8500000000001,-19.6,39.85)) ;
#101173 = CARTESIAN_POINT('Origin',(53.85,1.96542435371224E-13,39.85)) ;
#101174 = CARTESIAN_POINT('Origin',(53.8500000000001,-19.6,39.85)) ;
#101175 = CARTESIAN_POINT('Origin',(53.85,-1.74999999999998,-39.85)) ;
#101176 = CARTESIAN_POINT('Origin',(53.8500000000001,-19.6,-39.85)) ;
#101177 = CARTESIAN_POINT('Origin',(54.0000000000001,-19.6,-39.85)) ;
#101178 = CARTESIAN_POINT('Origin',(53.8500000000001,-19.6,-39.85)) ;
#101179 = CARTESIAN_POINT('Origin',(53.8500000000001,-19.6,39.85)) ;
#101180 = CARTESIAN_POINT('Origin',(53.8500000000001,-19.6,39.85)) ;
#101181 = CARTESIAN_POINT('Origin',(53.8500000000001,-19.6,-39.85)) ;
#101182 = CARTESIAN_POINT('Origin',(53.8500000000001,-19.6,-39.85)) ;
#101183 = CARTESIAN_POINT('Origin',(53.8500000000001,-19.6,-3.55561622265573E-15)) ;
#101184 = CARTESIAN_POINT('',(0.,0.,0.)) ;
#101185 = CARTESIAN_POINT('Ctrl Pts',(8.55305389383868,6.58518362856711,0.660183628567108)) ;
#101186 = CARTESIAN_POINT('Ctrl Pts',(8.56447181517253,6.58947636230805,0.664476362308047)) ;
#101187 = CARTESIAN_POINT('Ctrl Pts',(8.57705842661295,6.59157413088145,0.66657413088145)) ;
#101188 = CARTESIAN_POINT('Ctrl Pts',(8.55305102515198,6.55898702014116,0.686379540222498)) ;
#101189 = CARTESIAN_POINT('Ctrl Pts',(8.56446969712852,6.56479854221784,0.68915347690881)) ;
#101190 = CARTESIAN_POINT('Ctrl Pts',(8.57705842709768,6.56766897765923,0.690479284265246)) ;
#101191 = CARTESIAN_POINT('Ctrl Pts',(8.55608440539073,6.54967077654144,0.726527573965357)) ;
#101192 = CARTESIAN_POINT('Ctrl Pts',(8.56803673427363,6.55578248257735,0.726868875765167)) ;
#101193 = CARTESIAN_POINT('Ctrl Pts',(8.58110225049763,6.55837193275,0.726735153349558)) ;
#101194 = CARTESIAN_POINT('Ctrl Pts',(8.56106007075016,6.56033186051354,0.763021538403806)) ;
#101195 = CARTESIAN_POINT('Ctrl Pts',(8.57385418571953,6.56560017282096,0.761796116238336)) ;
#101196 = CARTESIAN_POINT('Ctrl Pts',(8.58763814880121,6.56727264871055,0.761407094307452)) ;
#101197 = CARTESIAN_POINT('',(8.56104219912065,6.56017369985344,0.762366149055595)) ;
#101198 = CARTESIAN_POINT('',(8.55704445183394,6.58320973295714,0.665168358807856)) ;
#101199 = CARTESIAN_POINT('Ctrl Pts',(8.56104219912065,6.56017369985344,0.762366149055595)) ;
#101200 = CARTESIAN_POINT('Ctrl Pts',(8.56172006948825,6.55755272988493,0.749490016573775)) ;
#101201 = CARTESIAN_POINT('Ctrl Pts',(8.56178854742204,6.55691761311389,0.735981136540874)) ;
#101202 = CARTESIAN_POINT('Ctrl Pts',(8.56147572200372,6.55855061087387,0.722928962845481)) ;
#101203 = CARTESIAN_POINT('Ctrl Pts',(8.56116227470662,6.56018685493861,0.709850842186457)) ;
#101204 = CARTESIAN_POINT('Ctrl Pts',(8.5604843297899,6.56417103596015,0.696870920866104)) ;
#101205 = CARTESIAN_POINT('Ctrl Pts',(8.55945615587251,6.57017322470283,0.685177787303522)) ;
#101206 = CARTESIAN_POINT('Ctrl Pts',(8.55883284154061,6.57381195760861,0.678089008244737)) ;
#101207 = CARTESIAN_POINT('Ctrl Pts',(8.55807185541709,6.57823677723146,0.671364951604696)) ;
#101208 = CARTESIAN_POINT('Ctrl Pts',(8.55704487707426,6.58320791316502,0.665167537880534)) ;
#101209 = CARTESIAN_POINT('',(8.55635403291171,6.58636921675996,0.661369767825604)) ;
#101210 = CARTESIAN_POINT('Origin',(8.54420289523221,6.6281733287991,0.698058895172689)) ;
#101211 = CARTESIAN_POINT('',(8.57705842661295,6.59157413088145,0.66657413088145)) ;
#101212 = CARTESIAN_POINT('Origin',(8.6,6.52274941072028,0.597749410720281)) ;
#101213 = CARTESIAN_POINT('',(8.58355189313842,6.56397635572684,0.737566223574004)) ;
#101214 = CARTESIAN_POINT('Origin',(8.597771292818,6.65641294722129,0.739117764068465)) ;
#101215 = CARTESIAN_POINT('Ctrl Pts',(8.56104311409707,6.56017375480331,0.762365190627708)) ;
#101216 = CARTESIAN_POINT('Ctrl Pts',(8.56569547918968,6.5609490208508,0.756877613830519)) ;
#101217 = CARTESIAN_POINT('Ctrl Pts',(8.57049938306334,6.56176641478979,0.751490748652533)) ;
#101218 = CARTESIAN_POINT('Ctrl Pts',(8.57538893105717,6.56259599225628,0.746213733861456)) ;
#101219 = CARTESIAN_POINT('Ctrl Pts',(8.57808773793836,6.56305388107911,0.743301063028025)) ;
#101220 = CARTESIAN_POINT('Ctrl Pts',(8.58081254036867,6.56351521010419,0.740420620632313)) ;
#101221 = CARTESIAN_POINT('Ctrl Pts',(8.58355195315297,6.56397636517831,0.7375663802795)) ;
#101222 = CARTESIAN_POINT('Ctrl Pts',(8.5,8.3521616921714,0.647593901749794)) ;
#101223 = CARTESIAN_POINT('Ctrl Pts',(8.5,8.2900428850829,0.678653305294049)) ;
#101224 = CARTESIAN_POINT('Ctrl Pts',(8.56507848521152,8.26835005667905,0.689499719495969)) ;
#101225 = CARTESIAN_POINT('Ctrl Pts',(8.5,8.31945293993531,0.582176402731433)) ;
#101226 = CARTESIAN_POINT('Ctrl Pts',(8.5,8.26922013491182,0.637007811203667)) ;
#101227 = CARTESIAN_POINT('Ctrl Pts',(8.56507848600996,8.25199117628908,0.656781959381388)) ;
#101228 = CARTESIAN_POINT('Ctrl Pts',(8.5,8.24922766844397,0.540287293148598)) ;
#101229 = CARTESIAN_POINT('Ctrl Pts',(8.5,8.21777561643093,0.615522630177237)) ;
#101230 = CARTESIAN_POINT('Ctrl Pts',(8.57228151929423,8.21451202732349,0.637046919882372)) ;
#101231 = CARTESIAN_POINT('Ctrl Pts',(8.5,8.17221734381475,0.540287291161696)) ;
#101232 = CARTESIAN_POINT('Ctrl Pts',(8.5,8.17221734381475,0.625)) ;
#101233 = CARTESIAN_POINT('Ctrl Pts',(8.58356010126947,8.17221734381475,0.638926683544911)) ;
#101234 = CARTESIAN_POINT('',(8.50000000249538,8.20000280433619,0.542095256361575)) ;
#101235 = CARTESIAN_POINT('',(8.54742025481395,8.27608084305204,0.685634338044055)) ;
#101236 = CARTESIAN_POINT('Ctrl Pts',(8.50000000249538,8.20000280433619,0.542095256361575)) ;
#101237 = CARTESIAN_POINT('Ctrl Pts',(8.50000274011724,8.20154143765779,0.554364551548918)) ;
#101238 = CARTESIAN_POINT('Ctrl Pts',(8.50225788919788,8.20358050335012,0.566733525020421)) ;
#101239 = CARTESIAN_POINT('Ctrl Pts',(8.50614710304112,8.20657022673326,0.578084018986108)) ;
#101240 = CARTESIAN_POINT('Ctrl Pts',(8.51002595055128,8.20955198129041,0.589404259279535)) ;
#101241 = CARTESIAN_POINT('Ctrl Pts',(8.51564213392183,8.21362262975068,0.599953866479339)) ;
#101242 = CARTESIAN_POINT('Ctrl Pts',(8.52129493663065,8.21921832196825,0.609378207766048)) ;
#101243 = CARTESIAN_POINT('Ctrl Pts',(8.52933132065201,8.22717351408127,0.622776451014487)) ;
#101244 = CARTESIAN_POINT('Ctrl Pts',(8.53683691159804,8.23885362788864,0.634337556556648)) ;
#101245 = CARTESIAN_POINT('Ctrl Pts',(8.54097226482464,8.25011947738646,0.647118830382909)) ;
#101246 = CARTESIAN_POINT('Ctrl Pts',(8.54447125915462,8.25965170869904,0.657933288591762)) ;
#101247 = CARTESIAN_POINT('Ctrl Pts',(8.54617119150717,8.26873789958222,0.67006038981035)) ;
#101248 = CARTESIAN_POINT('Ctrl Pts',(8.54724932284106,8.27506683274844,0.683433539748685)) ;
#101249 = CARTESIAN_POINT('Ctrl Pts',(8.54730817192851,8.27541229338911,0.684163504313674)) ;
#101250 = CARTESIAN_POINT('Ctrl Pts',(8.5473651061662,8.27575037116516,0.684897167393986)) ;
#101251 = CARTESIAN_POINT('Ctrl Pts',(8.54742024083733,8.27608084608571,0.685634324792657)) ;
#101252 = CARTESIAN_POINT('',(8.56507848521152,8.26835005667905,0.68949971949597)) ;
#101253 = CARTESIAN_POINT('Origin',(8.6,8.3521616921714,0.647593901749795)) ;
#101254 = CARTESIAN_POINT('',(8.58356010126947,8.17221734381475,0.638926683544911)) ;
#101255 = CARTESIAN_POINT('Origin',(8.59670327708548,8.16883734299703,0.732931030480332)) ;
#101256 = CARTESIAN_POINT('',(8.5,8.17221734381475,0.540287291161696)) ;
#101257 = CARTESIAN_POINT('Origin',(8.6,8.17221734381475,0.540287291161696)) ;
#101258 = CARTESIAN_POINT('Origin',(8.5,8.16642648774923,0.762892247498121)) ;
#101259 = CARTESIAN_POINT('Origin',(2.9,3.8,0.)) ;
#101260 = CARTESIAN_POINT('',(3.,2.4,-1.7145055188063E-16)) ;
#101261 = CARTESIAN_POINT('Origin',(3.,3.8,0.)) ;
#101262 = CARTESIAN_POINT('',(2.9,2.3,-1.83697019872103E-16)) ;
#101263 = CARTESIAN_POINT('Origin',(2.9,2.4,-1.71450551880629E-16)) ;
#101264 = CARTESIAN_POINT('Origin',(2.9,3.8,0.)) ;
#101265 = CARTESIAN_POINT('Origin',(1.35,3.8,0.)) ;
#101266 = CARTESIAN_POINT('',(1.35,2.3,-1.83697019872103E-16)) ;
#101267 = CARTESIAN_POINT('Origin',(1.35,3.8,0.)) ;
#101268 = CARTESIAN_POINT('',(1.25,2.2,-1.95943487863577E-16)) ;
#101269 = CARTESIAN_POINT('Origin',(1.35,2.2,-1.95943487863577E-16)) ;
#101270 = CARTESIAN_POINT('Origin',(1.25,3.8,0.)) ;
#101271 = CARTESIAN_POINT('Origin',(13.9153543900904,1.02736587339764,0.849999999999999)) ;
#101272 = CARTESIAN_POINT('',(1.15,1.02736587339764,0.749999999999999)) ;
#101273 = CARTESIAN_POINT('',(1.15,0.931757800066529,0.879310344827585)) ;
#101274 = CARTESIAN_POINT('Origin',(1.15,1.02736587339764,0.849999999999999)) ;
#101275 = CARTESIAN_POINT('',(-0.900000000000002,1.02736587339765,0.749999999999999)) ;
#101276 = CARTESIAN_POINT('',(-1.,1.02736587339765,0.749999999999999)) ;
#101277 = CARTESIAN_POINT('',(-0.900000000000002,0.982644513847654,0.760557280900007)) ;
#101278 = CARTESIAN_POINT('Origin',(-0.900000000000002,1.02736587339765,0.849999999999999)) ;
#101279 = CARTESIAN_POINT('',(-0.900000000000002,0.93175780006653,0.879310344827585)) ;
#101280 = CARTESIAN_POINT('Origin',(-0.900000000000002,1.02736587339765,0.849999999999999)) ;
#101281 = CARTESIAN_POINT('',(13.9153543900904,0.931757800066525,0.879310344827585)) ;
#101282 = CARTESIAN_POINT('Origin',(13.9153543900904,1.02736587339764,-0.850000000000001)) ;
#101283 = CARTESIAN_POINT('',(1.15,0.93175780006653,-0.879310344827587)) ;
#101284 = CARTESIAN_POINT('',(1.15,1.02736587339765,-0.750000000000001)) ;
#101285 = CARTESIAN_POINT('Origin',(1.15,1.02736587339765,-0.850000000000001)) ;
#101286 = CARTESIAN_POINT('',(-0.900000000000002,0.931757800066531,-0.879310344827587)) ;
#101287 = CARTESIAN_POINT('',(13.9153543900904,0.931757800066525,-0.879310344827587)) ;
#101288 = CARTESIAN_POINT('',(-0.900000000000002,1.02736587339765,-0.750000000000001)) ;
#101289 = CARTESIAN_POINT('Origin',(-0.900000000000002,1.02736587339765,-0.850000000000001)) ;
#101290 = CARTESIAN_POINT('',(-1.,1.02736587339765,-0.750000000000001)) ;
#101291 = CARTESIAN_POINT('Origin',(8.49172374697003,3.8,0.)) ;
#101292 = CARTESIAN_POINT('',(8.49172374697003,1.47741935483871,1.89884679390471)) ;
#101293 = CARTESIAN_POINT('',(8.49172374697003,1.47741935483871,-1.89884679390471)) ;
#101294 = CARTESIAN_POINT('Origin',(8.49172374697003,3.8,0.)) ;
#101295 = CARTESIAN_POINT('',(8.50816364570057,1.47636598119991,1.89970798904167)) ;
#101296 = CARTESIAN_POINT('Origin',(8.49172374697003,1.4,1.96214168703486)) ;
#101297 = CARTESIAN_POINT('',(8.50816364570057,1.47636598119991,-1.89970798904167)) ;
#101298 = CARTESIAN_POINT('Origin',(8.50816364570057,3.8,0.)) ;
#101299 = CARTESIAN_POINT('Origin',(8.49172374697003,1.4,-1.96214168703486)) ;
#101300 = CARTESIAN_POINT('Origin',(1.25,3.8,0.)) ;
#101301 = CARTESIAN_POINT('',(1.25,2.3,-1.83697019872103E-16)) ;
#101302 = CARTESIAN_POINT('Origin',(13.9153543900904,3.8,0.)) ;
#101303 = CARTESIAN_POINT('',(-0.900000000000002,1.47741935483872,-1.89884679390471)) ;
#101304 = CARTESIAN_POINT('',(13.9153543900904,1.47741935483871,-1.89884679390471)) ;
#101305 = CARTESIAN_POINT('Origin',(-0.900000000000001,3.8,0.)) ;
#101306 = CARTESIAN_POINT('',(1.35,0.876327704607742,-0.672413793103449)) ;
#101307 = CARTESIAN_POINT('Ctrl Pts',(1.35,0.876327704607742,-0.672413793103449)) ;
#101308 = CARTESIAN_POINT('Ctrl Pts',(1.35,0.888571289407569,-0.725649211595278)) ;
#101309 = CARTESIAN_POINT('Ctrl Pts',(1.32969623836296,0.902340613578954,
-0.77792959702133)) ;
#101310 = CARTESIAN_POINT('Ctrl Pts',(1.25741074236298,0.924142973728496,
-0.855015053715771)) ;
#101311 = CARTESIAN_POINT('Ctrl Pts',(1.20472523187106,0.93175780006653,-0.879310344827587)) ;
#101312 = CARTESIAN_POINT('Ctrl Pts',(1.15,0.93175780006653,-0.879310344827587)) ;
#101313 = CARTESIAN_POINT('',(1.35,0.876327704607742,0.672413793103447)) ;
#101314 = CARTESIAN_POINT('Origin',(1.35,3.8,0.)) ;
#101315 = CARTESIAN_POINT('Ctrl Pts',(1.15,0.931757800066529,0.879310344827585)) ;
#101316 = CARTESIAN_POINT('Ctrl Pts',(1.20475877631964,0.931757800066529,
0.879310344827585)) ;
#101317 = CARTESIAN_POINT('Ctrl Pts',(1.2574100247738,0.924155896380523,0.855065639111651)) ;
#101318 = CARTESIAN_POINT('Ctrl Pts',(1.32987646938161,0.9022735155524,0.777687454472096)) ;
#101319 = CARTESIAN_POINT('Ctrl Pts',(1.35,0.888577265820266,0.725675197189874)) ;
#101320 = CARTESIAN_POINT('Ctrl Pts',(1.35,0.876327704607742,0.672413793103447)) ;
#101321 = CARTESIAN_POINT('',(-0.900000000000002,1.47741935483872,1.89884679390471)) ;
#101322 = CARTESIAN_POINT('Origin',(-0.900000000000001,3.8,0.)) ;
#101323 = CARTESIAN_POINT('',(13.9153543900904,1.47741935483871,1.89884679390471)) ;
#101324 = CARTESIAN_POINT('Origin',(0.55,3.09772049281573E-17,-2.67525834540015E-32)) ;
#101325 = CARTESIAN_POINT('',(0.549999999999999,4.4,0.45)) ;
#101326 = CARTESIAN_POINT('',(0.549999999999999,4.4,-0.45)) ;
#101327 = CARTESIAN_POINT('',(0.549999999999999,4.4,-2.67525834540015E-32)) ;
#101328 = CARTESIAN_POINT('',(0.55,4.04473197180486,-0.45)) ;
#101329 = CARTESIAN_POINT('',(0.55,1.39397422176708E-16,-0.450000000000001)) ;
#101330 = CARTESIAN_POINT('',(0.55,4.05997159067981,-0.4)) ;
#101331 = CARTESIAN_POINT('Ctrl Pts',(0.549999999999999,4.04473197180486,
-0.450000000000001)) ;
#101332 = CARTESIAN_POINT('Ctrl Pts',(0.549999999999999,4.04764757798806,
-0.445564861127741)) ;
#101333 = CARTESIAN_POINT('Ctrl Pts',(0.55,4.05014503921306,-0.440948144865881)) ;
#101334 = CARTESIAN_POINT('Ctrl Pts',(0.549999999999999,4.0569489863933,-0.425681445690252)) ;
#101335 = CARTESIAN_POINT('Ctrl Pts',(0.549999999999999,4.0599715906798,-0.411821456441416)) ;
#101336 = CARTESIAN_POINT('Ctrl Pts',(0.549999999999999,4.0599715906798,-0.4)) ;
#101337 = CARTESIAN_POINT('',(0.55,4.05997159067981,0.4)) ;
#101338 = CARTESIAN_POINT('',(0.55,4.05997159067981,0.5)) ;
#101339 = CARTESIAN_POINT('',(0.55,4.04473197181449,0.449999999985356)) ;
#101340 = CARTESIAN_POINT('Origin',(0.55003450380262,3.93869457791467,0.39758397030464)) ;
#101341 = CARTESIAN_POINT('',(0.55,6.35032701027224E-17,0.450000000000001)) ;
#101342 = CARTESIAN_POINT('Origin',(10.,7.8,-2.54)) ;
#101343 = CARTESIAN_POINT('',(9.93162277660169,7.82279240779944,-2.54)) ;
#101344 = CARTESIAN_POINT('',(8.51539501058484,8.29486832980505,-2.54)) ;
#101345 = CARTESIAN_POINT('',(10.,7.8,-2.54)) ;
#101346 = CARTESIAN_POINT('',(8.5154009551171,8.29487265903615,-0.769060759934173)) ;
#101347 = CARTESIAN_POINT('',(8.51539501058484,8.29486832980505,-2.54)) ;
#101348 = CARTESIAN_POINT('',(8.54856023413469,8.28398586203114,-0.756008066565519)) ;
#101349 = CARTESIAN_POINT('Ctrl Pts',(8.5154009551171,8.29487265903615,-0.769060759934173)) ;
#101350 = CARTESIAN_POINT('Ctrl Pts',(8.51716444659958,8.29428466923188,-0.769642482818871)) ;
#101351 = CARTESIAN_POINT('Ctrl Pts',(8.51901954868166,8.29366521079576,-0.769970450858189)) ;
#101352 = CARTESIAN_POINT('Ctrl Pts',(8.52087614409666,8.2930450194617,-0.770072502578372)) ;
#101353 = CARTESIAN_POINT('Ctrl Pts',(8.52171779595217,8.29276386763785,-0.770118765764716)) ;
#101354 = CARTESIAN_POINT('Ctrl Pts',(8.52256005861364,8.29248252453828,-0.770119087778023)) ;
#101355 = CARTESIAN_POINT('Ctrl Pts',(8.52339613191994,8.29220315552769,-0.770079446014073)) ;
#101356 = CARTESIAN_POINT('Ctrl Pts',(8.52456316579569,8.29181319797644,-0.770024112012765)) ;
#101357 = CARTESIAN_POINT('Ctrl Pts',(8.52573147766847,8.29142195356396,-0.769893004995753)) ;
#101358 = CARTESIAN_POINT('Ctrl Pts',(8.52689074379088,8.29103442649366,-0.769691327086012)) ;
#101359 = CARTESIAN_POINT('Ctrl Pts',(8.52858695132694,8.29046740713169,-0.76939623730141)) ;
#101360 = CARTESIAN_POINT('Ctrl Pts',(8.53026630212632,8.28992123633277,-0.768943921814253)) ;
#101361 = CARTESIAN_POINT('Ctrl Pts',(8.53190117913127,8.28939883282065,-0.768368372916171)) ;
#101362 = CARTESIAN_POINT('Ctrl Pts',(8.53241671440281,8.28923410028379,-0.76818688173576)) ;
#101363 = CARTESIAN_POINT('Ctrl Pts',(8.5329279003779,8.28907155799427,-0.767993397517365)) ;
#101364 = CARTESIAN_POINT('Ctrl Pts',(8.53343404910736,8.28891083250768,-0.767789837955259)) ;
#101365 = CARTESIAN_POINT('Ctrl Pts',(8.53529681408171,8.28831931900687,-0.767040683407564)) ;
#101366 = CARTESIAN_POINT('Ctrl Pts',(8.53711612169874,8.28774836357889,-0.766131008833549)) ;
#101367 = CARTESIAN_POINT('Ctrl Pts',(8.53885192161983,8.28720494689876,-0.765061264748013)) ;
#101368 = CARTESIAN_POINT('Ctrl Pts',(8.5401592515911,8.28679566878773,-0.764255579433931)) ;
#101369 = CARTESIAN_POINT('Ctrl Pts',(8.54141951580281,8.286401527759,-0.763359746191826)) ;
#101370 = CARTESIAN_POINT('Ctrl Pts',(8.54261761299017,8.28602171215282,-0.762392710785422)) ;
#101371 = CARTESIAN_POINT('Ctrl Pts',(8.54427390694789,8.28549664098145,-0.761055845197686)) ;
#101372 = CARTESIAN_POINT('Ctrl Pts',(8.54582756795259,8.28499592220792,-0.759557433696207)) ;
#101373 = CARTESIAN_POINT('Ctrl Pts',(8.54719190273355,8.28456181678112,-0.757913976052287)) ;
#101374 = CARTESIAN_POINT('Ctrl Pts',(8.54768505754695,8.28440490428153,-0.757319929005303)) ;
#101375 = CARTESIAN_POINT('Ctrl Pts',(8.54815358395156,8.28425671205377,-0.756707432307545)) ;
#101376 = CARTESIAN_POINT('Ctrl Pts',(8.54859369700692,8.28411936587099,-0.756078854561789)) ;
#101377 = CARTESIAN_POINT('',(8.56837597005373,8.27720399148448,-0.732505421266908)) ;
#101378 = CARTESIAN_POINT('Ctrl Pts',(8.5485198670553,8.28382649282421,-0.756014052775836)) ;
#101379 = CARTESIAN_POINT('Ctrl Pts',(8.55267891820636,8.28243778061537,-0.750563127305208)) ;
#101380 = CARTESIAN_POINT('Ctrl Pts',(8.55701747195692,8.28096933708252,-0.745259057781419)) ;
#101381 = CARTESIAN_POINT('Ctrl Pts',(8.56150853123457,8.27945301063652,-0.740113210213359)) ;
#101382 = CARTESIAN_POINT('Ctrl Pts',(8.56331520072595,8.27884302075226,-0.738043131589642)) ;
#101383 = CARTESIAN_POINT('Ctrl Pts',(8.56514663435535,8.27822544298232,-0.7359980022295)) ;
#101384 = CARTESIAN_POINT('Ctrl Pts',(8.56700126712395,8.27760232477898,-0.733975785658495)) ;
#101385 = CARTESIAN_POINT('Ctrl Pts',(8.56745273479657,8.27745064099026,-0.73348352356526)) ;
#101386 = CARTESIAN_POINT('Ctrl Pts',(8.56790562999349,8.27729861980368,-0.732995195362696)) ;
#101387 = CARTESIAN_POINT('Ctrl Pts',(8.56835731300613,8.27714712982919,-0.732505596582496)) ;
#101388 = CARTESIAN_POINT('',(9.93162277660169,7.82279240779944,-0.959712708838304)) ;
#101389 = CARTESIAN_POINT('',(9.98593528106273,7.80468823964576,-0.968764792915145)) ;
#101390 = CARTESIAN_POINT('',(9.93162277660169,7.82279240779944,-2.54)) ;
#101391 = CARTESIAN_POINT('Origin',(10.,6.8,-2.54)) ;
#101392 = CARTESIAN_POINT('',(10.,6.8847127088383,-2.54)) ;
#101393 = CARTESIAN_POINT('',(10.,7.72792407799439,-2.54)) ;
#101394 = CARTESIAN_POINT('',(10.,6.8,-2.54)) ;
#101395 = CARTESIAN_POINT('',(10.,7.72792407799439,-0.959712708838304)) ;
#101396 = CARTESIAN_POINT('',(10.,7.72792407799439,-2.54)) ;
#101397 = CARTESIAN_POINT('',(10.,6.8847127088383,-0.959712708838304)) ;
#101398 = CARTESIAN_POINT('',(10.,6.8,-0.959712708838304)) ;
#101399 = CARTESIAN_POINT('',(10.,6.8847127088383,-2.54)) ;
#101400 = CARTESIAN_POINT('Origin',(8.5,6.55,-2.54)) ;
#101401 = CARTESIAN_POINT('',(9.91643989873054,6.78607331645509,-0.959712708838304)) ;
#101402 = CARTESIAN_POINT('',(8.58355805979357,6.56393854759965,-0.737566541570668)) ;
#101403 = CARTESIAN_POINT('',(8.48442535909739,6.54740422651623,-0.721043618899445)) ;
#101404 = CARTESIAN_POINT('',(8.56107669735261,6.56009388000089,-0.762383847222383)) ;
#101405 = CARTESIAN_POINT('Ctrl Pts',(8.58354728038624,6.56400494118525,-0.737566748635123)) ;
#101406 = CARTESIAN_POINT('Ctrl Pts',(8.5783885388571,6.56313097816981,-0.742936569647583)) ;
#101407 = CARTESIAN_POINT('Ctrl Pts',(8.5733012794658,6.56225500583444,-0.748388168656423)) ;
#101408 = CARTESIAN_POINT('Ctrl Pts',(8.56834297134844,6.5614089984297,-0.753960783789144)) ;
#101409 = CARTESIAN_POINT('Ctrl Pts',(8.56587587079896,6.56098805134781,-0.756733544483026)) ;
#101410 = CARTESIAN_POINT('Ctrl Pts',(8.56344049907325,6.56057499921407,-0.75953530332024)) ;
#101411 = CARTESIAN_POINT('Ctrl Pts',(8.56104288133097,6.56017406260212,-0.762365036245923)) ;
#101412 = CARTESIAN_POINT('',(8.50816305748499,6.55136011924236,-0.777372622105259)) ;
#101413 = CARTESIAN_POINT('Ctrl Pts',(8.56125813732197,6.56020968955366,-0.76255063535366)) ;
#101414 = CARTESIAN_POINT('Ctrl Pts',(8.55737139916473,6.55956189986079,-0.767208599473684)) ;
#101415 = CARTESIAN_POINT('Ctrl Pts',(8.553063351902,6.55884389198366,-0.769967466087569)) ;
#101416 = CARTESIAN_POINT('Ctrl Pts',(8.54121332232624,6.55686888705437,-0.776523740784031)) ;
#101417 = CARTESIAN_POINT('Ctrl Pts',(8.53496267038527,6.55582711173088,-0.777961360668917)) ;
#101418 = CARTESIAN_POINT('Ctrl Pts',(8.52888665185105,6.55481444197518,-0.779279553931391)) ;
#101419 = CARTESIAN_POINT('Ctrl Pts',(8.52471102104665,6.55411850350777,-0.779597749401341)) ;
#101420 = CARTESIAN_POINT('Ctrl Pts',(8.52011475164503,6.55335245860751,-0.779702959935202)) ;
#101421 = CARTESIAN_POINT('Ctrl Pts',(8.51754797133863,6.55292466188977,-0.779718645942938)) ;
#101422 = CARTESIAN_POINT('Ctrl Pts',(8.51248317870075,6.55208052978346,-0.778963822862177)) ;
#101423 = CARTESIAN_POINT('Ctrl Pts',(8.51021540604914,6.55170256767486,-0.778370896111508)) ;
#101424 = CARTESIAN_POINT('Ctrl Pts',(8.50816120922224,6.55136020153704,-0.777376411526063)) ;
#101425 = CARTESIAN_POINT('',(8.50816364570071,6.55136060761679,-2.54)) ;
#101426 = CARTESIAN_POINT('',(8.50816364570071,6.55136060761679,-2.54)) ;
#101427 = CARTESIAN_POINT('',(9.91643989873054,6.78607331645509,-2.54)) ;
#101428 = CARTESIAN_POINT('',(8.5,6.55,-2.54)) ;
#101429 = CARTESIAN_POINT('',(9.91643989873054,6.78607331645509,-2.54)) ;
#101430 = CARTESIAN_POINT('Origin',(10.,1.5,-2.54)) ;
#101431 = CARTESIAN_POINT('',(-0.900000000000002,1.5,-1.96214168703487)) ;
#101432 = CARTESIAN_POINT('',(8.49172374697003,1.5,-1.96214168703487)) ;
#101433 = CARTESIAN_POINT('',(10.,1.5,-1.96214168703487)) ;
#101434 = CARTESIAN_POINT('',(8.49172374697003,1.5,-2.54)) ;
#101435 = CARTESIAN_POINT('',(8.49172374697003,1.5,-2.54)) ;
#101436 = CARTESIAN_POINT('',(-0.900000000000001,1.5,-2.54)) ;
#101437 = CARTESIAN_POINT('',(10.,1.5,-2.54)) ;
#101438 = CARTESIAN_POINT('',(-0.900000000000002,1.5,-1.92613602842582)) ;
#101439 = CARTESIAN_POINT('Origin',(10.,1.5,-2.54)) ;
#101440 = CARTESIAN_POINT('',(8.49172374697003,1.5,2.54)) ;
#101441 = CARTESIAN_POINT('',(-0.900000000000001,1.5,2.54)) ;
#101442 = CARTESIAN_POINT('',(10.,1.5,2.54)) ;
#101443 = CARTESIAN_POINT('',(8.49172374697003,1.5,1.96214168703487)) ;
#101444 = CARTESIAN_POINT('',(8.49172374697003,1.5,-2.54)) ;
#101445 = CARTESIAN_POINT('',(-0.900000000000002,1.5,1.96214168703487)) ;
#101446 = CARTESIAN_POINT('',(10.,1.5,1.96214168703487)) ;
#101447 = CARTESIAN_POINT('',(-0.900000000000001,1.5,-2.54)) ;
#101448 = CARTESIAN_POINT('Origin',(10.,0.,-2.54)) ;
#101449 = CARTESIAN_POINT('',(10.,0.1,2.54)) ;
#101450 = CARTESIAN_POINT('',(10.,1.16528729116168,2.54)) ;
#101451 = CARTESIAN_POINT('',(10.,0.,2.54)) ;
#101452 = CARTESIAN_POINT('',(10.,0.1,-2.54)) ;
#101453 = CARTESIAN_POINT('',(10.,0.1,-2.54)) ;
#101454 = CARTESIAN_POINT('',(10.,1.16528729116168,-2.54)) ;
#101455 = CARTESIAN_POINT('',(10.,0.,-2.54)) ;
#101456 = CARTESIAN_POINT('',(10.,1.16528729116168,-2.04416188017819)) ;
#101457 = CARTESIAN_POINT('',(10.,1.16528729116168,-2.54)) ;
#101458 = CARTESIAN_POINT('',(10.,1.16528729116168,2.04416188017819)) ;
#101459 = CARTESIAN_POINT('Origin',(10.,3.8,0.)) ;
#101460 = CARTESIAN_POINT('',(10.,1.16528729116168,-2.54)) ;
#101461 = CARTESIAN_POINT('Origin',(0.,0.,-2.54)) ;
#101462 = CARTESIAN_POINT('',(8.48377223398316,8.3,-2.54)) ;
#101463 = CARTESIAN_POINT('',(7.1,8.3,-2.54)) ;
#101464 = CARTESIAN_POINT('',(8.5,8.3,-2.54)) ;
#101465 = CARTESIAN_POINT('Origin',(8.48377223398316,8.2,-2.54)) ;
#101466 = CARTESIAN_POINT('Origin',(9.9,7.72792407799439,-2.54)) ;
#101467 = CARTESIAN_POINT('Origin',(9.9,6.8847127088383,-2.54)) ;
#101468 = CARTESIAN_POINT('',(8.49172374697018,6.55,-2.54)) ;
#101469 = CARTESIAN_POINT('Origin',(8.49172374697018,6.65,-2.54)) ;
#101470 = CARTESIAN_POINT('',(-0.900000000000001,6.55,-2.54)) ;
#101471 = CARTESIAN_POINT('',(1.25,6.55,-2.54)) ;
#101472 = CARTESIAN_POINT('',(-1.,6.45,-2.54)) ;
#101473 = CARTESIAN_POINT('Origin',(-0.9,6.45,-2.54)) ;
#101474 = CARTESIAN_POINT('',(-1.,4.65,-2.54)) ;
#101475 = CARTESIAN_POINT('',(-1.,3.46944695195362E-16,-2.54)) ;
#101476 = CARTESIAN_POINT('',(-0.900000000000001,4.55,-2.54)) ;
#101477 = CARTESIAN_POINT('Origin',(-0.900000000000001,4.65,-2.54)) ;
#101478 = CARTESIAN_POINT('',(1.15,4.55,-2.54)) ;
#101479 = CARTESIAN_POINT('',(1.57859836313889E-15,4.55,-2.54)) ;
#101480 = CARTESIAN_POINT('',(1.25,4.45,-2.54)) ;
#101481 = CARTESIAN_POINT('Origin',(1.15,4.45,-2.54)) ;
#101482 = CARTESIAN_POINT('',(1.25,3.15,-2.54)) ;
#101483 = CARTESIAN_POINT('',(1.25,1.5,-2.54)) ;
#101484 = CARTESIAN_POINT('',(1.15,3.05,-2.54)) ;
#101485 = CARTESIAN_POINT('Origin',(1.15,3.15,-2.54)) ;
#101486 = CARTESIAN_POINT('',(-0.900000000000002,3.05,-2.54)) ;
#101487 = CARTESIAN_POINT('',(1.05818132034585E-15,3.05,-2.54)) ;
#101488 = CARTESIAN_POINT('',(-1.,2.95,-2.54)) ;
#101489 = CARTESIAN_POINT('Origin',(-0.900000000000002,2.95,-2.54)) ;
#101490 = CARTESIAN_POINT('',(-1.,1.6,-2.54)) ;
#101491 = CARTESIAN_POINT('',(-1.,3.46944695195362E-16,-2.54)) ;
#101492 = CARTESIAN_POINT('Origin',(-0.900000000000002,1.6,-2.54)) ;
#101493 = CARTESIAN_POINT('',(8.50816364570057,1.49863939238321,-2.54)) ;
#101494 = CARTESIAN_POINT('Origin',(8.49172374697003,1.4,-2.54)) ;
#101495 = CARTESIAN_POINT('',(9.91643989873054,1.26392668354489,-2.54)) ;
#101496 = CARTESIAN_POINT('',(10.,1.24999999999998,-2.54)) ;
#101497 = CARTESIAN_POINT('Origin',(9.9,1.16528729116168,-2.54)) ;
#101498 = CARTESIAN_POINT('',(9.9,0.,-2.54)) ;
#101499 = CARTESIAN_POINT('Origin',(9.9,0.1,-2.54)) ;
#101500 = CARTESIAN_POINT('',(-2.,0.,-2.54)) ;
#101501 = CARTESIAN_POINT('',(-2.,0.,-2.54)) ;
#101502 = CARTESIAN_POINT('',(-2.,7.55,-2.54)) ;
#101503 = CARTESIAN_POINT('',(-2.,7.65,-2.54)) ;
#101504 = CARTESIAN_POINT('',(-1.9,7.65,-2.54)) ;
#101505 = CARTESIAN_POINT('Origin',(-1.9,7.55,-2.54)) ;
#101506 = CARTESIAN_POINT('',(6.9,7.65,-2.54)) ;
#101507 = CARTESIAN_POINT('',(7.,7.65,-2.54)) ;
#101508 = CARTESIAN_POINT('',(7.,7.75,-2.54)) ;
#101509 = CARTESIAN_POINT('Origin',(6.9,7.75,-2.54)) ;
#101510 = CARTESIAN_POINT('',(7.,8.2,-2.54)) ;
#101511 = CARTESIAN_POINT('',(7.,8.3,-2.54)) ;
#101512 = CARTESIAN_POINT('Origin',(7.1,8.2,-2.54)) ;
#101513 = CARTESIAN_POINT('Origin',(0.,0.,2.54)) ;
#101514 = CARTESIAN_POINT('',(9.93162277660169,7.82279240779944,2.54)) ;
#101515 = CARTESIAN_POINT('',(8.51539501058484,8.29486832980505,2.54)) ;
#101516 = CARTESIAN_POINT('',(10.,7.8,2.54)) ;
#101517 = CARTESIAN_POINT('',(8.48377223398316,8.3,2.54)) ;
#101518 = CARTESIAN_POINT('Origin',(8.48377223398316,8.2,2.54)) ;
#101519 = CARTESIAN_POINT('',(7.1,8.3,2.54)) ;
#101520 = CARTESIAN_POINT('',(8.5,8.3,2.54)) ;
#101521 = CARTESIAN_POINT('',(7.,8.2,2.54)) ;
#101522 = CARTESIAN_POINT('Origin',(7.1,8.2,2.54)) ;
#101523 = CARTESIAN_POINT('',(7.,7.75,2.54)) ;
#101524 = CARTESIAN_POINT('',(7.,8.3,2.54)) ;
#101525 = CARTESIAN_POINT('',(6.9,7.65,2.54)) ;
#101526 = CARTESIAN_POINT('Origin',(6.9,7.75,2.54)) ;
#101527 = CARTESIAN_POINT('',(-1.9,7.65,2.54)) ;
#101528 = CARTESIAN_POINT('',(7.,7.65,2.54)) ;
#101529 = CARTESIAN_POINT('',(-2.,7.55,2.54)) ;
#101530 = CARTESIAN_POINT('Origin',(-1.9,7.55,2.54)) ;
#101531 = CARTESIAN_POINT('',(-2.,0.,2.54)) ;
#101532 = CARTESIAN_POINT('',(-2.,7.65,2.54)) ;
#101533 = CARTESIAN_POINT('',(9.9,0.,2.54)) ;
#101534 = CARTESIAN_POINT('',(-2.,0.,2.54)) ;
#101535 = CARTESIAN_POINT('Origin',(9.9,0.1,2.54)) ;
#101536 = CARTESIAN_POINT('',(9.91643989873054,1.26392668354489,2.54)) ;
#101537 = CARTESIAN_POINT('Origin',(9.9,1.16528729116168,2.54)) ;
#101538 = CARTESIAN_POINT('',(8.50816364570057,1.49863939238321,2.54)) ;
#101539 = CARTESIAN_POINT('',(0.472972972972955,2.83783783783779,2.54)) ;
#101540 = CARTESIAN_POINT('Origin',(8.49172374697003,1.4,2.54)) ;
#101541 = CARTESIAN_POINT('',(-1.,1.6,2.54)) ;
#101542 = CARTESIAN_POINT('Origin',(-0.900000000000002,1.6,2.54)) ;
#101543 = CARTESIAN_POINT('',(-1.,2.95,2.54)) ;
#101544 = CARTESIAN_POINT('',(-1.,3.46944695195362E-16,2.54)) ;
#101545 = CARTESIAN_POINT('',(-0.900000000000002,3.05,2.54)) ;
#101546 = CARTESIAN_POINT('Origin',(-0.900000000000002,2.95,2.54)) ;
#101547 = CARTESIAN_POINT('',(1.15,3.05,2.54)) ;
#101548 = CARTESIAN_POINT('',(1.05818132034585E-15,3.05,2.54)) ;
#101549 = CARTESIAN_POINT('',(1.25,3.15,2.54)) ;
#101550 = CARTESIAN_POINT('Origin',(1.15,3.15,2.54)) ;
#101551 = CARTESIAN_POINT('',(1.25,4.45,2.54)) ;
#101552 = CARTESIAN_POINT('',(1.25,5.3,2.54)) ;
#101553 = CARTESIAN_POINT('',(1.15,4.55,2.54)) ;
#101554 = CARTESIAN_POINT('Origin',(1.15,4.45,2.54)) ;
#101555 = CARTESIAN_POINT('',(-0.900000000000001,4.55,2.54)) ;
#101556 = CARTESIAN_POINT('',(1.57859836313889E-15,4.55,2.54)) ;
#101557 = CARTESIAN_POINT('',(-1.,4.65,2.54)) ;
#101558 = CARTESIAN_POINT('Origin',(-0.900000000000001,4.65,2.54)) ;
#101559 = CARTESIAN_POINT('',(-1.,6.45,2.54)) ;
#101560 = CARTESIAN_POINT('',(-1.,3.46944695195362E-16,2.54)) ;
#101561 = CARTESIAN_POINT('',(-0.900000000000001,6.55,2.54)) ;
#101562 = CARTESIAN_POINT('Origin',(-0.9,6.45,2.54)) ;
#101563 = CARTESIAN_POINT('',(8.49172374697018,6.55,2.54)) ;
#101564 = CARTESIAN_POINT('',(1.25,6.55,2.54)) ;
#101565 = CARTESIAN_POINT('',(8.50816364570071,6.55136060761679,2.54)) ;
#101566 = CARTESIAN_POINT('Origin',(8.49172374697018,6.65,2.54)) ;
#101567 = CARTESIAN_POINT('',(9.91643989873054,6.78607331645509,2.54)) ;
#101568 = CARTESIAN_POINT('',(8.5,6.55,2.54)) ;
#101569 = CARTESIAN_POINT('',(10.,6.8847127088383,2.54)) ;
#101570 = CARTESIAN_POINT('Origin',(9.9,6.8847127088383,2.54)) ;
#101571 = CARTESIAN_POINT('',(10.,7.72792407799439,2.54)) ;
#101572 = CARTESIAN_POINT('',(10.,6.8,2.54)) ;
#101573 = CARTESIAN_POINT('Origin',(9.9,7.72792407799439,2.54)) ;
#101574 = CARTESIAN_POINT('Origin',(7.,7.65,-2.54)) ;
#101575 = CARTESIAN_POINT('',(-1.9,7.65,-2.54)) ;
#101576 = CARTESIAN_POINT('',(6.9,7.65,-2.54)) ;
#101577 = CARTESIAN_POINT('Origin',(7.,8.3,-2.54)) ;
#101578 = CARTESIAN_POINT('',(7.,7.75,2.54)) ;
#101579 = CARTESIAN_POINT('',(7.,8.2,-2.54)) ;
#101580 = CARTESIAN_POINT('Origin',(8.5,8.3,-2.54)) ;
#101581 = CARTESIAN_POINT('',(8.4,8.3,-0.542072889850983)) ;
#101582 = CARTESIAN_POINT('',(8.48377267093845,8.29999999999968,-0.758052545004225)) ;
#101583 = CARTESIAN_POINT('Ctrl Pts',(8.40000000000001,8.3,-0.542072889850983)) ;
#101584 = CARTESIAN_POINT('Ctrl Pts',(8.40000007660114,8.3,-0.559229650193567)) ;
#101585 = CARTESIAN_POINT('Ctrl Pts',(8.40222537906589,8.3,-0.576196239113767)) ;
#101586 = CARTESIAN_POINT('Ctrl Pts',(8.40642689896062,8.3,-0.592616256499238)) ;
#101587 = CARTESIAN_POINT('Ctrl Pts',(8.41084238024274,8.3,-0.609872459310139)) ;
#101588 = CARTESIAN_POINT('Ctrl Pts',(8.41744096860901,8.3,-0.626526744361822)) ;
#101589 = CARTESIAN_POINT('Ctrl Pts',(8.42598957610089,8.3,-0.642162200721529)) ;
#101590 = CARTESIAN_POINT('Ctrl Pts',(8.429275781256,8.3,-0.648172690423003)) ;
#101591 = CARTESIAN_POINT('Ctrl Pts',(8.43285067318442,8.3,-0.654032446959054)) ;
#101592 = CARTESIAN_POINT('Ctrl Pts',(8.43670279785317,8.3,-0.659716786785451)) ;
#101593 = CARTESIAN_POINT('Ctrl Pts',(8.43684245837178,8.3,-0.659922875091612)) ;
#101594 = CARTESIAN_POINT('Ctrl Pts',(8.4369824793911,8.3,-0.660128726822443)) ;
#101595 = CARTESIAN_POINT('Ctrl Pts',(8.43712286024713,8.3,-0.660334340694031)) ;
#101596 = CARTESIAN_POINT('Ctrl Pts',(8.4430409279857,8.3,-0.669002451535619)) ;
#101597 = CARTESIAN_POINT('Ctrl Pts',(8.4496323269955,8.300000000002,-0.677331731364526)) ;
#101598 = CARTESIAN_POINT('Ctrl Pts',(8.45667836512368,8.29999999999776,-0.685188273964224)) ;
#101599 = CARTESIAN_POINT('Ctrl Pts',(8.46347186896914,8.29999999999367,-0.692763233309057)) ;
#101600 = CARTESIAN_POINT('Ctrl Pts',(8.47075094334182,8.29999999998296,-0.699909865515332)) ;
#101601 = CARTESIAN_POINT('Ctrl Pts',(8.47818849074308,8.29999999991001,-0.70688161282847)) ;
#101602 = CARTESIAN_POINT('Ctrl Pts',(8.47846436286148,8.2999999999073,-0.707140207577044)) ;
#101603 = CARTESIAN_POINT('Ctrl Pts',(8.47874045306876,8.29999999990447,-0.707398560599132)) ;
#101604 = CARTESIAN_POINT('Ctrl Pts',(8.47901674447045,8.29999999990152,-0.707656685200035)) ;
#101605 = CARTESIAN_POINT('Ctrl Pts',(8.48287938578321,8.29999999986032,-0.711265348883327)) ;
#101606 = CARTESIAN_POINT('Ctrl Pts',(8.48681205529409,8.29999999978803,-0.714807936727803)) ;
#101607 = CARTESIAN_POINT('Ctrl Pts',(8.49047938959116,8.29999999977836,-0.718602706021786)) ;
#101608 = CARTESIAN_POINT('Ctrl Pts',(8.49231307405274,8.29999999977353,-0.720500108583422)) ;
#101609 = CARTESIAN_POINT('Ctrl Pts',(8.49410676862313,8.29999999978935,-0.722469327124991)) ;
#101610 = CARTESIAN_POINT('Ctrl Pts',(8.49555027122445,8.29999999981726,-0.724696807009918)) ;
#101611 = CARTESIAN_POINT('Ctrl Pts',(8.49675259850851,8.2999999998405,-0.726552127421465)) ;
#101612 = CARTESIAN_POINT('Ctrl Pts',(8.49764594203226,8.29999999986456,-0.728636815743195)) ;
#101613 = CARTESIAN_POINT('Ctrl Pts',(8.49795530287013,8.29999999987615,-0.730811037449387)) ;
#101614 = CARTESIAN_POINT('Ctrl Pts',(8.49801735255452,8.29999999987847,-0.731247129398159)) ;
#101615 = CARTESIAN_POINT('Ctrl Pts',(8.49805590844335,8.29999999988033,-0.731686822978028)) ;
#101616 = CARTESIAN_POINT('Ctrl Pts',(8.49806875158487,8.29999999988168,-0.732128989661398)) ;
#101617 = CARTESIAN_POINT('Ctrl Pts',(8.49822249685463,8.2999999998978,-0.737422167806758)) ;
#101618 = CARTESIAN_POINT('Ctrl Pts',(8.49538250015675,8.29999999989889,-0.742355344268398)) ;
#101619 = CARTESIAN_POINT('Ctrl Pts',(8.49246863081132,8.29999999993393,-0.746722860550965)) ;
#101620 = CARTESIAN_POINT('Ctrl Pts',(8.48983292606215,8.29999999996562,-0.750673443793859)) ;
#101621 = CARTESIAN_POINT('Ctrl Pts',(8.48683766317129,8.3,-0.754392211069768)) ;
#101622 = CARTESIAN_POINT('Ctrl Pts',(8.48377316486173,8.3,-0.75805195629754)) ;
#101623 = CARTESIAN_POINT('',(8.48377223398316,8.3,-2.54)) ;
#101624 = CARTESIAN_POINT('',(7.1,8.3,-2.54)) ;
#101625 = CARTESIAN_POINT('',(8.48377267093845,8.29999999999968,0.758052545004229)) ;
#101626 = CARTESIAN_POINT('',(8.48377223398316,8.3,-2.54)) ;
#101627 = CARTESIAN_POINT('',(8.4,8.3,0.542072889850983)) ;
#101628 = CARTESIAN_POINT('Ctrl Pts',(8.48377316486173,8.3,0.758051956297541)) ;
#101629 = CARTESIAN_POINT('Ctrl Pts',(8.48683766317129,8.3,0.754392211069772)) ;
#101630 = CARTESIAN_POINT('Ctrl Pts',(8.48983292606214,8.29999999996562,0.750673443793859)) ;
#101631 = CARTESIAN_POINT('Ctrl Pts',(8.49246863081131,8.29999999993393,0.746722860550971)) ;
#101632 = CARTESIAN_POINT('Ctrl Pts',(8.49538250015675,8.29999999989889,0.742355344268411)) ;
#101633 = CARTESIAN_POINT('Ctrl Pts',(8.49822249685463,8.2999999998978,0.737422167806773)) ;
#101634 = CARTESIAN_POINT('Ctrl Pts',(8.49806875158486,8.29999999988168,0.732128989661413)) ;
#101635 = CARTESIAN_POINT('Ctrl Pts',(8.49805590844334,8.29999999988033,0.731686822978042)) ;
#101636 = CARTESIAN_POINT('Ctrl Pts',(8.49801735255452,8.29999999987847,0.731247129398171)) ;
#101637 = CARTESIAN_POINT('Ctrl Pts',(8.49795530287013,8.29999999987615,0.730811037449398)) ;
#101638 = CARTESIAN_POINT('Ctrl Pts',(8.49764594190814,8.29999999986456,0.728636814870931)) ;
#101639 = CARTESIAN_POINT('Ctrl Pts',(8.49675259754384,8.2999999998405,0.726552125932736)) ;
#101640 = CARTESIAN_POINT('Ctrl Pts',(8.49555027122432,8.29999999981726,0.72469680701002)) ;
#101641 = CARTESIAN_POINT('Ctrl Pts',(8.49410676570211,8.29999999978935,0.722469322618388)) ;
#101642 = CARTESIAN_POINT('Ctrl Pts',(8.49231306928119,8.29999999977353,0.720500103647998)) ;
#101643 = CARTESIAN_POINT('Ctrl Pts',(8.49047938958768,8.29999999977836,0.718602706025179)) ;
#101644 = CARTESIAN_POINT('Ctrl Pts',(8.48681202348067,8.29999999978804,0.714807903826052)) ;
#101645 = CARTESIAN_POINT('Ctrl Pts',(8.48287934332708,8.29999999986032,0.711265309269797)) ;
#101646 = CARTESIAN_POINT('Ctrl Pts',(8.47901674443308,8.29999999990152,0.707656685240044)) ;
#101647 = CARTESIAN_POINT('Ctrl Pts',(8.47874052296043,8.29999999990447,0.707398625971892)) ;
#101648 = CARTESIAN_POINT('Ctrl Pts',(8.47846450284309,8.2999999999073,0.707140338643466)) ;
#101649 = CARTESIAN_POINT('Ctrl Pts',(8.47818870097126,8.29999999991001,0.706881809970104)) ;
#101650 = CARTESIAN_POINT('Ctrl Pts',(8.47075185325581,8.29999999998296,0.699910724672022)) ;
#101651 = CARTESIAN_POINT('Ctrl Pts',(8.46347271757075,8.29999999998104,0.692763178993)) ;
#101652 = CARTESIAN_POINT('Ctrl Pts',(8.45667934899942,8.29999999998018,0.685187391684601)) ;
#101653 = CARTESIAN_POINT('Ctrl Pts',(8.44963335392746,8.29999999997929,0.677329881896828)) ;
#101654 = CARTESIAN_POINT('Ctrl Pts',(8.44304226791565,8.29999999996634,0.668999743655032)) ;
#101655 = CARTESIAN_POINT('Ctrl Pts',(8.43712466127421,8.29999999997622,0.660333111058006)) ;
#101656 = CARTESIAN_POINT('Ctrl Pts',(8.43698358608697,8.29999999997646,0.660126499349853)) ;
#101657 = CARTESIAN_POINT('Ctrl Pts',(8.43684287437574,8.29999999997671,0.659919648720668)) ;
#101658 = CARTESIAN_POINT('Ctrl Pts',(8.43670252680326,8.29999999997696,0.659712560504486)) ;
#101659 = CARTESIAN_POINT('Ctrl Pts',(8.42665365624175,8.29999999999548,0.644885067285366)) ;
#101660 = CARTESIAN_POINT('Ctrl Pts',(8.41848789916264,8.29999999999779,0.628865136807051)) ;
#101661 = CARTESIAN_POINT('Ctrl Pts',(8.4124226058234,8.29999999999911,0.612081948601152)) ;
#101662 = CARTESIAN_POINT('Ctrl Pts',(8.40662497274128,8.30000000000037,0.596039399342023)) ;
#101663 = CARTESIAN_POINT('Ctrl Pts',(8.40274598945885,8.3,0.579297806080646)) ;
#101664 = CARTESIAN_POINT('Ctrl Pts',(8.40101973895688,8.3,0.562220211658976)) ;
#101665 = CARTESIAN_POINT('Ctrl Pts',(8.40034533497805,8.3,0.555548411932522)) ;
#101666 = CARTESIAN_POINT('Ctrl Pts',(8.40000003014814,8.3,0.548825326960162)) ;
#101667 = CARTESIAN_POINT('Ctrl Pts',(8.4,8.3,0.542072889850983)) ;
#101668 = CARTESIAN_POINT('',(8.4,8.3,-0.583654556300909)) ;
#101669 = CARTESIAN_POINT('Origin',(10.,7.8,-2.54)) ;
#101670 = CARTESIAN_POINT('',(8.56837722373805,8.27720759208727,0.732505116750499)) ;
#101671 = CARTESIAN_POINT('',(8.54843785958925,8.28385404680359,0.756019687739306)) ;
#101672 = CARTESIAN_POINT('Ctrl Pts',(8.56837722339832,8.27720759220056,0.732505116637743)) ;
#101673 = CARTESIAN_POINT('Ctrl Pts',(8.56792584473107,8.27735805175631,0.732995309772253)) ;
#101674 = CARTESIAN_POINT('Ctrl Pts',(8.56747319573485,8.27750893475505,0.733484206736226)) ;
#101675 = CARTESIAN_POINT('Ctrl Pts',(8.56702308739659,8.2776589708678,0.733975696041276)) ;
#101676 = CARTESIAN_POINT('Ctrl Pts',(8.56055949575605,8.27981350141465,0.741033521665688)) ;
#101677 = CARTESIAN_POINT('Ctrl Pts',(8.55435459773969,8.28188180075344,0.748371604530841)) ;
#101678 = CARTESIAN_POINT('Ctrl Pts',(8.54852002808959,8.28382665730347,0.756014133648572)) ;
#101679 = CARTESIAN_POINT('',(8.51539953939799,8.29486682020067,0.769059669877081)) ;
#101680 = CARTESIAN_POINT('Origin',(8.52916905055952,8.29027698314683,0.749265529521156)) ;
#101681 = CARTESIAN_POINT('',(8.51539501058484,8.29486832980505,-2.54)) ;
#101682 = CARTESIAN_POINT('',(9.93162277660169,7.82279240779944,0.959712708838304)) ;
#101683 = CARTESIAN_POINT('',(9.93162277660169,7.82279240779944,-2.54)) ;
#101684 = CARTESIAN_POINT('',(8.48593528106273,8.30468823964576,0.718764792915145)) ;
#101685 = CARTESIAN_POINT('Origin',(10.,6.8,-2.54)) ;
#101686 = CARTESIAN_POINT('',(10.,6.8847127088383,0.959712708838305)) ;
#101687 = CARTESIAN_POINT('',(10.,7.72792407799439,0.959712708838304)) ;
#101688 = CARTESIAN_POINT('',(10.,7.8,0.959712708838304)) ;
#101689 = CARTESIAN_POINT('',(10.,7.72792407799439,-2.54)) ;
#101690 = CARTESIAN_POINT('',(10.,6.8847127088383,-2.54)) ;
#101691 = CARTESIAN_POINT('Origin',(8.5,6.55,-2.54)) ;
#101692 = CARTESIAN_POINT('',(8.50816305748853,6.55136011924294,0.777372622108107)) ;
#101693 = CARTESIAN_POINT('Ctrl Pts',(8.5081612092262,6.5513602015377,0.777376411528006)) ;
#101694 = CARTESIAN_POINT('Ctrl Pts',(8.5098233077521,6.55163721795868,0.778181072182122)) ;
#101695 = CARTESIAN_POINT('Ctrl Pts',(8.51162127657737,6.55193687942956,0.778720971558941)) ;
#101696 = CARTESIAN_POINT('Ctrl Pts',(8.51523682141473,6.55253947023579,0.779428907664883)) ;
#101697 = CARTESIAN_POINT('Ctrl Pts',(8.51710259142427,6.55285043190404,0.77960653206074)) ;
#101698 = CARTESIAN_POINT('Ctrl Pts',(8.52217030373272,6.55369505062212,0.779764308873419)) ;
#101699 = CARTESIAN_POINT('Ctrl Pts',(8.52587381749938,6.55431230291657,0.779516116605555)) ;
#101700 = CARTESIAN_POINT('Ctrl Pts',(8.53482421527959,6.55580403587993,0.778270149815854)) ;
#101701 = CARTESIAN_POINT('Ctrl Pts',(8.53952102462637,6.55658683673477,0.776779552576415)) ;
#101702 = CARTESIAN_POINT('Ctrl Pts',(8.54640674065797,6.55773445607337,0.773631787754093)) ;
#101703 = CARTESIAN_POINT('Ctrl Pts',(8.55013419152225,6.55835569858704,0.771763269769364)) ;
#101704 = CARTESIAN_POINT('Ctrl Pts',(8.55581906875147,6.55930317812525,0.767956624570398)) ;
#101705 = CARTESIAN_POINT('Ctrl Pts',(8.55861150732124,6.55976858455354,0.76572244443715)) ;
#101706 = CARTESIAN_POINT('Ctrl Pts',(8.56125821409731,6.56020970234955,0.762550543343891)) ;
#101707 = CARTESIAN_POINT('',(9.91643989873054,6.78607331645509,0.959712708838304)) ;
#101708 = CARTESIAN_POINT('',(9.98442535909739,6.79740422651623,0.971043618899446)) ;
#101709 = CARTESIAN_POINT('',(9.91643989873054,6.78607331645509,-2.54)) ;
#101710 = CARTESIAN_POINT('',(8.50816364570071,6.55136060761679,-2.54)) ;
#101711 = CARTESIAN_POINT('Origin',(1.25,6.55,-2.54)) ;
#101712 = CARTESIAN_POINT('',(8.49172372711481,6.55000000000007,-0.7694558427306)) ;
#101713 = CARTESIAN_POINT('',(8.49172374697018,6.55,-2.54)) ;
#101714 = CARTESIAN_POINT('',(8.4,6.55,-0.540678001899701)) ;
#101715 = CARTESIAN_POINT('Ctrl Pts',(8.49172374697018,6.55000000000105,-0.769455745655721)) ;
#101716 = CARTESIAN_POINT('Ctrl Pts',(8.49606803673628,6.55000000001052,-0.765950586326939)) ;
#101717 = CARTESIAN_POINT('Ctrl Pts',(8.50046735944502,6.54999999990302,-0.762511904249297)) ;
#101718 = CARTESIAN_POINT('Ctrl Pts',(8.50920280475187,6.55000000136501,-0.755516026702047)) ;
#101719 = CARTESIAN_POINT('Ctrl Pts',(8.51365366733357,6.55000000372466,-0.752018918292477)) ;
#101720 = CARTESIAN_POINT('Ctrl Pts',(8.51786969589098,6.55000000840872,-0.7475740514919)) ;
#101721 = CARTESIAN_POINT('Ctrl Pts',(8.51824835575331,6.5500000088438,-0.747162834355834)) ;
#101722 = CARTESIAN_POINT('Ctrl Pts',(8.51893753951064,6.55000000964298,-0.74638941226421)) ;
#101723 = CARTESIAN_POINT('Ctrl Pts',(8.51925555226618,6.55000001000021,-0.746024683061041)) ;
#101724 = CARTESIAN_POINT('Ctrl Pts',(8.5212536251891,6.55000001218547,-0.743636966400871)) ;
#101725 = CARTESIAN_POINT('Ctrl Pts',(8.5228013177651,6.55000000862054,-0.741362521573822)) ;
#101726 = CARTESIAN_POINT('Ctrl Pts',(8.52354796988917,6.55000000490364,-0.736217268201258)) ;
#101727 = CARTESIAN_POINT('Ctrl Pts',(8.52233587755859,6.5500000056078,-0.733562917823344)) ;
#101728 = CARTESIAN_POINT('Ctrl Pts',(8.52032554216557,6.55000000470579,-0.731161010570529)) ;
#101729 = CARTESIAN_POINT('Ctrl Pts',(8.52004618744965,6.55000000456892,-0.730855467224597)) ;
#101730 = CARTESIAN_POINT('Ctrl Pts',(8.51943244221713,6.55000000425258,-0.730237557550688)) ;
#101731 = CARTESIAN_POINT('Ctrl Pts',(8.51910103101863,6.55000000405877,-0.729917277321387)) ;
#101732 = CARTESIAN_POINT('Ctrl Pts',(8.51460799223814,6.5500000014124,-0.725734931004252)) ;
#101733 = CARTESIAN_POINT('Ctrl Pts',(8.50969722522567,6.55000000036127,-0.722960241153036)) ;
#101734 = CARTESIAN_POINT('Ctrl Pts',(8.50463600502766,6.55000000021577,-0.719663474838837)) ;
#101735 = CARTESIAN_POINT('Ctrl Pts',(8.50427412871952,6.55000000020764,-0.719427280126575)) ;
#101736 = CARTESIAN_POINT('Ctrl Pts',(8.49410349041856,6.55000000002642,-0.712774331281524)) ;
#101737 = CARTESIAN_POINT('Ctrl Pts',(8.48448997361529,6.54999999999179,-0.706080938962322)) ;
#101738 = CARTESIAN_POINT('Ctrl Pts',(8.46629237463083,6.55000000001684,-0.690977024388696)) ;
#101739 = CARTESIAN_POINT('Ctrl Pts',(8.45766562693777,6.55000000000152,-0.682593931661903)) ;
#101740 = CARTESIAN_POINT('Ctrl Pts',(8.44955830666695,6.55,-0.673212334268187)) ;
#101741 = CARTESIAN_POINT('Ctrl Pts',(8.44937081015221,6.55,-0.672994428311737)) ;
#101742 = CARTESIAN_POINT('Ctrl Pts',(8.43720071044349,6.5500000000026,-0.65878927402097)) ;
#101743 = CARTESIAN_POINT('Ctrl Pts',(8.42721384365643,6.55000000009149,-0.643256668187946)) ;
#101744 = CARTESIAN_POINT('Ctrl Pts',(8.41184903642185,6.55000000007035,-0.610595055314441)) ;
#101745 = CARTESIAN_POINT('Ctrl Pts',(8.4063554780816,6.5500000000232,-0.593517332523761)) ;
#101746 = CARTESIAN_POINT('Ctrl Pts',(8.40108598764536,6.5499999999995,-0.564358808750087)) ;
#101747 = CARTESIAN_POINT('Ctrl Pts',(8.4,6.55,-0.552559527935716)) ;
#101748 = CARTESIAN_POINT('Ctrl Pts',(8.4,6.55,-0.540678001899701)) ;
#101749 = CARTESIAN_POINT('',(8.4,6.55,0.540678001899701)) ;
#101750 = CARTESIAN_POINT('',(8.4,6.55,0.723639392383214)) ;
#101751 = CARTESIAN_POINT('',(8.4917237271148,6.5500000000004,0.769455842731608)) ;
#101752 = CARTESIAN_POINT('Ctrl Pts',(8.4,6.55000000000001,0.540678001899701)) ;
#101753 = CARTESIAN_POINT('Ctrl Pts',(8.4,6.55000000000001,0.558539648405557)) ;
#101754 = CARTESIAN_POINT('Ctrl Pts',(8.40245177849658,6.55000000000111,0.57621494191016)) ;
#101755 = CARTESIAN_POINT('Ctrl Pts',(8.40709634751528,6.55000000003439,0.593248151244056)) ;
#101756 = CARTESIAN_POINT('Ctrl Pts',(8.41193897064627,6.55000000006908,0.611007692158)) ;
#101757 = CARTESIAN_POINT('Ctrl Pts',(8.4191659430817,6.55000000013771,0.628071111857661)) ;
#101758 = CARTESIAN_POINT('Ctrl Pts',(8.42853896333683,6.55000000013582,0.643918732683401)) ;
#101759 = CARTESIAN_POINT('Ctrl Pts',(8.43455058705941,6.55000000013461,0.654083005320109)) ;
#101760 = CARTESIAN_POINT('Ctrl Pts',(8.44144611055298,6.55000000009671,0.663746999277865)) ;
#101761 = CARTESIAN_POINT('Ctrl Pts',(8.44917210140207,6.55000000005186,0.672767316898348)) ;
#101762 = CARTESIAN_POINT('Ctrl Pts',(8.4493621952364,6.55000000005075,0.672989256944207)) ;
#101763 = CARTESIAN_POINT('Ctrl Pts',(8.44955278293316,6.55000000004968,0.673210797713723)) ;
#101764 = CARTESIAN_POINT('Ctrl Pts',(8.44974386351697,6.55000000004864,0.67343193698325)) ;
#101765 = CARTESIAN_POINT('Ctrl Pts',(8.45766118910685,6.55000000000559,0.682594728736607)) ;
#101766 = CARTESIAN_POINT('Ctrl Pts',(8.4662887064648,6.54999999999865,0.690978448496742)) ;
#101767 = CARTESIAN_POINT('Ctrl Pts',(8.47555348469885,6.55000000000007,0.69866472405094)) ;
#101768 = CARTESIAN_POINT('Ctrl Pts',(8.48448851770303,6.55000000000144,0.70607743529141)) ;
#101769 = CARTESIAN_POINT('Ctrl Pts',(8.49410273695376,6.5500000000304,0.712765307029448)) ;
#101770 = CARTESIAN_POINT('Ctrl Pts',(8.50391213313781,6.55000000016212,0.719176104228815)) ;
#101771 = CARTESIAN_POINT('Ctrl Pts',(8.50409415224108,6.55000000016456,0.719295060333305)) ;
#101772 = CARTESIAN_POINT('Ctrl Pts',(8.50427622716234,6.55000000016576,0.719413940206856)) ;
#101773 = CARTESIAN_POINT('Ctrl Pts',(8.50445835579895,6.55000000016577,0.71953274536795)) ;
#101774 = CARTESIAN_POINT('Ctrl Pts',(8.50464048443556,6.55000000016577,0.719651550529044)) ;
#101775 = CARTESIAN_POINT('Ctrl Pts',(8.50482266678753,6.55000000016459,0.719770280977681)) ;
#101776 = CARTESIAN_POINT('Ctrl Pts',(8.50500490075221,6.55000000016234,0.719888938232344)) ;
#101777 = CARTESIAN_POINT('Ctrl Pts',(8.50970297364421,6.55000000010443,0.722947975182689)) ;
#101778 = CARTESIAN_POINT('Ctrl Pts',(8.51460443926436,6.55000000028677,0.725724345929427)) ;
#101779 = CARTESIAN_POINT('Ctrl Pts',(8.51874830926329,6.55000000038295,0.729563015271579)) ;
#101780 = CARTESIAN_POINT('Ctrl Pts',(8.51909542442957,6.550000000391,0.729884565017908)) ;
#101781 = CARTESIAN_POINT('Ctrl Pts',(8.51943721516333,6.55000000039357,0.730213585498476)) ;
#101782 = CARTESIAN_POINT('Ctrl Pts',(8.51977310187182,6.55000000039098,0.730550883852702)) ;
#101783 = CARTESIAN_POINT('Ctrl Pts',(8.52085916897635,6.5500000003826,0.731641515418871)) ;
#101784 = CARTESIAN_POINT('Ctrl Pts',(8.52182399801739,6.55000000033868,0.732955379118005)) ;
#101785 = CARTESIAN_POINT('Ctrl Pts',(8.52246334063462,6.55000000029842,0.734373233340337)) ;
#101786 = CARTESIAN_POINT('Ctrl Pts',(8.52278301194323,6.55000000027828,0.735082160451502)) ;
#101787 = CARTESIAN_POINT('Ctrl Pts',(8.52302131164589,6.55000000025926,0.735817085193467)) ;
#101788 = CARTESIAN_POINT('Ctrl Pts',(8.52315270869756,6.55000000024662,0.73656310236501)) ;
#101789 = CARTESIAN_POINT('Ctrl Pts',(8.52328410574922,6.55000000023398,0.737309119536553)) ;
#101790 = CARTESIAN_POINT('Ctrl Pts',(8.5233086001499,6.55000000022778,0.738066229137675)) ;
#101791 = CARTESIAN_POINT('Ctrl Pts',(8.52320066085453,6.55000000023233,0.738819525967153)) ;
#101792 = CARTESIAN_POINT('Ctrl Pts',(8.52284031330749,6.55000000024754,0.741334353063084)) ;
#101793 = CARTESIAN_POINT('Ctrl Pts',(8.52133564423351,6.55000000029586,0.743593261986886)) ;
#101794 = CARTESIAN_POINT('Ctrl Pts',(8.5196587899188,6.55000000031744,0.745601348504568)) ;
#101795 = CARTESIAN_POINT('Ctrl Pts',(8.51932554032813,6.55000000032173,0.746000425516912)) ;
#101796 = CARTESIAN_POINT('Ctrl Pts',(8.51898545723479,6.55000000032523,0.746389624235137)) ;
#101797 = CARTESIAN_POINT('Ctrl Pts',(8.51864615038491,6.5500000003277,0.74676898768062)) ;
#101798 = CARTESIAN_POINT('Ctrl Pts',(8.5145508165866,6.55000000035749,0.751347792796721)) ;
#101799 = CARTESIAN_POINT('Ctrl Pts',(8.50963987409779,6.55000000028078,0.755179791381347)) ;
#101800 = CARTESIAN_POINT('Ctrl Pts',(8.50482177382261,6.55000000018958,0.759031129874613)) ;
#101801 = CARTESIAN_POINT('Ctrl Pts',(8.50046402923751,6.5500000001071,0.762514483998816)) ;
#101802 = CARTESIAN_POINT('Ctrl Pts',(8.49606692679174,6.55000000001227,0.765950989453777)) ;
#101803 = CARTESIAN_POINT('Ctrl Pts',(8.49172374697017,6.55000000000105,0.769455745656203)) ;
#101804 = CARTESIAN_POINT('',(8.49172374697018,6.55,-2.54)) ;
#101805 = CARTESIAN_POINT('',(-0.9,6.55,0.850000000000003)) ;
#101806 = CARTESIAN_POINT('',(-0.900000000000001,6.55,-2.54)) ;
#101807 = CARTESIAN_POINT('',(1.15,6.55,0.850000000000003)) ;
#101808 = CARTESIAN_POINT('',(1.25,6.55,0.850000000000003)) ;
#101809 = CARTESIAN_POINT('',(1.35,6.55,0.650000000000003)) ;
#101810 = CARTESIAN_POINT('Origin',(1.15,6.55,0.650000000000003)) ;
#101811 = CARTESIAN_POINT('',(1.35,6.55,-0.65)) ;
#101812 = CARTESIAN_POINT('',(1.35,6.55,-0.75)) ;
#101813 = CARTESIAN_POINT('',(1.15,6.55,-0.85)) ;
#101814 = CARTESIAN_POINT('Origin',(1.15,6.55,-0.65)) ;
#101815 = CARTESIAN_POINT('',(-0.9,6.55,-0.85)) ;
#101816 = CARTESIAN_POINT('',(1.25,6.55,-0.85)) ;
#101817 = CARTESIAN_POINT('',(-0.9,6.55,-2.54)) ;
#101818 = CARTESIAN_POINT('Origin',(1.25,5.3,-2.54)) ;
#101819 = CARTESIAN_POINT('',(1.25,3.15,-1.6431676725155)) ;
#101820 = CARTESIAN_POINT('',(1.25,3.04189189189189,-1.46552792413544)) ;
#101821 = CARTESIAN_POINT('Origin',(1.25,2.95,-1.6431676725155)) ;
#101822 = CARTESIAN_POINT('',(1.25,3.15,-2.54)) ;
#101823 = CARTESIAN_POINT('',(1.25,4.45,-1.6431676725155)) ;
#101824 = CARTESIAN_POINT('',(1.25,4.45,-1.58113883008419)) ;
#101825 = CARTESIAN_POINT('',(1.25,4.55810810810811,-1.46552792413544)) ;
#101826 = CARTESIAN_POINT('Origin',(1.25,4.65,-1.6431676725155)) ;
#101827 = CARTESIAN_POINT('',(1.25,5.26552792413544,-0.758108108108109)) ;
#101828 = CARTESIAN_POINT('Origin',(1.25,3.8,0.)) ;
#101829 = CARTESIAN_POINT('',(1.25,5.4431676725155,-0.65)) ;
#101830 = CARTESIAN_POINT('Origin',(1.25,5.4431676725155,-0.850000000000001)) ;
#101831 = CARTESIAN_POINT('',(1.25,6.45,-0.65)) ;
#101832 = CARTESIAN_POINT('',(1.25,6.55,-0.65)) ;
#101833 = CARTESIAN_POINT('',(1.25,6.45,0.650000000000003)) ;
#101834 = CARTESIAN_POINT('',(1.25,6.45,0.750000000000003)) ;
#101835 = CARTESIAN_POINT('',(1.25,5.4431676725155,0.650000000000002)) ;
#101836 = CARTESIAN_POINT('',(1.25,5.38113883008419,0.650000000000002)) ;
#101837 = CARTESIAN_POINT('',(1.25,5.26552792413544,0.75810810810811)) ;
#101838 = CARTESIAN_POINT('Origin',(1.25,5.4431676725155,0.850000000000002)) ;
#101839 = CARTESIAN_POINT('',(1.25,4.55810810810811,1.46552792413544)) ;
#101840 = CARTESIAN_POINT('Origin',(1.25,3.8,0.)) ;
#101841 = CARTESIAN_POINT('',(1.25,4.45,1.6431676725155)) ;
#101842 = CARTESIAN_POINT('Origin',(1.25,4.65,1.6431676725155)) ;
#101843 = CARTESIAN_POINT('',(1.25,4.45,2.54)) ;
#101844 = CARTESIAN_POINT('',(1.25,3.15,1.6431676725155)) ;
#101845 = CARTESIAN_POINT('',(1.25,3.15,1.58113883008419)) ;
#101846 = CARTESIAN_POINT('',(1.25,3.04189189189189,1.46552792413544)) ;
#101847 = CARTESIAN_POINT('Origin',(1.25,2.95,1.6431676725155)) ;
#101848 = CARTESIAN_POINT('',(1.25,2.33447207586456,0.758108108108108)) ;
#101849 = CARTESIAN_POINT('Origin',(1.25,3.8,0.)) ;
#101850 = CARTESIAN_POINT('',(1.25,2.1568323274845,0.65)) ;
#101851 = CARTESIAN_POINT('Origin',(1.25,2.1568323274845,0.850000000000001)) ;
#101852 = CARTESIAN_POINT('',(1.25,0.973783447787483,0.649999999999999)) ;
#101853 = CARTESIAN_POINT('',(1.25,0.895262490344437,0.649999999999999)) ;
#101854 = CARTESIAN_POINT('',(1.25,0.973783447787483,-0.650000000000001)) ;
#101855 = CARTESIAN_POINT('Origin',(1.25,3.8,0.)) ;
#101856 = CARTESIAN_POINT('',(1.25,2.1568323274845,-0.65)) ;
#101857 = CARTESIAN_POINT('',(1.25,2.21886116991581,-0.65)) ;
#101858 = CARTESIAN_POINT('',(1.25,2.33447207586456,-0.758108108108109)) ;
#101859 = CARTESIAN_POINT('Origin',(1.25,2.1568323274845,-0.850000000000001)) ;
#101860 = CARTESIAN_POINT('Origin',(1.25,3.8,0.)) ;
#101861 = CARTESIAN_POINT('Origin',(-2.,0.,-2.54)) ;
#101862 = CARTESIAN_POINT('',(0.899999999999999,0.,-1.6)) ;
#101863 = CARTESIAN_POINT('',(1.1,0.,-1.4)) ;
#101864 = CARTESIAN_POINT('Origin',(0.899999999999999,0.,-1.4)) ;
#101865 = CARTESIAN_POINT('',(-2.,0.,-1.6)) ;
#101866 = CARTESIAN_POINT('',(-2.,0.,-1.6)) ;
#101867 = CARTESIAN_POINT('',(-2.,0.,-2.54)) ;
#101868 = CARTESIAN_POINT('',(9.9,0.,-2.54)) ;
#101869 = CARTESIAN_POINT('',(-2.,0.,1.6)) ;
#101870 = CARTESIAN_POINT('',(-2.,0.,-2.54)) ;
#101871 = CARTESIAN_POINT('',(0.899999999999999,0.,1.6)) ;
#101872 = CARTESIAN_POINT('',(0.999999999999999,0.,1.6)) ;
#101873 = CARTESIAN_POINT('',(1.1,0.,1.4)) ;
#101874 = CARTESIAN_POINT('Origin',(0.899999999999999,0.,1.4)) ;
#101875 = CARTESIAN_POINT('',(1.1,0.,-1.5)) ;
#101876 = CARTESIAN_POINT('Origin',(-2.,7.65,-2.54)) ;
#101877 = CARTESIAN_POINT('',(-2.,6.9,1.6)) ;
#101878 = CARTESIAN_POINT('',(-2.,7.1,1.4)) ;
#101879 = CARTESIAN_POINT('Origin',(-2.,6.9,1.4)) ;
#101880 = CARTESIAN_POINT('',(-2.,-1.13380619344889E-17,1.6)) ;
#101881 = CARTESIAN_POINT('',(-2.,7.55,-2.54)) ;
#101882 = CARTESIAN_POINT('',(-2.,6.9,-1.6)) ;
#101883 = CARTESIAN_POINT('',(-2.,7.,-1.6)) ;
#101884 = CARTESIAN_POINT('',(-2.,7.1,-1.4)) ;
#101885 = CARTESIAN_POINT('Origin',(-2.,6.9,-1.4)) ;
#101886 = CARTESIAN_POINT('',(-2.,7.1,1.5)) ;
#101887 = CARTESIAN_POINT('Origin',(-1.8,7.,1.5)) ;
#101888 = CARTESIAN_POINT('',(-1.7,0.1,1.5)) ;
#101889 = CARTESIAN_POINT('',(-1.9,0.1,1.5)) ;
#101890 = CARTESIAN_POINT('',(-2.,0.1,1.5)) ;
#101891 = CARTESIAN_POINT('',(-1.9,0.3,1.5)) ;
#101892 = CARTESIAN_POINT('',(-1.9,7.,1.5)) ;
#101893 = CARTESIAN_POINT('Origin',(-1.7,0.3,1.5)) ;
#101894 = CARTESIAN_POINT('Origin',(-1.8,7.,-1.5)) ;
#101895 = CARTESIAN_POINT('',(-1.9,0.3,-1.5)) ;
#101896 = CARTESIAN_POINT('',(-1.7,0.1,-1.5)) ;
#101897 = CARTESIAN_POINT('Origin',(-1.7,0.3,-1.5)) ;
#101898 = CARTESIAN_POINT('',(-1.9,0.1,-1.5)) ;
#101899 = CARTESIAN_POINT('',(-1.9,1.23908819712629E-17,-1.5)) ;
#101900 = CARTESIAN_POINT('',(0.999999999999999,0.1,-1.5)) ;
#101901 = CARTESIAN_POINT('Origin',(-1.8,-2.2514151555628E-16,-1.7912294869673E-32)) ;
#101902 = CARTESIAN_POINT('',(-1.8,4.6,-0.65)) ;
#101903 = CARTESIAN_POINT('',(-1.8,4.6,0.65)) ;
#101904 = CARTESIAN_POINT('',(-1.8,4.6,0.55)) ;
#101905 = CARTESIAN_POINT('',(-1.8,0.3,0.650000000000001)) ;
#101906 = CARTESIAN_POINT('',(-1.8,0.2,0.650000000000001)) ;
#101907 = CARTESIAN_POINT('',(-1.8,0.3,1.4)) ;
#101908 = CARTESIAN_POINT('',(-1.8,0.3,1.5)) ;
#101909 = CARTESIAN_POINT('',(-1.8,6.9,1.4)) ;
#101910 = CARTESIAN_POINT('',(-1.8,-5.16691679585995E-17,1.4)) ;
#101911 = CARTESIAN_POINT('',(-1.8,6.9,-1.4)) ;
#101912 = CARTESIAN_POINT('',(-1.8,6.9,-1.7912294869673E-32)) ;
#101913 = CARTESIAN_POINT('',(-1.8,0.3,-1.4)) ;
#101914 = CARTESIAN_POINT('',(-1.8,-3.98613863153961E-16,-1.4)) ;
#101915 = CARTESIAN_POINT('',(-1.8,0.3,-0.65)) ;
#101916 = CARTESIAN_POINT('',(-1.8,0.3,-0.550000000000001)) ;
#101917 = CARTESIAN_POINT('',(-1.8,4.5,-0.65)) ;
#101918 = CARTESIAN_POINT('Origin',(0.549999999999999,4.5,0.55)) ;
#101919 = CARTESIAN_POINT('',(-1.7,0.3,0.550000000000001)) ;
#101920 = CARTESIAN_POINT('',(-1.7,4.4,0.55)) ;
#101921 = CARTESIAN_POINT('',(-1.7,4.5,0.55)) ;
#101922 = CARTESIAN_POINT('',(0.45,4.4,0.55)) ;
#101923 = CARTESIAN_POINT('',(0.45,4.4,0.55)) ;
#101924 = CARTESIAN_POINT('',(0.45,0.3,0.550000000000001)) ;
#101925 = CARTESIAN_POINT('',(0.45,4.5,0.55)) ;
#101926 = CARTESIAN_POINT('',(0.549999999999999,0.3,0.550000000000001)) ;
#101927 = CARTESIAN_POINT('Origin',(0.549999999999999,4.5,-0.549999999999999)) ;
#101928 = CARTESIAN_POINT('',(0.45,0.3,-0.55)) ;
#101929 = CARTESIAN_POINT('',(0.45,4.4,-0.549999999999999)) ;
#101930 = CARTESIAN_POINT('',(0.45,4.5,-0.549999999999999)) ;
#101931 = CARTESIAN_POINT('',(-1.7,4.4,-0.55)) ;
#101932 = CARTESIAN_POINT('',(-1.7,4.4,-0.549999999999999)) ;
#101933 = CARTESIAN_POINT('',(-1.7,0.3,-0.55)) ;
#101934 = CARTESIAN_POINT('',(-1.7,0.2,-0.550000000000001)) ;
#101935 = CARTESIAN_POINT('',(0.549999999999999,0.3,-0.55)) ;
#101936 = CARTESIAN_POINT('Origin',(0.549999999999999,4.5,-0.549999999999999)) ;
#101937 = CARTESIAN_POINT('',(-1.7,4.5,0.45)) ;
#101938 = CARTESIAN_POINT('',(-1.7,4.5,-0.45)) ;
#101939 = CARTESIAN_POINT('',(-1.7,4.5,-0.549999999999999)) ;
#101940 = CARTESIAN_POINT('',(0.45,4.5,-0.45)) ;
#101941 = CARTESIAN_POINT('',(0.45,4.5,-0.45)) ;
#101942 = CARTESIAN_POINT('',(0.45,4.5,0.45)) ;
#101943 = CARTESIAN_POINT('',(0.45,4.5,-0.549999999999999)) ;
#101944 = CARTESIAN_POINT('',(-1.7,4.5,0.45)) ;
#101945 = CARTESIAN_POINT('Origin',(0.55,3.09772049281573E-17,-2.67525834540015E-32)) ;
#101946 = CARTESIAN_POINT('',(0.55,2.61224989991992,-0.4)) ;
#101947 = CARTESIAN_POINT('',(0.55,2.65280931275608,-0.45)) ;
#101948 = CARTESIAN_POINT('Ctrl Pts',(0.55,2.61224989991992,-0.4)) ;
#101949 = CARTESIAN_POINT('Ctrl Pts',(0.55,2.61224989991992,-0.403869744161984)) ;
#101950 = CARTESIAN_POINT('Ctrl Pts',(0.55,2.61317624258758,-0.408420103915689)) ;
#101951 = CARTESIAN_POINT('Ctrl Pts',(0.55,2.61634258087509,-0.416633000858876)) ;
#101952 = CARTESIAN_POINT('Ctrl Pts',(0.55,2.61951410407877,-0.421630428645295)) ;
#101953 = CARTESIAN_POINT('Ctrl Pts',(0.55,2.63040394024853,-0.43493871907015)) ;
#101954 = CARTESIAN_POINT('Ctrl Pts',(0.55,2.64148366881061,-0.443170580967422)) ;
#101955 = CARTESIAN_POINT('Ctrl Pts',(0.55,2.65280931275608,-0.449999999999997)) ;
#101956 = CARTESIAN_POINT('',(0.55,0.3,-0.450000000000001)) ;
#101957 = CARTESIAN_POINT('',(0.55,1.39397422176708E-16,-0.450000000000001)) ;
#101958 = CARTESIAN_POINT('',(0.55,0.3,0.450000000000001)) ;
#101959 = CARTESIAN_POINT('',(0.55,0.3,0.550000000000001)) ;
#101960 = CARTESIAN_POINT('',(0.55,2.65280931275594,0.449999999999914)) ;
#101961 = CARTESIAN_POINT('',(0.55,6.35032701027224E-17,0.450000000000001)) ;
#101962 = CARTESIAN_POINT('',(0.55,2.61224989991992,0.4)) ;
#101963 = CARTESIAN_POINT('Ctrl Pts',(0.55,2.65280931275594,0.449999999999911)) ;
#101964 = CARTESIAN_POINT('Ctrl Pts',(0.55,2.64148366881051,0.443170580967354)) ;
#101965 = CARTESIAN_POINT('Ctrl Pts',(0.55,2.6304039402485,0.434938719070111)) ;
#101966 = CARTESIAN_POINT('Ctrl Pts',(0.55,2.61951410407877,0.421630428645295)) ;
#101967 = CARTESIAN_POINT('Ctrl Pts',(0.55,2.61634258087509,0.416633000858876)) ;
#101968 = CARTESIAN_POINT('Ctrl Pts',(0.55,2.61317624258758,0.408420103915689)) ;
#101969 = CARTESIAN_POINT('Ctrl Pts',(0.55,2.61224989991992,0.403869744161984)) ;
#101970 = CARTESIAN_POINT('Ctrl Pts',(0.55,2.61224989991992,0.4)) ;
#101971 = CARTESIAN_POINT('',(0.55,2.61224989991992,0.5)) ;
#101972 = CARTESIAN_POINT('Origin',(0.,0.2,0.)) ;
#101973 = CARTESIAN_POINT('',(-1.7,0.2,-0.65)) ;
#101974 = CARTESIAN_POINT('',(-1.7,0.2,-1.4)) ;
#101975 = CARTESIAN_POINT('',(-1.7,0.2,-1.5)) ;
#101976 = CARTESIAN_POINT('',(0.899999999999999,0.2,-1.4)) ;
#101977 = CARTESIAN_POINT('',(0.999999999999999,0.2,-1.4)) ;
#101978 = CARTESIAN_POINT('',(0.899999999999999,0.2,1.4)) ;
#101979 = CARTESIAN_POINT('',(0.899999999999999,0.2,1.5)) ;
#101980 = CARTESIAN_POINT('',(-1.7,0.2,1.4)) ;
#101981 = CARTESIAN_POINT('',(-1.8,0.2,1.4)) ;
#101982 = CARTESIAN_POINT('',(-1.7,0.2,0.650000000000001)) ;
#101983 = CARTESIAN_POINT('',(-1.7,0.2,0.550000000000001)) ;
#101984 = CARTESIAN_POINT('',(0.65,0.2,0.650000000000001)) ;
#101985 = CARTESIAN_POINT('',(-1.16429916652874E-32,0.2,0.650000000000001)) ;
#101986 = CARTESIAN_POINT('',(0.65,0.2,-0.65)) ;
#101987 = CARTESIAN_POINT('',(0.65,0.2,-0.550000000000001)) ;
#101988 = CARTESIAN_POINT('',(-1.35834902761687E-32,0.2,-0.65)) ;
#101989 = CARTESIAN_POINT('Origin',(3.,2.3,-2.54)) ;
#101990 = CARTESIAN_POINT('',(3.,4.2,0.5)) ;
#101991 = CARTESIAN_POINT('',(3.,3.4,0.5)) ;
#101992 = CARTESIAN_POINT('',(3.,2.3,0.5)) ;
#101993 = CARTESIAN_POINT('',(3.,4.3,0.4)) ;
#101994 = CARTESIAN_POINT('Origin',(3.,4.2,0.4)) ;
#101995 = CARTESIAN_POINT('',(3.,4.3,-0.4)) ;
#101996 = CARTESIAN_POINT('',(3.,4.3,-2.54)) ;
#101997 = CARTESIAN_POINT('',(3.,4.2,-0.5)) ;
#101998 = CARTESIAN_POINT('Origin',(3.,4.2,-0.4)) ;
#101999 = CARTESIAN_POINT('',(3.,3.4,-0.5)) ;
#102000 = CARTESIAN_POINT('',(3.,2.3,-0.5)) ;
#102001 = CARTESIAN_POINT('',(3.,3.3,-0.4)) ;
#102002 = CARTESIAN_POINT('Origin',(3.,3.4,-0.4)) ;
#102003 = CARTESIAN_POINT('',(3.,3.3,0.4)) ;
#102004 = CARTESIAN_POINT('',(3.,3.3,-2.54)) ;
#102005 = CARTESIAN_POINT('Origin',(3.,3.4,0.4)) ;
#102006 = CARTESIAN_POINT('Origin',(-1.,3.8,0.)) ;
#102007 = CARTESIAN_POINT('',(-1.,1.6,-1.96214168703487)) ;
#102008 = CARTESIAN_POINT('',(-1.,1.55483870967742,-1.83555190077455)) ;
#102009 = CARTESIAN_POINT('Origin',(-1.,1.40000000000001,-1.96214168703487)) ;
#102010 = CARTESIAN_POINT('',(-1.,1.6,-2.54)) ;
#102011 = CARTESIAN_POINT('',(-1.,2.95,-1.6431676725155)) ;
#102012 = CARTESIAN_POINT('',(-1.,2.95,-3.80476326321452E-16)) ;
#102013 = CARTESIAN_POINT('',(-1.,2.1568323274845,-0.850000000000001)) ;
#102014 = CARTESIAN_POINT('Origin',(-1.,3.8,0.)) ;
#102015 = CARTESIAN_POINT('',(-1.,1.02736587339765,-0.850000000000001)) ;
#102016 = CARTESIAN_POINT('',(-1.,3.8,-0.85)) ;
#102017 = CARTESIAN_POINT('Origin',(-1.,3.8,0.)) ;
#102018 = CARTESIAN_POINT('Origin',(-1.,3.05,-2.55)) ;
#102019 = CARTESIAN_POINT('',(1.15,3.05,-1.6431676725155)) ;
#102020 = CARTESIAN_POINT('',(1.15,3.05,-1.58113883008419)) ;
#102021 = CARTESIAN_POINT('',(-0.900000000000002,3.05,-1.6431676725155)) ;
#102022 = CARTESIAN_POINT('',(-1.,3.05,-1.6431676725155)) ;
#102023 = CARTESIAN_POINT('',(-0.900000000000002,3.05,-2.55)) ;
#102024 = CARTESIAN_POINT('Origin',(-1.,2.21886116991581,-0.750000000000001)) ;
#102025 = CARTESIAN_POINT('',(-0.900000000000002,2.1568323274845,-0.750000000000001)) ;
#102026 = CARTESIAN_POINT('',(1.15,2.1568323274845,-0.750000000000001)) ;
#102027 = CARTESIAN_POINT('',(1.25,2.1568323274845,-0.750000000000001)) ;
#102028 = CARTESIAN_POINT('',(1.15,0.895262490344437,-0.750000000000001)) ;
#102029 = CARTESIAN_POINT('',(-0.900000000000002,2.21886116991581,-0.750000000000001)) ;
#102030 = CARTESIAN_POINT('Origin',(-1.,3.8,0.)) ;
#102031 = CARTESIAN_POINT('',(-0.900000000000002,2.24565220167453,-0.804054054054055)) ;
#102032 = CARTESIAN_POINT('',(-0.900000000000001,2.99594594594595,-1.55434779832547)) ;
#102033 = CARTESIAN_POINT('Origin',(-0.900000000000001,3.8,0.)) ;
#102034 = CARTESIAN_POINT('',(1.15,2.99594594594595,-1.55434779832547)) ;
#102035 = CARTESIAN_POINT('',(-1.,2.99594594594595,-1.55434779832547)) ;
#102036 = CARTESIAN_POINT('',(1.15,2.24565220167453,-0.804054054054055)) ;
#102037 = CARTESIAN_POINT('Origin',(1.15,3.8,0.)) ;
#102038 = CARTESIAN_POINT('',(-1.,2.24565220167453,-0.804054054054055)) ;
#102039 = CARTESIAN_POINT('Origin',(-1.,3.8,0.)) ;
#102040 = CARTESIAN_POINT('',(-0.900000000000002,2.99594594594594,1.55434779832547)) ;
#102041 = CARTESIAN_POINT('',(-0.900000000000002,2.24565220167453,0.804054054054054)) ;
#102042 = CARTESIAN_POINT('Origin',(-0.900000000000001,3.8,0.)) ;
#102043 = CARTESIAN_POINT('',(1.15,2.24565220167453,0.804054054054054)) ;
#102044 = CARTESIAN_POINT('',(-1.,2.24565220167453,0.804054054054054)) ;
#102045 = CARTESIAN_POINT('',(1.15,2.99594594594594,1.55434779832547)) ;
#102046 = CARTESIAN_POINT('Origin',(1.15,3.8,0.)) ;
#102047 = CARTESIAN_POINT('',(-1.,2.99594594594594,1.55434779832547)) ;
#102048 = CARTESIAN_POINT('Origin',(-1.,2.21886116991581,0.75)) ;
#102049 = CARTESIAN_POINT('',(1.15,2.1568323274845,0.75)) ;
#102050 = CARTESIAN_POINT('',(1.15,2.21886116991581,0.75)) ;
#102051 = CARTESIAN_POINT('',(-0.900000000000002,2.1568323274845,0.75)) ;
#102052 = CARTESIAN_POINT('',(-1.,2.1568323274845,0.75)) ;
#102053 = CARTESIAN_POINT('',(-0.900000000000002,0.895262490344437,0.749999999999999)) ;
#102054 = CARTESIAN_POINT('Origin',(-1.,3.05,2.55)) ;
#102055 = CARTESIAN_POINT('',(-0.900000000000002,3.05,1.6431676725155)) ;
#102056 = CARTESIAN_POINT('',(1.15,3.05,1.6431676725155)) ;
#102057 = CARTESIAN_POINT('',(1.25,3.05,1.6431676725155)) ;
#102058 = CARTESIAN_POINT('',(1.15,3.05,2.54)) ;
#102059 = CARTESIAN_POINT('',(-0.900000000000002,3.05,1.58113883008419)) ;
#102060 = CARTESIAN_POINT('Origin',(-1.,3.8,0.)) ;
#102061 = CARTESIAN_POINT('',(-1.,2.1568323274845,0.85)) ;
#102062 = CARTESIAN_POINT('',(-1.,2.95,1.6431676725155)) ;
#102063 = CARTESIAN_POINT('Origin',(-1.,3.8,0.)) ;
#102064 = CARTESIAN_POINT('',(-1.,2.95,2.54)) ;
#102065 = CARTESIAN_POINT('',(-1.,1.6,1.96214168703487)) ;
#102066 = CARTESIAN_POINT('',(-1.,1.6,0.)) ;
#102067 = CARTESIAN_POINT('',(-1.,1.55483870967743,1.83555190077455)) ;
#102068 = CARTESIAN_POINT('Origin',(-1.,1.40000000000001,1.96214168703487)) ;
#102069 = CARTESIAN_POINT('',(-1.,1.02736587339765,0.849999999999999)) ;
#102070 = CARTESIAN_POINT('Origin',(-1.,3.8,0.)) ;
#102071 = CARTESIAN_POINT('',(-1.,2.21886116991581,0.850000000000001)) ;
#102072 = CARTESIAN_POINT('Origin',(-1.,3.8,0.)) ;
#102073 = CARTESIAN_POINT('',(-1.,5.4431676725155,-0.850000000000001)) ;
#102074 = CARTESIAN_POINT('',(-1.,4.65,-1.6431676725155)) ;
#102075 = CARTESIAN_POINT('Origin',(-1.,3.8,0.)) ;
#102076 = CARTESIAN_POINT('',(-1.,4.65,0.)) ;
#102077 = CARTESIAN_POINT('',(-1.,6.45,-0.85)) ;
#102078 = CARTESIAN_POINT('',(-1.,6.45,-0.75)) ;
#102079 = CARTESIAN_POINT('',(-1.,3.8,-0.850000000000001)) ;
#102080 = CARTESIAN_POINT('Origin',(-1.,4.55,-1.58113883008419)) ;
#102081 = CARTESIAN_POINT('',(-0.900000000000001,4.55,-1.6431676725155)) ;
#102082 = CARTESIAN_POINT('',(1.15,4.55,-1.6431676725155)) ;
#102083 = CARTESIAN_POINT('',(1.25,4.55,-1.6431676725155)) ;
#102084 = CARTESIAN_POINT('',(1.15,4.55,-2.54)) ;
#102085 = CARTESIAN_POINT('',(-0.900000000000001,4.55,-1.58113883008419)) ;
#102086 = CARTESIAN_POINT('Origin',(-1.,3.8,0.)) ;
#102087 = CARTESIAN_POINT('',(-0.900000000000001,4.60405405405406,-1.55434779832547)) ;
#102088 = CARTESIAN_POINT('',(-0.900000000000001,5.35434779832547,-0.804054054054054)) ;
#102089 = CARTESIAN_POINT('Origin',(-0.900000000000001,3.8,0.)) ;
#102090 = CARTESIAN_POINT('',(1.15,5.35434779832547,-0.804054054054055)) ;
#102091 = CARTESIAN_POINT('',(-1.,5.35434779832547,-0.804054054054055)) ;
#102092 = CARTESIAN_POINT('',(1.15,4.60405405405405,-1.55434779832547)) ;
#102093 = CARTESIAN_POINT('Origin',(1.15,3.8,0.)) ;
#102094 = CARTESIAN_POINT('',(-1.,4.60405405405406,-1.55434779832547)) ;
#102095 = CARTESIAN_POINT('Origin',(-1.,6.55,-0.75)) ;
#102096 = CARTESIAN_POINT('',(-0.900000000000001,5.4431676725155,-0.75)) ;
#102097 = CARTESIAN_POINT('',(-0.9,6.45,-0.75)) ;
#102098 = CARTESIAN_POINT('',(-0.9,6.55,-0.75)) ;
#102099 = CARTESIAN_POINT('',(1.15,6.45,-0.75)) ;
#102100 = CARTESIAN_POINT('',(-1.,6.45,-0.75)) ;
#102101 = CARTESIAN_POINT('',(1.15,5.4431676725155,-0.75)) ;
#102102 = CARTESIAN_POINT('',(1.15,5.38113883008419,-0.75)) ;
#102103 = CARTESIAN_POINT('',(-1.,5.4431676725155,-0.75)) ;
#102104 = CARTESIAN_POINT('Origin',(-1.,3.8,0.)) ;
#102105 = CARTESIAN_POINT('',(-0.900000000000001,5.35434779832547,0.804054054054056)) ;
#102106 = CARTESIAN_POINT('',(-0.900000000000001,4.60405405405405,1.55434779832547)) ;
#102107 = CARTESIAN_POINT('Origin',(-0.900000000000001,3.8,0.)) ;
#102108 = CARTESIAN_POINT('',(1.15,4.60405405405405,1.55434779832547)) ;
#102109 = CARTESIAN_POINT('',(-1.,4.60405405405405,1.55434779832547)) ;
#102110 = CARTESIAN_POINT('',(1.15,5.35434779832547,0.804054054054056)) ;
#102111 = CARTESIAN_POINT('Origin',(1.15,3.8,0.)) ;
#102112 = CARTESIAN_POINT('',(-1.,5.35434779832547,0.804054054054056)) ;
#102113 = CARTESIAN_POINT('Origin',(-1.,4.55,1.58113883008419)) ;
#102114 = CARTESIAN_POINT('',(1.15,4.55,1.6431676725155)) ;
#102115 = CARTESIAN_POINT('',(1.15,4.55,1.58113883008419)) ;
#102116 = CARTESIAN_POINT('',(-0.900000000000001,4.55,1.6431676725155)) ;
#102117 = CARTESIAN_POINT('',(-1.,4.55,1.6431676725155)) ;
#102118 = CARTESIAN_POINT('',(-0.900000000000001,4.55,2.54)) ;
#102119 = CARTESIAN_POINT('Origin',(-1.,6.55,0.750000000000003)) ;
#102120 = CARTESIAN_POINT('',(1.15,5.4431676725155,0.750000000000002)) ;
#102121 = CARTESIAN_POINT('',(1.15,6.45,0.750000000000003)) ;
#102122 = CARTESIAN_POINT('',(1.15,6.55,0.750000000000003)) ;
#102123 = CARTESIAN_POINT('',(-0.9,6.45,0.750000000000003)) ;
#102124 = CARTESIAN_POINT('',(-1.,6.45,0.750000000000003)) ;
#102125 = CARTESIAN_POINT('',(-0.900000000000001,5.4431676725155,0.750000000000002)) ;
#102126 = CARTESIAN_POINT('',(-0.900000000000001,5.38113883008419,0.750000000000002)) ;
#102127 = CARTESIAN_POINT('',(1.25,5.4431676725155,0.750000000000002)) ;
#102128 = CARTESIAN_POINT('Origin',(-1.,3.8,0.)) ;
#102129 = CARTESIAN_POINT('',(-1.,5.4431676725155,0.850000000000002)) ;
#102130 = CARTESIAN_POINT('',(-1.,6.45,0.850000000000003)) ;
#102131 = CARTESIAN_POINT('',(-1.,6.55,0.850000000000003)) ;
#102132 = CARTESIAN_POINT('',(-1.,6.45,0.)) ;
#102133 = CARTESIAN_POINT('',(-1.,4.65,1.6431676725155)) ;
#102134 = CARTESIAN_POINT('',(-1.,4.65,1.58113883008419)) ;
#102135 = CARTESIAN_POINT('Origin',(-1.,3.8,0.)) ;
#102136 = CARTESIAN_POINT('Origin',(10.,4.35421736843756,-0.875)) ;
#102137 = CARTESIAN_POINT('',(9.91643989873054,7.72792407799439,-0.86107331645509)) ;
#102138 = CARTESIAN_POINT('',(8.58356010126947,8.17221734381475,-0.638926683544911)) ;
#102139 = CARTESIAN_POINT('',(8.47075240319158,8.20981990984071,-0.62012540053193)) ;
#102140 = CARTESIAN_POINT('',(8.58356010126947,6.66256607592813,-0.638926683544911)) ;
#102141 = CARTESIAN_POINT('',(8.58356010126947,6.64863939238321,-0.638926683544911)) ;
#102142 = CARTESIAN_POINT('',(9.91643989873054,6.8847127088383,-0.86107331645509)) ;
#102143 = CARTESIAN_POINT('',(9.98442535909739,6.89604361889945,-0.872404226516232)) ;
#102144 = CARTESIAN_POINT('',(9.91643989873054,7.8,-0.86107331645509)) ;
#102145 = CARTESIAN_POINT('Origin',(8.5,4.35421736843756,-0.625)) ;
#102146 = CARTESIAN_POINT('',(8.5,8.17221734381475,-0.540287291161696)) ;
#102147 = CARTESIAN_POINT('',(8.50000000129681,8.20000000266558,-0.542105625353022)) ;
#102148 = CARTESIAN_POINT('Origin',(8.5,8.17870774541185,-0.729037639375355)) ;
#102149 = CARTESIAN_POINT('',(8.5,8.2,0.583654556300909)) ;
#102150 = CARTESIAN_POINT('',(8.5,6.66256607592813,0.540287291161697)) ;
#102151 = CARTESIAN_POINT('',(8.5,6.64863939238321,0.540287291161696)) ;
#102152 = CARTESIAN_POINT('',(8.50000000002143,6.64999999935441,0.540682155673763)) ;
#102153 = CARTESIAN_POINT('Origin',(8.5,6.65811550095888,0.736811514826147)) ;
#102154 = CARTESIAN_POINT('',(8.49999999999933,6.65000073218972,-0.540689690963651)) ;
#102155 = CARTESIAN_POINT('',(8.5,6.65,-0.723639392383214)) ;
#102156 = CARTESIAN_POINT('',(8.5,6.66256607592813,-0.540287291161696)) ;
#102157 = CARTESIAN_POINT('Origin',(8.5,6.65133313751723,-0.737010066702972)) ;
#102158 = CARTESIAN_POINT('',(8.5,8.20007071090457,-0.540287291161696)) ;
#102159 = CARTESIAN_POINT('Origin',(8.5,4.35421736843756,0.625)) ;
#102160 = CARTESIAN_POINT('',(9.91643989873054,6.8847127088383,0.86107331645509)) ;
#102161 = CARTESIAN_POINT('',(8.58356010126947,6.66256607592813,0.638926683544911)) ;
#102162 = CARTESIAN_POINT('',(8.48442535909739,6.64604361889945,0.622404226516231)) ;
#102163 = CARTESIAN_POINT('',(8.58356010126947,8.20007071090456,0.638926683544911)) ;
#102164 = CARTESIAN_POINT('',(9.91643989873054,7.72792407799439,0.86107331645509)) ;
#102165 = CARTESIAN_POINT('',(9.97075240319158,7.70981990984071,0.87012540053193)) ;
#102166 = CARTESIAN_POINT('',(9.91643989873054,6.8,0.86107331645509)) ;
#102167 = CARTESIAN_POINT('Origin',(8.5,3.65,0.5)) ;
#102168 = CARTESIAN_POINT('',(8.45734623443633,3.62014236410543,0.0979344438426624)) ;
#102169 = CARTESIAN_POINT('',(8.02582401135442,3.3180768079481,0.4)) ;
#102170 = CARTESIAN_POINT('',(8.34729988159781,3.54310991711847,0.174966890829628)) ;
#102171 = CARTESIAN_POINT('',(8.02582401135442,3.31807680794809,-0.4)) ;
#102172 = CARTESIAN_POINT('',(8.02582401135442,3.3180768079481,0.5)) ;
#102173 = CARTESIAN_POINT('',(8.45734623443633,3.62014236410543,-0.0979344438426621)) ;
#102174 = CARTESIAN_POINT('',(8.70083523513316,3.79058466459322,0.0725078566451196)) ;
#102175 = CARTESIAN_POINT('',(8.45734623443633,3.62014236410543,0.5)) ;
#102176 = CARTESIAN_POINT('Origin',(8.5,3.95,0.5)) ;
#102177 = CARTESIAN_POINT('',(8.5,3.89793444384266,-0.0979344438426626)) ;
#102178 = CARTESIAN_POINT('',(8.5,3.89793444384266,0.0979344438426625)) ;
#102179 = CARTESIAN_POINT('',(8.5,3.89793444384266,0.5)) ;
#102180 = CARTESIAN_POINT('',(8.5,3.70206555615734,0.0979344438426625)) ;
#102181 = CARTESIAN_POINT('',(8.5,3.95,0.0979344438426625)) ;
#102182 = CARTESIAN_POINT('',(8.5,3.70206555615734,-0.0979344438426626)) ;
#102183 = CARTESIAN_POINT('',(8.5,3.70206555615734,0.5)) ;
#102184 = CARTESIAN_POINT('',(8.5,3.95,-0.0979344438426626)) ;
#102185 = CARTESIAN_POINT('Origin',(8.,4.3,0.5)) ;
#102186 = CARTESIAN_POINT('',(8.45734623443633,3.97985763589457,-0.0979344438426625)) ;
#102187 = CARTESIAN_POINT('',(8.02582401135442,4.2819231920519,-0.4)) ;
#102188 = CARTESIAN_POINT('',(8.32457260887054,4.07279917379062,-0.190875981738719)) ;
#102189 = CARTESIAN_POINT('',(8.02582401135442,4.2819231920519,0.4)) ;
#102190 = CARTESIAN_POINT('',(8.02582401135442,4.2819231920519,0.5)) ;
#102191 = CARTESIAN_POINT('',(8.45734623443633,3.97985763589457,0.0979344438426624)) ;
#102192 = CARTESIAN_POINT('',(7.97103725533518,4.32027392126537,0.438350729213466)) ;
#102193 = CARTESIAN_POINT('',(8.45734623443633,3.97985763589457,0.5)) ;
#102194 = CARTESIAN_POINT('Origin',(1.5,2.3,0.5)) ;
#102195 = CARTESIAN_POINT('',(7.96847777691809,3.4,0.5)) ;
#102196 = CARTESIAN_POINT('',(8.,3.4,0.5)) ;
#102197 = CARTESIAN_POINT('',(7.96847777691809,4.2,0.5)) ;
#102198 = CARTESIAN_POINT('',(7.96847777691809,4.2,0.5)) ;
#102199 = CARTESIAN_POINT('',(3.,4.2,0.5)) ;
#102200 = CARTESIAN_POINT('Origin',(1.5,2.3,-0.5)) ;
#102201 = CARTESIAN_POINT('',(7.96847777691809,4.2,-0.5)) ;
#102202 = CARTESIAN_POINT('',(1.5,4.2,-0.5)) ;
#102203 = CARTESIAN_POINT('',(7.96847777691809,3.4,-0.5)) ;
#102204 = CARTESIAN_POINT('',(7.96847777691809,2.3,-0.5)) ;
#102205 = CARTESIAN_POINT('',(1.5,3.4,-0.5)) ;
#102206 = CARTESIAN_POINT('Origin',(8.,3.3,0.5)) ;
#102207 = CARTESIAN_POINT('',(7.96847777691809,3.3,-0.4)) ;
#102208 = CARTESIAN_POINT('',(8.,3.3,-0.4)) ;
#102209 = CARTESIAN_POINT('',(7.96847777691809,3.3,0.4)) ;
#102210 = CARTESIAN_POINT('',(7.96847777691809,3.3,0.5)) ;
#102211 = CARTESIAN_POINT('',(3.,3.3,0.4)) ;
#102212 = CARTESIAN_POINT('Origin',(1.5,4.3,0.5)) ;
#102213 = CARTESIAN_POINT('',(7.96847777691809,4.3,0.4)) ;
#102214 = CARTESIAN_POINT('',(8.,4.3,0.4)) ;
#102215 = CARTESIAN_POINT('',(7.96847777691809,4.3,-0.4)) ;
#102216 = CARTESIAN_POINT('',(7.96847777691809,4.3,0.5)) ;
#102217 = CARTESIAN_POINT('',(1.5,4.3,-0.4)) ;
#102218 = CARTESIAN_POINT('Origin',(1.5,2.3,0.5)) ;
#102219 = CARTESIAN_POINT('',(-0.4,2.3,0.5)) ;
#102220 = CARTESIAN_POINT('',(-0.4,-3.36847777691809,0.5)) ;
#102221 = CARTESIAN_POINT('',(-0.4,-3.4,0.5)) ;
#102222 = CARTESIAN_POINT('',(0.4,-3.36847777691809,0.5)) ;
#102223 = CARTESIAN_POINT('',(0.4,-3.36847777691809,0.5)) ;
#102224 = CARTESIAN_POINT('',(0.4,2.29999999999999,0.5)) ;
#102225 = CARTESIAN_POINT('',(0.4,2.29999999999999,0.5)) ;
#102226 = CARTESIAN_POINT('',(0.536602540378444,2.83090991212703,0.5)) ;
#102227 = CARTESIAN_POINT('Origin',(1.5,2.3,0.5)) ;
#102228 = CARTESIAN_POINT('',(0.536602540378444,3.93764017256378,0.5)) ;
#102229 = CARTESIAN_POINT('',(0.536602540378444,2.83090991212703,0.5)) ;
#102230 = CARTESIAN_POINT('Origin',(1.5,2.3,0.5)) ;
#102231 = CARTESIAN_POINT('Origin',(1.5,2.3,-0.5)) ;
#102232 = CARTESIAN_POINT('',(0.4,2.29999999999999,-0.5)) ;
#102233 = CARTESIAN_POINT('',(0.4,-3.36847777691809,-0.5)) ;
#102234 = CARTESIAN_POINT('',(0.4,2.3,-0.5)) ;
#102235 = CARTESIAN_POINT('',(-0.4,-3.36847777691809,-0.5)) ;
#102236 = CARTESIAN_POINT('',(1.5,-3.36847777691809,-0.5)) ;
#102237 = CARTESIAN_POINT('',(-0.4,2.3,-0.5)) ;
#102238 = CARTESIAN_POINT('',(-0.4,2.3,-0.5)) ;
#102239 = CARTESIAN_POINT('',(0.536602540378444,3.93764017256378,-0.5)) ;
#102240 = CARTESIAN_POINT('Origin',(1.5,2.3,-0.5)) ;
#102241 = CARTESIAN_POINT('',(0.536602540378444,2.83090991212703,-0.5)) ;
#102242 = CARTESIAN_POINT('',(0.536602540378444,3.93764017256378,-0.5)) ;
#102243 = CARTESIAN_POINT('Origin',(1.5,2.3,-0.5)) ;
#102244 = CARTESIAN_POINT('Origin',(1.5,2.3,0.5)) ;
#102245 = CARTESIAN_POINT('',(-0.5,2.3,0.4)) ;
#102246 = CARTESIAN_POINT('',(-0.5,2.3,-0.4)) ;
#102247 = CARTESIAN_POINT('',(-0.5,2.3,0.5)) ;
#102248 = CARTESIAN_POINT('Origin',(1.5,2.3,0.4)) ;
#102249 = CARTESIAN_POINT('Origin',(1.5,2.3,-0.4)) ;
#102250 = CARTESIAN_POINT('Origin',(-0.5,-3.4,0.5)) ;
#102251 = CARTESIAN_POINT('',(-0.5,-3.36847777691809,-0.4)) ;
#102252 = CARTESIAN_POINT('',(-0.5,-3.4,-0.4)) ;
#102253 = CARTESIAN_POINT('',(-0.5,-3.36847777691809,0.4)) ;
#102254 = CARTESIAN_POINT('',(-0.5,-3.36847777691809,0.5)) ;
#102255 = CARTESIAN_POINT('',(-0.5,2.3,0.4)) ;
#102256 = CARTESIAN_POINT('Origin',(-0.15,-3.9,0.5)) ;
#102257 = CARTESIAN_POINT('',(-0.179857635894567,-3.85734623443633,0.0979344438426625)) ;
#102258 = CARTESIAN_POINT('',(-0.481923192051905,-3.42582401135442,0.4)) ;
#102259 = CARTESIAN_POINT('',(-0.256890082881532,-3.74729988159781,0.174966890829628)) ;
#102260 = CARTESIAN_POINT('',(-0.481923192051905,-3.42582401135442,-0.4)) ;
#102261 = CARTESIAN_POINT('',(-0.481923192051905,-3.42582401135442,0.5)) ;
#102262 = CARTESIAN_POINT('',(-0.179857635894567,-3.85734623443633,-0.0979344438426628)) ;
#102263 = CARTESIAN_POINT('',(-0.00941533540678435,-4.10083523513317,0.0725078566451196)) ;
#102264 = CARTESIAN_POINT('',(-0.179857635894567,-3.85734623443633,0.5)) ;
#102265 = CARTESIAN_POINT('Origin',(0.15,-3.9,0.5)) ;
#102266 = CARTESIAN_POINT('',(0.0979344438426627,-3.9,-0.0979344438426626)) ;
#102267 = CARTESIAN_POINT('',(0.0979344438426627,-3.9,0.0979344438426627)) ;
#102268 = CARTESIAN_POINT('',(0.0979344438426627,-3.9,0.5)) ;
#102269 = CARTESIAN_POINT('',(-0.0979344438426628,-3.9,0.0979344438426627)) ;
#102270 = CARTESIAN_POINT('',(0.15,-3.9,0.0979344438426627)) ;
#102271 = CARTESIAN_POINT('',(-0.0979344438426628,-3.9,-0.0979344438426626)) ;
#102272 = CARTESIAN_POINT('',(-0.0979344438426628,-3.9,0.5)) ;
#102273 = CARTESIAN_POINT('',(0.15,-3.9,-0.0979344438426626)) ;
#102274 = CARTESIAN_POINT('Origin',(0.5,-3.4,0.5)) ;
#102275 = CARTESIAN_POINT('',(0.179857635894567,-3.85734623443633,-0.0979344438426625)) ;
#102276 = CARTESIAN_POINT('',(0.481923192051904,-3.42582401135442,-0.4)) ;
#102277 = CARTESIAN_POINT('',(0.272799173790623,-3.72457260887054,-0.190875981738719)) ;
#102278 = CARTESIAN_POINT('',(0.481923192051904,-3.42582401135442,0.4)) ;
#102279 = CARTESIAN_POINT('',(0.481923192051904,-3.42582401135442,0.5)) ;
#102280 = CARTESIAN_POINT('',(0.179857635894567,-3.85734623443633,0.0979344438426627)) ;
#102281 = CARTESIAN_POINT('',(0.520273921265371,-3.37103725533519,0.438350729213466)) ;
#102282 = CARTESIAN_POINT('',(0.179857635894567,-3.85734623443633,0.5)) ;
#102283 = CARTESIAN_POINT('Origin',(0.5,2.29999999999999,0.5)) ;
#102284 = CARTESIAN_POINT('',(0.500000000000001,2.29999999999999,0.4)) ;
#102285 = CARTESIAN_POINT('',(0.5,-3.36847777691809,0.4)) ;
#102286 = CARTESIAN_POINT('',(0.5,-3.4,0.4)) ;
#102287 = CARTESIAN_POINT('',(0.5,-3.36847777691809,-0.4)) ;
#102288 = CARTESIAN_POINT('',(0.5,-3.36847777691809,0.5)) ;
#102289 = CARTESIAN_POINT('',(0.500000000000001,2.29999999999999,-0.4)) ;
#102290 = CARTESIAN_POINT('',(0.5,2.29999999999999,-0.4)) ;
#102291 = CARTESIAN_POINT('',(0.500000000000001,2.29999999999999,0.5)) ;
#102292 = CARTESIAN_POINT('Origin',(1.5,2.3,0.5)) ;
#102293 = CARTESIAN_POINT('Origin',(1.5,2.3,0.4)) ;
#102294 = CARTESIAN_POINT('Origin',(1.5,2.3,-0.4)) ;
#102295 = CARTESIAN_POINT('Origin',(8.,2.68967221921331,-0.5)) ;
#102296 = CARTESIAN_POINT('',(8.45734623443633,3.70206555615734,-0.179857635894567)) ;
#102297 = CARTESIAN_POINT('',(8.02582401135442,3.4,-0.481923192051904)) ;
#102298 = CARTESIAN_POINT('',(7.75526480758232,3.21060855735952,-0.671314634692378)) ;
#102299 = CARTESIAN_POINT('',(8.02582401135442,4.2,-0.481923192051904)) ;
#102300 = CARTESIAN_POINT('',(8.02582401135442,2.68967221921331,-0.481923192051904)) ;
#102301 = CARTESIAN_POINT('',(8.45734623443633,3.89793444384266,-0.179857635894567)) ;
#102302 = CARTESIAN_POINT('',(8.54034505662341,3.83983526831171,-0.121758460363615)) ;
#102303 = CARTESIAN_POINT('',(8.45734623443633,2.68967221921331,-0.179857635894566)) ;
#102304 = CARTESIAN_POINT('Origin',(8.,2.68967221921331,0.5)) ;
#102305 = CARTESIAN_POINT('',(8.45734623443633,3.89793444384266,0.179857635894567)) ;
#102306 = CARTESIAN_POINT('',(8.02582401135442,4.2,0.481923192051904)) ;
#102307 = CARTESIAN_POINT('',(8.54034505662341,3.83983526831171,0.121758460363615)) ;
#102308 = CARTESIAN_POINT('',(8.02582401135442,3.4,0.481923192051904)) ;
#102309 = CARTESIAN_POINT('',(8.02582401135442,3.4,0.481923192051904)) ;
#102310 = CARTESIAN_POINT('',(8.45734623443633,3.70206555615734,0.179857635894567)) ;
#102311 = CARTESIAN_POINT('',(7.75526480758232,3.21060855735952,0.671314634692378)) ;
#102312 = CARTESIAN_POINT('',(8.45734623443633,2.68967221921331,0.179857635894566)) ;
#102313 = CARTESIAN_POINT('Origin',(-1.11032778078669,-3.9,0.15)) ;
#102314 = CARTESIAN_POINT('',(0.0979344438426626,-3.85734623443633,0.179857635894567)) ;
#102315 = CARTESIAN_POINT('',(0.4,-3.42582401135442,0.481923192051904)) ;
#102316 = CARTESIAN_POINT('',(-0.223548570072128,-4.31660768288603,-0.141625378020224)) ;
#102317 = CARTESIAN_POINT('',(-0.400000000000001,-3.42582401135442,0.481923192051904)) ;
#102318 = CARTESIAN_POINT('',(-0.400000000000001,-3.42582401135442,0.481923192051904)) ;
#102319 = CARTESIAN_POINT('',(-0.0979344438426627,-3.85734623443633,0.179857635894567)) ;
#102320 = CARTESIAN_POINT('',(-0.326007604256636,-3.53152743384494,0.40793079630854)) ;
#102321 = CARTESIAN_POINT('',(-1.11032778078669,-3.85734623443633,0.179857635894567)) ;
#102322 = CARTESIAN_POINT('Origin',(-1.11032778078669,-3.4,-0.5)) ;
#102323 = CARTESIAN_POINT('',(-0.0979344438426627,-3.85734623443633,-0.179857635894567)) ;
#102324 = CARTESIAN_POINT('',(-0.4,-3.42582401135442,-0.481923192051904)) ;
#102325 = CARTESIAN_POINT('',(-0.589391442640475,-3.15526480758232,-0.671314634692378)) ;
#102326 = CARTESIAN_POINT('',(0.400000000000001,-3.42582401135442,-0.481923192051904)) ;
#102327 = CARTESIAN_POINT('',(-1.11032778078669,-3.42582401135442,-0.481923192051904)) ;
#102328 = CARTESIAN_POINT('',(0.0979344438426626,-3.85734623443633,-0.179857635894567)) ;
#102329 = CARTESIAN_POINT('',(0.0398352683117103,-3.94034505662341,-0.121758460363614)) ;
#102330 = CARTESIAN_POINT('',(-1.11032778078669,-3.85734623443633,-0.179857635894567)) ;
#102331 = CARTESIAN_POINT('Origin',(10.,1.24999999999998,-2.54)) ;
#102332 = CARTESIAN_POINT('',(9.91643989873054,1.26392668354489,2.0441618801782)) ;
#102333 = CARTESIAN_POINT('',(9.91643989873054,1.26392668354489,-2.54)) ;
#102334 = CARTESIAN_POINT('',(8.50816364570057,1.49863939238321,1.96214168703487)) ;
#102335 = CARTESIAN_POINT('Origin',(43.7052916412087,-4.36754860759459,-606.688201691247)) ;
#102336 = CARTESIAN_POINT('',(8.50816364570057,1.49863939238321,-2.54)) ;
#102337 = CARTESIAN_POINT('Origin',(8.49999999999985,3.8,0.)) ;
#102338 = CARTESIAN_POINT('',(9.91643989873053,1.24322097942674,1.98369643580595)) ;
#102339 = CARTESIAN_POINT('',(9.91643989873053,1.24322097942648,-1.98369643580562)) ;
#102340 = CARTESIAN_POINT('Origin',(9.91643989873053,3.8,0.)) ;
#102341 = CARTESIAN_POINT('Origin',(36.5480652843801,-40.3802619076193,572.277654833716)) ;
#102342 = CARTESIAN_POINT('Origin',(36.548065291501,-40.3802618709639,-572.277654846232)) ;
#102343 = CARTESIAN_POINT('Origin',(10.,1.24999999999998,-2.54)) ;
#102344 = CARTESIAN_POINT('',(8.50816364570059,1.49863939238321,-1.96214168703472)) ;
#102345 = CARTESIAN_POINT('',(8.50816364570057,1.49863939238321,-2.54)) ;
#102346 = CARTESIAN_POINT('',(9.91643989873054,1.26392668354489,-2.04416188017819)) ;
#102347 = CARTESIAN_POINT('Origin',(43.7052916405325,-4.36754860730519,606.688201680236)) ;
#102348 = CARTESIAN_POINT('',(9.91643989873054,1.26392668354489,-2.54)) ;
#102349 = CARTESIAN_POINT('Origin',(-0.900000000000001,4.65,0.)) ;
#102350 = CARTESIAN_POINT('Origin',(-0.900000000000001,4.65,1.6431676725155)) ;
#102351 = CARTESIAN_POINT('Origin',(-0.900000000000001,4.65,1.6431676725155)) ;
#102352 = CARTESIAN_POINT('Origin',(-0.900000000000001,4.65,1.6431676725155)) ;
#102353 = CARTESIAN_POINT('Origin',(-0.900000000000001,4.65,1.6431676725155)) ;
#102354 = CARTESIAN_POINT('Origin',(1.15,4.45,1.58113883008419)) ;
#102355 = CARTESIAN_POINT('Origin',(1.15,4.45,1.6431676725155)) ;
#102356 = CARTESIAN_POINT('Origin',(-1.,4.65,1.6431676725155)) ;
#102357 = CARTESIAN_POINT('Origin',(1.15,4.65,1.6431676725155)) ;
#102358 = CARTESIAN_POINT('Origin',(-0.900000000000001,3.8,0.)) ;
#102359 = CARTESIAN_POINT('Origin',(-0.900000000000001,5.4431676725155,0.850000000000002)) ;
#102360 = CARTESIAN_POINT('Origin',(1.15,4.65,1.6431676725155)) ;
#102361 = CARTESIAN_POINT('Origin',(1.15,4.55810810810811,1.46552792413544)) ;
#102362 = CARTESIAN_POINT('Origin',(-0.900000000000001,5.4431676725155,0.850000000000002)) ;
#102363 = CARTESIAN_POINT('Origin',(-0.900000000000001,5.4431676725155,0.850000000000002)) ;
#102364 = CARTESIAN_POINT('Origin',(-0.900000000000001,5.4431676725155,0.850000000000002)) ;
#102365 = CARTESIAN_POINT('Origin',(-0.900000000000001,4.65,0.)) ;
#102366 = CARTESIAN_POINT('Origin',(-0.900000000000001,4.65,-1.6431676725155)) ;
#102367 = CARTESIAN_POINT('Origin',(-1.,4.65,-1.6431676725155)) ;
#102368 = CARTESIAN_POINT('Origin',(1.15,4.65,-1.6431676725155)) ;
#102369 = CARTESIAN_POINT('Origin',(-0.900000000000001,4.65,-1.6431676725155)) ;
#102370 = CARTESIAN_POINT('Origin',(1.15,4.45,-1.58113883008419)) ;
#102371 = CARTESIAN_POINT('Origin',(1.15,4.45,-1.6431676725155)) ;
#102372 = CARTESIAN_POINT('Origin',(1.15,3.8,0.)) ;
#102373 = CARTESIAN_POINT('Origin',(1.15,5.26552792413544,0.75810810810811)) ;
#102374 = CARTESIAN_POINT('Origin',(-1.,5.4431676725155,0.850000000000002)) ;
#102375 = CARTESIAN_POINT('Origin',(1.15,5.4431676725155,0.850000000000002)) ;
#102376 = CARTESIAN_POINT('Origin',(-0.900000000000001,3.8,0.850000000000001)) ;
#102377 = CARTESIAN_POINT('Origin',(-0.9,6.45,0.850000000000003)) ;
#102378 = CARTESIAN_POINT('Origin',(-0.9,6.45,0.)) ;
#102379 = CARTESIAN_POINT('Origin',(-0.9,6.45,0.850000000000003)) ;
#102380 = CARTESIAN_POINT('Origin',(-0.900000000000001,4.65,-1.6431676725155)) ;
#102381 = CARTESIAN_POINT('Origin',(-0.900000000000001,4.65,-1.6431676725155)) ;
#102382 = CARTESIAN_POINT('Origin',(1.15,4.65,-1.6431676725155)) ;
#102383 = CARTESIAN_POINT('Origin',(1.15,4.55810810810811,-1.46552792413544)) ;
#102384 = CARTESIAN_POINT('Origin',(1.15,5.4431676725155,0.850000000000002)) ;
#102385 = CARTESIAN_POINT('Origin',(1.15,5.4431676725155,0.650000000000002)) ;
#102386 = CARTESIAN_POINT('Origin',(-0.9,6.45,0.850000000000003)) ;
#102387 = CARTESIAN_POINT('Origin',(-0.9,6.45,0.850000000000003)) ;
#102388 = CARTESIAN_POINT('Origin',(-0.900000000000001,3.8,0.)) ;
#102389 = CARTESIAN_POINT('Origin',(-0.900000000000001,5.4431676725155,-0.850000000000001)) ;
#102390 = CARTESIAN_POINT('Origin',(-1.,5.4431676725155,-0.850000000000001)) ;
#102391 = CARTESIAN_POINT('Origin',(1.15,5.4431676725155,-0.850000000000001)) ;
#102392 = CARTESIAN_POINT('Origin',(-0.900000000000001,5.4431676725155,-0.850000000000001)) ;
#102393 = CARTESIAN_POINT('Origin',(1.15,3.8,0.)) ;
#102394 = CARTESIAN_POINT('Origin',(1.15,5.26552792413544,-0.758108108108109)) ;
#102395 = CARTESIAN_POINT('Origin',(1.15,6.55,0.650000000000003)) ;
#102396 = CARTESIAN_POINT('Origin',(1.15,6.45,0.650000000000003)) ;
#102397 = CARTESIAN_POINT('Origin',(1.25,6.45,0.850000000000003)) ;
#102398 = CARTESIAN_POINT('Origin',(1.15,6.45,0.850000000000003)) ;
#102399 = CARTESIAN_POINT('Origin',(-0.900000000000001,5.4431676725155,-0.850000000000001)) ;
#102400 = CARTESIAN_POINT('Origin',(-0.900000000000001,5.4431676725155,-0.850000000000001)) ;
#102401 = CARTESIAN_POINT('Origin',(1.15,5.4431676725155,-0.850000000000001)) ;
#102402 = CARTESIAN_POINT('Origin',(1.15,5.4431676725155,-0.65)) ;
#102403 = CARTESIAN_POINT('Origin',(1.15,6.45,0.650000000000003)) ;
#102404 = CARTESIAN_POINT('Origin',(1.35,6.45,0.650000000000003)) ;
#102405 = CARTESIAN_POINT('Origin',(-0.9,6.45,0.)) ;
#102406 = CARTESIAN_POINT('Origin',(-0.9,6.45,-0.85)) ;
#102407 = CARTESIAN_POINT('Origin',(-0.900000000000001,3.8,-0.850000000000001)) ;
#102408 = CARTESIAN_POINT('Origin',(-0.9,6.45,-0.85)) ;
#102409 = CARTESIAN_POINT('Origin',(1.15,6.55,-0.65)) ;
#102410 = CARTESIAN_POINT('Origin',(1.15,6.45,-0.65)) ;
#102411 = CARTESIAN_POINT('Origin',(1.35,6.45,-2.54)) ;
#102412 = CARTESIAN_POINT('Origin',(1.35,6.45,-0.65)) ;
#102413 = CARTESIAN_POINT('Origin',(-0.9,6.45,-0.85)) ;
#102414 = CARTESIAN_POINT('Origin',(-0.9,6.45,-0.85)) ;
#102415 = CARTESIAN_POINT('Origin',(1.15,6.45,-0.65)) ;
#102416 = CARTESIAN_POINT('Origin',(1.15,6.45,-0.85)) ;
#102417 = CARTESIAN_POINT('Origin',(-1.,6.45,-0.85)) ;
#102418 = CARTESIAN_POINT('Origin',(-1.7,0.3,-0.65)) ;
#102419 = CARTESIAN_POINT('Origin',(-1.7,0.3,-0.65)) ;
#102420 = CARTESIAN_POINT('Origin',(-1.7,0.3,-0.65)) ;
#102421 = CARTESIAN_POINT('Origin',(-1.7,0.3,-0.65)) ;
#102422 = CARTESIAN_POINT('Origin',(0.549999999999999,0.3,-0.65)) ;
#102423 = CARTESIAN_POINT('',(0.50857864376269,0.229289321881345,-0.579289321881346)) ;
#102424 = CARTESIAN_POINT('Ctrl Pts',(0.65,0.2,-0.650000000000001)) ;
#102425 = CARTESIAN_POINT('Ctrl Pts',(0.639834283464162,0.2,-0.644917141732082)) ;
#102426 = CARTESIAN_POINT('Ctrl Pts',(0.629316849080556,0.200389688120422,
-0.639657683858013)) ;
#102427 = CARTESIAN_POINT('Ctrl Pts',(0.606957334719702,0.202165884217644,
-0.628467949719354)) ;
#102428 = CARTESIAN_POINT('Ctrl Pts',(0.595086727401132,0.203647820493439,
-0.622522761794938)) ;
#102429 = CARTESIAN_POINT('Ctrl Pts',(0.572283837380418,0.207685608831266,
-0.611106760395993)) ;
#102430 = CARTESIAN_POINT('Ctrl Pts',(0.561337481650347,0.210178193248346,
-0.605629861308006)) ;
#102431 = CARTESIAN_POINT('Ctrl Pts',(0.549549942885282,0.213544620665578,
-0.599740696039287)) ;
#102432 = CARTESIAN_POINT('Ctrl Pts',(0.548290718945597,0.213913346522004,
-0.599111682766023)) ;
#102433 = CARTESIAN_POINT('Ctrl Pts',(0.536119229732665,0.217566912232542,
-0.593032751351762)) ;
#102434 = CARTESIAN_POINT('Ctrl Pts',(0.525706917362415,0.221400308602604,
-0.587842238429113)) ;
#102435 = CARTESIAN_POINT('Ctrl Pts',(0.51354511002719,0.226871185484683,
-0.5817711869643)) ;
#102436 = CARTESIAN_POINT('Ctrl Pts',(0.511029334128286,0.228063976698547,
-0.580514667064143)) ;
#102437 = CARTESIAN_POINT('Ctrl Pts',(0.50857864376269,0.229289321881345,
-0.579289321881346)) ;
#102438 = CARTESIAN_POINT('Origin',(0.664280054304529,0.302990743362704,-0.657142104251322)) ;
#102439 = CARTESIAN_POINT('Origin',(-1.7,4.5,-0.65)) ;
#102440 = CARTESIAN_POINT('',(-1.77071067811866,4.45857864376269,-0.579289321881345)) ;
#102441 = CARTESIAN_POINT('Origin',(-1.69703459697416,4.61417009505667,-0.657086685382634)) ;
#102442 = CARTESIAN_POINT('Ctrl Pts',(-1.77071067811866,4.45857864376269,
-0.579289321881348)) ;
#102443 = CARTESIAN_POINT('Ctrl Pts',(-1.77521675558368,4.46759079869274,
-0.583795399346371)) ;
#102444 = CARTESIAN_POINT('Ctrl Pts',(-1.77928079264423,4.47748625817287,
-0.588726481671654)) ;
#102445 = CARTESIAN_POINT('Ctrl Pts',(-1.78624680748625,4.49811277056867,
-0.599020882547782)) ;
#102446 = CARTESIAN_POINT('Ctrl Pts',(-1.7891803078179,4.50880509433462,-0.604363984149067)) ;
#102447 = CARTESIAN_POINT('Ctrl Pts',(-1.7918598550029,4.52101859322019,-0.610474754532795)) ;
#102448 = CARTESIAN_POINT('Ctrl Pts',(-1.79213045061227,4.52228751722695,
-0.611109709908939)) ;
#102449 = CARTESIAN_POINT('Ctrl Pts',(-1.7947746790983,4.53504937002861,-0.617496289133973)) ;
#102450 = CARTESIAN_POINT('Ctrl Pts',(-1.79657370273654,4.54677936428205,
-0.623371572406224)) ;
#102451 = CARTESIAN_POINT('Ctrl Pts',(-1.79896007643137,4.569200258884,-0.634595774761239)) ;
#102452 = CARTESIAN_POINT('Ctrl Pts',(-1.79963010255188,4.57990192168164,
-0.639950075945062)) ;
#102453 = CARTESIAN_POINT('Ctrl Pts',(-1.79996164986963,4.59357116034304,
-0.646785573817069)) ;
#102454 = CARTESIAN_POINT('Ctrl Pts',(-1.8,4.59680282631918,-0.648401413159594)) ;
#102455 = CARTESIAN_POINT('Ctrl Pts',(-1.8,4.6,-0.65)) ;
#102456 = CARTESIAN_POINT('Origin',(-1.7,0.3,-1.5225450639222E-32)) ;
#102457 = CARTESIAN_POINT('Origin',(-1.7,0.3,-1.4)) ;
#102458 = CARTESIAN_POINT('Origin',(0.65,0.3,1.72609413621187E-32)) ;
#102459 = CARTESIAN_POINT('',(0.579289321881342,0.229289321881349,-0.508578643762698)) ;
#102460 = CARTESIAN_POINT('Origin',(0.657086685384304,0.30296540302664,-0.664170095060029)) ;
#102461 = CARTESIAN_POINT('Ctrl Pts',(0.579289321881342,0.229289321881349,
-0.508578643762698)) ;
#102462 = CARTESIAN_POINT('Ctrl Pts',(0.583795399346366,0.224783244416324,
-0.517590798692747)) ;
#102463 = CARTESIAN_POINT('Ctrl Pts',(0.588726481671643,0.220719207355776,
-0.527486258172869)) ;
#102464 = CARTESIAN_POINT('Ctrl Pts',(0.599020882547802,0.213753192513734,
-0.548112770568737)) ;
#102465 = CARTESIAN_POINT('Ctrl Pts',(0.604363984149125,0.210819692182067,
-0.558805094334768)) ;
#102466 = CARTESIAN_POINT('Ctrl Pts',(0.610474754532853,0.208140144997073,
-0.571018593220337)) ;
#102467 = CARTESIAN_POINT('Ctrl Pts',(0.611109709908958,0.207869549387722,
-0.572287517227017)) ;
#102468 = CARTESIAN_POINT('Ctrl Pts',(0.617496289133948,0.205225320901705,
-0.585049370028594)) ;
#102469 = CARTESIAN_POINT('Ctrl Pts',(0.623371572406196,0.20342629726347,
-0.596779364282033)) ;
#102470 = CARTESIAN_POINT('Ctrl Pts',(0.634595774761209,0.201039923568639,
-0.619200258883972)) ;
#102471 = CARTESIAN_POINT('Ctrl Pts',(0.639950075945033,0.20036989744812,
-0.629901921681599)) ;
#102472 = CARTESIAN_POINT('Ctrl Pts',(0.646785573817052,0.200038350130375,
-0.643571160343016)) ;
#102473 = CARTESIAN_POINT('Ctrl Pts',(0.648401413159585,0.2,-0.646802826319172)) ;
#102474 = CARTESIAN_POINT('Ctrl Pts',(0.65,0.2,-0.65)) ;
#102475 = CARTESIAN_POINT('',(0.579289321881342,0.229289321881349,0.508578643762698)) ;
#102476 = CARTESIAN_POINT('Ctrl Pts',(0.65,0.2,0.650000000000001)) ;
#102477 = CARTESIAN_POINT('Ctrl Pts',(0.644917141732077,0.2,0.639834283464156)) ;
#102478 = CARTESIAN_POINT('Ctrl Pts',(0.639657683858002,0.200389688120423,
0.629316849080544)) ;
#102479 = CARTESIAN_POINT('Ctrl Pts',(0.62846794971934,0.202165884217647,
0.606957334719689)) ;
#102480 = CARTESIAN_POINT('Ctrl Pts',(0.622522761794926,0.203647820493443,
0.595086727401124)) ;
#102481 = CARTESIAN_POINT('Ctrl Pts',(0.611106760395994,0.207685608831266,
0.572283837380437)) ;
#102482 = CARTESIAN_POINT('Ctrl Pts',(0.605629861308018,0.210178193248342,
0.561337481650389)) ;
#102483 = CARTESIAN_POINT('Ctrl Pts',(0.599740696039299,0.213544620665571,
0.549549942885324)) ;
#102484 = CARTESIAN_POINT('Ctrl Pts',(0.599111682766026,0.213913346522003,
0.54829071894562)) ;
#102485 = CARTESIAN_POINT('Ctrl Pts',(0.593032751351754,0.217566912232547,
0.536119229732666)) ;
#102486 = CARTESIAN_POINT('Ctrl Pts',(0.587842238429105,0.22140030860261,
0.525706917362413)) ;
#102487 = CARTESIAN_POINT('Ctrl Pts',(0.581771186964293,0.22687118548469,
0.51354511002719)) ;
#102488 = CARTESIAN_POINT('Ctrl Pts',(0.580514667064138,0.228063976698553,
0.51102933412829)) ;
#102489 = CARTESIAN_POINT('Ctrl Pts',(0.579289321881342,0.229289321881349,
0.508578643762698)) ;
#102490 = CARTESIAN_POINT('Origin',(0.657142104251401,0.302990743362705,0.664280054304728)) ;
#102491 = CARTESIAN_POINT('Origin',(-1.7,4.6,-0.549999999999999)) ;
#102492 = CARTESIAN_POINT('',(-1.77071067811866,4.52928932188135,-0.508578643762691)) ;
#102493 = CARTESIAN_POINT('Ctrl Pts',(-1.8,4.6,-0.65)) ;
#102494 = CARTESIAN_POINT('Ctrl Pts',(-1.8,4.59491714173209,-0.639834283464162)) ;
#102495 = CARTESIAN_POINT('Ctrl Pts',(-1.79961031187958,4.58965768385802,
-0.629316849080557)) ;
#102496 = CARTESIAN_POINT('Ctrl Pts',(-1.79783411578236,4.57846794971937,
-0.606957334719712)) ;
#102497 = CARTESIAN_POINT('Ctrl Pts',(-1.79635217950657,4.57252276179496,
-0.595086727401151)) ;
#102498 = CARTESIAN_POINT('Ctrl Pts',(-1.7923143911687,4.56110676039589,-0.57228383738021)) ;
#102499 = CARTESIAN_POINT('Ctrl Pts',(-1.78982180675156,4.55562986130779,
-0.561337481649912)) ;
#102500 = CARTESIAN_POINT('Ctrl Pts',(-1.7864553793343,4.54974069603908,-0.549549942884871)) ;
#102501 = CARTESIAN_POINT('Ctrl Pts',(-1.78608665347794,4.54911168276593,
-0.548290718945413)) ;
#102502 = CARTESIAN_POINT('Ctrl Pts',(-1.78243308776747,4.54303275135178,
-0.536119229732704)) ;
#102503 = CARTESIAN_POINT('Ctrl Pts',(-1.77859969139741,4.53784223842913,
-0.525706917362452)) ;
#102504 = CARTESIAN_POINT('Ctrl Pts',(-1.77312881451533,4.53177118696431,
-0.513545110027213)) ;
#102505 = CARTESIAN_POINT('Ctrl Pts',(-1.77193602330146,4.53051466706415,
-0.511029334128298)) ;
#102506 = CARTESIAN_POINT('Ctrl Pts',(-1.77071067811866,4.52928932188135,
-0.508578643762691)) ;
#102507 = CARTESIAN_POINT('Origin',(-1.69700925663759,4.60714210425063,-0.664280054303076)) ;
#102508 = CARTESIAN_POINT('',(-1.77071067811866,4.52928932188135,0.508578643762691)) ;
#102509 = CARTESIAN_POINT('Origin',(-1.69703459697298,4.60708668538534,0.664170095062018)) ;
#102510 = CARTESIAN_POINT('Ctrl Pts',(-1.77071067811866,4.52928932188135,
0.508578643762691)) ;
#102511 = CARTESIAN_POINT('Ctrl Pts',(-1.77521675558368,4.53379539934637,
0.517590798692744)) ;
#102512 = CARTESIAN_POINT('Ctrl Pts',(-1.77928079264423,4.53872648167165,
0.52748625817287)) ;
#102513 = CARTESIAN_POINT('Ctrl Pts',(-1.78624680748627,4.54902088254781,
0.548112770568734)) ;
#102514 = CARTESIAN_POINT('Ctrl Pts',(-1.78918030781794,4.55436398414913,
0.558805094334758)) ;
#102515 = CARTESIAN_POINT('Ctrl Pts',(-1.79185985500293,4.56047475453286,
0.571018593220325)) ;
#102516 = CARTESIAN_POINT('Ctrl Pts',(-1.79213045061228,4.56110970990897,
0.572287517227011)) ;
#102517 = CARTESIAN_POINT('Ctrl Pts',(-1.7947746790983,4.56749628913396,0.585049370028587)) ;
#102518 = CARTESIAN_POINT('Ctrl Pts',(-1.79657370273653,4.5733715724062,0.596779364282017)) ;
#102519 = CARTESIAN_POINT('Ctrl Pts',(-1.79896007643136,4.58459577476122,
0.619200258883955)) ;
#102520 = CARTESIAN_POINT('Ctrl Pts',(-1.79963010255188,4.58995007594504,
0.629901921681588)) ;
#102521 = CARTESIAN_POINT('Ctrl Pts',(-1.79996164986962,4.59678557381705,
0.643571160343013)) ;
#102522 = CARTESIAN_POINT('Ctrl Pts',(-1.8,4.59840141315959,0.64680282631917)) ;
#102523 = CARTESIAN_POINT('Ctrl Pts',(-1.8,4.6,0.65)) ;
#102524 = CARTESIAN_POINT('Origin',(-1.7,0.3,-1.4)) ;
#102525 = CARTESIAN_POINT('Origin',(-1.7,0.1,-1.4)) ;
#102526 = CARTESIAN_POINT('Origin',(-1.9,0.3,-1.4)) ;
#102527 = CARTESIAN_POINT('Origin',(1.9668402209837E-32,0.1,-1.4)) ;
#102528 = CARTESIAN_POINT('',(0.899999999999999,0.1,-1.5)) ;
#102529 = CARTESIAN_POINT('',(-1.8,0.1,-1.5)) ;
#102530 = CARTESIAN_POINT('Origin',(0.899999999999999,0.1,-1.4)) ;
#102531 = CARTESIAN_POINT('Origin',(0.899999999999999,0.1,-1.4)) ;
#102532 = CARTESIAN_POINT('',(0.999999999999999,0.1,-1.4)) ;
#102533 = CARTESIAN_POINT('Origin',(0.899999999999999,0.1,-1.4)) ;
#102534 = CARTESIAN_POINT('Origin',(0.899999999999999,0.1,-1.4)) ;
#102535 = CARTESIAN_POINT('Origin',(0.549999999999999,0.3,0.650000000000001)) ;
#102536 = CARTESIAN_POINT('',(0.50857864376269,0.229289321881345,0.579289321881346)) ;
#102537 = CARTESIAN_POINT('Origin',(0.664170095060202,0.302965403026731,0.657086685384413)) ;
#102538 = CARTESIAN_POINT('Ctrl Pts',(0.50857864376269,0.229289321881345,
0.579289321881346)) ;
#102539 = CARTESIAN_POINT('Ctrl Pts',(0.51759079869273,0.224783244416326,
0.583795399346365)) ;
#102540 = CARTESIAN_POINT('Ctrl Pts',(0.527486258172839,0.220719207355783,
0.588726481671636)) ;
#102541 = CARTESIAN_POINT('Ctrl Pts',(0.54811277056867,0.213753192513749,
0.599020882547779)) ;
#102542 = CARTESIAN_POINT('Ctrl Pts',(0.558805094334679,0.210819692182086,
0.60436398414909)) ;
#102543 = CARTESIAN_POINT('Ctrl Pts',(0.571018593220245,0.208140144997089,
0.610474754532817)) ;
#102544 = CARTESIAN_POINT('Ctrl Pts',(0.572287517226946,0.207869549387733,
0.611109709908932)) ;
#102545 = CARTESIAN_POINT('Ctrl Pts',(0.58504937002854,0.205225320901711,
0.617496289133931)) ;
#102546 = CARTESIAN_POINT('Ctrl Pts',(0.596779364281974,0.203426297263476,
0.623371572406175)) ;
#102547 = CARTESIAN_POINT('Ctrl Pts',(0.61920025888392,0.201039923568642,
0.634595774761189)) ;
#102548 = CARTESIAN_POINT('Ctrl Pts',(0.629901921681556,0.200369897448122,
0.639950075945017)) ;
#102549 = CARTESIAN_POINT('Ctrl Pts',(0.643571160342994,0.200038350130376,
0.646785573817043)) ;
#102550 = CARTESIAN_POINT('Ctrl Pts',(0.646802826319161,0.2,0.648401413159581)) ;
#102551 = CARTESIAN_POINT('Ctrl Pts',(0.65,0.2,0.650000000000001)) ;
#102552 = CARTESIAN_POINT('Origin',(-1.7,0.3,0.650000000000001)) ;
#102553 = CARTESIAN_POINT('Origin',(-1.7,4.5,0.65)) ;
#102554 = CARTESIAN_POINT('',(-1.77071067811866,4.45857864376269,0.579289321881346)) ;
#102555 = CARTESIAN_POINT('Ctrl Pts',(-1.8,4.6,0.65)) ;
#102556 = CARTESIAN_POINT('Ctrl Pts',(-1.8,4.58983428346415,0.644917141732085)) ;
#102557 = CARTESIAN_POINT('Ctrl Pts',(-1.79961031187958,4.57931684908054,
0.639657683858016)) ;
#102558 = CARTESIAN_POINT('Ctrl Pts',(-1.79783411578236,4.55695733471967,
0.628467949719358)) ;
#102559 = CARTESIAN_POINT('Ctrl Pts',(-1.79635217950656,4.5450867274011,0.622522761794939)) ;
#102560 = CARTESIAN_POINT('Ctrl Pts',(-1.79231439116879,4.5222838373807,0.611106760396153)) ;
#102561 = CARTESIAN_POINT('Ctrl Pts',(-1.7898218067518,4.51133748165095,0.605629861308319)) ;
#102562 = CARTESIAN_POINT('Ctrl Pts',(-1.7864553793346,4.49954994288585,0.599740696039583)) ;
#102563 = CARTESIAN_POINT('Ctrl Pts',(-1.78608665347808,4.49829071894586,
0.599111682766165)) ;
#102564 = CARTESIAN_POINT('Ctrl Pts',(-1.78243308776745,4.48611922973263,
0.593032751351754)) ;
#102565 = CARTESIAN_POINT('Ctrl Pts',(-1.77859969139739,4.47570691736239,
0.587842238429103)) ;
#102566 = CARTESIAN_POINT('Ctrl Pts',(-1.77312881451531,4.46354511002718,
0.581771186964297)) ;
#102567 = CARTESIAN_POINT('Ctrl Pts',(-1.77193602330145,4.46102933412828,
0.580514667064141)) ;
#102568 = CARTESIAN_POINT('Ctrl Pts',(-1.77071067811866,4.45857864376269,
0.579289321881348)) ;
#102569 = CARTESIAN_POINT('Origin',(-1.6970092566387,4.61428005429881,0.657142104248473)) ;
#102570 = CARTESIAN_POINT('Origin',(-1.7,0.3,0.650000000000001)) ;
#102571 = CARTESIAN_POINT('Origin',(-1.9,-4.11004745125224E-16,-1.4)) ;
#102572 = CARTESIAN_POINT('',(-1.9,6.9,-1.5)) ;
#102573 = CARTESIAN_POINT('Origin',(-1.9,6.9,-1.4)) ;
#102574 = CARTESIAN_POINT('',(-1.9,7.,-1.5)) ;
#102575 = CARTESIAN_POINT('Origin',(-2.,0.1,-1.6)) ;
#102576 = CARTESIAN_POINT('Origin',(-1.89999999999999,0.100000000000007,-1.6)) ;
#102577 = CARTESIAN_POINT('Origin',(0.899999999999999,0.1,-1.6)) ;
#102578 = CARTESIAN_POINT('Origin',(0.899999999999999,0.1,-1.4)) ;
#102579 = CARTESIAN_POINT('Origin',(1.1,0.1,-1.4)) ;
#102580 = CARTESIAN_POINT('Origin',(0.899999999999999,0.1,6.50521303491302E-17)) ;
#102581 = CARTESIAN_POINT('',(0.999999999999999,0.1,1.4)) ;
#102582 = CARTESIAN_POINT('',(0.999999999999999,0.1,-1.5)) ;
#102583 = CARTESIAN_POINT('Origin',(0.899999999999999,0.1,1.4)) ;
#102584 = CARTESIAN_POINT('Origin',(-1.7,0.3,0.650000000000001)) ;
#102585 = CARTESIAN_POINT('Origin',(-1.7,0.3,0.650000000000001)) ;
#102586 = CARTESIAN_POINT('Origin',(-1.9,6.9,-1.4)) ;
#102587 = CARTESIAN_POINT('',(-1.9,7.,-1.4)) ;
#102588 = CARTESIAN_POINT('Origin',(-1.9,6.9,-1.4)) ;
#102589 = CARTESIAN_POINT('Origin',(-1.9,6.9,-1.4)) ;
#102590 = CARTESIAN_POINT('Origin',(-1.9,7.,-1.6)) ;
#102591 = CARTESIAN_POINT('Origin',(-1.9,6.9,-1.6)) ;
#102592 = CARTESIAN_POINT('Origin',(1.1,0.1,1.5)) ;
#102593 = CARTESIAN_POINT('Origin',(1.1,0.1,1.4)) ;
#102594 = CARTESIAN_POINT('Origin',(0.899999999999999,0.1,1.4)) ;
#102595 = CARTESIAN_POINT('',(0.899999999999999,0.1,1.5)) ;
#102596 = CARTESIAN_POINT('Origin',(0.899999999999999,0.1,1.4)) ;
#102597 = CARTESIAN_POINT('Origin',(0.899999999999999,0.1,1.4)) ;
#102598 = CARTESIAN_POINT('Origin',(-1.7,0.3,-1.5225450639222E-32)) ;
#102599 = CARTESIAN_POINT('Origin',(-1.7,0.3,1.4)) ;
#102600 = CARTESIAN_POINT('Origin',(-1.9,6.9,-1.88079096131566E-32)) ;
#102601 = CARTESIAN_POINT('',(-1.9,7.,1.4)) ;
#102602 = CARTESIAN_POINT('Origin',(-1.9,6.9,1.4)) ;
#102603 = CARTESIAN_POINT('',(-1.9,7.,-1.5)) ;
#102604 = CARTESIAN_POINT('Origin',(-1.9,6.9,-1.4)) ;
#102605 = CARTESIAN_POINT('Origin',(-1.9,7.1,-1.4)) ;
#102606 = CARTESIAN_POINT('Origin',(0.899999999999999,0.1,1.4)) ;
#102607 = CARTESIAN_POINT('Origin',(0.899999999999999,0.1,1.6)) ;
#102608 = CARTESIAN_POINT('Origin',(-1.9668402209837E-32,0.1,1.4)) ;
#102609 = CARTESIAN_POINT('',(0.999999999999999,0.1,1.5)) ;
#102610 = CARTESIAN_POINT('Origin',(-1.7,0.1,1.4)) ;
#102611 = CARTESIAN_POINT('Origin',(-1.7,0.3,1.4)) ;
#102612 = CARTESIAN_POINT('Origin',(-1.9,0.3,1.4)) ;
#102613 = CARTESIAN_POINT('Origin',(-1.9,6.9,1.4)) ;
#102614 = CARTESIAN_POINT('',(-1.9,6.9,1.5)) ;
#102615 = CARTESIAN_POINT('Origin',(-1.9,6.9,1.4)) ;
#102616 = CARTESIAN_POINT('Origin',(-1.9,6.9,1.4)) ;
#102617 = CARTESIAN_POINT('Origin',(-1.9,7.1,-1.5)) ;
#102618 = CARTESIAN_POINT('Origin',(-1.9,7.1,1.4)) ;
#102619 = CARTESIAN_POINT('Origin',(-1.8,0.1,1.6)) ;
#102620 = CARTESIAN_POINT('Origin',(-1.9,0.0999999999999979,1.6)) ;
#102621 = CARTESIAN_POINT('Origin',(-1.9,-6.40600499298624E-17,1.4)) ;
#102622 = CARTESIAN_POINT('',(-1.9,7.,1.5)) ;
#102623 = CARTESIAN_POINT('Origin',(-1.9,6.9,1.4)) ;
#102624 = CARTESIAN_POINT('Origin',(-1.9,6.9,1.6)) ;
#102625 = CARTESIAN_POINT('Origin',(-1.9,7.,1.6)) ;
#102626 = CARTESIAN_POINT('Origin',(-0.900000000000002,2.95,-3.80476326321452E-16)) ;
#102627 = CARTESIAN_POINT('Origin',(-0.900000000000001,2.95,-1.6431676725155)) ;
#102628 = CARTESIAN_POINT('Origin',(-0.900000000000002,2.95,-1.6431676725155)) ;
#102629 = CARTESIAN_POINT('Origin',(-0.900000000000001,2.95,-1.6431676725155)) ;
#102630 = CARTESIAN_POINT('Origin',(-0.900000000000002,2.95,-1.6431676725155)) ;
#102631 = CARTESIAN_POINT('Origin',(1.15,3.15,-2.55)) ;
#102632 = CARTESIAN_POINT('Origin',(1.15,3.15,-1.6431676725155)) ;
#102633 = CARTESIAN_POINT('Origin',(-1.,2.95,-1.6431676725155)) ;
#102634 = CARTESIAN_POINT('Origin',(1.15,2.95,-1.6431676725155)) ;
#102635 = CARTESIAN_POINT('Origin',(-0.900000000000001,3.8,0.)) ;
#102636 = CARTESIAN_POINT('Origin',(-0.900000000000002,2.1568323274845,-0.850000000000001)) ;
#102637 = CARTESIAN_POINT('Origin',(-0.900000000000002,1.6,0.)) ;
#102638 = CARTESIAN_POINT('Origin',(-0.900000000000002,1.6,-1.96214168703487)) ;
#102639 = CARTESIAN_POINT('Origin',(13.9153543900904,1.4,-1.96214168703487)) ;
#102640 = CARTESIAN_POINT('Origin',(8.49172374697002,1.4,-1.96214168703487)) ;
#102641 = CARTESIAN_POINT('Origin',(-0.900000000000001,1.40000000000001,-1.96214168703487)) ;
#102642 = CARTESIAN_POINT('Origin',(1.15,2.95,-1.6431676725155)) ;
#102643 = CARTESIAN_POINT('Origin',(1.15,3.04189189189189,-1.46552792413544)) ;
#102644 = CARTESIAN_POINT('Origin',(-0.900000000000002,2.1568323274845,-0.850000000000001)) ;
#102645 = CARTESIAN_POINT('Origin',(-0.900000000000002,2.1568323274845,-0.850000000000001)) ;
#102646 = CARTESIAN_POINT('Origin',(-0.900000000000002,2.1568323274845,-0.850000000000001)) ;
#102647 = CARTESIAN_POINT('Origin',(-0.900000000000001,1.40000000000001,-1.96214168703487)) ;
#102648 = CARTESIAN_POINT('Origin',(-0.900000000000002,1.55483870967742,-1.83555190077455)) ;
#102649 = CARTESIAN_POINT('Origin',(1.15,3.8,0.)) ;
#102650 = CARTESIAN_POINT('Origin',(1.15,2.33447207586456,-0.758108108108109)) ;
#102651 = CARTESIAN_POINT('Origin',(-1.,2.1568323274845,-0.850000000000001)) ;
#102652 = CARTESIAN_POINT('Origin',(1.15,2.1568323274845,-0.850000000000001)) ;
#102653 = CARTESIAN_POINT('Origin',(-0.900000000000001,3.8,-0.85)) ;
#102654 = CARTESIAN_POINT('Origin',(-0.900000000000002,1.02736587339765,-0.850000000000001)) ;
#102655 = CARTESIAN_POINT('Origin',(-0.900000000000001,3.8,0.)) ;
#102656 = CARTESIAN_POINT('Origin',(-0.900000000000002,1.02736587339765,-0.850000000000001)) ;
#102657 = CARTESIAN_POINT('Origin',(13.9153543900904,1.4,1.96214168703487)) ;
#102658 = CARTESIAN_POINT('Origin',(8.49172374697002,1.4,1.96214168703487)) ;
#102659 = CARTESIAN_POINT('Origin',(-0.900000000000001,1.40000000000001,1.96214168703487)) ;
#102660 = CARTESIAN_POINT('Origin',(-0.900000000000002,1.6,0.)) ;
#102661 = CARTESIAN_POINT('Origin',(-0.900000000000002,1.6,1.96214168703487)) ;
#102662 = CARTESIAN_POINT('Origin',(-0.900000000000002,2.95,3.80476326321453E-16)) ;
#102663 = CARTESIAN_POINT('Origin',(-0.900000000000002,2.95,1.6431676725155)) ;
#102664 = CARTESIAN_POINT('Origin',(1.15,2.1568323274845,-0.850000000000001)) ;
#102665 = CARTESIAN_POINT('Origin',(1.15,2.1568323274845,-0.65)) ;
#102666 = CARTESIAN_POINT('Origin',(-0.900000000000002,1.02736587339765,-0.850000000000001)) ;
#102667 = CARTESIAN_POINT('Origin',(-0.900000000000001,1.40000000000001,1.96214168703487)) ;
#102668 = CARTESIAN_POINT('Origin',(-0.900000000000002,1.55483870967743,1.83555190077455)) ;
#102669 = CARTESIAN_POINT('Origin',(-0.900000000000002,2.95,1.6431676725155)) ;
#102670 = CARTESIAN_POINT('Origin',(-0.900000000000002,2.95,1.6431676725155)) ;
#102671 = CARTESIAN_POINT('Origin',(-0.900000000000001,2.95,1.6431676725155)) ;
#102672 = CARTESIAN_POINT('Origin',(1.15,2.21886116991581,-0.65)) ;
#102673 = CARTESIAN_POINT('Ctrl Pts',(1.15,1.02736587339765,-0.750000000000001)) ;
#102674 = CARTESIAN_POINT('Ctrl Pts',(1.1608920328805,1.02736587339765,-0.750000000000001)) ;
#102675 = CARTESIAN_POINT('Ctrl Pts',(1.17195716626105,1.02622125393927,-0.748143843925991)) ;
#102676 = CARTESIAN_POINT('Ctrl Pts',(1.1820844490224,1.02414637334385,-0.74471318879084)) ;
#102677 = CARTESIAN_POINT('Ctrl Pts',(1.19245005921088,1.02202266415684,-0.741201799343137)) ;
#102678 = CARTESIAN_POINT('Ctrl Pts',(1.20216743701154,1.01888103823701,-0.735960198070275)) ;
#102679 = CARTESIAN_POINT('Ctrl Pts',(1.21053792402812,1.01518120925307,-0.72959371680205)) ;
#102680 = CARTESIAN_POINT('Ctrl Pts',(1.219343173684,1.01128921135341,-0.722896560843853)) ;
#102681 = CARTESIAN_POINT('Ctrl Pts',(1.22692289939014,1.00668521903338,-0.714785161531543)) ;
#102682 = CARTESIAN_POINT('Ctrl Pts',(1.23290049538659,1.00186003905466,-0.70592412596239)) ;
#102683 = CARTESIAN_POINT('Ctrl Pts',(1.23922345568944,0.9967560772818,-0.696551131169983)) ;
#102684 = CARTESIAN_POINT('Ctrl Pts',(1.24392209779927,0.991279542094837,
-0.68610455998969)) ;
#102685 = CARTESIAN_POINT('Ctrl Pts',(1.24674870216524,0.985895902333124,
-0.675292066529666)) ;
#102686 = CARTESIAN_POINT('Ctrl Pts',(1.24889292215336,0.981811953364218,
-0.667089869972722)) ;
#102687 = CARTESIAN_POINT('Ctrl Pts',(1.25,0.977715885027402,-0.658549168629227)) ;
#102688 = CARTESIAN_POINT('Ctrl Pts',(1.25,0.973783447787483,-0.650000000000001)) ;
#102689 = CARTESIAN_POINT('Origin',(-0.900000000000001,3.8,0.)) ;
#102690 = CARTESIAN_POINT('Origin',(-0.900000000000002,1.02736587339765,0.849999999999999)) ;
#102691 = CARTESIAN_POINT('Origin',(-0.900000000000001,3.8,0.850000000000002)) ;
#102692 = CARTESIAN_POINT('Origin',(-0.900000000000002,2.1568323274845,0.85)) ;
#102693 = CARTESIAN_POINT('Origin',(-0.900000000000002,1.02736587339765,0.849999999999999)) ;
#102694 = CARTESIAN_POINT('Origin',(-0.900000000000001,3.8,0.)) ;
#102695 = CARTESIAN_POINT('Origin',(-0.900000000000002,2.1568323274845,0.85)) ;
#102696 = CARTESIAN_POINT('Origin',(-1.,2.95,1.6431676725155)) ;
#102697 = CARTESIAN_POINT('Origin',(1.15,2.95,1.6431676725155)) ;
#102698 = CARTESIAN_POINT('Origin',(1.15,3.15,2.55)) ;
#102699 = CARTESIAN_POINT('Origin',(1.15,3.15,1.6431676725155)) ;
#102700 = CARTESIAN_POINT('Ctrl Pts',(1.110285585749,0.930383836951471,-0.87499428365811)) ;
#102701 = CARTESIAN_POINT('Ctrl Pts',(1.14039000477526,0.892136466138004,
-0.749969718594225)) ;
#102702 = CARTESIAN_POINT('Ctrl Pts',(1.13015013463565,1.02610337426265,-0.747851124882802)) ;
#102703 = CARTESIAN_POINT('Ctrl Pts',(1.17639690652713,0.935225109827677,
-0.890125739946714)) ;
#102704 = CARTESIAN_POINT('Ctrl Pts',(1.15491086542926,0.891146666106694,
-0.749276050401193)) ;
#102705 = CARTESIAN_POINT('Ctrl Pts',(1.16319405445818,1.03078047702079,-0.755164874245163)) ;
#102706 = CARTESIAN_POINT('Ctrl Pts',(1.24701363206613,0.927145283841823,
-0.865552203825101)) ;
#102707 = CARTESIAN_POINT('Ctrl Pts',(1.17759980831448,0.893467326853883,
-0.752637312031294)) ;
#102708 = CARTESIAN_POINT('Ctrl Pts',(1.19848758201045,1.02297467453102,-0.74328712255501)) ;
#102709 = CARTESIAN_POINT('Ctrl Pts',(1.33816236560061,0.900022463714227,
-0.769808850614887)) ;
#102710 = CARTESIAN_POINT('Ctrl Pts',(1.22862786282604,0.888037626603987,
-0.723153964324038)) ;
#102711 = CARTESIAN_POINT('Ctrl Pts',(1.24403288504499,0.996768276947731,
-0.697026659413336)) ;
#102712 = CARTESIAN_POINT('Ctrl Pts',(1.35959492575604,0.881455895025373,
-0.698532341229029)) ;
#102713 = CARTESIAN_POINT('Ctrl Pts',(1.25320519750685,0.880428099081617,
-0.691064937827297)) ;
#102714 = CARTESIAN_POINT('Ctrl Pts',(1.25473603279824,0.978811277328854,
-0.662557487150855)) ;
#102715 = CARTESIAN_POINT('Ctrl Pts',(1.34615355831623,0.867571605181204,
-0.632792582533412)) ;
#102716 = CARTESIAN_POINT('Ctrl Pts',(1.25176090202797,0.870950130624675,
-0.649449017057823)) ;
#102717 = CARTESIAN_POINT('Ctrl Pts',(1.24801589497572,0.965423101361815,
-0.630869548163999)) ;
#102718 = CARTESIAN_POINT('Origin',(1.35,0.973783447787483,-0.650000000000001)) ;
#102719 = CARTESIAN_POINT('Origin',(-0.900000000000002,1.02736587339765,0.849999999999999)) ;
#102720 = CARTESIAN_POINT('',(-0.957735026918965,0.969630846478688,0.792264973081036)) ;
#102721 = CARTESIAN_POINT('Origin',(-0.900000000000002,1.02736587339765,0.849999999999999)) ;
#102722 = CARTESIAN_POINT('Origin',(-0.900000000000002,2.1568323274845,0.85)) ;
#102723 = CARTESIAN_POINT('Origin',(-0.900000000000002,2.1568323274845,0.85)) ;
#102724 = CARTESIAN_POINT('Origin',(1.15,2.95,1.6431676725155)) ;
#102725 = CARTESIAN_POINT('Origin',(1.15,3.04189189189189,1.46552792413544)) ;
#102726 = CARTESIAN_POINT('Origin',(1.35,3.8,0.)) ;
#102727 = CARTESIAN_POINT('Origin',(1.35,0.973783447787484,0.649999999999999)) ;
#102728 = CARTESIAN_POINT('Origin',(-1.,2.1568323274845,0.850000000000001)) ;
#102729 = CARTESIAN_POINT('Origin',(1.15,2.1568323274845,0.850000000000001)) ;
#102730 = CARTESIAN_POINT('Origin',(1.15,3.8,0.)) ;
#102731 = CARTESIAN_POINT('Origin',(1.15,2.33447207586456,0.758108108108108)) ;
#102732 = CARTESIAN_POINT('Ctrl Pts',(1.34754079198594,0.869159571293157,
0.640251465214486)) ;
#102733 = CARTESIAN_POINT('Ctrl Pts',(1.25183398383323,0.871999770424339,
0.654001348239709)) ;
#102734 = CARTESIAN_POINT('Ctrl Pts',(1.24871534599026,0.966951450593888,
0.634464286926457)) ;
#102735 = CARTESIAN_POINT('Ctrl Pts',(1.3578897130187,0.882932151572343,0.704222571731899)) ;
#102736 = CARTESIAN_POINT('Ctrl Pts',(1.25138796519089,0.881019151005411,
0.693512718576227)) ;
#102737 = CARTESIAN_POINT('Ctrl Pts',(1.25389076424432,0.980237216252359,
0.665311365740565)) ;
#102738 = CARTESIAN_POINT('Ctrl Pts',(1.33642796493171,0.900551643074787,
0.771683281031192)) ;
#102739 = CARTESIAN_POINT('Ctrl Pts',(1.22773025960898,0.888154519889407,
0.723697645847668)) ;
#102740 = CARTESIAN_POINT('Ctrl Pts',(1.24317203399027,0.997278352451065,
0.697935541716943)) ;
#102741 = CARTESIAN_POINT('Ctrl Pts',(1.24851212064761,0.926675670999746,
0.863888145813442)) ;
#102742 = CARTESIAN_POINT('Ctrl Pts',(1.17855408504648,0.893378082604329,
0.752064154599799)) ;
#102743 = CARTESIAN_POINT('Ctrl Pts',(1.19923947710883,1.02252144543593,0.742488815939334)) ;
#102744 = CARTESIAN_POINT('Ctrl Pts',(1.18212686068544,0.934567888698255,
0.888107740099251)) ;
#102745 = CARTESIAN_POINT('Ctrl Pts',(1.15690947476176,0.891342319659343,
0.749498697761042)) ;
#102746 = CARTESIAN_POINT('Ctrl Pts',(1.16605892368789,1.03014681530423,0.754195876479622)) ;
#102747 = CARTESIAN_POINT('Ctrl Pts',(1.11776263740947,0.930888708579169,
0.876576418083976)) ;
#102748 = CARTESIAN_POINT('Ctrl Pts',(1.14197710563589,0.892059806626672,
0.749917700344492)) ;
#102749 = CARTESIAN_POINT('Ctrl Pts',(1.13388624958144,1.02659206201249,0.748622143898735)) ;
#102750 = CARTESIAN_POINT('Ctrl Pts',(1.15,1.02736587339764,0.749999999999999)) ;
#102751 = CARTESIAN_POINT('Ctrl Pts',(1.15623005440502,1.02736587339759,0.750000000000132)) ;
#102752 = CARTESIAN_POINT('Ctrl Pts',(1.16249579431471,1.02700282517053,0.749409133931021)) ;
#102753 = CARTESIAN_POINT('Ctrl Pts',(1.16857840195431,1.02630083270769,0.748259060553334)) ;
#102754 = CARTESIAN_POINT('Ctrl Pts',(1.1798885498395,1.02499553092934,0.746120586275334)) ;
#102755 = CARTESIAN_POINT('Ctrl Pts',(1.19084787809767,1.02245621903271,0.741949303384784)) ;
#102756 = CARTESIAN_POINT('Ctrl Pts',(1.20043335385463,1.01914369852331,0.736350893562102)) ;
#102757 = CARTESIAN_POINT('Ctrl Pts',(1.21063893018497,1.01561688548223,0.730390313177509)) ;
#102758 = CARTESIAN_POINT('Ctrl Pts',(1.21965078109605,1.01112191387731,0.722645148898142)) ;
#102759 = CARTESIAN_POINT('Ctrl Pts',(1.226898722009,1.00626683908294,0.713926415145715)) ;
#102760 = CARTESIAN_POINT('Ctrl Pts',(1.23435386869391,1.0012729663137,0.704958428263417)) ;
#102761 = CARTESIAN_POINT('Ctrl Pts',(1.24017476602864,0.995763540409855,
0.694712973593074)) ;
#102762 = CARTESIAN_POINT('Ctrl Pts',(1.24405759382605,0.990267693778535,
0.683958342769537)) ;
#102763 = CARTESIAN_POINT('Ctrl Pts',(1.24795610732226,0.9847496452368,0.673160265800921)) ;
#102764 = CARTESIAN_POINT('Ctrl Pts',(1.25,0.97910634898267,0.661572054972022)) ;
#102765 = CARTESIAN_POINT('Ctrl Pts',(1.25,0.973783447787483,0.649999999999999)) ;
#102766 = CARTESIAN_POINT('Origin',(1.15,2.1568323274845,0.850000000000001)) ;
#102767 = CARTESIAN_POINT('Origin',(1.15,2.1568323274845,0.65)) ;
#102768 = CARTESIAN_POINT('Origin',(1.15,2.21886116991581,0.65)) ;
#102769 = CARTESIAN_POINT('Origin',(1.5,2.3,-0.4)) ;
#102770 = CARTESIAN_POINT('Ctrl Pts',(0.55,4.04473197180486,-0.449999999999999)) ;
#102771 = CARTESIAN_POINT('Ctrl Pts',(0.55,4.04340510574361,-0.452018391674586)) ;
#102772 = CARTESIAN_POINT('Ctrl Pts',(0.549938912488053,4.04197482121868,
-0.453979909355823)) ;
#102773 = CARTESIAN_POINT('Ctrl Pts',(0.549362579613731,4.03414945156067,
-0.463763201696885)) ;
#102774 = CARTESIAN_POINT('Ctrl Pts',(0.548040652125116,4.02633974827564,
-0.470545826227087)) ;
#102775 = CARTESIAN_POINT('Ctrl Pts',(0.544205267183646,4.00519499286859,
-0.484683942788798)) ;
#102776 = CARTESIAN_POINT('Ctrl Pts',(0.541221332378524,3.99011995637992,
-0.49122511544812)) ;
#102777 = CARTESIAN_POINT('Ctrl Pts',(0.537814556431593,3.96385893187685,
-0.497930592239943)) ;
#102778 = CARTESIAN_POINT('Ctrl Pts',(0.536602540378443,3.95132390702873,
-0.5)) ;
#102779 = CARTESIAN_POINT('Ctrl Pts',(0.536602540378443,3.93764017256378,
-0.5)) ;
#102780 = CARTESIAN_POINT('Origin',(-0.4,2.3,-0.4)) ;
#102781 = CARTESIAN_POINT('Origin',(-0.4,-3.4,-0.4)) ;
#102782 = CARTESIAN_POINT('Origin',(-0.4,-3.36847777691809,-0.4)) ;
#102783 = CARTESIAN_POINT('Origin',(1.5,2.3,-0.4)) ;
#102784 = CARTESIAN_POINT('Ctrl Pts',(0.536602540378444,2.83090991212703,
-0.5)) ;
#102785 = CARTESIAN_POINT('Ctrl Pts',(0.536602540378444,2.80627146475495,
-0.5)) ;
#102786 = CARTESIAN_POINT('Ctrl Pts',(0.538106903229181,2.77742679387655,
-0.497952790812571)) ;
#102787 = CARTESIAN_POINT('Ctrl Pts',(0.545186976568881,2.71156844363323,
-0.48208398098003)) ;
#102788 = CARTESIAN_POINT('Ctrl Pts',(0.55,2.68282906082667,-0.468102055813631)) ;
#102789 = CARTESIAN_POINT('Ctrl Pts',(0.55,2.65280931275608,-0.449999999999997)) ;
#102790 = CARTESIAN_POINT('Origin',(0.400000000000001,2.29999999999999,-0.4)) ;
#102791 = CARTESIAN_POINT('Origin',(0.0725078566451197,-4.04348900069683,
0.0725078566451195)) ;
#102792 = CARTESIAN_POINT('Origin',(-0.4,-3.36847777691809,-0.4)) ;
#102793 = CARTESIAN_POINT('Origin',(-0.0979344438426628,-3.8,-0.0979344438426628)) ;
#102794 = CARTESIAN_POINT('Origin',(1.5,2.3,0.4)) ;
#102795 = CARTESIAN_POINT('Ctrl Pts',(0.536602540378444,3.93764017256378,
0.5)) ;
#102796 = CARTESIAN_POINT('Ctrl Pts',(0.536602540378444,3.93925361219656,
0.5)) ;
#102797 = CARTESIAN_POINT('Ctrl Pts',(0.536619300889434,3.94087098263999,
0.499971002742215)) ;
#102798 = CARTESIAN_POINT('Ctrl Pts',(0.536997639747709,3.95938954612074,
0.499314187104252)) ;
#102799 = CARTESIAN_POINT('Ctrl Pts',(0.539142315171056,3.97567120869891,
0.495687938438414)) ;
#102800 = CARTESIAN_POINT('Ctrl Pts',(0.544035197036655,4.00535605098085,
0.484600608334013)) ;
#102801 = CARTESIAN_POINT('Ctrl Pts',(0.546989816174414,4.01946236900604,
0.476430055365021)) ;
#102802 = CARTESIAN_POINT('Ctrl Pts',(0.549463062495691,4.03595536007401,
0.461452618302868)) ;
#102803 = CARTESIAN_POINT('Ctrl Pts',(0.550000000000879,4.04078397701435,
0.456005579653646)) ;
#102804 = CARTESIAN_POINT('Ctrl Pts',(0.549999999999999,4.04473197181449,
0.449999999985356)) ;
#102805 = CARTESIAN_POINT('Origin',(-0.4,2.3,0.4)) ;
#102806 = CARTESIAN_POINT('Origin',(0.4,2.29999999999999,-0.4)) ;
#102807 = CARTESIAN_POINT('Origin',(0.4,-3.36847777691809,-0.4)) ;
#102808 = CARTESIAN_POINT('Origin',(-0.0979344438426628,-3.8,-0.0979344438426627)) ;
#102809 = CARTESIAN_POINT('Origin',(-0.0979344438426628,-3.8,-0.0979344438426626)) ;
#102810 = CARTESIAN_POINT('Origin',(-0.0979344438426627,-3.8,-0.0979344438426627)) ;
#102811 = CARTESIAN_POINT('Origin',(-0.4,2.3,0.4)) ;
#102812 = CARTESIAN_POINT('Origin',(-0.4,-3.36847777691809,0.4)) ;
#102813 = CARTESIAN_POINT('Origin',(0.190875981738719,-3.6672263744342,-0.190875981738719)) ;
#102814 = CARTESIAN_POINT('Origin',(0.400000000000001,-3.36847777691809,-0.4)) ;
#102815 = CARTESIAN_POINT('Origin',(0.0979344438426626,-3.8,-0.0979344438426627)) ;
#102816 = CARTESIAN_POINT('Origin',(0.15,-3.8,-0.0979344438426626)) ;
#102817 = CARTESIAN_POINT('Origin',(0.0979344438426627,-3.8,-0.0979344438426626)) ;
#102818 = CARTESIAN_POINT('Origin',(-0.0979344438426628,-3.8,0.5)) ;
#102819 = CARTESIAN_POINT('Origin',(-0.0979344438426628,-3.8,0.0979344438426625)) ;
#102820 = CARTESIAN_POINT('Origin',(-0.174966890829628,-3.68995364716148,
0.174966890829628)) ;
#102821 = CARTESIAN_POINT('Origin',(-0.400000000000001,-3.36847777691809,
0.4)) ;
#102822 = CARTESIAN_POINT('Origin',(-0.0979344438426627,-3.8,0.0979344438426627)) ;
#102823 = CARTESIAN_POINT('Origin',(0.0979344438426627,-3.8,-0.0979344438426628)) ;
#102824 = CARTESIAN_POINT('Origin',(0.0979344438426628,-3.8,-0.0979344438426625)) ;
#102825 = CARTESIAN_POINT('Origin',(-0.0979344438426628,-3.8,0.0979344438426627)) ;
#102826 = CARTESIAN_POINT('Origin',(-0.0979344438426628,-3.8,0.0979344438426627)) ;
#102827 = CARTESIAN_POINT('Origin',(0.0979344438426627,-3.8,0.5)) ;
#102828 = CARTESIAN_POINT('Origin',(0.0979344438426627,-3.8,0.0979344438426627)) ;
#102829 = CARTESIAN_POINT('Origin',(-1.11032778078669,-3.8,0.0979344438426627)) ;
#102830 = CARTESIAN_POINT('Origin',(0.0979344438426626,-3.8,0.0979344438426627)) ;
#102831 = CARTESIAN_POINT('Origin',(0.0979344438426627,-3.8,0.0979344438426627)) ;
#102832 = CARTESIAN_POINT('Origin',(0.0979344438426627,-3.8,0.0979344438426626)) ;
#102833 = CARTESIAN_POINT('Origin',(0.438350729213467,-3.31369102089885,0.438350729213466)) ;
#102834 = CARTESIAN_POINT('Origin',(0.399999999999999,-3.36847777691809,0.399999999999999)) ;
#102835 = CARTESIAN_POINT('Origin',(0.4,2.3,0.4)) ;
#102836 = CARTESIAN_POINT('Origin',(0.4,-3.36847777691809,0.4)) ;
#102837 = CARTESIAN_POINT('Origin',(0.4,2.29999999999999,0.4)) ;
#102838 = CARTESIAN_POINT('Origin',(1.5,2.3,0.4)) ;
#102839 = CARTESIAN_POINT('Ctrl Pts',(0.55,2.65280931275594,0.449999999999912)) ;
#102840 = CARTESIAN_POINT('Ctrl Pts',(0.550000000000012,2.67648433237899,
0.464276153337302)) ;
#102841 = CARTESIAN_POINT('Ctrl Pts',(0.546908864252786,2.69988533923264,
0.476474299152385)) ;
#102842 = CARTESIAN_POINT('Ctrl Pts',(0.539540151921445,2.76165254733708,
0.495908401809885)) ;
#102843 = CARTESIAN_POINT('Ctrl Pts',(0.536602540378444,2.79600904778113,
0.5)) ;
#102844 = CARTESIAN_POINT('Ctrl Pts',(0.536602540378444,2.83090991212703,
0.5)) ;
#102845 = CARTESIAN_POINT('Origin',(8.,3.4,-0.4)) ;
#102846 = CARTESIAN_POINT('Origin',(7.96847777691809,3.4,-0.4)) ;
#102847 = CARTESIAN_POINT('Origin',(1.5,4.2,-0.4)) ;
#102848 = CARTESIAN_POINT('Origin',(7.96847777691809,4.2,-0.4)) ;
#102849 = CARTESIAN_POINT('Origin',(8.64348900069683,3.87250785664512,0.0725078566451195)) ;
#102850 = CARTESIAN_POINT('Origin',(7.96847777691809,3.4,-0.4)) ;
#102851 = CARTESIAN_POINT('Origin',(8.4,3.70206555615734,-0.0979344438426621)) ;
#102852 = CARTESIAN_POINT('Origin',(8.26722637443421,3.99087598173872,-0.190875981738719)) ;
#102853 = CARTESIAN_POINT('Origin',(7.96847777691809,4.2,-0.4)) ;
#102854 = CARTESIAN_POINT('Origin',(8.4,3.89793444384266,-0.0979344438426626)) ;
#102855 = CARTESIAN_POINT('Origin',(8.4,3.95,-0.0979344438426626)) ;
#102856 = CARTESIAN_POINT('Origin',(8.4,3.70206555615734,-0.0979344438426625)) ;
#102857 = CARTESIAN_POINT('Origin',(8.4,3.89793444384266,-0.0979344438426626)) ;
#102858 = CARTESIAN_POINT('Origin',(8.4,3.70206555615734,-0.0979344438426625)) ;
#102859 = CARTESIAN_POINT('Origin',(8.4,3.70206555615734,-0.0979344438426626)) ;
#102860 = CARTESIAN_POINT('Origin',(1.5,3.4,0.4)) ;
#102861 = CARTESIAN_POINT('Origin',(7.96847777691809,3.4,0.4)) ;
#102862 = CARTESIAN_POINT('Origin',(1.5,4.2,0.4)) ;
#102863 = CARTESIAN_POINT('Origin',(7.96847777691809,4.2,0.4)) ;
#102864 = CARTESIAN_POINT('Origin',(8.4,3.89793444384266,-0.0979344438426626)) ;
#102865 = CARTESIAN_POINT('Origin',(8.4,3.89793444384266,-0.0979344438426625)) ;
#102866 = CARTESIAN_POINT('Origin',(8.4,3.70206555615734,0.5)) ;
#102867 = CARTESIAN_POINT('Origin',(8.4,3.70206555615734,0.0979344438426624)) ;
#102868 = CARTESIAN_POINT('Origin',(8.28995364716148,3.62503310917037,0.174966890829628)) ;
#102869 = CARTESIAN_POINT('Origin',(7.96847777691809,3.4,0.4)) ;
#102870 = CARTESIAN_POINT('Origin',(8.4,3.70206555615734,0.0979344438426625)) ;
#102871 = CARTESIAN_POINT('Origin',(7.91369102089885,4.23835072921347,0.438350729213466)) ;
#102872 = CARTESIAN_POINT('Origin',(7.96847777691809,4.2,0.4)) ;
#102873 = CARTESIAN_POINT('Origin',(8.4,3.89793444384266,0.0979344438426624)) ;
#102874 = CARTESIAN_POINT('Origin',(8.4,3.89793444384266,0.5)) ;
#102875 = CARTESIAN_POINT('Origin',(8.4,3.89793444384266,0.0979344438426625)) ;
#102876 = CARTESIAN_POINT('Origin',(8.4,3.70206555615734,0.0979344438426625)) ;
#102877 = CARTESIAN_POINT('Origin',(8.4,3.70206555615734,0.0979344438426625)) ;
#102878 = CARTESIAN_POINT('Origin',(8.4,3.89793444384266,0.0979344438426626)) ;
#102879 = CARTESIAN_POINT('Origin',(8.4,3.89793444384266,0.0979344438426626)) ;
#102880 = CARTESIAN_POINT('Origin',(8.4,2.68967221921331,0.0979344438426624)) ;
#102881 = CARTESIAN_POINT('Origin',(9.9,6.8847127088383,-2.54)) ;
#102882 = CARTESIAN_POINT('Origin',(9.9,6.8847127088383,-0.959712708838304)) ;
#102883 = CARTESIAN_POINT('Origin',(8.77035388141948,6.69643835574155,-0.771438355741551)) ;
#102884 = CARTESIAN_POINT('Ctrl Pts',(8.58356010126947,6.66256607592813,-0.638926683544912)) ;
#102885 = CARTESIAN_POINT('Ctrl Pts',(8.58266714977878,6.65676189123867,-0.638777858296464)) ;
#102886 = CARTESIAN_POINT('Ctrl Pts',(8.58182526931896,6.6507714222091,-0.639114171474057)) ;
#102887 = CARTESIAN_POINT('Ctrl Pts',(8.58032528754334,6.63886560514808,-0.640912735099675)) ;
#102888 = CARTESIAN_POINT('Ctrl Pts',(8.57966270906106,6.63295370212158,-0.64234482433286)) ;
#102889 = CARTESIAN_POINT('Ctrl Pts',(8.57906641006218,6.62681909302492,-0.644477174493837)) ;
#102890 = CARTESIAN_POINT('Ctrl Pts',(8.57903375157327,6.62647998752492,-0.644597169728486)) ;
#102891 = CARTESIAN_POINT('Ctrl Pts',(8.5784656962419,6.62052582174859,-0.646741731680975)) ;
#102892 = CARTESIAN_POINT('Ctrl Pts',(8.57802501793962,6.61503168015214,-0.649314285855883)) ;
#102893 = CARTESIAN_POINT('Ctrl Pts',(8.57766199200566,6.60925146760271,-0.652746213323561)) ;
#102894 = CARTESIAN_POINT('Ctrl Pts',(8.57762821177171,6.60869602779083,-0.653083835164735)) ;
#102895 = CARTESIAN_POINT('Ctrl Pts',(8.57728522755448,6.60286036001494,-0.656714798956953)) ;
#102896 = CARTESIAN_POINT('Ctrl Pts',(8.57709550103274,6.59788070192403,-0.660548221055747)) ;
#102897 = CARTESIAN_POINT('Ctrl Pts',(8.57703980289278,6.59299711069459,-0.665172337354183)) ;
#102898 = CARTESIAN_POINT('Ctrl Pts',(8.5770367027102,6.59265952430071,-0.665496892541691)) ;
#102899 = CARTESIAN_POINT('Ctrl Pts',(8.57701334129167,6.58927432516126,-0.668801381595255)) ;
#102900 = CARTESIAN_POINT('Ctrl Pts',(8.57705699426433,6.58642971201548,-0.671991744408714)) ;
#102901 = CARTESIAN_POINT('Ctrl Pts',(8.57735031225518,6.57961409340219,-0.680795441755407)) ;
#102902 = CARTESIAN_POINT('Ctrl Pts',(8.57770856513435,6.57604383182912,-0.686668245539852)) ;
#102903 = CARTESIAN_POINT('Ctrl Pts',(8.57865704971091,6.57055741297625,-0.698332219338929)) ;
#102904 = CARTESIAN_POINT('Ctrl Pts',(8.57922107378972,6.5685147605043,-0.704073634908064)) ;
#102905 = CARTESIAN_POINT('Ctrl Pts',(8.57993695782547,6.56687610193741,-0.710455934816734)) ;
#102906 = CARTESIAN_POINT('Ctrl Pts',(8.58000419042985,6.5667300168205,-0.711047835184081)) ;
#102907 = CARTESIAN_POINT('Ctrl Pts',(8.58074399738022,6.56520526212512,-0.717481251735679)) ;
#102908 = CARTESIAN_POINT('Ctrl Pts',(8.58149993293357,6.56438134785765,-0.723354180094219)) ;
#102909 = CARTESIAN_POINT('Ctrl Pts',(8.58236768178488,6.56403389662198,-0.729498757823986)) ;
#102910 = CARTESIAN_POINT('Ctrl Pts',(8.58242358604554,6.56401394107884,-0.729892173631949)) ;
#102911 = CARTESIAN_POINT('Ctrl Pts',(8.58283067264383,6.56388592662946,-0.732739423426399)) ;
#102912 = CARTESIAN_POINT('Ctrl Pts',(8.5831915624065,6.56386525642004,-0.735169950582818)) ;
#102913 = CARTESIAN_POINT('Ctrl Pts',(8.58356019967708,6.56392669994633,-0.737566265064708)) ;
#102914 = CARTESIAN_POINT('Origin',(9.9,6.8847127088383,-0.959712708838304)) ;
#102915 = CARTESIAN_POINT('Origin',(9.9,6.8847127088383,-0.959712708838304)) ;
#102916 = CARTESIAN_POINT('Origin',(9.9,6.8847127088383,-0.959712708838304)) ;
#102917 = CARTESIAN_POINT('Origin',(9.9,7.72792407799439,-2.54)) ;
#102918 = CARTESIAN_POINT('Origin',(9.9,7.72792407799439,-0.959712708838304)) ;
#102919 = CARTESIAN_POINT('Origin',(9.90000000000001,4.35421736843756,-0.959712708838305)) ;
#102920 = CARTESIAN_POINT('Origin',(9.9,7.72792407799439,-0.959712708838304)) ;
#102921 = CARTESIAN_POINT('Origin',(9.9,7.72792407799439,-0.959712708838304)) ;
#102922 = CARTESIAN_POINT('Origin',(9.9,7.72792407799439,-0.959712708838304)) ;
#102923 = CARTESIAN_POINT('Origin',(10.9628342502842,7.37364599456632,-1.13685175055234)) ;
#102924 = CARTESIAN_POINT('Ctrl Pts',(8.56837732530586,8.27720755823131,-0.73250525379773)) ;
#102925 = CARTESIAN_POINT('Ctrl Pts',(8.56753565030796,8.2774881236726,-0.726612992197404)) ;
#102926 = CARTESIAN_POINT('Ctrl Pts',(8.56682045541688,8.27721180667909,-0.720541294439539)) ;
#102927 = CARTESIAN_POINT('Ctrl Pts',(8.56575413148033,8.27538624160241,-0.708728472119804)) ;
#102928 = CARTESIAN_POINT('Ctrl Pts',(8.56538426077877,8.27391165896585,-0.702990562432011)) ;
#102929 = CARTESIAN_POINT('Ctrl Pts',(8.56517777855942,8.27166501362671,-0.697014775451337)) ;
#102930 = CARTESIAN_POINT('Ctrl Pts',(8.56516523451685,8.27151619608678,-0.696627638285824)) ;
#102931 = CARTESIAN_POINT('Ctrl Pts',(8.56497390811211,8.26902793125447,-0.69029533599113)) ;
#102932 = CARTESIAN_POINT('Ctrl Pts',(8.56499903025531,8.26597630129447,-0.684535778465806)) ;
#102933 = CARTESIAN_POINT('Ctrl Pts',(8.56538588200255,8.26046191593053,-0.676590672368122)) ;
#102934 = CARTESIAN_POINT('Ctrl Pts',(8.56556309332504,8.25853771611454,-0.674121236455737)) ;
#102935 = CARTESIAN_POINT('Ctrl Pts',(8.56628156514546,8.25214511987157,-0.666801756689111)) ;
#102936 = CARTESIAN_POINT('Ctrl Pts',(8.5670074287479,8.24720216256266,-0.662305445230979)) ;
#102937 = CARTESIAN_POINT('Ctrl Pts',(8.56880713798121,8.23661566152184,-0.654624494880154)) ;
#102938 = CARTESIAN_POINT('Ctrl Pts',(8.5698603939131,8.23102391527008,-0.651384880725776)) ;
#102939 = CARTESIAN_POINT('Ctrl Pts',(8.57116255171742,8.2245955219417,-0.648446774527188)) ;
#102940 = CARTESIAN_POINT('Ctrl Pts',(8.57127495810211,8.22404408343807,-0.648200660790281)) ;
#102941 = CARTESIAN_POINT('Ctrl Pts',(8.57260511146323,8.21755901312516,-0.645374915305223)) ;
#102942 = CARTESIAN_POINT('Ctrl Pts',(8.57395629672867,8.21135759730777,-0.643346386427245)) ;
#102943 = CARTESIAN_POINT('Ctrl Pts',(8.57552311082447,8.20452945286151,-0.641749544317012)) ;
#102944 = CARTESIAN_POINT('Ctrl Pts',(8.57564505123027,8.2040002630702,-0.641629826955897)) ;
#102945 = CARTESIAN_POINT('Ctrl Pts',(8.57731301559524,8.19679193622633,-0.640053462537017)) ;
#102946 = CARTESIAN_POINT('Ctrl Pts',(8.57896065127871,8.19002168485358,-0.639210969344035)) ;
#102947 = CARTESIAN_POINT('Ctrl Pts',(8.58161366784366,8.17959769015476,-0.638755317277183)) ;
#102948 = CARTESIAN_POINT('Ctrl Pts',(8.5825836286427,8.17587911616512,-0.63876393810712)) ;
#102949 = CARTESIAN_POINT('Ctrl Pts',(8.58356010126947,8.17221734381475,-0.638926683544914)) ;
#102950 = CARTESIAN_POINT('Origin',(7.96824861826159,6.56275414521524,0.637754145215235)) ;
#102951 = CARTESIAN_POINT('Origin',(8.59688370202641,6.66156024040334,0.728756524736636)) ;
#102952 = CARTESIAN_POINT('Origin',(9.9,6.8847127088383,0.959712708838304)) ;
#102953 = CARTESIAN_POINT('Origin',(9.9,6.8847127088383,-2.54)) ;
#102954 = CARTESIAN_POINT('Origin',(9.9,6.8847127088383,0.959712708838305)) ;
#102955 = CARTESIAN_POINT('Origin',(9.9,6.8847127088383,0.959712708838304)) ;
#102956 = CARTESIAN_POINT('Origin',(9.9,6.8847127088383,0.959712708838304)) ;
#102957 = CARTESIAN_POINT('Origin',(9.9,6.8,0.959712708838305)) ;
#102958 = CARTESIAN_POINT('Origin',(9.9,7.72792407799439,0.959712708838304)) ;
#102959 = CARTESIAN_POINT('Origin',(9.9,7.72792407799439,-2.54)) ;
#102960 = CARTESIAN_POINT('Origin',(9.9,7.72792407799439,0.959712708838304)) ;
#102961 = CARTESIAN_POINT('Origin',(9.9,7.72792407799439,0.959712708838304)) ;
#102962 = CARTESIAN_POINT('Origin',(9.9,7.72792407799439,0.959712708838304)) ;
#102963 = CARTESIAN_POINT('Origin',(9.60917571369883,7.82486550676144,0.911241994454776)) ;
#102964 = CARTESIAN_POINT('Origin',(8.59099001845934,8.18966234087067,0.734839026100492)) ;
#102965 = CARTESIAN_POINT('Origin',(0.45,4.4,-2.94081128943275E-32)) ;
#102966 = CARTESIAN_POINT('Origin',(0.45,4.4,-0.45)) ;
#102967 = CARTESIAN_POINT('Origin',(0.45,4.4,0.45)) ;
#102968 = CARTESIAN_POINT('Origin',(-1.9,7.55,-2.54)) ;
#102969 = CARTESIAN_POINT('Origin',(6.9,7.75,-2.54)) ;
#102970 = CARTESIAN_POINT('Origin',(7.1,8.2,-2.54)) ;
#102971 = CARTESIAN_POINT('Origin',(9.9,0.1,-2.54)) ;
#102972 = CARTESIAN_POINT('Origin',(9.9,1.16528729116168,-2.54)) ;
#102973 = CARTESIAN_POINT('Origin',(9.9,1.16528729116168,-2.04416188017819)) ;
#102974 = CARTESIAN_POINT('Origin',(9.9,3.8,0.)) ;
#102975 = CARTESIAN_POINT('Origin',(9.9,1.16528729116168,2.0441618801782)) ;
#102976 = CARTESIAN_POINT('Origin',(9.9,1.16528729116168,-2.04416188017819)) ;
#102977 = CARTESIAN_POINT('Origin',(9.9,1.16528729116168,-2.54)) ;
#102978 = CARTESIAN_POINT('Origin',(9.9,1.16528729116168,2.0441618801782)) ;
#102979 = CARTESIAN_POINT('Ctrl Pts',(0.55,0.3,-0.450000000000001)) ;
#102980 = CARTESIAN_POINT('Ctrl Pts',(0.55,0.3,-0.55)) ;
#102981 = CARTESIAN_POINT('Ctrl Pts',(0.45,0.3,-0.550000000000001)) ;
#102982 = CARTESIAN_POINT('Ctrl Pts',(0.55,0.28690770353672,-0.45000000081826)) ;
#102983 = CARTESIAN_POINT('Ctrl Pts',(0.549992696057548,0.30054349846765,
-0.549992696055191)) ;
#102984 = CARTESIAN_POINT('Ctrl Pts',(0.450000000818259,0.286907703536719,
-0.550000000000001)) ;
#102985 = CARTESIAN_POINT('Ctrl Pts',(0.552602750539093,0.273825167611082,
-0.455205501078186)) ;
#102986 = CARTESIAN_POINT('Ctrl Pts',(0.546703256435901,0.299059401315788,
-0.5467032564359)) ;
#102987 = CARTESIAN_POINT('Ctrl Pts',(0.455205501078185,0.273825167611082,
-0.552602750539093)) ;
#102988 = CARTESIAN_POINT('Ctrl Pts',(0.56262134295865,0.249638145915901,
-0.4752426859173)) ;
#102989 = CARTESIAN_POINT('Ctrl Pts',(0.544986924117067,0.282072776439537,
-0.544986924117069)) ;
#102990 = CARTESIAN_POINT('Ctrl Pts',(0.4752426859173,0.2496381459159,-0.56262134295865)) ;
#102991 = CARTESIAN_POINT('Ctrl Pts',(0.570033341471288,0.238545302291403,
-0.490066682942577)) ;
#102992 = CARTESIAN_POINT('Ctrl Pts',(0.547116196858396,0.267914459835244,
-0.547116196858398)) ;
#102993 = CARTESIAN_POINT('Ctrl Pts',(0.490066682942577,0.238545302291402,
-0.570033341471289)) ;
#102994 = CARTESIAN_POINT('Ctrl Pts',(0.597801282701459,0.210777361061231,
-0.545602565402918)) ;
#102995 = CARTESIAN_POINT('Ctrl Pts',(0.570853448890183,0.226374713859281,
-0.57085344889018)) ;
#102996 = CARTESIAN_POINT('Ctrl Pts',(0.545602565402917,0.210777361061233,
-0.597801282701458)) ;
#102997 = CARTESIAN_POINT('Ctrl Pts',(0.623746567173635,0.2,-0.597493134347285)) ;
#102998 = CARTESIAN_POINT('Ctrl Pts',(0.610458667314981,0.2,-0.610458667314981)) ;
#102999 = CARTESIAN_POINT('Ctrl Pts',(0.597493134347281,0.2,-0.623746567173645)) ;
#103000 = CARTESIAN_POINT('Ctrl Pts',(0.65,0.2,-0.650000000000001)) ;
#103001 = CARTESIAN_POINT('Ctrl Pts',(0.65,0.2,-0.650000000000001)) ;
#103002 = CARTESIAN_POINT('Ctrl Pts',(0.65,0.2,-0.650000000000001)) ;
#103003 = CARTESIAN_POINT('Origin',(0.45,0.3,-0.45)) ;
#103004 = CARTESIAN_POINT('Origin',(0.45,1.24941393210234E-16,-0.450000000000001)) ;
#103005 = CARTESIAN_POINT('Origin',(0.45,4.4,-0.45)) ;
#103006 = CARTESIAN_POINT('Origin',(0.45,4.4,-0.45)) ;
#103007 = CARTESIAN_POINT('Origin',(0.45,4.4,-0.45)) ;
#103008 = CARTESIAN_POINT('Origin',(0.549999999999999,4.4,-0.45)) ;
#103009 = CARTESIAN_POINT('Origin',(-1.7,4.4,-0.45)) ;
#103010 = CARTESIAN_POINT('Ctrl Pts',(-1.8,4.6,-0.65)) ;
#103011 = CARTESIAN_POINT('Ctrl Pts',(-1.8,4.6,-0.65)) ;
#103012 = CARTESIAN_POINT('Ctrl Pts',(-1.8,4.6,-0.65)) ;
#103013 = CARTESIAN_POINT('Ctrl Pts',(-1.8,4.57374656717367,-0.597493134347272)) ;
#103014 = CARTESIAN_POINT('Ctrl Pts',(-1.8,4.56045866731613,-0.610458667316091)) ;
#103015 = CARTESIAN_POINT('Ctrl Pts',(-1.8,4.54749313434727,-0.62374656717366)) ;
#103016 = CARTESIAN_POINT('Ctrl Pts',(-1.78922263893876,4.54780128270145,
-0.545602565402917)) ;
#103017 = CARTESIAN_POINT('Ctrl Pts',(-1.77362528614073,4.52085344889015,
-0.570853448890188)) ;
#103018 = CARTESIAN_POINT('Ctrl Pts',(-1.78922263893877,4.49560256540291,
-0.597801282701462)) ;
#103019 = CARTESIAN_POINT('Ctrl Pts',(-1.7614546977086,4.5200333414713,-0.490066682942577)) ;
#103020 = CARTESIAN_POINT('Ctrl Pts',(-1.73208554016475,4.49711619685842,
-0.547116196858392)) ;
#103021 = CARTESIAN_POINT('Ctrl Pts',(-1.7614546977086,4.44006668294258,-0.570033341471286)) ;
#103022 = CARTESIAN_POINT('Ctrl Pts',(-1.7503618540841,4.51262134295865,-0.475242685917298)) ;
#103023 = CARTESIAN_POINT('Ctrl Pts',(-1.71792722356046,4.49498692411707,
-0.544986924117066)) ;
#103024 = CARTESIAN_POINT('Ctrl Pts',(-1.7503618540841,4.42524268591729,-0.562621342958649)) ;
#103025 = CARTESIAN_POINT('Ctrl Pts',(-1.72617483238892,4.50260275053909,
-0.455205501078186)) ;
#103026 = CARTESIAN_POINT('Ctrl Pts',(-1.70094059868421,4.4967032564359,-0.546703256435901)) ;
#103027 = CARTESIAN_POINT('Ctrl Pts',(-1.72617483238892,4.4052055010782,-0.552602750539093)) ;
#103028 = CARTESIAN_POINT('Ctrl Pts',(-1.71309229646328,4.5,-0.450000000818259)) ;
#103029 = CARTESIAN_POINT('Ctrl Pts',(-1.69945650153965,4.49999269603991,
-0.549992696055229)) ;
#103030 = CARTESIAN_POINT('Ctrl Pts',(-1.71309229646328,4.40000000081823,
-0.55)) ;
#103031 = CARTESIAN_POINT('Ctrl Pts',(-1.7,4.5,-0.45)) ;
#103032 = CARTESIAN_POINT('Ctrl Pts',(-1.7,4.5,-0.55)) ;
#103033 = CARTESIAN_POINT('Ctrl Pts',(-1.7,4.4,-0.55)) ;
#103034 = CARTESIAN_POINT('Ctrl Pts',(-1.8,4.6,0.65)) ;
#103035 = CARTESIAN_POINT('Ctrl Pts',(-1.8,4.6,0.65)) ;
#103036 = CARTESIAN_POINT('Ctrl Pts',(-1.8,4.6,0.65)) ;
#103037 = CARTESIAN_POINT('Ctrl Pts',(-1.8,4.54749313434727,0.623746567173674)) ;
#103038 = CARTESIAN_POINT('Ctrl Pts',(-1.8,4.56045866731613,0.61045866731609)) ;
#103039 = CARTESIAN_POINT('Ctrl Pts',(-1.8,4.57374656717367,0.597493134347274)) ;
#103040 = CARTESIAN_POINT('Ctrl Pts',(-1.78922263893877,4.49560256540291,
0.597801282701463)) ;
#103041 = CARTESIAN_POINT('Ctrl Pts',(-1.77362528614073,4.52085344889015,
0.570853448890189)) ;
#103042 = CARTESIAN_POINT('Ctrl Pts',(-1.78922263893876,4.54780128270145,
0.545602565402918)) ;
#103043 = CARTESIAN_POINT('Ctrl Pts',(-1.7614546977086,4.44006668294258,0.570033341471287)) ;
#103044 = CARTESIAN_POINT('Ctrl Pts',(-1.73208554016475,4.49711619685842,
0.547116196858393)) ;
#103045 = CARTESIAN_POINT('Ctrl Pts',(-1.7614546977086,4.5200333414713,0.490066682942578)) ;
#103046 = CARTESIAN_POINT('Ctrl Pts',(-1.7503618540841,4.42524268591729,0.56262134295865)) ;
#103047 = CARTESIAN_POINT('Ctrl Pts',(-1.71792722356046,4.49498692411707,
0.544986924117068)) ;
#103048 = CARTESIAN_POINT('Ctrl Pts',(-1.7503618540841,4.51262134295865,0.475242685917299)) ;
#103049 = CARTESIAN_POINT('Ctrl Pts',(-1.72617483238892,4.4052055010782,0.552602750539093)) ;
#103050 = CARTESIAN_POINT('Ctrl Pts',(-1.70094059868421,4.4967032564359,0.5467032564359)) ;
#103051 = CARTESIAN_POINT('Ctrl Pts',(-1.72617483238892,4.50260275053909,
0.455205501078187)) ;
#103052 = CARTESIAN_POINT('Ctrl Pts',(-1.71309229646328,4.40000000081823,
0.55)) ;
#103053 = CARTESIAN_POINT('Ctrl Pts',(-1.69945650153893,4.4999926960399,0.549992696056988)) ;
#103054 = CARTESIAN_POINT('Ctrl Pts',(-1.71309229646328,4.5,0.450000000818259)) ;
#103055 = CARTESIAN_POINT('Ctrl Pts',(-1.7,4.4,0.55)) ;
#103056 = CARTESIAN_POINT('Ctrl Pts',(-1.7,4.5,0.55)) ;
#103057 = CARTESIAN_POINT('Ctrl Pts',(-1.7,4.5,0.45)) ;
#103058 = CARTESIAN_POINT('Origin',(-1.7,4.4,0.45)) ;
#103059 = CARTESIAN_POINT('Origin',(0.549999999999999,4.4,0.45)) ;
#103060 = CARTESIAN_POINT('Origin',(0.45,4.4,0.45)) ;
#103061 = CARTESIAN_POINT('Origin',(0.45,4.4,0.45)) ;
#103062 = CARTESIAN_POINT('Origin',(0.45,4.4,0.45)) ;
#103063 = CARTESIAN_POINT('Origin',(0.45,4.9047241136249E-17,0.450000000000001)) ;
#103064 = CARTESIAN_POINT('Origin',(0.45,0.3,0.450000000000001)) ;
#103065 = CARTESIAN_POINT('Ctrl Pts',(0.45,0.3,0.550000000000001)) ;
#103066 = CARTESIAN_POINT('Ctrl Pts',(0.55,0.3,0.55)) ;
#103067 = CARTESIAN_POINT('Ctrl Pts',(0.55,0.3,0.450000000000001)) ;
#103068 = CARTESIAN_POINT('Ctrl Pts',(0.450000000818259,0.286907703536719,
0.550000000000001)) ;
#103069 = CARTESIAN_POINT('Ctrl Pts',(0.54999269605693,0.300543498469827,
0.549992696061056)) ;
#103070 = CARTESIAN_POINT('Ctrl Pts',(0.55,0.28690770353672,0.45000000081826)) ;
#103071 = CARTESIAN_POINT('Ctrl Pts',(0.455205501078185,0.273825167611082,
0.552602750539094)) ;
#103072 = CARTESIAN_POINT('Ctrl Pts',(0.546703256435901,0.299059401315788,
0.5467032564359)) ;
#103073 = CARTESIAN_POINT('Ctrl Pts',(0.552602750539093,0.273825167611082,
0.455205501078186)) ;
#103074 = CARTESIAN_POINT('Ctrl Pts',(0.4752426859173,0.2496381459159,0.56262134295865)) ;
#103075 = CARTESIAN_POINT('Ctrl Pts',(0.544986924117067,0.282072776439536,
0.544986924117069)) ;
#103076 = CARTESIAN_POINT('Ctrl Pts',(0.56262134295865,0.249638145915901,
0.475242685917301)) ;
#103077 = CARTESIAN_POINT('Ctrl Pts',(0.490066682942577,0.238545302291402,
0.570033341471289)) ;
#103078 = CARTESIAN_POINT('Ctrl Pts',(0.547116196858396,0.267914459835244,
0.547116196858399)) ;
#103079 = CARTESIAN_POINT('Ctrl Pts',(0.570033341471288,0.238545302291403,
0.490066682942577)) ;
#103080 = CARTESIAN_POINT('Ctrl Pts',(0.545602565402917,0.210777361061233,
0.597801282701458)) ;
#103081 = CARTESIAN_POINT('Ctrl Pts',(0.570853448890183,0.226374713859281,
0.57085344889018)) ;
#103082 = CARTESIAN_POINT('Ctrl Pts',(0.597801282701459,0.210777361061231,
0.545602565402918)) ;
#103083 = CARTESIAN_POINT('Ctrl Pts',(0.597493134347281,0.2,0.623746567173645)) ;
#103084 = CARTESIAN_POINT('Ctrl Pts',(0.610458667314981,0.2,0.610458667314981)) ;
#103085 = CARTESIAN_POINT('Ctrl Pts',(0.623746567173635,0.2,0.597493134347285)) ;
#103086 = CARTESIAN_POINT('Ctrl Pts',(0.65,0.2,0.650000000000001)) ;
#103087 = CARTESIAN_POINT('Ctrl Pts',(0.65,0.2,0.650000000000001)) ;
#103088 = CARTESIAN_POINT('Ctrl Pts',(0.65,0.2,0.650000000000001)) ;
#103089 = CARTESIAN_POINT('Ctrl Pts',(8.5,8.17221734381475,-0.540287291161696)) ;
#103090 = CARTESIAN_POINT('Ctrl Pts',(8.5,8.17221734381475,-0.625)) ;
#103091 = CARTESIAN_POINT('Ctrl Pts',(8.58356010126947,8.17221734381475,-0.638926683544911)) ;
#103092 = CARTESIAN_POINT('Ctrl Pts',(8.5,8.23335379241386,-0.540287292739054)) ;
#103093 = CARTESIAN_POINT('Ctrl Pts',(8.5,8.20847425960651,-0.617457567421702)) ;
#103094 = CARTESIAN_POINT('Ctrl Pts',(8.57460439031229,8.20580126077888,-0.637434065052048)) ;
#103095 = CARTESIAN_POINT('Ctrl Pts',(8.5,8.29192178062155,-0.567174115078498)) ;
#103096 = CARTESIAN_POINT('Ctrl Pts',(8.5,8.25010493984403,-0.629254608311669)) ;
#103097 = CARTESIAN_POINT('Ctrl Pts',(8.56800970738923,8.23725302684488,-0.649778363189931)) ;
#103098 = CARTESIAN_POINT('Ctrl Pts',(8.5,8.36583651094028,-0.656550623291365)) ;
#103099 = CARTESIAN_POINT('Ctrl Pts',(8.5,8.29925403146167,-0.683361437036636)) ;
#103100 = CARTESIAN_POINT('Ctrl Pts',(8.56373266208983,8.27563607377073,-0.693753776413148)) ;
#103101 = CARTESIAN_POINT('Ctrl Pts',(8.5,8.38029241321764,-0.71795520569968)) ;
#103102 = CARTESIAN_POINT('Ctrl Pts',(8.5,8.30669116589107,-0.724808849941012)) ;
#103103 = CARTESIAN_POINT('Ctrl Pts',(8.56610123859386,8.28208399509953,-0.724808702406988)) ;
#103104 = CARTESIAN_POINT('Ctrl Pts',(8.5,8.36719795478507,-0.776054723479883)) ;
#103105 = CARTESIAN_POINT('Ctrl Pts',(8.5,8.29381262650623,-0.759515149671807)) ;
#103106 = CARTESIAN_POINT('Ctrl Pts',(8.57227762885807,8.27346847343705,-0.754929987635437)) ;
#103107 = CARTESIAN_POINT('Ctrl Pts',(8.54852133092351,8.28383177029354,-0.755986532733631)) ;
#103108 = CARTESIAN_POINT('Ctrl Pts',(8.54913757890788,8.28625057716298,-0.742921659183987)) ;
#103109 = CARTESIAN_POINT('Ctrl Pts',(8.54914636139901,8.28675781111762,-0.729264789402619)) ;
#103110 = CARTESIAN_POINT('Ctrl Pts',(8.54883414737369,8.28489376483071,-0.716098869425042)) ;
#103111 = CARTESIAN_POINT('Ctrl Pts',(8.54852072231757,8.28302248819127,-0.702881880842787)) ;
#103112 = CARTESIAN_POINT('Ctrl Pts',(8.54791723678494,8.27865742078997,-0.689831295811734)) ;
#103113 = CARTESIAN_POINT('Ctrl Pts',(8.54677696932927,8.27237937104781,-0.678102076729669)) ;
#103114 = CARTESIAN_POINT('Ctrl Pts',(8.5454465495755,8.26505438658866,-0.664416879730159)) ;
#103115 = CARTESIAN_POINT('Ctrl Pts',(8.54324462275112,8.25487237915563,-0.652253753338803)) ;
#103116 = CARTESIAN_POINT('Ctrl Pts',(8.53884071267076,8.24480815719263,-0.64120716819918)) ;
#103117 = CARTESIAN_POINT('Ctrl Pts',(8.5342440055524,8.23430333763594,-0.629676978976814)) ;
#103118 = CARTESIAN_POINT('Ctrl Pts',(8.52670159721618,8.22420330618022,-0.618704260242989)) ;
#103119 = CARTESIAN_POINT('Ctrl Pts',(8.51928858688475,8.21729138318396,-0.605988175465276)) ;
#103120 = CARTESIAN_POINT('Ctrl Pts',(8.51327528614099,8.21168455548023,-0.595673116045033)) ;
#103121 = CARTESIAN_POINT('Ctrl Pts',(8.50759525524367,8.20778929846109,-0.58398494308279)) ;
#103122 = CARTESIAN_POINT('Ctrl Pts',(8.50412058850191,8.20498026622232,-0.571573948662816)) ;
#103123 = CARTESIAN_POINT('Ctrl Pts',(8.50147164778345,8.20283877743224,-0.562112325169396)) ;
#103124 = CARTESIAN_POINT('Ctrl Pts',(8.50000317248551,8.2012555848359,-0.552083357654996)) ;
#103125 = CARTESIAN_POINT('Ctrl Pts',(8.50000000513446,8.20000405629318,-0.542105238728424)) ;
#103126 = CARTESIAN_POINT('Origin',(8.6,8.17221734381475,-0.540287291161696)) ;
#103127 = CARTESIAN_POINT('Origin',(8.6,4.35421736843756,-0.540287291161696)) ;
#103128 = CARTESIAN_POINT('Origin',(8.6,6.66256607592813,-0.540287291161696)) ;
#103129 = CARTESIAN_POINT('Ctrl Pts',(8.5,6.47083593368087,-0.784808109924428)) ;
#103130 = CARTESIAN_POINT('Ctrl Pts',(8.5,6.55684090505321,-0.76438773869521)) ;
#103131 = CARTESIAN_POINT('Ctrl Pts',(8.58772778625753,6.56739561896918,-0.761881707090954)) ;
#103132 = CARTESIAN_POINT('Ctrl Pts',(8.5,6.45680686388583,-0.72572152971769)) ;
#103133 = CARTESIAN_POINT('Ctrl Pts',(8.5000000000001,6.54406229478621,-0.732510165403657)) ;
#103134 = CARTESIAN_POINT('Ctrl Pts',(8.58195196310366,6.55941415012444,-0.731357686877846)) ;
#103135 = CARTESIAN_POINT('Ctrl Pts',(8.5,6.4706155658439,-0.661952456804846)) ;
#103136 = CARTESIAN_POINT('Ctrl Pts',(8.5,6.54836369988887,-0.69239872740711)) ;
#103137 = CARTESIAN_POINT('Ctrl Pts',(8.57801125828726,6.56566601372231,-0.698834459202782)) ;
#103138 = CARTESIAN_POINT('Ctrl Pts',(8.5,6.54379299301796,-0.568626471658098)) ;
#103139 = CARTESIAN_POINT('Ctrl Pts',(8.5,6.59071789516225,-0.636226515292209)) ;
#103140 = CARTESIAN_POINT('Ctrl Pts',(8.57642058265787,6.60198961470444,-0.651906354024515)) ;
#103141 = CARTESIAN_POINT('Ctrl Pts',(8.5,6.60220518075381,-0.540287292974651)) ;
#103142 = CARTESIAN_POINT('Ctrl Pts',(8.5,6.62800697860325,-0.620917670762679)) ;
#103143 = CARTESIAN_POINT('Ctrl Pts',(8.57879135173926,6.63156920211805,-0.638131891956542)) ;
#103144 = CARTESIAN_POINT('Ctrl Pts',(8.5,6.66256607592813,-0.540287291161696)) ;
#103145 = CARTESIAN_POINT('Ctrl Pts',(8.5,6.66256607592813,-0.625)) ;
#103146 = CARTESIAN_POINT('Ctrl Pts',(8.58356010126947,6.66256607592813,-0.638926683544911)) ;
#103147 = CARTESIAN_POINT('',(8.54565366748554,6.61650711946996,-0.633965318291701)) ;
#103148 = CARTESIAN_POINT('Ctrl Pts',(8.54565366716104,6.61650712004131,-0.633965317813484)) ;
#103149 = CARTESIAN_POINT('Ctrl Pts',(8.54527684775569,6.61717057264361,-0.63341000086369)) ;
#103150 = CARTESIAN_POINT('Ctrl Pts',(8.54488909344004,6.61782772231432,-0.632855429899671)) ;
#103151 = CARTESIAN_POINT('Ctrl Pts',(8.54449064961561,6.61847724592616,-0.632300871385118)) ;
#103152 = CARTESIAN_POINT('Ctrl Pts',(8.54445329550707,6.61853813876477,-0.632248881524379)) ;
#103153 = CARTESIAN_POINT('Ctrl Pts',(8.54441584757977,6.6185989645223,-0.632196891791653)) ;
#103154 = CARTESIAN_POINT('Ctrl Pts',(8.544378306106,6.61865972207467,-0.632144901585903)) ;
#103155 = CARTESIAN_POINT('Ctrl Pts',(8.54363538409149,6.6198620755966,-0.631116048306817)) ;
#103156 = CARTESIAN_POINT('Ctrl Pts',(8.54285495000591,6.62104203503532,-0.630084862174671)) ;
#103157 = CARTESIAN_POINT('Ctrl Pts',(8.54204093171152,6.62218056960126,-0.629051115167204)) ;
#103158 = CARTESIAN_POINT('Ctrl Pts',(8.54157979215439,6.62282554690599,-0.628465499781785)) ;
#103159 = CARTESIAN_POINT('Ctrl Pts',(8.54110770812188,6.62345780120147,-0.627878649906638)) ;
#103160 = CARTESIAN_POINT('Ctrl Pts',(8.54062344907118,6.6240789244817,-0.627286954139643)) ;
#103161 = CARTESIAN_POINT('Ctrl Pts',(8.54011932596483,6.62472552591744,-0.62667098731849)) ;
#103162 = CARTESIAN_POINT('Ctrl Pts',(8.53960207832255,6.62535666566135,-0.626050990589038)) ;
#103163 = CARTESIAN_POINT('Ctrl Pts',(8.53907286520405,6.62597244099098,-0.625425228811039)) ;
#103164 = CARTESIAN_POINT('Ctrl Pts',(8.53887441028461,6.62620335673959,-0.62519056814429)) ;
#103165 = CARTESIAN_POINT('Ctrl Pts',(8.5386742766414,6.62643211299941,-0.624955099821045)) ;
#103166 = CARTESIAN_POINT('Ctrl Pts',(8.53847256319996,6.62665871795109,-0.624718764218343)) ;
#103167 = CARTESIAN_POINT('Ctrl Pts',(8.53842843838465,6.62670828778427,-0.624667065805252)) ;
#103168 = CARTESIAN_POINT('Ctrl Pts',(8.53838423811749,6.62675775467668,-0.624615326017445)) ;
#103169 = CARTESIAN_POINT('Ctrl Pts',(8.53833996369344,6.62680711871688,-0.62456354446014)) ;
#103170 = CARTESIAN_POINT('Ctrl Pts',(8.53829707284515,6.62685494013082,-0.624513381076501)) ;
#103171 = CARTESIAN_POINT('Ctrl Pts',(8.53825411240223,6.6269026650202,-0.624463178493077)) ;
#103172 = CARTESIAN_POINT('Ctrl Pts',(8.53821108363804,6.62695029346534,-0.624412936437729)) ;
#103173 = CARTESIAN_POINT('Ctrl Pts',(8.5380357143533,6.62714440934377,-0.624208168453412)) ;
#103174 = CARTESIAN_POINT('Ctrl Pts',(8.53785876035509,6.62733753498025,-0.62400218366478)) ;
#103175 = CARTESIAN_POINT('Ctrl Pts',(8.53767995296707,6.62753033615253,-0.623794466565225)) ;
#103176 = CARTESIAN_POINT('Ctrl Pts',(8.53649871780658,6.62880401687795,-0.622422248425076)) ;
#103177 = CARTESIAN_POINT('Ctrl Pts',(8.53528300832267,6.62998038079526,-0.621038076059647)) ;
#103178 = CARTESIAN_POINT('Ctrl Pts',(8.53403203676339,6.63110281535144,-0.619604486564905)) ;
#103179 = CARTESIAN_POINT('Ctrl Pts',(8.53346870389682,6.63160826591215,-0.618958917867875)) ;
#103180 = CARTESIAN_POINT('Ctrl Pts',(8.53289959536919,6.63209979040223,-0.618305425659429)) ;
#103181 = CARTESIAN_POINT('Ctrl Pts',(8.5323266134032,6.63257735344031,-0.617643701443846)) ;
#103182 = CARTESIAN_POINT('Ctrl Pts',(8.53206474273905,6.63279561467256,-0.617341272798442)) ;
#103183 = CARTESIAN_POINT('Ctrl Pts',(8.53180206199566,6.63301096017663,-0.617037126080686)) ;
#103184 = CARTESIAN_POINT('Ctrl Pts',(8.53153874718657,6.63322338883724,-0.616731238880717)) ;
#103185 = CARTESIAN_POINT('Ctrl Pts',(8.53007363658216,6.63440536369245,-0.615029251127047)) ;
#103186 = CARTESIAN_POINT('Ctrl Pts',(8.52858926277508,6.63549697414125,-0.613273083913089)) ;
#103187 = CARTESIAN_POINT('Ctrl Pts',(8.52711342564664,6.63649856635112,-0.61146113930632)) ;
#103188 = CARTESIAN_POINT('Ctrl Pts',(8.52634316954117,6.63702130866459,-0.610515464902798)) ;
#103189 = CARTESIAN_POINT('Ctrl Pts',(8.5255761534997,6.63751985710295,-0.609555719311186)) ;
#103190 = CARTESIAN_POINT('Ctrl Pts',(8.52481401823432,6.63799287689813,-0.608580326161291)) ;
#103191 = CARTESIAN_POINT('Ctrl Pts',(8.52460710835823,6.63812129566007,-0.608315519525312)) ;
#103192 = CARTESIAN_POINT('Ctrl Pts',(8.52440075574005,6.63824801482192,-0.608049753902253)) ;
#103193 = CARTESIAN_POINT('Ctrl Pts',(8.52419502810871,6.63837284070831,-0.607783086081022)) ;
#103194 = CARTESIAN_POINT('Ctrl Pts',(8.52404824365685,6.63846190263543,-0.607592821459237)) ;
#103195 = CARTESIAN_POINT('Ctrl Pts',(8.52390173612804,6.63855002749203,-0.607402043734724)) ;
#103196 = CARTESIAN_POINT('Ctrl Pts',(8.52375553261476,6.63863721305423,-0.607210762804845)) ;
#103197 = CARTESIAN_POINT('Ctrl Pts',(8.52294204127162,6.6391223224644,-0.606146456092442)) ;
#103198 = CARTESIAN_POINT('Ctrl Pts',(8.52213801365707,6.6395783474869,-0.60506653755636)) ;
#103199 = CARTESIAN_POINT('Ctrl Pts',(8.52134774490512,6.6400049409798,-0.603972961446361)) ;
#103200 = CARTESIAN_POINT('Ctrl Pts',(8.51876608595597,6.64139854145543,-0.600400454569433)) ;
#103201 = CARTESIAN_POINT('Ctrl Pts',(8.51630176076721,6.64256282842068,-0.596624566784401)) ;
#103202 = CARTESIAN_POINT('Ctrl Pts',(8.51404737801024,6.64354662431173,-0.592668758228679)) ;
#103203 = CARTESIAN_POINT('Ctrl Pts',(8.5117427137702,6.64455236266853,-0.58862471979261)) ;
#103204 = CARTESIAN_POINT('Ctrl Pts',(8.50965863261303,6.64536892721963,-0.584393778069628)) ;
#103205 = CARTESIAN_POINT('Ctrl Pts',(8.50786496313904,6.64606338785378,-0.580044165485977)) ;
#103206 = CARTESIAN_POINT('Ctrl Pts',(8.50767015284865,6.64613881316472,-0.579571754429886)) ;
#103207 = CARTESIAN_POINT('Ctrl Pts',(8.50747873128294,6.64621281334902,-0.579097973687544)) ;
#103208 = CARTESIAN_POINT('Ctrl Pts',(8.50729076020858,6.64628549377757,-0.578622930193838)) ;
#103209 = CARTESIAN_POINT('Ctrl Pts',(8.50722027105569,6.64631274893828,-0.578444788883699)) ;
#103210 = CARTESIAN_POINT('Ctrl Pts',(8.50715026706479,6.64633981850992,-0.578266470019251)) ;
#103211 = CARTESIAN_POINT('Ctrl Pts',(8.50708075128543,6.64636670806329,-0.578087979359469)) ;
#103212 = CARTESIAN_POINT('Ctrl Pts',(8.50659414082988,6.6465549349369,-0.576838544740993)) ;
#103213 = CARTESIAN_POINT('Ctrl Pts',(8.50613147592892,6.64673434010345,-0.575580683754983)) ;
#103214 = CARTESIAN_POINT('Ctrl Pts',(8.50569363751095,6.64690683932497,-0.574316427502283)) ;
#103215 = CARTESIAN_POINT('Ctrl Pts',(8.50395436040214,6.64759207829661,-0.569294273507268)) ;
#103216 = CARTESIAN_POINT('Ctrl Pts',(8.50258205288311,6.64816393978924,-0.564091559615236)) ;
#103217 = CARTESIAN_POINT('Ctrl Pts',(8.50162662717148,6.648647209875,-0.55880412474374)) ;
#103218 = CARTESIAN_POINT('Ctrl Pts',(8.50156399248221,6.64867889153406,-0.558457497228713)) ;
#103219 = CARTESIAN_POINT('Ctrl Pts',(8.50150313499581,6.64871019935922,-0.558110507516074)) ;
#103220 = CARTESIAN_POINT('Ctrl Pts',(8.50144406283925,6.64874114271687,-0.557763183502011)) ;
#103221 = CARTESIAN_POINT('Ctrl Pts',(8.50057491246573,6.64919642372275,-0.552652877493898)) ;
#103222 = CARTESIAN_POINT('Ctrl Pts',(8.50009537300581,6.64957062705847,-0.54747132905142)) ;
#103223 = CARTESIAN_POINT('Ctrl Pts',(8.50001293997571,6.64989933182544,-0.542314443541065)) ;
#103224 = CARTESIAN_POINT('Ctrl Pts',(8.5000043087827,6.64993374902791,-0.541774489179143)) ;
#103225 = CARTESIAN_POINT('Ctrl Pts',(8.5,6.64996765698295,-0.541234814428359)) ;
#103226 = CARTESIAN_POINT('Ctrl Pts',(8.5,6.65000108682384,-0.540695536105911)) ;
#103227 = CARTESIAN_POINT('',(8.55245136877623,6.600979943726,-0.646780119379722)) ;
#103228 = CARTESIAN_POINT('Ctrl Pts',(8.55238056475496,6.60105295171764,-0.64688861549872)) ;
#103229 = CARTESIAN_POINT('Ctrl Pts',(8.551705231719,6.6030854236859,-0.645102265614611)) ;
#103230 = CARTESIAN_POINT('Ctrl Pts',(8.55095829520337,6.60513808680195,-0.64336273482155)) ;
#103231 = CARTESIAN_POINT('Ctrl Pts',(8.55012599030481,6.60719152980482,-0.641654444180554)) ;
#103232 = CARTESIAN_POINT('Ctrl Pts',(8.54968322947851,6.60828389886605,-0.640745685650989)) ;
#103233 = CARTESIAN_POINT('Ctrl Pts',(8.54921644930856,6.60937569995297,-0.639846249123207)) ;
#103234 = CARTESIAN_POINT('Ctrl Pts',(8.54872481267401,6.61045954913285,-0.638955746549559)) ;
#103235 = CARTESIAN_POINT('Ctrl Pts',(8.54779539897823,6.61250851009536,-0.637272297372044)) ;
#103236 = CARTESIAN_POINT('Ctrl Pts',(8.54677348694556,6.61453549290059,-0.635615590886287)) ;
#103237 = CARTESIAN_POINT('Ctrl Pts',(8.54565366748553,6.61650711946996,-0.6339653182917)) ;
#103238 = CARTESIAN_POINT('',(8.55735473176754,6.58264207262424,-0.664955797361829)) ;
#103239 = CARTESIAN_POINT('Ctrl Pts',(8.55735473168708,6.5826420730276,-0.664955796844377)) ;
#103240 = CARTESIAN_POINT('Ctrl Pts',(8.55706916598062,6.58397660851238,-0.663229693371652)) ;
#103241 = CARTESIAN_POINT('Ctrl Pts',(8.55678088122713,6.58528501693225,-0.661662100960593)) ;
#103242 = CARTESIAN_POINT('Ctrl Pts',(8.55647408091831,6.58661569125855,-0.660171823251799)) ;
#103243 = CARTESIAN_POINT('Ctrl Pts',(8.55614409617588,6.58804692262372,-0.658568927518812)) ;
#103244 = CARTESIAN_POINT('Ctrl Pts',(8.55579261555197,6.58950524590079,-0.657056795017548)) ;
#103245 = CARTESIAN_POINT('Ctrl Pts',(8.55539993844513,6.59102291080503,-0.655587567779556)) ;
#103246 = CARTESIAN_POINT('Ctrl Pts',(8.55517214917315,6.59190329771229,-0.654735279227253)) ;
#103247 = CARTESIAN_POINT('Ctrl Pts',(8.5549304988197,6.59280308289125,-0.653898397754101)) ;
#103248 = CARTESIAN_POINT('Ctrl Pts',(8.55467134659055,6.5937211373212,-0.653070794642137)) ;
#103249 = CARTESIAN_POINT('Ctrl Pts',(8.55434805237174,6.59486641664498,-0.65203835397031)) ;
#103250 = CARTESIAN_POINT('Ctrl Pts',(8.55400737519031,6.59602723165027,-0.65103619819577)) ;
#103251 = CARTESIAN_POINT('Ctrl Pts',(8.55365328858765,6.59718920061515,-0.650045215513273)) ;
#103252 = CARTESIAN_POINT('Ctrl Pts',(8.55328167888691,6.598408673298,-0.649005190911051)) ;
#103253 = CARTESIAN_POINT('Ctrl Pts',(8.55289390107695,6.5996354646002,-0.647973679676364)) ;
#103254 = CARTESIAN_POINT('Ctrl Pts',(8.55249886556666,6.60083562835443,-0.646908149434967)) ;
#103255 = CARTESIAN_POINT('Ctrl Pts',(8.55248304763322,6.60088368507309,-0.64686548368468)) ;
#103256 = CARTESIAN_POINT('Ctrl Pts',(8.55246721522814,6.60093179017207,-0.646822806733157)) ;
#103257 = CARTESIAN_POINT('Ctrl Pts',(8.55245136877623,6.600979943726,-0.646780119379722)) ;
#103258 = CARTESIAN_POINT('Ctrl Pts',(8.56107669735261,6.56009388000089,-0.762383847222383)) ;
#103259 = CARTESIAN_POINT('Ctrl Pts',(8.56115635543004,6.5597817052481,-0.760820734383275)) ;
#103260 = CARTESIAN_POINT('Ctrl Pts',(8.56122592915387,6.55950119162287,-0.759250712980609)) ;
#103261 = CARTESIAN_POINT('Ctrl Pts',(8.56128584055879,6.55925348717443,-0.757693391948652)) ;
#103262 = CARTESIAN_POINT('Ctrl Pts',(8.56142626445293,6.55867290283846,-0.754043250811132)) ;
#103263 = CARTESIAN_POINT('Ctrl Pts',(8.56152217534692,6.55825854507372,-0.750375633877455)) ;
#103264 = CARTESIAN_POINT('Ctrl Pts',(8.56158081746989,6.55798577878939,-0.746670135426049)) ;
#103265 = CARTESIAN_POINT('Ctrl Pts',(8.5615891784535,6.55794688875065,-0.746141818743938)) ;
#103266 = CARTESIAN_POINT('Ctrl Pts',(8.56159677639835,6.55791088241233,-0.7456126452602)) ;
#103267 = CARTESIAN_POINT('Ctrl Pts',(8.56160362608006,6.55787769947535,-0.745082467472401)) ;
#103268 = CARTESIAN_POINT('Ctrl Pts',(8.56164117305277,6.55769580506316,-0.742176263686379)) ;
#103269 = CARTESIAN_POINT('Ctrl Pts',(8.56164095204357,6.55766773657215,-0.739264011996683)) ;
#103270 = CARTESIAN_POINT('Ctrl Pts',(8.56161306230089,6.55774920537473,-0.736365567258155)) ;
#103271 = CARTESIAN_POINT('Ctrl Pts',(8.56157759693122,6.55785280336172,-0.732679824607675)) ;
#103272 = CARTESIAN_POINT('Ctrl Pts',(8.56150275624661,6.55813669070953,-0.729004928020692)) ;
#103273 = CARTESIAN_POINT('Ctrl Pts',(8.56141108129146,6.55856506509341,-0.725363292547789)) ;
#103274 = CARTESIAN_POINT('Ctrl Pts',(8.56136615997221,6.55877497130415,-0.723578867680741)) ;
#103275 = CARTESIAN_POINT('Ctrl Pts',(8.56131707129299,6.55902016312283,-0.721801670968291)) ;
#103276 = CARTESIAN_POINT('Ctrl Pts',(8.56126585691694,6.55929956116443,-0.720031525468218)) ;
#103277 = CARTESIAN_POINT('Ctrl Pts',(8.56116752027495,6.55983603289963,-0.716632671909467)) ;
#103278 = CARTESIAN_POINT('Ctrl Pts',(8.56104954130218,6.56049109659199,-0.713254007575518)) ;
#103279 = CARTESIAN_POINT('Ctrl Pts',(8.56091150449777,6.56129147625798,-0.709830471024781)) ;
#103280 = CARTESIAN_POINT('Ctrl Pts',(8.56080235670744,6.56192434857303,-0.707123428861444)) ;
#103281 = CARTESIAN_POINT('Ctrl Pts',(8.56068045333715,6.56264902401856,-0.704387266689058)) ;
#103282 = CARTESIAN_POINT('Ctrl Pts',(8.56054379825318,6.56349285586908,-0.701623487720724)) ;
#103283 = CARTESIAN_POINT('Ctrl Pts',(8.56050762866484,6.56371619955873,-0.70089197635173)) ;
#103284 = CARTESIAN_POINT('Ctrl Pts',(8.56047042218819,6.56394794674723,-0.700158791698164)) ;
#103285 = CARTESIAN_POINT('Ctrl Pts',(8.56043213901762,6.56418871538691,-0.699424623470902)) ;
#103286 = CARTESIAN_POINT('Ctrl Pts',(8.56026887460242,6.56521550994361,-0.696293651179561)) ;
#103287 = CARTESIAN_POINT('Ctrl Pts',(8.56008532870549,6.56636514336248,-0.693261214935318)) ;
#103288 = CARTESIAN_POINT('Ctrl Pts',(8.55988915918716,6.56762686151788,-0.690471327667742)) ;
#103289 = CARTESIAN_POINT('Ctrl Pts',(8.55964574654531,6.56919243680243,-0.687009557276224)) ;
#103290 = CARTESIAN_POINT('Ctrl Pts',(8.55938661160135,6.57080906160851,-0.683732634051197)) ;
#103291 = CARTESIAN_POINT('Ctrl Pts',(8.55911582090258,6.57246439798287,-0.680667212427968)) ;
#103292 = CARTESIAN_POINT('Ctrl Pts',(8.55888928658552,6.5738491962672,-0.678102784635318)) ;
#103293 = CARTESIAN_POINT('Ctrl Pts',(8.55863813502891,6.57544444689331,-0.675365345431122)) ;
#103294 = CARTESIAN_POINT('Ctrl Pts',(8.55834707044209,6.57718152485399,-0.672668125822793)) ;
#103295 = CARTESIAN_POINT('Ctrl Pts',(8.55828762047113,6.5775363232011,-0.672117218448187)) ;
#103296 = CARTESIAN_POINT('Ctrl Pts',(8.55822651695173,6.57789694345781,-0.671567846579033)) ;
#103297 = CARTESIAN_POINT('Ctrl Pts',(8.5581636495887,6.57826264684151,-0.671021571079284)) ;
#103298 = CARTESIAN_POINT('Ctrl Pts',(8.55792499569725,6.57965091145826,-0.668947827764096)) ;
#103299 = CARTESIAN_POINT('Ctrl Pts',(8.55766032614236,6.58110993502766,-0.66692131328784)) ;
#103300 = CARTESIAN_POINT('Ctrl Pts',(8.55735473176754,6.58264207262424,-0.664955797361829)) ;
#103301 = CARTESIAN_POINT('Origin',(8.49172374697018,6.65,-2.54)) ;
#103302 = CARTESIAN_POINT('Origin',(8.49226931273351,6.63793757405409,-0.772988271638203)) ;
#103303 = CARTESIAN_POINT('Ctrl Pts',(8.40188506081764,6.5500005341705,-0.511545830815321)) ;
#103304 = CARTESIAN_POINT('Ctrl Pts',(8.50280744587445,6.54966497091124,-0.525195040754151)) ;
#103305 = CARTESIAN_POINT('Ctrl Pts',(8.50109204799973,6.65199687180768,-0.525680454939853)) ;
#103306 = CARTESIAN_POINT('Ctrl Pts',(8.39296932930791,6.55000052027914,-0.569675802422008)) ;
#103307 = CARTESIAN_POINT('Ctrl Pts',(8.49725036372774,6.54968051003369,-0.556913602683179)) ;
#103308 = CARTESIAN_POINT('Ctrl Pts',(8.4966529651636,6.64935672317807,-0.556024711463538)) ;
#103309 = CARTESIAN_POINT('Ctrl Pts',(8.41146079558551,6.55000052635931,-0.629608884645994)) ;
#103310 = CARTESIAN_POINT('Ctrl Pts',(8.50278789772746,6.54967384197884,-0.581014351980562)) ;
#103311 = CARTESIAN_POINT('Ctrl Pts',(8.5059095425555,6.65051247736751,-0.584427212093591)) ;
#103312 = CARTESIAN_POINT('Ctrl Pts',(8.45744515914178,6.55000045243509,-0.682802191882288)) ;
#103313 = CARTESIAN_POINT('Ctrl Pts',(8.52023811680815,6.54973725194856,-0.621633015820999)) ;
#103314 = CARTESIAN_POINT('Ctrl Pts',(8.52891723073134,6.6364300977738,-0.613475163078278)) ;
#103315 = CARTESIAN_POINT('Ctrl Pts',(8.46608867121686,6.55000043643008,-0.69119509917481)) ;
#103316 = CARTESIAN_POINT('Ctrl Pts',(8.5233427016762,6.54974993059826,-0.628470240078956)) ;
#103317 = CARTESIAN_POINT('Ctrl Pts',(8.53324349789235,6.63337968978885,-0.618220891300047)) ;
#103318 = CARTESIAN_POINT('Ctrl Pts',(8.48465388181692,6.55000038323734,-0.70657631387452)) ;
#103319 = CARTESIAN_POINT('Ctrl Pts',(8.53001210036432,6.54978938646811,-0.645124595123328)) ;
#103320 = CARTESIAN_POINT('Ctrl Pts',(8.54253954944039,6.62323710347992,-0.62886314626903)) ;
#103321 = CARTESIAN_POINT('Ctrl Pts',(8.4946704807492,6.55000035131511,-0.713488494461478)) ;
#103322 = CARTESIAN_POINT('Ctrl Pts',(8.53347884787446,6.54981166882493,-0.653059031150021)) ;
#103323 = CARTESIAN_POINT('Ctrl Pts',(8.54755337534736,6.61714793548866,-0.632867688126296)) ;
#103324 = CARTESIAN_POINT('Ctrl Pts',(8.50997930894014,6.55000022766094,-0.723388902785886)) ;
#103325 = CARTESIAN_POINT('Ctrl Pts',(8.53869035159219,6.54988741100164,-0.678774232755077)) ;
#103326 = CARTESIAN_POINT('Ctrl Pts',(8.55523846583767,6.59353839814603,-0.653527883108543)) ;
#103327 = CARTESIAN_POINT('Ctrl Pts',(8.51532901080113,6.55000016113069,-0.726338967319371)) ;
#103328 = CARTESIAN_POINT('Ctrl Pts',(8.54023459682693,6.54992340374043,-0.688489748387105)) ;
#103329 = CARTESIAN_POINT('Ctrl Pts',(8.55790835982317,6.58082417519527,-0.661582308572545)) ;
#103330 = CARTESIAN_POINT('Ctrl Pts',(8.52186010906351,6.55000005932357,-0.732792759877374)) ;
#103331 = CARTESIAN_POINT('Ctrl Pts',(8.54265823247975,6.5499732773141,-0.71793164411612)) ;
#103332 = CARTESIAN_POINT('Ctrl Pts',(8.56121746518605,6.56135337205696,-0.70458837007694)) ;
#103333 = CARTESIAN_POINT('Ctrl Pts',(8.5235499393997,6.55000003603139,-0.735824262228055)) ;
#103334 = CARTESIAN_POINT('Ctrl Pts',(8.5435076996824,6.54998394755847,-0.731423873201171)) ;
#103335 = CARTESIAN_POINT('Ctrl Pts',(8.56214310615443,6.55689632415127,-0.727450133563353)) ;
#103336 = CARTESIAN_POINT('Ctrl Pts',(8.52268461318103,6.55000004733862,-0.741787530415828)) ;
#103337 = CARTESIAN_POINT('Ctrl Pts',(8.54305517585919,6.54997881410036,-0.752813412140242)) ;
#103338 = CARTESIAN_POINT('Ctrl Pts',(8.56153259171388,6.55906016573932,-0.762790181581043)) ;
#103339 = CARTESIAN_POINT('Ctrl Pts',(8.52060566253918,6.55000006807331,-0.74441380654971)) ;
#103340 = CARTESIAN_POINT('Ctrl Pts',(8.54195943530534,6.54996919659462,-0.760494574886098)) ;
#103341 = CARTESIAN_POINT('Ctrl Pts',(8.56058441628597,6.56302742363398,-0.774507921514082)) ;
#103342 = CARTESIAN_POINT('Ctrl Pts',(8.51445291480377,6.55000012130567,-0.751232814955295)) ;
#103343 = CARTESIAN_POINT('Ctrl Pts',(8.53868948987834,6.54994355920608,-0.779419181767537)) ;
#103344 = CARTESIAN_POINT('Ctrl Pts',(8.55750149922672,6.57320954252663,-0.801184435306907)) ;
#103345 = CARTESIAN_POINT('Ctrl Pts',(8.50953280296009,6.55000015625148,-0.755047946437262)) ;
#103346 = CARTESIAN_POINT('Ctrl Pts',(8.53616288920966,6.54992588038504,-0.787764748526664)) ;
#103347 = CARTESIAN_POINT('Ctrl Pts',(8.55504783006515,6.57989127253972,-0.810699316792922)) ;
#103348 = CARTESIAN_POINT('Ctrl Pts',(8.49261655785708,6.55000026291039,-0.768492606568883)) ;
#103349 = CARTESIAN_POINT('Ctrl Pts',(8.52778251455087,6.54986718408744,-0.815769160894697)) ;
#103350 = CARTESIAN_POINT('Ctrl Pts',(8.5465866761693,6.60027178071331,-0.839353375743825)) ;
#103351 = CARTESIAN_POINT('Ctrl Pts',(8.4802216582452,6.55000031608562,-0.777768534160336)) ;
#103352 = CARTESIAN_POINT('Ctrl Pts',(8.52288681814197,6.5498343726202,-0.827455948929167)) ;
#103353 = CARTESIAN_POINT('Ctrl Pts',(8.54045339450475,6.61042388759294,-0.846301990960487)) ;
#103354 = CARTESIAN_POINT('Ctrl Pts',(8.46952991654748,6.55000035836672,-0.789095446218494)) ;
#103355 = CARTESIAN_POINT('Ctrl Pts',(8.51900842894086,6.54980714069604,-0.843367684676165)) ;
#103356 = CARTESIAN_POINT('Ctrl Pts',(8.53471369258652,6.61849392543648,-0.861383368442905)) ;
#103357 = CARTESIAN_POINT('Origin',(8.4,6.65,-0.540678001899701)) ;
#103358 = CARTESIAN_POINT('Ctrl Pts',(8.54848814460235,8.28374914930622,0.75646282522011)) ;
#103359 = CARTESIAN_POINT('Ctrl Pts',(8.55964225199693,8.27720012980426,0.755032051677707)) ;
#103360 = CARTESIAN_POINT('Ctrl Pts',(8.572140519951,8.27365818248462,0.754258237443071)) ;
#103361 = CARTESIAN_POINT('Ctrl Pts',(8.54519582228992,8.29111303851995,0.732039621192373)) ;
#103362 = CARTESIAN_POINT('Ctrl Pts',(8.55569959891144,8.28406912459879,0.731962382559104)) ;
#103363 = CARTESIAN_POINT('Ctrl Pts',(8.56757951573637,8.27991709749369,0.731808366088123)) ;
#103364 = CARTESIAN_POINT('Ctrl Pts',(8.54340782920287,8.28927570119138,0.706177006876757)) ;
#103365 = CARTESIAN_POINT('Ctrl Pts',(8.5535505383751,8.28232618564302,0.707845355710233)) ;
#103366 = CARTESIAN_POINT('Ctrl Pts',(8.56507848568419,8.27803412520749,0.708867856946723)) ;
#103367 = CARTESIAN_POINT('Ctrl Pts',(8.54340835145922,8.27841951799441,0.684464988838289)) ;
#103368 = CARTESIAN_POINT('Ctrl Pts',(8.55355093564017,8.27219257320284,0.687578461234078)) ;
#103369 = CARTESIAN_POINT('Ctrl Pts',(8.56507848521152,8.26835005667905,0.689499719495969)) ;
#103370 = CARTESIAN_POINT('Ctrl Pts',(8.54742026180266,8.27608084857564,0.685634358751393)) ;
#103371 = CARTESIAN_POINT('Ctrl Pts',(8.54754672558908,8.27683897030433,0.687325426963469)) ;
#103372 = CARTESIAN_POINT('Ctrl Pts',(8.54766225486892,8.27755642830995,0.689034502691608)) ;
#103373 = CARTESIAN_POINT('Ctrl Pts',(8.54776713596767,8.27823455672262,0.690764983222443)) ;
#103374 = CARTESIAN_POINT('Ctrl Pts',(8.54791712013337,8.27920430747292,0.693239639588089)) ;
#103375 = CARTESIAN_POINT('Ctrl Pts',(8.54806168001142,8.28008011045347,0.695753662732336)) ;
#103376 = CARTESIAN_POINT('Ctrl Pts',(8.54818998754193,8.28086237513953,0.69828131614101)) ;
#103377 = CARTESIAN_POINT('Ctrl Pts',(8.5482419492675,8.28117917511832,0.699304960133263)) ;
#103378 = CARTESIAN_POINT('Ctrl Pts',(8.54829140719363,8.28148078264965,0.700331325709524)) ;
#103379 = CARTESIAN_POINT('Ctrl Pts',(8.54833813644415,8.28176759858569,0.701360370022629)) ;
#103380 = CARTESIAN_POINT('Ctrl Pts',(8.54850061324771,8.2827648526819,0.704938339470869)) ;
#103381 = CARTESIAN_POINT('Ctrl Pts',(8.54863339756396,8.28360845633781,0.708649876470984)) ;
#103382 = CARTESIAN_POINT('Ctrl Pts',(8.54873421749657,8.28426438239343,0.712386913242184)) ;
#103383 = CARTESIAN_POINT('Ctrl Pts',(8.54878752953696,8.28461122607273,0.714363001205664)) ;
#103384 = CARTESIAN_POINT('Ctrl Pts',(8.54883168679925,8.28490640714037,0.716345917925883)) ;
#103385 = CARTESIAN_POINT('Ctrl Pts',(8.54886500248132,8.28515040605082,0.718318140970176)) ;
#103386 = CARTESIAN_POINT('Ctrl Pts',(8.5488738542235,8.28521523484357,0.718842146748514)) ;
#103387 = CARTESIAN_POINT('Ctrl Pts',(8.54888411330031,8.285275121517,0.719364990807687)) ;
#103388 = CARTESIAN_POINT('Ctrl Pts',(8.54889386083024,8.28533143086091,0.719887913213841)) ;
#103389 = CARTESIAN_POINT('Ctrl Pts',(8.54894969070932,8.28565394783544,0.722882999653076)) ;
#103390 = CARTESIAN_POINT('Ctrl Pts',(8.5489793513821,8.2858668042412,0.725901363617001)) ;
#103391 = CARTESIAN_POINT('Ctrl Pts',(8.54899968230029,8.28595875954338,0.728932422198607)) ;
#103392 = CARTESIAN_POINT('Ctrl Pts',(8.54900356561228,8.2859763234883,0.729511370282527)) ;
#103393 = CARTESIAN_POINT('Ctrl Pts',(8.54900713937599,8.28598945835117,0.730090691195829)) ;
#103394 = CARTESIAN_POINT('Ctrl Pts',(8.5490105728891,8.28599806377621,0.730670159781498)) ;
#103395 = CARTESIAN_POINT('Ctrl Pts',(8.54902784271198,8.28604134718936,0.733584760524092)) ;
#103396 = CARTESIAN_POINT('Ctrl Pts',(8.54901619593281,8.28598556136224,0.736484224278308)) ;
#103397 = CARTESIAN_POINT('Ctrl Pts',(8.54898431260111,8.28582669412324,0.739393571324556)) ;
#103398 = CARTESIAN_POINT('Ctrl Pts',(8.54893914418925,8.28560163041441,0.743515179030308)) ;
#103399 = CARTESIAN_POINT('Ctrl Pts',(8.54884805310403,8.28517290646446,0.747622900033123)) ;
#103400 = CARTESIAN_POINT('Ctrl Pts',(8.54869940582914,8.28455561418427,0.751692922585911)) ;
#103401 = CARTESIAN_POINT('Ctrl Pts',(8.54864697316337,8.28433787538056,0.753128550197273)) ;
#103402 = CARTESIAN_POINT('Ctrl Pts',(8.54858736435355,8.28409676597419,0.754559160407532)) ;
#103403 = CARTESIAN_POINT('Ctrl Pts',(8.54851996240545,8.28383343043592,0.755982796914733)) ;
#103404 = CARTESIAN_POINT('Origin',(8.4,6.65,-2.54)) ;
#103405 = CARTESIAN_POINT('Origin',(8.4,6.65,0.540678001899701)) ;
#103406 = CARTESIAN_POINT('Origin',(8.49172374697018,6.65,-2.54)) ;
#103407 = CARTESIAN_POINT('Origin',(8.49225485638824,6.63809817984101,0.772991371636644)) ;
#103408 = CARTESIAN_POINT('Origin',(8.6,4.35421736843756,0.540287291161696)) ;
#103409 = CARTESIAN_POINT('Origin',(8.6,6.66256607592813,0.540287291161696)) ;
#103410 = CARTESIAN_POINT('Ctrl Pts',(8.5013487493624,6.65217253603379,0.524014743919239)) ;
#103411 = CARTESIAN_POINT('Ctrl Pts',(8.50315244876578,6.54997127577019,0.523413630741524)) ;
#103412 = CARTESIAN_POINT('Ctrl Pts',(8.40269444133659,6.55000000392138,0.508403503424183)) ;
#103413 = CARTESIAN_POINT('Ctrl Pts',(8.49631753783951,6.64933701877088,0.554984347604346)) ;
#103414 = CARTESIAN_POINT('Ctrl Pts',(8.49707874924866,6.54997270174419,0.55603877650159)) ;
#103415 = CARTESIAN_POINT('Ctrl Pts',(8.39261127161987,6.55000000381175,0.567444979189231)) ;
#103416 = CARTESIAN_POINT('Ctrl Pts',(8.50556246021204,6.65075235208953,0.583988954498525)) ;
#103417 = CARTESIAN_POINT('Ctrl Pts',(8.502539579467,6.54997202229483,0.580355869545521)) ;
#103418 = CARTESIAN_POINT('Ctrl Pts',(8.41103525938982,6.55000000386643,0.628661650365513)) ;
#103419 = CARTESIAN_POINT('Ctrl Pts',(8.52891970071471,6.63645479210452,0.613472841517229)) ;
#103420 = CARTESIAN_POINT('Ctrl Pts',(8.52027792490145,6.54997752826667,0.621595060038875)) ;
#103421 = CARTESIAN_POINT('Ctrl Pts',(8.4576425585103,6.5500000033157,0.682609898416985)) ;
#103422 = CARTESIAN_POINT('Ctrl Pts',(8.53324635448928,6.63340383613799,0.618217934261831)) ;
#103423 = CARTESIAN_POINT('Ctrl Pts',(8.52338394863778,6.54997861189313,0.62842668610914)) ;
#103424 = CARTESIAN_POINT('Ctrl Pts',(8.46627109069292,6.55000000319828,0.69099525146731)) ;
#103425 = CARTESIAN_POINT('Ctrl Pts',(8.5425433201124,6.62325922024828,0.62885825178222)) ;
#103426 = CARTESIAN_POINT('Ctrl Pts',(8.53005572430512,6.54998198465676,0.645067357531962)) ;
#103427 = CARTESIAN_POINT('Ctrl Pts',(8.48480454940901,6.55000000280808,0.706372191176904)) ;
#103428 = CARTESIAN_POINT('Ctrl Pts',(8.54755771953122,6.61716872587346,0.632861456122815)) ;
#103429 = CARTESIAN_POINT('Ctrl Pts',(8.53352383957147,6.54998388968238,0.652993385085483)) ;
#103430 = CARTESIAN_POINT('Ctrl Pts',(8.49480263348501,6.55000000257396,0.71328272370085)) ;
#103431 = CARTESIAN_POINT('Ctrl Pts',(8.55524400651031,6.59355301617591,0.653519430104509)) ;
#103432 = CARTESIAN_POINT('Ctrl Pts',(8.5387355250133,6.54999036710749,0.67870514119052)) ;
#103433 = CARTESIAN_POINT('Ctrl Pts',(8.51008526949052,6.55000000166752,0.723224250581485)) ;
#103434 = CARTESIAN_POINT('Ctrl Pts',(8.55791451833569,6.5808349442903,0.661572932536089)) ;
#103435 = CARTESIAN_POINT('Ctrl Pts',(8.54027978136634,6.54999344602542,0.688420971165681)) ;
#103436 = CARTESIAN_POINT('Ctrl Pts',(8.51542462880457,6.55000000118004,0.72619365566139)) ;
#103437 = CARTESIAN_POINT('Ctrl Pts',(8.56122429319342,6.56135755929244,0.704583461036361)) ;
#103438 = CARTESIAN_POINT('Ctrl Pts',(8.54270214007072,6.54999771321877,0.717900094355645)) ;
#103439 = CARTESIAN_POINT('Ctrl Pts',(8.52194436340203,6.55000000043436,0.732732556326117)) ;
#103440 = CARTESIAN_POINT('Ctrl Pts',(8.56215003896756,6.55689889598544,0.727448655243819)) ;
#103441 = CARTESIAN_POINT('Ctrl Pts',(8.54355112280983,6.54999862629018,0.731414585978538)) ;
#103442 = CARTESIAN_POINT('Ctrl Pts',(8.52363168464777,6.55000000026381,0.735806239205465)) ;
#103443 = CARTESIAN_POINT('Ctrl Pts',(8.56153943432816,6.55906352913392,0.762793876209075)) ;
#103444 = CARTESIAN_POINT('Ctrl Pts',(8.54309854033143,6.5499981870035,0.752836831731517)) ;
#103445 = CARTESIAN_POINT('Ctrl Pts',(8.52276767133745,6.5500000003466,0.74183248681998)) ;
#103446 = CARTESIAN_POINT('Ctrl Pts',(8.56059123720041,6.56303220640811,0.774513053537472)) ;
#103447 = CARTESIAN_POINT('Ctrl Pts',(8.54200379397877,6.54999736403672,0.760527952934338)) ;
#103448 = CARTESIAN_POINT('Ctrl Pts',(8.52069177703238,6.55000000049844,0.744478656263915)) ;
#103449 = CARTESIAN_POINT('Ctrl Pts',(8.55750819780171,6.5732178281489,0.801192185467493)) ;
#103450 = CARTESIAN_POINT('Ctrl Pts',(8.53873610184732,6.54999517041881,0.779473140357088)) ;
#103451 = CARTESIAN_POINT('Ctrl Pts',(8.5145479773404,6.55000000088831,0.751343369175894)) ;
#103452 = CARTESIAN_POINT('Ctrl Pts',(8.55505442469282,6.57990173798307,0.810707325538746)) ;
#103453 = CARTESIAN_POINT('Ctrl Pts',(8.53621107118181,6.54999365791211,0.787823339593337)) ;
#103454 = CARTESIAN_POINT('Ctrl Pts',(8.50963525726154,6.55000000114429,0.755173817084272)) ;
#103455 = CARTESIAN_POINT('Ctrl Pts',(8.55022399280472,6.59153973477785,0.82706479408145)) ;
#103456 = CARTESIAN_POINT('Ctrl Pts',(8.53156015545167,6.54999086985381,0.803378832820653)) ;
#103457 = CARTESIAN_POINT('Ctrl Pts',(8.49999539447557,6.55000000159032,0.762872176320595)) ;
#103458 = CARTESIAN_POINT('Ctrl Pts',(8.54779538881608,6.59665349532938,0.833083808301692)) ;
#103459 = CARTESIAN_POINT('Ctrl Pts',(8.52936575151139,6.54998957391998,0.810004452644074)) ;
#103460 = CARTESIAN_POINT('Ctrl Pts',(8.49512741158074,6.55000000178643,0.766663584101366)) ;
#103461 = CARTESIAN_POINT('Ctrl Pts',(8.54538355337155,6.60121171185026,0.838324825515742)) ;
#103462 = CARTESIAN_POINT('Ctrl Pts',(8.5273341553617,6.54998837980796,0.816101642790049)) ;
#103463 = CARTESIAN_POINT('Ctrl Pts',(8.49033880598513,6.55000000196131,0.770551402901284)) ;
#103464 = CARTESIAN_POINT('',(8.54582344182383,6.61635369861666,0.633936348427079)) ;
#103465 = CARTESIAN_POINT('Ctrl Pts',(8.54582344182383,6.61635369861666,0.633936348427079)) ;
#103466 = CARTESIAN_POINT('Ctrl Pts',(8.5449359516352,6.61793460914653,0.632605923790104)) ;
#103467 = CARTESIAN_POINT('Ctrl Pts',(8.54398448171071,6.61948114927953,0.631282607169297)) ;
#103468 = CARTESIAN_POINT('Ctrl Pts',(8.54296332801272,6.6209780844369,0.629959263220174)) ;
#103469 = CARTESIAN_POINT('Ctrl Pts',(8.53827263106763,6.62785429629763,0.623880447238088)) ;
#103470 = CARTESIAN_POINT('Ctrl Pts',(8.53198779426187,6.63349037496299,0.617388431475615)) ;
#103471 = CARTESIAN_POINT('Ctrl Pts',(8.5259873730411,6.63731070037229,0.6099294107578)) ;
#103472 = CARTESIAN_POINT('Ctrl Pts',(8.52000560405467,6.64111915034781,0.602493576312632)) ;
#103473 = CARTESIAN_POINT('Ctrl Pts',(8.51430181273566,6.64349626850742,0.593962352698589)) ;
#103474 = CARTESIAN_POINT('Ctrl Pts',(8.50998586672548,6.64522349213896,0.584799013029946)) ;
#103475 = CARTESIAN_POINT('Ctrl Pts',(8.50534188065424,6.64708199603772,0.574939199749866)) ;
#103476 = CARTESIAN_POINT('Ctrl Pts',(8.50212992821339,6.64824261275105,0.564112456325158)) ;
#103477 = CARTESIAN_POINT('Ctrl Pts',(8.50077314609738,6.64911992656046,0.553175088083247)) ;
#103478 = CARTESIAN_POINT('Ctrl Pts',(8.50025986706873,6.64945181977648,0.549037414332315)) ;
#103479 = CARTESIAN_POINT('Ctrl Pts',(8.50000017127792,6.64974165917873,0.544856744898765)) ;
#103480 = CARTESIAN_POINT('Ctrl Pts',(8.5000000000847,6.64999974464545,0.540682132504374)) ;
#103481 = CARTESIAN_POINT('',(8.55242393572495,6.6010617218254,0.646757901283908)) ;
#103482 = CARTESIAN_POINT('Ctrl Pts',(8.55241775170035,6.60106807917175,0.64676718384559)) ;
#103483 = CARTESIAN_POINT('Ctrl Pts',(8.55072388788562,6.60619026743357,0.642278523047584)) ;
#103484 = CARTESIAN_POINT('Ctrl Pts',(8.54858294048571,6.61143812822771,0.638073075855162)) ;
#103485 = CARTESIAN_POINT('Ctrl Pts',(8.54582344182383,6.61635369861666,0.633936348427079)) ;
#103486 = CARTESIAN_POINT('Ctrl Pts',(8.55635360773812,6.58637108369506,0.661367609266196)) ;
#103487 = CARTESIAN_POINT('Ctrl Pts',(8.55606387390183,6.58765239867385,0.659887617192456)) ;
#103488 = CARTESIAN_POINT('Ctrl Pts',(8.55575324501782,6.58896823902363,0.658434058666365)) ;
#103489 = CARTESIAN_POINT('Ctrl Pts',(8.55541196992768,6.59037241127509,0.656956795059579)) ;
#103490 = CARTESIAN_POINT('Ctrl Pts',(8.55524290008379,6.59106804711318,0.656224949300535)) ;
#103491 = CARTESIAN_POINT('Ctrl Pts',(8.55506631250719,6.59178496983024,0.655488041162307)) ;
#103492 = CARTESIAN_POINT('Ctrl Pts',(8.55488049708425,6.59252693597571,0.654743722380964)) ;
#103493 = CARTESIAN_POINT('Ctrl Pts',(8.55445908016384,6.59420966544518,0.653055657291086)) ;
#103494 = CARTESIAN_POINT('Ctrl Pts',(8.55403589309458,6.5958403790653,0.651511622277546)) ;
#103495 = CARTESIAN_POINT('Ctrl Pts',(8.55359592981647,6.59737680581848,0.650096843766778)) ;
#103496 = CARTESIAN_POINT('Ctrl Pts',(8.55324292160434,6.59860957066091,0.648961684408028)) ;
#103497 = CARTESIAN_POINT('Ctrl Pts',(8.55287861047125,6.59978201473819,0.647908957492877)) ;
#103498 = CARTESIAN_POINT('Ctrl Pts',(8.55248933155915,6.60087815532545,0.646922873013271)) ;
#103499 = CARTESIAN_POINT('Ctrl Pts',(8.55246754857565,6.60093949235549,0.646867694422083)) ;
#103500 = CARTESIAN_POINT('Ctrl Pts',(8.5524457495603,6.6010006820315,0.646812703721496)) ;
#103501 = CARTESIAN_POINT('Ctrl Pts',(8.55242393572495,6.6010617218254,0.646757901283908)) ;
#103502 = CARTESIAN_POINT('Ctrl Pts',(8.5,6.66256607592813,0.540287291161697)) ;
#103503 = CARTESIAN_POINT('Ctrl Pts',(8.5,6.66256607592813,0.625)) ;
#103504 = CARTESIAN_POINT('Ctrl Pts',(8.58356010126947,6.66256607592813,0.638926683544911)) ;
#103505 = CARTESIAN_POINT('Ctrl Pts',(8.5,6.61011302719823,0.540287292737137)) ;
#103506 = CARTESIAN_POINT('Ctrl Pts',(8.5,6.63245216822983,0.621442763400598)) ;
#103507 = CARTESIAN_POINT('Ctrl Pts',(8.57941760042979,6.63563981885128,0.638236266738299)) ;
#103508 = CARTESIAN_POINT('Ctrl Pts',(8.5,6.55934573373324,0.561153090057277)) ;
#103509 = CARTESIAN_POINT('Ctrl Pts',(8.5,6.60054351783569,0.631918604172277)) ;
#103510 = CARTESIAN_POINT('Ctrl Pts',(8.57705842698408,6.60987578993432,0.648272471952291)) ;
#103511 = CARTESIAN_POINT('Ctrl Pts',(8.5,6.52274941072028,0.597749410720281)) ;
#103512 = CARTESIAN_POINT('Ctrl Pts',(8.5,6.57873105977929,0.653731059779292)) ;
#103513 = CARTESIAN_POINT('Ctrl Pts',(8.57705842661295,6.59157413088145,0.66657413088145)) ;
#103514 = CARTESIAN_POINT('Origin',(8.49172374697003,1.4,-2.54)) ;
#103515 = CARTESIAN_POINT('Origin',(8.49172374697003,1.4,1.96214168703487)) ;
#103516 = CARTESIAN_POINT('Origin',(8.49172374697002,1.4,1.96214168703487)) ;
#103517 = CARTESIAN_POINT('Origin',(8.49172374697003,1.4,1.96214168703486)) ;
#103518 = CARTESIAN_POINT('Ctrl Pts',(8.50816364570057,1.49863939238321,1.96214168703488)) ;
#103519 = CARTESIAN_POINT('Ctrl Pts',(8.51019246767907,1.4983012553868,1.92707241592901)) ;
#103520 = CARTESIAN_POINT('Ctrl Pts',(8.50816364570057,1.47636598119991,1.89970798904169)) ;
#103521 = CARTESIAN_POINT('Ctrl Pts',(8.97755831131118,1.42040694811478,1.99005134884688)) ;
#103522 = CARTESIAN_POINT('Ctrl Pts',(8.97879997398668,1.42020000433584,1.95543332681748)) ;
#103523 = CARTESIAN_POINT('Ctrl Pts',(8.97755831689155,1.39869563385799,1.92830518304939)) ;
#103524 = CARTESIAN_POINT('Ctrl Pts',(9.4469849630597,1.34216917282336,2.01736862936927)) ;
#103525 = CARTESIAN_POINT('Ctrl Pts',(9.44827639615878,1.34195393397319,1.98322247139131)) ;
#103526 = CARTESIAN_POINT('Ctrl Pts',(9.44698496887878,1.3209776491576,1.95627701528915)) ;
#103527 = CARTESIAN_POINT('Ctrl Pts',(9.91643989873053,1.26392668354489,2.04416188017823)) ;
#103528 = CARTESIAN_POINT('Ctrl Pts',(9.91830968165731,1.26361505305709,2.01049065580299)) ;
#103529 = CARTESIAN_POINT('Ctrl Pts',(9.91643989873053,1.24322097942674,1.98369643580598)) ;
#103530 = CARTESIAN_POINT('Origin',(9.9,1.16528729116168,2.0441618801782)) ;
#103531 = CARTESIAN_POINT('Origin',(9.9,1.16528729116168,2.0441618801782)) ;
#103532 = CARTESIAN_POINT('Origin',(-0.4,-3.36847777691809,-0.4)) ;
#103533 = CARTESIAN_POINT('Origin',(-0.400000000000001,-3.36847777691809,
-0.4)) ;
#103534 = CARTESIAN_POINT('Origin',(-0.4,-3.36847777691809,-0.4)) ;
#103535 = CARTESIAN_POINT('Origin',(-0.400000000000001,-3.36847777691809,
0.5)) ;
#103536 = CARTESIAN_POINT('Origin',(-0.4,-3.36847777691809,0.4)) ;
#103537 = CARTESIAN_POINT('Origin',(-1.11032778078669,-3.36847777691809,-0.4)) ;
#103538 = CARTESIAN_POINT('Origin',(0.4,-3.36847777691809,-0.4)) ;
#103539 = CARTESIAN_POINT('Origin',(-0.400000000000001,-3.36847777691809,
0.4)) ;
#103540 = CARTESIAN_POINT('Origin',(-0.4,-3.36847777691809,0.4)) ;
#103541 = CARTESIAN_POINT('Origin',(0.400000000000001,-3.36847777691809,-0.4)) ;
#103542 = CARTESIAN_POINT('Origin',(0.400000000000001,-3.36847777691809,-0.4)) ;
#103543 = CARTESIAN_POINT('Origin',(1.5,-3.36847777691809,0.4)) ;
#103544 = CARTESIAN_POINT('Origin',(0.4,-3.36847777691809,0.4)) ;
#103545 = CARTESIAN_POINT('Origin',(0.4,-3.36847777691809,0.5)) ;
#103546 = CARTESIAN_POINT('Origin',(0.4,-3.36847777691809,0.4)) ;
#103547 = CARTESIAN_POINT('Origin',(0.4,-3.36847777691809,0.4)) ;
#103548 = CARTESIAN_POINT('Origin',(7.96847777691809,3.4,-0.4)) ;
#103549 = CARTESIAN_POINT('Origin',(7.96847777691809,3.4,-0.4)) ;
#103550 = CARTESIAN_POINT('Origin',(7.96847777691809,3.4,-0.4)) ;
#103551 = CARTESIAN_POINT('Origin',(7.96847777691809,3.4,0.5)) ;
#103552 = CARTESIAN_POINT('Origin',(7.96847777691809,3.4,0.4)) ;
#103553 = CARTESIAN_POINT('Origin',(7.96847777691809,2.68967221921331,-0.4)) ;
#103554 = CARTESIAN_POINT('Origin',(7.96847777691809,4.2,-0.4)) ;
#103555 = CARTESIAN_POINT('Origin',(7.96847777691809,3.4,0.4)) ;
#103556 = CARTESIAN_POINT('Origin',(7.96847777691809,3.4,0.4)) ;
#103557 = CARTESIAN_POINT('Origin',(7.96847777691809,4.2,-0.4)) ;
#103558 = CARTESIAN_POINT('Origin',(7.96847777691809,4.2,-0.4)) ;
#103559 = CARTESIAN_POINT('Origin',(7.96847777691809,2.3,0.4)) ;
#103560 = CARTESIAN_POINT('Origin',(7.96847777691809,4.2,0.4)) ;
#103561 = CARTESIAN_POINT('Origin',(7.96847777691809,4.2,0.5)) ;
#103562 = CARTESIAN_POINT('Origin',(7.96847777691809,4.2,0.4)) ;
#103563 = CARTESIAN_POINT('Origin',(7.96847777691809,4.2,0.4)) ;
#103564 = CARTESIAN_POINT('Origin',(8.49172374697003,1.4,-2.54)) ;
#103565 = CARTESIAN_POINT('Origin',(8.49172374697003,1.4,-1.96214168703487)) ;
#103566 = CARTESIAN_POINT('Origin',(8.49172374697002,1.4,-1.96214168703487)) ;
#103567 = CARTESIAN_POINT('Origin',(8.49172374697003,1.39999999999989,-1.96214168703472)) ;
#103568 = CARTESIAN_POINT('Ctrl Pts',(8.50816364570058,1.47636598119991,-1.89970798904169)) ;
#103569 = CARTESIAN_POINT('Ctrl Pts',(8.51019246767908,1.4983012553868,-1.92707241592901)) ;
#103570 = CARTESIAN_POINT('Ctrl Pts',(8.50816364570058,1.49863939238321,-1.96214168703488)) ;
#103571 = CARTESIAN_POINT('Ctrl Pts',(8.97755831689156,1.39869563385799,-1.92830518304939)) ;
#103572 = CARTESIAN_POINT('Ctrl Pts',(8.9787999739867,1.42020000433584,-1.95543332681749)) ;
#103573 = CARTESIAN_POINT('Ctrl Pts',(8.97755831131119,1.42040694811478,-1.99005134884688)) ;
#103574 = CARTESIAN_POINT('Ctrl Pts',(9.44698496887878,1.32097764915769,-1.95627701528927)) ;
#103575 = CARTESIAN_POINT('Ctrl Pts',(9.44827639615882,1.34195393397354,-1.98322247139135)) ;
#103576 = CARTESIAN_POINT('Ctrl Pts',(9.44698496305968,1.34216917282336,-2.0173686293693)) ;
#103577 = CARTESIAN_POINT('Ctrl Pts',(9.91643989873053,1.24322097942674,-1.98369643580598)) ;
#103578 = CARTESIAN_POINT('Ctrl Pts',(9.91830968165732,1.26361505305709,-2.01049065580299)) ;
#103579 = CARTESIAN_POINT('Ctrl Pts',(9.91643989873053,1.26392668354489,-2.04416188017823)) ;
#103580 = CARTESIAN_POINT('Origin',(9.9,1.16528729116168,-2.0441618801782)) ;
#103581 = CARTESIAN_POINT('Origin',(9.9,1.16528729116168,-2.04416188017819)) ;
#103582 = CARTESIAN_POINT('Origin',(8.48377223398316,8.2,-2.54)) ;
#103583 = CARTESIAN_POINT('Origin',(8.48238054867376,8.20007133352901,0.74682106876079)) ;
#103584 = CARTESIAN_POINT('Ctrl Pts',(8.4020166297015,8.3,0.514024022078609)) ;
#103585 = CARTESIAN_POINT('Ctrl Pts',(8.50299337454956,8.3,0.527325188736439)) ;
#103586 = CARTESIAN_POINT('Ctrl Pts',(8.50100123624932,8.19773961376455,0.527311153882261)) ;
#103587 = CARTESIAN_POINT('Ctrl Pts',(8.39454129798958,8.3,0.565501818649352)) ;
#103588 = CARTESIAN_POINT('Ctrl Pts',(8.49697875237674,8.3,0.554625888665333)) ;
#103589 = CARTESIAN_POINT('Ctrl Pts',(8.49727262260755,8.20135231978535,0.554932936037724)) ;
#103590 = CARTESIAN_POINT('Ctrl Pts',(8.40820218948343,8.3,0.617974636475715)) ;
#103591 = CARTESIAN_POINT('Ctrl Pts',(8.49818669687003,8.3,0.577528272198747)) ;
#103592 = CARTESIAN_POINT('Ctrl Pts',(8.50412619268404,8.20300739730711,0.579611589975179)) ;
#103593 = CARTESIAN_POINT('Ctrl Pts',(8.44304134766321,8.3,0.669003066912872)) ;
#103594 = CARTESIAN_POINT('Ctrl Pts',(8.5089417438721,8.3,0.619144944619423)) ;
#103595 = CARTESIAN_POINT('Ctrl Pts',(8.52157716465942,8.21896555381604,0.609833873349667)) ;
#103596 = CARTESIAN_POINT('Ctrl Pts',(8.44963266995284,8.3,0.677332168021774)) ;
#103597 = CARTESIAN_POINT('Ctrl Pts',(8.51095981317519,8.3,0.626250559516498)) ;
#103598 = CARTESIAN_POINT('Ctrl Pts',(8.52487915500778,8.22226238914487,0.615048381948129)) ;
#103599 = CARTESIAN_POINT('Ctrl Pts',(8.46372306360151,8.3,0.693045273680071)) ;
#103600 = CARTESIAN_POINT('Ctrl Pts',(8.51547368264943,8.3,0.642367208944066)) ;
#103601 = CARTESIAN_POINT('Ctrl Pts',(8.53193863144478,8.23129792829963,0.626682521614473)) ;
#103602 = CARTESIAN_POINT('Ctrl Pts',(8.47128983770083,8.3,0.700441372853609)) ;
#103603 = CARTESIAN_POINT('Ctrl Pts',(8.51796237042372,8.3,0.650753505087224)) ;
#103604 = CARTESIAN_POINT('Ctrl Pts',(8.53572833262715,8.23677343862354,0.632570411492244)) ;
#103605 = CARTESIAN_POINT('Ctrl Pts',(8.48287565264707,8.3,0.711269205166843)) ;
#103606 = CARTESIAN_POINT('Ctrl Pts',(8.52168214469875,8.3,0.669256480570013)) ;
#103607 = CARTESIAN_POINT('Ctrl Pts',(8.54153766811345,8.25077321967987,0.647955012892664)) ;
#103608 = CARTESIAN_POINT('Ctrl Pts',(8.48680760428677,8.3,0.714812702597994)) ;
#103609 = CARTESIAN_POINT('Ctrl Pts',(8.52287759291298,8.3,0.675856495068285)) ;
#103610 = CARTESIAN_POINT('Ctrl Pts',(8.54350322705384,8.25646917637537,0.653737733396524)) ;
#103611 = CARTESIAN_POINT('Ctrl Pts',(8.49230810302881,8.3,0.720504650004493)) ;
#103612 = CARTESIAN_POINT('Ctrl Pts',(8.52426411271139,8.3,0.691433475366392)) ;
#103613 = CARTESIAN_POINT('Ctrl Pts',(8.54627296401924,8.26866384868896,0.671447430638399)) ;
#103614 = CARTESIAN_POINT('Ctrl Pts',(8.49410170711668,8.3,0.722473481065998)) ;
#103615 = CARTESIAN_POINT('Ctrl Pts',(8.52463604790915,8.3,0.697594474634863)) ;
#103616 = CARTESIAN_POINT('Ctrl Pts',(8.54716490137965,8.27360757863442,0.679204040517475)) ;
#103617 = CARTESIAN_POINT('Ctrl Pts',(8.49698869685298,8.3,0.726926721190466)) ;
#103618 = CARTESIAN_POINT('Ctrl Pts',(8.52523118911551,8.3,0.713407065561665)) ;
#103619 = CARTESIAN_POINT('Ctrl Pts',(8.54862931231184,8.28262305001769,0.702158650729551)) ;
#103620 = CARTESIAN_POINT('Ctrl Pts',(8.49798687771249,8.3,0.729483478843415)) ;
#103621 = CARTESIAN_POINT('Ctrl Pts',(8.52551930315387,8.3,0.723093723956201)) ;
#103622 = CARTESIAN_POINT('Ctrl Pts',(8.54912969489066,8.28574379441723,0.717618102506755)) ;
#103623 = CARTESIAN_POINT('Ctrl Pts',(8.49821791151748,8.3,0.737420429062632)) ;
#103624 = CARTESIAN_POINT('Ctrl Pts',(8.52559423327562,8.3,0.747810875295178)) ;
#103625 = CARTESIAN_POINT('Ctrl Pts',(8.54922875625408,8.28635135062007,0.756761329953168)) ;
#103626 = CARTESIAN_POINT('Ctrl Pts',(8.49537847603514,8.3,0.742353089154235)) ;
#103627 = CARTESIAN_POINT('Ctrl Pts',(8.52439331053439,8.3,0.758526725017863)) ;
#103628 = CARTESIAN_POINT('Ctrl Pts',(8.5478189041853,8.28040548672881,0.771528206627957)) ;
#103629 = CARTESIAN_POINT('Ctrl Pts',(8.48955273785443,8.3,0.751088596543062)) ;
#103630 = CARTESIAN_POINT('Ctrl Pts',(8.52168703568128,8.3,0.775947414871858)) ;
#103631 = CARTESIAN_POINT('Ctrl Pts',(8.54489815533717,8.27194212599121,0.793832992292969)) ;
#103632 = CARTESIAN_POINT('Ctrl Pts',(8.48620077197361,8.3,0.755173692495235)) ;
#103633 = CARTESIAN_POINT('Ctrl Pts',(8.52012703453237,8.3,0.782892667106739)) ;
#103634 = CARTESIAN_POINT('Ctrl Pts',(8.54324008387896,8.26788967346962,0.801685764361643)) ;
#103635 = CARTESIAN_POINT('Ctrl Pts',(8.48280151347419,8.3,0.759208890359289)) ;
#103636 = CARTESIAN_POINT('Ctrl Pts',(8.51858761497412,8.3,0.7893479742148)) ;
#103637 = CARTESIAN_POINT('Ctrl Pts',(8.54152015125556,8.26408224232382,0.808661774965266)) ;
#103638 = CARTESIAN_POINT('Origin',(8.4,8.2,0.542072889850983)) ;
#103639 = CARTESIAN_POINT('Origin',(8.4,8.2,-0.625)) ;
#103640 = CARTESIAN_POINT('Origin',(8.4,8.2,-0.542072889850983)) ;
#103641 = CARTESIAN_POINT('Ctrl Pts',(8.50101530037395,8.19768718256763,-0.527201774581488)) ;
#103642 = CARTESIAN_POINT('Ctrl Pts',(8.50305639000872,8.3,-0.52721981135723)) ;
#103643 = CARTESIAN_POINT('Ctrl Pts',(8.40204633857705,8.3,-0.513820202125374)) ;
#103644 = CARTESIAN_POINT('Ctrl Pts',(8.4972546444163,8.20131038948434,-0.554867911909504)) ;
#103645 = CARTESIAN_POINT('Ctrl Pts',(8.49701391805274,8.3,-0.554560942340225)) ;
#103646 = CARTESIAN_POINT('Ctrl Pts',(8.39450526457596,8.3,-0.565363291070999)) ;
#103647 = CARTESIAN_POINT('Ctrl Pts',(8.50410935041313,8.20295267265882,-0.579579296811489)) ;
#103648 = CARTESIAN_POINT('Ctrl Pts',(8.498207495215,8.3,-0.577464337890648)) ;
#103649 = CARTESIAN_POINT('Ctrl Pts',(8.40816401923485,8.3,-0.617918729043422)) ;
#103650 = CARTESIAN_POINT('Ctrl Pts',(8.52158236570989,8.21893216789649,-0.60983004077578)) ;
#103651 = CARTESIAN_POINT('Ctrl Pts',(8.50896456566522,8.3,-0.619127678384042)) ;
#103652 = CARTESIAN_POINT('Ctrl Pts',(8.4430413476632,8.3,-0.669003066912864)) ;
#103653 = CARTESIAN_POINT('Ctrl Pts',(8.5248849650705,8.222229916312,-0.615043706178146)) ;
#103654 = CARTESIAN_POINT('Ctrl Pts',(8.51098076140207,8.3,-0.626233110976269)) ;
#103655 = CARTESIAN_POINT('Ctrl Pts',(8.44963266995283,8.3,-0.677332168021764)) ;
#103656 = CARTESIAN_POINT('Ctrl Pts',(8.53194575580938,8.23126818558571,-0.626675734966566)) ;
#103657 = CARTESIAN_POINT('Ctrl Pts',(8.51549074202138,8.3,-0.642350503135092)) ;
#103658 = CARTESIAN_POINT('Ctrl Pts',(8.46372306360151,8.3,-0.693045273680065)) ;
#103659 = CARTESIAN_POINT('Ctrl Pts',(8.53573618291038,8.23674548871789,-0.632562377027298)) ;
#103660 = CARTESIAN_POINT('Ctrl Pts',(8.51797743940285,8.3,-0.650737462558641)) ;
#103661 = CARTESIAN_POINT('Ctrl Pts',(8.47128983770083,8.3,-0.700441372853603)) ;
#103662 = CARTESIAN_POINT('Ctrl Pts',(8.54154687836688,8.25075037830457,-0.647945131945504)) ;
#103663 = CARTESIAN_POINT('Ctrl Pts',(8.52169408444523,8.3,-0.669243554349282)) ;
#103664 = CARTESIAN_POINT('Ctrl Pts',(8.48287565264705,8.3,-0.711269205166832)) ;
#103665 = CARTESIAN_POINT('Ctrl Pts',(8.54351297666181,8.25644859419422,-0.65372727801617)) ;
#103666 = CARTESIAN_POINT('Ctrl Pts',(8.52288848488737,8.3,-0.675844731548773)) ;
#103667 = CARTESIAN_POINT('Ctrl Pts',(8.48680760428675,8.3,-0.714812702597982)) ;
#103668 = CARTESIAN_POINT('Ctrl Pts',(8.54628376412584,8.268648468274,-0.671437623160067)) ;
#103669 = CARTESIAN_POINT('Ctrl Pts',(8.52427341038692,8.3,-0.691425017040316)) ;
#103670 = CARTESIAN_POINT('Ctrl Pts',(8.4923081030288,8.3,-0.720504650004482)) ;
#103671 = CARTESIAN_POINT('Ctrl Pts',(8.54717611873857,8.27359443500938,-0.679194883718743)) ;
#103672 = CARTESIAN_POINT('Ctrl Pts',(8.52464480444821,8.3,-0.697587339914159)) ;
#103673 = CARTESIAN_POINT('Ctrl Pts',(8.49410170711666,8.3,-0.722473481065988)) ;
#103674 = CARTESIAN_POINT('Ctrl Pts',(8.54864126180654,8.28261417405719,-0.702152906124747)) ;
#103675 = CARTESIAN_POINT('Ctrl Pts',(8.52523908688553,8.3,-0.71340328490623)) ;
#103676 = CARTESIAN_POINT('Ctrl Pts',(8.49698869685298,8.3,-0.726926721190451)) ;
#103677 = CARTESIAN_POINT('Ctrl Pts',(8.54914185487159,8.28573645090423,-0.717615282415987)) ;
#103678 = CARTESIAN_POINT('Ctrl Pts',(8.52552693815803,8.3,-0.723091952016155)) ;
#103679 = CARTESIAN_POINT('Ctrl Pts',(8.49798687771249,8.3,-0.7294834788434)) ;
#103680 = CARTESIAN_POINT('Ctrl Pts',(8.54924094958849,8.28634430798887,-0.756765947598448)) ;
#103681 = CARTESIAN_POINT('Ctrl Pts',(8.52560181204939,8.30000000000001,-0.74781375175313)) ;
#103682 = CARTESIAN_POINT('Ctrl Pts',(8.49821791151748,8.3,-0.737420429062617)) ;
#103683 = CARTESIAN_POINT('Ctrl Pts',(8.54783079466743,8.28039553911298,-0.771534805981169)) ;
#103684 = CARTESIAN_POINT('Ctrl Pts',(8.52440147378976,8.3,-0.758531275432198)) ;
#103685 = CARTESIAN_POINT('Ctrl Pts',(8.49537847603514,8.3,-0.742353089154222)) ;
#103686 = CARTESIAN_POINT('Ctrl Pts',(8.54465883986931,8.27120119512632,-0.795757194703311)) ;
#103687 = CARTESIAN_POINT('Ctrl Pts',(8.52145785975948,8.3,-0.777490278330103)) ;
#103688 = CARTESIAN_POINT('Ctrl Pts',(8.48905244827038,8.3,-0.751838764714472)) ;
#103689 = CARTESIAN_POINT('Ctrl Pts',(8.54267599402788,8.26648669506706,-0.804294990430303)) ;
#103690 = CARTESIAN_POINT('Ctrl Pts',(8.51958784692422,8.3,-0.78526413214459)) ;
#103691 = CARTESIAN_POINT('Ctrl Pts',(8.48503640902804,8.3,-0.756568597065939)) ;
#103692 = CARTESIAN_POINT('Ctrl Pts',(8.54064021294342,8.26212437554838,-0.812200029823916)) ;
#103693 = CARTESIAN_POINT('Ctrl Pts',(8.51779796763701,8.3,-0.792689517015178)) ;
#103694 = CARTESIAN_POINT('Ctrl Pts',(8.48104783026777,8.3,-0.761284807495046)) ;
#103695 = CARTESIAN_POINT('Origin',(8.48238054717662,8.2000713259188,-0.746821067394115)) ;
#103696 = CARTESIAN_POINT('Origin',(8.48377223398316,8.2,-2.54)) ;
#103697 = CARTESIAN_POINT('Ctrl Pts',(8.55305389383868,6.58518362856711,-4.41981637143289)) ;
#103698 = CARTESIAN_POINT('Ctrl Pts',(8.56447181517253,6.58947636230805,-4.41552363769195)) ;
#103699 = CARTESIAN_POINT('Ctrl Pts',(8.57705842661295,6.59157413088145,-4.41342586911855)) ;
#103700 = CARTESIAN_POINT('Ctrl Pts',(8.55305102515197,6.55898702014115,-4.39362045977753)) ;
#103701 = CARTESIAN_POINT('Ctrl Pts',(8.56446969712851,6.56479854221783,-4.39084652309121)) ;
#103702 = CARTESIAN_POINT('Ctrl Pts',(8.57705842709767,6.56766897765924,-4.38952071573476)) ;
#103703 = CARTESIAN_POINT('Ctrl Pts',(8.55608440539073,6.54967077654144,-4.35347242603462)) ;
#103704 = CARTESIAN_POINT('Ctrl Pts',(8.56803673427363,6.55578248257735,-4.35313112423482)) ;
#103705 = CARTESIAN_POINT('Ctrl Pts',(8.58110225049762,6.55837193275,-4.35326484665044)) ;
#103706 = CARTESIAN_POINT('Ctrl Pts',(8.56106007075016,6.56033186051354,-4.3169784615962)) ;
#103707 = CARTESIAN_POINT('Ctrl Pts',(8.57385418571952,6.56560017282095,-4.31820388376166)) ;
#103708 = CARTESIAN_POINT('Ctrl Pts',(8.58763814880121,6.56727264871055,-4.31859290569255)) ;
#103709 = CARTESIAN_POINT('',(8.56104219912065,6.56017369985344,-4.3176338509444)) ;
#103710 = CARTESIAN_POINT('',(8.55704445183396,6.58320973295706,-4.41483164119205)) ;
#103711 = CARTESIAN_POINT('Ctrl Pts',(8.56104219912065,6.56017369985344,-4.3176338509444)) ;
#103712 = CARTESIAN_POINT('Ctrl Pts',(8.56172006948825,6.55755272988493,-4.33050998342623)) ;
#103713 = CARTESIAN_POINT('Ctrl Pts',(8.56178854742204,6.55691761311389,-4.34401886345913)) ;
#103714 = CARTESIAN_POINT('Ctrl Pts',(8.56147572200372,6.55855061087387,-4.35707103715452)) ;
#103715 = CARTESIAN_POINT('Ctrl Pts',(8.56116227470662,6.56018685493862,-4.37014915781354)) ;
#103716 = CARTESIAN_POINT('Ctrl Pts',(8.5604843297899,6.56417103596015,-4.3831290791339)) ;
#103717 = CARTESIAN_POINT('Ctrl Pts',(8.55945615587251,6.57017322470283,-4.39482221269648)) ;
#103718 = CARTESIAN_POINT('Ctrl Pts',(8.55883284154061,6.57381195760859,-4.40191099175523)) ;
#103719 = CARTESIAN_POINT('Ctrl Pts',(8.5580718554171,6.57823677723142,-4.40863504839524)) ;
#103720 = CARTESIAN_POINT('Ctrl Pts',(8.55704487707428,6.58320791316494,-4.41483246211937)) ;
#103721 = CARTESIAN_POINT('',(8.5563540329117,6.58636921675996,-4.41863023217439)) ;
#103722 = CARTESIAN_POINT('Origin',(8.54420290866466,6.62817328219149,-4.38194114231836)) ;
#103723 = CARTESIAN_POINT('',(8.57705842661295,6.59157413088145,-4.41342586911855)) ;
#103724 = CARTESIAN_POINT('Origin',(8.6,6.52274941072028,-4.48225058927972)) ;
#103725 = CARTESIAN_POINT('',(8.58355189313842,6.56397635572684,-4.342433776426)) ;
#103726 = CARTESIAN_POINT('Origin',(8.59777129281767,6.65641294721993,-4.34088223593214)) ;
#103727 = CARTESIAN_POINT('Ctrl Pts',(8.56104311409706,6.5601737548033,-4.31763480937229)) ;
#103728 = CARTESIAN_POINT('Ctrl Pts',(8.56569547918975,6.56094902085081,-4.32312238616956)) ;
#103729 = CARTESIAN_POINT('Ctrl Pts',(8.57049938306349,6.56176641478981,-4.32850925134764)) ;
#103730 = CARTESIAN_POINT('Ctrl Pts',(8.57538893105739,6.56259599225632,-4.33378626613879)) ;
#103731 = CARTESIAN_POINT('Ctrl Pts',(8.5780877379385,6.56305388107913,-4.33669893697213)) ;
#103732 = CARTESIAN_POINT('Ctrl Pts',(8.58081254036875,6.5635152101042,-4.33957937936776)) ;
#103733 = CARTESIAN_POINT('Ctrl Pts',(8.58355195315297,6.56397636517831,-4.3424336197205)) ;
#103734 = CARTESIAN_POINT('Ctrl Pts',(8.5,8.3521616921714,-4.43240609825021)) ;
#103735 = CARTESIAN_POINT('Ctrl Pts',(8.5,8.2900428850829,-4.40134669470595)) ;
#103736 = CARTESIAN_POINT('Ctrl Pts',(8.56507848521152,8.26835005667905,-4.39050028050403)) ;
#103737 = CARTESIAN_POINT('Ctrl Pts',(8.5,8.31945293993532,-4.49782359726859)) ;
#103738 = CARTESIAN_POINT('Ctrl Pts',(8.5,8.26922013491181,-4.44299218879635)) ;
#103739 = CARTESIAN_POINT('Ctrl Pts',(8.56507848600996,8.25199117628908,-4.42321804061861)) ;
#103740 = CARTESIAN_POINT('Ctrl Pts',(8.5,8.24922766844395,-4.53971270685138)) ;
#103741 = CARTESIAN_POINT('Ctrl Pts',(8.5,8.21777561643094,-4.46447736982275)) ;
#103742 = CARTESIAN_POINT('Ctrl Pts',(8.57228151929423,8.21451202732349,-4.44295308011763)) ;
#103743 = CARTESIAN_POINT('Ctrl Pts',(8.5,8.17221734381475,-4.5397127088383)) ;
#103744 = CARTESIAN_POINT('Ctrl Pts',(8.5,8.17221734381474,-4.455)) ;
#103745 = CARTESIAN_POINT('Ctrl Pts',(8.58356010126947,8.17221734381475,-4.44107331645509)) ;
#103746 = CARTESIAN_POINT('',(8.50000000249538,8.20000280433619,-4.53790474363842)) ;
#103747 = CARTESIAN_POINT('',(8.54742025481396,8.27608084305204,-4.39436566195595)) ;
#103748 = CARTESIAN_POINT('Ctrl Pts',(8.50000000249538,8.20000280433619,-4.53790474363842)) ;
#103749 = CARTESIAN_POINT('Ctrl Pts',(8.50000274011724,8.2015414376578,-4.52563544845108)) ;
#103750 = CARTESIAN_POINT('Ctrl Pts',(8.50225788919788,8.20358050335012,-4.51326647497958)) ;
#103751 = CARTESIAN_POINT('Ctrl Pts',(8.50614710304112,8.20657022673326,-4.50191598101389)) ;
#103752 = CARTESIAN_POINT('Ctrl Pts',(8.51002595055128,8.20955198129041,-4.49059574072047)) ;
#103753 = CARTESIAN_POINT('Ctrl Pts',(8.51564213392183,8.21362262975068,-4.48004613352066)) ;
#103754 = CARTESIAN_POINT('Ctrl Pts',(8.52129493663065,8.21921832196825,-4.47062179223395)) ;
#103755 = CARTESIAN_POINT('Ctrl Pts',(8.52933132065201,8.22717351408127,-4.45722354898551)) ;
#103756 = CARTESIAN_POINT('Ctrl Pts',(8.53683691159804,8.23885362788864,-4.44566244344335)) ;
#103757 = CARTESIAN_POINT('Ctrl Pts',(8.54097226482464,8.25011947738646,-4.43288116961709)) ;
#103758 = CARTESIAN_POINT('Ctrl Pts',(8.54447125915462,8.25965170869904,-4.42206671140824)) ;
#103759 = CARTESIAN_POINT('Ctrl Pts',(8.54617119150717,8.26873789958222,-4.40993961018965)) ;
#103760 = CARTESIAN_POINT('Ctrl Pts',(8.54724932284106,8.27506683274844,-4.39656646025132)) ;
#103761 = CARTESIAN_POINT('Ctrl Pts',(8.54730817192851,8.27541229338911,-4.39583649568633)) ;
#103762 = CARTESIAN_POINT('Ctrl Pts',(8.5473651061662,8.27575037116516,-4.39510283260601)) ;
#103763 = CARTESIAN_POINT('Ctrl Pts',(8.54742024083733,8.27608084608571,-4.39436567520734)) ;
#103764 = CARTESIAN_POINT('',(8.56507848521152,8.26835005667905,-4.39050028050403)) ;
#103765 = CARTESIAN_POINT('Origin',(8.6,8.3521616921714,-4.43240609825021)) ;
#103766 = CARTESIAN_POINT('',(8.58356010126947,8.17221734381475,-4.44107331645509)) ;
#103767 = CARTESIAN_POINT('Origin',(8.59670327708554,8.1688373429969,-4.34706896951945)) ;
#103768 = CARTESIAN_POINT('',(8.5,8.17221734381475,-4.5397127088383)) ;
#103769 = CARTESIAN_POINT('Origin',(8.6,8.17221734381475,-4.5397127088383)) ;
#103770 = CARTESIAN_POINT('Origin',(8.50000000000027,8.16642648762921,-4.31710775120157)) ;
#103771 = CARTESIAN_POINT('Origin',(2.9,3.8,-5.08)) ;
#103772 = CARTESIAN_POINT('',(3.,2.4,-5.08)) ;
#103773 = CARTESIAN_POINT('Origin',(3.,3.8,-5.08)) ;
#103774 = CARTESIAN_POINT('',(2.9,2.3,-5.08)) ;
#103775 = CARTESIAN_POINT('Origin',(2.9,2.4,-5.08)) ;
#103776 = CARTESIAN_POINT('Origin',(2.9,3.8,-5.08)) ;
#103777 = CARTESIAN_POINT('Origin',(1.35,3.8,-5.08)) ;
#103778 = CARTESIAN_POINT('',(1.35,2.3,-5.08)) ;
#103779 = CARTESIAN_POINT('Origin',(1.35,3.8,-5.08)) ;
#103780 = CARTESIAN_POINT('',(1.25,2.2,-5.08)) ;
#103781 = CARTESIAN_POINT('Origin',(1.35,2.2,-5.08)) ;
#103782 = CARTESIAN_POINT('Origin',(1.25,3.8,-5.08)) ;
#103783 = CARTESIAN_POINT('Origin',(13.9153543900904,1.02736587339764,-4.23)) ;
#103784 = CARTESIAN_POINT('',(1.15,1.02736587339764,-4.33)) ;
#103785 = CARTESIAN_POINT('',(1.15,0.931757800066529,-4.20068965517241)) ;
#103786 = CARTESIAN_POINT('Origin',(1.15,1.02736587339764,-4.23)) ;
#103787 = CARTESIAN_POINT('',(-0.900000000000002,1.02736587339765,-4.33)) ;
#103788 = CARTESIAN_POINT('',(-1.,1.02736587339765,-4.33)) ;
#103789 = CARTESIAN_POINT('',(-0.900000000000002,0.982644513847654,-4.31944271909999)) ;
#103790 = CARTESIAN_POINT('Origin',(-0.900000000000002,1.02736587339765,-4.23)) ;
#103791 = CARTESIAN_POINT('',(-0.900000000000002,0.93175780006653,-4.20068965517241)) ;
#103792 = CARTESIAN_POINT('Origin',(-0.900000000000002,1.02736587339765,-4.23)) ;
#103793 = CARTESIAN_POINT('',(13.9153543900904,0.931757800066525,-4.20068965517241)) ;
#103794 = CARTESIAN_POINT('Origin',(13.9153543900904,1.02736587339764,-5.93)) ;
#103795 = CARTESIAN_POINT('',(1.15,0.93175780006653,-5.95931034482759)) ;
#103796 = CARTESIAN_POINT('',(1.15,1.02736587339765,-5.83)) ;
#103797 = CARTESIAN_POINT('Origin',(1.15,1.02736587339765,-5.93)) ;
#103798 = CARTESIAN_POINT('',(-0.900000000000002,0.931757800066531,-5.95931034482759)) ;
#103799 = CARTESIAN_POINT('',(13.9153543900904,0.931757800066525,-5.95931034482759)) ;
#103800 = CARTESIAN_POINT('',(-0.900000000000002,1.02736587339765,-5.83)) ;
#103801 = CARTESIAN_POINT('Origin',(-0.900000000000002,1.02736587339765,-5.93)) ;
#103802 = CARTESIAN_POINT('',(-1.,1.02736587339765,-5.83)) ;
#103803 = CARTESIAN_POINT('Origin',(8.49172374697003,3.8,-5.08)) ;
#103804 = CARTESIAN_POINT('',(8.49172374697003,1.47741935483871,-3.18115320609529)) ;
#103805 = CARTESIAN_POINT('',(8.49172374697003,1.47741935483871,-6.97884679390471)) ;
#103806 = CARTESIAN_POINT('Origin',(8.49172374697003,3.8,-5.08)) ;
#103807 = CARTESIAN_POINT('',(8.50816364570057,1.47636598119991,-3.18029201095833)) ;
#103808 = CARTESIAN_POINT('Origin',(8.49172374697003,1.4,-3.11785831296514)) ;
#103809 = CARTESIAN_POINT('',(8.50816364570057,1.47636598119991,-6.97970798904167)) ;
#103810 = CARTESIAN_POINT('Origin',(8.50816364570057,3.8,-5.08)) ;
#103811 = CARTESIAN_POINT('Origin',(8.49172374697003,1.4,-7.04214168703486)) ;
#103812 = CARTESIAN_POINT('Origin',(1.25,3.8,-5.08)) ;
#103813 = CARTESIAN_POINT('',(1.25,2.3,-5.08)) ;
#103814 = CARTESIAN_POINT('Origin',(13.9153543900904,3.8,-5.08)) ;
#103815 = CARTESIAN_POINT('',(-0.900000000000002,1.47741935483872,-6.97884679390471)) ;
#103816 = CARTESIAN_POINT('',(13.9153543900904,1.47741935483871,-6.97884679390471)) ;
#103817 = CARTESIAN_POINT('Origin',(-0.900000000000001,3.8,-5.08)) ;
#103818 = CARTESIAN_POINT('',(1.35,0.876327704607742,-5.75241379310345)) ;
#103819 = CARTESIAN_POINT('Ctrl Pts',(1.35,0.876327704607742,-5.75241379310345)) ;
#103820 = CARTESIAN_POINT('Ctrl Pts',(1.35,0.888571289407569,-5.80564921159528)) ;
#103821 = CARTESIAN_POINT('Ctrl Pts',(1.32969623836296,0.902340613578954,
-5.85792959702133)) ;
#103822 = CARTESIAN_POINT('Ctrl Pts',(1.25741074236298,0.924142973728496,
-5.93501505371577)) ;
#103823 = CARTESIAN_POINT('Ctrl Pts',(1.20472523187106,0.93175780006653,-5.95931034482759)) ;
#103824 = CARTESIAN_POINT('Ctrl Pts',(1.15,0.93175780006653,-5.95931034482759)) ;
#103825 = CARTESIAN_POINT('',(1.35,0.876327704607742,-4.40758620689655)) ;
#103826 = CARTESIAN_POINT('Origin',(1.35,3.8,-5.08)) ;
#103827 = CARTESIAN_POINT('Ctrl Pts',(1.15,0.931757800066529,-4.20068965517241)) ;
#103828 = CARTESIAN_POINT('Ctrl Pts',(1.20475877631964,0.931757800066529,
-4.20068965517242)) ;
#103829 = CARTESIAN_POINT('Ctrl Pts',(1.2574100247738,0.924155896380522,-4.22493436088835)) ;
#103830 = CARTESIAN_POINT('Ctrl Pts',(1.32987646938161,0.9022735155524,-4.30231254552791)) ;
#103831 = CARTESIAN_POINT('Ctrl Pts',(1.35,0.888577265820266,-4.35432480281013)) ;
#103832 = CARTESIAN_POINT('Ctrl Pts',(1.35,0.876327704607742,-4.40758620689655)) ;
#103833 = CARTESIAN_POINT('',(-0.900000000000002,1.47741935483872,-3.18115320609529)) ;
#103834 = CARTESIAN_POINT('Origin',(-0.900000000000001,3.8,-5.08)) ;
#103835 = CARTESIAN_POINT('',(13.9153543900904,1.47741935483871,-3.18115320609529)) ;
#103836 = CARTESIAN_POINT('Origin',(0.55,3.09772049281573E-17,-5.08)) ;
#103837 = CARTESIAN_POINT('',(0.549999999999999,4.4,-4.63)) ;
#103838 = CARTESIAN_POINT('',(0.549999999999999,4.4,-5.53)) ;
#103839 = CARTESIAN_POINT('',(0.549999999999999,4.4,-5.08)) ;
#103840 = CARTESIAN_POINT('',(0.55,4.04473197180486,-5.53)) ;
#103841 = CARTESIAN_POINT('',(0.55,1.39397422176708E-16,-5.53)) ;
#103842 = CARTESIAN_POINT('',(0.55,4.05997159067981,-5.48)) ;
#103843 = CARTESIAN_POINT('Ctrl Pts',(0.549999999999999,4.04473197180486,
-5.53)) ;
#103844 = CARTESIAN_POINT('Ctrl Pts',(0.549999999999999,4.04764757798806,
-5.52556486112774)) ;
#103845 = CARTESIAN_POINT('Ctrl Pts',(0.549999999999999,4.05014503921306,
-5.52094814486588)) ;
#103846 = CARTESIAN_POINT('Ctrl Pts',(0.549999999999999,4.0569489863933,-5.50568144569025)) ;
#103847 = CARTESIAN_POINT('Ctrl Pts',(0.549999999999999,4.0599715906798,-5.49182145644142)) ;
#103848 = CARTESIAN_POINT('Ctrl Pts',(0.549999999999999,4.0599715906798,-5.48)) ;
#103849 = CARTESIAN_POINT('',(0.55,4.05997159067981,-4.68)) ;
#103850 = CARTESIAN_POINT('',(0.55,4.05997159067981,-4.58)) ;
#103851 = CARTESIAN_POINT('',(0.55,4.04473197181449,-4.63000000001465)) ;
#103852 = CARTESIAN_POINT('Origin',(0.550034503802618,3.93869457792365,-4.68241602969307)) ;
#103853 = CARTESIAN_POINT('',(0.55,6.35032701027224E-17,-4.63)) ;
#103854 = CARTESIAN_POINT('Origin',(10.,7.8,-7.62)) ;
#103855 = CARTESIAN_POINT('',(9.93162277660169,7.82279240779944,-7.62)) ;
#103856 = CARTESIAN_POINT('',(8.51539501058484,8.29486832980505,-7.62)) ;
#103857 = CARTESIAN_POINT('',(10.,7.8,-7.62)) ;
#103858 = CARTESIAN_POINT('',(8.51540095511711,8.29487265903615,-5.84906075993417)) ;
#103859 = CARTESIAN_POINT('',(8.51539501058484,8.29486832980505,-7.62)) ;
#103860 = CARTESIAN_POINT('',(8.54856023413468,8.28398586203113,-5.83600806656551)) ;
#103861 = CARTESIAN_POINT('Ctrl Pts',(8.51540095511711,8.29487265903615,-5.84906075993417)) ;
#103862 = CARTESIAN_POINT('Ctrl Pts',(8.51716444659958,8.29428466923188,-5.84964248281888)) ;
#103863 = CARTESIAN_POINT('Ctrl Pts',(8.51901954868165,8.29366521079576,-5.84997045085819)) ;
#103864 = CARTESIAN_POINT('Ctrl Pts',(8.52087614409667,8.2930450194617,-5.85007250257837)) ;
#103865 = CARTESIAN_POINT('Ctrl Pts',(8.52171779595218,8.29276386763785,-5.85011876576471)) ;
#103866 = CARTESIAN_POINT('Ctrl Pts',(8.52256005861364,8.29248252453828,-5.85011908777802)) ;
#103867 = CARTESIAN_POINT('Ctrl Pts',(8.52339613191994,8.29220315552769,-5.85007944601408)) ;
#103868 = CARTESIAN_POINT('Ctrl Pts',(8.52456316579569,8.29181319797644,-5.85002411201277)) ;
#103869 = CARTESIAN_POINT('Ctrl Pts',(8.52573147766845,8.29142195356397,-5.84989300499575)) ;
#103870 = CARTESIAN_POINT('Ctrl Pts',(8.52689074379086,8.29103442649367,-5.84969132708601)) ;
#103871 = CARTESIAN_POINT('Ctrl Pts',(8.52858695132691,8.2904674071317,-5.84939623730142)) ;
#103872 = CARTESIAN_POINT('Ctrl Pts',(8.53026630212626,8.28992123633279,-5.84894392181427)) ;
#103873 = CARTESIAN_POINT('Ctrl Pts',(8.5319011791312,8.28939883282067,-5.8483683729162)) ;
#103874 = CARTESIAN_POINT('Ctrl Pts',(8.53241671440276,8.28923410028381,-5.84818688173578)) ;
#103875 = CARTESIAN_POINT('Ctrl Pts',(8.53292790037787,8.28907155799427,-5.84799339751737)) ;
#103876 = CARTESIAN_POINT('Ctrl Pts',(8.53343404910736,8.28891083250768,-5.84778983795526)) ;
#103877 = CARTESIAN_POINT('Ctrl Pts',(8.5352968140817,8.28831931900687,-5.84704068340757)) ;
#103878 = CARTESIAN_POINT('Ctrl Pts',(8.53711612169873,8.28774836357889,-5.84613100883356)) ;
#103879 = CARTESIAN_POINT('Ctrl Pts',(8.5388519216198,8.28720494689876,-5.84506126474803)) ;
#103880 = CARTESIAN_POINT('Ctrl Pts',(8.54015925159107,8.28679566878773,-5.84425557943394)) ;
#103881 = CARTESIAN_POINT('Ctrl Pts',(8.54141951580281,8.286401527759,-5.84335974619183)) ;
#103882 = CARTESIAN_POINT('Ctrl Pts',(8.54261761299017,8.28602171215281,-5.84239271078543)) ;
#103883 = CARTESIAN_POINT('Ctrl Pts',(8.54427390694791,8.28549664098143,-5.84105584519768)) ;
#103884 = CARTESIAN_POINT('Ctrl Pts',(8.5458275679526,8.28499592220792,-5.83955743369619)) ;
#103885 = CARTESIAN_POINT('Ctrl Pts',(8.54719190273357,8.28456181678111,-5.83791397605226)) ;
#103886 = CARTESIAN_POINT('Ctrl Pts',(8.54768505754697,8.28440490428152,-5.83731992900528)) ;
#103887 = CARTESIAN_POINT('Ctrl Pts',(8.54815358395156,8.28425671205376,-5.83670743230753)) ;
#103888 = CARTESIAN_POINT('Ctrl Pts',(8.54859369700692,8.28411936587098,-5.83607885456179)) ;
#103889 = CARTESIAN_POINT('',(8.56837597005372,8.27720399148448,-5.81250542126692)) ;
#103890 = CARTESIAN_POINT('Ctrl Pts',(8.5485198670553,8.28382649282421,-5.83601405277584)) ;
#103891 = CARTESIAN_POINT('Ctrl Pts',(8.55267891820636,8.28243778061537,-5.83056312730521)) ;
#103892 = CARTESIAN_POINT('Ctrl Pts',(8.5570174719569,8.28096933708253,-5.82525905778143)) ;
#103893 = CARTESIAN_POINT('Ctrl Pts',(8.56150853123455,8.27945301063652,-5.82011321021338)) ;
#103894 = CARTESIAN_POINT('Ctrl Pts',(8.56331520072594,8.27884302075226,-5.81804313158965)) ;
#103895 = CARTESIAN_POINT('Ctrl Pts',(8.56514663435534,8.27822544298232,-5.8159980022295)) ;
#103896 = CARTESIAN_POINT('Ctrl Pts',(8.56700126712393,8.27760232477898,-5.81397578565849)) ;
#103897 = CARTESIAN_POINT('Ctrl Pts',(8.56745273479656,8.27745064099026,-5.81348352356526)) ;
#103898 = CARTESIAN_POINT('Ctrl Pts',(8.56790562999349,8.27729861980367,-5.81299519536269)) ;
#103899 = CARTESIAN_POINT('Ctrl Pts',(8.56835731300612,8.27714712982918,-5.8125055965825)) ;
#103900 = CARTESIAN_POINT('',(9.93162277660169,7.82279240779944,-6.03971270883831)) ;
#103901 = CARTESIAN_POINT('',(9.98593528106273,7.80468823964576,-6.04876479291514)) ;
#103902 = CARTESIAN_POINT('',(9.93162277660169,7.82279240779944,-7.62)) ;
#103903 = CARTESIAN_POINT('Origin',(10.,6.8,-7.62)) ;
#103904 = CARTESIAN_POINT('',(10.,6.8847127088383,-7.62)) ;
#103905 = CARTESIAN_POINT('',(10.,7.72792407799439,-7.62)) ;
#103906 = CARTESIAN_POINT('',(10.,6.8,-7.62)) ;
#103907 = CARTESIAN_POINT('',(10.,7.72792407799439,-6.03971270883831)) ;
#103908 = CARTESIAN_POINT('',(10.,7.72792407799439,-7.62)) ;
#103909 = CARTESIAN_POINT('',(10.,6.8847127088383,-6.03971270883831)) ;
#103910 = CARTESIAN_POINT('',(10.,6.8,-6.03971270883831)) ;
#103911 = CARTESIAN_POINT('',(10.,6.8847127088383,-7.62)) ;
#103912 = CARTESIAN_POINT('Origin',(8.5,6.55,-7.62)) ;
#103913 = CARTESIAN_POINT('',(9.91643989873054,6.78607331645509,-6.03971270883831)) ;
#103914 = CARTESIAN_POINT('',(8.58355805979357,6.56393854759965,-5.81756654157067)) ;
#103915 = CARTESIAN_POINT('',(8.48442535909739,6.54740422651623,-5.80104361889945)) ;
#103916 = CARTESIAN_POINT('',(8.56107669735261,6.56009388000089,-5.84238384722239)) ;
#103917 = CARTESIAN_POINT('Ctrl Pts',(8.58354728038625,6.56400494118525,-5.81756674863513)) ;
#103918 = CARTESIAN_POINT('Ctrl Pts',(8.57838853885709,6.56313097816981,-5.82293656964759)) ;
#103919 = CARTESIAN_POINT('Ctrl Pts',(8.57330127946578,6.56225500583444,-5.82838816865645)) ;
#103920 = CARTESIAN_POINT('Ctrl Pts',(8.56834297134842,6.5614089984297,-5.83396078378918)) ;
#103921 = CARTESIAN_POINT('Ctrl Pts',(8.56587587079895,6.56098805134781,-5.83673354448305)) ;
#103922 = CARTESIAN_POINT('Ctrl Pts',(8.56344049907324,6.56057499921406,-5.83953530332025)) ;
#103923 = CARTESIAN_POINT('Ctrl Pts',(8.56104288133098,6.56017406260213,-5.84236503624593)) ;
#103924 = CARTESIAN_POINT('',(8.508163057485,6.55136011924237,-5.85737262210526)) ;
#103925 = CARTESIAN_POINT('Ctrl Pts',(8.56125813732197,6.56020968955366,-5.84255063535367)) ;
#103926 = CARTESIAN_POINT('Ctrl Pts',(8.55737139916423,6.55956189986071,-5.84720859947429)) ;
#103927 = CARTESIAN_POINT('Ctrl Pts',(8.55306335190085,6.55884389198347,-5.8499674660883)) ;
#103928 = CARTESIAN_POINT('Ctrl Pts',(8.5412133223275,6.55686888705458,-5.8565237407831)) ;
#103929 = CARTESIAN_POINT('Ctrl Pts',(8.53496267039085,6.55582711173181,-5.85796136066778)) ;
#103930 = CARTESIAN_POINT('Ctrl Pts',(8.52888665184994,6.55481444197499,-5.85927955393154)) ;
#103931 = CARTESIAN_POINT('Ctrl Pts',(8.52471102104564,6.55411850350761,-5.85959774940141)) ;
#103932 = CARTESIAN_POINT('Ctrl Pts',(8.52011475164494,6.55335245860749,-5.85970295993519)) ;
#103933 = CARTESIAN_POINT('Ctrl Pts',(8.51754797133843,6.55292466188974,-5.85971864594294)) ;
#103934 = CARTESIAN_POINT('Ctrl Pts',(8.5124831787005,6.55208052978342,-5.8589638228621)) ;
#103935 = CARTESIAN_POINT('Ctrl Pts',(8.51021540604904,6.55170256767484,-5.85837089611144)) ;
#103936 = CARTESIAN_POINT('Ctrl Pts',(8.50816120922225,6.55136020153704,-5.85737641152605)) ;
#103937 = CARTESIAN_POINT('',(8.50816364570071,6.55136060761679,-7.62)) ;
#103938 = CARTESIAN_POINT('',(8.50816364570071,6.55136060761679,-7.62)) ;
#103939 = CARTESIAN_POINT('',(9.91643989873054,6.78607331645509,-7.62)) ;
#103940 = CARTESIAN_POINT('',(8.5,6.55,-7.62)) ;
#103941 = CARTESIAN_POINT('',(9.91643989873054,6.78607331645509,-7.62)) ;
#103942 = CARTESIAN_POINT('Origin',(10.,1.5,-7.62)) ;
#103943 = CARTESIAN_POINT('',(-0.900000000000002,1.5,-7.04214168703487)) ;
#103944 = CARTESIAN_POINT('',(8.49172374697003,1.5,-7.04214168703487)) ;
#103945 = CARTESIAN_POINT('',(10.,1.5,-7.04214168703487)) ;
#103946 = CARTESIAN_POINT('',(8.49172374697003,1.5,-7.62)) ;
#103947 = CARTESIAN_POINT('',(8.49172374697003,1.5,-7.62)) ;
#103948 = CARTESIAN_POINT('',(-0.900000000000001,1.5,-7.62)) ;
#103949 = CARTESIAN_POINT('',(10.,1.5,-7.62)) ;
#103950 = CARTESIAN_POINT('',(-0.900000000000002,1.5,-7.00613602842582)) ;
#103951 = CARTESIAN_POINT('Origin',(10.,1.5,-7.62)) ;
#103952 = CARTESIAN_POINT('',(8.49172374697003,1.5,-2.54)) ;
#103953 = CARTESIAN_POINT('',(-0.900000000000001,1.5,-2.54)) ;
#103954 = CARTESIAN_POINT('',(10.,1.5,-2.54)) ;
#103955 = CARTESIAN_POINT('',(8.49172374697003,1.5,-3.11785831296514)) ;
#103956 = CARTESIAN_POINT('',(8.49172374697003,1.5,-7.62)) ;
#103957 = CARTESIAN_POINT('',(-0.900000000000002,1.5,-3.11785831296514)) ;
#103958 = CARTESIAN_POINT('',(10.,1.5,-3.11785831296514)) ;
#103959 = CARTESIAN_POINT('',(-0.900000000000001,1.5,-7.62)) ;
#103960 = CARTESIAN_POINT('Origin',(10.,0.,-7.62)) ;
#103961 = CARTESIAN_POINT('',(10.,0.1,-2.54)) ;
#103962 = CARTESIAN_POINT('',(10.,1.16528729116168,-2.54)) ;
#103963 = CARTESIAN_POINT('',(10.,0.,-2.54)) ;
#103964 = CARTESIAN_POINT('',(10.,0.1,-7.62)) ;
#103965 = CARTESIAN_POINT('',(10.,0.1,-7.62)) ;
#103966 = CARTESIAN_POINT('',(10.,1.16528729116168,-7.62)) ;
#103967 = CARTESIAN_POINT('',(10.,0.,-7.62)) ;
#103968 = CARTESIAN_POINT('',(10.,1.16528729116168,-7.12416188017819)) ;
#103969 = CARTESIAN_POINT('',(10.,1.16528729116168,-7.62)) ;
#103970 = CARTESIAN_POINT('',(10.,1.16528729116168,-3.03583811982181)) ;
#103971 = CARTESIAN_POINT('Origin',(10.,3.8,-5.08)) ;
#103972 = CARTESIAN_POINT('',(10.,1.16528729116168,-7.62)) ;
#103973 = CARTESIAN_POINT('Origin',(0.,0.,-7.62)) ;
#103974 = CARTESIAN_POINT('',(8.48377223398316,8.3,-7.62)) ;
#103975 = CARTESIAN_POINT('',(7.1,8.3,-7.62)) ;
#103976 = CARTESIAN_POINT('',(8.5,8.3,-7.62)) ;
#103977 = CARTESIAN_POINT('Origin',(8.48377223398316,8.2,-7.62)) ;
#103978 = CARTESIAN_POINT('Origin',(9.9,7.72792407799439,-7.62)) ;
#103979 = CARTESIAN_POINT('Origin',(9.9,6.8847127088383,-7.62)) ;
#103980 = CARTESIAN_POINT('',(8.49172374697018,6.55,-7.62)) ;
#103981 = CARTESIAN_POINT('Origin',(8.49172374697018,6.65,-7.62)) ;
#103982 = CARTESIAN_POINT('',(-0.900000000000001,6.55,-7.62)) ;
#103983 = CARTESIAN_POINT('',(1.25,6.55,-7.62)) ;
#103984 = CARTESIAN_POINT('',(-1.,6.45,-7.62)) ;
#103985 = CARTESIAN_POINT('Origin',(-0.9,6.45,-7.62)) ;
#103986 = CARTESIAN_POINT('',(-1.,4.65,-7.62)) ;
#103987 = CARTESIAN_POINT('',(-1.,3.46944695195362E-16,-7.62)) ;
#103988 = CARTESIAN_POINT('',(-0.900000000000001,4.55,-7.62)) ;
#103989 = CARTESIAN_POINT('Origin',(-0.900000000000001,4.65,-7.62)) ;
#103990 = CARTESIAN_POINT('',(1.15,4.55,-7.62)) ;
#103991 = CARTESIAN_POINT('',(1.57859836313889E-15,4.55,-7.62)) ;
#103992 = CARTESIAN_POINT('',(1.25,4.45,-7.62)) ;
#103993 = CARTESIAN_POINT('Origin',(1.15,4.45,-7.62)) ;
#103994 = CARTESIAN_POINT('',(1.25,3.15,-7.62)) ;
#103995 = CARTESIAN_POINT('',(1.25,1.5,-7.62)) ;
#103996 = CARTESIAN_POINT('',(1.15,3.05,-7.62)) ;
#103997 = CARTESIAN_POINT('Origin',(1.15,3.15,-7.62)) ;
#103998 = CARTESIAN_POINT('',(-0.900000000000002,3.05,-7.62)) ;
#103999 = CARTESIAN_POINT('',(1.05818132034585E-15,3.05,-7.62)) ;
#104000 = CARTESIAN_POINT('',(-1.,2.95,-7.62)) ;
#104001 = CARTESIAN_POINT('Origin',(-0.900000000000002,2.95,-7.62)) ;
#104002 = CARTESIAN_POINT('',(-1.,1.6,-7.62)) ;
#104003 = CARTESIAN_POINT('',(-1.,3.46944695195362E-16,-7.62)) ;
#104004 = CARTESIAN_POINT('Origin',(-0.900000000000002,1.6,-7.62)) ;
#104005 = CARTESIAN_POINT('',(8.50816364570057,1.49863939238321,-7.62)) ;
#104006 = CARTESIAN_POINT('Origin',(8.49172374697003,1.4,-7.62)) ;
#104007 = CARTESIAN_POINT('',(9.91643989873054,1.26392668354489,-7.62)) ;
#104008 = CARTESIAN_POINT('',(10.,1.24999999999998,-7.62)) ;
#104009 = CARTESIAN_POINT('Origin',(9.9,1.16528729116168,-7.62)) ;
#104010 = CARTESIAN_POINT('',(9.9,0.,-7.62)) ;
#104011 = CARTESIAN_POINT('Origin',(9.9,0.1,-7.62)) ;
#104012 = CARTESIAN_POINT('',(-2.,0.,-7.62)) ;
#104013 = CARTESIAN_POINT('',(-2.,0.,-7.62)) ;
#104014 = CARTESIAN_POINT('',(-2.,7.55,-7.62)) ;
#104015 = CARTESIAN_POINT('',(-2.,7.65,-7.62)) ;
#104016 = CARTESIAN_POINT('',(-1.9,7.65,-7.62)) ;
#104017 = CARTESIAN_POINT('Origin',(-1.9,7.55,-7.62)) ;
#104018 = CARTESIAN_POINT('',(6.9,7.65,-7.62)) ;
#104019 = CARTESIAN_POINT('',(7.,7.65,-7.62)) ;
#104020 = CARTESIAN_POINT('',(7.,7.75,-7.62)) ;
#104021 = CARTESIAN_POINT('Origin',(6.9,7.75,-7.62)) ;
#104022 = CARTESIAN_POINT('',(7.,8.2,-7.62)) ;
#104023 = CARTESIAN_POINT('',(7.,8.3,-7.62)) ;
#104024 = CARTESIAN_POINT('Origin',(7.1,8.2,-7.62)) ;
#104025 = CARTESIAN_POINT('Origin',(0.,0.,-2.54)) ;
#104026 = CARTESIAN_POINT('',(9.93162277660169,7.82279240779944,-2.54)) ;
#104027 = CARTESIAN_POINT('',(8.51539501058484,8.29486832980505,-2.54)) ;
#104028 = CARTESIAN_POINT('',(10.,7.8,-2.54)) ;
#104029 = CARTESIAN_POINT('',(8.48377223398316,8.3,-2.54)) ;
#104030 = CARTESIAN_POINT('Origin',(8.48377223398316,8.2,-2.54)) ;
#104031 = CARTESIAN_POINT('',(7.1,8.3,-2.54)) ;
#104032 = CARTESIAN_POINT('',(8.5,8.3,-2.54)) ;
#104033 = CARTESIAN_POINT('',(7.,8.2,-2.54)) ;
#104034 = CARTESIAN_POINT('Origin',(7.1,8.2,-2.54)) ;
#104035 = CARTESIAN_POINT('',(7.,7.75,-2.54)) ;
#104036 = CARTESIAN_POINT('',(7.,8.3,-2.54)) ;
#104037 = CARTESIAN_POINT('',(6.9,7.65,-2.54)) ;
#104038 = CARTESIAN_POINT('Origin',(6.9,7.75,-2.54)) ;
#104039 = CARTESIAN_POINT('',(-1.9,7.65,-2.54)) ;
#104040 = CARTESIAN_POINT('',(7.,7.65,-2.54)) ;
#104041 = CARTESIAN_POINT('',(-2.,7.55,-2.54)) ;
#104042 = CARTESIAN_POINT('Origin',(-1.9,7.55,-2.54)) ;
#104043 = CARTESIAN_POINT('',(-2.,0.,-2.54)) ;
#104044 = CARTESIAN_POINT('',(-2.,7.65,-2.54)) ;
#104045 = CARTESIAN_POINT('',(9.9,0.,-2.54)) ;
#104046 = CARTESIAN_POINT('',(-2.,0.,-2.54)) ;
#104047 = CARTESIAN_POINT('Origin',(9.9,0.1,-2.54)) ;
#104048 = CARTESIAN_POINT('',(9.91643989873054,1.26392668354489,-2.54)) ;
#104049 = CARTESIAN_POINT('Origin',(9.9,1.16528729116168,-2.54)) ;
#104050 = CARTESIAN_POINT('',(8.50816364570057,1.49863939238321,-2.54)) ;
#104051 = CARTESIAN_POINT('',(0.472972972972955,2.83783783783779,-2.54)) ;
#104052 = CARTESIAN_POINT('Origin',(8.49172374697003,1.4,-2.54)) ;
#104053 = CARTESIAN_POINT('',(-1.,1.6,-2.54)) ;
#104054 = CARTESIAN_POINT('Origin',(-0.900000000000002,1.6,-2.54)) ;
#104055 = CARTESIAN_POINT('',(-1.,2.95,-2.54)) ;
#104056 = CARTESIAN_POINT('',(-1.,3.46944695195362E-16,-2.54)) ;
#104057 = CARTESIAN_POINT('',(-0.900000000000002,3.05,-2.54)) ;
#104058 = CARTESIAN_POINT('Origin',(-0.900000000000002,2.95,-2.54)) ;
#104059 = CARTESIAN_POINT('',(1.15,3.05,-2.54)) ;
#104060 = CARTESIAN_POINT('',(1.05818132034585E-15,3.05,-2.54)) ;
#104061 = CARTESIAN_POINT('',(1.25,3.15,-2.54)) ;
#104062 = CARTESIAN_POINT('Origin',(1.15,3.15,-2.54)) ;
#104063 = CARTESIAN_POINT('',(1.25,4.45,-2.54)) ;
#104064 = CARTESIAN_POINT('',(1.25,5.3,-2.54)) ;
#104065 = CARTESIAN_POINT('',(1.15,4.55,-2.54)) ;
#104066 = CARTESIAN_POINT('Origin',(1.15,4.45,-2.54)) ;
#104067 = CARTESIAN_POINT('',(-0.900000000000001,4.55,-2.54)) ;
#104068 = CARTESIAN_POINT('',(1.57859836313889E-15,4.55,-2.54)) ;
#104069 = CARTESIAN_POINT('',(-1.,4.65,-2.54)) ;
#104070 = CARTESIAN_POINT('Origin',(-0.900000000000001,4.65,-2.54)) ;
#104071 = CARTESIAN_POINT('',(-1.,6.45,-2.54)) ;
#104072 = CARTESIAN_POINT('',(-1.,3.46944695195362E-16,-2.54)) ;
#104073 = CARTESIAN_POINT('',(-0.900000000000001,6.55,-2.54)) ;
#104074 = CARTESIAN_POINT('Origin',(-0.9,6.45,-2.54)) ;
#104075 = CARTESIAN_POINT('',(8.49172374697018,6.55,-2.54)) ;
#104076 = CARTESIAN_POINT('',(1.25,6.55,-2.54)) ;
#104077 = CARTESIAN_POINT('',(8.50816364570071,6.55136060761679,-2.54)) ;
#104078 = CARTESIAN_POINT('Origin',(8.49172374697018,6.65,-2.54)) ;
#104079 = CARTESIAN_POINT('',(9.91643989873054,6.78607331645509,-2.54)) ;
#104080 = CARTESIAN_POINT('',(8.5,6.55,-2.54)) ;
#104081 = CARTESIAN_POINT('',(10.,6.8847127088383,-2.54)) ;
#104082 = CARTESIAN_POINT('Origin',(9.9,6.8847127088383,-2.54)) ;
#104083 = CARTESIAN_POINT('',(10.,7.72792407799439,-2.54)) ;
#104084 = CARTESIAN_POINT('',(10.,6.8,-2.54)) ;
#104085 = CARTESIAN_POINT('Origin',(9.9,7.72792407799439,-2.54)) ;
#104086 = CARTESIAN_POINT('Origin',(7.,7.65,-7.62)) ;
#104087 = CARTESIAN_POINT('',(-1.9,7.65,-7.62)) ;
#104088 = CARTESIAN_POINT('',(6.9,7.65,-7.62)) ;
#104089 = CARTESIAN_POINT('Origin',(7.,8.3,-7.62)) ;
#104090 = CARTESIAN_POINT('',(7.,7.75,-2.54)) ;
#104091 = CARTESIAN_POINT('',(7.,8.2,-7.62)) ;
#104092 = CARTESIAN_POINT('Origin',(8.5,8.3,-7.62)) ;
#104093 = CARTESIAN_POINT('',(8.4,8.3,-5.62207288985098)) ;
#104094 = CARTESIAN_POINT('',(8.48377267093845,8.29999999999968,-5.83805254500423)) ;
#104095 = CARTESIAN_POINT('Ctrl Pts',(8.4,8.3,-5.62207288985098)) ;
#104096 = CARTESIAN_POINT('Ctrl Pts',(8.40000007660113,8.3,-5.63922965019375)) ;
#104097 = CARTESIAN_POINT('Ctrl Pts',(8.40222537906592,8.3,-5.65619623911413)) ;
#104098 = CARTESIAN_POINT('Ctrl Pts',(8.40642689896074,8.3,-5.67261625649977)) ;
#104099 = CARTESIAN_POINT('Ctrl Pts',(8.41084238024295,8.3,-5.68987245931085)) ;
#104100 = CARTESIAN_POINT('Ctrl Pts',(8.41744096860936,8.3,-5.70652674436269)) ;
#104101 = CARTESIAN_POINT('Ctrl Pts',(8.42598957610141,8.3,-5.72216220072253)) ;
#104102 = CARTESIAN_POINT('Ctrl Pts',(8.42927578125638,8.3,-5.72817269042366)) ;
#104103 = CARTESIAN_POINT('Ctrl Pts',(8.43285067318462,8.3,-5.73403244695937)) ;
#104104 = CARTESIAN_POINT('Ctrl Pts',(8.43670279785317,8.3,-5.73971678678546)) ;
#104105 = CARTESIAN_POINT('Ctrl Pts',(8.43684245837178,8.3,-5.73992287509162)) ;
#104106 = CARTESIAN_POINT('Ctrl Pts',(8.43698247939111,8.3,-5.74012872682246)) ;
#104107 = CARTESIAN_POINT('Ctrl Pts',(8.43712286024713,8.3,-5.74033434069405)) ;
#104108 = CARTESIAN_POINT('Ctrl Pts',(8.44304092798571,8.3,-5.74900245153563)) ;
#104109 = CARTESIAN_POINT('Ctrl Pts',(8.4496323269955,8.300000000002,-5.75733173136454)) ;
#104110 = CARTESIAN_POINT('Ctrl Pts',(8.45667836512368,8.29999999999776,-5.76518827396423)) ;
#104111 = CARTESIAN_POINT('Ctrl Pts',(8.46347186896914,8.29999999999367,-5.77276323330906)) ;
#104112 = CARTESIAN_POINT('Ctrl Pts',(8.47075094334182,8.29999999998297,-5.77990986551535)) ;
#104113 = CARTESIAN_POINT('Ctrl Pts',(8.47818849074308,8.29999999991001,-5.78688161282849)) ;
#104114 = CARTESIAN_POINT('Ctrl Pts',(8.47846436286148,8.2999999999073,-5.78714020757706)) ;
#104115 = CARTESIAN_POINT('Ctrl Pts',(8.47874045306876,8.29999999990447,-5.78739856059915)) ;
#104116 = CARTESIAN_POINT('Ctrl Pts',(8.47901674447045,8.29999999990152,-5.78765668520005)) ;
#104117 = CARTESIAN_POINT('Ctrl Pts',(8.48287938578322,8.29999999986032,-5.79126534888334)) ;
#104118 = CARTESIAN_POINT('Ctrl Pts',(8.4868120552941,8.29999999978803,-5.79480793672782)) ;
#104119 = CARTESIAN_POINT('Ctrl Pts',(8.49047938959117,8.29999999977836,-5.79860270602181)) ;
#104120 = CARTESIAN_POINT('Ctrl Pts',(8.49231307405274,8.29999999977353,-5.80050010858344)) ;
#104121 = CARTESIAN_POINT('Ctrl Pts',(8.49410676862313,8.29999999978935,-5.802469327125)) ;
#104122 = CARTESIAN_POINT('Ctrl Pts',(8.49555027122445,8.29999999981726,-5.80469680700993)) ;
#104123 = CARTESIAN_POINT('Ctrl Pts',(8.49675259850851,8.2999999998405,-5.80655212742148)) ;
#104124 = CARTESIAN_POINT('Ctrl Pts',(8.49764594203226,8.29999999986456,-5.80863681574321)) ;
#104125 = CARTESIAN_POINT('Ctrl Pts',(8.49795530287013,8.29999999987615,-5.8108110374494)) ;
#104126 = CARTESIAN_POINT('Ctrl Pts',(8.49801735255452,8.29999999987847,-5.81124712939817)) ;
#104127 = CARTESIAN_POINT('Ctrl Pts',(8.49805590844335,8.29999999988033,-5.81168682297804)) ;
#104128 = CARTESIAN_POINT('Ctrl Pts',(8.49806875158487,8.29999999988168,-5.81212898966141)) ;
#104129 = CARTESIAN_POINT('Ctrl Pts',(8.49822249685464,8.2999999998978,-5.81742216780677)) ;
#104130 = CARTESIAN_POINT('Ctrl Pts',(8.49538250015675,8.29999999989889,-5.82235534426841)) ;
#104131 = CARTESIAN_POINT('Ctrl Pts',(8.49246863081132,8.29999999993392,-5.82672286055097)) ;
#104132 = CARTESIAN_POINT('Ctrl Pts',(8.48983292606215,8.29999999996562,-5.83067344379386)) ;
#104133 = CARTESIAN_POINT('Ctrl Pts',(8.48683766317129,8.3,-5.83439221106978)) ;
#104134 = CARTESIAN_POINT('Ctrl Pts',(8.48377316486173,8.3,-5.83805195629754)) ;
#104135 = CARTESIAN_POINT('',(8.48377223398316,8.3,-7.62)) ;
#104136 = CARTESIAN_POINT('',(7.1,8.3,-7.62)) ;
#104137 = CARTESIAN_POINT('',(8.48377267093845,8.29999999999968,-4.32194745499577)) ;
#104138 = CARTESIAN_POINT('',(8.48377223398316,8.3,-7.62)) ;
#104139 = CARTESIAN_POINT('',(8.4,8.3,-4.53792711014902)) ;
#104140 = CARTESIAN_POINT('Ctrl Pts',(8.48377316486179,8.3,-4.3219480437024)) ;
#104141 = CARTESIAN_POINT('Ctrl Pts',(8.48683766317134,8.3,-4.32560778893017)) ;
#104142 = CARTESIAN_POINT('Ctrl Pts',(8.48983292606214,8.29999999996562,-4.32932655620614)) ;
#104143 = CARTESIAN_POINT('Ctrl Pts',(8.49246863081131,8.29999999993393,-4.33327713944903)) ;
#104144 = CARTESIAN_POINT('Ctrl Pts',(8.49538250015675,8.29999999989889,-4.33764465573159)) ;
#104145 = CARTESIAN_POINT('Ctrl Pts',(8.49822249685463,8.2999999998978,-4.34257783219323)) ;
#104146 = CARTESIAN_POINT('Ctrl Pts',(8.49806875158488,8.29999999988168,-4.34787101033859)) ;
#104147 = CARTESIAN_POINT('Ctrl Pts',(8.49805590844336,8.29999999988033,-4.34831317702196)) ;
#104148 = CARTESIAN_POINT('Ctrl Pts',(8.49801735255452,8.29999999987847,-4.34875287060183)) ;
#104149 = CARTESIAN_POINT('Ctrl Pts',(8.49795530287013,8.29999999987615,-4.3491889625506)) ;
#104150 = CARTESIAN_POINT('Ctrl Pts',(8.49764594190815,8.29999999986456,-4.35136318512907)) ;
#104151 = CARTESIAN_POINT('Ctrl Pts',(8.49675259754384,8.2999999998405,-4.35344787406726)) ;
#104152 = CARTESIAN_POINT('Ctrl Pts',(8.49555027122432,8.29999999981726,-4.35530319298998)) ;
#104153 = CARTESIAN_POINT('Ctrl Pts',(8.49410676570211,8.29999999978935,-4.35753067738161)) ;
#104154 = CARTESIAN_POINT('Ctrl Pts',(8.4923130692812,8.29999999977353,-4.359499896352)) ;
#104155 = CARTESIAN_POINT('Ctrl Pts',(8.49047938958768,8.29999999977836,-4.36139729397482)) ;
#104156 = CARTESIAN_POINT('Ctrl Pts',(8.48681202348067,8.29999999978803,-4.36519209617395)) ;
#104157 = CARTESIAN_POINT('Ctrl Pts',(8.48287934332708,8.29999999986032,-4.36873469073021)) ;
#104158 = CARTESIAN_POINT('Ctrl Pts',(8.47901674443308,8.29999999990152,-4.37234331475996)) ;
#104159 = CARTESIAN_POINT('Ctrl Pts',(8.47874052296043,8.29999999990447,-4.37260137402811)) ;
#104160 = CARTESIAN_POINT('Ctrl Pts',(8.4784645028431,8.2999999999073,-4.37285966135654)) ;
#104161 = CARTESIAN_POINT('Ctrl Pts',(8.47818870097127,8.29999999991001,-4.3731181900299)) ;
#104162 = CARTESIAN_POINT('Ctrl Pts',(8.47075185325582,8.29999999998296,-4.38008927532798)) ;
#104163 = CARTESIAN_POINT('Ctrl Pts',(8.46347271757077,8.29999999998104,-4.38723682100701)) ;
#104164 = CARTESIAN_POINT('Ctrl Pts',(8.45667934899943,8.29999999998018,-4.39481260831541)) ;
#104165 = CARTESIAN_POINT('Ctrl Pts',(8.44963335392746,8.29999999997929,-4.40267011810317)) ;
#104166 = CARTESIAN_POINT('Ctrl Pts',(8.44304226791565,8.29999999996634,-4.41100025634497)) ;
#104167 = CARTESIAN_POINT('Ctrl Pts',(8.43712466127421,8.29999999997622,-4.419666888942)) ;
#104168 = CARTESIAN_POINT('Ctrl Pts',(8.43698358608697,8.29999999997646,-4.41987350065015)) ;
#104169 = CARTESIAN_POINT('Ctrl Pts',(8.43684287437574,8.2999999999767,-4.42008035127934)) ;
#104170 = CARTESIAN_POINT('Ctrl Pts',(8.43670252680326,8.29999999997696,-4.42028743949552)) ;
#104171 = CARTESIAN_POINT('Ctrl Pts',(8.42665365624234,8.29999999999548,-4.43511493271378)) ;
#104172 = CARTESIAN_POINT('Ctrl Pts',(8.41848789916361,8.29999999999779,-4.45113486319109)) ;
#104173 = CARTESIAN_POINT('Ctrl Pts',(8.41242260582447,8.29999999999911,-4.46791805139592)) ;
#104174 = CARTESIAN_POINT('Ctrl Pts',(8.40662497274242,8.30000000000037,-4.48396060065411)) ;
#104175 = CARTESIAN_POINT('Ctrl Pts',(8.40274598945985,8.3,-4.50070219391449)) ;
#104176 = CARTESIAN_POINT('Ctrl Pts',(8.40101973895747,8.3,-4.51777978833517)) ;
#104177 = CARTESIAN_POINT('Ctrl Pts',(8.40034533497825,8.3,-4.52445158806355)) ;
#104178 = CARTESIAN_POINT('Ctrl Pts',(8.40000003014814,8.3,-4.53117467303786)) ;
#104179 = CARTESIAN_POINT('Ctrl Pts',(8.4,8.3,-4.53792711014902)) ;
#104180 = CARTESIAN_POINT('',(8.4,8.3,-5.66365455630091)) ;
#104181 = CARTESIAN_POINT('Origin',(10.,7.8,-7.62)) ;
#104182 = CARTESIAN_POINT('',(8.56837722373805,8.27720759208727,-4.3474948832495)) ;
#104183 = CARTESIAN_POINT('',(8.54843785958924,8.28385404680359,-4.3239803122607)) ;
#104184 = CARTESIAN_POINT('Ctrl Pts',(8.56837722339832,8.27720759220056,-4.34749488336226)) ;
#104185 = CARTESIAN_POINT('Ctrl Pts',(8.56792584473107,8.27735805175631,-4.34700469022775)) ;
#104186 = CARTESIAN_POINT('Ctrl Pts',(8.56747319573485,8.27750893475505,-4.34651579326377)) ;
#104187 = CARTESIAN_POINT('Ctrl Pts',(8.56702308739659,8.2776589708678,-4.34602430395872)) ;
#104188 = CARTESIAN_POINT('Ctrl Pts',(8.56055949575605,8.27981350141465,-4.33896647833431)) ;
#104189 = CARTESIAN_POINT('Ctrl Pts',(8.5543545977397,8.28188180075344,-4.33162839546916)) ;
#104190 = CARTESIAN_POINT('Ctrl Pts',(8.54852002808959,8.28382665730347,-4.32398586635143)) ;
#104191 = CARTESIAN_POINT('',(8.51539953939799,8.29486682020067,-4.31094033012292)) ;
#104192 = CARTESIAN_POINT('Origin',(8.52916905055949,8.29027698314684,-4.330734470479)) ;
#104193 = CARTESIAN_POINT('',(8.51539501058484,8.29486832980505,-7.62)) ;
#104194 = CARTESIAN_POINT('',(9.93162277660169,7.82279240779944,-4.1202872911617)) ;
#104195 = CARTESIAN_POINT('',(9.93162277660169,7.82279240779944,-7.62)) ;
#104196 = CARTESIAN_POINT('',(8.48593528106273,8.30468823964576,-4.36123520708486)) ;
#104197 = CARTESIAN_POINT('Origin',(10.,6.8,-7.62)) ;
#104198 = CARTESIAN_POINT('',(10.,6.8847127088383,-4.1202872911617)) ;
#104199 = CARTESIAN_POINT('',(10.,7.72792407799439,-4.1202872911617)) ;
#104200 = CARTESIAN_POINT('',(10.,7.8,-4.1202872911617)) ;
#104201 = CARTESIAN_POINT('',(10.,7.72792407799439,-7.62)) ;
#104202 = CARTESIAN_POINT('',(10.,6.8847127088383,-7.62)) ;
#104203 = CARTESIAN_POINT('Origin',(8.5,6.55,-7.62)) ;
#104204 = CARTESIAN_POINT('',(8.50816305748853,6.55136011924294,-4.3026273778919)) ;
#104205 = CARTESIAN_POINT('Ctrl Pts',(8.5081612092262,6.5513602015377,-4.30262358847201)) ;
#104206 = CARTESIAN_POINT('Ctrl Pts',(8.50982330775196,6.55163721795866,-4.30181892781797)) ;
#104207 = CARTESIAN_POINT('Ctrl Pts',(8.51162127657706,6.55193687942951,-4.30127902844118)) ;
#104208 = CARTESIAN_POINT('Ctrl Pts',(8.51523682141403,6.55253947023567,-4.30057109233524)) ;
#104209 = CARTESIAN_POINT('Ctrl Pts',(8.51710259142332,6.55285043190389,-4.30039346793935)) ;
#104210 = CARTESIAN_POINT('Ctrl Pts',(8.52217030373161,6.55369505062194,-4.30023569112656)) ;
#104211 = CARTESIAN_POINT('Ctrl Pts',(8.52587381749813,6.55431230291636,-4.30048388339438)) ;
#104212 = CARTESIAN_POINT('Ctrl Pts',(8.53482421527827,6.55580403587971,-4.3017298501838)) ;
#104213 = CARTESIAN_POINT('Ctrl Pts',(8.53952102462486,6.55658683673452,-4.30322044742312)) ;
#104214 = CARTESIAN_POINT('Ctrl Pts',(8.54640674065651,6.55773445607313,-4.30636821224513)) ;
#104215 = CARTESIAN_POINT('Ctrl Pts',(8.55013419152096,6.55835569858683,-4.30823673022989)) ;
#104216 = CARTESIAN_POINT('Ctrl Pts',(8.55581906875064,6.55930317812511,-4.31204337542897)) ;
#104217 = CARTESIAN_POINT('Ctrl Pts',(8.55861150732083,6.55976858455347,-4.31427755556237)) ;
#104218 = CARTESIAN_POINT('Ctrl Pts',(8.5612582140973,6.56020970234955,-4.31744945665611)) ;
#104219 = CARTESIAN_POINT('',(9.91643989873054,6.78607331645509,-4.1202872911617)) ;
#104220 = CARTESIAN_POINT('',(9.98442535909739,6.79740422651623,-4.10895638110055)) ;
#104221 = CARTESIAN_POINT('',(9.91643989873054,6.78607331645509,-7.62)) ;
#104222 = CARTESIAN_POINT('',(8.50816364570071,6.55136060761679,-7.62)) ;
#104223 = CARTESIAN_POINT('Origin',(1.25,6.55,-7.62)) ;
#104224 = CARTESIAN_POINT('',(8.49172372711481,6.55000000000007,-5.8494558427306)) ;
#104225 = CARTESIAN_POINT('',(8.49172374697018,6.55,-7.62)) ;
#104226 = CARTESIAN_POINT('',(8.4,6.55,-5.6206780018997)) ;
#104227 = CARTESIAN_POINT('Ctrl Pts',(8.49172374697018,6.55000000000105,-5.84945574565572)) ;
#104228 = CARTESIAN_POINT('Ctrl Pts',(8.49606803673628,6.55000000001052,-5.84595058632692)) ;
#104229 = CARTESIAN_POINT('Ctrl Pts',(8.50046735944504,6.54999999990302,-5.84251190424928)) ;
#104230 = CARTESIAN_POINT('Ctrl Pts',(8.50920280475187,6.55000000136501,-5.83551602670204)) ;
#104231 = CARTESIAN_POINT('Ctrl Pts',(8.51365366733357,6.55000000372466,-5.83201891829248)) ;
#104232 = CARTESIAN_POINT('Ctrl Pts',(8.51786969589099,6.55000000840872,-5.82757405149189)) ;
#104233 = CARTESIAN_POINT('Ctrl Pts',(8.51824835575334,6.5500000088438,-5.82716283435581)) ;
#104234 = CARTESIAN_POINT('Ctrl Pts',(8.51893753951069,6.55000000964298,-5.82638941226416)) ;
#104235 = CARTESIAN_POINT('Ctrl Pts',(8.51925555226623,6.55000001000021,-5.82602468306099)) ;
#104236 = CARTESIAN_POINT('Ctrl Pts',(8.52125362518914,6.55000001218547,-5.82363696640081)) ;
#104237 = CARTESIAN_POINT('Ctrl Pts',(8.52280131776513,6.55000000862055,-5.82136252157375)) ;
#104238 = CARTESIAN_POINT('Ctrl Pts',(8.52354796988915,6.55000000490364,-5.8162172682012)) ;
#104239 = CARTESIAN_POINT('Ctrl Pts',(8.52233587755857,6.5500000056078,-5.81356291782334)) ;
#104240 = CARTESIAN_POINT('Ctrl Pts',(8.52032554216556,6.55000000470579,-5.81116101057052)) ;
#104241 = CARTESIAN_POINT('Ctrl Pts',(8.52004618744961,6.55000000456892,-5.81085546722455)) ;
#104242 = CARTESIAN_POINT('Ctrl Pts',(8.51943244221705,6.55000000425259,-5.81023755755062)) ;
#104243 = CARTESIAN_POINT('Ctrl Pts',(8.51910103101855,6.55000000405877,-5.80991727732132)) ;
#104244 = CARTESIAN_POINT('Ctrl Pts',(8.51460799223804,6.5500000014124,-5.8057349310042)) ;
#104245 = CARTESIAN_POINT('Ctrl Pts',(8.50969722522559,6.55000000036127,-5.80296024115299)) ;
#104246 = CARTESIAN_POINT('Ctrl Pts',(8.50463600502758,6.55000000021577,-5.79966347483879)) ;
#104247 = CARTESIAN_POINT('Ctrl Pts',(8.50427412871944,6.55000000020764,-5.79942728012652)) ;
#104248 = CARTESIAN_POINT('Ctrl Pts',(8.49410349041847,6.55000000002642,-5.79277433128147)) ;
#104249 = CARTESIAN_POINT('Ctrl Pts',(8.48448997361522,6.54999999999179,-5.78608093896228)) ;
#104250 = CARTESIAN_POINT('Ctrl Pts',(8.46629237463077,6.55000000001684,-5.77097702438866)) ;
#104251 = CARTESIAN_POINT('Ctrl Pts',(8.45766562693772,6.55000000000152,-5.76259393166186)) ;
#104252 = CARTESIAN_POINT('Ctrl Pts',(8.44955830666691,6.54999999999999,-5.75321233426814)) ;
#104253 = CARTESIAN_POINT('Ctrl Pts',(8.44937081015217,6.54999999999999,-5.75299442831169)) ;
#104254 = CARTESIAN_POINT('Ctrl Pts',(8.43720071044327,6.5500000000026,-5.7387892740207)) ;
#104255 = CARTESIAN_POINT('Ctrl Pts',(8.42721384365609,6.55000000009149,-5.72325666818742)) ;
#104256 = CARTESIAN_POINT('Ctrl Pts',(8.41184903642134,6.55000000007035,-5.6905950553132)) ;
#104257 = CARTESIAN_POINT('Ctrl Pts',(8.40635547808108,6.5500000000232,-5.67351733252205)) ;
#104258 = CARTESIAN_POINT('Ctrl Pts',(8.40108598764522,6.5499999999995,-5.6443588087486)) ;
#104259 = CARTESIAN_POINT('Ctrl Pts',(8.4,6.55,-5.63255952793497)) ;
#104260 = CARTESIAN_POINT('Ctrl Pts',(8.4,6.55,-5.6206780018997)) ;
#104261 = CARTESIAN_POINT('',(8.4,6.55,-4.5393219981003)) ;
#104262 = CARTESIAN_POINT('',(8.4,6.55,-4.35636060761679)) ;
#104263 = CARTESIAN_POINT('',(8.4917237271148,6.5500000000004,-4.31054415726839)) ;
#104264 = CARTESIAN_POINT('Ctrl Pts',(8.4,6.55,-4.5393219981003)) ;
#104265 = CARTESIAN_POINT('Ctrl Pts',(8.4,6.55,-4.52146035159378)) ;
#104266 = CARTESIAN_POINT('Ctrl Pts',(8.40245177849675,6.55000000000111,-4.50378505808852)) ;
#104267 = CARTESIAN_POINT('Ctrl Pts',(8.40709634751579,6.55000000003438,-4.48675184875404)) ;
#104268 = CARTESIAN_POINT('Ctrl Pts',(8.41193897064716,6.55000000006908,-4.46899230783935)) ;
#104269 = CARTESIAN_POINT('Ctrl Pts',(8.41916594308319,6.55000000013771,-4.45192888813902)) ;
#104270 = CARTESIAN_POINT('Ctrl Pts',(8.42853896333909,6.55000000013582,-4.43608126731276)) ;
#104271 = CARTESIAN_POINT('Ctrl Pts',(8.43455058706114,6.55000000013461,-4.42591699467746)) ;
#104272 = CARTESIAN_POINT('Ctrl Pts',(8.44144611055395,6.55000000009671,-4.416253000721)) ;
#104273 = CARTESIAN_POINT('Ctrl Pts',(8.44917210140206,6.55000000005186,-4.40723268310165)) ;
#104274 = CARTESIAN_POINT('Ctrl Pts',(8.44936219523639,6.55000000005075,-4.40701074305579)) ;
#104275 = CARTESIAN_POINT('Ctrl Pts',(8.44955278293316,6.55000000004968,-4.40678920228627)) ;
#104276 = CARTESIAN_POINT('Ctrl Pts',(8.44974386351697,6.55000000004865,-4.40656806301674)) ;
#104277 = CARTESIAN_POINT('Ctrl Pts',(8.45766118910685,6.55000000000559,-4.39740527126338)) ;
#104278 = CARTESIAN_POINT('Ctrl Pts',(8.46628870646479,6.54999999999864,-4.38902155150326)) ;
#104279 = CARTESIAN_POINT('Ctrl Pts',(8.47555348469884,6.55000000000007,-4.38133527594906)) ;
#104280 = CARTESIAN_POINT('Ctrl Pts',(8.48448851770303,6.55000000000144,-4.37392256470859)) ;
#104281 = CARTESIAN_POINT('Ctrl Pts',(8.49410273695376,6.5500000000304,-4.36723469297055)) ;
#104282 = CARTESIAN_POINT('Ctrl Pts',(8.50391213313781,6.55000000016212,-4.36082389577119)) ;
#104283 = CARTESIAN_POINT('Ctrl Pts',(8.50409415224108,6.55000000016456,-4.3607049396667)) ;
#104284 = CARTESIAN_POINT('Ctrl Pts',(8.50427622716234,6.55000000016576,-4.36058605979315)) ;
#104285 = CARTESIAN_POINT('Ctrl Pts',(8.50445835579895,6.55000000016577,-4.36046725463206)) ;
#104286 = CARTESIAN_POINT('Ctrl Pts',(8.50464048443556,6.55000000016577,-4.36034844947096)) ;
#104287 = CARTESIAN_POINT('Ctrl Pts',(8.50482266678753,6.55000000016459,-4.36022971902233)) ;
#104288 = CARTESIAN_POINT('Ctrl Pts',(8.50500490075221,6.55000000016234,-4.36011106176766)) ;
#104289 = CARTESIAN_POINT('Ctrl Pts',(8.50970297364421,6.55000000010443,-4.35705202481731)) ;
#104290 = CARTESIAN_POINT('Ctrl Pts',(8.51460443926437,6.55000000028677,-4.35427565407058)) ;
#104291 = CARTESIAN_POINT('Ctrl Pts',(8.5187483092633,6.55000000038295,-4.35043698472842)) ;
#104292 = CARTESIAN_POINT('Ctrl Pts',(8.51909542442958,6.550000000391,-4.35011543498209)) ;
#104293 = CARTESIAN_POINT('Ctrl Pts',(8.51943721516333,6.55000000039357,-4.34978641450153)) ;
#104294 = CARTESIAN_POINT('Ctrl Pts',(8.51977310187182,6.55000000039098,-4.3494491161473)) ;
#104295 = CARTESIAN_POINT('Ctrl Pts',(8.52085916897636,6.5500000003826,-4.34835848458113)) ;
#104296 = CARTESIAN_POINT('Ctrl Pts',(8.52182399801739,6.55000000033868,-4.347044620882)) ;
#104297 = CARTESIAN_POINT('Ctrl Pts',(8.52246334063461,6.55000000029842,-4.34562676665967)) ;
#104298 = CARTESIAN_POINT('Ctrl Pts',(8.52278301194322,6.55000000027829,-4.34491783954851)) ;
#104299 = CARTESIAN_POINT('Ctrl Pts',(8.52302131164588,6.55000000025926,-4.34418291480655)) ;
#104300 = CARTESIAN_POINT('Ctrl Pts',(8.52315270869754,6.55000000024662,-4.343436897635)) ;
#104301 = CARTESIAN_POINT('Ctrl Pts',(8.5232841057492,6.55000000023398,-4.34269088046346)) ;
#104302 = CARTESIAN_POINT('Ctrl Pts',(8.52330860014988,6.55000000022778,-4.34193377086234)) ;
#104303 = CARTESIAN_POINT('Ctrl Pts',(8.52320066085452,6.55000000023233,-4.34118047403285)) ;
#104304 = CARTESIAN_POINT('Ctrl Pts',(8.52284031330749,6.55000000024754,-4.33866564693691)) ;
#104305 = CARTESIAN_POINT('Ctrl Pts',(8.52133564423351,6.55000000029586,-4.33640673801311)) ;
#104306 = CARTESIAN_POINT('Ctrl Pts',(8.5196587899188,6.55000000031744,-4.33439865149543)) ;
#104307 = CARTESIAN_POINT('Ctrl Pts',(8.51932554032813,6.55000000032173,-4.33399957448309)) ;
#104308 = CARTESIAN_POINT('Ctrl Pts',(8.51898545723479,6.55000000032523,-4.33361037576486)) ;
#104309 = CARTESIAN_POINT('Ctrl Pts',(8.51864615038492,6.55000000032769,-4.33323101231938)) ;
#104310 = CARTESIAN_POINT('Ctrl Pts',(8.5145508165866,6.55000000035749,-4.32865220720328)) ;
#104311 = CARTESIAN_POINT('Ctrl Pts',(8.50963987409779,6.55000000028079,-4.32482020861865)) ;
#104312 = CARTESIAN_POINT('Ctrl Pts',(8.5048217738226,6.55000000018959,-4.32096887012539)) ;
#104313 = CARTESIAN_POINT('Ctrl Pts',(8.5004640292375,6.5500000001071,-4.31748551600118)) ;
#104314 = CARTESIAN_POINT('Ctrl Pts',(8.49606692679176,6.55000000001227,-4.31404901054623)) ;
#104315 = CARTESIAN_POINT('Ctrl Pts',(8.49172374697018,6.55000000000105,-4.3105442543438)) ;
#104316 = CARTESIAN_POINT('',(8.49172374697018,6.55,-7.62)) ;
#104317 = CARTESIAN_POINT('',(-0.9,6.55,-4.23)) ;
#104318 = CARTESIAN_POINT('',(-0.900000000000001,6.55,-7.62)) ;
#104319 = CARTESIAN_POINT('',(1.15,6.55,-4.23)) ;
#104320 = CARTESIAN_POINT('',(1.25,6.55,-4.23)) ;
#104321 = CARTESIAN_POINT('',(1.35,6.55,-4.43)) ;
#104322 = CARTESIAN_POINT('Origin',(1.15,6.55,-4.43)) ;
#104323 = CARTESIAN_POINT('',(1.35,6.55,-5.73)) ;
#104324 = CARTESIAN_POINT('',(1.35,6.55,-5.83)) ;
#104325 = CARTESIAN_POINT('',(1.15,6.55,-5.93)) ;
#104326 = CARTESIAN_POINT('Origin',(1.15,6.55,-5.73)) ;
#104327 = CARTESIAN_POINT('',(-0.9,6.55,-5.93)) ;
#104328 = CARTESIAN_POINT('',(1.25,6.55,-5.93)) ;
#104329 = CARTESIAN_POINT('',(-0.9,6.55,-7.62)) ;
#104330 = CARTESIAN_POINT('Origin',(1.25,5.3,-7.62)) ;
#104331 = CARTESIAN_POINT('',(1.25,3.15,-6.7231676725155)) ;
#104332 = CARTESIAN_POINT('',(1.25,3.04189189189189,-6.54552792413544)) ;
#104333 = CARTESIAN_POINT('Origin',(1.25,2.95,-6.7231676725155)) ;
#104334 = CARTESIAN_POINT('',(1.25,3.15,-7.62)) ;
#104335 = CARTESIAN_POINT('',(1.25,4.45,-6.7231676725155)) ;
#104336 = CARTESIAN_POINT('',(1.25,4.45,-6.66113883008419)) ;
#104337 = CARTESIAN_POINT('',(1.25,4.55810810810811,-6.54552792413544)) ;
#104338 = CARTESIAN_POINT('Origin',(1.25,4.65,-6.7231676725155)) ;
#104339 = CARTESIAN_POINT('',(1.25,5.26552792413544,-5.83810810810811)) ;
#104340 = CARTESIAN_POINT('Origin',(1.25,3.8,-5.08)) ;
#104341 = CARTESIAN_POINT('',(1.25,5.4431676725155,-5.73)) ;
#104342 = CARTESIAN_POINT('Origin',(1.25,5.4431676725155,-5.93)) ;
#104343 = CARTESIAN_POINT('',(1.25,6.45,-5.73)) ;
#104344 = CARTESIAN_POINT('',(1.25,6.55,-5.73)) ;
#104345 = CARTESIAN_POINT('',(1.25,6.45,-4.43)) ;
#104346 = CARTESIAN_POINT('',(1.25,6.45,-4.33)) ;
#104347 = CARTESIAN_POINT('',(1.25,5.4431676725155,-4.43)) ;
#104348 = CARTESIAN_POINT('',(1.25,5.38113883008419,-4.43)) ;
#104349 = CARTESIAN_POINT('',(1.25,5.26552792413544,-4.32189189189189)) ;
#104350 = CARTESIAN_POINT('Origin',(1.25,5.4431676725155,-4.23)) ;
#104351 = CARTESIAN_POINT('',(1.25,4.55810810810811,-3.61447207586456)) ;
#104352 = CARTESIAN_POINT('Origin',(1.25,3.8,-5.08)) ;
#104353 = CARTESIAN_POINT('',(1.25,4.45,-3.4368323274845)) ;
#104354 = CARTESIAN_POINT('Origin',(1.25,4.65,-3.4368323274845)) ;
#104355 = CARTESIAN_POINT('',(1.25,4.45,-2.54)) ;
#104356 = CARTESIAN_POINT('',(1.25,3.15,-3.4368323274845)) ;
#104357 = CARTESIAN_POINT('',(1.25,3.15,-3.49886116991581)) ;
#104358 = CARTESIAN_POINT('',(1.25,3.04189189189189,-3.61447207586456)) ;
#104359 = CARTESIAN_POINT('Origin',(1.25,2.95,-3.4368323274845)) ;
#104360 = CARTESIAN_POINT('',(1.25,2.33447207586456,-4.32189189189189)) ;
#104361 = CARTESIAN_POINT('Origin',(1.25,3.8,-5.08)) ;
#104362 = CARTESIAN_POINT('',(1.25,2.1568323274845,-4.43)) ;
#104363 = CARTESIAN_POINT('Origin',(1.25,2.1568323274845,-4.23)) ;
#104364 = CARTESIAN_POINT('',(1.25,0.973783447787483,-4.43)) ;
#104365 = CARTESIAN_POINT('',(1.25,0.895262490344437,-4.43)) ;
#104366 = CARTESIAN_POINT('',(1.25,0.973783447787483,-5.73)) ;
#104367 = CARTESIAN_POINT('Origin',(1.25,3.8,-5.08)) ;
#104368 = CARTESIAN_POINT('',(1.25,2.1568323274845,-5.73)) ;
#104369 = CARTESIAN_POINT('',(1.25,2.21886116991581,-5.73)) ;
#104370 = CARTESIAN_POINT('',(1.25,2.33447207586456,-5.83810810810811)) ;
#104371 = CARTESIAN_POINT('Origin',(1.25,2.1568323274845,-5.93)) ;
#104372 = CARTESIAN_POINT('Origin',(1.25,3.8,-5.08)) ;
#104373 = CARTESIAN_POINT('Origin',(-2.,0.,-7.62)) ;
#104374 = CARTESIAN_POINT('',(0.899999999999999,0.,-6.68)) ;
#104375 = CARTESIAN_POINT('',(1.1,0.,-6.48)) ;
#104376 = CARTESIAN_POINT('Origin',(0.899999999999999,0.,-6.48)) ;
#104377 = CARTESIAN_POINT('',(-2.,0.,-6.68)) ;
#104378 = CARTESIAN_POINT('',(-2.,0.,-6.68)) ;
#104379 = CARTESIAN_POINT('',(-2.,0.,-7.62)) ;
#104380 = CARTESIAN_POINT('',(9.9,0.,-7.62)) ;
#104381 = CARTESIAN_POINT('',(-2.,0.,-3.48)) ;
#104382 = CARTESIAN_POINT('',(-2.,0.,-7.62)) ;
#104383 = CARTESIAN_POINT('',(0.899999999999999,0.,-3.48)) ;
#104384 = CARTESIAN_POINT('',(0.999999999999999,0.,-3.48)) ;
#104385 = CARTESIAN_POINT('',(1.1,0.,-3.68)) ;
#104386 = CARTESIAN_POINT('Origin',(0.899999999999999,0.,-3.68)) ;
#104387 = CARTESIAN_POINT('',(1.1,0.,-6.58)) ;
#104388 = CARTESIAN_POINT('Origin',(-2.,7.65,-7.62)) ;
#104389 = CARTESIAN_POINT('',(-2.,6.9,-3.48)) ;
#104390 = CARTESIAN_POINT('',(-2.,7.1,-3.68)) ;
#104391 = CARTESIAN_POINT('Origin',(-2.,6.9,-3.68)) ;
#104392 = CARTESIAN_POINT('',(-2.,-1.13380619344889E-17,-3.48)) ;
#104393 = CARTESIAN_POINT('',(-2.,7.55,-7.62)) ;
#104394 = CARTESIAN_POINT('',(-2.,6.9,-6.68)) ;
#104395 = CARTESIAN_POINT('',(-2.,7.,-6.68)) ;
#104396 = CARTESIAN_POINT('',(-2.,7.1,-6.48)) ;
#104397 = CARTESIAN_POINT('Origin',(-2.,6.9,-6.48)) ;
#104398 = CARTESIAN_POINT('',(-2.,7.1,-3.58)) ;
#104399 = CARTESIAN_POINT('Origin',(-1.8,7.,-3.58)) ;
#104400 = CARTESIAN_POINT('',(-1.7,0.1,-3.58)) ;
#104401 = CARTESIAN_POINT('',(-1.9,0.1,-3.58)) ;
#104402 = CARTESIAN_POINT('',(-2.,0.1,-3.58)) ;
#104403 = CARTESIAN_POINT('',(-1.9,0.3,-3.58)) ;
#104404 = CARTESIAN_POINT('',(-1.9,7.,-3.58)) ;
#104405 = CARTESIAN_POINT('Origin',(-1.7,0.3,-3.58)) ;
#104406 = CARTESIAN_POINT('Origin',(-1.8,7.,-6.58)) ;
#104407 = CARTESIAN_POINT('',(-1.9,0.3,-6.58)) ;
#104408 = CARTESIAN_POINT('',(-1.7,0.1,-6.58)) ;
#104409 = CARTESIAN_POINT('Origin',(-1.7,0.3,-6.58)) ;
#104410 = CARTESIAN_POINT('',(-1.9,0.1,-6.58)) ;
#104411 = CARTESIAN_POINT('',(-1.9,1.23908819712629E-17,-6.58)) ;
#104412 = CARTESIAN_POINT('',(0.999999999999999,0.1,-6.58)) ;
#104413 = CARTESIAN_POINT('Origin',(-1.8,-2.2514151555628E-16,-5.08)) ;
#104414 = CARTESIAN_POINT('',(-1.8,4.6,-5.73)) ;
#104415 = CARTESIAN_POINT('',(-1.8,4.6,-4.43)) ;
#104416 = CARTESIAN_POINT('',(-1.8,4.6,-4.53)) ;
#104417 = CARTESIAN_POINT('',(-1.8,0.3,-4.43)) ;
#104418 = CARTESIAN_POINT('',(-1.8,0.2,-4.43)) ;
#104419 = CARTESIAN_POINT('',(-1.8,0.3,-3.68)) ;
#104420 = CARTESIAN_POINT('',(-1.8,0.3,-3.58)) ;
#104421 = CARTESIAN_POINT('',(-1.8,6.9,-3.68)) ;
#104422 = CARTESIAN_POINT('',(-1.8,-5.16691679585995E-17,-3.68)) ;
#104423 = CARTESIAN_POINT('',(-1.8,6.9,-6.48)) ;
#104424 = CARTESIAN_POINT('',(-1.8,6.9,-5.08)) ;
#104425 = CARTESIAN_POINT('',(-1.8,0.3,-6.48)) ;
#104426 = CARTESIAN_POINT('',(-1.8,-3.98613863153961E-16,-6.48)) ;
#104427 = CARTESIAN_POINT('',(-1.8,0.3,-5.73)) ;
#104428 = CARTESIAN_POINT('',(-1.8,0.3,-5.63)) ;
#104429 = CARTESIAN_POINT('',(-1.8,4.5,-5.73)) ;
#104430 = CARTESIAN_POINT('Origin',(0.549999999999999,4.5,-4.53)) ;
#104431 = CARTESIAN_POINT('',(-1.7,0.3,-4.53)) ;
#104432 = CARTESIAN_POINT('',(-1.7,4.4,-4.53)) ;
#104433 = CARTESIAN_POINT('',(-1.7,4.5,-4.53)) ;
#104434 = CARTESIAN_POINT('',(0.45,4.4,-4.53)) ;
#104435 = CARTESIAN_POINT('',(0.45,4.4,-4.53)) ;
#104436 = CARTESIAN_POINT('',(0.45,0.3,-4.53)) ;
#104437 = CARTESIAN_POINT('',(0.45,4.5,-4.53)) ;
#104438 = CARTESIAN_POINT('',(0.549999999999999,0.3,-4.53)) ;
#104439 = CARTESIAN_POINT('Origin',(0.549999999999999,4.5,-5.63)) ;
#104440 = CARTESIAN_POINT('',(0.45,0.3,-5.63)) ;
#104441 = CARTESIAN_POINT('',(0.45,4.4,-5.63)) ;
#104442 = CARTESIAN_POINT('',(0.45,4.5,-5.63)) ;
#104443 = CARTESIAN_POINT('',(-1.7,4.4,-5.63)) ;
#104444 = CARTESIAN_POINT('',(-1.7,4.4,-5.63)) ;
#104445 = CARTESIAN_POINT('',(-1.7,0.3,-5.63)) ;
#104446 = CARTESIAN_POINT('',(-1.7,0.2,-5.63)) ;
#104447 = CARTESIAN_POINT('',(0.549999999999999,0.3,-5.63)) ;
#104448 = CARTESIAN_POINT('Origin',(0.549999999999999,4.5,-5.63)) ;
#104449 = CARTESIAN_POINT('',(-1.7,4.5,-4.63)) ;
#104450 = CARTESIAN_POINT('',(-1.7,4.5,-5.53)) ;
#104451 = CARTESIAN_POINT('',(-1.7,4.5,-5.63)) ;
#104452 = CARTESIAN_POINT('',(0.45,4.5,-5.53)) ;
#104453 = CARTESIAN_POINT('',(0.45,4.5,-5.53)) ;
#104454 = CARTESIAN_POINT('',(0.45,4.5,-4.63)) ;
#104455 = CARTESIAN_POINT('',(0.45,4.5,-5.63)) ;
#104456 = CARTESIAN_POINT('',(-1.7,4.5,-4.63)) ;
#104457 = CARTESIAN_POINT('Origin',(0.55,3.09772049281573E-17,-5.08)) ;
#104458 = CARTESIAN_POINT('',(0.55,2.61224989991992,-5.48)) ;
#104459 = CARTESIAN_POINT('',(0.55,2.65280931275608,-5.53)) ;
#104460 = CARTESIAN_POINT('Ctrl Pts',(0.55,2.61224989991992,-5.48)) ;
#104461 = CARTESIAN_POINT('Ctrl Pts',(0.55,2.61224989991992,-5.48386974416198)) ;
#104462 = CARTESIAN_POINT('Ctrl Pts',(0.55,2.61317624258758,-5.48842010391569)) ;
#104463 = CARTESIAN_POINT('Ctrl Pts',(0.55,2.61634258087509,-5.49663300085887)) ;
#104464 = CARTESIAN_POINT('Ctrl Pts',(0.55,2.61951410407877,-5.50163042864529)) ;
#104465 = CARTESIAN_POINT('Ctrl Pts',(0.55,2.63040394024853,-5.51493871907015)) ;
#104466 = CARTESIAN_POINT('Ctrl Pts',(0.55,2.64148366881061,-5.52317058096742)) ;
#104467 = CARTESIAN_POINT('Ctrl Pts',(0.55,2.65280931275608,-5.53)) ;
#104468 = CARTESIAN_POINT('',(0.55,0.3,-5.53)) ;
#104469 = CARTESIAN_POINT('',(0.55,1.39397422176708E-16,-5.53)) ;
#104470 = CARTESIAN_POINT('',(0.55,0.3,-4.63)) ;
#104471 = CARTESIAN_POINT('',(0.55,0.3,-4.53)) ;
#104472 = CARTESIAN_POINT('',(0.55,2.65280931275594,-4.63000000000009)) ;
#104473 = CARTESIAN_POINT('',(0.55,6.35032701027224E-17,-4.63)) ;
#104474 = CARTESIAN_POINT('',(0.55,2.61224989991992,-4.68)) ;
#104475 = CARTESIAN_POINT('Ctrl Pts',(0.55,2.65280931275594,-4.63000000000009)) ;
#104476 = CARTESIAN_POINT('Ctrl Pts',(0.55,2.64148366881051,-4.63682941903265)) ;
#104477 = CARTESIAN_POINT('Ctrl Pts',(0.55,2.6304039402485,-4.64506128092989)) ;
#104478 = CARTESIAN_POINT('Ctrl Pts',(0.55,2.61951410407877,-4.6583695713547)) ;
#104479 = CARTESIAN_POINT('Ctrl Pts',(0.55,2.61634258087509,-4.66336699914112)) ;
#104480 = CARTESIAN_POINT('Ctrl Pts',(0.55,2.61317624258758,-4.67157989608431)) ;
#104481 = CARTESIAN_POINT('Ctrl Pts',(0.55,2.61224989991992,-4.67613025583802)) ;
#104482 = CARTESIAN_POINT('Ctrl Pts',(0.55,2.61224989991992,-4.68)) ;
#104483 = CARTESIAN_POINT('',(0.55,2.61224989991992,-4.58)) ;
#104484 = CARTESIAN_POINT('Origin',(0.,0.2,-5.08)) ;
#104485 = CARTESIAN_POINT('',(-1.7,0.2,-5.73)) ;
#104486 = CARTESIAN_POINT('',(-1.7,0.2,-6.48)) ;
#104487 = CARTESIAN_POINT('',(-1.7,0.2,-6.58)) ;
#104488 = CARTESIAN_POINT('',(0.899999999999999,0.2,-6.48)) ;
#104489 = CARTESIAN_POINT('',(0.999999999999999,0.2,-6.48)) ;
#104490 = CARTESIAN_POINT('',(0.899999999999999,0.2,-3.68)) ;
#104491 = CARTESIAN_POINT('',(0.899999999999999,0.2,-3.58)) ;
#104492 = CARTESIAN_POINT('',(-1.7,0.2,-3.68)) ;
#104493 = CARTESIAN_POINT('',(-1.8,0.2,-3.68)) ;
#104494 = CARTESIAN_POINT('',(-1.7,0.2,-4.43)) ;
#104495 = CARTESIAN_POINT('',(-1.7,0.2,-4.53)) ;
#104496 = CARTESIAN_POINT('',(0.65,0.2,-4.43)) ;
#104497 = CARTESIAN_POINT('',(-1.16429916652874E-32,0.2,-4.43)) ;
#104498 = CARTESIAN_POINT('',(0.65,0.2,-5.73)) ;
#104499 = CARTESIAN_POINT('',(0.65,0.2,-5.63)) ;
#104500 = CARTESIAN_POINT('',(-1.35834902761687E-32,0.2,-5.73)) ;
#104501 = CARTESIAN_POINT('Origin',(3.,2.3,-7.62)) ;
#104502 = CARTESIAN_POINT('',(3.,4.2,-4.58)) ;
#104503 = CARTESIAN_POINT('',(3.,3.4,-4.58)) ;
#104504 = CARTESIAN_POINT('',(3.,2.3,-4.58)) ;
#104505 = CARTESIAN_POINT('',(3.,4.3,-4.68)) ;
#104506 = CARTESIAN_POINT('Origin',(3.,4.2,-4.68)) ;
#104507 = CARTESIAN_POINT('',(3.,4.3,-5.48)) ;
#104508 = CARTESIAN_POINT('',(3.,4.3,-7.62)) ;
#104509 = CARTESIAN_POINT('',(3.,4.2,-5.58)) ;
#104510 = CARTESIAN_POINT('Origin',(3.,4.2,-5.48)) ;
#104511 = CARTESIAN_POINT('',(3.,3.4,-5.58)) ;
#104512 = CARTESIAN_POINT('',(3.,2.3,-5.58)) ;
#104513 = CARTESIAN_POINT('',(3.,3.3,-5.48)) ;
#104514 = CARTESIAN_POINT('Origin',(3.,3.4,-5.48)) ;
#104515 = CARTESIAN_POINT('',(3.,3.3,-4.68)) ;
#104516 = CARTESIAN_POINT('',(3.,3.3,-7.62)) ;
#104517 = CARTESIAN_POINT('Origin',(3.,3.4,-4.68)) ;
#104518 = CARTESIAN_POINT('Origin',(-1.,3.8,-5.08)) ;
#104519 = CARTESIAN_POINT('',(-1.,1.6,-7.04214168703487)) ;
#104520 = CARTESIAN_POINT('',(-1.,1.55483870967742,-6.91555190077455)) ;
#104521 = CARTESIAN_POINT('Origin',(-1.,1.40000000000001,-7.04214168703487)) ;
#104522 = CARTESIAN_POINT('',(-1.,1.6,-7.62)) ;
#104523 = CARTESIAN_POINT('',(-1.,2.95,-6.7231676725155)) ;
#104524 = CARTESIAN_POINT('',(-1.,2.95,-5.08)) ;
#104525 = CARTESIAN_POINT('',(-1.,2.1568323274845,-5.93)) ;
#104526 = CARTESIAN_POINT('Origin',(-1.,3.8,-5.08)) ;
#104527 = CARTESIAN_POINT('',(-1.,1.02736587339765,-5.93)) ;
#104528 = CARTESIAN_POINT('',(-1.,3.8,-5.93)) ;
#104529 = CARTESIAN_POINT('Origin',(-1.,3.8,-5.08)) ;
#104530 = CARTESIAN_POINT('Origin',(-1.,3.05,-7.63)) ;
#104531 = CARTESIAN_POINT('',(1.15,3.05,-6.7231676725155)) ;
#104532 = CARTESIAN_POINT('',(1.15,3.05,-6.66113883008419)) ;
#104533 = CARTESIAN_POINT('',(-0.900000000000002,3.05,-6.7231676725155)) ;
#104534 = CARTESIAN_POINT('',(-1.,3.05,-6.7231676725155)) ;
#104535 = CARTESIAN_POINT('',(-0.900000000000002,3.05,-7.63)) ;
#104536 = CARTESIAN_POINT('Origin',(-1.,2.21886116991581,-5.83)) ;
#104537 = CARTESIAN_POINT('',(-0.900000000000002,2.1568323274845,-5.83)) ;
#104538 = CARTESIAN_POINT('',(1.15,2.1568323274845,-5.83)) ;
#104539 = CARTESIAN_POINT('',(1.25,2.1568323274845,-5.83)) ;
#104540 = CARTESIAN_POINT('',(1.15,0.895262490344437,-5.83)) ;
#104541 = CARTESIAN_POINT('',(-0.900000000000002,2.21886116991581,-5.83)) ;
#104542 = CARTESIAN_POINT('Origin',(-1.,3.8,-5.08)) ;
#104543 = CARTESIAN_POINT('',(-0.900000000000002,2.24565220167453,-5.88405405405406)) ;
#104544 = CARTESIAN_POINT('',(-0.900000000000001,2.99594594594595,-6.63434779832547)) ;
#104545 = CARTESIAN_POINT('Origin',(-0.900000000000001,3.8,-5.08)) ;
#104546 = CARTESIAN_POINT('',(1.15,2.99594594594595,-6.63434779832547)) ;
#104547 = CARTESIAN_POINT('',(-1.,2.99594594594595,-6.63434779832547)) ;
#104548 = CARTESIAN_POINT('',(1.15,2.24565220167453,-5.88405405405406)) ;
#104549 = CARTESIAN_POINT('Origin',(1.15,3.8,-5.08)) ;
#104550 = CARTESIAN_POINT('',(-1.,2.24565220167453,-5.88405405405406)) ;
#104551 = CARTESIAN_POINT('Origin',(-1.,3.8,-5.08)) ;
#104552 = CARTESIAN_POINT('',(-0.900000000000002,2.99594594594594,-3.52565220167453)) ;
#104553 = CARTESIAN_POINT('',(-0.900000000000002,2.24565220167453,-4.27594594594595)) ;
#104554 = CARTESIAN_POINT('Origin',(-0.900000000000001,3.8,-5.08)) ;
#104555 = CARTESIAN_POINT('',(1.15,2.24565220167453,-4.27594594594595)) ;
#104556 = CARTESIAN_POINT('',(-1.,2.24565220167453,-4.27594594594595)) ;
#104557 = CARTESIAN_POINT('',(1.15,2.99594594594594,-3.52565220167453)) ;
#104558 = CARTESIAN_POINT('Origin',(1.15,3.8,-5.08)) ;
#104559 = CARTESIAN_POINT('',(-1.,2.99594594594594,-3.52565220167453)) ;
#104560 = CARTESIAN_POINT('Origin',(-1.,2.21886116991581,-4.33)) ;
#104561 = CARTESIAN_POINT('',(1.15,2.1568323274845,-4.33)) ;
#104562 = CARTESIAN_POINT('',(1.15,2.21886116991581,-4.33)) ;
#104563 = CARTESIAN_POINT('',(-0.900000000000002,2.1568323274845,-4.33)) ;
#104564 = CARTESIAN_POINT('',(-1.,2.1568323274845,-4.33)) ;
#104565 = CARTESIAN_POINT('',(-0.900000000000002,0.895262490344437,-4.33)) ;
#104566 = CARTESIAN_POINT('Origin',(-1.,3.05,-2.53)) ;
#104567 = CARTESIAN_POINT('',(-0.900000000000002,3.05,-3.4368323274845)) ;
#104568 = CARTESIAN_POINT('',(1.15,3.05,-3.4368323274845)) ;
#104569 = CARTESIAN_POINT('',(1.25,3.05,-3.4368323274845)) ;
#104570 = CARTESIAN_POINT('',(1.15,3.05,-2.54)) ;
#104571 = CARTESIAN_POINT('',(-0.900000000000002,3.05,-3.49886116991581)) ;
#104572 = CARTESIAN_POINT('Origin',(-1.,3.8,-5.08)) ;
#104573 = CARTESIAN_POINT('',(-1.,2.1568323274845,-4.23)) ;
#104574 = CARTESIAN_POINT('',(-1.,2.95,-3.4368323274845)) ;
#104575 = CARTESIAN_POINT('Origin',(-1.,3.8,-5.08)) ;
#104576 = CARTESIAN_POINT('',(-1.,2.95,-2.54)) ;
#104577 = CARTESIAN_POINT('',(-1.,1.6,-3.11785831296514)) ;
#104578 = CARTESIAN_POINT('',(-1.,1.6,-5.08)) ;
#104579 = CARTESIAN_POINT('',(-1.,1.55483870967743,-3.24444809922545)) ;
#104580 = CARTESIAN_POINT('Origin',(-1.,1.40000000000001,-3.11785831296514)) ;
#104581 = CARTESIAN_POINT('',(-1.,1.02736587339765,-4.23)) ;
#104582 = CARTESIAN_POINT('Origin',(-1.,3.8,-5.08)) ;
#104583 = CARTESIAN_POINT('',(-1.,2.21886116991581,-4.23)) ;
#104584 = CARTESIAN_POINT('Origin',(-1.,3.8,-5.08)) ;
#104585 = CARTESIAN_POINT('',(-1.,5.4431676725155,-5.93)) ;
#104586 = CARTESIAN_POINT('',(-1.,4.65,-6.7231676725155)) ;
#104587 = CARTESIAN_POINT('Origin',(-1.,3.8,-5.08)) ;
#104588 = CARTESIAN_POINT('',(-1.,4.65,-5.08)) ;
#104589 = CARTESIAN_POINT('',(-1.,6.45,-5.93)) ;
#104590 = CARTESIAN_POINT('',(-1.,6.45,-5.83)) ;
#104591 = CARTESIAN_POINT('',(-1.,3.8,-5.93)) ;
#104592 = CARTESIAN_POINT('Origin',(-1.,4.55,-6.66113883008419)) ;
#104593 = CARTESIAN_POINT('',(-0.900000000000001,4.55,-6.7231676725155)) ;
#104594 = CARTESIAN_POINT('',(1.15,4.55,-6.7231676725155)) ;
#104595 = CARTESIAN_POINT('',(1.25,4.55,-6.7231676725155)) ;
#104596 = CARTESIAN_POINT('',(1.15,4.55,-7.62)) ;
#104597 = CARTESIAN_POINT('',(-0.900000000000001,4.55,-6.66113883008419)) ;
#104598 = CARTESIAN_POINT('Origin',(-1.,3.8,-5.08)) ;
#104599 = CARTESIAN_POINT('',(-0.900000000000001,4.60405405405406,-6.63434779832547)) ;
#104600 = CARTESIAN_POINT('',(-0.900000000000001,5.35434779832547,-5.88405405405405)) ;
#104601 = CARTESIAN_POINT('Origin',(-0.900000000000001,3.8,-5.08)) ;
#104602 = CARTESIAN_POINT('',(1.15,5.35434779832547,-5.88405405405406)) ;
#104603 = CARTESIAN_POINT('',(-1.,5.35434779832547,-5.88405405405406)) ;
#104604 = CARTESIAN_POINT('',(1.15,4.60405405405405,-6.63434779832547)) ;
#104605 = CARTESIAN_POINT('Origin',(1.15,3.8,-5.08)) ;
#104606 = CARTESIAN_POINT('',(-1.,4.60405405405406,-6.63434779832547)) ;
#104607 = CARTESIAN_POINT('Origin',(-1.,6.55,-5.83)) ;
#104608 = CARTESIAN_POINT('',(-0.900000000000001,5.4431676725155,-5.83)) ;
#104609 = CARTESIAN_POINT('',(-0.9,6.45,-5.83)) ;
#104610 = CARTESIAN_POINT('',(-0.9,6.55,-5.83)) ;
#104611 = CARTESIAN_POINT('',(1.15,6.45,-5.83)) ;
#104612 = CARTESIAN_POINT('',(-1.,6.45,-5.83)) ;
#104613 = CARTESIAN_POINT('',(1.15,5.4431676725155,-5.83)) ;
#104614 = CARTESIAN_POINT('',(1.15,5.38113883008419,-5.83)) ;
#104615 = CARTESIAN_POINT('',(-1.,5.4431676725155,-5.83)) ;
#104616 = CARTESIAN_POINT('Origin',(-1.,3.8,-5.08)) ;
#104617 = CARTESIAN_POINT('',(-0.900000000000001,5.35434779832547,-4.27594594594594)) ;
#104618 = CARTESIAN_POINT('',(-0.900000000000001,4.60405405405405,-3.52565220167453)) ;
#104619 = CARTESIAN_POINT('Origin',(-0.900000000000001,3.8,-5.08)) ;
#104620 = CARTESIAN_POINT('',(1.15,4.60405405405405,-3.52565220167453)) ;
#104621 = CARTESIAN_POINT('',(-1.,4.60405405405405,-3.52565220167453)) ;
#104622 = CARTESIAN_POINT('',(1.15,5.35434779832547,-4.27594594594594)) ;
#104623 = CARTESIAN_POINT('Origin',(1.15,3.8,-5.08)) ;
#104624 = CARTESIAN_POINT('',(-1.,5.35434779832547,-4.27594594594594)) ;
#104625 = CARTESIAN_POINT('Origin',(-1.,4.55,-3.49886116991581)) ;
#104626 = CARTESIAN_POINT('',(1.15,4.55,-3.4368323274845)) ;
#104627 = CARTESIAN_POINT('',(1.15,4.55,-3.49886116991581)) ;
#104628 = CARTESIAN_POINT('',(-0.900000000000001,4.55,-3.4368323274845)) ;
#104629 = CARTESIAN_POINT('',(-1.,4.55,-3.4368323274845)) ;
#104630 = CARTESIAN_POINT('',(-0.900000000000001,4.55,-2.54)) ;
#104631 = CARTESIAN_POINT('Origin',(-1.,6.55,-4.33)) ;
#104632 = CARTESIAN_POINT('',(1.15,5.4431676725155,-4.33)) ;
#104633 = CARTESIAN_POINT('',(1.15,6.45,-4.33)) ;
#104634 = CARTESIAN_POINT('',(1.15,6.55,-4.33)) ;
#104635 = CARTESIAN_POINT('',(-0.9,6.45,-4.33)) ;
#104636 = CARTESIAN_POINT('',(-1.,6.45,-4.33)) ;
#104637 = CARTESIAN_POINT('',(-0.900000000000001,5.4431676725155,-4.33)) ;
#104638 = CARTESIAN_POINT('',(-0.900000000000001,5.38113883008419,-4.33)) ;
#104639 = CARTESIAN_POINT('',(1.25,5.4431676725155,-4.33)) ;
#104640 = CARTESIAN_POINT('Origin',(-1.,3.8,-5.08)) ;
#104641 = CARTESIAN_POINT('',(-1.,5.4431676725155,-4.23)) ;
#104642 = CARTESIAN_POINT('',(-1.,6.45,-4.23)) ;
#104643 = CARTESIAN_POINT('',(-1.,6.55,-4.23)) ;
#104644 = CARTESIAN_POINT('',(-1.,6.45,-5.08)) ;
#104645 = CARTESIAN_POINT('',(-1.,4.65,-3.4368323274845)) ;
#104646 = CARTESIAN_POINT('',(-1.,4.65,-3.49886116991581)) ;
#104647 = CARTESIAN_POINT('Origin',(-1.,3.8,-5.08)) ;
#104648 = CARTESIAN_POINT('Origin',(10.,4.35421736843756,-5.955)) ;
#104649 = CARTESIAN_POINT('',(9.91643989873054,7.72792407799439,-5.94107331645509)) ;
#104650 = CARTESIAN_POINT('',(8.58356010126947,8.17221734381475,-5.71892668354491)) ;
#104651 = CARTESIAN_POINT('',(8.47075240319158,8.20981990984071,-5.70012540053193)) ;
#104652 = CARTESIAN_POINT('',(8.58356010126947,6.66256607592813,-5.71892668354491)) ;
#104653 = CARTESIAN_POINT('',(8.58356010126947,6.64863939238321,-5.71892668354491)) ;
#104654 = CARTESIAN_POINT('',(9.91643989873054,6.8847127088383,-5.94107331645509)) ;
#104655 = CARTESIAN_POINT('',(9.98442535909739,6.89604361889945,-5.95240422651623)) ;
#104656 = CARTESIAN_POINT('',(9.91643989873054,7.8,-5.94107331645509)) ;
#104657 = CARTESIAN_POINT('Origin',(8.5,4.35421736843756,-5.705)) ;
#104658 = CARTESIAN_POINT('',(8.5,8.17221734381475,-5.6202872911617)) ;
#104659 = CARTESIAN_POINT('',(8.50000000129681,8.20000000266558,-5.62210562535302)) ;
#104660 = CARTESIAN_POINT('Origin',(8.5,8.17870774541385,-5.8090376393979)) ;
#104661 = CARTESIAN_POINT('',(8.5,8.2,-4.49634544369909)) ;
#104662 = CARTESIAN_POINT('',(8.5,6.66256607592813,-4.5397127088383)) ;
#104663 = CARTESIAN_POINT('',(8.5,6.64863939238321,-4.5397127088383)) ;
#104664 = CARTESIAN_POINT('',(8.50000000002143,6.64999999935441,-4.53931784432623)) ;
#104665 = CARTESIAN_POINT('Origin',(8.5,6.65811550100372,-4.34318848269215)) ;
#104666 = CARTESIAN_POINT('',(8.49999999999933,6.65000073218972,-5.62068969096366)) ;
#104667 = CARTESIAN_POINT('',(8.5,6.65,-5.80363939238321)) ;
#104668 = CARTESIAN_POINT('',(8.5,6.66256607592813,-5.6202872911617)) ;
#104669 = CARTESIAN_POINT('Origin',(8.5,6.65133313742082,-5.81701007179561)) ;
#104670 = CARTESIAN_POINT('',(8.5,8.20007071090457,-5.6202872911617)) ;
#104671 = CARTESIAN_POINT('Origin',(8.5,4.35421736843756,-4.455)) ;
#104672 = CARTESIAN_POINT('',(9.91643989873054,6.8847127088383,-4.21892668354491)) ;
#104673 = CARTESIAN_POINT('',(8.58356010126947,6.66256607592813,-4.44107331645509)) ;
#104674 = CARTESIAN_POINT('',(8.48442535909739,6.64604361889945,-4.45759577348377)) ;
#104675 = CARTESIAN_POINT('',(8.58356010126947,8.20007071090456,-4.44107331645509)) ;
#104676 = CARTESIAN_POINT('',(9.91643989873054,7.72792407799439,-4.21892668354491)) ;
#104677 = CARTESIAN_POINT('',(9.97075240319158,7.70981990984071,-4.20987459946807)) ;
#104678 = CARTESIAN_POINT('',(9.91643989873054,6.8,-4.21892668354491)) ;
#104679 = CARTESIAN_POINT('Origin',(8.5,3.65,-4.58)) ;
#104680 = CARTESIAN_POINT('',(8.45734623443633,3.62014236410543,-4.98206555615734)) ;
#104681 = CARTESIAN_POINT('',(8.02582401135442,3.3180768079481,-4.68)) ;
#104682 = CARTESIAN_POINT('',(8.34729988159781,3.54310991711847,-4.90503310917037)) ;
#104683 = CARTESIAN_POINT('',(8.02582401135442,3.31807680794809,-5.48)) ;
#104684 = CARTESIAN_POINT('',(8.02582401135442,3.3180768079481,-4.58)) ;
#104685 = CARTESIAN_POINT('',(8.45734623443633,3.62014236410543,-5.17793444384266)) ;
#104686 = CARTESIAN_POINT('',(8.70083523513316,3.79058466459322,-5.00749214335488)) ;
#104687 = CARTESIAN_POINT('',(8.45734623443633,3.62014236410543,-4.58)) ;
#104688 = CARTESIAN_POINT('Origin',(8.5,3.95,-4.58)) ;
#104689 = CARTESIAN_POINT('',(8.5,3.89793444384266,-5.17793444384266)) ;
#104690 = CARTESIAN_POINT('',(8.5,3.89793444384266,-4.98206555615734)) ;
#104691 = CARTESIAN_POINT('',(8.5,3.89793444384266,-4.58)) ;
#104692 = CARTESIAN_POINT('',(8.5,3.70206555615734,-4.98206555615734)) ;
#104693 = CARTESIAN_POINT('',(8.5,3.95,-4.98206555615734)) ;
#104694 = CARTESIAN_POINT('',(8.5,3.70206555615734,-5.17793444384266)) ;
#104695 = CARTESIAN_POINT('',(8.5,3.70206555615734,-4.58)) ;
#104696 = CARTESIAN_POINT('',(8.5,3.95,-5.17793444384266)) ;
#104697 = CARTESIAN_POINT('Origin',(8.,4.3,-4.58)) ;
#104698 = CARTESIAN_POINT('',(8.45734623443633,3.97985763589457,-5.17793444384266)) ;
#104699 = CARTESIAN_POINT('',(8.02582401135442,4.2819231920519,-5.48)) ;
#104700 = CARTESIAN_POINT('',(8.32457260887054,4.07279917379062,-5.27087598173872)) ;
#104701 = CARTESIAN_POINT('',(8.02582401135442,4.2819231920519,-4.68)) ;
#104702 = CARTESIAN_POINT('',(8.02582401135442,4.2819231920519,-4.58)) ;
#104703 = CARTESIAN_POINT('',(8.45734623443633,3.97985763589457,-4.98206555615734)) ;
#104704 = CARTESIAN_POINT('',(7.97103725533518,4.32027392126537,-4.64164927078653)) ;
#104705 = CARTESIAN_POINT('',(8.45734623443633,3.97985763589457,-4.58)) ;
#104706 = CARTESIAN_POINT('Origin',(1.5,2.3,-4.58)) ;
#104707 = CARTESIAN_POINT('',(7.96847777691809,3.4,-4.58)) ;
#104708 = CARTESIAN_POINT('',(8.,3.4,-4.58)) ;
#104709 = CARTESIAN_POINT('',(7.96847777691809,4.2,-4.58)) ;
#104710 = CARTESIAN_POINT('',(7.96847777691809,4.2,-4.58)) ;
#104711 = CARTESIAN_POINT('',(3.,4.2,-4.58)) ;
#104712 = CARTESIAN_POINT('Origin',(1.5,2.3,-5.58)) ;
#104713 = CARTESIAN_POINT('',(7.96847777691809,4.2,-5.58)) ;
#104714 = CARTESIAN_POINT('',(1.5,4.2,-5.58)) ;
#104715 = CARTESIAN_POINT('',(7.96847777691809,3.4,-5.58)) ;
#104716 = CARTESIAN_POINT('',(7.96847777691809,2.3,-5.58)) ;
#104717 = CARTESIAN_POINT('',(1.5,3.4,-5.58)) ;
#104718 = CARTESIAN_POINT('Origin',(8.,3.3,-4.58)) ;
#104719 = CARTESIAN_POINT('',(7.96847777691809,3.3,-5.48)) ;
#104720 = CARTESIAN_POINT('',(8.,3.3,-5.48)) ;
#104721 = CARTESIAN_POINT('',(7.96847777691809,3.3,-4.68)) ;
#104722 = CARTESIAN_POINT('',(7.96847777691809,3.3,-4.58)) ;
#104723 = CARTESIAN_POINT('',(3.,3.3,-4.68)) ;
#104724 = CARTESIAN_POINT('Origin',(1.5,4.3,-4.58)) ;
#104725 = CARTESIAN_POINT('',(7.96847777691809,4.3,-4.68)) ;
#104726 = CARTESIAN_POINT('',(8.,4.3,-4.68)) ;
#104727 = CARTESIAN_POINT('',(7.96847777691809,4.3,-5.48)) ;
#104728 = CARTESIAN_POINT('',(7.96847777691809,4.3,-4.58)) ;
#104729 = CARTESIAN_POINT('',(1.5,4.3,-5.48)) ;
#104730 = CARTESIAN_POINT('Origin',(1.5,2.3,-4.58)) ;
#104731 = CARTESIAN_POINT('',(-0.4,2.3,-4.58)) ;
#104732 = CARTESIAN_POINT('',(-0.4,-3.36847777691809,-4.58)) ;
#104733 = CARTESIAN_POINT('',(-0.4,-3.4,-4.58)) ;
#104734 = CARTESIAN_POINT('',(0.4,-3.36847777691809,-4.58)) ;
#104735 = CARTESIAN_POINT('',(0.4,-3.36847777691809,-4.58)) ;
#104736 = CARTESIAN_POINT('',(0.4,2.29999999999999,-4.58)) ;
#104737 = CARTESIAN_POINT('',(0.4,2.29999999999999,-4.58)) ;
#104738 = CARTESIAN_POINT('',(0.536602540378444,2.83090991212703,-4.58)) ;
#104739 = CARTESIAN_POINT('Origin',(1.5,2.3,-4.58)) ;
#104740 = CARTESIAN_POINT('',(0.536602540378444,3.93764017256378,-4.58)) ;
#104741 = CARTESIAN_POINT('',(0.536602540378444,2.83090991212703,-4.58)) ;
#104742 = CARTESIAN_POINT('Origin',(1.5,2.3,-4.58)) ;
#104743 = CARTESIAN_POINT('Origin',(1.5,2.3,-5.58)) ;
#104744 = CARTESIAN_POINT('',(0.4,2.29999999999999,-5.58)) ;
#104745 = CARTESIAN_POINT('',(0.4,-3.36847777691809,-5.58)) ;
#104746 = CARTESIAN_POINT('',(0.4,2.3,-5.58)) ;
#104747 = CARTESIAN_POINT('',(-0.4,-3.36847777691809,-5.58)) ;
#104748 = CARTESIAN_POINT('',(1.5,-3.36847777691809,-5.58)) ;
#104749 = CARTESIAN_POINT('',(-0.4,2.3,-5.58)) ;
#104750 = CARTESIAN_POINT('',(-0.4,2.3,-5.58)) ;
#104751 = CARTESIAN_POINT('',(0.536602540378444,3.93764017256378,-5.58)) ;
#104752 = CARTESIAN_POINT('Origin',(1.5,2.3,-5.58)) ;
#104753 = CARTESIAN_POINT('',(0.536602540378444,2.83090991212703,-5.58)) ;
#104754 = CARTESIAN_POINT('',(0.536602540378444,3.93764017256378,-5.58)) ;
#104755 = CARTESIAN_POINT('Origin',(1.5,2.3,-5.58)) ;
#104756 = CARTESIAN_POINT('Origin',(1.5,2.3,-4.58)) ;
#104757 = CARTESIAN_POINT('',(-0.5,2.3,-4.68)) ;
#104758 = CARTESIAN_POINT('',(-0.5,2.3,-5.48)) ;
#104759 = CARTESIAN_POINT('',(-0.5,2.3,-4.58)) ;
#104760 = CARTESIAN_POINT('Origin',(1.5,2.3,-4.68)) ;
#104761 = CARTESIAN_POINT('Origin',(1.5,2.3,-5.48)) ;
#104762 = CARTESIAN_POINT('Origin',(-0.5,-3.4,-4.58)) ;
#104763 = CARTESIAN_POINT('',(-0.5,-3.36847777691809,-5.48)) ;
#104764 = CARTESIAN_POINT('',(-0.5,-3.4,-5.48)) ;
#104765 = CARTESIAN_POINT('',(-0.5,-3.36847777691809,-4.68)) ;
#104766 = CARTESIAN_POINT('',(-0.5,-3.36847777691809,-4.58)) ;
#104767 = CARTESIAN_POINT('',(-0.5,2.3,-4.68)) ;
#104768 = CARTESIAN_POINT('Origin',(-0.15,-3.9,-4.58)) ;
#104769 = CARTESIAN_POINT('',(-0.179857635894567,-3.85734623443633,-4.98206555615734)) ;
#104770 = CARTESIAN_POINT('',(-0.481923192051905,-3.42582401135442,-4.68)) ;
#104771 = CARTESIAN_POINT('',(-0.256890082881532,-3.74729988159781,-4.90503310917037)) ;
#104772 = CARTESIAN_POINT('',(-0.481923192051905,-3.42582401135442,-5.48)) ;
#104773 = CARTESIAN_POINT('',(-0.481923192051905,-3.42582401135442,-4.58)) ;
#104774 = CARTESIAN_POINT('',(-0.179857635894567,-3.85734623443633,-5.17793444384266)) ;
#104775 = CARTESIAN_POINT('',(-0.00941533540678435,-4.10083523513317,-5.00749214335488)) ;
#104776 = CARTESIAN_POINT('',(-0.179857635894567,-3.85734623443633,-4.58)) ;
#104777 = CARTESIAN_POINT('Origin',(0.15,-3.9,-4.58)) ;
#104778 = CARTESIAN_POINT('',(0.0979344438426627,-3.9,-5.17793444384266)) ;
#104779 = CARTESIAN_POINT('',(0.0979344438426627,-3.9,-4.98206555615734)) ;
#104780 = CARTESIAN_POINT('',(0.0979344438426627,-3.9,-4.58)) ;
#104781 = CARTESIAN_POINT('',(-0.0979344438426628,-3.9,-4.98206555615734)) ;
#104782 = CARTESIAN_POINT('',(0.15,-3.9,-4.98206555615734)) ;
#104783 = CARTESIAN_POINT('',(-0.0979344438426628,-3.9,-5.17793444384266)) ;
#104784 = CARTESIAN_POINT('',(-0.0979344438426628,-3.9,-4.58)) ;
#104785 = CARTESIAN_POINT('',(0.15,-3.9,-5.17793444384266)) ;
#104786 = CARTESIAN_POINT('Origin',(0.5,-3.4,-4.58)) ;
#104787 = CARTESIAN_POINT('',(0.179857635894567,-3.85734623443633,-5.17793444384266)) ;
#104788 = CARTESIAN_POINT('',(0.481923192051904,-3.42582401135442,-5.48)) ;
#104789 = CARTESIAN_POINT('',(0.272799173790623,-3.72457260887054,-5.27087598173872)) ;
#104790 = CARTESIAN_POINT('',(0.481923192051904,-3.42582401135442,-4.68)) ;
#104791 = CARTESIAN_POINT('',(0.481923192051904,-3.42582401135442,-4.58)) ;
#104792 = CARTESIAN_POINT('',(0.179857635894567,-3.85734623443633,-4.98206555615734)) ;
#104793 = CARTESIAN_POINT('',(0.520273921265371,-3.37103725533519,-4.64164927078653)) ;
#104794 = CARTESIAN_POINT('',(0.179857635894567,-3.85734623443633,-4.58)) ;
#104795 = CARTESIAN_POINT('Origin',(0.5,2.29999999999999,-4.58)) ;
#104796 = CARTESIAN_POINT('',(0.500000000000001,2.29999999999999,-4.68)) ;
#104797 = CARTESIAN_POINT('',(0.5,-3.36847777691809,-4.68)) ;
#104798 = CARTESIAN_POINT('',(0.5,-3.4,-4.68)) ;
#104799 = CARTESIAN_POINT('',(0.5,-3.36847777691809,-5.48)) ;
#104800 = CARTESIAN_POINT('',(0.5,-3.36847777691809,-4.58)) ;
#104801 = CARTESIAN_POINT('',(0.500000000000001,2.29999999999999,-5.48)) ;
#104802 = CARTESIAN_POINT('',(0.5,2.29999999999999,-5.48)) ;
#104803 = CARTESIAN_POINT('',(0.500000000000001,2.29999999999999,-4.58)) ;
#104804 = CARTESIAN_POINT('Origin',(1.5,2.3,-4.58)) ;
#104805 = CARTESIAN_POINT('Origin',(1.5,2.3,-4.68)) ;
#104806 = CARTESIAN_POINT('Origin',(1.5,2.3,-5.48)) ;
#104807 = CARTESIAN_POINT('Origin',(8.,2.68967221921331,-5.58)) ;
#104808 = CARTESIAN_POINT('',(8.45734623443633,3.70206555615734,-5.25985763589457)) ;
#104809 = CARTESIAN_POINT('',(8.02582401135442,3.4,-5.5619231920519)) ;
#104810 = CARTESIAN_POINT('',(7.75526480758232,3.21060855735952,-5.75131463469238)) ;
#104811 = CARTESIAN_POINT('',(8.02582401135442,4.2,-5.5619231920519)) ;
#104812 = CARTESIAN_POINT('',(8.02582401135442,2.68967221921331,-5.5619231920519)) ;
#104813 = CARTESIAN_POINT('',(8.45734623443633,3.89793444384266,-5.25985763589457)) ;
#104814 = CARTESIAN_POINT('',(8.54034505662341,3.83983526831171,-5.20175846036362)) ;
#104815 = CARTESIAN_POINT('',(8.45734623443633,2.68967221921331,-5.25985763589457)) ;
#104816 = CARTESIAN_POINT('Origin',(8.,2.68967221921331,-4.58)) ;
#104817 = CARTESIAN_POINT('',(8.45734623443633,3.89793444384266,-4.90014236410543)) ;
#104818 = CARTESIAN_POINT('',(8.02582401135442,4.2,-4.5980768079481)) ;
#104819 = CARTESIAN_POINT('',(8.54034505662341,3.83983526831171,-4.95824153963639)) ;
#104820 = CARTESIAN_POINT('',(8.02582401135442,3.4,-4.5980768079481)) ;
#104821 = CARTESIAN_POINT('',(8.02582401135442,3.4,-4.5980768079481)) ;
#104822 = CARTESIAN_POINT('',(8.45734623443633,3.70206555615734,-4.90014236410543)) ;
#104823 = CARTESIAN_POINT('',(7.75526480758232,3.21060855735952,-4.40868536530762)) ;
#104824 = CARTESIAN_POINT('',(8.45734623443633,2.68967221921331,-4.90014236410543)) ;
#104825 = CARTESIAN_POINT('Origin',(-1.11032778078669,-3.9,-4.93)) ;
#104826 = CARTESIAN_POINT('',(0.0979344438426626,-3.85734623443633,-4.90014236410543)) ;
#104827 = CARTESIAN_POINT('',(0.4,-3.42582401135442,-4.5980768079481)) ;
#104828 = CARTESIAN_POINT('',(-0.223548570072128,-4.31660768288603,-5.22162537802022)) ;
#104829 = CARTESIAN_POINT('',(-0.400000000000001,-3.42582401135442,-4.5980768079481)) ;
#104830 = CARTESIAN_POINT('',(-0.400000000000001,-3.42582401135442,-4.5980768079481)) ;
#104831 = CARTESIAN_POINT('',(-0.0979344438426627,-3.85734623443633,-4.90014236410543)) ;
#104832 = CARTESIAN_POINT('',(-0.326007604256636,-3.53152743384494,-4.67206920369146)) ;
#104833 = CARTESIAN_POINT('',(-1.11032778078669,-3.85734623443633,-4.90014236410543)) ;
#104834 = CARTESIAN_POINT('Origin',(-1.11032778078669,-3.4,-5.58)) ;
#104835 = CARTESIAN_POINT('',(-0.0979344438426627,-3.85734623443633,-5.25985763589457)) ;
#104836 = CARTESIAN_POINT('',(-0.4,-3.42582401135442,-5.5619231920519)) ;
#104837 = CARTESIAN_POINT('',(-0.589391442640475,-3.15526480758232,-5.75131463469238)) ;
#104838 = CARTESIAN_POINT('',(0.400000000000001,-3.42582401135442,-5.5619231920519)) ;
#104839 = CARTESIAN_POINT('',(-1.11032778078669,-3.42582401135442,-5.5619231920519)) ;
#104840 = CARTESIAN_POINT('',(0.0979344438426626,-3.85734623443633,-5.25985763589457)) ;
#104841 = CARTESIAN_POINT('',(0.0398352683117103,-3.94034505662341,-5.20175846036361)) ;
#104842 = CARTESIAN_POINT('',(-1.11032778078669,-3.85734623443633,-5.25985763589457)) ;
#104843 = CARTESIAN_POINT('Origin',(10.,1.24999999999998,-7.62)) ;
#104844 = CARTESIAN_POINT('',(9.91643989873054,1.26392668354489,-3.0358381198218)) ;
#104845 = CARTESIAN_POINT('',(9.91643989873054,1.26392668354489,-7.62)) ;
#104846 = CARTESIAN_POINT('',(8.50816364570057,1.49863939238321,-3.11785831296514)) ;
#104847 = CARTESIAN_POINT('Origin',(43.7052916416609,-4.36754860786629,-611.768201693183)) ;
#104848 = CARTESIAN_POINT('',(8.50816364570057,1.49863939238321,-7.62)) ;
#104849 = CARTESIAN_POINT('Origin',(8.49999999999985,3.8,-5.08)) ;
#104850 = CARTESIAN_POINT('',(9.91643989873053,1.24322097942674,-3.09630356419405)) ;
#104851 = CARTESIAN_POINT('',(9.91643989873053,1.24322097942648,-7.06369643580562)) ;
#104852 = CARTESIAN_POINT('Origin',(9.91643989873053,3.8,-5.08)) ;
#104853 = CARTESIAN_POINT('Origin',(36.5480653059678,-40.380261828241,567.197654967682)) ;
#104854 = CARTESIAN_POINT('Origin',(36.5480653017837,-40.3802618313523,-577.357654913403)) ;
#104855 = CARTESIAN_POINT('Origin',(10.,1.24999999999998,-7.62)) ;
#104856 = CARTESIAN_POINT('',(8.50816364570059,1.49863939238321,-7.04214168703472)) ;
#104857 = CARTESIAN_POINT('',(8.50816364570057,1.49863939238321,-7.62)) ;
#104858 = CARTESIAN_POINT('',(9.91643989873054,1.26392668354489,-7.12416188017819)) ;
#104859 = CARTESIAN_POINT('Origin',(43.7052916530562,-4.3675486096968,601.608201900582)) ;
#104860 = CARTESIAN_POINT('',(9.91643989873054,1.26392668354489,-7.62)) ;
#104861 = CARTESIAN_POINT('Origin',(-0.900000000000001,4.65,-5.08)) ;
#104862 = CARTESIAN_POINT('Origin',(-0.900000000000001,4.65,-3.4368323274845)) ;
#104863 = CARTESIAN_POINT('Origin',(-0.900000000000001,4.65,-3.4368323274845)) ;
#104864 = CARTESIAN_POINT('Origin',(-0.900000000000001,4.65,-3.4368323274845)) ;
#104865 = CARTESIAN_POINT('Origin',(-0.900000000000001,4.65,-3.4368323274845)) ;
#104866 = CARTESIAN_POINT('Origin',(1.15,4.45,-3.49886116991581)) ;
#104867 = CARTESIAN_POINT('Origin',(1.15,4.45,-3.4368323274845)) ;
#104868 = CARTESIAN_POINT('Origin',(-1.,4.65,-3.4368323274845)) ;
#104869 = CARTESIAN_POINT('Origin',(1.15,4.65,-3.4368323274845)) ;
#104870 = CARTESIAN_POINT('Origin',(-0.900000000000001,3.8,-5.08)) ;
#104871 = CARTESIAN_POINT('Origin',(-0.900000000000001,5.4431676725155,-4.23)) ;
#104872 = CARTESIAN_POINT('Origin',(1.15,4.65,-3.4368323274845)) ;
#104873 = CARTESIAN_POINT('Origin',(1.15,4.55810810810811,-3.61447207586456)) ;
#104874 = CARTESIAN_POINT('Origin',(-0.900000000000001,5.4431676725155,-4.23)) ;
#104875 = CARTESIAN_POINT('Origin',(-0.900000000000001,5.4431676725155,-4.23)) ;
#104876 = CARTESIAN_POINT('Origin',(-0.900000000000001,5.4431676725155,-4.23)) ;
#104877 = CARTESIAN_POINT('Origin',(-0.900000000000001,4.65,-5.08)) ;
#104878 = CARTESIAN_POINT('Origin',(-0.900000000000001,4.65,-6.7231676725155)) ;
#104879 = CARTESIAN_POINT('Origin',(-1.,4.65,-6.7231676725155)) ;
#104880 = CARTESIAN_POINT('Origin',(1.15,4.65,-6.7231676725155)) ;
#104881 = CARTESIAN_POINT('Origin',(-0.900000000000001,4.65,-6.7231676725155)) ;
#104882 = CARTESIAN_POINT('Origin',(1.15,4.45,-6.66113883008419)) ;
#104883 = CARTESIAN_POINT('Origin',(1.15,4.45,-6.7231676725155)) ;
#104884 = CARTESIAN_POINT('Origin',(1.15,3.8,-5.08)) ;
#104885 = CARTESIAN_POINT('Origin',(1.15,5.26552792413544,-4.32189189189189)) ;
#104886 = CARTESIAN_POINT('Origin',(-1.,5.4431676725155,-4.23)) ;
#104887 = CARTESIAN_POINT('Origin',(1.15,5.4431676725155,-4.23)) ;
#104888 = CARTESIAN_POINT('Origin',(-0.900000000000001,3.8,-4.23)) ;
#104889 = CARTESIAN_POINT('Origin',(-0.9,6.45,-4.23)) ;
#104890 = CARTESIAN_POINT('Origin',(-0.9,6.45,-5.08)) ;
#104891 = CARTESIAN_POINT('Origin',(-0.9,6.45,-4.23)) ;
#104892 = CARTESIAN_POINT('Origin',(-0.900000000000001,4.65,-6.7231676725155)) ;
#104893 = CARTESIAN_POINT('Origin',(-0.900000000000001,4.65,-6.7231676725155)) ;
#104894 = CARTESIAN_POINT('Origin',(1.15,4.65,-6.7231676725155)) ;
#104895 = CARTESIAN_POINT('Origin',(1.15,4.55810810810811,-6.54552792413544)) ;
#104896 = CARTESIAN_POINT('Origin',(1.15,5.4431676725155,-4.23)) ;
#104897 = CARTESIAN_POINT('Origin',(1.15,5.4431676725155,-4.43)) ;
#104898 = CARTESIAN_POINT('Origin',(-0.9,6.45,-4.23)) ;
#104899 = CARTESIAN_POINT('Origin',(-0.9,6.45,-4.23)) ;
#104900 = CARTESIAN_POINT('Origin',(-0.900000000000001,3.8,-5.08)) ;
#104901 = CARTESIAN_POINT('Origin',(-0.900000000000001,5.4431676725155,-5.93)) ;
#104902 = CARTESIAN_POINT('Origin',(-1.,5.4431676725155,-5.93)) ;
#104903 = CARTESIAN_POINT('Origin',(1.15,5.4431676725155,-5.93)) ;
#104904 = CARTESIAN_POINT('Origin',(-0.900000000000001,5.4431676725155,-5.93)) ;
#104905 = CARTESIAN_POINT('Origin',(1.15,3.8,-5.08)) ;
#104906 = CARTESIAN_POINT('Origin',(1.15,5.26552792413544,-5.83810810810811)) ;
#104907 = CARTESIAN_POINT('Origin',(1.15,6.55,-4.43)) ;
#104908 = CARTESIAN_POINT('Origin',(1.15,6.45,-4.43)) ;
#104909 = CARTESIAN_POINT('Origin',(1.25,6.45,-4.23)) ;
#104910 = CARTESIAN_POINT('Origin',(1.15,6.45,-4.23)) ;
#104911 = CARTESIAN_POINT('Origin',(-0.900000000000001,5.4431676725155,-5.93)) ;
#104912 = CARTESIAN_POINT('Origin',(-0.900000000000001,5.4431676725155,-5.93)) ;
#104913 = CARTESIAN_POINT('Origin',(1.15,5.4431676725155,-5.93)) ;
#104914 = CARTESIAN_POINT('Origin',(1.15,5.4431676725155,-5.73)) ;
#104915 = CARTESIAN_POINT('Origin',(1.15,6.45,-4.43)) ;
#104916 = CARTESIAN_POINT('Origin',(1.35,6.45,-4.43)) ;
#104917 = CARTESIAN_POINT('Origin',(-0.9,6.45,-5.08)) ;
#104918 = CARTESIAN_POINT('Origin',(-0.9,6.45,-5.93)) ;
#104919 = CARTESIAN_POINT('Origin',(-0.900000000000001,3.8,-5.93)) ;
#104920 = CARTESIAN_POINT('Origin',(-0.9,6.45,-5.93)) ;
#104921 = CARTESIAN_POINT('Origin',(1.15,6.55,-5.73)) ;
#104922 = CARTESIAN_POINT('Origin',(1.15,6.45,-5.73)) ;
#104923 = CARTESIAN_POINT('Origin',(1.35,6.45,-7.62)) ;
#104924 = CARTESIAN_POINT('Origin',(1.35,6.45,-5.73)) ;
#104925 = CARTESIAN_POINT('Origin',(-0.9,6.45,-5.93)) ;
#104926 = CARTESIAN_POINT('Origin',(-0.9,6.45,-5.93)) ;
#104927 = CARTESIAN_POINT('Origin',(1.15,6.45,-5.73)) ;
#104928 = CARTESIAN_POINT('Origin',(1.15,6.45,-5.93)) ;
#104929 = CARTESIAN_POINT('Origin',(-1.,6.45,-5.93)) ;
#104930 = CARTESIAN_POINT('Origin',(-1.7,0.3,-5.73)) ;
#104931 = CARTESIAN_POINT('Origin',(-1.7,0.3,-5.73)) ;
#104932 = CARTESIAN_POINT('Origin',(-1.7,0.3,-5.73)) ;
#104933 = CARTESIAN_POINT('Origin',(-1.7,0.3,-5.73)) ;
#104934 = CARTESIAN_POINT('Origin',(0.549999999999999,0.3,-5.73)) ;
#104935 = CARTESIAN_POINT('',(0.50857864376269,0.229289321881345,-5.65928932188135)) ;
#104936 = CARTESIAN_POINT('Ctrl Pts',(0.65,0.2,-5.73)) ;
#104937 = CARTESIAN_POINT('Ctrl Pts',(0.639834283464151,0.2,-5.72491714173208)) ;
#104938 = CARTESIAN_POINT('Ctrl Pts',(0.629316849080535,0.200389688120422,
-5.71965768385801)) ;
#104939 = CARTESIAN_POINT('Ctrl Pts',(0.606957334719669,0.202165884217645,
-5.70846794971935)) ;
#104940 = CARTESIAN_POINT('Ctrl Pts',(0.595086727401099,0.203647820493442,
-5.70252276179493)) ;
#104941 = CARTESIAN_POINT('Ctrl Pts',(0.572283837380409,0.207685608831265,
-5.691106760396)) ;
#104942 = CARTESIAN_POINT('Ctrl Pts',(0.561337481650365,0.21017819324834,
-5.68562986130802)) ;
#104943 = CARTESIAN_POINT('Ctrl Pts',(0.549549942885299,0.213544620665569,
-5.6797406960393)) ;
#104944 = CARTESIAN_POINT('Ctrl Pts',(0.548290718945592,0.213913346522002,
-5.67911168276603)) ;
#104945 = CARTESIAN_POINT('Ctrl Pts',(0.536119229732643,0.217566912232546,
-5.67303275135176)) ;
#104946 = CARTESIAN_POINT('Ctrl Pts',(0.525706917362398,0.221400308602611,
-5.66784223842911)) ;
#104947 = CARTESIAN_POINT('Ctrl Pts',(0.513545110027183,0.226871185484688,
-5.6617711869643)) ;
#104948 = CARTESIAN_POINT('Ctrl Pts',(0.511029334128283,0.22806397669855,
-5.66051466706414)) ;
#104949 = CARTESIAN_POINT('Ctrl Pts',(0.50857864376269,0.229289321881343,
-5.65928932188135)) ;
#104950 = CARTESIAN_POINT('Origin',(0.664280054301624,0.302990743362135,-5.73714210424988)) ;
#104951 = CARTESIAN_POINT('Origin',(-1.7,4.5,-5.73)) ;
#104952 = CARTESIAN_POINT('',(-1.77071067811863,4.45857864376274,-5.65928932188132)) ;
#104953 = CARTESIAN_POINT('Origin',(-1.69703459697506,4.61417009505288,-5.73708668538063)) ;
#104954 = CARTESIAN_POINT('Ctrl Pts',(-1.77071067811863,4.45857864376274,
-5.65928932188132)) ;
#104955 = CARTESIAN_POINT('Ctrl Pts',(-1.77521675558366,4.46759079869281,
-5.66379539934635)) ;
#104956 = CARTESIAN_POINT('Ctrl Pts',(-1.77928079264422,4.47748625817296,
-5.66872648167164)) ;
#104957 = CARTESIAN_POINT('Ctrl Pts',(-1.78624680748626,4.49811277056884,
-5.6790208825478)) ;
#104958 = CARTESIAN_POINT('Ctrl Pts',(-1.78918030781792,4.50880509433485,
-5.68436398414911)) ;
#104959 = CARTESIAN_POINT('Ctrl Pts',(-1.79185985500292,4.52101859322041,
-5.69047475453283)) ;
#104960 = CARTESIAN_POINT('Ctrl Pts',(-1.79213045061227,4.52228751722709,
-5.69110970990894)) ;
#104961 = CARTESIAN_POINT('Ctrl Pts',(-1.79477467909828,4.53504937002863,
-5.69749628913391)) ;
#104962 = CARTESIAN_POINT('Ctrl Pts',(-1.79657370273651,4.54677936428202,
-5.70337157240614)) ;
#104963 = CARTESIAN_POINT('Ctrl Pts',(-1.79896007643135,4.56920025888388,
-5.71459577476113)) ;
#104964 = CARTESIAN_POINT('Ctrl Pts',(-1.79963010255187,4.57990192168148,
-5.71995007594496)) ;
#104965 = CARTESIAN_POINT('Ctrl Pts',(-1.79996164986962,4.59357116034292,
-5.726785573817)) ;
#104966 = CARTESIAN_POINT('Ctrl Pts',(-1.8,4.59680282631912,-5.72840141315956)) ;
#104967 = CARTESIAN_POINT('Ctrl Pts',(-1.8,4.6,-5.73)) ;
#104968 = CARTESIAN_POINT('Origin',(-1.7,0.3,-5.08)) ;
#104969 = CARTESIAN_POINT('Origin',(-1.7,0.3,-6.48)) ;
#104970 = CARTESIAN_POINT('Origin',(0.65,0.3,-5.08)) ;
#104971 = CARTESIAN_POINT('',(0.579289321881328,0.229289321881363,-5.58857864376273)) ;
#104972 = CARTESIAN_POINT('Origin',(0.657086685378504,0.302965403023971,-5.74417009504855)) ;
#104973 = CARTESIAN_POINT('Ctrl Pts',(0.579289321881328,0.229289321881363,
-5.58857864376273)) ;
#104974 = CARTESIAN_POINT('Ctrl Pts',(0.583795399346357,0.224783244416332,
-5.59759079869279)) ;
#104975 = CARTESIAN_POINT('Ctrl Pts',(0.588726481671639,0.220719207355779,
-5.60748625817292)) ;
#104976 = CARTESIAN_POINT('Ctrl Pts',(0.599020882547819,0.213753192513722,
-5.62811277056884)) ;
#104977 = CARTESIAN_POINT('Ctrl Pts',(0.604363984149159,0.210819692182048,
-5.6388050943349)) ;
#104978 = CARTESIAN_POINT('Ctrl Pts',(0.610474754532884,0.20814014499706,
-5.65101859322046)) ;
#104979 = CARTESIAN_POINT('Ctrl Pts',(0.611109709908967,0.207869549387718,
-5.65228751722709)) ;
#104980 = CARTESIAN_POINT('Ctrl Pts',(0.617496289133925,0.205225320901714,
-5.6650493700286)) ;
#104981 = CARTESIAN_POINT('Ctrl Pts',(0.62337157240616,0.203426297263481,
-5.67677936428201)) ;
#104982 = CARTESIAN_POINT('Ctrl Pts',(0.634595774761163,0.201039923568647,
-5.69920025888391)) ;
#104983 = CARTESIAN_POINT('Ctrl Pts',(0.639950075944988,0.200369897448124,
-5.70990192168153)) ;
#104984 = CARTESIAN_POINT('Ctrl Pts',(0.646785573817023,0.200038350130376,
-5.72357116034297)) ;
#104985 = CARTESIAN_POINT('Ctrl Pts',(0.648401413159571,0.2,-5.72680282631915)) ;
#104986 = CARTESIAN_POINT('Ctrl Pts',(0.65,0.2,-5.73)) ;
#104987 = CARTESIAN_POINT('',(0.579289321881328,0.229289321881363,-4.57142135623727)) ;
#104988 = CARTESIAN_POINT('Ctrl Pts',(0.65,0.2,-4.43)) ;
#104989 = CARTESIAN_POINT('Ctrl Pts',(0.644917141732079,0.2,-4.44016571653583)) ;
#104990 = CARTESIAN_POINT('Ctrl Pts',(0.639657683858008,0.200389688120423,
-4.45068315091942)) ;
#104991 = CARTESIAN_POINT('Ctrl Pts',(0.628467949719361,0.202165884217643,
-4.47304266528023)) ;
#104992 = CARTESIAN_POINT('Ctrl Pts',(0.622522761794958,0.203647820493435,
-4.48491327259876)) ;
#104993 = CARTESIAN_POINT('Ctrl Pts',(0.611106760396026,0.207685608831252,
-4.50771616261944)) ;
#104994 = CARTESIAN_POINT('Ctrl Pts',(0.60562986130804,0.21017819324833,-4.51866251834951)) ;
#104995 = CARTESIAN_POINT('Ctrl Pts',(0.59974069603932,0.213544620665559,
-4.53045005711458)) ;
#104996 = CARTESIAN_POINT('Ctrl Pts',(0.599111682766055,0.213913346521986,
-4.53170928105426)) ;
#104997 = CARTESIAN_POINT('Ctrl Pts',(0.593032751351781,0.217566912232528,
-4.54388077026722)) ;
#104998 = CARTESIAN_POINT('Ctrl Pts',(0.587842238429123,0.221400308602595,
-4.55429308263749)) ;
#104999 = CARTESIAN_POINT('Ctrl Pts',(0.581771186964295,0.226871185484688,
-4.56645488997275)) ;
#105000 = CARTESIAN_POINT('Ctrl Pts',(0.580514667064132,0.228063976698558,
-4.56897066587167)) ;
#105001 = CARTESIAN_POINT('Ctrl Pts',(0.579289321881328,0.229289321881363,
-4.57142135623728)) ;
#105002 = CARTESIAN_POINT('Origin',(0.657142104246849,0.302990743360512,-4.41571994570428)) ;
#105003 = CARTESIAN_POINT('Origin',(-1.7,4.6,-5.63)) ;
#105004 = CARTESIAN_POINT('',(-1.77071067811866,4.52928932188135,-5.58857864376269)) ;
#105005 = CARTESIAN_POINT('Ctrl Pts',(-1.8,4.6,-5.73)) ;
#105006 = CARTESIAN_POINT('Ctrl Pts',(-1.8,4.59491714173209,-5.71983428346416)) ;
#105007 = CARTESIAN_POINT('Ctrl Pts',(-1.79961031187958,4.58965768385802,
-5.70931684908055)) ;
#105008 = CARTESIAN_POINT('Ctrl Pts',(-1.79783411578236,4.57846794971937,
-5.68695733471969)) ;
#105009 = CARTESIAN_POINT('Ctrl Pts',(-1.79635217950657,4.57252276179496,
-5.67508672740113)) ;
#105010 = CARTESIAN_POINT('Ctrl Pts',(-1.79231439116882,4.56110676039622,
-5.65228383738084)) ;
#105011 = CARTESIAN_POINT('Ctrl Pts',(-1.78982180675185,4.55562986130843,
-5.64133748165119)) ;
#105012 = CARTESIAN_POINT('Ctrl Pts',(-1.78645537933466,4.54974069603969,
-5.62954994288609)) ;
#105013 = CARTESIAN_POINT('Ctrl Pts',(-1.78608665347812,4.54911168276623,
-5.628290718946)) ;
#105014 = CARTESIAN_POINT('Ctrl Pts',(-1.78243308776746,4.54303275135176,
-5.61611922973268)) ;
#105015 = CARTESIAN_POINT('Ctrl Pts',(-1.7785996913974,4.53784223842911,-5.60570691736243)) ;
#105016 = CARTESIAN_POINT('Ctrl Pts',(-1.77312881451532,4.5317711869643,-5.5935451100272)) ;
#105017 = CARTESIAN_POINT('Ctrl Pts',(-1.77193602330145,4.53051466706415,
-5.59102933412829)) ;
#105018 = CARTESIAN_POINT('Ctrl Pts',(-1.77071067811866,4.52928932188135,
-5.58857864376269)) ;
#105019 = CARTESIAN_POINT('Origin',(-1.6970092566394,4.60714210424635,-5.74428005429455)) ;
#105020 = CARTESIAN_POINT('',(-1.77071067811866,4.52928932188135,-4.57142135623731)) ;
#105021 = CARTESIAN_POINT('Origin',(-1.69703459697486,4.6070866853807,-4.41582990494723)) ;
#105022 = CARTESIAN_POINT('Ctrl Pts',(-1.77071067811866,4.52928932188135,
-4.57142135623731)) ;
#105023 = CARTESIAN_POINT('Ctrl Pts',(-1.77521675558368,4.53379539934637,
-4.56240920130726)) ;
#105024 = CARTESIAN_POINT('Ctrl Pts',(-1.77928079264423,4.53872648167164,
-4.55251374182714)) ;
#105025 = CARTESIAN_POINT('Ctrl Pts',(-1.78624680748632,4.54902088254787,
-4.53188722943115)) ;
#105026 = CARTESIAN_POINT('Ctrl Pts',(-1.78918030781801,4.55436398414927,
-4.52119490566499)) ;
#105027 = CARTESIAN_POINT('Ctrl Pts',(-1.79185985500299,4.560474754533,-4.50898140677941)) ;
#105028 = CARTESIAN_POINT('Ctrl Pts',(-1.79213045061231,4.56110970990904,
-4.50771248277287)) ;
#105029 = CARTESIAN_POINT('Ctrl Pts',(-1.7947746790983,4.56749628913397,-4.49495062997143)) ;
#105030 = CARTESIAN_POINT('Ctrl Pts',(-1.79657370273653,4.57337157240621,
-4.483220635718)) ;
#105031 = CARTESIAN_POINT('Ctrl Pts',(-1.79896007643136,4.58459577476122,
-4.46079974111606)) ;
#105032 = CARTESIAN_POINT('Ctrl Pts',(-1.79963010255188,4.58995007594504,
-4.45009807831843)) ;
#105033 = CARTESIAN_POINT('Ctrl Pts',(-1.79996164986962,4.59678557381705,
-4.436428839657)) ;
#105034 = CARTESIAN_POINT('Ctrl Pts',(-1.8,4.59840141315958,-4.43319717368084)) ;
#105035 = CARTESIAN_POINT('Ctrl Pts',(-1.8,4.6,-4.43)) ;
#105036 = CARTESIAN_POINT('Origin',(-1.7,0.3,-6.48)) ;
#105037 = CARTESIAN_POINT('Origin',(-1.7,0.1,-6.48)) ;
#105038 = CARTESIAN_POINT('Origin',(-1.9,0.3,-6.48)) ;
#105039 = CARTESIAN_POINT('Origin',(1.9668402209837E-32,0.1,-6.48)) ;
#105040 = CARTESIAN_POINT('',(0.899999999999999,0.1,-6.58)) ;
#105041 = CARTESIAN_POINT('',(-1.8,0.1,-6.58)) ;
#105042 = CARTESIAN_POINT('Origin',(0.899999999999999,0.1,-6.48)) ;
#105043 = CARTESIAN_POINT('Origin',(0.899999999999999,0.1,-6.48)) ;
#105044 = CARTESIAN_POINT('',(0.999999999999999,0.1,-6.48)) ;
#105045 = CARTESIAN_POINT('Origin',(0.899999999999999,0.1,-6.48)) ;
#105046 = CARTESIAN_POINT('Origin',(0.899999999999999,0.1,-6.48)) ;
#105047 = CARTESIAN_POINT('Origin',(0.549999999999999,0.3,-4.43)) ;
#105048 = CARTESIAN_POINT('',(0.508578643762691,0.229289321881345,-4.50071067811866)) ;
#105049 = CARTESIAN_POINT('Origin',(0.664170095058604,0.302965403026464,-4.42291331461641)) ;
#105050 = CARTESIAN_POINT('Ctrl Pts',(0.50857864376269,0.229289321881348,
-4.50071067811866)) ;
#105051 = CARTESIAN_POINT('Ctrl Pts',(0.517590798692739,0.224783244416321,
-4.49620460065363)) ;
#105052 = CARTESIAN_POINT('Ctrl Pts',(0.527486258172858,0.220719207355774,
-4.49127351832835)) ;
#105053 = CARTESIAN_POINT('Ctrl Pts',(0.548112770568679,0.213753192513746,
-4.48097911745222)) ;
#105054 = CARTESIAN_POINT('Ctrl Pts',(0.558805094334662,0.210819692182089,
-4.47563601585092)) ;
#105055 = CARTESIAN_POINT('Ctrl Pts',(0.571018593220227,0.20814014499709,
-4.46952524546719)) ;
#105056 = CARTESIAN_POINT('Ctrl Pts',(0.572287517226953,0.207869549387729,
-4.46889029009106)) ;
#105057 = CARTESIAN_POINT('Ctrl Pts',(0.585049370028579,0.205225320901701,
-4.46250371086604)) ;
#105058 = CARTESIAN_POINT('Ctrl Pts',(0.59677936428202,0.203426297263468,
-4.45662842759379)) ;
#105059 = CARTESIAN_POINT('Ctrl Pts',(0.619200258883963,0.201039923568638,
-4.44540422523878)) ;
#105060 = CARTESIAN_POINT('Ctrl Pts',(0.62990192168159,0.20036989744812,-4.44004992405496)) ;
#105061 = CARTESIAN_POINT('Ctrl Pts',(0.64357116034301,0.200038350130375,
-4.43321442618295)) ;
#105062 = CARTESIAN_POINT('Ctrl Pts',(0.646802826319169,0.2,-4.43159858684041)) ;
#105063 = CARTESIAN_POINT('Ctrl Pts',(0.65,0.2,-4.43)) ;
#105064 = CARTESIAN_POINT('Origin',(-1.7,0.3,-4.43)) ;
#105065 = CARTESIAN_POINT('Origin',(-1.7,4.5,-4.43)) ;
#105066 = CARTESIAN_POINT('',(-1.77071067811863,4.45857864376274,-4.50071067811868)) ;
#105067 = CARTESIAN_POINT('Ctrl Pts',(-1.8,4.6,-4.43)) ;
#105068 = CARTESIAN_POINT('Ctrl Pts',(-1.8,4.58983428346418,-4.43508285826792)) ;
#105069 = CARTESIAN_POINT('Ctrl Pts',(-1.79961031187958,4.5793168490806,-4.44034231614199)) ;
#105070 = CARTESIAN_POINT('Ctrl Pts',(-1.79783411578236,4.55695733471983,
-4.45153205028063)) ;
#105071 = CARTESIAN_POINT('Ctrl Pts',(-1.79635217950657,4.54508672740132,
-4.45747723820502)) ;
#105072 = CARTESIAN_POINT('Ctrl Pts',(-1.79231439116875,4.52228383738059,
-4.46889323960399)) ;
#105073 = CARTESIAN_POINT('Ctrl Pts',(-1.78982180675165,4.51133748165043,
-4.47437013869202)) ;
#105074 = CARTESIAN_POINT('Ctrl Pts',(-1.78645537933441,4.49954994288537,
-4.48025930396073)) ;
#105075 = CARTESIAN_POINT('Ctrl Pts',(-1.78608665347801,4.49829071894577,
-4.48088831723395)) ;
#105076 = CARTESIAN_POINT('Ctrl Pts',(-1.78243308776749,4.48611922973289,
-4.48696724864819)) ;
#105077 = CARTESIAN_POINT('Ctrl Pts',(-1.77859969139742,4.4757069173626,-4.49215776157085)) ;
#105078 = CARTESIAN_POINT('Ctrl Pts',(-1.77312881451532,4.46354511002731,
-4.49822881303569)) ;
#105079 = CARTESIAN_POINT('Ctrl Pts',(-1.77193602330144,4.46102933412837,
-4.49948533293587)) ;
#105080 = CARTESIAN_POINT('Ctrl Pts',(-1.77071067811863,4.45857864376274,
-4.50071067811868)) ;
#105081 = CARTESIAN_POINT('Origin',(-1.6970092566383,4.61428005430142,-4.42285789575035)) ;
#105082 = CARTESIAN_POINT('Origin',(-1.7,0.3,-4.43)) ;
#105083 = CARTESIAN_POINT('Origin',(-1.9,-4.11004745125224E-16,-6.48)) ;
#105084 = CARTESIAN_POINT('',(-1.9,6.9,-6.58)) ;
#105085 = CARTESIAN_POINT('Origin',(-1.9,6.9,-6.48)) ;
#105086 = CARTESIAN_POINT('',(-1.9,7.,-6.58)) ;
#105087 = CARTESIAN_POINT('Origin',(-2.,0.1,-6.68)) ;
#105088 = CARTESIAN_POINT('Origin',(-1.89999999999995,0.100000000000053,-6.68000000000005)) ;
#105089 = CARTESIAN_POINT('Origin',(0.899999999999999,0.1,-6.68)) ;
#105090 = CARTESIAN_POINT('Origin',(0.899999999999999,0.1,-6.48)) ;
#105091 = CARTESIAN_POINT('Origin',(1.1,0.1,-6.48)) ;
#105092 = CARTESIAN_POINT('Origin',(0.899999999999999,0.1,-5.08)) ;
#105093 = CARTESIAN_POINT('',(0.999999999999999,0.1,-3.68)) ;
#105094 = CARTESIAN_POINT('',(0.999999999999999,0.1,-6.58)) ;
#105095 = CARTESIAN_POINT('Origin',(0.899999999999999,0.1,-3.68)) ;
#105096 = CARTESIAN_POINT('Origin',(-1.7,0.3,-4.43)) ;
#105097 = CARTESIAN_POINT('Origin',(-1.7,0.3,-4.43)) ;
#105098 = CARTESIAN_POINT('Origin',(-1.9,6.9,-6.48)) ;
#105099 = CARTESIAN_POINT('',(-1.9,7.,-6.48)) ;
#105100 = CARTESIAN_POINT('Origin',(-1.9,6.9,-6.48)) ;
#105101 = CARTESIAN_POINT('Origin',(-1.9,6.9,-6.48)) ;
#105102 = CARTESIAN_POINT('Origin',(-1.9,7.,-6.68)) ;
#105103 = CARTESIAN_POINT('Origin',(-1.9,6.9,-6.68)) ;
#105104 = CARTESIAN_POINT('Origin',(1.1,0.1,-3.58)) ;
#105105 = CARTESIAN_POINT('Origin',(1.1,0.1,-3.68)) ;
#105106 = CARTESIAN_POINT('Origin',(0.899999999999999,0.1,-3.68)) ;
#105107 = CARTESIAN_POINT('',(0.899999999999999,0.1,-3.58)) ;
#105108 = CARTESIAN_POINT('Origin',(0.899999999999999,0.1,-3.68)) ;
#105109 = CARTESIAN_POINT('Origin',(0.899999999999999,0.1,-3.68)) ;
#105110 = CARTESIAN_POINT('Origin',(-1.7,0.3,-5.08)) ;
#105111 = CARTESIAN_POINT('Origin',(-1.7,0.3,-3.68)) ;
#105112 = CARTESIAN_POINT('Origin',(-1.9,6.9,-5.08)) ;
#105113 = CARTESIAN_POINT('',(-1.9,7.,-3.68)) ;
#105114 = CARTESIAN_POINT('Origin',(-1.9,6.9,-3.68)) ;
#105115 = CARTESIAN_POINT('',(-1.9,7.,-6.58)) ;
#105116 = CARTESIAN_POINT('Origin',(-1.9,6.9,-6.48)) ;
#105117 = CARTESIAN_POINT('Origin',(-1.9,7.1,-6.48)) ;
#105118 = CARTESIAN_POINT('Origin',(0.899999999999999,0.1,-3.68)) ;
#105119 = CARTESIAN_POINT('Origin',(0.899999999999999,0.1,-3.48)) ;
#105120 = CARTESIAN_POINT('Origin',(-1.9668402209837E-32,0.1,-3.68)) ;
#105121 = CARTESIAN_POINT('',(0.999999999999999,0.1,-3.58)) ;
#105122 = CARTESIAN_POINT('Origin',(-1.7,0.1,-3.68)) ;
#105123 = CARTESIAN_POINT('Origin',(-1.7,0.3,-3.68)) ;
#105124 = CARTESIAN_POINT('Origin',(-1.9,0.3,-3.68)) ;
#105125 = CARTESIAN_POINT('Origin',(-1.9,6.9,-3.68)) ;
#105126 = CARTESIAN_POINT('',(-1.9,6.9,-3.58)) ;
#105127 = CARTESIAN_POINT('Origin',(-1.9,6.9,-3.68)) ;
#105128 = CARTESIAN_POINT('Origin',(-1.9,6.9,-3.68)) ;
#105129 = CARTESIAN_POINT('Origin',(-1.9,7.1,-6.58)) ;
#105130 = CARTESIAN_POINT('Origin',(-1.9,7.1,-3.68)) ;
#105131 = CARTESIAN_POINT('Origin',(-1.8,0.1,-3.48)) ;
#105132 = CARTESIAN_POINT('Origin',(-1.89999999999997,0.100000000000027,-3.47999999999998)) ;
#105133 = CARTESIAN_POINT('Origin',(-1.9,-6.40600499298624E-17,-3.68)) ;
#105134 = CARTESIAN_POINT('',(-1.9,7.,-3.58)) ;
#105135 = CARTESIAN_POINT('Origin',(-1.9,6.9,-3.68)) ;
#105136 = CARTESIAN_POINT('Origin',(-1.9,6.9,-3.48)) ;
#105137 = CARTESIAN_POINT('Origin',(-1.9,7.,-3.48)) ;
#105138 = CARTESIAN_POINT('Origin',(-0.900000000000002,2.95,-5.08)) ;
#105139 = CARTESIAN_POINT('Origin',(-0.900000000000001,2.95,-6.7231676725155)) ;
#105140 = CARTESIAN_POINT('Origin',(-0.900000000000002,2.95,-6.7231676725155)) ;
#105141 = CARTESIAN_POINT('Origin',(-0.900000000000001,2.95,-6.7231676725155)) ;
#105142 = CARTESIAN_POINT('Origin',(-0.900000000000002,2.95,-6.7231676725155)) ;
#105143 = CARTESIAN_POINT('Origin',(1.15,3.15,-7.63)) ;
#105144 = CARTESIAN_POINT('Origin',(1.15,3.15,-6.7231676725155)) ;
#105145 = CARTESIAN_POINT('Origin',(-1.,2.95,-6.7231676725155)) ;
#105146 = CARTESIAN_POINT('Origin',(1.15,2.95,-6.7231676725155)) ;
#105147 = CARTESIAN_POINT('Origin',(-0.900000000000001,3.8,-5.08)) ;
#105148 = CARTESIAN_POINT('Origin',(-0.900000000000002,2.1568323274845,-5.93)) ;
#105149 = CARTESIAN_POINT('Origin',(-0.900000000000002,1.6,-5.08)) ;
#105150 = CARTESIAN_POINT('Origin',(-0.900000000000002,1.6,-7.04214168703487)) ;
#105151 = CARTESIAN_POINT('Origin',(13.9153543900904,1.4,-7.04214168703487)) ;
#105152 = CARTESIAN_POINT('Origin',(8.49172374697002,1.4,-7.04214168703487)) ;
#105153 = CARTESIAN_POINT('Origin',(-0.900000000000001,1.40000000000001,-7.04214168703487)) ;
#105154 = CARTESIAN_POINT('Origin',(1.15,2.95,-6.7231676725155)) ;
#105155 = CARTESIAN_POINT('Origin',(1.15,3.04189189189189,-6.54552792413544)) ;
#105156 = CARTESIAN_POINT('Origin',(-0.900000000000002,2.1568323274845,-5.93)) ;
#105157 = CARTESIAN_POINT('Origin',(-0.900000000000002,2.1568323274845,-5.93)) ;
#105158 = CARTESIAN_POINT('Origin',(-0.900000000000002,2.1568323274845,-5.93)) ;
#105159 = CARTESIAN_POINT('Origin',(-0.900000000000001,1.40000000000001,-7.04214168703487)) ;
#105160 = CARTESIAN_POINT('Origin',(-0.900000000000002,1.55483870967742,-6.91555190077455)) ;
#105161 = CARTESIAN_POINT('Origin',(1.15,3.8,-5.08)) ;
#105162 = CARTESIAN_POINT('Origin',(1.15,2.33447207586456,-5.83810810810811)) ;
#105163 = CARTESIAN_POINT('Origin',(-1.,2.1568323274845,-5.93)) ;
#105164 = CARTESIAN_POINT('Origin',(1.15,2.1568323274845,-5.93)) ;
#105165 = CARTESIAN_POINT('Origin',(-0.900000000000001,3.8,-5.93)) ;
#105166 = CARTESIAN_POINT('Origin',(-0.900000000000002,1.02736587339765,-5.93)) ;
#105167 = CARTESIAN_POINT('Origin',(-0.900000000000001,3.8,-5.08)) ;
#105168 = CARTESIAN_POINT('Origin',(-0.900000000000002,1.02736587339765,-5.93)) ;
#105169 = CARTESIAN_POINT('Origin',(13.9153543900904,1.4,-3.11785831296514)) ;
#105170 = CARTESIAN_POINT('Origin',(8.49172374697002,1.4,-3.11785831296514)) ;
#105171 = CARTESIAN_POINT('Origin',(-0.900000000000001,1.40000000000001,-3.11785831296514)) ;
#105172 = CARTESIAN_POINT('Origin',(-0.900000000000002,1.6,-5.08)) ;
#105173 = CARTESIAN_POINT('Origin',(-0.900000000000002,1.6,-3.11785831296514)) ;
#105174 = CARTESIAN_POINT('Origin',(-0.900000000000002,2.95,-5.08)) ;
#105175 = CARTESIAN_POINT('Origin',(-0.900000000000002,2.95,-3.4368323274845)) ;
#105176 = CARTESIAN_POINT('Origin',(1.15,2.1568323274845,-5.93)) ;
#105177 = CARTESIAN_POINT('Origin',(1.15,2.1568323274845,-5.73)) ;
#105178 = CARTESIAN_POINT('Origin',(-0.900000000000002,1.02736587339765,-5.93)) ;
#105179 = CARTESIAN_POINT('Origin',(-0.900000000000001,1.40000000000001,-3.11785831296514)) ;
#105180 = CARTESIAN_POINT('Origin',(-0.900000000000002,1.55483870967743,-3.24444809922545)) ;
#105181 = CARTESIAN_POINT('Origin',(-0.900000000000002,2.95,-3.4368323274845)) ;
#105182 = CARTESIAN_POINT('Origin',(-0.900000000000002,2.95,-3.4368323274845)) ;
#105183 = CARTESIAN_POINT('Origin',(-0.900000000000001,2.95,-3.4368323274845)) ;
#105184 = CARTESIAN_POINT('Origin',(1.15,2.21886116991581,-5.73)) ;
#105185 = CARTESIAN_POINT('Ctrl Pts',(1.15,1.02736587339765,-5.83)) ;
#105186 = CARTESIAN_POINT('Ctrl Pts',(1.1608920328805,1.02736587339765,-5.83)) ;
#105187 = CARTESIAN_POINT('Ctrl Pts',(1.17195716626105,1.02622125393927,-5.82814384392599)) ;
#105188 = CARTESIAN_POINT('Ctrl Pts',(1.1820844490224,1.02414637334385,-5.82471318879084)) ;
#105189 = CARTESIAN_POINT('Ctrl Pts',(1.19245005921088,1.02202266415684,-5.82120179934314)) ;
#105190 = CARTESIAN_POINT('Ctrl Pts',(1.20216743701154,1.01888103823701,-5.81596019807028)) ;
#105191 = CARTESIAN_POINT('Ctrl Pts',(1.21053792402812,1.01518120925307,-5.80959371680205)) ;
#105192 = CARTESIAN_POINT('Ctrl Pts',(1.219343173684,1.01128921135341,-5.80289656084385)) ;
#105193 = CARTESIAN_POINT('Ctrl Pts',(1.22692289939014,1.00668521903338,-5.79478516153154)) ;
#105194 = CARTESIAN_POINT('Ctrl Pts',(1.23290049538659,1.00186003905466,-5.78592412596239)) ;
#105195 = CARTESIAN_POINT('Ctrl Pts',(1.23922345568944,0.9967560772818,-5.77655113116998)) ;
#105196 = CARTESIAN_POINT('Ctrl Pts',(1.24392209779927,0.991279542094837,
-5.76610455998969)) ;
#105197 = CARTESIAN_POINT('Ctrl Pts',(1.24674870216524,0.985895902333124,
-5.75529206652967)) ;
#105198 = CARTESIAN_POINT('Ctrl Pts',(1.24889292215336,0.981811953364218,
-5.74708986997272)) ;
#105199 = CARTESIAN_POINT('Ctrl Pts',(1.25,0.977715885027402,-5.73854916862923)) ;
#105200 = CARTESIAN_POINT('Ctrl Pts',(1.25,0.973783447787483,-5.73)) ;
#105201 = CARTESIAN_POINT('Origin',(-0.900000000000001,3.8,-5.08)) ;
#105202 = CARTESIAN_POINT('Origin',(-0.900000000000002,1.02736587339765,-4.23)) ;
#105203 = CARTESIAN_POINT('Origin',(-0.900000000000001,3.8,-4.23)) ;
#105204 = CARTESIAN_POINT('Origin',(-0.900000000000002,2.1568323274845,-4.23)) ;
#105205 = CARTESIAN_POINT('Origin',(-0.900000000000002,1.02736587339765,-4.23)) ;
#105206 = CARTESIAN_POINT('Origin',(-0.900000000000001,3.8,-5.08)) ;
#105207 = CARTESIAN_POINT('Origin',(-0.900000000000002,2.1568323274845,-4.23)) ;
#105208 = CARTESIAN_POINT('Origin',(-1.,2.95,-3.4368323274845)) ;
#105209 = CARTESIAN_POINT('Origin',(1.15,2.95,-3.4368323274845)) ;
#105210 = CARTESIAN_POINT('Origin',(1.15,3.15,-2.53)) ;
#105211 = CARTESIAN_POINT('Origin',(1.15,3.15,-3.4368323274845)) ;
#105212 = CARTESIAN_POINT('Ctrl Pts',(1.110285585749,0.930383836951459,-5.95499428365807)) ;
#105213 = CARTESIAN_POINT('Ctrl Pts',(1.14039000477524,0.892136466137966,
-5.82996971859421)) ;
#105214 = CARTESIAN_POINT('Ctrl Pts',(1.13015013463564,1.02610337426259,-5.82785112488281)) ;
#105215 = CARTESIAN_POINT('Ctrl Pts',(1.17639690652714,0.935225109827694,
-5.97012573994677)) ;
#105216 = CARTESIAN_POINT('Ctrl Pts',(1.15491086542928,0.891146666106776,
-5.82927605040126)) ;
#105217 = CARTESIAN_POINT('Ctrl Pts',(1.16319405445818,1.03078047702086,-5.83516487424516)) ;
#105218 = CARTESIAN_POINT('Ctrl Pts',(1.24701363206612,0.927145283841818,
-5.94555220382508)) ;
#105219 = CARTESIAN_POINT('Ctrl Pts',(1.17759980831448,0.893467326853881,
-5.83263731203129)) ;
#105220 = CARTESIAN_POINT('Ctrl Pts',(1.19848758201044,1.02297467453099,-5.82328712255501)) ;
#105221 = CARTESIAN_POINT('Ctrl Pts',(1.33816236560061,0.900022463714231,
-5.8498088506149)) ;
#105222 = CARTESIAN_POINT('Ctrl Pts',(1.22862786282608,0.888037626604003,
-5.80315396432406)) ;
#105223 = CARTESIAN_POINT('Ctrl Pts',(1.24403288504499,0.996768276947733,
-5.77702665941333)) ;
#105224 = CARTESIAN_POINT('Ctrl Pts',(1.35959492575603,0.881455895025369,
-5.77853234122901)) ;
#105225 = CARTESIAN_POINT('Ctrl Pts',(1.25320519750694,0.880428099081613,
-5.77106493782729)) ;
#105226 = CARTESIAN_POINT('Ctrl Pts',(1.25473603279823,0.978811277328813,
-5.74255748715087)) ;
#105227 = CARTESIAN_POINT('Ctrl Pts',(1.34615355831622,0.867571605181207,
-5.71279258253342)) ;
#105228 = CARTESIAN_POINT('Ctrl Pts',(1.25176090202793,0.87095013062468,-5.72944901705783)) ;
#105229 = CARTESIAN_POINT('Ctrl Pts',(1.24801589497572,0.965423101361823,
-5.710869548164)) ;
#105230 = CARTESIAN_POINT('Origin',(1.35,0.973783447787483,-5.73)) ;
#105231 = CARTESIAN_POINT('Origin',(-0.900000000000002,1.02736587339765,-4.23)) ;
#105232 = CARTESIAN_POINT('',(-0.957735026918965,0.969630846478687,-4.28773502691896)) ;
#105233 = CARTESIAN_POINT('Origin',(-0.900000000000002,1.02736587339765,-4.23)) ;
#105234 = CARTESIAN_POINT('Origin',(-0.900000000000002,2.1568323274845,-4.23)) ;
#105235 = CARTESIAN_POINT('Origin',(-0.900000000000002,2.1568323274845,-4.23)) ;
#105236 = CARTESIAN_POINT('Origin',(1.15,2.95,-3.4368323274845)) ;
#105237 = CARTESIAN_POINT('Origin',(1.15,3.04189189189189,-3.61447207586456)) ;
#105238 = CARTESIAN_POINT('Origin',(1.35,3.8,-5.08)) ;
#105239 = CARTESIAN_POINT('Origin',(1.35,0.973783447787484,-4.43)) ;
#105240 = CARTESIAN_POINT('Origin',(-1.,2.1568323274845,-4.23)) ;
#105241 = CARTESIAN_POINT('Origin',(1.15,2.1568323274845,-4.23)) ;
#105242 = CARTESIAN_POINT('Origin',(1.15,3.8,-5.08)) ;
#105243 = CARTESIAN_POINT('Origin',(1.15,2.33447207586456,-4.32189189189189)) ;
#105244 = CARTESIAN_POINT('Ctrl Pts',(1.34754079198594,0.869159571293155,
-4.43974853478553)) ;
#105245 = CARTESIAN_POINT('Ctrl Pts',(1.25183398383321,0.87199977042434,-4.4259986517603)) ;
#105246 = CARTESIAN_POINT('Ctrl Pts',(1.24871534599026,0.966951450593901,
-4.44553571307355)) ;
#105247 = CARTESIAN_POINT('Ctrl Pts',(1.35788971301869,0.882932151572348,
-4.37577742826808)) ;
#105248 = CARTESIAN_POINT('Ctrl Pts',(1.2513879651909,0.881019151005419,-4.38648728142376)) ;
#105249 = CARTESIAN_POINT('Ctrl Pts',(1.25389076424432,0.980237216252362,
-4.41468863425942)) ;
#105250 = CARTESIAN_POINT('Ctrl Pts',(1.33642796493172,0.900551643074782,
-4.30831671896883)) ;
#105251 = CARTESIAN_POINT('Ctrl Pts',(1.22773025960899,0.888154519889423,
-4.35630235415234)) ;
#105252 = CARTESIAN_POINT('Ctrl Pts',(1.24317203399028,0.997278352451075,
-4.38206445828307)) ;
#105253 = CARTESIAN_POINT('Ctrl Pts',(1.24851212064759,0.92667567099975,-4.21611185418655)) ;
#105254 = CARTESIAN_POINT('Ctrl Pts',(1.17855408504645,0.893378082604316,
-4.32793584540021)) ;
#105255 = CARTESIAN_POINT('Ctrl Pts',(1.19923947710882,1.02252144543594,-4.33751118406066)) ;
#105256 = CARTESIAN_POINT('Ctrl Pts',(1.18212686068546,0.934567888698244,
-4.19189225990079)) ;
#105257 = CARTESIAN_POINT('Ctrl Pts',(1.15690947476179,0.891342319659344,
-4.33050130223878)) ;
#105258 = CARTESIAN_POINT('Ctrl Pts',(1.1660589236879,1.03014681530414,-4.32580412352038)) ;
#105259 = CARTESIAN_POINT('Ctrl Pts',(1.11776263740946,0.930888708579174,
-4.20342358191601)) ;
#105260 = CARTESIAN_POINT('Ctrl Pts',(1.14197710563588,0.892059806626676,
-4.33008229965564)) ;
#105261 = CARTESIAN_POINT('Ctrl Pts',(1.13388624958144,1.02659206201256,-4.33137785610126)) ;
#105262 = CARTESIAN_POINT('Ctrl Pts',(1.15,1.02736587339764,-4.33)) ;
#105263 = CARTESIAN_POINT('Ctrl Pts',(1.15623005440502,1.02736587339759,-4.32999999999987)) ;
#105264 = CARTESIAN_POINT('Ctrl Pts',(1.16249579431471,1.02700282517053,-4.33059086606898)) ;
#105265 = CARTESIAN_POINT('Ctrl Pts',(1.16857840195431,1.02630083270769,-4.33174093944667)) ;
#105266 = CARTESIAN_POINT('Ctrl Pts',(1.1798885498395,1.02499553092934,-4.33387941372467)) ;
#105267 = CARTESIAN_POINT('Ctrl Pts',(1.19084787809767,1.02245621903271,-4.33805069661522)) ;
#105268 = CARTESIAN_POINT('Ctrl Pts',(1.20043335385463,1.01914369852331,-4.3436491064379)) ;
#105269 = CARTESIAN_POINT('Ctrl Pts',(1.21063893018497,1.01561688548223,-4.34960968682249)) ;
#105270 = CARTESIAN_POINT('Ctrl Pts',(1.21965078109605,1.01112191387731,-4.35735485110186)) ;
#105271 = CARTESIAN_POINT('Ctrl Pts',(1.226898722009,1.00626683908294,-4.36607358485428)) ;
#105272 = CARTESIAN_POINT('Ctrl Pts',(1.23435386869391,1.0012729663137,-4.37504157173658)) ;
#105273 = CARTESIAN_POINT('Ctrl Pts',(1.24017476602864,0.995763540409855,
-4.38528702640693)) ;
#105274 = CARTESIAN_POINT('Ctrl Pts',(1.24405759382605,0.990267693778535,
-4.39604165723046)) ;
#105275 = CARTESIAN_POINT('Ctrl Pts',(1.24795610732226,0.9847496452368,-4.40683973419908)) ;
#105276 = CARTESIAN_POINT('Ctrl Pts',(1.25,0.97910634898267,-4.41842794502798)) ;
#105277 = CARTESIAN_POINT('Ctrl Pts',(1.25,0.973783447787483,-4.43)) ;
#105278 = CARTESIAN_POINT('Origin',(1.15,2.1568323274845,-4.23)) ;
#105279 = CARTESIAN_POINT('Origin',(1.15,2.1568323274845,-4.43)) ;
#105280 = CARTESIAN_POINT('Origin',(1.15,2.21886116991581,-4.43)) ;
#105281 = CARTESIAN_POINT('Origin',(1.5,2.3,-5.48)) ;
#105282 = CARTESIAN_POINT('Ctrl Pts',(0.55,4.04473197180486,-5.53)) ;
#105283 = CARTESIAN_POINT('Ctrl Pts',(0.55,4.04340510574361,-5.53201839167459)) ;
#105284 = CARTESIAN_POINT('Ctrl Pts',(0.549938912488052,4.04197482121868,
-5.53397990935583)) ;
#105285 = CARTESIAN_POINT('Ctrl Pts',(0.549362579613729,4.03414945156065,
-5.5437632016969)) ;
#105286 = CARTESIAN_POINT('Ctrl Pts',(0.54804065212511,4.02633974827561,-5.5505458262271)) ;
#105287 = CARTESIAN_POINT('Ctrl Pts',(0.544205267183641,4.00519499286857,
-5.56468394278881)) ;
#105288 = CARTESIAN_POINT('Ctrl Pts',(0.54122133237852,3.9901199563799,-5.57122511544813)) ;
#105289 = CARTESIAN_POINT('Ctrl Pts',(0.537814556431591,3.96385893187682,
-5.57793059223995)) ;
#105290 = CARTESIAN_POINT('Ctrl Pts',(0.536602540378443,3.95132390702871,
-5.58)) ;
#105291 = CARTESIAN_POINT('Ctrl Pts',(0.536602540378443,3.93764017256378,
-5.58)) ;
#105292 = CARTESIAN_POINT('Origin',(-0.4,2.3,-5.48)) ;
#105293 = CARTESIAN_POINT('Origin',(-0.4,-3.4,-5.48)) ;
#105294 = CARTESIAN_POINT('Origin',(-0.4,-3.36847777691809,-5.48)) ;
#105295 = CARTESIAN_POINT('Origin',(1.5,2.3,-5.48)) ;
#105296 = CARTESIAN_POINT('Ctrl Pts',(0.536602540378443,2.83090991212703,
-5.58)) ;
#105297 = CARTESIAN_POINT('Ctrl Pts',(0.536602540378443,2.80627146475523,
-5.58)) ;
#105298 = CARTESIAN_POINT('Ctrl Pts',(0.538106903229135,2.77742679387697,
-5.57795279081267)) ;
#105299 = CARTESIAN_POINT('Ctrl Pts',(0.545186976568789,2.7115684436341,-5.56208398098024)) ;
#105300 = CARTESIAN_POINT('Ctrl Pts',(0.55,2.6828290608274,-5.54810205581407)) ;
#105301 = CARTESIAN_POINT('Ctrl Pts',(0.55,2.65280931275608,-5.53)) ;
#105302 = CARTESIAN_POINT('Origin',(0.400000000000001,2.29999999999999,-5.48)) ;
#105303 = CARTESIAN_POINT('Origin',(0.0725078566451197,-4.04348900069683,
-5.00749214335488)) ;
#105304 = CARTESIAN_POINT('Origin',(-0.4,-3.36847777691809,-5.48)) ;
#105305 = CARTESIAN_POINT('Origin',(-0.0979344438426628,-3.8,-5.17793444384266)) ;
#105306 = CARTESIAN_POINT('Origin',(1.5,2.3,-4.68)) ;
#105307 = CARTESIAN_POINT('Ctrl Pts',(0.536602540378443,3.93764017256378,
-4.58)) ;
#105308 = CARTESIAN_POINT('Ctrl Pts',(0.536602540378443,3.93925361219655,
-4.58)) ;
#105309 = CARTESIAN_POINT('Ctrl Pts',(0.536619300889434,3.94087098263999,
-4.58002899725778)) ;
#105310 = CARTESIAN_POINT('Ctrl Pts',(0.536997639747708,3.95938954612073,
-4.58068581289575)) ;
#105311 = CARTESIAN_POINT('Ctrl Pts',(0.539142315171053,3.9756712086989,-4.58431206156158)) ;
#105312 = CARTESIAN_POINT('Ctrl Pts',(0.544035197036652,4.00535605098083,
-4.59539939166598)) ;
#105313 = CARTESIAN_POINT('Ctrl Pts',(0.546989816174412,4.01946236900603,
-4.60356994463497)) ;
#105314 = CARTESIAN_POINT('Ctrl Pts',(0.54946306249569,4.035955360074,-4.61854738169713)) ;
#105315 = CARTESIAN_POINT('Ctrl Pts',(0.550000000000879,4.04078397701435,
-4.62399442034635)) ;
#105316 = CARTESIAN_POINT('Ctrl Pts',(0.549999999999999,4.04473197181449,
-4.63000000001465)) ;
#105317 = CARTESIAN_POINT('Origin',(-0.4,2.3,-4.68)) ;
#105318 = CARTESIAN_POINT('Origin',(0.4,2.29999999999999,-5.48)) ;
#105319 = CARTESIAN_POINT('Origin',(0.4,-3.36847777691809,-5.48)) ;
#105320 = CARTESIAN_POINT('Origin',(-0.0979344438426628,-3.8,-5.17793444384266)) ;
#105321 = CARTESIAN_POINT('Origin',(-0.0979344438426628,-3.8,-5.17793444384266)) ;
#105322 = CARTESIAN_POINT('Origin',(-0.0979344438426627,-3.8,-5.17793444384266)) ;
#105323 = CARTESIAN_POINT('Origin',(-0.4,2.3,-4.68)) ;
#105324 = CARTESIAN_POINT('Origin',(-0.4,-3.36847777691809,-4.68)) ;
#105325 = CARTESIAN_POINT('Origin',(0.190875981738719,-3.6672263744342,-5.27087598173872)) ;
#105326 = CARTESIAN_POINT('Origin',(0.400000000000001,-3.36847777691809,-5.48)) ;
#105327 = CARTESIAN_POINT('Origin',(0.0979344438426626,-3.8,-5.17793444384266)) ;
#105328 = CARTESIAN_POINT('Origin',(0.15,-3.8,-5.17793444384266)) ;
#105329 = CARTESIAN_POINT('Origin',(0.0979344438426627,-3.8,-5.17793444384266)) ;
#105330 = CARTESIAN_POINT('Origin',(-0.0979344438426628,-3.8,-4.58)) ;
#105331 = CARTESIAN_POINT('Origin',(-0.0979344438426628,-3.8,-4.98206555615734)) ;
#105332 = CARTESIAN_POINT('Origin',(-0.174966890829628,-3.68995364716148,
-4.90503310917037)) ;
#105333 = CARTESIAN_POINT('Origin',(-0.400000000000001,-3.36847777691809,
-4.68)) ;
#105334 = CARTESIAN_POINT('Origin',(-0.0979344438426627,-3.8,-4.98206555615734)) ;
#105335 = CARTESIAN_POINT('Origin',(0.0979344438426627,-3.8,-5.17793444384266)) ;
#105336 = CARTESIAN_POINT('Origin',(0.0979344438426628,-3.8,-5.17793444384266)) ;
#105337 = CARTESIAN_POINT('Origin',(-0.0979344438426628,-3.8,-4.98206555615734)) ;
#105338 = CARTESIAN_POINT('Origin',(-0.0979344438426628,-3.8,-4.98206555615734)) ;
#105339 = CARTESIAN_POINT('Origin',(0.0979344438426627,-3.8,-4.58)) ;
#105340 = CARTESIAN_POINT('Origin',(0.0979344438426627,-3.8,-4.98206555615734)) ;
#105341 = CARTESIAN_POINT('Origin',(-1.11032778078669,-3.8,-4.98206555615734)) ;
#105342 = CARTESIAN_POINT('Origin',(0.0979344438426626,-3.8,-4.98206555615734)) ;
#105343 = CARTESIAN_POINT('Origin',(0.0979344438426627,-3.8,-4.98206555615734)) ;
#105344 = CARTESIAN_POINT('Origin',(0.0979344438426627,-3.8,-4.98206555615734)) ;
#105345 = CARTESIAN_POINT('Origin',(0.438350729213467,-3.31369102089885,-4.64164927078653)) ;
#105346 = CARTESIAN_POINT('Origin',(0.399999999999999,-3.36847777691809,-4.68)) ;
#105347 = CARTESIAN_POINT('Origin',(0.4,2.3,-4.68)) ;
#105348 = CARTESIAN_POINT('Origin',(0.4,-3.36847777691809,-4.68)) ;
#105349 = CARTESIAN_POINT('Origin',(0.4,2.29999999999999,-4.68)) ;
#105350 = CARTESIAN_POINT('Origin',(1.5,2.3,-4.68)) ;
#105351 = CARTESIAN_POINT('Ctrl Pts',(0.55,2.65280931275594,-4.63000000000009)) ;
#105352 = CARTESIAN_POINT('Ctrl Pts',(0.550000000000012,2.67648433237898,
-4.6157238466627)) ;
#105353 = CARTESIAN_POINT('Ctrl Pts',(0.546908864252786,2.69988533923263,
-4.60352570084762)) ;
#105354 = CARTESIAN_POINT('Ctrl Pts',(0.539540151921445,2.76165254733708,
-4.58409159819012)) ;
#105355 = CARTESIAN_POINT('Ctrl Pts',(0.536602540378443,2.79600904778112,
-4.58)) ;
#105356 = CARTESIAN_POINT('Ctrl Pts',(0.536602540378443,2.83090991212703,
-4.58)) ;
#105357 = CARTESIAN_POINT('Origin',(8.,3.4,-5.48)) ;
#105358 = CARTESIAN_POINT('Origin',(7.96847777691809,3.4,-5.48)) ;
#105359 = CARTESIAN_POINT('Origin',(1.5,4.2,-5.48)) ;
#105360 = CARTESIAN_POINT('Origin',(7.96847777691809,4.2,-5.48)) ;
#105361 = CARTESIAN_POINT('Origin',(8.64348900069683,3.87250785664512,-5.00749214335488)) ;
#105362 = CARTESIAN_POINT('Origin',(7.96847777691809,3.4,-5.48)) ;
#105363 = CARTESIAN_POINT('Origin',(8.4,3.70206555615734,-5.17793444384266)) ;
#105364 = CARTESIAN_POINT('Origin',(8.26722637443421,3.99087598173872,-5.27087598173872)) ;
#105365 = CARTESIAN_POINT('Origin',(7.96847777691809,4.2,-5.48)) ;
#105366 = CARTESIAN_POINT('Origin',(8.4,3.89793444384266,-5.17793444384266)) ;
#105367 = CARTESIAN_POINT('Origin',(8.4,3.95,-5.17793444384266)) ;
#105368 = CARTESIAN_POINT('Origin',(8.4,3.70206555615734,-5.17793444384266)) ;
#105369 = CARTESIAN_POINT('Origin',(8.4,3.89793444384266,-5.17793444384266)) ;
#105370 = CARTESIAN_POINT('Origin',(8.4,3.70206555615734,-5.17793444384266)) ;
#105371 = CARTESIAN_POINT('Origin',(8.4,3.70206555615734,-5.17793444384266)) ;
#105372 = CARTESIAN_POINT('Origin',(1.5,3.4,-4.68)) ;
#105373 = CARTESIAN_POINT('Origin',(7.96847777691809,3.4,-4.68)) ;
#105374 = CARTESIAN_POINT('Origin',(1.5,4.2,-4.68)) ;
#105375 = CARTESIAN_POINT('Origin',(7.96847777691809,4.2,-4.68)) ;
#105376 = CARTESIAN_POINT('Origin',(8.4,3.89793444384266,-5.17793444384266)) ;
#105377 = CARTESIAN_POINT('Origin',(8.4,3.89793444384266,-5.17793444384266)) ;
#105378 = CARTESIAN_POINT('Origin',(8.4,3.70206555615734,-4.58)) ;
#105379 = CARTESIAN_POINT('Origin',(8.4,3.70206555615734,-4.98206555615734)) ;
#105380 = CARTESIAN_POINT('Origin',(8.28995364716148,3.62503310917037,-4.90503310917037)) ;
#105381 = CARTESIAN_POINT('Origin',(7.96847777691809,3.4,-4.68)) ;
#105382 = CARTESIAN_POINT('Origin',(8.4,3.70206555615734,-4.98206555615734)) ;
#105383 = CARTESIAN_POINT('Origin',(7.91369102089885,4.23835072921347,-4.64164927078653)) ;
#105384 = CARTESIAN_POINT('Origin',(7.96847777691809,4.2,-4.68)) ;
#105385 = CARTESIAN_POINT('Origin',(8.4,3.89793444384266,-4.98206555615734)) ;
#105386 = CARTESIAN_POINT('Origin',(8.4,3.89793444384266,-4.58)) ;
#105387 = CARTESIAN_POINT('Origin',(8.4,3.89793444384266,-4.98206555615734)) ;
#105388 = CARTESIAN_POINT('Origin',(8.4,3.70206555615734,-4.98206555615734)) ;
#105389 = CARTESIAN_POINT('Origin',(8.4,3.70206555615734,-4.98206555615734)) ;
#105390 = CARTESIAN_POINT('Origin',(8.4,3.89793444384266,-4.98206555615734)) ;
#105391 = CARTESIAN_POINT('Origin',(8.4,3.89793444384266,-4.98206555615734)) ;
#105392 = CARTESIAN_POINT('Origin',(8.4,2.68967221921331,-4.98206555615734)) ;
#105393 = CARTESIAN_POINT('Origin',(9.9,6.8847127088383,-7.62)) ;
#105394 = CARTESIAN_POINT('Origin',(9.9,6.8847127088383,-6.03971270883831)) ;
#105395 = CARTESIAN_POINT('Origin',(8.77035388141948,6.69643835574155,-5.85143835574155)) ;
#105396 = CARTESIAN_POINT('Ctrl Pts',(8.58356010126947,6.66256607592813,-5.71892668354491)) ;
#105397 = CARTESIAN_POINT('Ctrl Pts',(8.58266714977878,6.65676189123867,-5.71877785829646)) ;
#105398 = CARTESIAN_POINT('Ctrl Pts',(8.58182526931896,6.6507714222091,-5.71911417147406)) ;
#105399 = CARTESIAN_POINT('Ctrl Pts',(8.58032528754339,6.63886560514846,-5.72091273509962)) ;
#105400 = CARTESIAN_POINT('Ctrl Pts',(8.57966270906115,6.63295370212233,-5.72234482433268)) ;
#105401 = CARTESIAN_POINT('Ctrl Pts',(8.57906641006225,6.62681909302566,-5.72447717449357)) ;
#105402 = CARTESIAN_POINT('Ctrl Pts',(8.57903375157331,6.62647998752528,-5.72459716972835)) ;
#105403 = CARTESIAN_POINT('Ctrl Pts',(8.57846569624192,6.62052582174872,-5.72674173168093)) ;
#105404 = CARTESIAN_POINT('Ctrl Pts',(8.57802501793963,6.61503168015239,-5.72931428585577)) ;
#105405 = CARTESIAN_POINT('Ctrl Pts',(8.57766199200567,6.60925146760294,-5.73274621332342)) ;
#105406 = CARTESIAN_POINT('Ctrl Pts',(8.57762821177171,6.60869602779095,-5.73308383516466)) ;
#105407 = CARTESIAN_POINT('Ctrl Pts',(8.57728522755448,6.60286036001487,-5.736714798957)) ;
#105408 = CARTESIAN_POINT('Ctrl Pts',(8.57709550103272,6.59788070192389,-5.74054822105585)) ;
#105409 = CARTESIAN_POINT('Ctrl Pts',(8.57703980289277,6.59299711069447,-5.7451723373543)) ;
#105410 = CARTESIAN_POINT('Ctrl Pts',(8.5770367027102,6.59265952430066,-5.74549689254174)) ;
#105411 = CARTESIAN_POINT('Ctrl Pts',(8.57701334129167,6.58927432516127,-5.74880138159525)) ;
#105412 = CARTESIAN_POINT('Ctrl Pts',(8.57705699426433,6.58642971201549,-5.75199174440871)) ;
#105413 = CARTESIAN_POINT('Ctrl Pts',(8.57735031225518,6.57961409340219,-5.76079544175541)) ;
#105414 = CARTESIAN_POINT('Ctrl Pts',(8.57770856513435,6.57604383182912,-5.76666824553985)) ;
#105415 = CARTESIAN_POINT('Ctrl Pts',(8.5786570497109,6.57055741297632,-5.77833221933877)) ;
#105416 = CARTESIAN_POINT('Ctrl Pts',(8.57922107378969,6.56851476050442,-5.78407363490774)) ;
#105417 = CARTESIAN_POINT('Ctrl Pts',(8.57993695782544,6.5668761019375,-5.79045593481641)) ;
#105418 = CARTESIAN_POINT('Ctrl Pts',(8.58000419042984,6.56673001682054,-5.79104783518392)) ;
#105419 = CARTESIAN_POINT('Ctrl Pts',(8.58074399738023,6.56520526212514,-5.7974812517356)) ;
#105420 = CARTESIAN_POINT('Ctrl Pts',(8.58149993293355,6.56438134785768,-5.80335418009406)) ;
#105421 = CARTESIAN_POINT('Ctrl Pts',(8.58236768178486,6.56403389662199,-5.80949875782384)) ;
#105422 = CARTESIAN_POINT('Ctrl Pts',(8.58242358604552,6.56401394107884,-5.80989217363188)) ;
#105423 = CARTESIAN_POINT('Ctrl Pts',(8.58283067264383,6.56388592662946,-5.81273942342641)) ;
#105424 = CARTESIAN_POINT('Ctrl Pts',(8.5831915624065,6.56386525642004,-5.81516995058283)) ;
#105425 = CARTESIAN_POINT('Ctrl Pts',(8.58356019967708,6.56392669994633,-5.81756626506471)) ;
#105426 = CARTESIAN_POINT('Origin',(9.9,6.8847127088383,-6.03971270883831)) ;
#105427 = CARTESIAN_POINT('Origin',(9.9,6.8847127088383,-6.03971270883831)) ;
#105428 = CARTESIAN_POINT('Origin',(9.9,6.8847127088383,-6.03971270883831)) ;
#105429 = CARTESIAN_POINT('Origin',(9.9,7.72792407799439,-7.62)) ;
#105430 = CARTESIAN_POINT('Origin',(9.9,7.72792407799439,-6.03971270883831)) ;
#105431 = CARTESIAN_POINT('Origin',(9.90000000000001,4.35421736843756,-6.03971270883831)) ;
#105432 = CARTESIAN_POINT('Origin',(9.9,7.72792407799439,-6.03971270883831)) ;
#105433 = CARTESIAN_POINT('Origin',(9.9,7.72792407799439,-6.03971270883831)) ;
#105434 = CARTESIAN_POINT('Origin',(9.9,7.72792407799439,-6.03971270883831)) ;
#105435 = CARTESIAN_POINT('Origin',(10.9628342502842,7.37364599456632,-6.21685175055234)) ;
#105436 = CARTESIAN_POINT('Ctrl Pts',(8.56837732530586,8.27720755823131,-5.81250525379773)) ;
#105437 = CARTESIAN_POINT('Ctrl Pts',(8.56753565030796,8.2774881236726,-5.80661299219742)) ;
#105438 = CARTESIAN_POINT('Ctrl Pts',(8.5668204554169,8.27721180667909,-5.80054129443957)) ;
#105439 = CARTESIAN_POINT('Ctrl Pts',(8.56575413148036,8.2753862416024,-5.78872847211981)) ;
#105440 = CARTESIAN_POINT('Ctrl Pts',(8.56538426077881,8.27391165896583,-5.78299056243199)) ;
#105441 = CARTESIAN_POINT('Ctrl Pts',(8.56517777855947,8.27166501362668,-5.77701477545133)) ;
#105442 = CARTESIAN_POINT('Ctrl Pts',(8.56516523451691,8.27151619608676,-5.77662763828585)) ;
#105443 = CARTESIAN_POINT('Ctrl Pts',(8.56497390811218,8.26902793125447,-5.77029533599119)) ;
#105444 = CARTESIAN_POINT('Ctrl Pts',(8.56499903025539,8.26597630129447,-5.76453577846586)) ;
#105445 = CARTESIAN_POINT('Ctrl Pts',(8.56538588200264,8.26046191593052,-5.75659067236816)) ;
#105446 = CARTESIAN_POINT('Ctrl Pts',(8.56556309332513,8.25853771611453,-5.75412123645577)) ;
#105447 = CARTESIAN_POINT('Ctrl Pts',(8.56628156514555,8.25214511987154,-5.74680175668912)) ;
#105448 = CARTESIAN_POINT('Ctrl Pts',(8.56700742874798,8.24720216256262,-5.74230544523098)) ;
#105449 = CARTESIAN_POINT('Ctrl Pts',(8.5688071379813,8.23661566152166,-5.73462449488006)) ;
#105450 = CARTESIAN_POINT('Ctrl Pts',(8.56986039391321,8.23102391526976,-5.73138488072561)) ;
#105451 = CARTESIAN_POINT('Ctrl Pts',(8.57116255171754,8.22459552194136,-5.72844677452705)) ;
#105452 = CARTESIAN_POINT('Ctrl Pts',(8.5712749581022,8.22404408343787,-5.72820066079021)) ;
#105453 = CARTESIAN_POINT('Ctrl Pts',(8.57260511146326,8.21755901312516,-5.72537491530524)) ;
#105454 = CARTESIAN_POINT('Ctrl Pts',(8.57395629672869,8.21135759730784,-5.72334638642728)) ;
#105455 = CARTESIAN_POINT('Ctrl Pts',(8.57552311082448,8.20452945286157,-5.72174954431703)) ;
#105456 = CARTESIAN_POINT('Ctrl Pts',(8.57564505123029,8.20400026307019,-5.7216298269559)) ;
#105457 = CARTESIAN_POINT('Ctrl Pts',(8.57731301559527,8.19679193622625,-5.72005346253701)) ;
#105458 = CARTESIAN_POINT('Ctrl Pts',(8.57896065127873,8.1900216848535,-5.71921096934403)) ;
#105459 = CARTESIAN_POINT('Ctrl Pts',(8.58161366784367,8.17959769015469,-5.71875531727718)) ;
#105460 = CARTESIAN_POINT('Ctrl Pts',(8.58258362864271,8.17587911616509,-5.71876393810712)) ;
#105461 = CARTESIAN_POINT('Ctrl Pts',(8.58356010126947,8.17221734381475,-5.71892668354492)) ;
#105462 = CARTESIAN_POINT('Origin',(7.96824861826159,6.56275414521524,-4.44224585478477)) ;
#105463 = CARTESIAN_POINT('Origin',(8.59688370202654,6.66156024040368,-4.35124347526272)) ;
#105464 = CARTESIAN_POINT('Origin',(9.9,6.8847127088383,-4.1202872911617)) ;
#105465 = CARTESIAN_POINT('Origin',(9.9,6.8847127088383,-7.62)) ;
#105466 = CARTESIAN_POINT('Origin',(9.9,6.8847127088383,-4.1202872911617)) ;
#105467 = CARTESIAN_POINT('Origin',(9.9,6.8847127088383,-4.1202872911617)) ;
#105468 = CARTESIAN_POINT('Origin',(9.9,6.8847127088383,-4.1202872911617)) ;
#105469 = CARTESIAN_POINT('Origin',(9.9,6.8,-4.1202872911617)) ;
#105470 = CARTESIAN_POINT('Origin',(9.9,7.72792407799439,-4.1202872911617)) ;
#105471 = CARTESIAN_POINT('Origin',(9.9,7.72792407799439,-7.62)) ;
#105472 = CARTESIAN_POINT('Origin',(9.9,7.72792407799439,-4.1202872911617)) ;
#105473 = CARTESIAN_POINT('Origin',(9.9,7.72792407799439,-4.1202872911617)) ;
#105474 = CARTESIAN_POINT('Origin',(9.9,7.72792407799439,-4.1202872911617)) ;
#105475 = CARTESIAN_POINT('Origin',(9.60917571369883,7.82486550676144,-4.16875800554523)) ;
#105476 = CARTESIAN_POINT('Origin',(8.5909900184595,8.18966234087008,-4.34516097389893)) ;
#105477 = CARTESIAN_POINT('Origin',(0.45,4.4,-5.08)) ;
#105478 = CARTESIAN_POINT('Origin',(0.45,4.4,-5.53)) ;
#105479 = CARTESIAN_POINT('Origin',(0.45,4.4,-4.63)) ;
#105480 = CARTESIAN_POINT('Origin',(-1.9,7.55,-7.62)) ;
#105481 = CARTESIAN_POINT('Origin',(6.9,7.75,-7.62)) ;
#105482 = CARTESIAN_POINT('Origin',(7.1,8.2,-7.62)) ;
#105483 = CARTESIAN_POINT('Origin',(9.9,0.1,-7.62)) ;
#105484 = CARTESIAN_POINT('Origin',(9.9,1.16528729116168,-7.62)) ;
#105485 = CARTESIAN_POINT('Origin',(9.9,1.16528729116168,-7.12416188017819)) ;
#105486 = CARTESIAN_POINT('Origin',(9.9,3.8,-5.08)) ;
#105487 = CARTESIAN_POINT('Origin',(9.9,1.16528729116168,-3.0358381198218)) ;
#105488 = CARTESIAN_POINT('Origin',(9.9,1.16528729116168,-7.12416188017819)) ;
#105489 = CARTESIAN_POINT('Origin',(9.9,1.16528729116168,-7.62)) ;
#105490 = CARTESIAN_POINT('Origin',(9.9,1.16528729116168,-3.0358381198218)) ;
#105491 = CARTESIAN_POINT('Ctrl Pts',(0.55,0.3,-5.53)) ;
#105492 = CARTESIAN_POINT('Ctrl Pts',(0.55,0.3,-5.63)) ;
#105493 = CARTESIAN_POINT('Ctrl Pts',(0.45,0.3,-5.63)) ;
#105494 = CARTESIAN_POINT('Ctrl Pts',(0.55,0.28690770353672,-5.53000000081823)) ;
#105495 = CARTESIAN_POINT('Ctrl Pts',(0.549992696052345,0.300543498459179,
-5.62999269603997)) ;
#105496 = CARTESIAN_POINT('Ctrl Pts',(0.450000000818259,0.286907703536718,
-5.63)) ;
#105497 = CARTESIAN_POINT('Ctrl Pts',(0.552602750539093,0.273825167611082,
-5.53520550107818)) ;
#105498 = CARTESIAN_POINT('Ctrl Pts',(0.546703256435892,0.299059401315782,
-5.62670325643589)) ;
#105499 = CARTESIAN_POINT('Ctrl Pts',(0.455205501078185,0.273825167611084,
-5.63260275053909)) ;
#105500 = CARTESIAN_POINT('Ctrl Pts',(0.56262134295865,0.249638145915901,
-5.5552426859173)) ;
#105501 = CARTESIAN_POINT('Ctrl Pts',(0.544986924117075,0.282072776439542,
-5.62498692411708)) ;
#105502 = CARTESIAN_POINT('Ctrl Pts',(0.4752426859173,0.249638145915898,-5.64262134295865)) ;
#105503 = CARTESIAN_POINT('Ctrl Pts',(0.570033341471288,0.238545302291403,
-5.57006668294258)) ;
#105504 = CARTESIAN_POINT('Ctrl Pts',(0.547116196858396,0.267914459835244,
-5.6271161968584)) ;
#105505 = CARTESIAN_POINT('Ctrl Pts',(0.490066682942577,0.238545302291402,
-5.65003334147129)) ;
#105506 = CARTESIAN_POINT('Ctrl Pts',(0.597801282701459,0.210777361061231,
-5.62560256540292)) ;
#105507 = CARTESIAN_POINT('Ctrl Pts',(0.570853448890183,0.226374713859281,
-5.65085344889018)) ;
#105508 = CARTESIAN_POINT('Ctrl Pts',(0.545602565402917,0.210777361061233,
-5.67780128270146)) ;
#105509 = CARTESIAN_POINT('Ctrl Pts',(0.623746567173609,0.2,-5.6774931343473)) ;
#105510 = CARTESIAN_POINT('Ctrl Pts',(0.610458667315046,0.2,-5.69045866731505)) ;
#105511 = CARTESIAN_POINT('Ctrl Pts',(0.59749313434727,0.2,-5.70374656717367)) ;
#105512 = CARTESIAN_POINT('Ctrl Pts',(0.65,0.2,-5.73)) ;
#105513 = CARTESIAN_POINT('Ctrl Pts',(0.65,0.2,-5.73)) ;
#105514 = CARTESIAN_POINT('Ctrl Pts',(0.65,0.2,-5.73)) ;
#105515 = CARTESIAN_POINT('Origin',(0.45,0.3,-5.53)) ;
#105516 = CARTESIAN_POINT('Origin',(0.45,1.24941393210234E-16,-5.53)) ;
#105517 = CARTESIAN_POINT('Origin',(0.45,4.4,-5.53)) ;
#105518 = CARTESIAN_POINT('Origin',(0.45,4.4,-5.53)) ;
#105519 = CARTESIAN_POINT('Origin',(0.45,4.4,-5.53)) ;
#105520 = CARTESIAN_POINT('Origin',(0.549999999999999,4.4,-5.53)) ;
#105521 = CARTESIAN_POINT('Origin',(-1.7,4.4,-5.53)) ;
#105522 = CARTESIAN_POINT('Ctrl Pts',(-1.8,4.6,-5.73)) ;
#105523 = CARTESIAN_POINT('Ctrl Pts',(-1.8,4.6,-5.73)) ;
#105524 = CARTESIAN_POINT('Ctrl Pts',(-1.8,4.6,-5.73)) ;
#105525 = CARTESIAN_POINT('Ctrl Pts',(-1.8,4.5737465671737,-5.67749313434726)) ;
#105526 = CARTESIAN_POINT('Ctrl Pts',(-1.8,4.56045866731625,-5.69045866731612)) ;
#105527 = CARTESIAN_POINT('Ctrl Pts',(-1.8,4.54749313434731,-5.70374656717359)) ;
#105528 = CARTESIAN_POINT('Ctrl Pts',(-1.78922263893876,4.54780128270145,
-5.62560256540292)) ;
#105529 = CARTESIAN_POINT('Ctrl Pts',(-1.77362528614073,4.52085344889015,
-5.65085344889015)) ;
#105530 = CARTESIAN_POINT('Ctrl Pts',(-1.78922263893876,4.49560256540291,
-5.67780128270145)) ;
#105531 = CARTESIAN_POINT('Ctrl Pts',(-1.7614546977086,4.5200333414713,-5.57006668294258)) ;
#105532 = CARTESIAN_POINT('Ctrl Pts',(-1.73208554016475,4.49711619685841,
-5.62711619685841)) ;
#105533 = CARTESIAN_POINT('Ctrl Pts',(-1.7614546977086,4.44006668294258,-5.6500333414713)) ;
#105534 = CARTESIAN_POINT('Ctrl Pts',(-1.7503618540841,4.51262134295865,-5.55524268591729)) ;
#105535 = CARTESIAN_POINT('Ctrl Pts',(-1.71792722356046,4.49498692411707,
-5.62498692411707)) ;
#105536 = CARTESIAN_POINT('Ctrl Pts',(-1.7503618540841,4.42524268591729,-5.64262134295865)) ;
#105537 = CARTESIAN_POINT('Ctrl Pts',(-1.72617483238892,4.50260275053909,
-5.5352055010782)) ;
#105538 = CARTESIAN_POINT('Ctrl Pts',(-1.70094059868422,4.4967032564359,-5.6267032564359)) ;
#105539 = CARTESIAN_POINT('Ctrl Pts',(-1.72617483238892,4.4052055010782,-5.63260275053909)) ;
#105540 = CARTESIAN_POINT('Ctrl Pts',(-1.71309229646328,4.5,-5.53000000081823)) ;
#105541 = CARTESIAN_POINT('Ctrl Pts',(-1.69945650154594,4.49999269603999,
-5.62999269603999)) ;
#105542 = CARTESIAN_POINT('Ctrl Pts',(-1.71309229646328,4.40000000081823,
-5.63)) ;
#105543 = CARTESIAN_POINT('Ctrl Pts',(-1.7,4.5,-5.53)) ;
#105544 = CARTESIAN_POINT('Ctrl Pts',(-1.7,4.5,-5.63)) ;
#105545 = CARTESIAN_POINT('Ctrl Pts',(-1.7,4.4,-5.63)) ;
#105546 = CARTESIAN_POINT('Ctrl Pts',(-1.8,4.6,-4.43)) ;
#105547 = CARTESIAN_POINT('Ctrl Pts',(-1.8,4.6,-4.43)) ;
#105548 = CARTESIAN_POINT('Ctrl Pts',(-1.8,4.6,-4.43)) ;
#105549 = CARTESIAN_POINT('Ctrl Pts',(-1.8,4.54749313434731,-4.45625343282641)) ;
#105550 = CARTESIAN_POINT('Ctrl Pts',(-1.8,4.56045866731625,-4.46954133268388)) ;
#105551 = CARTESIAN_POINT('Ctrl Pts',(-1.8,4.57374656717369,-4.48250686565274)) ;
#105552 = CARTESIAN_POINT('Ctrl Pts',(-1.78922263893876,4.49560256540291,
-4.48219871729855)) ;
#105553 = CARTESIAN_POINT('Ctrl Pts',(-1.77362528614073,4.52085344889015,
-4.50914655110985)) ;
#105554 = CARTESIAN_POINT('Ctrl Pts',(-1.78922263893876,4.54780128270145,
-4.53439743459709)) ;
#105555 = CARTESIAN_POINT('Ctrl Pts',(-1.7614546977086,4.44006668294258,-4.5099666585287)) ;
#105556 = CARTESIAN_POINT('Ctrl Pts',(-1.73208554016475,4.49711619685842,
-4.53288380314159)) ;
#105557 = CARTESIAN_POINT('Ctrl Pts',(-1.7614546977086,4.5200333414713,-4.58993331705742)) ;
#105558 = CARTESIAN_POINT('Ctrl Pts',(-1.7503618540841,4.42524268591729,-4.51737865704135)) ;
#105559 = CARTESIAN_POINT('Ctrl Pts',(-1.71792722356046,4.49498692411707,
-4.53501307588293)) ;
#105560 = CARTESIAN_POINT('Ctrl Pts',(-1.7503618540841,4.51262134295865,-4.60475731408271)) ;
#105561 = CARTESIAN_POINT('Ctrl Pts',(-1.72617483238892,4.4052055010782,-4.52739724946091)) ;
#105562 = CARTESIAN_POINT('Ctrl Pts',(-1.70094059868422,4.4967032564359,-4.5332967435641)) ;
#105563 = CARTESIAN_POINT('Ctrl Pts',(-1.72617483238892,4.50260275053909,
-4.6247944989218)) ;
#105564 = CARTESIAN_POINT('Ctrl Pts',(-1.71309229646328,4.40000000081823,
-4.53)) ;
#105565 = CARTESIAN_POINT('Ctrl Pts',(-1.69945650154594,4.49999269603999,
-4.53000730396001)) ;
#105566 = CARTESIAN_POINT('Ctrl Pts',(-1.71309229646328,4.5,-4.62999999918177)) ;
#105567 = CARTESIAN_POINT('Ctrl Pts',(-1.7,4.4,-4.53)) ;
#105568 = CARTESIAN_POINT('Ctrl Pts',(-1.7,4.5,-4.53)) ;
#105569 = CARTESIAN_POINT('Ctrl Pts',(-1.7,4.5,-4.63)) ;
#105570 = CARTESIAN_POINT('Origin',(-1.7,4.4,-4.63)) ;
#105571 = CARTESIAN_POINT('Origin',(0.549999999999999,4.4,-4.63)) ;
#105572 = CARTESIAN_POINT('Origin',(0.45,4.4,-4.63)) ;
#105573 = CARTESIAN_POINT('Origin',(0.45,4.4,-4.63)) ;
#105574 = CARTESIAN_POINT('Origin',(0.45,4.4,-4.63)) ;
#105575 = CARTESIAN_POINT('Origin',(0.45,4.9047241136249E-17,-4.63)) ;
#105576 = CARTESIAN_POINT('Origin',(0.45,0.3,-4.63)) ;
#105577 = CARTESIAN_POINT('Ctrl Pts',(0.45,0.3,-4.53)) ;
#105578 = CARTESIAN_POINT('Ctrl Pts',(0.55,0.3,-4.53)) ;
#105579 = CARTESIAN_POINT('Ctrl Pts',(0.55,0.3,-4.63)) ;
#105580 = CARTESIAN_POINT('Ctrl Pts',(0.450000000818259,0.286907703536718,
-4.53)) ;
#105581 = CARTESIAN_POINT('Ctrl Pts',(0.549992696057035,0.30054349846111,
-4.53000730396006)) ;
#105582 = CARTESIAN_POINT('Ctrl Pts',(0.55,0.28690770353672,-4.62999999918177)) ;
#105583 = CARTESIAN_POINT('Ctrl Pts',(0.455205501078185,0.273825167611084,
-4.52739724946091)) ;
#105584 = CARTESIAN_POINT('Ctrl Pts',(0.5467032564359,0.299059401315787,-4.53329674356411)) ;
#105585 = CARTESIAN_POINT('Ctrl Pts',(0.552602750539093,0.273825167611082,
-4.62479449892182)) ;
#105586 = CARTESIAN_POINT('Ctrl Pts',(0.4752426859173,0.249638145915898,-4.51737865704135)) ;
#105587 = CARTESIAN_POINT('Ctrl Pts',(0.544986924117068,0.282072776439538,
-4.53501307588292)) ;
#105588 = CARTESIAN_POINT('Ctrl Pts',(0.56262134295865,0.249638145915901,
-4.6047573140827)) ;
#105589 = CARTESIAN_POINT('Ctrl Pts',(0.490066682942577,0.238545302291402,
-4.50996665852871)) ;
#105590 = CARTESIAN_POINT('Ctrl Pts',(0.547116196858396,0.267914459835244,
-4.5328838031416)) ;
#105591 = CARTESIAN_POINT('Ctrl Pts',(0.570033341471288,0.238545302291403,
-4.58993331705742)) ;
#105592 = CARTESIAN_POINT('Ctrl Pts',(0.545602565402917,0.210777361061233,
-4.48219871729854)) ;
#105593 = CARTESIAN_POINT('Ctrl Pts',(0.570853448890183,0.226374713859281,
-4.50914655110982)) ;
#105594 = CARTESIAN_POINT('Ctrl Pts',(0.597801282701459,0.210777361061231,
-4.53439743459709)) ;
#105595 = CARTESIAN_POINT('Ctrl Pts',(0.59749313434727,0.2,-4.45625343282633)) ;
#105596 = CARTESIAN_POINT('Ctrl Pts',(0.610458667315046,0.2,-4.46954133268495)) ;
#105597 = CARTESIAN_POINT('Ctrl Pts',(0.62374656717361,0.2,-4.4825068656527)) ;
#105598 = CARTESIAN_POINT('Ctrl Pts',(0.65,0.2,-4.43)) ;
#105599 = CARTESIAN_POINT('Ctrl Pts',(0.65,0.2,-4.43)) ;
#105600 = CARTESIAN_POINT('Ctrl Pts',(0.65,0.2,-4.43)) ;
#105601 = CARTESIAN_POINT('Ctrl Pts',(8.5,8.17221734381475,-5.6202872911617)) ;
#105602 = CARTESIAN_POINT('Ctrl Pts',(8.5,8.17221734381474,-5.705)) ;
#105603 = CARTESIAN_POINT('Ctrl Pts',(8.58356010126947,8.17221734381475,-5.71892668354491)) ;
#105604 = CARTESIAN_POINT('Ctrl Pts',(8.5,8.23335379241386,-5.62028729273906)) ;
#105605 = CARTESIAN_POINT('Ctrl Pts',(8.5,8.20847425960651,-5.69745756742167)) ;
#105606 = CARTESIAN_POINT('Ctrl Pts',(8.57460439031225,8.20580126077887,-5.71743406505204)) ;
#105607 = CARTESIAN_POINT('Ctrl Pts',(8.5,8.29192178062155,-5.64717411507849)) ;
#105608 = CARTESIAN_POINT('Ctrl Pts',(8.5,8.25010493984404,-5.70925460831168)) ;
#105609 = CARTESIAN_POINT('Ctrl Pts',(8.56800970738923,8.23725302684488,-5.72977836318993)) ;
#105610 = CARTESIAN_POINT('Ctrl Pts',(8.5,8.36583651094028,-5.73655062329137)) ;
#105611 = CARTESIAN_POINT('Ctrl Pts',(8.5,8.29925403146167,-5.76336143703663)) ;
#105612 = CARTESIAN_POINT('Ctrl Pts',(8.56373266208983,8.27563607377073,-5.77375377641315)) ;
#105613 = CARTESIAN_POINT('Ctrl Pts',(8.5,8.38029241321763,-5.79795520569967)) ;
#105614 = CARTESIAN_POINT('Ctrl Pts',(8.5,8.30669116589123,-5.80480884994108)) ;
#105615 = CARTESIAN_POINT('Ctrl Pts',(8.56610123859368,8.28208399509958,-5.80480870240703)) ;
#105616 = CARTESIAN_POINT('Ctrl Pts',(8.5,8.36719795478507,-5.85605472347988)) ;
#105617 = CARTESIAN_POINT('Ctrl Pts',(8.5,8.29381262650623,-5.83951514967181)) ;
#105618 = CARTESIAN_POINT('Ctrl Pts',(8.57227762885807,8.27346847343705,-5.83492998763544)) ;
#105619 = CARTESIAN_POINT('Ctrl Pts',(8.5485213309235,8.28383177029354,-5.83598653273363)) ;
#105620 = CARTESIAN_POINT('Ctrl Pts',(8.54913757890789,8.28625057716299,-5.82292165918399)) ;
#105621 = CARTESIAN_POINT('Ctrl Pts',(8.549146361399,8.28675781111762,-5.80926478940262)) ;
#105622 = CARTESIAN_POINT('Ctrl Pts',(8.54883414737369,8.28489376483071,-5.79609886942504)) ;
#105623 = CARTESIAN_POINT('Ctrl Pts',(8.54852072231757,8.28302248819127,-5.78288188084279)) ;
#105624 = CARTESIAN_POINT('Ctrl Pts',(8.54791723678494,8.27865742078997,-5.76983129581174)) ;
#105625 = CARTESIAN_POINT('Ctrl Pts',(8.54677696932927,8.27237937104781,-5.75810207672967)) ;
#105626 = CARTESIAN_POINT('Ctrl Pts',(8.5454465495755,8.26505438658866,-5.74441687973016)) ;
#105627 = CARTESIAN_POINT('Ctrl Pts',(8.54324462275112,8.25487237915563,-5.7322537533388)) ;
#105628 = CARTESIAN_POINT('Ctrl Pts',(8.53884071267076,8.24480815719263,-5.72120716819918)) ;
#105629 = CARTESIAN_POINT('Ctrl Pts',(8.5342440055524,8.23430333763594,-5.70967697897682)) ;
#105630 = CARTESIAN_POINT('Ctrl Pts',(8.52670159721618,8.22420330618022,-5.69870426024299)) ;
#105631 = CARTESIAN_POINT('Ctrl Pts',(8.51928858688475,8.21729138318396,-5.68598817546528)) ;
#105632 = CARTESIAN_POINT('Ctrl Pts',(8.51327528614099,8.21168455548023,-5.67567311604503)) ;
#105633 = CARTESIAN_POINT('Ctrl Pts',(8.50759525524367,8.20778929846109,-5.66398494308279)) ;
#105634 = CARTESIAN_POINT('Ctrl Pts',(8.50412058850191,8.20498026622232,-5.65157394866282)) ;
#105635 = CARTESIAN_POINT('Ctrl Pts',(8.50147164778346,8.20283877743224,-5.6421123251694)) ;
#105636 = CARTESIAN_POINT('Ctrl Pts',(8.50000317248551,8.2012555848359,-5.632083357655)) ;
#105637 = CARTESIAN_POINT('Ctrl Pts',(8.50000000513446,8.20000405629318,-5.62210523872843)) ;
#105638 = CARTESIAN_POINT('Origin',(8.6,8.17221734381475,-5.6202872911617)) ;
#105639 = CARTESIAN_POINT('Origin',(8.6,4.35421736843756,-5.6202872911617)) ;
#105640 = CARTESIAN_POINT('Origin',(8.6,6.66256607592813,-5.6202872911617)) ;
#105641 = CARTESIAN_POINT('Ctrl Pts',(8.5,6.47083593368087,-5.86480810992443)) ;
#105642 = CARTESIAN_POINT('Ctrl Pts',(8.5,6.55684090505321,-5.84438773869521)) ;
#105643 = CARTESIAN_POINT('Ctrl Pts',(8.58772778625753,6.56739561896918,-5.84188170709095)) ;
#105644 = CARTESIAN_POINT('Ctrl Pts',(8.5,6.45680686388573,-5.80572152971771)) ;
#105645 = CARTESIAN_POINT('Ctrl Pts',(8.5000000000001,6.54406229478618,-5.81251016540367)) ;
#105646 = CARTESIAN_POINT('Ctrl Pts',(8.58195196310365,6.55941415012444,-5.81135768687784)) ;
#105647 = CARTESIAN_POINT('Ctrl Pts',(8.5,6.4706155658439,-5.74195245680485)) ;
#105648 = CARTESIAN_POINT('Ctrl Pts',(8.5,6.5483636998889,-5.7723987274071)) ;
#105649 = CARTESIAN_POINT('Ctrl Pts',(8.57801125828726,6.56566601372231,-5.77883445920279)) ;
#105650 = CARTESIAN_POINT('Ctrl Pts',(8.5,6.54379299301796,-5.6486264716581)) ;
#105651 = CARTESIAN_POINT('Ctrl Pts',(8.5,6.59071789516222,-5.71622651529222)) ;
#105652 = CARTESIAN_POINT('Ctrl Pts',(8.57642058265786,6.60198961470444,-5.73190635402451)) ;
#105653 = CARTESIAN_POINT('Ctrl Pts',(8.5,6.6022051807538,-5.6202872929747)) ;
#105654 = CARTESIAN_POINT('Ctrl Pts',(8.5,6.62800697860326,-5.70091767076279)) ;
#105655 = CARTESIAN_POINT('Ctrl Pts',(8.57879135173926,6.63156920211804,-5.71813189195654)) ;
#105656 = CARTESIAN_POINT('Ctrl Pts',(8.5,6.66256607592813,-5.6202872911617)) ;
#105657 = CARTESIAN_POINT('Ctrl Pts',(8.5,6.66256607592813,-5.705)) ;
#105658 = CARTESIAN_POINT('Ctrl Pts',(8.58356010126947,6.66256607592813,-5.71892668354491)) ;
#105659 = CARTESIAN_POINT('',(8.5456536674855,6.61650711947,-5.71396531829168)) ;
#105660 = CARTESIAN_POINT('Ctrl Pts',(8.545653667161,6.61650712004134,-5.71396531781346)) ;
#105661 = CARTESIAN_POINT('Ctrl Pts',(8.54527684775566,6.61717057264364,-5.71341000086367)) ;
#105662 = CARTESIAN_POINT('Ctrl Pts',(8.54488909344002,6.61782772231436,-5.71285542989966)) ;
#105663 = CARTESIAN_POINT('Ctrl Pts',(8.54449064961559,6.61847724592619,-5.7123008713851)) ;
#105664 = CARTESIAN_POINT('Ctrl Pts',(8.54445329550705,6.6185381387648,-5.71224888152437)) ;
#105665 = CARTESIAN_POINT('Ctrl Pts',(8.54441584757974,6.61859896452233,-5.71219689179164)) ;
#105666 = CARTESIAN_POINT('Ctrl Pts',(8.54437830610597,6.6186597220747,-5.71214490158589)) ;
#105667 = CARTESIAN_POINT('Ctrl Pts',(8.54363538409146,6.61986207559664,-5.7111160483068)) ;
#105668 = CARTESIAN_POINT('Ctrl Pts',(8.54285495000587,6.62104203503536,-5.71008486217465)) ;
#105669 = CARTESIAN_POINT('Ctrl Pts',(8.54204093171147,6.62218056960131,-5.70905111516717)) ;
#105670 = CARTESIAN_POINT('Ctrl Pts',(8.54157979215435,6.62282554690603,-5.70846549978176)) ;
#105671 = CARTESIAN_POINT('Ctrl Pts',(8.54110770812185,6.62345780120148,-5.70787864990663)) ;
#105672 = CARTESIAN_POINT('Ctrl Pts',(8.54062344907116,6.62407892448169,-5.70728695413965)) ;
#105673 = CARTESIAN_POINT('Ctrl Pts',(8.54011932596481,6.62472552591744,-5.7066709873185)) ;
#105674 = CARTESIAN_POINT('Ctrl Pts',(8.53960207832254,6.62535666566135,-5.70605099058905)) ;
#105675 = CARTESIAN_POINT('Ctrl Pts',(8.53907286520404,6.62597244099099,-5.70542522881105)) ;
#105676 = CARTESIAN_POINT('Ctrl Pts',(8.53887441028459,6.6262033567396,-5.7051905681443)) ;
#105677 = CARTESIAN_POINT('Ctrl Pts',(8.53867427664139,6.62643211299942,-5.70495509982106)) ;
#105678 = CARTESIAN_POINT('Ctrl Pts',(8.53847256319995,6.6266587179511,-5.70471876421835)) ;
#105679 = CARTESIAN_POINT('Ctrl Pts',(8.53842843838463,6.62670828778428,-5.70466706580526)) ;
#105680 = CARTESIAN_POINT('Ctrl Pts',(8.53838423811747,6.62675775467668,-5.70461532601745)) ;
#105681 = CARTESIAN_POINT('Ctrl Pts',(8.53833996369343,6.62680711871688,-5.70456354446015)) ;
#105682 = CARTESIAN_POINT('Ctrl Pts',(8.53829707284513,6.62685494013081,-5.70451338107651)) ;
#105683 = CARTESIAN_POINT('Ctrl Pts',(8.53825411240222,6.62690266502019,-5.70446317849309)) ;
#105684 = CARTESIAN_POINT('Ctrl Pts',(8.53821108363803,6.62695029346533,-5.70441293643774)) ;
#105685 = CARTESIAN_POINT('Ctrl Pts',(8.53803571435328,6.62714440934378,-5.70420816845341)) ;
#105686 = CARTESIAN_POINT('Ctrl Pts',(8.53785876035506,6.62733753498028,-5.70400218366477)) ;
#105687 = CARTESIAN_POINT('Ctrl Pts',(8.53767995296703,6.62753033615257,-5.7037944665652)) ;
#105688 = CARTESIAN_POINT('Ctrl Pts',(8.53649871780654,6.62880401687798,-5.70242224842506)) ;
#105689 = CARTESIAN_POINT('Ctrl Pts',(8.53528300832265,6.62998038079526,-5.70103807605966)) ;
#105690 = CARTESIAN_POINT('Ctrl Pts',(8.53403203676338,6.63110281535143,-5.69960448656493)) ;
#105691 = CARTESIAN_POINT('Ctrl Pts',(8.53346870389682,6.63160826591214,-5.6989589178679)) ;
#105692 = CARTESIAN_POINT('Ctrl Pts',(8.53289959536919,6.63209979040222,-5.69830542565945)) ;
#105693 = CARTESIAN_POINT('Ctrl Pts',(8.53232661340319,6.6325773534403,-5.69764370144387)) ;
#105694 = CARTESIAN_POINT('Ctrl Pts',(8.53206474273905,6.63279561467254,-5.69734127279847)) ;
#105695 = CARTESIAN_POINT('Ctrl Pts',(8.53180206199566,6.63301096017663,-5.69703712608071)) ;
#105696 = CARTESIAN_POINT('Ctrl Pts',(8.53153874718657,6.63322338883724,-5.69673123888074)) ;
#105697 = CARTESIAN_POINT('Ctrl Pts',(8.53007363658217,6.63440536369244,-5.69502925112708)) ;
#105698 = CARTESIAN_POINT('Ctrl Pts',(8.52858926277508,6.63549697414123,-5.69327308391312)) ;
#105699 = CARTESIAN_POINT('Ctrl Pts',(8.52711342564664,6.6364985663511,-5.69146113930635)) ;
#105700 = CARTESIAN_POINT('Ctrl Pts',(8.52634316954116,6.63702130866459,-5.69051546490281)) ;
#105701 = CARTESIAN_POINT('Ctrl Pts',(8.52557615349968,6.63751985710295,-5.68955571931119)) ;
#105702 = CARTESIAN_POINT('Ctrl Pts',(8.52481401823429,6.63799287689814,-5.68858032616127)) ;
#105703 = CARTESIAN_POINT('Ctrl Pts',(8.5246071083582,6.63812129566007,-5.68831551952531)) ;
#105704 = CARTESIAN_POINT('Ctrl Pts',(8.52440075574004,6.63824801482192,-5.68804975390226)) ;
#105705 = CARTESIAN_POINT('Ctrl Pts',(8.5241950281087,6.63837284070829,-5.68778308608104)) ;
#105706 = CARTESIAN_POINT('Ctrl Pts',(8.52404824365684,6.63846190263542,-5.68759282145926)) ;
#105707 = CARTESIAN_POINT('Ctrl Pts',(8.52390173612804,6.63855002749203,-5.68740204373474)) ;
#105708 = CARTESIAN_POINT('Ctrl Pts',(8.52375553261475,6.63863721305423,-5.68721076280486)) ;
#105709 = CARTESIAN_POINT('Ctrl Pts',(8.5229420412716,6.63912232246441,-5.68614645609245)) ;
#105710 = CARTESIAN_POINT('Ctrl Pts',(8.52213801365706,6.63957834748689,-5.68506653755637)) ;
#105711 = CARTESIAN_POINT('Ctrl Pts',(8.52134774490511,6.64000494097979,-5.68397296144637)) ;
#105712 = CARTESIAN_POINT('Ctrl Pts',(8.51876608595595,6.64139854145543,-5.68040045456944)) ;
#105713 = CARTESIAN_POINT('Ctrl Pts',(8.51630176076719,6.64256282842068,-5.6766245667844)) ;
#105714 = CARTESIAN_POINT('Ctrl Pts',(8.51404737801022,6.64354662431173,-5.67266875822867)) ;
#105715 = CARTESIAN_POINT('Ctrl Pts',(8.51174271377018,6.64455236266853,-5.66862471979259)) ;
#105716 = CARTESIAN_POINT('Ctrl Pts',(8.50965863261302,6.64536892721963,-5.66439377806961)) ;
#105717 = CARTESIAN_POINT('Ctrl Pts',(8.50786496313902,6.64606338785378,-5.66004416548596)) ;
#105718 = CARTESIAN_POINT('Ctrl Pts',(8.50767015284864,6.64613881316472,-5.65957175442987)) ;
#105719 = CARTESIAN_POINT('Ctrl Pts',(8.50747873128293,6.64621281334902,-5.65909797368753)) ;
#105720 = CARTESIAN_POINT('Ctrl Pts',(8.50729076020857,6.64628549377757,-5.65862293019382)) ;
#105721 = CARTESIAN_POINT('Ctrl Pts',(8.50722027105568,6.64631274893828,-5.65844478888368)) ;
#105722 = CARTESIAN_POINT('Ctrl Pts',(8.50715026706477,6.64633981850992,-5.65826647001924)) ;
#105723 = CARTESIAN_POINT('Ctrl Pts',(8.50708075128541,6.64636670806329,-5.65808797935946)) ;
#105724 = CARTESIAN_POINT('Ctrl Pts',(8.50659414082988,6.6465549349369,-5.65683854474099)) ;
#105725 = CARTESIAN_POINT('Ctrl Pts',(8.50613147592891,6.64673434010344,-5.65558068375498)) ;
#105726 = CARTESIAN_POINT('Ctrl Pts',(8.50569363751094,6.64690683932496,-5.65431642750228)) ;
#105727 = CARTESIAN_POINT('Ctrl Pts',(8.5039543604021,6.64759207829661,-5.64929427350717)) ;
#105728 = CARTESIAN_POINT('Ctrl Pts',(8.50258205288306,6.64816393978926,-5.64409155961505)) ;
#105729 = CARTESIAN_POINT('Ctrl Pts',(8.50162662717143,6.64864720987502,-5.63880412474346)) ;
#105730 = CARTESIAN_POINT('Ctrl Pts',(8.50156399248218,6.64867889153407,-5.63845749722853)) ;
#105731 = CARTESIAN_POINT('Ctrl Pts',(8.50150313499579,6.64871019935924,-5.63811050751598)) ;
#105732 = CARTESIAN_POINT('Ctrl Pts',(8.50144406283925,6.64874114271688,-5.63776318350201)) ;
#105733 = CARTESIAN_POINT('Ctrl Pts',(8.50057491246572,6.64919642372276,-5.63265287749383)) ;
#105734 = CARTESIAN_POINT('Ctrl Pts',(8.5000953730058,6.64957062705848,-5.62747132905128)) ;
#105735 = CARTESIAN_POINT('Ctrl Pts',(8.50001293997571,6.64989933182545,-5.62231444354085)) ;
#105736 = CARTESIAN_POINT('Ctrl Pts',(8.5000043087827,6.64993374902791,-5.621774489179)) ;
#105737 = CARTESIAN_POINT('Ctrl Pts',(8.5,6.64996765698296,-5.62123481442829)) ;
#105738 = CARTESIAN_POINT('Ctrl Pts',(8.5,6.65000108682384,-5.62069553610592)) ;
#105739 = CARTESIAN_POINT('',(8.55245136877619,6.60097994372612,-5.72678011937962)) ;
#105740 = CARTESIAN_POINT('Ctrl Pts',(8.55238056475491,6.60105295171776,-5.72688861549862)) ;
#105741 = CARTESIAN_POINT('Ctrl Pts',(8.55170523171898,6.60308542368594,-5.72510226561458)) ;
#105742 = CARTESIAN_POINT('Ctrl Pts',(8.55095829520339,6.60513808680191,-5.72336273482159)) ;
#105743 = CARTESIAN_POINT('Ctrl Pts',(8.55012599030486,6.60719152980469,-5.72165444418067)) ;
#105744 = CARTESIAN_POINT('Ctrl Pts',(8.54968322947853,6.60828389886601,-5.72074568565103)) ;
#105745 = CARTESIAN_POINT('Ctrl Pts',(8.54921644930854,6.609375699953,-5.71984624912318)) ;
#105746 = CARTESIAN_POINT('Ctrl Pts',(8.54872481267395,6.61045954913296,-5.71895574654947)) ;
#105747 = CARTESIAN_POINT('Ctrl Pts',(8.54779539897818,6.61250851009545,-5.71727229737198)) ;
#105748 = CARTESIAN_POINT('Ctrl Pts',(8.54677348694552,6.61453549290067,-5.71561559088624)) ;
#105749 = CARTESIAN_POINT('Ctrl Pts',(8.5456536674855,6.61650711947,-5.71396531829168)) ;
#105750 = CARTESIAN_POINT('',(8.55735473176751,6.58264207262433,-5.74495579736184)) ;
#105751 = CARTESIAN_POINT('Ctrl Pts',(8.55735473168706,6.58264207302769,-5.74495579684439)) ;
#105752 = CARTESIAN_POINT('Ctrl Pts',(8.55706916598059,6.58397660851249,-5.74322969337166)) ;
#105753 = CARTESIAN_POINT('Ctrl Pts',(8.55678088122709,6.58528501693236,-5.74166210096059)) ;
#105754 = CARTESIAN_POINT('Ctrl Pts',(8.55647408091827,6.58661569125868,-5.74017182325178)) ;
#105755 = CARTESIAN_POINT('Ctrl Pts',(8.55614409617586,6.58804692262381,-5.73856892751883)) ;
#105756 = CARTESIAN_POINT('Ctrl Pts',(8.55579261555195,6.58950524590085,-5.73705679501759)) ;
#105757 = CARTESIAN_POINT('Ctrl Pts',(8.55539993844513,6.59102291080506,-5.73558756777962)) ;
#105758 = CARTESIAN_POINT('Ctrl Pts',(8.55517214917315,6.59190329771233,-5.7347352792273)) ;
#105759 = CARTESIAN_POINT('Ctrl Pts',(8.55493049881969,6.5928030828913,-5.73389839775413)) ;
#105760 = CARTESIAN_POINT('Ctrl Pts',(8.55467134659054,6.59372113732125,-5.73307079464215)) ;
#105761 = CARTESIAN_POINT('Ctrl Pts',(8.55434805237174,6.59486641664501,-5.73203835397032)) ;
#105762 = CARTESIAN_POINT('Ctrl Pts',(8.55400737519031,6.59602723165029,-5.73103619819578)) ;
#105763 = CARTESIAN_POINT('Ctrl Pts',(8.55365328858765,6.59718920061515,-5.73004521551328)) ;
#105764 = CARTESIAN_POINT('Ctrl Pts',(8.55328167888689,6.59840867329803,-5.72900519091102)) ;
#105765 = CARTESIAN_POINT('Ctrl Pts',(8.55289390107692,6.59963546460028,-5.7279736796763)) ;
#105766 = CARTESIAN_POINT('Ctrl Pts',(8.55249886556662,6.60083562835454,-5.72690814943487)) ;
#105767 = CARTESIAN_POINT('Ctrl Pts',(8.55248304763318,6.60088368507321,-5.72686548368458)) ;
#105768 = CARTESIAN_POINT('Ctrl Pts',(8.5524672152281,6.60093179017218,-5.72682280673305)) ;
#105769 = CARTESIAN_POINT('Ctrl Pts',(8.55245136877619,6.60097994372612,-5.72678011937962)) ;
#105770 = CARTESIAN_POINT('Ctrl Pts',(8.56107669735261,6.56009388000089,-5.84238384722239)) ;
#105771 = CARTESIAN_POINT('Ctrl Pts',(8.56115635543004,6.5597817052481,-5.84082073438328)) ;
#105772 = CARTESIAN_POINT('Ctrl Pts',(8.56122592915387,6.55950119162287,-5.83925071298061)) ;
#105773 = CARTESIAN_POINT('Ctrl Pts',(8.56128584055879,6.55925348717442,-5.83769339194866)) ;
#105774 = CARTESIAN_POINT('Ctrl Pts',(8.56142626445293,6.55867290283846,-5.83404325081112)) ;
#105775 = CARTESIAN_POINT('Ctrl Pts',(8.56152217534692,6.55825854507371,-5.83037563387743)) ;
#105776 = CARTESIAN_POINT('Ctrl Pts',(8.56158081746989,6.55798577878939,-5.82667013542601)) ;
#105777 = CARTESIAN_POINT('Ctrl Pts',(8.5615891784535,6.55794688875063,-5.82614181874374)) ;
#105778 = CARTESIAN_POINT('Ctrl Pts',(8.56159677639836,6.5579108824123,-5.82561264525984)) ;
#105779 = CARTESIAN_POINT('Ctrl Pts',(8.56160362608007,6.55787769947532,-5.82508246747188)) ;
#105780 = CARTESIAN_POINT('Ctrl Pts',(8.56164117305277,6.55769580506315,-5.82217626368602)) ;
#105781 = CARTESIAN_POINT('Ctrl Pts',(8.56164095204357,6.55766773657215,-5.81926401199649)) ;
#105782 = CARTESIAN_POINT('Ctrl Pts',(8.56161306230089,6.55774920537472,-5.81636556725813)) ;
#105783 = CARTESIAN_POINT('Ctrl Pts',(8.56157759693122,6.55785280336172,-5.81267982460765)) ;
#105784 = CARTESIAN_POINT('Ctrl Pts',(8.56150275624661,6.55813669070952,-5.80900492802066)) ;
#105785 = CARTESIAN_POINT('Ctrl Pts',(8.56141108129146,6.55856506509341,-5.80536329254776)) ;
#105786 = CARTESIAN_POINT('Ctrl Pts',(8.56136615997221,6.55877497130415,-5.80357886768072)) ;
#105787 = CARTESIAN_POINT('Ctrl Pts',(8.56131707129299,6.55902016312283,-5.80180167096828)) ;
#105788 = CARTESIAN_POINT('Ctrl Pts',(8.56126585691693,6.55929956116443,-5.80003152546822)) ;
#105789 = CARTESIAN_POINT('Ctrl Pts',(8.56116752027494,6.55983603289964,-5.79663267190947)) ;
#105790 = CARTESIAN_POINT('Ctrl Pts',(8.56104954130217,6.56049109659201,-5.79325400757552)) ;
#105791 = CARTESIAN_POINT('Ctrl Pts',(8.56091150449776,6.561291476258,-5.78983047102478)) ;
#105792 = CARTESIAN_POINT('Ctrl Pts',(8.56080235670743,6.56192434857303,-5.7871234288615)) ;
#105793 = CARTESIAN_POINT('Ctrl Pts',(8.56068045333715,6.56264902401855,-5.78438726668918)) ;
#105794 = CARTESIAN_POINT('Ctrl Pts',(8.56054379825318,6.56349285586905,-5.7816234877209)) ;
#105795 = CARTESIAN_POINT('Ctrl Pts',(8.56050762866483,6.56371619955872,-5.78089197635184)) ;
#105796 = CARTESIAN_POINT('Ctrl Pts',(8.56047042218818,6.56394794674723,-5.78015879169821)) ;
#105797 = CARTESIAN_POINT('Ctrl Pts',(8.5604321390176,6.56418871538693,-5.77942462347088)) ;
#105798 = CARTESIAN_POINT('Ctrl Pts',(8.5602688746024,6.56521550994367,-5.77629365117944)) ;
#105799 = CARTESIAN_POINT('Ctrl Pts',(8.56008532870547,6.56636514336257,-5.77326121493511)) ;
#105800 = CARTESIAN_POINT('Ctrl Pts',(8.55988915918713,6.567626861518,-5.77047132766748)) ;
#105801 = CARTESIAN_POINT('Ctrl Pts',(8.55964574654529,6.56919243680251,-5.76700955727607)) ;
#105802 = CARTESIAN_POINT('Ctrl Pts',(8.55938661160133,6.57080906160856,-5.76373263405113)) ;
#105803 = CARTESIAN_POINT('Ctrl Pts',(8.55911582090256,6.57246439798288,-5.76066721242798)) ;
#105804 = CARTESIAN_POINT('Ctrl Pts',(8.55888928658551,6.57384919626718,-5.75810278463541)) ;
#105805 = CARTESIAN_POINT('Ctrl Pts',(8.5586381350289,6.57544444689325,-5.7553653454313)) ;
#105806 = CARTESIAN_POINT('Ctrl Pts',(8.55834707044209,6.57718152485387,-5.75266812582306)) ;
#105807 = CARTESIAN_POINT('Ctrl Pts',(8.55828762047113,6.57753632320103,-5.75211721844838)) ;
#105808 = CARTESIAN_POINT('Ctrl Pts',(8.55822651695171,6.5778969434578,-5.75156784657914)) ;
#105809 = CARTESIAN_POINT('Ctrl Pts',(8.55816364958868,6.57826264684156,-5.75102157107932)) ;
#105810 = CARTESIAN_POINT('Ctrl Pts',(8.55792499569723,6.57965091145832,-5.74894782776412)) ;
#105811 = CARTESIAN_POINT('Ctrl Pts',(8.55766032614232,6.58110993502773,-5.74692131328785)) ;
#105812 = CARTESIAN_POINT('Ctrl Pts',(8.55735473176751,6.58264207262433,-5.74495579736184)) ;
#105813 = CARTESIAN_POINT('Origin',(8.49172374697018,6.65,-7.62)) ;
#105814 = CARTESIAN_POINT('Origin',(8.49226931268683,6.63793757459679,-5.85298827163609)) ;
#105815 = CARTESIAN_POINT('Ctrl Pts',(8.40188506081772,6.5500005341705,-5.59154583081534)) ;
#105816 = CARTESIAN_POINT('Ctrl Pts',(8.50280744587447,6.54966497091134,-5.60519504075416)) ;
#105817 = CARTESIAN_POINT('Ctrl Pts',(8.50109204799972,6.6519968718077,-5.60568045493985)) ;
#105818 = CARTESIAN_POINT('Ctrl Pts',(8.39296932930804,6.55000052027914,-5.649675802422)) ;
#105819 = CARTESIAN_POINT('Ctrl Pts',(8.49725036372775,6.54968051003378,-5.63691360268317)) ;
#105820 = CARTESIAN_POINT('Ctrl Pts',(8.49665296516361,6.6493567231781,-5.63602471146354)) ;
#105821 = CARTESIAN_POINT('Ctrl Pts',(8.41146079558552,6.55000052635931,-5.7096088846459)) ;
#105822 = CARTESIAN_POINT('Ctrl Pts',(8.50278789772753,6.54967384197893,-5.66101435198054)) ;
#105823 = CARTESIAN_POINT('Ctrl Pts',(8.50590954255548,6.65051247736752,-5.66442721209356)) ;
#105824 = CARTESIAN_POINT('Ctrl Pts',(8.4574451591418,6.55000045243508,-5.76280219188218)) ;
#105825 = CARTESIAN_POINT('Ctrl Pts',(8.52023811680814,6.54973725194865,-5.70163301582095)) ;
#105826 = CARTESIAN_POINT('Ctrl Pts',(8.52891723073132,6.63643009777383,-5.69347516307825)) ;
#105827 = CARTESIAN_POINT('Ctrl Pts',(8.46608867121686,6.55000043643008,-5.7711950991747)) ;
#105828 = CARTESIAN_POINT('Ctrl Pts',(8.52334270167619,6.54974993059834,-5.7084702400789)) ;
#105829 = CARTESIAN_POINT('Ctrl Pts',(8.53324349789233,6.63337968978889,-5.69822089130001)) ;
#105830 = CARTESIAN_POINT('Ctrl Pts',(8.48465388181691,6.55000038323734,-5.78657631387441)) ;
#105831 = CARTESIAN_POINT('Ctrl Pts',(8.53001210036432,6.54978938646817,-5.72512459512324)) ;
#105832 = CARTESIAN_POINT('Ctrl Pts',(8.54253954944035,6.62323710347999,-5.70886314626898)) ;
#105833 = CARTESIAN_POINT('Ctrl Pts',(8.49467048074916,6.55000035131511,-5.79348849446136)) ;
#105834 = CARTESIAN_POINT('Ctrl Pts',(8.53347884787439,6.549811668825,-5.73305903115006)) ;
#105835 = CARTESIAN_POINT('Ctrl Pts',(8.54755337534732,6.6171479354886,-5.71286768812636)) ;
#105836 = CARTESIAN_POINT('Ctrl Pts',(8.5099793089401,6.55000022766094,-5.80338890278579)) ;
#105837 = CARTESIAN_POINT('Ctrl Pts',(8.53869035159221,6.54988741100167,-5.75877423275484)) ;
#105838 = CARTESIAN_POINT('Ctrl Pts',(8.55523846583764,6.59353839814626,-5.73352788310835)) ;
#105839 = CARTESIAN_POINT('Ctrl Pts',(8.51532901080107,6.55000016113069,-5.80633896731928)) ;
#105840 = CARTESIAN_POINT('Ctrl Pts',(8.54023459682687,6.54992340374045,-5.76848974838733)) ;
#105841 = CARTESIAN_POINT('Ctrl Pts',(8.55790835982317,6.58082417519513,-5.741582308573)) ;
#105842 = CARTESIAN_POINT('Ctrl Pts',(8.52186010906347,6.55000005932357,-5.81279275987727)) ;
#105843 = CARTESIAN_POINT('Ctrl Pts',(8.54265823247975,6.5499732773141,-5.79793164411572)) ;
#105844 = CARTESIAN_POINT('Ctrl Pts',(8.561217465186,6.56135337205721,-5.78458837007632)) ;
#105845 = CARTESIAN_POINT('Ctrl Pts',(8.52354993939971,6.55000003603139,-5.81582426222795)) ;
#105846 = CARTESIAN_POINT('Ctrl Pts',(8.54350769968241,6.54998394755847,-5.81142387320079)) ;
#105847 = CARTESIAN_POINT('Ctrl Pts',(8.56214310615443,6.55689632415131,-5.8074501335627)) ;
#105848 = CARTESIAN_POINT('Ctrl Pts',(8.5226846131811,6.55000004733863,-5.82178753041577)) ;
#105849 = CARTESIAN_POINT('Ctrl Pts',(8.54305517585924,6.54997881410037,-5.83281341214)) ;
#105850 = CARTESIAN_POINT('Ctrl Pts',(8.5615325917139,6.55906016573922,-5.84279018158066)) ;
#105851 = CARTESIAN_POINT('Ctrl Pts',(8.52060566253926,6.55000006807331,-5.82441380654967)) ;
#105852 = CARTESIAN_POINT('Ctrl Pts',(8.54195943530538,6.54996919659462,-5.84049457488593)) ;
#105853 = CARTESIAN_POINT('Ctrl Pts',(8.560584416286,6.5630274236339,-5.85450792151382)) ;
#105854 = CARTESIAN_POINT('Ctrl Pts',(8.51445291480386,6.55000012130567,-5.8312328149553)) ;
#105855 = CARTESIAN_POINT('Ctrl Pts',(8.53868948987839,6.54994355920609,-5.85941918176749)) ;
#105856 = CARTESIAN_POINT('Ctrl Pts',(8.55750149922674,6.57320954252657,-5.88118443530683)) ;
#105857 = CARTESIAN_POINT('Ctrl Pts',(8.50953280296015,6.55000015625148,-5.83504794643728)) ;
#105858 = CARTESIAN_POINT('Ctrl Pts',(8.5361628892097,6.54992588038506,-5.86776474852663)) ;
#105859 = CARTESIAN_POINT('Ctrl Pts',(8.55504783006517,6.57989127253968,-5.89069931679286)) ;
#105860 = CARTESIAN_POINT('Ctrl Pts',(8.49261655785714,6.55000026291039,-5.84849260656893)) ;
#105861 = CARTESIAN_POINT('Ctrl Pts',(8.5277825145509,6.54986718408749,-5.89576916089473)) ;
#105862 = CARTESIAN_POINT('Ctrl Pts',(8.54658667616931,6.60027178071332,-5.91935337574384)) ;
#105863 = CARTESIAN_POINT('Ctrl Pts',(8.48022165824512,6.55000031608562,-5.85776853416037)) ;
#105864 = CARTESIAN_POINT('Ctrl Pts',(8.52288681814166,6.54983437262025,-5.90745594892907)) ;
#105865 = CARTESIAN_POINT('Ctrl Pts',(8.5404533945046,6.61042388759286,-5.92630199096054)) ;
#105866 = CARTESIAN_POINT('Ctrl Pts',(8.46952991654791,6.55000035836672,-5.86909544621882)) ;
#105867 = CARTESIAN_POINT('Ctrl Pts',(8.51900842894237,6.54980714069607,-5.92336768467695)) ;
#105868 = CARTESIAN_POINT('Ctrl Pts',(8.53471369258715,6.61849392543707,-5.94138336844284)) ;
#105869 = CARTESIAN_POINT('Origin',(8.4,6.65,-5.6206780018997)) ;
#105870 = CARTESIAN_POINT('Ctrl Pts',(8.54848814460235,8.28374914930622,-4.32353717477989)) ;
#105871 = CARTESIAN_POINT('Ctrl Pts',(8.55964225199693,8.27720012980426,-4.32496794832229)) ;
#105872 = CARTESIAN_POINT('Ctrl Pts',(8.572140519951,8.27365818248462,-4.32574176255693)) ;
#105873 = CARTESIAN_POINT('Ctrl Pts',(8.54519582228991,8.29111303851995,-4.34796037880762)) ;
#105874 = CARTESIAN_POINT('Ctrl Pts',(8.55569959891143,8.2840691245988,-4.34803761744089)) ;
#105875 = CARTESIAN_POINT('Ctrl Pts',(8.56757951573636,8.27991709749369,-4.34819163391188)) ;
#105876 = CARTESIAN_POINT('Ctrl Pts',(8.54340782920288,8.28927570119137,-4.37382299312324)) ;
#105877 = CARTESIAN_POINT('Ctrl Pts',(8.5535505383751,8.28232618564302,-4.37215464428977)) ;
#105878 = CARTESIAN_POINT('Ctrl Pts',(8.5650784856842,8.27803412520748,-4.37113214305328)) ;
#105879 = CARTESIAN_POINT('Ctrl Pts',(8.54340835145922,8.27841951799442,-4.39553501116171)) ;
#105880 = CARTESIAN_POINT('Ctrl Pts',(8.55355093564017,8.27219257320284,-4.39242153876592)) ;
#105881 = CARTESIAN_POINT('Ctrl Pts',(8.56507848521152,8.26835005667905,-4.39050028050403)) ;
#105882 = CARTESIAN_POINT('Ctrl Pts',(8.54742026180266,8.27608084857565,-4.3943656412486)) ;
#105883 = CARTESIAN_POINT('Ctrl Pts',(8.54754672558908,8.27683897030433,-4.39267457303653)) ;
#105884 = CARTESIAN_POINT('Ctrl Pts',(8.54766225486892,8.27755642830995,-4.39096549730839)) ;
#105885 = CARTESIAN_POINT('Ctrl Pts',(8.54776713596767,8.27823455672262,-4.38923501677756)) ;
#105886 = CARTESIAN_POINT('Ctrl Pts',(8.54791712013337,8.27920430747291,-4.38676036041194)) ;
#105887 = CARTESIAN_POINT('Ctrl Pts',(8.54806168001142,8.28008011045346,-4.38424633726772)) ;
#105888 = CARTESIAN_POINT('Ctrl Pts',(8.54818998754192,8.28086237513951,-4.38171868385907)) ;
#105889 = CARTESIAN_POINT('Ctrl Pts',(8.5482419492675,8.28117917511831,-4.38069503986677)) ;
#105890 = CARTESIAN_POINT('Ctrl Pts',(8.54829140719362,8.28148078264966,-4.37966867429046)) ;
#105891 = CARTESIAN_POINT('Ctrl Pts',(8.54833813644415,8.28176759858571,-4.3786396299773)) ;
#105892 = CARTESIAN_POINT('Ctrl Pts',(8.54850061324771,8.28276485268192,-4.37506166052903)) ;
#105893 = CARTESIAN_POINT('Ctrl Pts',(8.54863339756396,8.28360845633784,-4.37135012352888)) ;
#105894 = CARTESIAN_POINT('Ctrl Pts',(8.54873421749658,8.28426438239345,-4.36761308675765)) ;
#105895 = CARTESIAN_POINT('Ctrl Pts',(8.54878752953697,8.28461122607275,-4.36563699879419)) ;
#105896 = CARTESIAN_POINT('Ctrl Pts',(8.54883168679926,8.28490640714038,-4.36365408207398)) ;
#105897 = CARTESIAN_POINT('Ctrl Pts',(8.54886500248133,8.28515040605083,-4.3616818590297)) ;
#105898 = CARTESIAN_POINT('Ctrl Pts',(8.54887385422351,8.28521523484357,-4.3611578532514)) ;
#105899 = CARTESIAN_POINT('Ctrl Pts',(8.54888411330031,8.285275121517,-4.36063500919228)) ;
#105900 = CARTESIAN_POINT('Ctrl Pts',(8.54889386083024,8.28533143086091,-4.36011208678616)) ;
#105901 = CARTESIAN_POINT('Ctrl Pts',(8.54894969070932,8.28565394783545,-4.35711700034689)) ;
#105902 = CARTESIAN_POINT('Ctrl Pts',(8.5489793513821,8.28586680424121,-4.35409863638292)) ;
#105903 = CARTESIAN_POINT('Ctrl Pts',(8.54899968230028,8.28595875954338,-4.35106757780128)) ;
#105904 = CARTESIAN_POINT('Ctrl Pts',(8.54900356561227,8.28597632348831,-4.3504886297174)) ;
#105905 = CARTESIAN_POINT('Ctrl Pts',(8.54900713937599,8.28598945835117,-4.34990930880415)) ;
#105906 = CARTESIAN_POINT('Ctrl Pts',(8.54901057288909,8.28599806377621,-4.34932984021852)) ;
#105907 = CARTESIAN_POINT('Ctrl Pts',(8.54902784271198,8.28604134718936,-4.34641523947593)) ;
#105908 = CARTESIAN_POINT('Ctrl Pts',(8.54901619593281,8.28598556136224,-4.34351577572171)) ;
#105909 = CARTESIAN_POINT('Ctrl Pts',(8.54898431260111,8.28582669412323,-4.34060642867547)) ;
#105910 = CARTESIAN_POINT('Ctrl Pts',(8.54893914418926,8.2856016304144,-4.33648482096958)) ;
#105911 = CARTESIAN_POINT('Ctrl Pts',(8.54884805310403,8.28517290646443,-4.33237709996661)) ;
#105912 = CARTESIAN_POINT('Ctrl Pts',(8.54869940582912,8.28455561418421,-4.32830707741367)) ;
#105913 = CARTESIAN_POINT('Ctrl Pts',(8.54864697316336,8.28433787538052,-4.32687144980245)) ;
#105914 = CARTESIAN_POINT('Ctrl Pts',(8.54858736435354,8.28409676597416,-4.32544083959233)) ;
#105915 = CARTESIAN_POINT('Ctrl Pts',(8.54851996240544,8.28383343043593,-4.32401720308527)) ;
#105916 = CARTESIAN_POINT('Origin',(8.4,6.65,-7.62)) ;
#105917 = CARTESIAN_POINT('Origin',(8.4,6.65,-4.5393219981003)) ;
#105918 = CARTESIAN_POINT('Origin',(8.49172374697018,6.65,-7.62)) ;
#105919 = CARTESIAN_POINT('Origin',(8.49225485648112,6.63809817882833,-4.30700862835662)) ;
#105920 = CARTESIAN_POINT('Origin',(8.6,4.35421736843756,-4.5397127088383)) ;
#105921 = CARTESIAN_POINT('Origin',(8.6,6.66256607592813,-4.5397127088383)) ;
#105922 = CARTESIAN_POINT('Ctrl Pts',(8.5013487493624,6.65217253603376,-4.55598525608077)) ;
#105923 = CARTESIAN_POINT('Ctrl Pts',(8.50315244876574,6.54997127577019,-4.55658636925847)) ;
#105924 = CARTESIAN_POINT('Ctrl Pts',(8.40269444133658,6.55000000392136,-4.57159649657583)) ;
#105925 = CARTESIAN_POINT('Ctrl Pts',(8.4963175378395,6.64933701877085,-4.52501565239563)) ;
#105926 = CARTESIAN_POINT('Ctrl Pts',(8.49707874924865,6.5499727017442,-4.52396122349841)) ;
#105927 = CARTESIAN_POINT('Ctrl Pts',(8.39261127161987,6.55000000381175,-4.51255502081071)) ;
#105928 = CARTESIAN_POINT('Ctrl Pts',(8.50556246021204,6.65075235208947,-4.4960110455015)) ;
#105929 = CARTESIAN_POINT('Ctrl Pts',(8.50253957946693,6.54997202229481,-4.49964413045446)) ;
#105930 = CARTESIAN_POINT('Ctrl Pts',(8.41103525938983,6.55000000386643,-4.45133834963453)) ;
#105931 = CARTESIAN_POINT('Ctrl Pts',(8.52891970071471,6.63645479210449,-4.46652715848277)) ;
#105932 = CARTESIAN_POINT('Ctrl Pts',(8.52027792490144,6.54997752826668,-4.45840493996111)) ;
#105933 = CARTESIAN_POINT('Ctrl Pts',(8.4576425585103,6.5500000033157,-4.39739010158301)) ;
#105934 = CARTESIAN_POINT('Ctrl Pts',(8.53324635448928,6.63340383613797,-4.46178206573816)) ;
#105935 = CARTESIAN_POINT('Ctrl Pts',(8.52338394863778,6.54997861189313,-4.45157331389085)) ;
#105936 = CARTESIAN_POINT('Ctrl Pts',(8.46627109069292,6.55000000319827,-4.38900474853269)) ;
#105937 = CARTESIAN_POINT('Ctrl Pts',(8.54254332011239,6.62325922024825,-4.45114174821778)) ;
#105938 = CARTESIAN_POINT('Ctrl Pts',(8.53005572430509,6.54998198465676,-4.43493264246801)) ;
#105939 = CARTESIAN_POINT('Ctrl Pts',(8.48480454940901,6.55000000280808,-4.3736278088231)) ;
#105940 = CARTESIAN_POINT('Ctrl Pts',(8.54755771953121,6.61716872587346,-4.44713854387719)) ;
#105941 = CARTESIAN_POINT('Ctrl Pts',(8.53352383957147,6.54998388968238,-4.42700661491452)) ;
#105942 = CARTESIAN_POINT('Ctrl Pts',(8.49480263348501,6.55000000257396,-4.36671727629915)) ;
#105943 = CARTESIAN_POINT('Ctrl Pts',(8.5552440065103,6.59355301617591,-4.42648056989549)) ;
#105944 = CARTESIAN_POINT('Ctrl Pts',(8.53873552501329,6.54999036710749,-4.40129485880948)) ;
#105945 = CARTESIAN_POINT('Ctrl Pts',(8.51008526949052,6.55000000166752,-4.35677574941852)) ;
#105946 = CARTESIAN_POINT('Ctrl Pts',(8.55791451833571,6.58083494429015,-4.41842706746372)) ;
#105947 = CARTESIAN_POINT('Ctrl Pts',(8.54027978136633,6.54999344602542,-4.39157902883419)) ;
#105948 = CARTESIAN_POINT('Ctrl Pts',(8.51542462880457,6.55000000118004,-4.35380634433862)) ;
#105949 = CARTESIAN_POINT('Ctrl Pts',(8.5612242931934,6.5613575592924,-4.37541653896351)) ;
#105950 = CARTESIAN_POINT('Ctrl Pts',(8.54270214007071,6.54999771321876,-4.36209990564428)) ;
#105951 = CARTESIAN_POINT('Ctrl Pts',(8.52194436340204,6.55000000043436,-4.34726744367388)) ;
#105952 = CARTESIAN_POINT('Ctrl Pts',(8.56215003896755,6.55689889598543,-4.35255134475617)) ;
#105953 = CARTESIAN_POINT('Ctrl Pts',(8.54355112280983,6.54999862629018,-4.34858541402145)) ;
#105954 = CARTESIAN_POINT('Ctrl Pts',(8.52363168464777,6.55000000026381,-4.34419376079453)) ;
#105955 = CARTESIAN_POINT('Ctrl Pts',(8.56153943432815,6.55906352913392,-4.31720612379092)) ;
#105956 = CARTESIAN_POINT('Ctrl Pts',(8.54309854033142,6.5499981870035,-4.32716316826848)) ;
#105957 = CARTESIAN_POINT('Ctrl Pts',(8.52276767133745,6.5500000003466,-4.33816751318002)) ;
#105958 = CARTESIAN_POINT('Ctrl Pts',(8.5605912372004,6.56303220640811,-4.30548694646253)) ;
#105959 = CARTESIAN_POINT('Ctrl Pts',(8.54200379397877,6.54999736403672,-4.31947204706566)) ;
#105960 = CARTESIAN_POINT('Ctrl Pts',(8.52069177703238,6.55000000049844,-4.33552134373608)) ;
#105961 = CARTESIAN_POINT('Ctrl Pts',(8.5575081978017,6.5732178281489,-4.27880781453251)) ;
#105962 = CARTESIAN_POINT('Ctrl Pts',(8.53873610184731,6.54999517041881,-4.30052685964291)) ;
#105963 = CARTESIAN_POINT('Ctrl Pts',(8.5145479773404,6.55000000088831,-4.3286566308241)) ;
#105964 = CARTESIAN_POINT('Ctrl Pts',(8.55505442469281,6.57990173798307,-4.26929267446125)) ;
#105965 = CARTESIAN_POINT('Ctrl Pts',(8.53621107118181,6.54999365791211,-4.29217666040666)) ;
#105966 = CARTESIAN_POINT('Ctrl Pts',(8.50963525726155,6.5500000011443,-4.32482618291572)) ;
#105967 = CARTESIAN_POINT('Ctrl Pts',(8.55022399280471,6.59153973477783,-4.25293520591856)) ;
#105968 = CARTESIAN_POINT('Ctrl Pts',(8.53156015545166,6.54999086985382,-4.27662116717936)) ;
#105969 = CARTESIAN_POINT('Ctrl Pts',(8.49999539447557,6.55000000159032,-4.3171278236794)) ;
#105970 = CARTESIAN_POINT('Ctrl Pts',(8.54779538881607,6.59665349532936,-4.24691619169831)) ;
#105971 = CARTESIAN_POINT('Ctrl Pts',(8.52936575151138,6.54998957391998,-4.26999554735594)) ;
#105972 = CARTESIAN_POINT('Ctrl Pts',(8.49512741158075,6.55000000178643,-4.31333641589864)) ;
#105973 = CARTESIAN_POINT('Ctrl Pts',(8.54538355337154,6.60121171185025,-4.24167517448427)) ;
#105974 = CARTESIAN_POINT('Ctrl Pts',(8.52733415536169,6.54998837980796,-4.26389835720996)) ;
#105975 = CARTESIAN_POINT('Ctrl Pts',(8.49033880598513,6.55000000196131,-4.30944859709871)) ;
#105976 = CARTESIAN_POINT('',(8.54582344182383,6.61635369861666,-4.44606365157292)) ;
#105977 = CARTESIAN_POINT('Ctrl Pts',(8.54582344182383,6.61635369861666,-4.44606365157292)) ;
#105978 = CARTESIAN_POINT('Ctrl Pts',(8.5449359516352,6.61793460914653,-4.4473940762099)) ;
#105979 = CARTESIAN_POINT('Ctrl Pts',(8.54398448171071,6.61948114927953,-4.4487173928307)) ;
#105980 = CARTESIAN_POINT('Ctrl Pts',(8.54296332801272,6.6209780844369,-4.45004073677983)) ;
#105981 = CARTESIAN_POINT('Ctrl Pts',(8.53827263106763,6.62785429629763,-4.45611955276191)) ;
#105982 = CARTESIAN_POINT('Ctrl Pts',(8.53198779426187,6.63349037496299,-4.46261156852438)) ;
#105983 = CARTESIAN_POINT('Ctrl Pts',(8.5259873730411,6.63731070037229,-4.4700705892422)) ;
#105984 = CARTESIAN_POINT('Ctrl Pts',(8.52000560405467,6.64111915034781,-4.47750642368737)) ;
#105985 = CARTESIAN_POINT('Ctrl Pts',(8.51430181273566,6.64349626850742,-4.48603764730141)) ;
#105986 = CARTESIAN_POINT('Ctrl Pts',(8.50998586672548,6.64522349213896,-4.49520098697005)) ;
#105987 = CARTESIAN_POINT('Ctrl Pts',(8.50534188065424,6.64708199603772,-4.50506080025013)) ;
#105988 = CARTESIAN_POINT('Ctrl Pts',(8.50212992821339,6.64824261275105,-4.51588754367484)) ;
#105989 = CARTESIAN_POINT('Ctrl Pts',(8.50077314609738,6.64911992656046,-4.52682491191675)) ;
#105990 = CARTESIAN_POINT('Ctrl Pts',(8.50025986706873,6.64945181977648,-4.53096258566768)) ;
#105991 = CARTESIAN_POINT('Ctrl Pts',(8.50000017127793,6.64974165917873,-4.53514325510123)) ;
#105992 = CARTESIAN_POINT('Ctrl Pts',(8.5000000000847,6.64999974464545,-4.53931786749562)) ;
#105993 = CARTESIAN_POINT('',(8.55242393572496,6.60106172182542,-4.4332420987161)) ;
#105994 = CARTESIAN_POINT('Ctrl Pts',(8.55241775170035,6.60106807917176,-4.43323281615442)) ;
#105995 = CARTESIAN_POINT('Ctrl Pts',(8.55072388788562,6.60619026743357,-4.43772147695242)) ;
#105996 = CARTESIAN_POINT('Ctrl Pts',(8.54858294048571,6.61143812822772,-4.44192692414484)) ;
#105997 = CARTESIAN_POINT('Ctrl Pts',(8.54582344182383,6.61635369861666,-4.44606365157292)) ;
#105998 = CARTESIAN_POINT('Ctrl Pts',(8.55635360773813,6.58637108369506,-4.4186323907338)) ;
#105999 = CARTESIAN_POINT('Ctrl Pts',(8.55606387390183,6.58765239867385,-4.42011238280755)) ;
#106000 = CARTESIAN_POINT('Ctrl Pts',(8.55575324501781,6.58896823902363,-4.42156594133364)) ;
#106001 = CARTESIAN_POINT('Ctrl Pts',(8.55541196992767,6.5903724112751,-4.42304320494043)) ;
#106002 = CARTESIAN_POINT('Ctrl Pts',(8.55524290008378,6.59106804711319,-4.42377505069948)) ;
#106003 = CARTESIAN_POINT('Ctrl Pts',(8.5550663125072,6.59178496983024,-4.4245119588377)) ;
#106004 = CARTESIAN_POINT('Ctrl Pts',(8.55488049708426,6.59252693597571,-4.42525627761904)) ;
#106005 = CARTESIAN_POINT('Ctrl Pts',(8.55445908016385,6.59420966544518,-4.42694434270892)) ;
#106006 = CARTESIAN_POINT('Ctrl Pts',(8.55403589309457,6.5958403790653,-4.42848837772246)) ;
#106007 = CARTESIAN_POINT('Ctrl Pts',(8.55359592981647,6.59737680581848,-4.42990315623323)) ;
#106008 = CARTESIAN_POINT('Ctrl Pts',(8.55324292160435,6.59860957066092,-4.43103831559198)) ;
#106009 = CARTESIAN_POINT('Ctrl Pts',(8.55287861047124,6.59978201473819,-4.43209104250714)) ;
#106010 = CARTESIAN_POINT('Ctrl Pts',(8.55248933155915,6.60087815532546,-4.43307712698674)) ;
#106011 = CARTESIAN_POINT('Ctrl Pts',(8.55246754857565,6.6009394923555,-4.43313230557793)) ;
#106012 = CARTESIAN_POINT('Ctrl Pts',(8.5524457495603,6.60100068203151,-4.43318729627852)) ;
#106013 = CARTESIAN_POINT('Ctrl Pts',(8.55242393572496,6.60106172182542,-4.4332420987161)) ;
#106014 = CARTESIAN_POINT('Ctrl Pts',(8.5,6.66256607592813,-4.5397127088383)) ;
#106015 = CARTESIAN_POINT('Ctrl Pts',(8.5,6.66256607592813,-4.455)) ;
#106016 = CARTESIAN_POINT('Ctrl Pts',(8.58356010126947,6.66256607592813,-4.44107331645509)) ;
#106017 = CARTESIAN_POINT('Ctrl Pts',(8.5,6.6101130271982,-4.53971270726282)) ;
#106018 = CARTESIAN_POINT('Ctrl Pts',(8.5,6.63245216822986,-4.4585572365994)) ;
#106019 = CARTESIAN_POINT('Ctrl Pts',(8.5794176004298,6.63563981885127,-4.4417637332617)) ;
#106020 = CARTESIAN_POINT('Ctrl Pts',(8.5,6.55934573373329,-4.51884690994274)) ;
#106021 = CARTESIAN_POINT('Ctrl Pts',(8.5,6.60054351783565,-4.44808139582774)) ;
#106022 = CARTESIAN_POINT('Ctrl Pts',(8.57705842698408,6.60987578993432,-4.43172752804771)) ;
#106023 = CARTESIAN_POINT('Ctrl Pts',(8.5,6.52274941072028,-4.48225058927972)) ;
#106024 = CARTESIAN_POINT('Ctrl Pts',(8.5,6.57873105977929,-4.42626894022071)) ;
#106025 = CARTESIAN_POINT('Ctrl Pts',(8.57705842661295,6.59157413088145,-4.41342586911855)) ;
#106026 = CARTESIAN_POINT('Origin',(8.49172374697003,1.4,-7.62)) ;
#106027 = CARTESIAN_POINT('Origin',(8.49172374697003,1.4,-3.11785831296514)) ;
#106028 = CARTESIAN_POINT('Origin',(8.49172374697002,1.4,-3.11785831296514)) ;
#106029 = CARTESIAN_POINT('Origin',(8.49172374697003,1.4,-3.11785831296514)) ;
#106030 = CARTESIAN_POINT('Ctrl Pts',(8.50816364570057,1.49863939238321,-3.11785831296512)) ;
#106031 = CARTESIAN_POINT('Ctrl Pts',(8.51019246767907,1.4983012553868,-3.15292758407099)) ;
#106032 = CARTESIAN_POINT('Ctrl Pts',(8.50816364570057,1.47636598119991,-3.18029201095831)) ;
#106033 = CARTESIAN_POINT('Ctrl Pts',(8.97755831131119,1.42040694811478,-3.08994865115312)) ;
#106034 = CARTESIAN_POINT('Ctrl Pts',(8.97879997398671,1.42020000433583,-3.12456667318282)) ;
#106035 = CARTESIAN_POINT('Ctrl Pts',(8.97755831689154,1.39869563385789,-3.15169481695074)) ;
#106036 = CARTESIAN_POINT('Ctrl Pts',(9.44698496305969,1.34216917282336,-3.06263137063073)) ;
#106037 = CARTESIAN_POINT('Ctrl Pts',(9.44827639615875,1.34195393397299,-3.0967775286091)) ;
#106038 = CARTESIAN_POINT('Ctrl Pts',(9.44698496887878,1.3209776491576,-3.12372298471085)) ;
#106039 = CARTESIAN_POINT('Ctrl Pts',(9.91643989873053,1.26392668354489,-3.03583811982177)) ;
#106040 = CARTESIAN_POINT('Ctrl Pts',(9.91830968165731,1.26361505305709,-3.06950934419701)) ;
#106041 = CARTESIAN_POINT('Ctrl Pts',(9.91643989873053,1.24322097942674,-3.09630356419402)) ;
#106042 = CARTESIAN_POINT('Origin',(9.9,1.16528729116168,-3.0358381198218)) ;
#106043 = CARTESIAN_POINT('Origin',(9.9,1.16528729116168,-3.0358381198218)) ;
#106044 = CARTESIAN_POINT('Origin',(-0.4,-3.36847777691809,-5.48)) ;
#106045 = CARTESIAN_POINT('Origin',(-0.400000000000001,-3.36847777691809,
-5.48)) ;
#106046 = CARTESIAN_POINT('Origin',(-0.4,-3.36847777691809,-5.48)) ;
#106047 = CARTESIAN_POINT('Origin',(-0.400000000000001,-3.36847777691809,
-4.58)) ;
#106048 = CARTESIAN_POINT('Origin',(-0.4,-3.36847777691809,-4.68)) ;
#106049 = CARTESIAN_POINT('Origin',(-1.11032778078669,-3.36847777691809,-5.48)) ;
#106050 = CARTESIAN_POINT('Origin',(0.4,-3.36847777691809,-5.48)) ;
#106051 = CARTESIAN_POINT('Origin',(-0.400000000000001,-3.36847777691809,
-4.68)) ;
#106052 = CARTESIAN_POINT('Origin',(-0.4,-3.36847777691809,-4.68)) ;
#106053 = CARTESIAN_POINT('Origin',(0.400000000000001,-3.36847777691809,-5.48)) ;
#106054 = CARTESIAN_POINT('Origin',(0.400000000000001,-3.36847777691809,-5.48)) ;
#106055 = CARTESIAN_POINT('Origin',(1.5,-3.36847777691809,-4.68)) ;
#106056 = CARTESIAN_POINT('Origin',(0.4,-3.36847777691809,-4.68)) ;
#106057 = CARTESIAN_POINT('Origin',(0.4,-3.36847777691809,-4.58)) ;
#106058 = CARTESIAN_POINT('Origin',(0.4,-3.36847777691809,-4.68)) ;
#106059 = CARTESIAN_POINT('Origin',(0.4,-3.36847777691809,-4.68)) ;
#106060 = CARTESIAN_POINT('Origin',(7.96847777691809,3.4,-5.48)) ;
#106061 = CARTESIAN_POINT('Origin',(7.96847777691809,3.4,-5.48)) ;
#106062 = CARTESIAN_POINT('Origin',(7.96847777691809,3.4,-5.48)) ;
#106063 = CARTESIAN_POINT('Origin',(7.96847777691809,3.4,-4.58)) ;
#106064 = CARTESIAN_POINT('Origin',(7.96847777691809,3.4,-4.68)) ;
#106065 = CARTESIAN_POINT('Origin',(7.96847777691809,2.68967221921331,-5.48)) ;
#106066 = CARTESIAN_POINT('Origin',(7.96847777691809,4.2,-5.48)) ;
#106067 = CARTESIAN_POINT('Origin',(7.96847777691809,3.4,-4.68)) ;
#106068 = CARTESIAN_POINT('Origin',(7.96847777691809,3.4,-4.68)) ;
#106069 = CARTESIAN_POINT('Origin',(7.96847777691809,4.2,-5.48)) ;
#106070 = CARTESIAN_POINT('Origin',(7.96847777691809,4.2,-5.48)) ;
#106071 = CARTESIAN_POINT('Origin',(7.96847777691809,2.3,-4.68)) ;
#106072 = CARTESIAN_POINT('Origin',(7.96847777691809,4.2,-4.68)) ;
#106073 = CARTESIAN_POINT('Origin',(7.96847777691809,4.2,-4.58)) ;
#106074 = CARTESIAN_POINT('Origin',(7.96847777691809,4.2,-4.68)) ;
#106075 = CARTESIAN_POINT('Origin',(7.96847777691809,4.2,-4.68)) ;
#106076 = CARTESIAN_POINT('Origin',(8.49172374697003,1.4,-7.62)) ;
#106077 = CARTESIAN_POINT('Origin',(8.49172374697003,1.4,-7.04214168703487)) ;
#106078 = CARTESIAN_POINT('Origin',(8.49172374697002,1.4,-7.04214168703487)) ;
#106079 = CARTESIAN_POINT('Origin',(8.49172374697003,1.39999999999989,-7.04214168703472)) ;
#106080 = CARTESIAN_POINT('Ctrl Pts',(8.50816364570058,1.47636598119991,-6.97970798904169)) ;
#106081 = CARTESIAN_POINT('Ctrl Pts',(8.51019246767908,1.4983012553868,-7.00707241592901)) ;
#106082 = CARTESIAN_POINT('Ctrl Pts',(8.50816364570058,1.49863939238321,-7.04214168703488)) ;
#106083 = CARTESIAN_POINT('Ctrl Pts',(8.97755831689153,1.39869563385779,-7.00830518304914)) ;
#106084 = CARTESIAN_POINT('Ctrl Pts',(8.97879997398671,1.42020000433583,-7.03543332681677)) ;
#106085 = CARTESIAN_POINT('Ctrl Pts',(8.97755831131121,1.42040694811478,-7.07005134884647)) ;
#106086 = CARTESIAN_POINT('Ctrl Pts',(9.44698496887879,1.32097764915769,-7.03627701528927)) ;
#106087 = CARTESIAN_POINT('Ctrl Pts',(9.44827639615876,1.34195393397361,-7.063222471393)) ;
#106088 = CARTESIAN_POINT('Ctrl Pts',(9.44698496305971,1.34216917282336,-7.09736862936899)) ;
#106089 = CARTESIAN_POINT('Ctrl Pts',(9.91643989873053,1.24322097942674,-7.06369643580598)) ;
#106090 = CARTESIAN_POINT('Ctrl Pts',(9.91830968165732,1.26361505305709,-7.09049065580299)) ;
#106091 = CARTESIAN_POINT('Ctrl Pts',(9.91643989873053,1.26392668354489,-7.12416188017823)) ;
#106092 = CARTESIAN_POINT('Origin',(9.9,1.16528729116168,-7.1241618801782)) ;
#106093 = CARTESIAN_POINT('Origin',(9.9,1.16528729116168,-7.12416188017819)) ;
#106094 = CARTESIAN_POINT('Origin',(8.48377223398316,8.2,-7.62)) ;
#106095 = CARTESIAN_POINT('Origin',(8.48238054865791,8.20007133344167,-4.3331789312541)) ;
#106096 = CARTESIAN_POINT('Ctrl Pts',(8.40201662970151,8.3,-4.56597597792137)) ;
#106097 = CARTESIAN_POINT('Ctrl Pts',(8.50299337454953,8.3,-4.55267481126356)) ;
#106098 = CARTESIAN_POINT('Ctrl Pts',(8.50100123624933,8.19773961376458,-4.55268884611771)) ;
#106099 = CARTESIAN_POINT('Ctrl Pts',(8.39454129798956,8.3,-4.51449818135068)) ;
#106100 = CARTESIAN_POINT('Ctrl Pts',(8.4969787523767,8.3,-4.52537411133468)) ;
#106101 = CARTESIAN_POINT('Ctrl Pts',(8.49727262260754,8.20135231978537,-4.52506706396232)) ;
#106102 = CARTESIAN_POINT('Ctrl Pts',(8.40820218948348,8.3,-4.46202536352427)) ;
#106103 = CARTESIAN_POINT('Ctrl Pts',(8.49818669687006,8.3,-4.50247172780123)) ;
#106104 = CARTESIAN_POINT('Ctrl Pts',(8.50412619268406,8.20300739730712,-4.50038841002479)) ;
#106105 = CARTESIAN_POINT('Ctrl Pts',(8.4430413476632,8.3,-4.41099693308713)) ;
#106106 = CARTESIAN_POINT('Ctrl Pts',(8.50894174387208,8.3,-4.46085505538057)) ;
#106107 = CARTESIAN_POINT('Ctrl Pts',(8.52157716465941,8.21896555381606,-4.47016612665034)) ;
#106108 = CARTESIAN_POINT('Ctrl Pts',(8.44963266995283,8.3,-4.40266783197822)) ;
#106109 = CARTESIAN_POINT('Ctrl Pts',(8.51095981317517,8.3,-4.45374944048349)) ;
#106110 = CARTESIAN_POINT('Ctrl Pts',(8.52487915500778,8.22226238914488,-4.46495161805187)) ;
#106111 = CARTESIAN_POINT('Ctrl Pts',(8.46372306360152,8.3,-4.38695472631993)) ;
#106112 = CARTESIAN_POINT('Ctrl Pts',(8.51547368264943,8.3,-4.43763279105593)) ;
#106113 = CARTESIAN_POINT('Ctrl Pts',(8.53193863144478,8.23129792829966,-4.45331747838552)) ;
#106114 = CARTESIAN_POINT('Ctrl Pts',(8.47128983770084,8.3,-4.37955862714639)) ;
#106115 = CARTESIAN_POINT('Ctrl Pts',(8.51796237042372,8.3,-4.42924649491277)) ;
#106116 = CARTESIAN_POINT('Ctrl Pts',(8.53572833262714,8.23677343862356,-4.44742958850775)) ;
#106117 = CARTESIAN_POINT('Ctrl Pts',(8.48287565264706,8.3,-4.36873079483316)) ;
#106118 = CARTESIAN_POINT('Ctrl Pts',(8.52168214469874,8.3,-4.41074351942997)) ;
#106119 = CARTESIAN_POINT('Ctrl Pts',(8.54153766811345,8.25077321967989,-4.43204498710732)) ;
#106120 = CARTESIAN_POINT('Ctrl Pts',(8.48680760428677,8.3,-4.365187297402)) ;
#106121 = CARTESIAN_POINT('Ctrl Pts',(8.52287759291297,8.3,-4.40414350493168)) ;
#106122 = CARTESIAN_POINT('Ctrl Pts',(8.54350322705384,8.25646917637541,-4.42626226660343)) ;
#106123 = CARTESIAN_POINT('Ctrl Pts',(8.49230810302881,8.3,-4.35949534999551)) ;
#106124 = CARTESIAN_POINT('Ctrl Pts',(8.52426411271137,8.3,-4.38856652463359)) ;
#106125 = CARTESIAN_POINT('Ctrl Pts',(8.54627296401923,8.26866384868897,-4.40855256936158)) ;
#106126 = CARTESIAN_POINT('Ctrl Pts',(8.49410170711667,8.3,-4.357526518934)) ;
#106127 = CARTESIAN_POINT('Ctrl Pts',(8.52463604790914,8.3,-4.38240552536515)) ;
#106128 = CARTESIAN_POINT('Ctrl Pts',(8.54716490137964,8.27360757863442,-4.40079595948255)) ;
#106129 = CARTESIAN_POINT('Ctrl Pts',(8.49698869685298,8.3,-4.35307327880953)) ;
#106130 = CARTESIAN_POINT('Ctrl Pts',(8.5252311891155,8.3,-4.36659293443832)) ;
#106131 = CARTESIAN_POINT('Ctrl Pts',(8.54862931231183,8.28262305001771,-4.37784134927042)) ;
#106132 = CARTESIAN_POINT('Ctrl Pts',(8.49798687771249,8.3,-4.35051652115659)) ;
#106133 = CARTESIAN_POINT('Ctrl Pts',(8.52551930315387,8.3,-4.3569062760438)) ;
#106134 = CARTESIAN_POINT('Ctrl Pts',(8.54912969489065,8.28574379441723,-4.36238189749325)) ;
#106135 = CARTESIAN_POINT('Ctrl Pts',(8.49821791151748,8.3,-4.34257957093737)) ;
#106136 = CARTESIAN_POINT('Ctrl Pts',(8.52559423327562,8.3,-4.33218912470485)) ;
#106137 = CARTESIAN_POINT('Ctrl Pts',(8.54922875625408,8.28635135062007,-4.32323867004689)) ;
#106138 = CARTESIAN_POINT('Ctrl Pts',(8.49537847603514,8.3,-4.33764691084577)) ;
#106139 = CARTESIAN_POINT('Ctrl Pts',(8.5243933105344,8.3,-4.32147327498212)) ;
#106140 = CARTESIAN_POINT('Ctrl Pts',(8.54781890418529,8.28040548672881,-4.30847179337202)) ;
#106141 = CARTESIAN_POINT('Ctrl Pts',(8.48955273785442,8.3,-4.32891140345694)) ;
#106142 = CARTESIAN_POINT('Ctrl Pts',(8.52168703568126,8.3,-4.30405258512816)) ;
#106143 = CARTESIAN_POINT('Ctrl Pts',(8.54489815533715,8.27194212599122,-4.28616700770705)) ;
#106144 = CARTESIAN_POINT('Ctrl Pts',(8.4862007719736,8.3,-4.32482630750477)) ;
#106145 = CARTESIAN_POINT('Ctrl Pts',(8.52012703453234,8.3,-4.29710733289327)) ;
#106146 = CARTESIAN_POINT('Ctrl Pts',(8.54324008387893,8.26788967346965,-4.27831423563835)) ;
#106147 = CARTESIAN_POINT('Ctrl Pts',(8.48280151347419,8.3,-4.32079110964071)) ;
#106148 = CARTESIAN_POINT('Ctrl Pts',(8.51858761497411,8.3,-4.2906520257852)) ;
#106149 = CARTESIAN_POINT('Ctrl Pts',(8.54152015125555,8.26408224232383,-4.27133822503473)) ;
#106150 = CARTESIAN_POINT('Origin',(8.4,8.2,-4.53792711014902)) ;
#106151 = CARTESIAN_POINT('Origin',(8.4,8.2,-5.705)) ;
#106152 = CARTESIAN_POINT('Origin',(8.4,8.2,-5.62207288985098)) ;
#106153 = CARTESIAN_POINT('Ctrl Pts',(8.50101530037395,8.19768718256759,-5.60720177458148)) ;
#106154 = CARTESIAN_POINT('Ctrl Pts',(8.50305639000875,8.3,-5.60721981135723)) ;
#106155 = CARTESIAN_POINT('Ctrl Pts',(8.40204633857705,8.3,-5.59382020212539)) ;
#106156 = CARTESIAN_POINT('Ctrl Pts',(8.49725464441629,8.20131038948434,-5.63486791190954)) ;
#106157 = CARTESIAN_POINT('Ctrl Pts',(8.49701391805276,8.3,-5.63456094234022)) ;
#106158 = CARTESIAN_POINT('Ctrl Pts',(8.39450526457597,8.3,-5.645363291071)) ;
#106159 = CARTESIAN_POINT('Ctrl Pts',(8.50410935041313,8.20295267265876,-5.65957929681148)) ;
#106160 = CARTESIAN_POINT('Ctrl Pts',(8.49820749521502,8.3,-5.65746433789065)) ;
#106161 = CARTESIAN_POINT('Ctrl Pts',(8.40816401923481,8.3,-5.69791872904343)) ;
#106162 = CARTESIAN_POINT('Ctrl Pts',(8.52158236570989,8.21893216789648,-5.68983004077579)) ;
#106163 = CARTESIAN_POINT('Ctrl Pts',(8.50896456566523,8.3,-5.69912767838404)) ;
#106164 = CARTESIAN_POINT('Ctrl Pts',(8.44304134766321,8.3,-5.74900306691287)) ;
#106165 = CARTESIAN_POINT('Ctrl Pts',(8.5248849650705,8.22222991631198,-5.69504370617815)) ;
#106166 = CARTESIAN_POINT('Ctrl Pts',(8.51098076140209,8.3,-5.70623311097626)) ;
#106167 = CARTESIAN_POINT('Ctrl Pts',(8.44963266995283,8.3,-5.75733216802178)) ;
#106168 = CARTESIAN_POINT('Ctrl Pts',(8.53194575580939,8.23126818558571,-5.70667573496657)) ;
#106169 = CARTESIAN_POINT('Ctrl Pts',(8.51549074202139,8.3,-5.7223505031351)) ;
#106170 = CARTESIAN_POINT('Ctrl Pts',(8.46372306360152,8.3,-5.77304527368007)) ;
#106171 = CARTESIAN_POINT('Ctrl Pts',(8.53573618291038,8.23674548871784,-5.71256237702727)) ;
#106172 = CARTESIAN_POINT('Ctrl Pts',(8.51797743940286,8.3,-5.73073746255862)) ;
#106173 = CARTESIAN_POINT('Ctrl Pts',(8.47128983770083,8.3,-5.78044137285362)) ;
#106174 = CARTESIAN_POINT('Ctrl Pts',(8.54154687836689,8.25075037830459,-5.72794513194553)) ;
#106175 = CARTESIAN_POINT('Ctrl Pts',(8.52169408444525,8.3,-5.74924355434931)) ;
#106176 = CARTESIAN_POINT('Ctrl Pts',(8.48287565264707,8.3,-5.79126920516684)) ;
#106177 = CARTESIAN_POINT('Ctrl Pts',(8.54351297666182,8.25644859419425,-5.73372727801621)) ;
#106178 = CARTESIAN_POINT('Ctrl Pts',(8.52288848488738,8.3,-5.75584473154881)) ;
#106179 = CARTESIAN_POINT('Ctrl Pts',(8.48680760428677,8.3,-5.79481270259799)) ;
#106180 = CARTESIAN_POINT('Ctrl Pts',(8.54628376412585,8.26864846827403,-5.75143762316011)) ;
#106181 = CARTESIAN_POINT('Ctrl Pts',(8.52427341038692,8.3,-5.77142501704035)) ;
#106182 = CARTESIAN_POINT('Ctrl Pts',(8.49230810302881,8.3,-5.80050465000449)) ;
#106183 = CARTESIAN_POINT('Ctrl Pts',(8.54717611873858,8.2735944350094,-5.75919488371877)) ;
#106184 = CARTESIAN_POINT('Ctrl Pts',(8.52464480444821,8.3,-5.77758733991419)) ;
#106185 = CARTESIAN_POINT('Ctrl Pts',(8.49410170711667,8.3,-5.802473481066)) ;
#106186 = CARTESIAN_POINT('Ctrl Pts',(8.54864126180655,8.28261417405722,-5.78215290612485)) ;
#106187 = CARTESIAN_POINT('Ctrl Pts',(8.52523908688554,8.3,-5.7934032849063)) ;
#106188 = CARTESIAN_POINT('Ctrl Pts',(8.49698869685298,8.3,-5.80692672119047)) ;
#106189 = CARTESIAN_POINT('Ctrl Pts',(8.54914185487161,8.28573645090424,-5.79761528241614)) ;
#106190 = CARTESIAN_POINT('Ctrl Pts',(8.52552693815804,8.3,-5.80309195201625)) ;
#106191 = CARTESIAN_POINT('Ctrl Pts',(8.49798687771249,8.3,-5.80948347884342)) ;
#106192 = CARTESIAN_POINT('Ctrl Pts',(8.54924094958849,8.28634430798884,-5.8367659475985)) ;
#106193 = CARTESIAN_POINT('Ctrl Pts',(8.5256018120494,8.3,-5.82781375175316)) ;
#106194 = CARTESIAN_POINT('Ctrl Pts',(8.49821791151748,8.3,-5.81742042906263)) ;
#106195 = CARTESIAN_POINT('Ctrl Pts',(8.54783079466744,8.28039553911293,-5.85153480598126)) ;
#106196 = CARTESIAN_POINT('Ctrl Pts',(8.52440147378977,8.3,-5.83853127543226)) ;
#106197 = CARTESIAN_POINT('Ctrl Pts',(8.49537847603514,8.3,-5.82235308915424)) ;
#106198 = CARTESIAN_POINT('Ctrl Pts',(8.54465883986932,8.27120119512635,-5.87575719470323)) ;
#106199 = CARTESIAN_POINT('Ctrl Pts',(8.52145785975948,8.3,-5.85749027833005)) ;
#106200 = CARTESIAN_POINT('Ctrl Pts',(8.48905244827037,8.3,-5.83183876471446)) ;
#106201 = CARTESIAN_POINT('Ctrl Pts',(8.54267599402787,8.26648669506702,-5.88429499043038)) ;
#106202 = CARTESIAN_POINT('Ctrl Pts',(8.51958784692424,8.3,-5.86526413214463)) ;
#106203 = CARTESIAN_POINT('Ctrl Pts',(8.48503640902806,8.3,-5.83656859706595)) ;
#106204 = CARTESIAN_POINT('Ctrl Pts',(8.54064021294344,8.26212437554838,-5.89220002982386)) ;
#106205 = CARTESIAN_POINT('Ctrl Pts',(8.51779796763702,8.3,-5.87268951701513)) ;
#106206 = CARTESIAN_POINT('Ctrl Pts',(8.48104783026778,8.3,-5.84128480749502)) ;
#106207 = CARTESIAN_POINT('Origin',(8.48238054717179,8.20007132587459,-5.82682106738604)) ;
#106208 = CARTESIAN_POINT('Origin',(8.48377223398316,8.2,-7.62)) ;
#106209 = CARTESIAN_POINT('Ctrl Pts',(8.55305389383868,6.58518362856711,-9.49981637143289)) ;
#106210 = CARTESIAN_POINT('Ctrl Pts',(8.56447181517253,6.58947636230805,-9.49552363769195)) ;
#106211 = CARTESIAN_POINT('Ctrl Pts',(8.57705842661295,6.59157413088145,-9.49342586911855)) ;
#106212 = CARTESIAN_POINT('Ctrl Pts',(8.553051025152,6.55898702014118,-9.47362045977747)) ;
#106213 = CARTESIAN_POINT('Ctrl Pts',(8.56446969712854,6.56479854221785,-9.47084652309117)) ;
#106214 = CARTESIAN_POINT('Ctrl Pts',(8.5770584270977,6.56766897765924,-9.46952071573475)) ;
#106215 = CARTESIAN_POINT('Ctrl Pts',(8.55608440539074,6.54967077654143,-9.43347242603467)) ;
#106216 = CARTESIAN_POINT('Ctrl Pts',(8.56803673427363,6.55578248257735,-9.43313112423485)) ;
#106217 = CARTESIAN_POINT('Ctrl Pts',(8.58110225049763,6.55837193275,-9.43326484665045)) ;
#106218 = CARTESIAN_POINT('Ctrl Pts',(8.56106007075017,6.56033186051355,-9.3969784615962)) ;
#106219 = CARTESIAN_POINT('Ctrl Pts',(8.57385418571953,6.56560017282096,-9.39820388376167)) ;
#106220 = CARTESIAN_POINT('Ctrl Pts',(8.58763814880121,6.56727264871055,-9.39859290569255)) ;
#106221 = CARTESIAN_POINT('',(8.56104219912065,6.56017369985344,-9.39763385094441)) ;
#106222 = CARTESIAN_POINT('',(8.55704445183394,6.5832097329571,-9.49483164119209)) ;
#106223 = CARTESIAN_POINT('Ctrl Pts',(8.56104219912065,6.56017369985344,-9.39763385094441)) ;
#106224 = CARTESIAN_POINT('Ctrl Pts',(8.56172006948825,6.55755272988493,-9.41050998342623)) ;
#106225 = CARTESIAN_POINT('Ctrl Pts',(8.56178854742204,6.55691761311389,-9.42401886345913)) ;
#106226 = CARTESIAN_POINT('Ctrl Pts',(8.56147572200372,6.55855061087387,-9.43707103715452)) ;
#106227 = CARTESIAN_POINT('Ctrl Pts',(8.56116227470662,6.56018685493861,-9.45014915781355)) ;
#106228 = CARTESIAN_POINT('Ctrl Pts',(8.5604843297899,6.56417103596015,-9.4631290791339)) ;
#106229 = CARTESIAN_POINT('Ctrl Pts',(8.55945615587251,6.57017322470283,-9.47482221269648)) ;
#106230 = CARTESIAN_POINT('Ctrl Pts',(8.55883284154061,6.5738119576086,-9.48191099175524)) ;
#106231 = CARTESIAN_POINT('Ctrl Pts',(8.5580718554171,6.57823677723143,-9.48863504839527)) ;
#106232 = CARTESIAN_POINT('Ctrl Pts',(8.55704487707427,6.58320791316498,-9.49483246211941)) ;
#106233 = CARTESIAN_POINT('',(8.55635403291171,6.58636921675996,-9.4986302321744)) ;
#106234 = CARTESIAN_POINT('Origin',(8.5442029138841,6.62817326403372,-9.46194115684657)) ;
#106235 = CARTESIAN_POINT('',(8.57705842661295,6.59157413088145,-9.49342586911855)) ;
#106236 = CARTESIAN_POINT('Origin',(8.6,6.52274941072028,-9.56225058927972)) ;
#106237 = CARTESIAN_POINT('',(8.58355189313841,6.56397635572685,-9.422433776426)) ;
#106238 = CARTESIAN_POINT('Origin',(8.59777129281774,6.65641294722022,-9.42088223593215)) ;
#106239 = CARTESIAN_POINT('Ctrl Pts',(8.56104311409705,6.56017375480331,-9.3976348093723)) ;
#106240 = CARTESIAN_POINT('Ctrl Pts',(8.56569547918967,6.5609490208508,-9.40312238616949)) ;
#106241 = CARTESIAN_POINT('Ctrl Pts',(8.57049938306336,6.56176641478979,-9.40850925134749)) ;
#106242 = CARTESIAN_POINT('Ctrl Pts',(8.5753889310572,6.56259599225629,-9.41378626613857)) ;
#106243 = CARTESIAN_POINT('Ctrl Pts',(8.57808773793837,6.56305388107911,-9.41669893697199)) ;
#106244 = CARTESIAN_POINT('Ctrl Pts',(8.58081254036868,6.5635152101042,-9.41957937936769)) ;
#106245 = CARTESIAN_POINT('Ctrl Pts',(8.58355195315299,6.56397636517832,-9.4224336197205)) ;
#106246 = CARTESIAN_POINT('Ctrl Pts',(8.5,8.35216169217141,-9.51240609825021)) ;
#106247 = CARTESIAN_POINT('Ctrl Pts',(8.5,8.2900428850829,-9.48134669470595)) ;
#106248 = CARTESIAN_POINT('Ctrl Pts',(8.56507848521152,8.26835005667906,-9.47050028050403)) ;
#106249 = CARTESIAN_POINT('Ctrl Pts',(8.5,8.31945293993511,-9.57782359726851)) ;
#106250 = CARTESIAN_POINT('Ctrl Pts',(8.5,8.2692201349117,-9.52299218879621)) ;
#106251 = CARTESIAN_POINT('Ctrl Pts',(8.56507848601002,8.25199117628906,-9.50321804061861)) ;
#106252 = CARTESIAN_POINT('Ctrl Pts',(8.5,8.24922766844411,-9.61971270685141)) ;
#106253 = CARTESIAN_POINT('Ctrl Pts',(8.5,8.21777561643101,-9.54447736982289)) ;
#106254 = CARTESIAN_POINT('Ctrl Pts',(8.57228151929421,8.21451202732351,-9.52295308011763)) ;
#106255 = CARTESIAN_POINT('Ctrl Pts',(8.5,8.17221734381475,-9.61971270883831)) ;
#106256 = CARTESIAN_POINT('Ctrl Pts',(8.5,8.17221734381475,-9.535)) ;
#106257 = CARTESIAN_POINT('Ctrl Pts',(8.58356010126947,8.17221734381475,-9.52107331645509)) ;
#106258 = CARTESIAN_POINT('',(8.50000000249538,8.20000280433619,-9.61790474363843)) ;
#106259 = CARTESIAN_POINT('',(8.54742025481395,8.27608084305204,-9.47436566195595)) ;
#106260 = CARTESIAN_POINT('Ctrl Pts',(8.50000000249538,8.20000280433619,-9.61790474363843)) ;
#106261 = CARTESIAN_POINT('Ctrl Pts',(8.50000274011724,8.20154143765779,-9.60563544845108)) ;
#106262 = CARTESIAN_POINT('Ctrl Pts',(8.50225788919788,8.20358050335012,-9.59326647497958)) ;
#106263 = CARTESIAN_POINT('Ctrl Pts',(8.50614710304112,8.20657022673326,-9.58191598101389)) ;
#106264 = CARTESIAN_POINT('Ctrl Pts',(8.51002595055128,8.20955198129041,-9.57059574072047)) ;
#106265 = CARTESIAN_POINT('Ctrl Pts',(8.51564213392183,8.21362262975068,-9.56004613352066)) ;
#106266 = CARTESIAN_POINT('Ctrl Pts',(8.52129493663065,8.21921832196825,-9.55062179223395)) ;
#106267 = CARTESIAN_POINT('Ctrl Pts',(8.52933132065201,8.22717351408127,-9.53722354898551)) ;
#106268 = CARTESIAN_POINT('Ctrl Pts',(8.53683691159804,8.23885362788864,-9.52566244344335)) ;
#106269 = CARTESIAN_POINT('Ctrl Pts',(8.54097226482464,8.25011947738646,-9.51288116961709)) ;
#106270 = CARTESIAN_POINT('Ctrl Pts',(8.54447125915462,8.25965170869904,-9.50206671140824)) ;
#106271 = CARTESIAN_POINT('Ctrl Pts',(8.54617119150717,8.26873789958222,-9.48993961018965)) ;
#106272 = CARTESIAN_POINT('Ctrl Pts',(8.54724932284106,8.27506683274844,-9.47656646025131)) ;
#106273 = CARTESIAN_POINT('Ctrl Pts',(8.54730817192851,8.27541229338911,-9.47583649568633)) ;
#106274 = CARTESIAN_POINT('Ctrl Pts',(8.5473651061662,8.27575037116516,-9.47510283260602)) ;
#106275 = CARTESIAN_POINT('Ctrl Pts',(8.54742024083733,8.27608084608571,-9.47436567520734)) ;
#106276 = CARTESIAN_POINT('',(8.56507848521152,8.26835005667905,-9.47050028050403)) ;
#106277 = CARTESIAN_POINT('Origin',(8.6,8.3521616921714,-9.51240609825021)) ;
#106278 = CARTESIAN_POINT('',(8.58356010126947,8.17221734381475,-9.52107331645509)) ;
#106279 = CARTESIAN_POINT('Origin',(8.59670327708553,8.16883734299696,-9.42706896951949)) ;
#106280 = CARTESIAN_POINT('',(8.5,8.17221734381475,-9.61971270883831)) ;
#106281 = CARTESIAN_POINT('Origin',(8.6,8.17221734381475,-9.61971270883831)) ;
#106282 = CARTESIAN_POINT('Origin',(8.5,8.16642648793215,-9.39710775449589)) ;
#106283 = CARTESIAN_POINT('Origin',(2.9,3.8,-10.16)) ;
#106284 = CARTESIAN_POINT('',(3.,2.4,-10.16)) ;
#106285 = CARTESIAN_POINT('Origin',(3.,3.8,-10.16)) ;
#106286 = CARTESIAN_POINT('',(2.9,2.3,-10.16)) ;
#106287 = CARTESIAN_POINT('Origin',(2.9,2.4,-10.16)) ;
#106288 = CARTESIAN_POINT('Origin',(2.9,3.8,-10.16)) ;
#106289 = CARTESIAN_POINT('Origin',(1.35,3.8,-10.16)) ;
#106290 = CARTESIAN_POINT('',(1.35,2.3,-10.16)) ;
#106291 = CARTESIAN_POINT('Origin',(1.35,3.8,-10.16)) ;
#106292 = CARTESIAN_POINT('',(1.25,2.2,-10.16)) ;
#106293 = CARTESIAN_POINT('Origin',(1.35,2.2,-10.16)) ;
#106294 = CARTESIAN_POINT('Origin',(1.25,3.8,-10.16)) ;
#106295 = CARTESIAN_POINT('Origin',(13.9153543900904,1.02736587339764,-9.31)) ;
#106296 = CARTESIAN_POINT('',(1.15,1.02736587339764,-9.41)) ;
#106297 = CARTESIAN_POINT('',(1.15,0.931757800066529,-9.28068965517241)) ;
#106298 = CARTESIAN_POINT('Origin',(1.15,1.02736587339764,-9.31)) ;
#106299 = CARTESIAN_POINT('',(-0.900000000000002,1.02736587339765,-9.41)) ;
#106300 = CARTESIAN_POINT('',(-1.,1.02736587339765,-9.41)) ;
#106301 = CARTESIAN_POINT('',(-0.900000000000002,0.982644513847654,-9.39944271909999)) ;
#106302 = CARTESIAN_POINT('Origin',(-0.900000000000002,1.02736587339765,-9.31)) ;
#106303 = CARTESIAN_POINT('',(-0.900000000000002,0.93175780006653,-9.28068965517241)) ;
#106304 = CARTESIAN_POINT('Origin',(-0.900000000000002,1.02736587339765,-9.31)) ;
#106305 = CARTESIAN_POINT('',(13.9153543900904,0.931757800066525,-9.28068965517241)) ;
#106306 = CARTESIAN_POINT('Origin',(13.9153543900904,1.02736587339764,-11.01)) ;
#106307 = CARTESIAN_POINT('',(1.15,0.93175780006653,-11.0393103448276)) ;
#106308 = CARTESIAN_POINT('',(1.15,1.02736587339765,-10.91)) ;
#106309 = CARTESIAN_POINT('Origin',(1.15,1.02736587339765,-11.01)) ;
#106310 = CARTESIAN_POINT('',(-0.900000000000002,0.931757800066531,-11.0393103448276)) ;
#106311 = CARTESIAN_POINT('',(13.9153543900904,0.931757800066525,-11.0393103448276)) ;
#106312 = CARTESIAN_POINT('',(-0.900000000000002,1.02736587339765,-10.91)) ;
#106313 = CARTESIAN_POINT('Origin',(-0.900000000000002,1.02736587339765,-11.01)) ;
#106314 = CARTESIAN_POINT('',(-1.,1.02736587339765,-10.91)) ;
#106315 = CARTESIAN_POINT('Origin',(8.49172374697003,3.8,-10.16)) ;
#106316 = CARTESIAN_POINT('',(8.49172374697003,1.47741935483871,-8.26115320609529)) ;
#106317 = CARTESIAN_POINT('',(8.49172374697003,1.47741935483871,-12.0588467939047)) ;
#106318 = CARTESIAN_POINT('Origin',(8.49172374697003,3.8,-10.16)) ;
#106319 = CARTESIAN_POINT('',(8.50816364570057,1.47636598119991,-8.26029201095833)) ;
#106320 = CARTESIAN_POINT('Origin',(8.49172374697003,1.4,-8.19785831296514)) ;
#106321 = CARTESIAN_POINT('',(8.50816364570057,1.47636598119991,-12.0597079890417)) ;
#106322 = CARTESIAN_POINT('Origin',(8.50816364570057,3.8,-10.16)) ;
#106323 = CARTESIAN_POINT('Origin',(8.49172374697003,1.4,-12.1221416870349)) ;
#106324 = CARTESIAN_POINT('Origin',(1.25,3.8,-10.16)) ;
#106325 = CARTESIAN_POINT('',(1.25,2.3,-10.16)) ;
#106326 = CARTESIAN_POINT('Origin',(13.9153543900904,3.8,-10.16)) ;
#106327 = CARTESIAN_POINT('',(-0.900000000000002,1.47741935483872,-12.0588467939047)) ;
#106328 = CARTESIAN_POINT('',(13.9153543900904,1.47741935483871,-12.0588467939047)) ;
#106329 = CARTESIAN_POINT('Origin',(-0.900000000000001,3.8,-10.16)) ;
#106330 = CARTESIAN_POINT('',(1.35,0.876327704607742,-10.8324137931035)) ;
#106331 = CARTESIAN_POINT('Ctrl Pts',(1.35,0.876327704607742,-10.8324137931035)) ;
#106332 = CARTESIAN_POINT('Ctrl Pts',(1.35,0.888571289407569,-10.8856492115953)) ;
#106333 = CARTESIAN_POINT('Ctrl Pts',(1.32969623836296,0.902340613578954,
-10.9379295970213)) ;
#106334 = CARTESIAN_POINT('Ctrl Pts',(1.25741074236298,0.924142973728496,
-11.0150150537158)) ;
#106335 = CARTESIAN_POINT('Ctrl Pts',(1.20472523187106,0.93175780006653,-11.0393103448276)) ;
#106336 = CARTESIAN_POINT('Ctrl Pts',(1.15,0.93175780006653,-11.0393103448276)) ;
#106337 = CARTESIAN_POINT('',(1.35,0.876327704607742,-9.48758620689656)) ;
#106338 = CARTESIAN_POINT('Origin',(1.35,3.8,-10.16)) ;
#106339 = CARTESIAN_POINT('Ctrl Pts',(1.15,0.931757800066529,-9.28068965517241)) ;
#106340 = CARTESIAN_POINT('Ctrl Pts',(1.20475877631964,0.931757800066529,
-9.28068965517241)) ;
#106341 = CARTESIAN_POINT('Ctrl Pts',(1.2574100247738,0.924155896380522,-9.30493436088835)) ;
#106342 = CARTESIAN_POINT('Ctrl Pts',(1.32987646938161,0.9022735155524,-9.3823125455279)) ;
#106343 = CARTESIAN_POINT('Ctrl Pts',(1.35,0.888577265820266,-9.43432480281013)) ;
#106344 = CARTESIAN_POINT('Ctrl Pts',(1.35,0.876327704607742,-9.48758620689656)) ;
#106345 = CARTESIAN_POINT('',(-0.900000000000002,1.47741935483872,-8.26115320609529)) ;
#106346 = CARTESIAN_POINT('Origin',(-0.900000000000001,3.8,-10.16)) ;
#106347 = CARTESIAN_POINT('',(13.9153543900904,1.47741935483871,-8.26115320609529)) ;
#106348 = CARTESIAN_POINT('Origin',(0.55,3.09772049281573E-17,-10.16)) ;
#106349 = CARTESIAN_POINT('',(0.549999999999999,4.4,-9.71)) ;
#106350 = CARTESIAN_POINT('',(0.549999999999999,4.4,-10.61)) ;
#106351 = CARTESIAN_POINT('',(0.549999999999999,4.4,-10.16)) ;
#106352 = CARTESIAN_POINT('',(0.55,4.04473197180486,-10.61)) ;
#106353 = CARTESIAN_POINT('',(0.55,1.39397422176708E-16,-10.61)) ;
#106354 = CARTESIAN_POINT('',(0.55,4.05997159067981,-10.56)) ;
#106355 = CARTESIAN_POINT('Ctrl Pts',(0.549999999999999,4.04473197180486,
-10.61)) ;
#106356 = CARTESIAN_POINT('Ctrl Pts',(0.549999999999999,4.04764757798806,
-10.6055648611277)) ;
#106357 = CARTESIAN_POINT('Ctrl Pts',(0.549999999999999,4.05014503921306,
-10.6009481448659)) ;
#106358 = CARTESIAN_POINT('Ctrl Pts',(0.549999999999999,4.0569489863933,-10.5856814456903)) ;
#106359 = CARTESIAN_POINT('Ctrl Pts',(0.549999999999999,4.0599715906798,-10.5718214564414)) ;
#106360 = CARTESIAN_POINT('Ctrl Pts',(0.549999999999999,4.0599715906798,-10.56)) ;
#106361 = CARTESIAN_POINT('',(0.55,4.05997159067981,-9.76)) ;
#106362 = CARTESIAN_POINT('',(0.55,4.05997159067981,-9.66)) ;
#106363 = CARTESIAN_POINT('',(0.55,4.04473197181449,-9.71000000001465)) ;
#106364 = CARTESIAN_POINT('Origin',(0.550034503802642,3.93869457791256,-9.76241602969578)) ;
#106365 = CARTESIAN_POINT('',(0.55,6.35032701027224E-17,-9.71)) ;
#106366 = CARTESIAN_POINT('Origin',(10.,7.8,-12.7)) ;
#106367 = CARTESIAN_POINT('',(9.93162277660169,7.82279240779944,-12.7)) ;
#106368 = CARTESIAN_POINT('',(8.51539501058484,8.29486832980505,-12.7)) ;
#106369 = CARTESIAN_POINT('',(10.,7.8,-12.7)) ;
#106370 = CARTESIAN_POINT('',(8.51540095511712,8.29487265903615,-10.9290607599342)) ;
#106371 = CARTESIAN_POINT('',(8.51539501058484,8.29486832980505,-12.7)) ;
#106372 = CARTESIAN_POINT('',(8.54856023413467,8.28398586203111,-10.9160080665656)) ;
#106373 = CARTESIAN_POINT('Ctrl Pts',(8.51540095511712,8.29487265903615,-10.9290607599342)) ;
#106374 = CARTESIAN_POINT('Ctrl Pts',(8.51716444659958,8.29428466923189,-10.9296424828188)) ;
#106375 = CARTESIAN_POINT('Ctrl Pts',(8.51901954868166,8.29366521079575,-10.9299704508582)) ;
#106376 = CARTESIAN_POINT('Ctrl Pts',(8.52087614409666,8.29304501946169,-10.9300725025784)) ;
#106377 = CARTESIAN_POINT('Ctrl Pts',(8.52171779595217,8.29276386763785,-10.9301187657647)) ;
#106378 = CARTESIAN_POINT('Ctrl Pts',(8.52256005861363,8.29248252453827,-10.930119087778)) ;
#106379 = CARTESIAN_POINT('Ctrl Pts',(8.52339613191993,8.29220315552769,-10.9300794460141)) ;
#106380 = CARTESIAN_POINT('Ctrl Pts',(8.5245631657957,8.29181319797643,-10.9300241120128)) ;
#106381 = CARTESIAN_POINT('Ctrl Pts',(8.52573147766849,8.29142195356395,-10.9298930049957)) ;
#106382 = CARTESIAN_POINT('Ctrl Pts',(8.52689074379091,8.29103442649364,-10.929691327086)) ;
#106383 = CARTESIAN_POINT('Ctrl Pts',(8.52858695132695,8.29046740713167,-10.9293962373014)) ;
#106384 = CARTESIAN_POINT('Ctrl Pts',(8.53026630212631,8.28992123633276,-10.9289439218143)) ;
#106385 = CARTESIAN_POINT('Ctrl Pts',(8.53190117913125,8.28939883282065,-10.9283683729162)) ;
#106386 = CARTESIAN_POINT('Ctrl Pts',(8.53241671440279,8.2892341002838,-10.9281868817357)) ;
#106387 = CARTESIAN_POINT('Ctrl Pts',(8.53292790037789,8.28907155799426,-10.9279933975174)) ;
#106388 = CARTESIAN_POINT('Ctrl Pts',(8.53343404910735,8.28891083250767,-10.9277898379553)) ;
#106389 = CARTESIAN_POINT('Ctrl Pts',(8.5352968140817,8.28831931900686,-10.9270406834076)) ;
#106390 = CARTESIAN_POINT('Ctrl Pts',(8.5371161216987,8.28774836357891,-10.9261310088335)) ;
#106391 = CARTESIAN_POINT('Ctrl Pts',(8.53885192161978,8.28720494689878,-10.925061264748)) ;
#106392 = CARTESIAN_POINT('Ctrl Pts',(8.54015925159107,8.28679566878774,-10.9242555794339)) ;
#106393 = CARTESIAN_POINT('Ctrl Pts',(8.54141951580281,8.28640152775902,-10.9233597461918)) ;
#106394 = CARTESIAN_POINT('Ctrl Pts',(8.54261761299018,8.28602171215282,-10.9223927107854)) ;
#106395 = CARTESIAN_POINT('Ctrl Pts',(8.54427390694789,8.28549664098145,-10.9210558451977)) ;
#106396 = CARTESIAN_POINT('Ctrl Pts',(8.54582756795257,8.28499592220795,-10.9195574336962)) ;
#106397 = CARTESIAN_POINT('Ctrl Pts',(8.54719190273352,8.28456181678114,-10.9179139760523)) ;
#106398 = CARTESIAN_POINT('Ctrl Pts',(8.54768505754694,8.28440490428155,-10.9173199290053)) ;
#106399 = CARTESIAN_POINT('Ctrl Pts',(8.54815358395155,8.28425671205378,-10.9167074323076)) ;
#106400 = CARTESIAN_POINT('Ctrl Pts',(8.54859369700693,8.284119365871,-10.9160788545618)) ;
#106401 = CARTESIAN_POINT('',(8.56837597005373,8.27720399148446,-10.8925054212669)) ;
#106402 = CARTESIAN_POINT('Ctrl Pts',(8.5485198670553,8.28382649282421,-10.9160140527758)) ;
#106403 = CARTESIAN_POINT('Ctrl Pts',(8.55267891820639,8.28243778061536,-10.9105631273052)) ;
#106404 = CARTESIAN_POINT('Ctrl Pts',(8.55701747195698,8.28096933708251,-10.9052590577814)) ;
#106405 = CARTESIAN_POINT('Ctrl Pts',(8.56150853123466,8.27945301063649,-10.9001132102133)) ;
#106406 = CARTESIAN_POINT('Ctrl Pts',(8.56331520072601,8.27884302075224,-10.8980431315896)) ;
#106407 = CARTESIAN_POINT('Ctrl Pts',(8.56514663435538,8.27822544298231,-10.8959980022295)) ;
#106408 = CARTESIAN_POINT('Ctrl Pts',(8.56700126712394,8.27760232477898,-10.8939757856585)) ;
#106409 = CARTESIAN_POINT('Ctrl Pts',(8.56745273479657,8.27745064099026,-10.8934835235653)) ;
#106410 = CARTESIAN_POINT('Ctrl Pts',(8.56790562999348,8.27729861980367,-10.8929951953627)) ;
#106411 = CARTESIAN_POINT('Ctrl Pts',(8.56835731300612,8.27714712982918,-10.8925055965825)) ;
#106412 = CARTESIAN_POINT('',(9.93162277660169,7.82279240779944,-11.1197127088383)) ;
#106413 = CARTESIAN_POINT('',(9.98593528106273,7.80468823964576,-11.1287647929151)) ;
#106414 = CARTESIAN_POINT('',(9.93162277660169,7.82279240779944,-12.7)) ;
#106415 = CARTESIAN_POINT('Origin',(10.,6.8,-12.7)) ;
#106416 = CARTESIAN_POINT('',(10.,6.8847127088383,-12.7)) ;
#106417 = CARTESIAN_POINT('',(10.,7.72792407799439,-12.7)) ;
#106418 = CARTESIAN_POINT('',(10.,6.8,-12.7)) ;
#106419 = CARTESIAN_POINT('',(10.,7.72792407799439,-11.1197127088383)) ;
#106420 = CARTESIAN_POINT('',(10.,7.72792407799439,-12.7)) ;
#106421 = CARTESIAN_POINT('',(10.,6.8847127088383,-11.1197127088383)) ;
#106422 = CARTESIAN_POINT('',(10.,6.8,-11.1197127088383)) ;
#106423 = CARTESIAN_POINT('',(10.,6.8847127088383,-12.7)) ;
#106424 = CARTESIAN_POINT('Origin',(8.5,6.55,-12.7)) ;
#106425 = CARTESIAN_POINT('',(9.91643989873054,6.78607331645509,-11.1197127088383)) ;
#106426 = CARTESIAN_POINT('',(8.58355805979355,6.56393854759964,-10.8975665415707)) ;
#106427 = CARTESIAN_POINT('',(8.48442535909739,6.54740422651623,-10.8810436188994)) ;
#106428 = CARTESIAN_POINT('',(8.56107669735261,6.5600938800009,-10.9223838472224)) ;
#106429 = CARTESIAN_POINT('Ctrl Pts',(8.58354728038623,6.56400494118526,-10.8975667486351)) ;
#106430 = CARTESIAN_POINT('Ctrl Pts',(8.57838853885701,6.56313097816979,-10.9029365696477)) ;
#106431 = CARTESIAN_POINT('Ctrl Pts',(8.57330127946562,6.56225500583441,-10.9083881686566)) ;
#106432 = CARTESIAN_POINT('Ctrl Pts',(8.56834297134819,6.56140899842965,-10.9139607837894)) ;
#106433 = CARTESIAN_POINT('Ctrl Pts',(8.5658758707988,6.56098805134778,-10.9167335444832)) ;
#106434 = CARTESIAN_POINT('Ctrl Pts',(8.56344049907318,6.56057499921404,-10.9195353033203)) ;
#106435 = CARTESIAN_POINT('Ctrl Pts',(8.56104288133097,6.56017406260212,-10.9223650362459)) ;
#106436 = CARTESIAN_POINT('',(8.50816305748499,6.55136011924236,-10.9373726221052)) ;
#106437 = CARTESIAN_POINT('Ctrl Pts',(8.56125813732195,6.56020968955366,-10.9225506353537)) ;
#106438 = CARTESIAN_POINT('Ctrl Pts',(8.55737139916546,6.55956189986091,-10.9272085994728)) ;
#106439 = CARTESIAN_POINT('Ctrl Pts',(8.55306335190366,6.55884389198394,-10.9299674660865)) ;
#106440 = CARTESIAN_POINT('Ctrl Pts',(8.54121332232485,6.55686888705414,-10.9365237407852)) ;
#106441 = CARTESIAN_POINT('Ctrl Pts',(8.53496267037859,6.55582711172976,-10.9379613606703)) ;
#106442 = CARTESIAN_POINT('Ctrl Pts',(8.52888665185255,6.55481444197543,-10.9392795539312)) ;
#106443 = CARTESIAN_POINT('Ctrl Pts',(8.52471102104795,6.55411850350799,-10.9395977494013)) ;
#106444 = CARTESIAN_POINT('Ctrl Pts',(8.52011475164576,6.55335245860763,-10.9397029599352)) ;
#106445 = CARTESIAN_POINT('Ctrl Pts',(8.51754797133926,6.55292466188988,-10.939718645943)) ;
#106446 = CARTESIAN_POINT('Ctrl Pts',(8.51248317870107,6.55208052978351,-10.9389638228623)) ;
#106447 = CARTESIAN_POINT('Ctrl Pts',(8.51021540604929,6.55170256767488,-10.9383708961116)) ;
#106448 = CARTESIAN_POINT('Ctrl Pts',(8.50816120922223,6.55136020153704,-10.9373764115261)) ;
#106449 = CARTESIAN_POINT('',(8.50816364570071,6.55136060761679,-12.7)) ;
#106450 = CARTESIAN_POINT('',(8.50816364570071,6.55136060761679,-12.7)) ;
#106451 = CARTESIAN_POINT('',(9.91643989873054,6.78607331645509,-12.7)) ;
#106452 = CARTESIAN_POINT('',(8.5,6.55,-12.7)) ;
#106453 = CARTESIAN_POINT('',(9.91643989873054,6.78607331645509,-12.7)) ;
#106454 = CARTESIAN_POINT('Origin',(10.,1.5,-12.7)) ;
#106455 = CARTESIAN_POINT('',(-0.900000000000002,1.5,-12.1221416870349)) ;
#106456 = CARTESIAN_POINT('',(8.49172374697003,1.5,-12.1221416870349)) ;
#106457 = CARTESIAN_POINT('',(10.,1.5,-12.1221416870349)) ;
#106458 = CARTESIAN_POINT('',(8.49172374697003,1.5,-12.7)) ;
#106459 = CARTESIAN_POINT('',(8.49172374697003,1.5,-12.7)) ;
#106460 = CARTESIAN_POINT('',(-0.900000000000001,1.5,-12.7)) ;
#106461 = CARTESIAN_POINT('',(10.,1.5,-12.7)) ;
#106462 = CARTESIAN_POINT('',(-0.900000000000002,1.5,-12.0861360284258)) ;
#106463 = CARTESIAN_POINT('Origin',(10.,1.5,-12.7)) ;
#106464 = CARTESIAN_POINT('',(8.49172374697003,1.5,-7.62)) ;
#106465 = CARTESIAN_POINT('',(-0.900000000000001,1.5,-7.62)) ;
#106466 = CARTESIAN_POINT('',(10.,1.5,-7.62)) ;
#106467 = CARTESIAN_POINT('',(8.49172374697003,1.5,-8.19785831296513)) ;
#106468 = CARTESIAN_POINT('',(8.49172374697003,1.5,-12.7)) ;
#106469 = CARTESIAN_POINT('',(-0.900000000000002,1.5,-8.19785831296513)) ;
#106470 = CARTESIAN_POINT('',(10.,1.5,-8.19785831296513)) ;
#106471 = CARTESIAN_POINT('',(-0.900000000000001,1.5,-12.7)) ;
#106472 = CARTESIAN_POINT('Origin',(10.,0.,-12.7)) ;
#106473 = CARTESIAN_POINT('',(10.,0.1,-7.62)) ;
#106474 = CARTESIAN_POINT('',(10.,1.16528729116168,-7.62)) ;
#106475 = CARTESIAN_POINT('',(10.,0.,-7.62)) ;
#106476 = CARTESIAN_POINT('',(10.,0.1,-12.7)) ;
#106477 = CARTESIAN_POINT('',(10.,0.1,-12.7)) ;
#106478 = CARTESIAN_POINT('',(10.,1.16528729116168,-12.7)) ;
#106479 = CARTESIAN_POINT('',(10.,0.,-12.7)) ;
#106480 = CARTESIAN_POINT('',(10.,1.16528729116168,-12.2041618801782)) ;
#106481 = CARTESIAN_POINT('',(10.,1.16528729116168,-12.7)) ;
#106482 = CARTESIAN_POINT('',(10.,1.16528729116168,-8.11583811982181)) ;
#106483 = CARTESIAN_POINT('Origin',(10.,3.8,-10.16)) ;
#106484 = CARTESIAN_POINT('',(10.,1.16528729116168,-12.7)) ;
#106485 = CARTESIAN_POINT('Origin',(0.,0.,-12.7)) ;
#106486 = CARTESIAN_POINT('',(8.48377223398316,8.3,-12.7)) ;
#106487 = CARTESIAN_POINT('',(7.1,8.3,-12.7)) ;
#106488 = CARTESIAN_POINT('',(8.5,8.3,-12.7)) ;
#106489 = CARTESIAN_POINT('Origin',(8.48377223398316,8.2,-12.7)) ;
#106490 = CARTESIAN_POINT('Origin',(9.9,7.72792407799439,-12.7)) ;
#106491 = CARTESIAN_POINT('Origin',(9.9,6.8847127088383,-12.7)) ;
#106492 = CARTESIAN_POINT('',(8.49172374697018,6.55,-12.7)) ;
#106493 = CARTESIAN_POINT('Origin',(8.49172374697018,6.65,-12.7)) ;
#106494 = CARTESIAN_POINT('',(-0.900000000000001,6.55,-12.7)) ;
#106495 = CARTESIAN_POINT('',(1.25,6.55,-12.7)) ;
#106496 = CARTESIAN_POINT('',(-1.,6.45,-12.7)) ;
#106497 = CARTESIAN_POINT('Origin',(-0.9,6.45,-12.7)) ;
#106498 = CARTESIAN_POINT('',(-1.,4.65,-12.7)) ;
#106499 = CARTESIAN_POINT('',(-1.,3.46944695195362E-16,-12.7)) ;
#106500 = CARTESIAN_POINT('',(-0.900000000000001,4.55,-12.7)) ;
#106501 = CARTESIAN_POINT('Origin',(-0.900000000000001,4.65,-12.7)) ;
#106502 = CARTESIAN_POINT('',(1.15,4.55,-12.7)) ;
#106503 = CARTESIAN_POINT('',(1.57859836313889E-15,4.55,-12.7)) ;
#106504 = CARTESIAN_POINT('',(1.25,4.45,-12.7)) ;
#106505 = CARTESIAN_POINT('Origin',(1.15,4.45,-12.7)) ;
#106506 = CARTESIAN_POINT('',(1.25,3.15,-12.7)) ;
#106507 = CARTESIAN_POINT('',(1.25,1.5,-12.7)) ;
#106508 = CARTESIAN_POINT('',(1.15,3.05,-12.7)) ;
#106509 = CARTESIAN_POINT('Origin',(1.15,3.15,-12.7)) ;
#106510 = CARTESIAN_POINT('',(-0.900000000000002,3.05,-12.7)) ;
#106511 = CARTESIAN_POINT('',(1.05818132034585E-15,3.05,-12.7)) ;
#106512 = CARTESIAN_POINT('',(-1.,2.95,-12.7)) ;
#106513 = CARTESIAN_POINT('Origin',(-0.900000000000002,2.95,-12.7)) ;
#106514 = CARTESIAN_POINT('',(-1.,1.6,-12.7)) ;
#106515 = CARTESIAN_POINT('',(-1.,3.46944695195362E-16,-12.7)) ;
#106516 = CARTESIAN_POINT('Origin',(-0.900000000000002,1.6,-12.7)) ;
#106517 = CARTESIAN_POINT('',(8.50816364570057,1.49863939238321,-12.7)) ;
#106518 = CARTESIAN_POINT('Origin',(8.49172374697003,1.4,-12.7)) ;
#106519 = CARTESIAN_POINT('',(9.91643989873054,1.26392668354489,-12.7)) ;
#106520 = CARTESIAN_POINT('',(10.,1.24999999999998,-12.7)) ;
#106521 = CARTESIAN_POINT('Origin',(9.9,1.16528729116168,-12.7)) ;
#106522 = CARTESIAN_POINT('',(9.9,0.,-12.7)) ;
#106523 = CARTESIAN_POINT('Origin',(9.9,0.1,-12.7)) ;
#106524 = CARTESIAN_POINT('',(-2.,0.,-12.7)) ;
#106525 = CARTESIAN_POINT('',(-2.,0.,-12.7)) ;
#106526 = CARTESIAN_POINT('',(-2.,7.55,-12.7)) ;
#106527 = CARTESIAN_POINT('',(-2.,7.65,-12.7)) ;
#106528 = CARTESIAN_POINT('',(-1.9,7.65,-12.7)) ;
#106529 = CARTESIAN_POINT('Origin',(-1.9,7.55,-12.7)) ;
#106530 = CARTESIAN_POINT('',(6.9,7.65,-12.7)) ;
#106531 = CARTESIAN_POINT('',(7.,7.65,-12.7)) ;
#106532 = CARTESIAN_POINT('',(7.,7.75,-12.7)) ;
#106533 = CARTESIAN_POINT('Origin',(6.9,7.75,-12.7)) ;
#106534 = CARTESIAN_POINT('',(7.,8.2,-12.7)) ;
#106535 = CARTESIAN_POINT('',(7.,8.3,-12.7)) ;
#106536 = CARTESIAN_POINT('Origin',(7.1,8.2,-12.7)) ;
#106537 = CARTESIAN_POINT('Origin',(0.,0.,-7.62)) ;
#106538 = CARTESIAN_POINT('',(9.93162277660169,7.82279240779944,-7.62)) ;
#106539 = CARTESIAN_POINT('',(8.51539501058484,8.29486832980505,-7.62)) ;
#106540 = CARTESIAN_POINT('',(10.,7.8,-7.62)) ;
#106541 = CARTESIAN_POINT('',(8.48377223398316,8.3,-7.62)) ;
#106542 = CARTESIAN_POINT('Origin',(8.48377223398316,8.2,-7.62)) ;
#106543 = CARTESIAN_POINT('',(7.1,8.3,-7.62)) ;
#106544 = CARTESIAN_POINT('',(8.5,8.3,-7.62)) ;
#106545 = CARTESIAN_POINT('',(7.,8.2,-7.62)) ;
#106546 = CARTESIAN_POINT('Origin',(7.1,8.2,-7.62)) ;
#106547 = CARTESIAN_POINT('',(7.,7.75,-7.62)) ;
#106548 = CARTESIAN_POINT('',(7.,8.3,-7.62)) ;
#106549 = CARTESIAN_POINT('',(6.9,7.65,-7.62)) ;
#106550 = CARTESIAN_POINT('Origin',(6.9,7.75,-7.62)) ;
#106551 = CARTESIAN_POINT('',(-1.9,7.65,-7.62)) ;
#106552 = CARTESIAN_POINT('',(7.,7.65,-7.62)) ;
#106553 = CARTESIAN_POINT('',(-2.,7.55,-7.62)) ;
#106554 = CARTESIAN_POINT('Origin',(-1.9,7.55,-7.62)) ;
#106555 = CARTESIAN_POINT('',(-2.,0.,-7.62)) ;
#106556 = CARTESIAN_POINT('',(-2.,7.65,-7.62)) ;
#106557 = CARTESIAN_POINT('',(9.9,0.,-7.62)) ;
#106558 = CARTESIAN_POINT('',(-2.,0.,-7.62)) ;
#106559 = CARTESIAN_POINT('Origin',(9.9,0.1,-7.62)) ;
#106560 = CARTESIAN_POINT('',(9.91643989873054,1.26392668354489,-7.62)) ;
#106561 = CARTESIAN_POINT('Origin',(9.9,1.16528729116168,-7.62)) ;
#106562 = CARTESIAN_POINT('',(8.50816364570057,1.49863939238321,-7.62)) ;
#106563 = CARTESIAN_POINT('',(0.472972972972955,2.83783783783779,-7.62)) ;
#106564 = CARTESIAN_POINT('Origin',(8.49172374697003,1.4,-7.62)) ;
#106565 = CARTESIAN_POINT('',(-1.,1.6,-7.62)) ;
#106566 = CARTESIAN_POINT('Origin',(-0.900000000000002,1.6,-7.62)) ;
#106567 = CARTESIAN_POINT('',(-1.,2.95,-7.62)) ;
#106568 = CARTESIAN_POINT('',(-1.,3.46944695195362E-16,-7.62)) ;
#106569 = CARTESIAN_POINT('',(-0.900000000000002,3.05,-7.62)) ;
#106570 = CARTESIAN_POINT('Origin',(-0.900000000000002,2.95,-7.62)) ;
#106571 = CARTESIAN_POINT('',(1.15,3.05,-7.62)) ;
#106572 = CARTESIAN_POINT('',(1.05818132034585E-15,3.05,-7.62)) ;
#106573 = CARTESIAN_POINT('',(1.25,3.15,-7.62)) ;
#106574 = CARTESIAN_POINT('Origin',(1.15,3.15,-7.62)) ;
#106575 = CARTESIAN_POINT('',(1.25,4.45,-7.62)) ;
#106576 = CARTESIAN_POINT('',(1.25,5.3,-7.62)) ;
#106577 = CARTESIAN_POINT('',(1.15,4.55,-7.62)) ;
#106578 = CARTESIAN_POINT('Origin',(1.15,4.45,-7.62)) ;
#106579 = CARTESIAN_POINT('',(-0.900000000000001,4.55,-7.62)) ;
#106580 = CARTESIAN_POINT('',(1.57859836313889E-15,4.55,-7.62)) ;
#106581 = CARTESIAN_POINT('',(-1.,4.65,-7.62)) ;
#106582 = CARTESIAN_POINT('Origin',(-0.900000000000001,4.65,-7.62)) ;
#106583 = CARTESIAN_POINT('',(-1.,6.45,-7.62)) ;
#106584 = CARTESIAN_POINT('',(-1.,3.46944695195362E-16,-7.62)) ;
#106585 = CARTESIAN_POINT('',(-0.900000000000001,6.55,-7.62)) ;
#106586 = CARTESIAN_POINT('Origin',(-0.9,6.45,-7.62)) ;
#106587 = CARTESIAN_POINT('',(8.49172374697018,6.55,-7.62)) ;
#106588 = CARTESIAN_POINT('',(1.25,6.55,-7.62)) ;
#106589 = CARTESIAN_POINT('',(8.50816364570071,6.55136060761679,-7.62)) ;
#106590 = CARTESIAN_POINT('Origin',(8.49172374697018,6.65,-7.62)) ;
#106591 = CARTESIAN_POINT('',(9.91643989873054,6.78607331645509,-7.62)) ;
#106592 = CARTESIAN_POINT('',(8.5,6.55,-7.62)) ;
#106593 = CARTESIAN_POINT('',(10.,6.8847127088383,-7.62)) ;
#106594 = CARTESIAN_POINT('Origin',(9.9,6.8847127088383,-7.62)) ;
#106595 = CARTESIAN_POINT('',(10.,7.72792407799439,-7.62)) ;
#106596 = CARTESIAN_POINT('',(10.,6.8,-7.62)) ;
#106597 = CARTESIAN_POINT('Origin',(9.9,7.72792407799439,-7.62)) ;
#106598 = CARTESIAN_POINT('Origin',(7.,7.65,-12.7)) ;
#106599 = CARTESIAN_POINT('',(-1.9,7.65,-12.7)) ;
#106600 = CARTESIAN_POINT('',(6.9,7.65,-12.7)) ;
#106601 = CARTESIAN_POINT('Origin',(7.,8.3,-12.7)) ;
#106602 = CARTESIAN_POINT('',(7.,7.75,-7.62)) ;
#106603 = CARTESIAN_POINT('',(7.,8.2,-12.7)) ;
#106604 = CARTESIAN_POINT('Origin',(8.5,8.3,-12.7)) ;
#106605 = CARTESIAN_POINT('',(8.4,8.3,-10.702072889851)) ;
#106606 = CARTESIAN_POINT('',(8.48377267093844,8.29999999999968,-10.9180525450042)) ;
#106607 = CARTESIAN_POINT('Ctrl Pts',(8.4,8.3,-10.702072889851)) ;
#106608 = CARTESIAN_POINT('Ctrl Pts',(8.40000007660114,8.3,-10.7192296501939)) ;
#106609 = CARTESIAN_POINT('Ctrl Pts',(8.40222537906598,8.3,-10.7361962391145)) ;
#106610 = CARTESIAN_POINT('Ctrl Pts',(8.40642689896089,8.3,-10.7526162565003)) ;
#106611 = CARTESIAN_POINT('Ctrl Pts',(8.4108423802432,8.3,-10.7698724593116)) ;
#106612 = CARTESIAN_POINT('Ctrl Pts',(8.41744096860975,8.3,-10.7865267443636)) ;
#106613 = CARTESIAN_POINT('Ctrl Pts',(8.42598957610198,8.3,-10.8021622007235)) ;
#106614 = CARTESIAN_POINT('Ctrl Pts',(8.42927578125679,8.3,-10.8081726904243)) ;
#106615 = CARTESIAN_POINT('Ctrl Pts',(8.43285067318485,8.3,-10.8140324469597)) ;
#106616 = CARTESIAN_POINT('Ctrl Pts',(8.43670279785317,8.3,-10.8197167867854)) ;
#106617 = CARTESIAN_POINT('Ctrl Pts',(8.43684245837178,8.3,-10.8199228750916)) ;
#106618 = CARTESIAN_POINT('Ctrl Pts',(8.43698247939112,8.3,-10.8201287268225)) ;
#106619 = CARTESIAN_POINT('Ctrl Pts',(8.43712286024714,8.3,-10.8203343406941)) ;
#106620 = CARTESIAN_POINT('Ctrl Pts',(8.4430409279857,8.3,-10.8290024515356)) ;
#106621 = CARTESIAN_POINT('Ctrl Pts',(8.44963232699551,8.300000000002,-10.8373317313645)) ;
#106622 = CARTESIAN_POINT('Ctrl Pts',(8.45667836512368,8.29999999999776,-10.8451882739642)) ;
#106623 = CARTESIAN_POINT('Ctrl Pts',(8.46347186896913,8.29999999999368,-10.8527632333091)) ;
#106624 = CARTESIAN_POINT('Ctrl Pts',(8.47075094334182,8.29999999998296,-10.8599098655153)) ;
#106625 = CARTESIAN_POINT('Ctrl Pts',(8.47818849074308,8.29999999991001,-10.8668816128285)) ;
#106626 = CARTESIAN_POINT('Ctrl Pts',(8.47846436286148,8.2999999999073,-10.8671402075771)) ;
#106627 = CARTESIAN_POINT('Ctrl Pts',(8.47874045306876,8.29999999990447,-10.8673985605991)) ;
#106628 = CARTESIAN_POINT('Ctrl Pts',(8.47901674447045,8.29999999990152,-10.8676566852)) ;
#106629 = CARTESIAN_POINT('Ctrl Pts',(8.48287938578321,8.29999999986032,-10.8712653488833)) ;
#106630 = CARTESIAN_POINT('Ctrl Pts',(8.4868120552941,8.29999999978804,-10.8748079367278)) ;
#106631 = CARTESIAN_POINT('Ctrl Pts',(8.49047938959117,8.29999999977837,-10.8786027060218)) ;
#106632 = CARTESIAN_POINT('Ctrl Pts',(8.49231307405274,8.29999999977353,-10.8805001085834)) ;
#106633 = CARTESIAN_POINT('Ctrl Pts',(8.49410676862313,8.29999999978935,-10.882469327125)) ;
#106634 = CARTESIAN_POINT('Ctrl Pts',(8.49555027122445,8.29999999981726,-10.8846968070099)) ;
#106635 = CARTESIAN_POINT('Ctrl Pts',(8.49675259850851,8.2999999998405,-10.8865521274215)) ;
#106636 = CARTESIAN_POINT('Ctrl Pts',(8.49764594203226,8.29999999986456,-10.8886368157432)) ;
#106637 = CARTESIAN_POINT('Ctrl Pts',(8.49795530287013,8.29999999987615,-10.8908110374494)) ;
#106638 = CARTESIAN_POINT('Ctrl Pts',(8.49801735255452,8.29999999987847,-10.8912471293982)) ;
#106639 = CARTESIAN_POINT('Ctrl Pts',(8.49805590844335,8.29999999988033,-10.891686822978)) ;
#106640 = CARTESIAN_POINT('Ctrl Pts',(8.49806875158487,8.29999999988168,-10.8921289896614)) ;
#106641 = CARTESIAN_POINT('Ctrl Pts',(8.49822249685463,8.2999999998978,-10.8974221678068)) ;
#106642 = CARTESIAN_POINT('Ctrl Pts',(8.49538250015675,8.29999999989889,-10.9023553442684)) ;
#106643 = CARTESIAN_POINT('Ctrl Pts',(8.49246863081132,8.29999999993393,-10.906722860551)) ;
#106644 = CARTESIAN_POINT('Ctrl Pts',(8.48983292606215,8.29999999996562,-10.9106734437939)) ;
#106645 = CARTESIAN_POINT('Ctrl Pts',(8.48683766317128,8.3,-10.9143922110698)) ;
#106646 = CARTESIAN_POINT('Ctrl Pts',(8.48377316486176,8.3,-10.9180519562975)) ;
#106647 = CARTESIAN_POINT('',(8.48377223398316,8.3,-12.7)) ;
#106648 = CARTESIAN_POINT('',(7.1,8.3,-12.7)) ;
#106649 = CARTESIAN_POINT('',(8.48377267093845,8.29999999999968,-9.40194745499578)) ;
#106650 = CARTESIAN_POINT('',(8.48377223398316,8.3,-12.7)) ;
#106651 = CARTESIAN_POINT('',(8.4,8.3,-9.61792711014902)) ;
#106652 = CARTESIAN_POINT('Ctrl Pts',(8.48377316486176,8.3,-9.40194804370243)) ;
#106653 = CARTESIAN_POINT('Ctrl Pts',(8.48683766317131,8.3,-9.4056077889302)) ;
#106654 = CARTESIAN_POINT('Ctrl Pts',(8.48983292606215,8.29999999996562,-9.40932655620614)) ;
#106655 = CARTESIAN_POINT('Ctrl Pts',(8.49246863081132,8.29999999993393,-9.41327713944902)) ;
#106656 = CARTESIAN_POINT('Ctrl Pts',(8.49538250015675,8.29999999989889,-9.41764465573158)) ;
#106657 = CARTESIAN_POINT('Ctrl Pts',(8.49822249685462,8.2999999998978,-9.42257783219323)) ;
#106658 = CARTESIAN_POINT('Ctrl Pts',(8.49806875158486,8.29999999988168,-9.42787101033858)) ;
#106659 = CARTESIAN_POINT('Ctrl Pts',(8.49805590844334,8.29999999988033,-9.42831317702195)) ;
#106660 = CARTESIAN_POINT('Ctrl Pts',(8.49801735255452,8.29999999987847,-9.42875287060182)) ;
#106661 = CARTESIAN_POINT('Ctrl Pts',(8.49795530287013,8.29999999987615,-9.42918896255059)) ;
#106662 = CARTESIAN_POINT('Ctrl Pts',(8.49764594190815,8.29999999986456,-9.43136318512906)) ;
#106663 = CARTESIAN_POINT('Ctrl Pts',(8.49675259754385,8.2999999998405,-9.43344787406726)) ;
#106664 = CARTESIAN_POINT('Ctrl Pts',(8.49555027122433,8.29999999981726,-9.43530319298998)) ;
#106665 = CARTESIAN_POINT('Ctrl Pts',(8.49410676570212,8.29999999978935,-9.43753067738161)) ;
#106666 = CARTESIAN_POINT('Ctrl Pts',(8.4923130692812,8.29999999977353,-9.439499896352)) ;
#106667 = CARTESIAN_POINT('Ctrl Pts',(8.49047938958768,8.29999999977837,-9.44139729397482)) ;
#106668 = CARTESIAN_POINT('Ctrl Pts',(8.48681202348067,8.29999999978804,-9.44519209617395)) ;
#106669 = CARTESIAN_POINT('Ctrl Pts',(8.48287934332709,8.29999999986032,-9.4487346907302)) ;
#106670 = CARTESIAN_POINT('Ctrl Pts',(8.47901674443308,8.29999999990152,-9.45234331475996)) ;
#106671 = CARTESIAN_POINT('Ctrl Pts',(8.47874052296043,8.29999999990447,-9.45260137402811)) ;
#106672 = CARTESIAN_POINT('Ctrl Pts',(8.4784645028431,8.2999999999073,-9.45285966135653)) ;
#106673 = CARTESIAN_POINT('Ctrl Pts',(8.47818870097127,8.29999999991001,-9.4531181900299)) ;
#106674 = CARTESIAN_POINT('Ctrl Pts',(8.47075185325581,8.29999999998296,-9.46008927532798)) ;
#106675 = CARTESIAN_POINT('Ctrl Pts',(8.46347271757077,8.29999999998104,-9.467236821007)) ;
#106676 = CARTESIAN_POINT('Ctrl Pts',(8.45667934899943,8.29999999998018,-9.4748126083154)) ;
#106677 = CARTESIAN_POINT('Ctrl Pts',(8.44963335392747,8.29999999997929,-9.48267011810317)) ;
#106678 = CARTESIAN_POINT('Ctrl Pts',(8.44304226791565,8.29999999996634,-9.49100025634497)) ;
#106679 = CARTESIAN_POINT('Ctrl Pts',(8.43712466127421,8.29999999997622,-9.499666888942)) ;
#106680 = CARTESIAN_POINT('Ctrl Pts',(8.43698358608697,8.29999999997646,-9.49987350065014)) ;
#106681 = CARTESIAN_POINT('Ctrl Pts',(8.43684287437575,8.2999999999767,-9.50008035127934)) ;
#106682 = CARTESIAN_POINT('Ctrl Pts',(8.43670252680327,8.29999999997696,-9.50028743949552)) ;
#106683 = CARTESIAN_POINT('Ctrl Pts',(8.42665365624217,8.29999999999548,-9.51511493271403)) ;
#106684 = CARTESIAN_POINT('Ctrl Pts',(8.41848789916333,8.29999999999779,-9.53113486319164)) ;
#106685 = CARTESIAN_POINT('Ctrl Pts',(8.41242260582416,8.29999999999911,-9.54791805139679)) ;
#106686 = CARTESIAN_POINT('Ctrl Pts',(8.40662497274209,8.30000000000037,-9.56396060065526)) ;
#106687 = CARTESIAN_POINT('Ctrl Pts',(8.40274598945956,8.3,-9.58070219391593)) ;
#106688 = CARTESIAN_POINT('Ctrl Pts',(8.40101973895731,8.3,-9.5977797883369)) ;
#106689 = CARTESIAN_POINT('Ctrl Pts',(8.4003453349782,8.3,-9.60445158806471)) ;
#106690 = CARTESIAN_POINT('Ctrl Pts',(8.40000003014814,8.3,-9.61117467303844)) ;
#106691 = CARTESIAN_POINT('Ctrl Pts',(8.4,8.3,-9.61792711014901)) ;
#106692 = CARTESIAN_POINT('',(8.4,8.3,-10.7436545563009)) ;
#106693 = CARTESIAN_POINT('Origin',(10.,7.8,-12.7)) ;
#106694 = CARTESIAN_POINT('',(8.56837722373804,8.27720759208727,-9.4274948832495)) ;
#106695 = CARTESIAN_POINT('',(8.54843785958924,8.2838540468036,-9.4039803122607)) ;
#106696 = CARTESIAN_POINT('Ctrl Pts',(8.56837722339832,8.27720759220056,-9.42749488336226)) ;
#106697 = CARTESIAN_POINT('Ctrl Pts',(8.56792584473107,8.27735805175631,-9.42700469022775)) ;
#106698 = CARTESIAN_POINT('Ctrl Pts',(8.56747319573485,8.27750893475505,-9.42651579326377)) ;
#106699 = CARTESIAN_POINT('Ctrl Pts',(8.56702308739659,8.2776589708678,-9.42602430395872)) ;
#106700 = CARTESIAN_POINT('Ctrl Pts',(8.56055949575605,8.27981350141465,-9.41896647833432)) ;
#106701 = CARTESIAN_POINT('Ctrl Pts',(8.5543545977397,8.28188180075344,-9.41162839546916)) ;
#106702 = CARTESIAN_POINT('Ctrl Pts',(8.54852002808959,8.28382665730347,-9.40398586635143)) ;
#106703 = CARTESIAN_POINT('',(8.51539953939799,8.29486682020068,-9.39094033012292)) ;
#106704 = CARTESIAN_POINT('Origin',(8.52916905055959,8.29027698314681,-9.41073447047856)) ;
#106705 = CARTESIAN_POINT('',(8.51539501058484,8.29486832980505,-12.7)) ;
#106706 = CARTESIAN_POINT('',(9.93162277660169,7.82279240779944,-9.2002872911617)) ;
#106707 = CARTESIAN_POINT('',(9.93162277660169,7.82279240779944,-12.7)) ;
#106708 = CARTESIAN_POINT('',(8.48593528106273,8.30468823964576,-9.44123520708485)) ;
#106709 = CARTESIAN_POINT('Origin',(10.,6.8,-12.7)) ;
#106710 = CARTESIAN_POINT('',(10.,6.8847127088383,-9.2002872911617)) ;
#106711 = CARTESIAN_POINT('',(10.,7.72792407799439,-9.2002872911617)) ;
#106712 = CARTESIAN_POINT('',(10.,7.8,-9.2002872911617)) ;
#106713 = CARTESIAN_POINT('',(10.,7.72792407799439,-12.7)) ;
#106714 = CARTESIAN_POINT('',(10.,6.8847127088383,-12.7)) ;
#106715 = CARTESIAN_POINT('Origin',(8.5,6.55,-12.7)) ;
#106716 = CARTESIAN_POINT('',(8.50816305748852,6.55136011924294,-9.38262737789189)) ;
#106717 = CARTESIAN_POINT('Ctrl Pts',(8.5081612092262,6.5513602015377,-9.382623588472)) ;
#106718 = CARTESIAN_POINT('Ctrl Pts',(8.50982330775211,6.55163721795868,-9.38181892781788)) ;
#106719 = CARTESIAN_POINT('Ctrl Pts',(8.51162127657737,6.55193687942956,-9.38127902844107)) ;
#106720 = CARTESIAN_POINT('Ctrl Pts',(8.51523682141479,6.5525394702358,-9.38057109233512)) ;
#106721 = CARTESIAN_POINT('Ctrl Pts',(8.51710259142427,6.55285043190405,-9.38039346793926)) ;
#106722 = CARTESIAN_POINT('Ctrl Pts',(8.52217030373287,6.55369505062214,-9.38023569112659)) ;
#106723 = CARTESIAN_POINT('Ctrl Pts',(8.52587381749955,6.55431230291659,-9.38048388339446)) ;
#106724 = CARTESIAN_POINT('Ctrl Pts',(8.53482421527996,6.55580403587999,-9.38172985018422)) ;
#106725 = CARTESIAN_POINT('Ctrl Pts',(8.53952102462675,6.55658683673483,-9.38322044742373)) ;
#106726 = CARTESIAN_POINT('Ctrl Pts',(8.54640674065816,6.5577344560734,-9.38636821224601)) ;
#106727 = CARTESIAN_POINT('Ctrl Pts',(8.55013419152241,6.55835569858707,-9.38823673023074)) ;
#106728 = CARTESIAN_POINT('Ctrl Pts',(8.55581906875222,6.55930317812537,-9.39204337543013)) ;
#106729 = CARTESIAN_POINT('Ctrl Pts',(8.55861150732171,6.55976858455362,-9.39427755556342)) ;
#106730 = CARTESIAN_POINT('Ctrl Pts',(8.56125821409731,6.56020970234955,-9.39744945665611)) ;
#106731 = CARTESIAN_POINT('',(9.91643989873054,6.78607331645509,-9.2002872911617)) ;
#106732 = CARTESIAN_POINT('',(9.98442535909739,6.79740422651623,-9.18895638110055)) ;
#106733 = CARTESIAN_POINT('',(9.91643989873054,6.78607331645509,-12.7)) ;
#106734 = CARTESIAN_POINT('',(8.50816364570071,6.55136060761679,-12.7)) ;
#106735 = CARTESIAN_POINT('Origin',(1.25,6.55,-12.7)) ;
#106736 = CARTESIAN_POINT('',(8.49172372711481,6.55000000000007,-10.9294558427306)) ;
#106737 = CARTESIAN_POINT('',(8.49172374697018,6.55,-12.7)) ;
#106738 = CARTESIAN_POINT('',(8.4,6.55,-10.7006780018997)) ;
#106739 = CARTESIAN_POINT('Ctrl Pts',(8.49172374697018,6.55000000000105,-10.9294557456557)) ;
#106740 = CARTESIAN_POINT('Ctrl Pts',(8.49606803673627,6.55000000001052,-10.9259505863269)) ;
#106741 = CARTESIAN_POINT('Ctrl Pts',(8.50046735944503,6.54999999990302,-10.9225119042493)) ;
#106742 = CARTESIAN_POINT('Ctrl Pts',(8.50920280475179,6.55000000136501,-10.9155160267021)) ;
#106743 = CARTESIAN_POINT('Ctrl Pts',(8.51365366733341,6.55000000372466,-10.9120189182925)) ;
#106744 = CARTESIAN_POINT('Ctrl Pts',(8.51786969589086,6.55000000840872,-10.907574051492)) ;
#106745 = CARTESIAN_POINT('Ctrl Pts',(8.51824835575326,6.5500000088438,-10.9071628343558)) ;
#106746 = CARTESIAN_POINT('Ctrl Pts',(8.51893753951067,6.55000000964298,-10.9063894122641)) ;
#106747 = CARTESIAN_POINT('Ctrl Pts',(8.51925555226623,6.55000001000021,-10.9060246830609)) ;
#106748 = CARTESIAN_POINT('Ctrl Pts',(8.52125362518914,6.55000001218547,-10.9036369664008)) ;
#106749 = CARTESIAN_POINT('Ctrl Pts',(8.52280131776511,6.55000000862055,-10.9013625215737)) ;
#106750 = CARTESIAN_POINT('Ctrl Pts',(8.52354796988914,6.55000000490364,-10.8962172682011)) ;
#106751 = CARTESIAN_POINT('Ctrl Pts',(8.52233587755844,6.5500000056078,-10.8935629178231)) ;
#106752 = CARTESIAN_POINT('Ctrl Pts',(8.52032554216538,6.55000000470579,-10.8911610105703)) ;
#106753 = CARTESIAN_POINT('Ctrl Pts',(8.5200461874495,6.55000000456892,-10.8908554672244)) ;
#106754 = CARTESIAN_POINT('Ctrl Pts',(8.51943244221702,6.55000000425258,-10.8902375575506)) ;
#106755 = CARTESIAN_POINT('Ctrl Pts',(8.51910103101852,6.55000000405877,-10.8899172773213)) ;
#106756 = CARTESIAN_POINT('Ctrl Pts',(8.51460799223802,6.5500000014124,-10.8857349310042)) ;
#106757 = CARTESIAN_POINT('Ctrl Pts',(8.50969722522556,6.55000000036127,-10.8829602411529)) ;
#106758 = CARTESIAN_POINT('Ctrl Pts',(8.50463600502755,6.55000000021577,-10.8796634748388)) ;
#106759 = CARTESIAN_POINT('Ctrl Pts',(8.50427412871942,6.55000000020764,-10.8794272801265)) ;
#106760 = CARTESIAN_POINT('Ctrl Pts',(8.49410349041847,6.55000000002642,-10.8727743312815)) ;
#106761 = CARTESIAN_POINT('Ctrl Pts',(8.48448997361521,6.54999999999179,-10.8660809389623)) ;
#106762 = CARTESIAN_POINT('Ctrl Pts',(8.46629237463078,6.55000000001684,-10.8509770243887)) ;
#106763 = CARTESIAN_POINT('Ctrl Pts',(8.45766562693773,6.55000000000151,-10.8425939316618)) ;
#106764 = CARTESIAN_POINT('Ctrl Pts',(8.44955830666693,6.54999999999999,-10.8332123342681)) ;
#106765 = CARTESIAN_POINT('Ctrl Pts',(8.4493708101522,6.54999999999999,-10.8329944283116)) ;
#106766 = CARTESIAN_POINT('Ctrl Pts',(8.43720071044502,6.5500000000026,-10.8187892740227)) ;
#106767 = CARTESIAN_POINT('Ctrl Pts',(8.427213843659,6.55000000009149,-10.8032566681918)) ;
#106768 = CARTESIAN_POINT('Ctrl Pts',(8.41184903642503,6.55000000007035,-10.7705950553225)) ;
#106769 = CARTESIAN_POINT('Ctrl Pts',(8.40635547808451,6.5500000000232,-10.7535173325337)) ;
#106770 = CARTESIAN_POINT('Ctrl Pts',(8.40108598764611,6.5499999999995,-10.7243588087582)) ;
#106771 = CARTESIAN_POINT('Ctrl Pts',(8.4,6.55,-10.7125595279398)) ;
#106772 = CARTESIAN_POINT('Ctrl Pts',(8.4,6.55,-10.7006780018997)) ;
#106773 = CARTESIAN_POINT('',(8.4,6.55,-9.6193219981003)) ;
#106774 = CARTESIAN_POINT('',(8.4,6.55,-9.43636060761679)) ;
#106775 = CARTESIAN_POINT('',(8.4917237271148,6.5500000000004,-9.39054415726839)) ;
#106776 = CARTESIAN_POINT('Ctrl Pts',(8.4,6.55,-9.6193219981003)) ;
#106777 = CARTESIAN_POINT('Ctrl Pts',(8.4,6.55,-9.60146035159508)) ;
#106778 = CARTESIAN_POINT('Ctrl Pts',(8.40245177849645,6.55000000000111,-9.58378505809112)) ;
#106779 = CARTESIAN_POINT('Ctrl Pts',(8.40709634751483,6.55000000003438,-9.56675184875779)) ;
#106780 = CARTESIAN_POINT('Ctrl Pts',(8.41193897064549,6.55000000006908,-9.54899230784436)) ;
#106781 = CARTESIAN_POINT('Ctrl Pts',(8.41916594308043,6.55000000013771,-9.53192888814512)) ;
#106782 = CARTESIAN_POINT('Ctrl Pts',(8.42853896333499,6.55000000013582,-9.51608126731972)) ;
#106783 = CARTESIAN_POINT('Ctrl Pts',(8.434550587058,6.55000000013461,-9.50591699468187)) ;
#106784 = CARTESIAN_POINT('Ctrl Pts',(8.44144611055218,6.55000000009671,-9.49625300072306)) ;
#106785 = CARTESIAN_POINT('Ctrl Pts',(8.44917210140205,6.55000000005186,-9.48723268310166)) ;
#106786 = CARTESIAN_POINT('Ctrl Pts',(8.44936219523638,6.55000000005075,-9.4870107430558)) ;
#106787 = CARTESIAN_POINT('Ctrl Pts',(8.44955278293316,6.55000000004968,-9.48678920228628)) ;
#106788 = CARTESIAN_POINT('Ctrl Pts',(8.44974386351697,6.55000000004864,-9.48656806301675)) ;
#106789 = CARTESIAN_POINT('Ctrl Pts',(8.45766118910685,6.55000000000559,-9.47740527126339)) ;
#106790 = CARTESIAN_POINT('Ctrl Pts',(8.46628870646479,6.54999999999864,-9.46902155150326)) ;
#106791 = CARTESIAN_POINT('Ctrl Pts',(8.47555348469885,6.55000000000007,-9.46133527594906)) ;
#106792 = CARTESIAN_POINT('Ctrl Pts',(8.48448851770303,6.55000000000144,-9.45392256470859)) ;
#106793 = CARTESIAN_POINT('Ctrl Pts',(8.49410273695376,6.5500000000304,-9.44723469297056)) ;
#106794 = CARTESIAN_POINT('Ctrl Pts',(8.50391213313781,6.55000000016212,-9.4408238957712)) ;
#106795 = CARTESIAN_POINT('Ctrl Pts',(8.50409415224108,6.55000000016456,-9.44070493966671)) ;
#106796 = CARTESIAN_POINT('Ctrl Pts',(8.50427622716233,6.55000000016576,-9.44058605979316)) ;
#106797 = CARTESIAN_POINT('Ctrl Pts',(8.50445835579895,6.55000000016577,-9.44046725463207)) ;
#106798 = CARTESIAN_POINT('Ctrl Pts',(8.50464048443556,6.55000000016577,-9.44034844947097)) ;
#106799 = CARTESIAN_POINT('Ctrl Pts',(8.50482266678753,6.55000000016459,-9.44022971902234)) ;
#106800 = CARTESIAN_POINT('Ctrl Pts',(8.50500490075221,6.55000000016234,-9.44011106176768)) ;
#106801 = CARTESIAN_POINT('Ctrl Pts',(8.50970297364421,6.55000000010443,-9.43705202481732)) ;
#106802 = CARTESIAN_POINT('Ctrl Pts',(8.51460443926437,6.55000000028677,-9.43427565407059)) ;
#106803 = CARTESIAN_POINT('Ctrl Pts',(8.5187483092633,6.55000000038295,-9.43043698472844)) ;
#106804 = CARTESIAN_POINT('Ctrl Pts',(8.51909542442958,6.55000000039101,-9.43011543498211)) ;
#106805 = CARTESIAN_POINT('Ctrl Pts',(8.51943721516333,6.55000000039358,-9.42978641450153)) ;
#106806 = CARTESIAN_POINT('Ctrl Pts',(8.51977310187182,6.55000000039099,-9.4294491161473)) ;
#106807 = CARTESIAN_POINT('Ctrl Pts',(8.52085916897636,6.55000000038261,-9.42835848458113)) ;
#106808 = CARTESIAN_POINT('Ctrl Pts',(8.5218239980174,6.55000000033869,-9.42704462088201)) ;
#106809 = CARTESIAN_POINT('Ctrl Pts',(8.52246334063461,6.55000000029842,-9.42562676665968)) ;
#106810 = CARTESIAN_POINT('Ctrl Pts',(8.52278301194322,6.55000000027829,-9.42491783954851)) ;
#106811 = CARTESIAN_POINT('Ctrl Pts',(8.52302131164588,6.55000000025926,-9.42418291480655)) ;
#106812 = CARTESIAN_POINT('Ctrl Pts',(8.52315270869754,6.55000000024662,-9.42343689763501)) ;
#106813 = CARTESIAN_POINT('Ctrl Pts',(8.5232841057492,6.55000000023398,-9.42269088046346)) ;
#106814 = CARTESIAN_POINT('Ctrl Pts',(8.52330860014988,6.55000000022778,-9.42193377086234)) ;
#106815 = CARTESIAN_POINT('Ctrl Pts',(8.52320066085452,6.55000000023233,-9.42118047403286)) ;
#106816 = CARTESIAN_POINT('Ctrl Pts',(8.5228403133075,6.55000000024754,-9.41866564693692)) ;
#106817 = CARTESIAN_POINT('Ctrl Pts',(8.52133564423351,6.55000000029586,-9.41640673801312)) ;
#106818 = CARTESIAN_POINT('Ctrl Pts',(8.5196587899188,6.55000000031744,-9.41439865149544)) ;
#106819 = CARTESIAN_POINT('Ctrl Pts',(8.51932554032813,6.55000000032173,-9.41399957448309)) ;
#106820 = CARTESIAN_POINT('Ctrl Pts',(8.51898545723479,6.55000000032523,-9.41361037576486)) ;
#106821 = CARTESIAN_POINT('Ctrl Pts',(8.51864615038491,6.5500000003277,-9.41323101231938)) ;
#106822 = CARTESIAN_POINT('Ctrl Pts',(8.5145508165866,6.55000000035749,-9.40865220720328)) ;
#106823 = CARTESIAN_POINT('Ctrl Pts',(8.50963987409778,6.55000000028078,-9.40482020861866)) ;
#106824 = CARTESIAN_POINT('Ctrl Pts',(8.5048217738226,6.55000000018958,-9.4009688701254)) ;
#106825 = CARTESIAN_POINT('Ctrl Pts',(8.50046402923751,6.5500000001071,-9.3974855160012)) ;
#106826 = CARTESIAN_POINT('Ctrl Pts',(8.49606692679175,6.55000000001227,-9.39404901054622)) ;
#106827 = CARTESIAN_POINT('Ctrl Pts',(8.49172374697017,6.55000000000105,-9.39054425434379)) ;
#106828 = CARTESIAN_POINT('',(8.49172374697018,6.55,-12.7)) ;
#106829 = CARTESIAN_POINT('',(-0.9,6.55,-9.31)) ;
#106830 = CARTESIAN_POINT('',(-0.900000000000001,6.55,-12.7)) ;
#106831 = CARTESIAN_POINT('',(1.15,6.55,-9.31)) ;
#106832 = CARTESIAN_POINT('',(1.25,6.55,-9.31)) ;
#106833 = CARTESIAN_POINT('',(1.35,6.55,-9.51)) ;
#106834 = CARTESIAN_POINT('Origin',(1.15,6.55,-9.51)) ;
#106835 = CARTESIAN_POINT('',(1.35,6.55,-10.81)) ;
#106836 = CARTESIAN_POINT('',(1.35,6.55,-10.91)) ;
#106837 = CARTESIAN_POINT('',(1.15,6.55,-11.01)) ;
#106838 = CARTESIAN_POINT('Origin',(1.15,6.55,-10.81)) ;
#106839 = CARTESIAN_POINT('',(-0.9,6.55,-11.01)) ;
#106840 = CARTESIAN_POINT('',(1.25,6.55,-11.01)) ;
#106841 = CARTESIAN_POINT('',(-0.9,6.55,-12.7)) ;
#106842 = CARTESIAN_POINT('Origin',(1.25,5.3,-12.7)) ;
#106843 = CARTESIAN_POINT('',(1.25,3.15,-11.8031676725155)) ;
#106844 = CARTESIAN_POINT('',(1.25,3.04189189189189,-11.6255279241354)) ;
#106845 = CARTESIAN_POINT('Origin',(1.25,2.95,-11.8031676725155)) ;
#106846 = CARTESIAN_POINT('',(1.25,3.15,-12.7)) ;
#106847 = CARTESIAN_POINT('',(1.25,4.45,-11.8031676725155)) ;
#106848 = CARTESIAN_POINT('',(1.25,4.45,-11.7411388300842)) ;
#106849 = CARTESIAN_POINT('',(1.25,4.55810810810811,-11.6255279241354)) ;
#106850 = CARTESIAN_POINT('Origin',(1.25,4.65,-11.8031676725155)) ;
#106851 = CARTESIAN_POINT('',(1.25,5.26552792413544,-10.9181081081081)) ;
#106852 = CARTESIAN_POINT('Origin',(1.25,3.8,-10.16)) ;
#106853 = CARTESIAN_POINT('',(1.25,5.4431676725155,-10.81)) ;
#106854 = CARTESIAN_POINT('Origin',(1.25,5.4431676725155,-11.01)) ;
#106855 = CARTESIAN_POINT('',(1.25,6.45,-10.81)) ;
#106856 = CARTESIAN_POINT('',(1.25,6.55,-10.81)) ;
#106857 = CARTESIAN_POINT('',(1.25,6.45,-9.51)) ;
#106858 = CARTESIAN_POINT('',(1.25,6.45,-9.41)) ;
#106859 = CARTESIAN_POINT('',(1.25,5.4431676725155,-9.51)) ;
#106860 = CARTESIAN_POINT('',(1.25,5.38113883008419,-9.51)) ;
#106861 = CARTESIAN_POINT('',(1.25,5.26552792413544,-9.40189189189189)) ;
#106862 = CARTESIAN_POINT('Origin',(1.25,5.4431676725155,-9.31)) ;
#106863 = CARTESIAN_POINT('',(1.25,4.55810810810811,-8.69447207586456)) ;
#106864 = CARTESIAN_POINT('Origin',(1.25,3.8,-10.16)) ;
#106865 = CARTESIAN_POINT('',(1.25,4.45,-8.5168323274845)) ;
#106866 = CARTESIAN_POINT('Origin',(1.25,4.65,-8.5168323274845)) ;
#106867 = CARTESIAN_POINT('',(1.25,4.45,-7.62)) ;
#106868 = CARTESIAN_POINT('',(1.25,3.15,-8.5168323274845)) ;
#106869 = CARTESIAN_POINT('',(1.25,3.15,-8.57886116991581)) ;
#106870 = CARTESIAN_POINT('',(1.25,3.04189189189189,-8.69447207586456)) ;
#106871 = CARTESIAN_POINT('Origin',(1.25,2.95,-8.5168323274845)) ;
#106872 = CARTESIAN_POINT('',(1.25,2.33447207586456,-9.40189189189189)) ;
#106873 = CARTESIAN_POINT('Origin',(1.25,3.8,-10.16)) ;
#106874 = CARTESIAN_POINT('',(1.25,2.1568323274845,-9.51)) ;
#106875 = CARTESIAN_POINT('Origin',(1.25,2.1568323274845,-9.31)) ;
#106876 = CARTESIAN_POINT('',(1.25,0.973783447787483,-9.51)) ;
#106877 = CARTESIAN_POINT('',(1.25,0.895262490344437,-9.51)) ;
#106878 = CARTESIAN_POINT('',(1.25,0.973783447787483,-10.81)) ;
#106879 = CARTESIAN_POINT('Origin',(1.25,3.8,-10.16)) ;
#106880 = CARTESIAN_POINT('',(1.25,2.1568323274845,-10.81)) ;
#106881 = CARTESIAN_POINT('',(1.25,2.21886116991581,-10.81)) ;
#106882 = CARTESIAN_POINT('',(1.25,2.33447207586456,-10.9181081081081)) ;
#106883 = CARTESIAN_POINT('Origin',(1.25,2.1568323274845,-11.01)) ;
#106884 = CARTESIAN_POINT('Origin',(1.25,3.8,-10.16)) ;
#106885 = CARTESIAN_POINT('Origin',(-2.,0.,-12.7)) ;
#106886 = CARTESIAN_POINT('',(0.899999999999999,0.,-11.76)) ;
#106887 = CARTESIAN_POINT('',(1.1,0.,-11.56)) ;
#106888 = CARTESIAN_POINT('Origin',(0.899999999999999,0.,-11.56)) ;
#106889 = CARTESIAN_POINT('',(-2.,0.,-11.76)) ;
#106890 = CARTESIAN_POINT('',(-2.,0.,-11.76)) ;
#106891 = CARTESIAN_POINT('',(-2.,0.,-12.7)) ;
#106892 = CARTESIAN_POINT('',(9.9,0.,-12.7)) ;
#106893 = CARTESIAN_POINT('',(-2.,0.,-8.56)) ;
#106894 = CARTESIAN_POINT('',(-2.,0.,-12.7)) ;
#106895 = CARTESIAN_POINT('',(0.899999999999999,0.,-8.56)) ;
#106896 = CARTESIAN_POINT('',(0.999999999999999,0.,-8.56)) ;
#106897 = CARTESIAN_POINT('',(1.1,0.,-8.76)) ;
#106898 = CARTESIAN_POINT('Origin',(0.899999999999999,0.,-8.76)) ;
#106899 = CARTESIAN_POINT('',(1.1,0.,-11.66)) ;
#106900 = CARTESIAN_POINT('Origin',(-2.,7.65,-12.7)) ;
#106901 = CARTESIAN_POINT('',(-2.,6.9,-8.56)) ;
#106902 = CARTESIAN_POINT('',(-2.,7.1,-8.76)) ;
#106903 = CARTESIAN_POINT('Origin',(-2.,6.9,-8.76)) ;
#106904 = CARTESIAN_POINT('',(-2.,-1.13380619344889E-17,-8.56)) ;
#106905 = CARTESIAN_POINT('',(-2.,7.55,-12.7)) ;
#106906 = CARTESIAN_POINT('',(-2.,6.9,-11.76)) ;
#106907 = CARTESIAN_POINT('',(-2.,7.,-11.76)) ;
#106908 = CARTESIAN_POINT('',(-2.,7.1,-11.56)) ;
#106909 = CARTESIAN_POINT('Origin',(-2.,6.9,-11.56)) ;
#106910 = CARTESIAN_POINT('',(-2.,7.1,-8.66)) ;
#106911 = CARTESIAN_POINT('Origin',(-1.8,7.,-8.66)) ;
#106912 = CARTESIAN_POINT('',(-1.7,0.1,-8.66)) ;
#106913 = CARTESIAN_POINT('',(-1.9,0.1,-8.66)) ;
#106914 = CARTESIAN_POINT('',(-2.,0.1,-8.66)) ;
#106915 = CARTESIAN_POINT('',(-1.9,0.3,-8.66)) ;
#106916 = CARTESIAN_POINT('',(-1.9,7.,-8.66)) ;
#106917 = CARTESIAN_POINT('Origin',(-1.7,0.3,-8.66)) ;
#106918 = CARTESIAN_POINT('Origin',(-1.8,7.,-11.66)) ;
#106919 = CARTESIAN_POINT('',(-1.9,0.3,-11.66)) ;
#106920 = CARTESIAN_POINT('',(-1.7,0.1,-11.66)) ;
#106921 = CARTESIAN_POINT('Origin',(-1.7,0.3,-11.66)) ;
#106922 = CARTESIAN_POINT('',(-1.9,0.1,-11.66)) ;
#106923 = CARTESIAN_POINT('',(-1.9,1.23908819712629E-17,-11.66)) ;
#106924 = CARTESIAN_POINT('',(0.999999999999999,0.1,-11.66)) ;
#106925 = CARTESIAN_POINT('Origin',(-1.8,-2.2514151555628E-16,-10.16)) ;
#106926 = CARTESIAN_POINT('',(-1.8,4.6,-10.81)) ;
#106927 = CARTESIAN_POINT('',(-1.8,4.6,-9.51)) ;
#106928 = CARTESIAN_POINT('',(-1.8,4.6,-9.61)) ;
#106929 = CARTESIAN_POINT('',(-1.8,0.3,-9.51)) ;
#106930 = CARTESIAN_POINT('',(-1.8,0.2,-9.51)) ;
#106931 = CARTESIAN_POINT('',(-1.8,0.3,-8.76)) ;
#106932 = CARTESIAN_POINT('',(-1.8,0.3,-8.66)) ;
#106933 = CARTESIAN_POINT('',(-1.8,6.9,-8.76)) ;
#106934 = CARTESIAN_POINT('',(-1.8,-5.16691679585995E-17,-8.76)) ;
#106935 = CARTESIAN_POINT('',(-1.8,6.9,-11.56)) ;
#106936 = CARTESIAN_POINT('',(-1.8,6.9,-10.16)) ;
#106937 = CARTESIAN_POINT('',(-1.8,0.3,-11.56)) ;
#106938 = CARTESIAN_POINT('',(-1.8,-3.98613863153961E-16,-11.56)) ;
#106939 = CARTESIAN_POINT('',(-1.8,0.3,-10.81)) ;
#106940 = CARTESIAN_POINT('',(-1.8,0.3,-10.71)) ;
#106941 = CARTESIAN_POINT('',(-1.8,4.5,-10.81)) ;
#106942 = CARTESIAN_POINT('Origin',(0.549999999999999,4.5,-9.61)) ;
#106943 = CARTESIAN_POINT('',(-1.7,0.3,-9.61)) ;
#106944 = CARTESIAN_POINT('',(-1.7,4.4,-9.61)) ;
#106945 = CARTESIAN_POINT('',(-1.7,4.5,-9.61)) ;
#106946 = CARTESIAN_POINT('',(0.45,4.4,-9.61)) ;
#106947 = CARTESIAN_POINT('',(0.45,4.4,-9.61)) ;
#106948 = CARTESIAN_POINT('',(0.45,0.3,-9.61)) ;
#106949 = CARTESIAN_POINT('',(0.45,4.5,-9.61)) ;
#106950 = CARTESIAN_POINT('',(0.549999999999999,0.3,-9.61)) ;
#106951 = CARTESIAN_POINT('Origin',(0.549999999999999,4.5,-10.71)) ;
#106952 = CARTESIAN_POINT('',(0.45,0.3,-10.71)) ;
#106953 = CARTESIAN_POINT('',(0.45,4.4,-10.71)) ;
#106954 = CARTESIAN_POINT('',(0.45,4.5,-10.71)) ;
#106955 = CARTESIAN_POINT('',(-1.7,4.4,-10.71)) ;
#106956 = CARTESIAN_POINT('',(-1.7,4.4,-10.71)) ;
#106957 = CARTESIAN_POINT('',(-1.7,0.3,-10.71)) ;
#106958 = CARTESIAN_POINT('',(-1.7,0.2,-10.71)) ;
#106959 = CARTESIAN_POINT('',(0.549999999999999,0.3,-10.71)) ;
#106960 = CARTESIAN_POINT('Origin',(0.549999999999999,4.5,-10.71)) ;
#106961 = CARTESIAN_POINT('',(-1.7,4.5,-9.71)) ;
#106962 = CARTESIAN_POINT('',(-1.7,4.5,-10.61)) ;
#106963 = CARTESIAN_POINT('',(-1.7,4.5,-10.71)) ;
#106964 = CARTESIAN_POINT('',(0.45,4.5,-10.61)) ;
#106965 = CARTESIAN_POINT('',(0.45,4.5,-10.61)) ;
#106966 = CARTESIAN_POINT('',(0.45,4.5,-9.71)) ;
#106967 = CARTESIAN_POINT('',(0.45,4.5,-10.71)) ;
#106968 = CARTESIAN_POINT('',(-1.7,4.5,-9.71)) ;
#106969 = CARTESIAN_POINT('Origin',(0.55,3.09772049281573E-17,-10.16)) ;
#106970 = CARTESIAN_POINT('',(0.55,2.61224989991992,-10.56)) ;
#106971 = CARTESIAN_POINT('',(0.55,2.65280931275608,-10.61)) ;
#106972 = CARTESIAN_POINT('Ctrl Pts',(0.55,2.61224989991992,-10.56)) ;
#106973 = CARTESIAN_POINT('Ctrl Pts',(0.55,2.61224989991992,-10.563869744162)) ;
#106974 = CARTESIAN_POINT('Ctrl Pts',(0.55,2.61317624258758,-10.5684201039157)) ;
#106975 = CARTESIAN_POINT('Ctrl Pts',(0.55,2.61634258087509,-10.5766330008589)) ;
#106976 = CARTESIAN_POINT('Ctrl Pts',(0.55,2.61951410407877,-10.5816304286453)) ;
#106977 = CARTESIAN_POINT('Ctrl Pts',(0.55,2.63040394024853,-10.5949387190701)) ;
#106978 = CARTESIAN_POINT('Ctrl Pts',(0.55,2.6414836688106,-10.6031705809674)) ;
#106979 = CARTESIAN_POINT('Ctrl Pts',(0.55,2.65280931275608,-10.61)) ;
#106980 = CARTESIAN_POINT('',(0.55,0.3,-10.61)) ;
#106981 = CARTESIAN_POINT('',(0.55,1.39397422176708E-16,-10.61)) ;
#106982 = CARTESIAN_POINT('',(0.55,0.3,-9.71)) ;
#106983 = CARTESIAN_POINT('',(0.55,0.3,-9.61)) ;
#106984 = CARTESIAN_POINT('',(0.55,2.65280931275594,-9.71000000000009)) ;
#106985 = CARTESIAN_POINT('',(0.55,6.35032701027224E-17,-9.71)) ;
#106986 = CARTESIAN_POINT('',(0.55,2.61224989991992,-9.76)) ;
#106987 = CARTESIAN_POINT('Ctrl Pts',(0.55,2.65280931275594,-9.71000000000009)) ;
#106988 = CARTESIAN_POINT('Ctrl Pts',(0.55,2.64148366881051,-9.71682941903265)) ;
#106989 = CARTESIAN_POINT('Ctrl Pts',(0.55,2.6304039402485,-9.72506128092989)) ;
#106990 = CARTESIAN_POINT('Ctrl Pts',(0.55,2.61951410407877,-9.73836957135471)) ;
#106991 = CARTESIAN_POINT('Ctrl Pts',(0.55,2.61634258087509,-9.74336699914113)) ;
#106992 = CARTESIAN_POINT('Ctrl Pts',(0.55,2.61317624258758,-9.75157989608431)) ;
#106993 = CARTESIAN_POINT('Ctrl Pts',(0.55,2.61224989991992,-9.75613025583802)) ;
#106994 = CARTESIAN_POINT('Ctrl Pts',(0.55,2.61224989991992,-9.76)) ;
#106995 = CARTESIAN_POINT('',(0.55,2.61224989991992,-9.66)) ;
#106996 = CARTESIAN_POINT('Origin',(0.,0.2,-10.16)) ;
#106997 = CARTESIAN_POINT('',(-1.7,0.2,-10.81)) ;
#106998 = CARTESIAN_POINT('',(-1.7,0.2,-11.56)) ;
#106999 = CARTESIAN_POINT('',(-1.7,0.2,-11.66)) ;
#107000 = CARTESIAN_POINT('',(0.899999999999999,0.2,-11.56)) ;
#107001 = CARTESIAN_POINT('',(0.999999999999999,0.2,-11.56)) ;
#107002 = CARTESIAN_POINT('',(0.899999999999999,0.2,-8.76)) ;
#107003 = CARTESIAN_POINT('',(0.899999999999999,0.2,-8.66)) ;
#107004 = CARTESIAN_POINT('',(-1.7,0.2,-8.76)) ;
#107005 = CARTESIAN_POINT('',(-1.8,0.2,-8.76)) ;
#107006 = CARTESIAN_POINT('',(-1.7,0.2,-9.51)) ;
#107007 = CARTESIAN_POINT('',(-1.7,0.2,-9.61)) ;
#107008 = CARTESIAN_POINT('',(0.65,0.2,-9.51)) ;
#107009 = CARTESIAN_POINT('',(-1.16429916652874E-32,0.2,-9.51)) ;
#107010 = CARTESIAN_POINT('',(0.65,0.2,-10.81)) ;
#107011 = CARTESIAN_POINT('',(0.65,0.2,-10.71)) ;
#107012 = CARTESIAN_POINT('',(-1.35834902761687E-32,0.2,-10.81)) ;
#107013 = CARTESIAN_POINT('Origin',(3.,2.3,-12.7)) ;
#107014 = CARTESIAN_POINT('',(3.,4.2,-9.66)) ;
#107015 = CARTESIAN_POINT('',(3.,3.4,-9.66)) ;
#107016 = CARTESIAN_POINT('',(3.,2.3,-9.66)) ;
#107017 = CARTESIAN_POINT('',(3.,4.3,-9.76)) ;
#107018 = CARTESIAN_POINT('Origin',(3.,4.2,-9.76)) ;
#107019 = CARTESIAN_POINT('',(3.,4.3,-10.56)) ;
#107020 = CARTESIAN_POINT('',(3.,4.3,-12.7)) ;
#107021 = CARTESIAN_POINT('',(3.,4.2,-10.66)) ;
#107022 = CARTESIAN_POINT('Origin',(3.,4.2,-10.56)) ;
#107023 = CARTESIAN_POINT('',(3.,3.4,-10.66)) ;
#107024 = CARTESIAN_POINT('',(3.,2.3,-10.66)) ;
#107025 = CARTESIAN_POINT('',(3.,3.3,-10.56)) ;
#107026 = CARTESIAN_POINT('Origin',(3.,3.4,-10.56)) ;
#107027 = CARTESIAN_POINT('',(3.,3.3,-9.76)) ;
#107028 = CARTESIAN_POINT('',(3.,3.3,-12.7)) ;
#107029 = CARTESIAN_POINT('Origin',(3.,3.4,-9.76)) ;
#107030 = CARTESIAN_POINT('Origin',(-1.,3.8,-10.16)) ;
#107031 = CARTESIAN_POINT('',(-1.,1.6,-12.1221416870349)) ;
#107032 = CARTESIAN_POINT('',(-1.,1.55483870967742,-11.9955519007746)) ;
#107033 = CARTESIAN_POINT('Origin',(-1.,1.40000000000001,-12.1221416870349)) ;
#107034 = CARTESIAN_POINT('',(-1.,1.6,-12.7)) ;
#107035 = CARTESIAN_POINT('',(-1.,2.95,-11.8031676725155)) ;
#107036 = CARTESIAN_POINT('',(-1.,2.95,-10.16)) ;
#107037 = CARTESIAN_POINT('',(-1.,2.1568323274845,-11.01)) ;
#107038 = CARTESIAN_POINT('Origin',(-1.,3.8,-10.16)) ;
#107039 = CARTESIAN_POINT('',(-1.,1.02736587339765,-11.01)) ;
#107040 = CARTESIAN_POINT('',(-1.,3.8,-11.01)) ;
#107041 = CARTESIAN_POINT('Origin',(-1.,3.8,-10.16)) ;
#107042 = CARTESIAN_POINT('Origin',(-1.,3.05,-12.71)) ;
#107043 = CARTESIAN_POINT('',(1.15,3.05,-11.8031676725155)) ;
#107044 = CARTESIAN_POINT('',(1.15,3.05,-11.7411388300842)) ;
#107045 = CARTESIAN_POINT('',(-0.900000000000002,3.05,-11.8031676725155)) ;
#107046 = CARTESIAN_POINT('',(-1.,3.05,-11.8031676725155)) ;
#107047 = CARTESIAN_POINT('',(-0.900000000000002,3.05,-12.71)) ;
#107048 = CARTESIAN_POINT('Origin',(-1.,2.21886116991581,-10.91)) ;
#107049 = CARTESIAN_POINT('',(-0.900000000000002,2.1568323274845,-10.91)) ;
#107050 = CARTESIAN_POINT('',(1.15,2.1568323274845,-10.91)) ;
#107051 = CARTESIAN_POINT('',(1.25,2.1568323274845,-10.91)) ;
#107052 = CARTESIAN_POINT('',(1.15,0.895262490344437,-10.91)) ;
#107053 = CARTESIAN_POINT('',(-0.900000000000002,2.21886116991581,-10.91)) ;
#107054 = CARTESIAN_POINT('Origin',(-1.,3.8,-10.16)) ;
#107055 = CARTESIAN_POINT('',(-0.900000000000002,2.24565220167453,-10.9640540540541)) ;
#107056 = CARTESIAN_POINT('',(-0.900000000000001,2.99594594594595,-11.7143477983255)) ;
#107057 = CARTESIAN_POINT('Origin',(-0.900000000000001,3.8,-10.16)) ;
#107058 = CARTESIAN_POINT('',(1.15,2.99594594594595,-11.7143477983255)) ;
#107059 = CARTESIAN_POINT('',(-1.,2.99594594594595,-11.7143477983255)) ;
#107060 = CARTESIAN_POINT('',(1.15,2.24565220167453,-10.9640540540541)) ;
#107061 = CARTESIAN_POINT('Origin',(1.15,3.8,-10.16)) ;
#107062 = CARTESIAN_POINT('',(-1.,2.24565220167453,-10.9640540540541)) ;
#107063 = CARTESIAN_POINT('Origin',(-1.,3.8,-10.16)) ;
#107064 = CARTESIAN_POINT('',(-0.900000000000002,2.99594594594594,-8.60565220167453)) ;
#107065 = CARTESIAN_POINT('',(-0.900000000000002,2.24565220167453,-9.35594594594595)) ;
#107066 = CARTESIAN_POINT('Origin',(-0.900000000000001,3.8,-10.16)) ;
#107067 = CARTESIAN_POINT('',(1.15,2.24565220167453,-9.35594594594595)) ;
#107068 = CARTESIAN_POINT('',(-1.,2.24565220167453,-9.35594594594595)) ;
#107069 = CARTESIAN_POINT('',(1.15,2.99594594594594,-8.60565220167453)) ;
#107070 = CARTESIAN_POINT('Origin',(1.15,3.8,-10.16)) ;
#107071 = CARTESIAN_POINT('',(-1.,2.99594594594594,-8.60565220167453)) ;
#107072 = CARTESIAN_POINT('Origin',(-1.,2.21886116991581,-9.41)) ;
#107073 = CARTESIAN_POINT('',(1.15,2.1568323274845,-9.41)) ;
#107074 = CARTESIAN_POINT('',(1.15,2.21886116991581,-9.41)) ;
#107075 = CARTESIAN_POINT('',(-0.900000000000002,2.1568323274845,-9.41)) ;
#107076 = CARTESIAN_POINT('',(-1.,2.1568323274845,-9.41)) ;
#107077 = CARTESIAN_POINT('',(-0.900000000000002,0.895262490344437,-9.41)) ;
#107078 = CARTESIAN_POINT('Origin',(-1.,3.05,-7.61)) ;
#107079 = CARTESIAN_POINT('',(-0.900000000000002,3.05,-8.5168323274845)) ;
#107080 = CARTESIAN_POINT('',(1.15,3.05,-8.5168323274845)) ;
#107081 = CARTESIAN_POINT('',(1.25,3.05,-8.5168323274845)) ;
#107082 = CARTESIAN_POINT('',(1.15,3.05,-7.62)) ;
#107083 = CARTESIAN_POINT('',(-0.900000000000002,3.05,-8.57886116991581)) ;
#107084 = CARTESIAN_POINT('Origin',(-1.,3.8,-10.16)) ;
#107085 = CARTESIAN_POINT('',(-1.,2.1568323274845,-9.31)) ;
#107086 = CARTESIAN_POINT('',(-1.,2.95,-8.5168323274845)) ;
#107087 = CARTESIAN_POINT('Origin',(-1.,3.8,-10.16)) ;
#107088 = CARTESIAN_POINT('',(-1.,2.95,-7.62)) ;
#107089 = CARTESIAN_POINT('',(-1.,1.6,-8.19785831296513)) ;
#107090 = CARTESIAN_POINT('',(-1.,1.6,-10.16)) ;
#107091 = CARTESIAN_POINT('',(-1.,1.55483870967743,-8.32444809922545)) ;
#107092 = CARTESIAN_POINT('Origin',(-1.,1.40000000000001,-8.19785831296513)) ;
#107093 = CARTESIAN_POINT('',(-1.,1.02736587339765,-9.31)) ;
#107094 = CARTESIAN_POINT('Origin',(-1.,3.8,-10.16)) ;
#107095 = CARTESIAN_POINT('',(-1.,2.21886116991581,-9.31)) ;
#107096 = CARTESIAN_POINT('Origin',(-1.,3.8,-10.16)) ;
#107097 = CARTESIAN_POINT('',(-1.,5.4431676725155,-11.01)) ;
#107098 = CARTESIAN_POINT('',(-1.,4.65,-11.8031676725155)) ;
#107099 = CARTESIAN_POINT('Origin',(-1.,3.8,-10.16)) ;
#107100 = CARTESIAN_POINT('',(-1.,4.65,-10.16)) ;
#107101 = CARTESIAN_POINT('',(-1.,6.45,-11.01)) ;
#107102 = CARTESIAN_POINT('',(-1.,6.45,-10.91)) ;
#107103 = CARTESIAN_POINT('',(-1.,3.8,-11.01)) ;
#107104 = CARTESIAN_POINT('Origin',(-1.,4.55,-11.7411388300842)) ;
#107105 = CARTESIAN_POINT('',(-0.900000000000001,4.55,-11.8031676725155)) ;
#107106 = CARTESIAN_POINT('',(1.15,4.55,-11.8031676725155)) ;
#107107 = CARTESIAN_POINT('',(1.25,4.55,-11.8031676725155)) ;
#107108 = CARTESIAN_POINT('',(1.15,4.55,-12.7)) ;
#107109 = CARTESIAN_POINT('',(-0.900000000000001,4.55,-11.7411388300842)) ;
#107110 = CARTESIAN_POINT('Origin',(-1.,3.8,-10.16)) ;
#107111 = CARTESIAN_POINT('',(-0.900000000000001,4.60405405405406,-11.7143477983255)) ;
#107112 = CARTESIAN_POINT('',(-0.900000000000001,5.35434779832547,-10.9640540540541)) ;
#107113 = CARTESIAN_POINT('Origin',(-0.900000000000001,3.8,-10.16)) ;
#107114 = CARTESIAN_POINT('',(1.15,5.35434779832547,-10.9640540540541)) ;
#107115 = CARTESIAN_POINT('',(-1.,5.35434779832547,-10.9640540540541)) ;
#107116 = CARTESIAN_POINT('',(1.15,4.60405405405405,-11.7143477983255)) ;
#107117 = CARTESIAN_POINT('Origin',(1.15,3.8,-10.16)) ;
#107118 = CARTESIAN_POINT('',(-1.,4.60405405405406,-11.7143477983255)) ;
#107119 = CARTESIAN_POINT('Origin',(-1.,6.55,-10.91)) ;
#107120 = CARTESIAN_POINT('',(-0.900000000000001,5.4431676725155,-10.91)) ;
#107121 = CARTESIAN_POINT('',(-0.9,6.45,-10.91)) ;
#107122 = CARTESIAN_POINT('',(-0.9,6.55,-10.91)) ;
#107123 = CARTESIAN_POINT('',(1.15,6.45,-10.91)) ;
#107124 = CARTESIAN_POINT('',(-1.,6.45,-10.91)) ;
#107125 = CARTESIAN_POINT('',(1.15,5.4431676725155,-10.91)) ;
#107126 = CARTESIAN_POINT('',(1.15,5.38113883008419,-10.91)) ;
#107127 = CARTESIAN_POINT('',(-1.,5.4431676725155,-10.91)) ;
#107128 = CARTESIAN_POINT('Origin',(-1.,3.8,-10.16)) ;
#107129 = CARTESIAN_POINT('',(-0.900000000000001,5.35434779832547,-9.35594594594594)) ;
#107130 = CARTESIAN_POINT('',(-0.900000000000001,4.60405405405405,-8.60565220167453)) ;
#107131 = CARTESIAN_POINT('Origin',(-0.900000000000001,3.8,-10.16)) ;
#107132 = CARTESIAN_POINT('',(1.15,4.60405405405405,-8.60565220167453)) ;
#107133 = CARTESIAN_POINT('',(-1.,4.60405405405405,-8.60565220167453)) ;
#107134 = CARTESIAN_POINT('',(1.15,5.35434779832547,-9.35594594594594)) ;
#107135 = CARTESIAN_POINT('Origin',(1.15,3.8,-10.16)) ;
#107136 = CARTESIAN_POINT('',(-1.,5.35434779832547,-9.35594594594594)) ;
#107137 = CARTESIAN_POINT('Origin',(-1.,4.55,-8.57886116991581)) ;
#107138 = CARTESIAN_POINT('',(1.15,4.55,-8.5168323274845)) ;
#107139 = CARTESIAN_POINT('',(1.15,4.55,-8.57886116991581)) ;
#107140 = CARTESIAN_POINT('',(-0.900000000000001,4.55,-8.5168323274845)) ;
#107141 = CARTESIAN_POINT('',(-1.,4.55,-8.5168323274845)) ;
#107142 = CARTESIAN_POINT('',(-0.900000000000001,4.55,-7.62)) ;
#107143 = CARTESIAN_POINT('Origin',(-1.,6.55,-9.41)) ;
#107144 = CARTESIAN_POINT('',(1.15,5.4431676725155,-9.41)) ;
#107145 = CARTESIAN_POINT('',(1.15,6.45,-9.41)) ;
#107146 = CARTESIAN_POINT('',(1.15,6.55,-9.41)) ;
#107147 = CARTESIAN_POINT('',(-0.9,6.45,-9.41)) ;
#107148 = CARTESIAN_POINT('',(-1.,6.45,-9.41)) ;
#107149 = CARTESIAN_POINT('',(-0.900000000000001,5.4431676725155,-9.41)) ;
#107150 = CARTESIAN_POINT('',(-0.900000000000001,5.38113883008419,-9.41)) ;
#107151 = CARTESIAN_POINT('',(1.25,5.4431676725155,-9.41)) ;
#107152 = CARTESIAN_POINT('Origin',(-1.,3.8,-10.16)) ;
#107153 = CARTESIAN_POINT('',(-1.,5.4431676725155,-9.31)) ;
#107154 = CARTESIAN_POINT('',(-1.,6.45,-9.31)) ;
#107155 = CARTESIAN_POINT('',(-1.,6.55,-9.31)) ;
#107156 = CARTESIAN_POINT('',(-1.,6.45,-10.16)) ;
#107157 = CARTESIAN_POINT('',(-1.,4.65,-8.5168323274845)) ;
#107158 = CARTESIAN_POINT('',(-1.,4.65,-8.57886116991581)) ;
#107159 = CARTESIAN_POINT('Origin',(-1.,3.8,-10.16)) ;
#107160 = CARTESIAN_POINT('Origin',(10.,4.35421736843756,-11.035)) ;
#107161 = CARTESIAN_POINT('',(9.91643989873054,7.72792407799439,-11.0210733164551)) ;
#107162 = CARTESIAN_POINT('',(8.58356010126947,8.17221734381475,-10.7989266835449)) ;
#107163 = CARTESIAN_POINT('',(8.47075240319158,8.20981990984071,-10.7801254005319)) ;
#107164 = CARTESIAN_POINT('',(8.58356010126947,6.66256607592813,-10.7989266835449)) ;
#107165 = CARTESIAN_POINT('',(8.58356010126947,6.64863939238321,-10.7989266835449)) ;
#107166 = CARTESIAN_POINT('',(9.91643989873054,6.8847127088383,-11.0210733164551)) ;
#107167 = CARTESIAN_POINT('',(9.98442535909739,6.89604361889945,-11.0324042265162)) ;
#107168 = CARTESIAN_POINT('',(9.91643989873054,7.8,-11.0210733164551)) ;
#107169 = CARTESIAN_POINT('Origin',(8.5,4.35421736843756,-10.785)) ;
#107170 = CARTESIAN_POINT('',(8.5,8.17221734381475,-10.7002872911617)) ;
#107171 = CARTESIAN_POINT('',(8.50000000129681,8.20000000266559,-10.702105625353)) ;
#107172 = CARTESIAN_POINT('Origin',(8.5,8.17870774546496,-10.8890376382098)) ;
#107173 = CARTESIAN_POINT('',(8.5,8.2,-9.57634544369909)) ;
#107174 = CARTESIAN_POINT('',(8.5,6.66256607592813,-9.61971270883831)) ;
#107175 = CARTESIAN_POINT('',(8.5,6.64863939238321,-9.61971270883831)) ;
#107176 = CARTESIAN_POINT('',(8.50000000002143,6.64999999935441,-9.61931784432624)) ;
#107177 = CARTESIAN_POINT('Origin',(8.5,6.65811550105781,-9.42318847658934)) ;
#107178 = CARTESIAN_POINT('',(8.49999999999933,6.65000073218972,-10.7006896909637)) ;
#107179 = CARTESIAN_POINT('',(8.5,6.65,-10.8836393923832)) ;
#107180 = CARTESIAN_POINT('',(8.5,6.66256607592813,-10.7002872911617)) ;
#107181 = CARTESIAN_POINT('Origin',(8.5,6.65133313785406,-10.8970100509337)) ;
#107182 = CARTESIAN_POINT('',(8.5,8.20007071090457,-10.7002872911617)) ;
#107183 = CARTESIAN_POINT('Origin',(8.5,4.35421736843756,-9.535)) ;
#107184 = CARTESIAN_POINT('',(9.91643989873054,6.8847127088383,-9.29892668354491)) ;
#107185 = CARTESIAN_POINT('',(8.58356010126947,6.66256607592813,-9.52107331645509)) ;
#107186 = CARTESIAN_POINT('',(8.48442535909739,6.64604361889945,-9.53759577348377)) ;
#107187 = CARTESIAN_POINT('',(8.58356010126947,8.20007071090456,-9.52107331645509)) ;
#107188 = CARTESIAN_POINT('',(9.91643989873054,7.72792407799439,-9.29892668354491)) ;
#107189 = CARTESIAN_POINT('',(9.97075240319158,7.70981990984071,-9.28987459946807)) ;
#107190 = CARTESIAN_POINT('',(9.91643989873054,6.8,-9.29892668354491)) ;
#107191 = CARTESIAN_POINT('Origin',(8.5,3.65,-9.66)) ;
#107192 = CARTESIAN_POINT('',(8.45734623443633,3.62014236410543,-10.0620655561573)) ;
#107193 = CARTESIAN_POINT('',(8.02582401135442,3.3180768079481,-9.76)) ;
#107194 = CARTESIAN_POINT('',(8.34729988159781,3.54310991711847,-9.98503310917037)) ;
#107195 = CARTESIAN_POINT('',(8.02582401135442,3.31807680794809,-10.56)) ;
#107196 = CARTESIAN_POINT('',(8.02582401135442,3.3180768079481,-9.66)) ;
#107197 = CARTESIAN_POINT('',(8.45734623443633,3.62014236410543,-10.2579344438427)) ;
#107198 = CARTESIAN_POINT('',(8.70083523513316,3.79058466459322,-10.0874921433549)) ;
#107199 = CARTESIAN_POINT('',(8.45734623443633,3.62014236410543,-9.66)) ;
#107200 = CARTESIAN_POINT('Origin',(8.5,3.95,-9.66)) ;
#107201 = CARTESIAN_POINT('',(8.5,3.89793444384266,-10.2579344438427)) ;
#107202 = CARTESIAN_POINT('',(8.5,3.89793444384266,-10.0620655561573)) ;
#107203 = CARTESIAN_POINT('',(8.5,3.89793444384266,-9.66)) ;
#107204 = CARTESIAN_POINT('',(8.5,3.70206555615734,-10.0620655561573)) ;
#107205 = CARTESIAN_POINT('',(8.5,3.95,-10.0620655561573)) ;
#107206 = CARTESIAN_POINT('',(8.5,3.70206555615734,-10.2579344438427)) ;
#107207 = CARTESIAN_POINT('',(8.5,3.70206555615734,-9.66)) ;
#107208 = CARTESIAN_POINT('',(8.5,3.95,-10.2579344438427)) ;
#107209 = CARTESIAN_POINT('Origin',(8.,4.3,-9.66)) ;
#107210 = CARTESIAN_POINT('',(8.45734623443633,3.97985763589457,-10.2579344438427)) ;
#107211 = CARTESIAN_POINT('',(8.02582401135442,4.2819231920519,-10.56)) ;
#107212 = CARTESIAN_POINT('',(8.32457260887054,4.07279917379062,-10.3508759817387)) ;
#107213 = CARTESIAN_POINT('',(8.02582401135442,4.2819231920519,-9.76)) ;
#107214 = CARTESIAN_POINT('',(8.02582401135442,4.2819231920519,-9.66)) ;
#107215 = CARTESIAN_POINT('',(8.45734623443633,3.97985763589457,-10.0620655561573)) ;
#107216 = CARTESIAN_POINT('',(7.97103725533518,4.32027392126537,-9.72164927078653)) ;
#107217 = CARTESIAN_POINT('',(8.45734623443633,3.97985763589457,-9.66)) ;
#107218 = CARTESIAN_POINT('Origin',(1.5,2.3,-9.66)) ;
#107219 = CARTESIAN_POINT('',(7.96847777691809,3.4,-9.66)) ;
#107220 = CARTESIAN_POINT('',(8.,3.4,-9.66)) ;
#107221 = CARTESIAN_POINT('',(7.96847777691809,4.2,-9.66)) ;
#107222 = CARTESIAN_POINT('',(7.96847777691809,4.2,-9.66)) ;
#107223 = CARTESIAN_POINT('',(3.,4.2,-9.66)) ;
#107224 = CARTESIAN_POINT('Origin',(1.5,2.3,-10.66)) ;
#107225 = CARTESIAN_POINT('',(7.96847777691809,4.2,-10.66)) ;
#107226 = CARTESIAN_POINT('',(1.5,4.2,-10.66)) ;
#107227 = CARTESIAN_POINT('',(7.96847777691809,3.4,-10.66)) ;
#107228 = CARTESIAN_POINT('',(7.96847777691809,2.3,-10.66)) ;
#107229 = CARTESIAN_POINT('',(1.5,3.4,-10.66)) ;
#107230 = CARTESIAN_POINT('Origin',(8.,3.3,-9.66)) ;
#107231 = CARTESIAN_POINT('',(7.96847777691809,3.3,-10.56)) ;
#107232 = CARTESIAN_POINT('',(8.,3.3,-10.56)) ;
#107233 = CARTESIAN_POINT('',(7.96847777691809,3.3,-9.76)) ;
#107234 = CARTESIAN_POINT('',(7.96847777691809,3.3,-9.66)) ;
#107235 = CARTESIAN_POINT('',(3.,3.3,-9.76)) ;
#107236 = CARTESIAN_POINT('Origin',(1.5,4.3,-9.66)) ;
#107237 = CARTESIAN_POINT('',(7.96847777691809,4.3,-9.76)) ;
#107238 = CARTESIAN_POINT('',(8.,4.3,-9.76)) ;
#107239 = CARTESIAN_POINT('',(7.96847777691809,4.3,-10.56)) ;
#107240 = CARTESIAN_POINT('',(7.96847777691809,4.3,-9.66)) ;
#107241 = CARTESIAN_POINT('',(1.5,4.3,-10.56)) ;
#107242 = CARTESIAN_POINT('Origin',(1.5,2.3,-9.66)) ;
#107243 = CARTESIAN_POINT('',(-0.4,2.3,-9.66)) ;
#107244 = CARTESIAN_POINT('',(-0.4,-3.36847777691809,-9.66)) ;
#107245 = CARTESIAN_POINT('',(-0.4,-3.4,-9.66)) ;
#107246 = CARTESIAN_POINT('',(0.4,-3.36847777691809,-9.66)) ;
#107247 = CARTESIAN_POINT('',(0.4,-3.36847777691809,-9.66)) ;
#107248 = CARTESIAN_POINT('',(0.4,2.29999999999999,-9.66)) ;
#107249 = CARTESIAN_POINT('',(0.4,2.29999999999999,-9.66)) ;
#107250 = CARTESIAN_POINT('',(0.536602540378444,2.83090991212703,-9.66)) ;
#107251 = CARTESIAN_POINT('Origin',(1.5,2.3,-9.66)) ;
#107252 = CARTESIAN_POINT('',(0.536602540378444,3.93764017256378,-9.66)) ;
#107253 = CARTESIAN_POINT('',(0.536602540378444,2.83090991212703,-9.66)) ;
#107254 = CARTESIAN_POINT('Origin',(1.5,2.3,-9.66)) ;
#107255 = CARTESIAN_POINT('Origin',(1.5,2.3,-10.66)) ;
#107256 = CARTESIAN_POINT('',(0.4,2.29999999999999,-10.66)) ;
#107257 = CARTESIAN_POINT('',(0.4,-3.36847777691809,-10.66)) ;
#107258 = CARTESIAN_POINT('',(0.4,2.3,-10.66)) ;
#107259 = CARTESIAN_POINT('',(-0.4,-3.36847777691809,-10.66)) ;
#107260 = CARTESIAN_POINT('',(1.5,-3.36847777691809,-10.66)) ;
#107261 = CARTESIAN_POINT('',(-0.4,2.3,-10.66)) ;
#107262 = CARTESIAN_POINT('',(-0.4,2.3,-10.66)) ;
#107263 = CARTESIAN_POINT('',(0.536602540378444,3.93764017256378,-10.66)) ;
#107264 = CARTESIAN_POINT('Origin',(1.5,2.3,-10.66)) ;
#107265 = CARTESIAN_POINT('',(0.536602540378444,2.83090991212703,-10.66)) ;
#107266 = CARTESIAN_POINT('',(0.536602540378444,3.93764017256378,-10.66)) ;
#107267 = CARTESIAN_POINT('Origin',(1.5,2.3,-10.66)) ;
#107268 = CARTESIAN_POINT('Origin',(1.5,2.3,-9.66)) ;
#107269 = CARTESIAN_POINT('',(-0.5,2.3,-9.76)) ;
#107270 = CARTESIAN_POINT('',(-0.5,2.3,-10.56)) ;
#107271 = CARTESIAN_POINT('',(-0.5,2.3,-9.66)) ;
#107272 = CARTESIAN_POINT('Origin',(1.5,2.3,-9.76)) ;
#107273 = CARTESIAN_POINT('Origin',(1.5,2.3,-10.56)) ;
#107274 = CARTESIAN_POINT('Origin',(-0.5,-3.4,-9.66)) ;
#107275 = CARTESIAN_POINT('',(-0.5,-3.36847777691809,-10.56)) ;
#107276 = CARTESIAN_POINT('',(-0.5,-3.4,-10.56)) ;
#107277 = CARTESIAN_POINT('',(-0.5,-3.36847777691809,-9.76)) ;
#107278 = CARTESIAN_POINT('',(-0.5,-3.36847777691809,-9.66)) ;
#107279 = CARTESIAN_POINT('',(-0.5,2.3,-9.76)) ;
#107280 = CARTESIAN_POINT('Origin',(-0.15,-3.9,-9.66)) ;
#107281 = CARTESIAN_POINT('',(-0.179857635894567,-3.85734623443633,-10.0620655561573)) ;
#107282 = CARTESIAN_POINT('',(-0.481923192051905,-3.42582401135442,-9.76)) ;
#107283 = CARTESIAN_POINT('',(-0.256890082881532,-3.74729988159781,-9.98503310917037)) ;
#107284 = CARTESIAN_POINT('',(-0.481923192051905,-3.42582401135442,-10.56)) ;
#107285 = CARTESIAN_POINT('',(-0.481923192051905,-3.42582401135442,-9.66)) ;
#107286 = CARTESIAN_POINT('',(-0.179857635894567,-3.85734623443633,-10.2579344438427)) ;
#107287 = CARTESIAN_POINT('',(-0.00941533540678435,-4.10083523513317,-10.0874921433549)) ;
#107288 = CARTESIAN_POINT('',(-0.179857635894567,-3.85734623443633,-9.66)) ;
#107289 = CARTESIAN_POINT('Origin',(0.15,-3.9,-9.66)) ;
#107290 = CARTESIAN_POINT('',(0.0979344438426627,-3.9,-10.2579344438427)) ;
#107291 = CARTESIAN_POINT('',(0.0979344438426627,-3.9,-10.0620655561573)) ;
#107292 = CARTESIAN_POINT('',(0.0979344438426627,-3.9,-9.66)) ;
#107293 = CARTESIAN_POINT('',(-0.0979344438426628,-3.9,-10.0620655561573)) ;
#107294 = CARTESIAN_POINT('',(0.15,-3.9,-10.0620655561573)) ;
#107295 = CARTESIAN_POINT('',(-0.0979344438426628,-3.9,-10.2579344438427)) ;
#107296 = CARTESIAN_POINT('',(-0.0979344438426628,-3.9,-9.66)) ;
#107297 = CARTESIAN_POINT('',(0.15,-3.9,-10.2579344438427)) ;
#107298 = CARTESIAN_POINT('Origin',(0.5,-3.4,-9.66)) ;
#107299 = CARTESIAN_POINT('',(0.179857635894567,-3.85734623443633,-10.2579344438427)) ;
#107300 = CARTESIAN_POINT('',(0.481923192051904,-3.42582401135442,-10.56)) ;
#107301 = CARTESIAN_POINT('',(0.272799173790623,-3.72457260887054,-10.3508759817387)) ;
#107302 = CARTESIAN_POINT('',(0.481923192051904,-3.42582401135442,-9.76)) ;
#107303 = CARTESIAN_POINT('',(0.481923192051904,-3.42582401135442,-9.66)) ;
#107304 = CARTESIAN_POINT('',(0.179857635894567,-3.85734623443633,-10.0620655561573)) ;
#107305 = CARTESIAN_POINT('',(0.520273921265371,-3.37103725533519,-9.72164927078653)) ;
#107306 = CARTESIAN_POINT('',(0.179857635894567,-3.85734623443633,-9.66)) ;
#107307 = CARTESIAN_POINT('Origin',(0.5,2.29999999999999,-9.66)) ;
#107308 = CARTESIAN_POINT('',(0.500000000000001,2.29999999999999,-9.76)) ;
#107309 = CARTESIAN_POINT('',(0.5,-3.36847777691809,-9.76)) ;
#107310 = CARTESIAN_POINT('',(0.5,-3.4,-9.76)) ;
#107311 = CARTESIAN_POINT('',(0.5,-3.36847777691809,-10.56)) ;
#107312 = CARTESIAN_POINT('',(0.5,-3.36847777691809,-9.66)) ;
#107313 = CARTESIAN_POINT('',(0.500000000000001,2.29999999999999,-10.56)) ;
#107314 = CARTESIAN_POINT('',(0.5,2.29999999999999,-10.56)) ;
#107315 = CARTESIAN_POINT('',(0.500000000000001,2.29999999999999,-9.66)) ;
#107316 = CARTESIAN_POINT('Origin',(1.5,2.3,-9.66)) ;
#107317 = CARTESIAN_POINT('Origin',(1.5,2.3,-9.76)) ;
#107318 = CARTESIAN_POINT('Origin',(1.5,2.3,-10.56)) ;
#107319 = CARTESIAN_POINT('Origin',(8.,2.68967221921331,-10.66)) ;
#107320 = CARTESIAN_POINT('',(8.45734623443633,3.70206555615734,-10.3398576358946)) ;
#107321 = CARTESIAN_POINT('',(8.02582401135442,3.4,-10.6419231920519)) ;
#107322 = CARTESIAN_POINT('',(7.75526480758232,3.21060855735952,-10.8313146346924)) ;
#107323 = CARTESIAN_POINT('',(8.02582401135442,4.2,-10.6419231920519)) ;
#107324 = CARTESIAN_POINT('',(8.02582401135442,2.68967221921331,-10.6419231920519)) ;
#107325 = CARTESIAN_POINT('',(8.45734623443633,3.89793444384266,-10.3398576358946)) ;
#107326 = CARTESIAN_POINT('',(8.54034505662341,3.83983526831171,-10.2817584603636)) ;
#107327 = CARTESIAN_POINT('',(8.45734623443633,2.68967221921331,-10.3398576358946)) ;
#107328 = CARTESIAN_POINT('Origin',(8.,2.68967221921331,-9.66)) ;
#107329 = CARTESIAN_POINT('',(8.45734623443633,3.89793444384266,-9.98014236410544)) ;
#107330 = CARTESIAN_POINT('',(8.02582401135442,4.2,-9.6780768079481)) ;
#107331 = CARTESIAN_POINT('',(8.54034505662341,3.83983526831171,-10.0382415396364)) ;
#107332 = CARTESIAN_POINT('',(8.02582401135442,3.4,-9.6780768079481)) ;
#107333 = CARTESIAN_POINT('',(8.02582401135442,3.4,-9.6780768079481)) ;
#107334 = CARTESIAN_POINT('',(8.45734623443633,3.70206555615734,-9.98014236410544)) ;
#107335 = CARTESIAN_POINT('',(7.75526480758232,3.21060855735952,-9.48868536530762)) ;
#107336 = CARTESIAN_POINT('',(8.45734623443633,2.68967221921331,-9.98014236410544)) ;
#107337 = CARTESIAN_POINT('Origin',(-1.11032778078669,-3.9,-10.01)) ;
#107338 = CARTESIAN_POINT('',(0.0979344438426626,-3.85734623443633,-9.98014236410544)) ;
#107339 = CARTESIAN_POINT('',(0.4,-3.42582401135442,-9.6780768079481)) ;
#107340 = CARTESIAN_POINT('',(-0.223548570072128,-4.31660768288603,-10.3016253780202)) ;
#107341 = CARTESIAN_POINT('',(-0.400000000000001,-3.42582401135442,-9.6780768079481)) ;
#107342 = CARTESIAN_POINT('',(-0.400000000000001,-3.42582401135442,-9.6780768079481)) ;
#107343 = CARTESIAN_POINT('',(-0.0979344438426627,-3.85734623443633,-9.98014236410544)) ;
#107344 = CARTESIAN_POINT('',(-0.326007604256636,-3.53152743384494,-9.75206920369146)) ;
#107345 = CARTESIAN_POINT('',(-1.11032778078669,-3.85734623443633,-9.98014236410544)) ;
#107346 = CARTESIAN_POINT('Origin',(-1.11032778078669,-3.4,-10.66)) ;
#107347 = CARTESIAN_POINT('',(-0.0979344438426627,-3.85734623443633,-10.3398576358946)) ;
#107348 = CARTESIAN_POINT('',(-0.4,-3.42582401135442,-10.6419231920519)) ;
#107349 = CARTESIAN_POINT('',(-0.589391442640475,-3.15526480758232,-10.8313146346924)) ;
#107350 = CARTESIAN_POINT('',(0.400000000000001,-3.42582401135442,-10.6419231920519)) ;
#107351 = CARTESIAN_POINT('',(-1.11032778078669,-3.42582401135442,-10.6419231920519)) ;
#107352 = CARTESIAN_POINT('',(0.0979344438426626,-3.85734623443633,-10.3398576358946)) ;
#107353 = CARTESIAN_POINT('',(0.0398352683117103,-3.94034505662341,-10.2817584603636)) ;
#107354 = CARTESIAN_POINT('',(-1.11032778078669,-3.85734623443633,-10.3398576358946)) ;
#107355 = CARTESIAN_POINT('Origin',(10.,1.24999999999998,-12.7)) ;
#107356 = CARTESIAN_POINT('',(9.91643989873054,1.26392668354489,-8.1158381198218)) ;
#107357 = CARTESIAN_POINT('',(9.91643989873054,1.26392668354489,-12.7)) ;
#107358 = CARTESIAN_POINT('',(8.50816364570057,1.49863939238321,-8.19785831296513)) ;
#107359 = CARTESIAN_POINT('Origin',(43.705291680055,-4.36754861360758,-616.848202367929)) ;
#107360 = CARTESIAN_POINT('',(8.50816364570057,1.49863939238321,-12.7)) ;
#107361 = CARTESIAN_POINT('Origin',(8.49999999999985,3.8,-10.16)) ;
#107362 = CARTESIAN_POINT('',(9.91643989873053,1.24322097942674,-8.17630356419405)) ;
#107363 = CARTESIAN_POINT('',(9.91643989873053,1.24322097942648,-12.1436964358056)) ;
#107364 = CARTESIAN_POINT('Origin',(9.91643989873053,3.8,-10.16)) ;
#107365 = CARTESIAN_POINT('Origin',(36.548065263586,-40.3802619823314,562.117654689231)) ;
#107366 = CARTESIAN_POINT('Origin',(36.5480653710647,-40.3802615702808,-582.437655339515)) ;
#107367 = CARTESIAN_POINT('Origin',(10.,1.24999999999998,-12.7)) ;
#107368 = CARTESIAN_POINT('',(8.50816364570059,1.49863939238321,-12.1221416870347)) ;
#107369 = CARTESIAN_POINT('',(8.50816364570057,1.49863939238321,-12.7)) ;
#107370 = CARTESIAN_POINT('',(9.91643989873054,1.26392668354489,-12.2041618801782)) ;
#107371 = CARTESIAN_POINT('Origin',(43.7052916277413,-4.36754860543838,596.528201456572)) ;
#107372 = CARTESIAN_POINT('',(9.91643989873054,1.26392668354489,-12.7)) ;
#107373 = CARTESIAN_POINT('Origin',(-0.900000000000001,4.65,-10.16)) ;
#107374 = CARTESIAN_POINT('Origin',(-0.900000000000001,4.65,-8.5168323274845)) ;
#107375 = CARTESIAN_POINT('Origin',(-0.900000000000001,4.65,-8.5168323274845)) ;
#107376 = CARTESIAN_POINT('Origin',(-0.900000000000001,4.65,-8.5168323274845)) ;
#107377 = CARTESIAN_POINT('Origin',(-0.900000000000001,4.65,-8.5168323274845)) ;
#107378 = CARTESIAN_POINT('Origin',(1.15,4.45,-8.57886116991581)) ;
#107379 = CARTESIAN_POINT('Origin',(1.15,4.45,-8.5168323274845)) ;
#107380 = CARTESIAN_POINT('Origin',(-1.,4.65,-8.5168323274845)) ;
#107381 = CARTESIAN_POINT('Origin',(1.15,4.65,-8.5168323274845)) ;
#107382 = CARTESIAN_POINT('Origin',(-0.900000000000001,3.8,-10.16)) ;
#107383 = CARTESIAN_POINT('Origin',(-0.900000000000001,5.4431676725155,-9.31)) ;
#107384 = CARTESIAN_POINT('Origin',(1.15,4.65,-8.5168323274845)) ;
#107385 = CARTESIAN_POINT('Origin',(1.15,4.55810810810811,-8.69447207586456)) ;
#107386 = CARTESIAN_POINT('Origin',(-0.900000000000001,5.4431676725155,-9.31)) ;
#107387 = CARTESIAN_POINT('Origin',(-0.900000000000001,5.4431676725155,-9.31)) ;
#107388 = CARTESIAN_POINT('Origin',(-0.900000000000001,5.4431676725155,-9.31)) ;
#107389 = CARTESIAN_POINT('Origin',(-0.900000000000001,4.65,-10.16)) ;
#107390 = CARTESIAN_POINT('Origin',(-0.900000000000001,4.65,-11.8031676725155)) ;
#107391 = CARTESIAN_POINT('Origin',(-1.,4.65,-11.8031676725155)) ;
#107392 = CARTESIAN_POINT('Origin',(1.15,4.65,-11.8031676725155)) ;
#107393 = CARTESIAN_POINT('Origin',(-0.900000000000001,4.65,-11.8031676725155)) ;
#107394 = CARTESIAN_POINT('Origin',(1.15,4.45,-11.7411388300842)) ;
#107395 = CARTESIAN_POINT('Origin',(1.15,4.45,-11.8031676725155)) ;
#107396 = CARTESIAN_POINT('Origin',(1.15,3.8,-10.16)) ;
#107397 = CARTESIAN_POINT('Origin',(1.15,5.26552792413544,-9.40189189189189)) ;
#107398 = CARTESIAN_POINT('Origin',(-1.,5.4431676725155,-9.31)) ;
#107399 = CARTESIAN_POINT('Origin',(1.15,5.4431676725155,-9.31)) ;
#107400 = CARTESIAN_POINT('Origin',(-0.900000000000001,3.8,-9.31)) ;
#107401 = CARTESIAN_POINT('Origin',(-0.9,6.45,-9.31)) ;
#107402 = CARTESIAN_POINT('Origin',(-0.9,6.45,-10.16)) ;
#107403 = CARTESIAN_POINT('Origin',(-0.9,6.45,-9.31)) ;
#107404 = CARTESIAN_POINT('Origin',(-0.900000000000001,4.65,-11.8031676725155)) ;
#107405 = CARTESIAN_POINT('Origin',(-0.900000000000001,4.65,-11.8031676725155)) ;
#107406 = CARTESIAN_POINT('Origin',(1.15,4.65,-11.8031676725155)) ;
#107407 = CARTESIAN_POINT('Origin',(1.15,4.55810810810811,-11.6255279241354)) ;
#107408 = CARTESIAN_POINT('Origin',(1.15,5.4431676725155,-9.31)) ;
#107409 = CARTESIAN_POINT('Origin',(1.15,5.4431676725155,-9.51)) ;
#107410 = CARTESIAN_POINT('Origin',(-0.9,6.45,-9.31)) ;
#107411 = CARTESIAN_POINT('Origin',(-0.9,6.45,-9.31)) ;
#107412 = CARTESIAN_POINT('Origin',(-0.900000000000001,3.8,-10.16)) ;
#107413 = CARTESIAN_POINT('Origin',(-0.900000000000001,5.4431676725155,-11.01)) ;
#107414 = CARTESIAN_POINT('Origin',(-1.,5.4431676725155,-11.01)) ;
#107415 = CARTESIAN_POINT('Origin',(1.15,5.4431676725155,-11.01)) ;
#107416 = CARTESIAN_POINT('Origin',(-0.900000000000001,5.4431676725155,-11.01)) ;
#107417 = CARTESIAN_POINT('Origin',(1.15,3.8,-10.16)) ;
#107418 = CARTESIAN_POINT('Origin',(1.15,5.26552792413544,-10.9181081081081)) ;
#107419 = CARTESIAN_POINT('Origin',(1.15,6.55,-9.51)) ;
#107420 = CARTESIAN_POINT('Origin',(1.15,6.45,-9.51)) ;
#107421 = CARTESIAN_POINT('Origin',(1.25,6.45,-9.31)) ;
#107422 = CARTESIAN_POINT('Origin',(1.15,6.45,-9.31)) ;
#107423 = CARTESIAN_POINT('Origin',(-0.900000000000001,5.4431676725155,-11.01)) ;
#107424 = CARTESIAN_POINT('Origin',(-0.900000000000001,5.4431676725155,-11.01)) ;
#107425 = CARTESIAN_POINT('Origin',(1.15,5.4431676725155,-11.01)) ;
#107426 = CARTESIAN_POINT('Origin',(1.15,5.4431676725155,-10.81)) ;
#107427 = CARTESIAN_POINT('Origin',(1.15,6.45,-9.51)) ;
#107428 = CARTESIAN_POINT('Origin',(1.35,6.45,-9.51)) ;
#107429 = CARTESIAN_POINT('Origin',(-0.9,6.45,-10.16)) ;
#107430 = CARTESIAN_POINT('Origin',(-0.9,6.45,-11.01)) ;
#107431 = CARTESIAN_POINT('Origin',(-0.900000000000001,3.8,-11.01)) ;
#107432 = CARTESIAN_POINT('Origin',(-0.9,6.45,-11.01)) ;
#107433 = CARTESIAN_POINT('Origin',(1.15,6.55,-10.81)) ;
#107434 = CARTESIAN_POINT('Origin',(1.15,6.45,-10.81)) ;
#107435 = CARTESIAN_POINT('Origin',(1.35,6.45,-12.7)) ;
#107436 = CARTESIAN_POINT('Origin',(1.35,6.45,-10.81)) ;
#107437 = CARTESIAN_POINT('Origin',(-0.9,6.45,-11.01)) ;
#107438 = CARTESIAN_POINT('Origin',(-0.9,6.45,-11.01)) ;
#107439 = CARTESIAN_POINT('Origin',(1.15,6.45,-10.81)) ;
#107440 = CARTESIAN_POINT('Origin',(1.15,6.45,-11.01)) ;
#107441 = CARTESIAN_POINT('Origin',(-1.,6.45,-11.01)) ;
#107442 = CARTESIAN_POINT('Origin',(-1.7,0.3,-10.81)) ;
#107443 = CARTESIAN_POINT('Origin',(-1.7,0.3,-10.81)) ;
#107444 = CARTESIAN_POINT('Origin',(-1.7,0.3,-10.81)) ;
#107445 = CARTESIAN_POINT('Origin',(-1.7,0.3,-10.81)) ;
#107446 = CARTESIAN_POINT('Origin',(0.549999999999999,0.3,-10.81)) ;
#107447 = CARTESIAN_POINT('',(0.50857864376269,0.229289321881345,-10.7392893218813)) ;
#107448 = CARTESIAN_POINT('Ctrl Pts',(0.65,0.200000000000001,-10.81)) ;
#107449 = CARTESIAN_POINT('Ctrl Pts',(0.639834283464158,0.200000000000001,
-10.8049171417321)) ;
#107450 = CARTESIAN_POINT('Ctrl Pts',(0.629316849080552,0.200389688120421,
-10.799657683858)) ;
#107451 = CARTESIAN_POINT('Ctrl Pts',(0.606957334719714,0.202165884217636,
-10.7884679497194)) ;
#107452 = CARTESIAN_POINT('Ctrl Pts',(0.595086727401161,0.203647820493433,
-10.782522761795)) ;
#107453 = CARTESIAN_POINT('Ctrl Pts',(0.572283837383465,0.207685608830711,
-10.7711067603976)) ;
#107454 = CARTESIAN_POINT('Ctrl Pts',(0.561337481656325,0.210178193246981,
-10.765629861311)) ;
#107455 = CARTESIAN_POINT('Ctrl Pts',(0.549549942891011,0.213544620663898,
-10.7597406960422)) ;
#107456 = CARTESIAN_POINT('Ctrl Pts',(0.548290718948482,0.213913346521136,
-10.7591116827675)) ;
#107457 = CARTESIAN_POINT('Ctrl Pts',(0.536119229732729,0.217566912232509,
-10.7530327513518)) ;
#107458 = CARTESIAN_POINT('Ctrl Pts',(0.525706917362472,0.221400308602604,
-10.7478422384291)) ;
#107459 = CARTESIAN_POINT('Ctrl Pts',(0.513545110027223,0.226871185484677,
-10.7417711869643)) ;
#107460 = CARTESIAN_POINT('Ctrl Pts',(0.511029334128303,0.228063976698517,
-10.7405146670642)) ;
#107461 = CARTESIAN_POINT('Ctrl Pts',(0.50857864376269,0.229289321881369,
-10.7392893218813)) ;
#107462 = CARTESIAN_POINT('Origin',(0.664280054289791,0.302990743360187,-10.8171421042438)) ;
#107463 = CARTESIAN_POINT('Origin',(-1.7,4.5,-10.81)) ;
#107464 = CARTESIAN_POINT('',(-1.77071067811864,4.45857864376272,-10.7392893218813)) ;
#107465 = CARTESIAN_POINT('Origin',(-1.69703459697676,4.61417009504429,-10.8170866853763)) ;
#107466 = CARTESIAN_POINT('Ctrl Pts',(-1.77071067811862,4.45857864376272,
-10.7392893218813)) ;
#107467 = CARTESIAN_POINT('Ctrl Pts',(-1.77521675558369,4.46759079869279,
-10.7437953993464)) ;
#107468 = CARTESIAN_POINT('Ctrl Pts',(-1.77928079264421,4.47748625817292,
-10.7487264816716)) ;
#107469 = CARTESIAN_POINT('Ctrl Pts',(-1.78624680748783,4.49811277057336,
-10.7590208825501)) ;
#107470 = CARTESIAN_POINT('Ctrl Pts',(-1.78918030782056,4.50880509434443,
-10.7643639841539)) ;
#107471 = CARTESIAN_POINT('Ctrl Pts',(-1.79185985500503,4.52101859323025,
-10.7704747545378)) ;
#107472 = CARTESIAN_POINT('Ctrl Pts',(-1.7921304506133,4.52228751723201,-10.7711097099114)) ;
#107473 = CARTESIAN_POINT('Ctrl Pts',(-1.7947746790983,4.53504937002863,-10.777496289134)) ;
#107474 = CARTESIAN_POINT('Ctrl Pts',(-1.79657370273653,4.54677936428204,
-10.7833715724062)) ;
#107475 = CARTESIAN_POINT('Ctrl Pts',(-1.79896007643136,4.56920025888396,
-10.7945957747612)) ;
#107476 = CARTESIAN_POINT('Ctrl Pts',(-1.79963010255188,4.57990192168158,
-10.799950075945)) ;
#107477 = CARTESIAN_POINT('Ctrl Pts',(-1.79996164986962,4.593571160343,-10.806785573817)) ;
#107478 = CARTESIAN_POINT('Ctrl Pts',(-1.8,4.59680282631916,-10.8084014131596)) ;
#107479 = CARTESIAN_POINT('Ctrl Pts',(-1.8,4.6,-10.81)) ;
#107480 = CARTESIAN_POINT('Origin',(-1.7,0.3,-10.16)) ;
#107481 = CARTESIAN_POINT('Origin',(-1.7,0.3,-11.56)) ;
#107482 = CARTESIAN_POINT('Origin',(0.65,0.3,-10.16)) ;
#107483 = CARTESIAN_POINT('',(0.579289321881328,0.229289321881363,-10.6685786437627)) ;
#107484 = CARTESIAN_POINT('Origin',(0.657086685372617,0.30296540302162,-10.8241700950363)) ;
#107485 = CARTESIAN_POINT('Ctrl Pts',(0.579289321881328,0.229289321881363,
-10.6685786437627)) ;
#107486 = CARTESIAN_POINT('Ctrl Pts',(0.583795399346358,0.22478324441633,
-10.6775907986928)) ;
#107487 = CARTESIAN_POINT('Ctrl Pts',(0.588726481671642,0.220719207355776,
-10.6874862581729)) ;
#107488 = CARTESIAN_POINT('Ctrl Pts',(0.599020882547812,0.213753192513727,
-10.7081127705688)) ;
#107489 = CARTESIAN_POINT('Ctrl Pts',(0.604363984149138,0.21081969218206,
-10.7188050943348)) ;
#107490 = CARTESIAN_POINT('Ctrl Pts',(0.610474754532864,0.208140144997068,
-10.7310185932204)) ;
#107491 = CARTESIAN_POINT('Ctrl Pts',(0.611109709908962,0.20786954938772,
-10.7322875172271)) ;
#107492 = CARTESIAN_POINT('Ctrl Pts',(0.617496289133932,0.205225320901711,
-10.7450493700286)) ;
#107493 = CARTESIAN_POINT('Ctrl Pts',(0.623371572406165,0.203426297263479,
-10.756779364282)) ;
#107494 = CARTESIAN_POINT('Ctrl Pts',(0.634595774761169,0.201039923568646,
-10.7792002588839)) ;
#107495 = CARTESIAN_POINT('Ctrl Pts',(0.639950075944996,0.200369897448124,
-10.7899019216815)) ;
#107496 = CARTESIAN_POINT('Ctrl Pts',(0.646785573817028,0.200038350130376,
-10.803571160343)) ;
#107497 = CARTESIAN_POINT('Ctrl Pts',(0.648401413159574,0.2,-10.8068028263192)) ;
#107498 = CARTESIAN_POINT('Ctrl Pts',(0.65,0.2,-10.81)) ;
#107499 = CARTESIAN_POINT('',(0.579289321881328,0.229289321881363,-9.65142135623727)) ;
#107500 = CARTESIAN_POINT('Ctrl Pts',(0.65,0.2,-9.51)) ;
#107501 = CARTESIAN_POINT('Ctrl Pts',(0.644917141732078,0.2,-9.52016571653583)) ;
#107502 = CARTESIAN_POINT('Ctrl Pts',(0.639657683858005,0.200389688120423,
-9.53068315091943)) ;
#107503 = CARTESIAN_POINT('Ctrl Pts',(0.628467949719355,0.202165884217645,
-9.55304266528024)) ;
#107504 = CARTESIAN_POINT('Ctrl Pts',(0.622522761794952,0.203647820493437,
-9.56491327259877)) ;
#107505 = CARTESIAN_POINT('Ctrl Pts',(0.611106760396028,0.207685608831252,
-9.58771616261943)) ;
#107506 = CARTESIAN_POINT('Ctrl Pts',(0.605629861308049,0.210178193248326,
-9.59866251834949)) ;
#107507 = CARTESIAN_POINT('Ctrl Pts',(0.599740696039329,0.213544620665554,
-9.61045005711456)) ;
#107508 = CARTESIAN_POINT('Ctrl Pts',(0.599111682766057,0.213913346521985,
-9.61170928105426)) ;
#107509 = CARTESIAN_POINT('Ctrl Pts',(0.593032751351777,0.217566912232531,
-9.62388077026723)) ;
#107510 = CARTESIAN_POINT('Ctrl Pts',(0.58784223842912,0.221400308602597,
-9.6342930826375)) ;
#107511 = CARTESIAN_POINT('Ctrl Pts',(0.581771186964294,0.226871185484689,
-9.64645488997275)) ;
#107512 = CARTESIAN_POINT('Ctrl Pts',(0.580514667064131,0.228063976698559,
-9.64897066587166)) ;
#107513 = CARTESIAN_POINT('Ctrl Pts',(0.579289321881328,0.229289321881363,
-9.65142135623727)) ;
#107514 = CARTESIAN_POINT('Origin',(0.657142104258034,0.302990743365752,-9.49571994568188)) ;
#107515 = CARTESIAN_POINT('Origin',(-1.7,4.6,-10.71)) ;
#107516 = CARTESIAN_POINT('',(-1.77071067811866,4.52928932188135,-10.6685786437627)) ;
#107517 = CARTESIAN_POINT('Ctrl Pts',(-1.8,4.6,-10.81)) ;
#107518 = CARTESIAN_POINT('Ctrl Pts',(-1.8,4.59491714173208,-10.7998342834642)) ;
#107519 = CARTESIAN_POINT('Ctrl Pts',(-1.79961031187958,4.58965768385801,
-10.7893168490806)) ;
#107520 = CARTESIAN_POINT('Ctrl Pts',(-1.79783411578236,4.57846794971936,
-10.7669573347197)) ;
#107521 = CARTESIAN_POINT('Ctrl Pts',(-1.79635217950656,4.57252276179495,
-10.7550867274012)) ;
#107522 = CARTESIAN_POINT('Ctrl Pts',(-1.79231439116873,4.56110676039597,
-10.7322838373804)) ;
#107523 = CARTESIAN_POINT('Ctrl Pts',(-1.78982180675163,4.55562986130795,
-10.7213374816503)) ;
#107524 = CARTESIAN_POINT('Ctrl Pts',(-1.78645537933439,4.54974069603923,
-10.7095499428852)) ;
#107525 = CARTESIAN_POINT('Ctrl Pts',(-1.78608665347798,4.549111682766,-10.7082907189456)) ;
#107526 = CARTESIAN_POINT('Ctrl Pts',(-1.78243308776746,4.54303275135177,
-10.6961192297327)) ;
#107527 = CARTESIAN_POINT('Ctrl Pts',(-1.7785996913974,4.53784223842912,-10.6857069173624)) ;
#107528 = CARTESIAN_POINT('Ctrl Pts',(-1.77312881451532,4.5317711869643,-10.6735451100272)) ;
#107529 = CARTESIAN_POINT('Ctrl Pts',(-1.77193602330145,4.53051466706415,
-10.6710293341283)) ;
#107530 = CARTESIAN_POINT('Ctrl Pts',(-1.77071067811866,4.52928932188135,
-10.6685786437627)) ;
#107531 = CARTESIAN_POINT('Origin',(-1.69700925662349,4.60714210428443,-10.8242800543711)) ;
#107532 = CARTESIAN_POINT('',(-1.77071067811866,4.52928932188135,-9.65142135623731)) ;
#107533 = CARTESIAN_POINT('Origin',(-1.69703459696962,4.60708668539217,-9.49582990492436)) ;
#107534 = CARTESIAN_POINT('Ctrl Pts',(-1.77071067811866,4.52928932188135,
-9.65142135623731)) ;
#107535 = CARTESIAN_POINT('Ctrl Pts',(-1.77521675558367,4.53379539934636,
-9.64240920130727)) ;
#107536 = CARTESIAN_POINT('Ctrl Pts',(-1.77928079264422,4.53872648167163,
-9.63251374182715)) ;
#107537 = CARTESIAN_POINT('Ctrl Pts',(-1.7862468074862,4.5490208825477,-9.61188722943147)) ;
#107538 = CARTESIAN_POINT('Ctrl Pts',(-1.78918030781783,4.55436398414893,
-9.60119490566563)) ;
#107539 = CARTESIAN_POINT('Ctrl Pts',(-1.79185985500284,4.56047475453265,
-9.58898140678007)) ;
#107540 = CARTESIAN_POINT('Ctrl Pts',(-1.79213045061223,4.56110970990885,
-9.58771248277321)) ;
#107541 = CARTESIAN_POINT('Ctrl Pts',(-1.79477467909829,4.56749628913393,
-9.57495062997146)) ;
#107542 = CARTESIAN_POINT('Ctrl Pts',(-1.79657370273652,4.57337157240617,
-9.56322063571803)) ;
#107543 = CARTESIAN_POINT('Ctrl Pts',(-1.79896007643136,4.58459577476118,
-9.54079974111609)) ;
#107544 = CARTESIAN_POINT('Ctrl Pts',(-1.79963010255188,4.58995007594501,
-9.53009807831846)) ;
#107545 = CARTESIAN_POINT('Ctrl Pts',(-1.79996164986962,4.59678557381704,
-9.51642883965702)) ;
#107546 = CARTESIAN_POINT('Ctrl Pts',(-1.8,4.59840141315958,-9.51319717368085)) ;
#107547 = CARTESIAN_POINT('Ctrl Pts',(-1.8,4.6,-9.51)) ;
#107548 = CARTESIAN_POINT('Origin',(-1.7,0.3,-11.56)) ;
#107549 = CARTESIAN_POINT('Origin',(-1.7,0.1,-11.56)) ;
#107550 = CARTESIAN_POINT('Origin',(-1.9,0.3,-11.56)) ;
#107551 = CARTESIAN_POINT('Origin',(1.9668402209837E-32,0.1,-11.56)) ;
#107552 = CARTESIAN_POINT('',(0.899999999999999,0.1,-11.66)) ;
#107553 = CARTESIAN_POINT('',(-1.8,0.1,-11.66)) ;
#107554 = CARTESIAN_POINT('Origin',(0.899999999999999,0.1,-11.56)) ;
#107555 = CARTESIAN_POINT('Origin',(0.899999999999999,0.1,-11.56)) ;
#107556 = CARTESIAN_POINT('',(0.999999999999999,0.1,-11.56)) ;
#107557 = CARTESIAN_POINT('Origin',(0.899999999999999,0.1,-11.56)) ;
#107558 = CARTESIAN_POINT('Origin',(0.899999999999999,0.1,-11.56)) ;
#107559 = CARTESIAN_POINT('Origin',(0.549999999999999,0.3,-9.51)) ;
#107560 = CARTESIAN_POINT('',(0.508578643762691,0.229289321881345,-9.58071067811866)) ;
#107561 = CARTESIAN_POINT('Origin',(0.664170095055986,0.302965403025977,-9.50291331461772)) ;
#107562 = CARTESIAN_POINT('Ctrl Pts',(0.50857864376269,0.229289321881343,
-9.58071067811865)) ;
#107563 = CARTESIAN_POINT('Ctrl Pts',(0.517590798692746,0.224783244416322,
-9.57620460065363)) ;
#107564 = CARTESIAN_POINT('Ctrl Pts',(0.527486258172873,0.220719207355776,
-9.57127351832836)) ;
#107565 = CARTESIAN_POINT('Ctrl Pts',(0.548112770568385,0.213753192513845,
-9.56097911745236)) ;
#107566 = CARTESIAN_POINT('Ctrl Pts',(0.558805094334016,0.210819692182259,
-9.55563601585123)) ;
#107567 = CARTESIAN_POINT('Ctrl Pts',(0.571018593219555,0.208140144997224,
-9.5495252454675)) ;
#107568 = CARTESIAN_POINT('Ctrl Pts',(0.572287517226615,0.207869549387789,
-9.54889029009121)) ;
#107569 = CARTESIAN_POINT('Ctrl Pts',(0.585049370028563,0.205225320901693,
-9.54250371086602)) ;
#107570 = CARTESIAN_POINT('Ctrl Pts',(0.596779364281993,0.203426297263461,
-9.53662842759377)) ;
#107571 = CARTESIAN_POINT('Ctrl Pts',(0.619200258883917,0.201039923568636,
-9.52540422523876)) ;
#107572 = CARTESIAN_POINT('Ctrl Pts',(0.629901921681539,0.20036989744812,
-9.52004992405495)) ;
#107573 = CARTESIAN_POINT('Ctrl Pts',(0.643571160342975,0.200038350130376,
-9.51321442618296)) ;
#107574 = CARTESIAN_POINT('Ctrl Pts',(0.646802826319151,0.200000000000001,
-9.51159858684042)) ;
#107575 = CARTESIAN_POINT('Ctrl Pts',(0.65,0.200000000000001,-9.51)) ;
#107576 = CARTESIAN_POINT('Origin',(-1.7,0.3,-9.51)) ;
#107577 = CARTESIAN_POINT('Origin',(-1.7,4.5,-9.51)) ;
#107578 = CARTESIAN_POINT('',(-1.77071067811864,4.45857864376272,-9.58071067811867)) ;
#107579 = CARTESIAN_POINT('Ctrl Pts',(-1.8,4.6,-9.51)) ;
#107580 = CARTESIAN_POINT('Ctrl Pts',(-1.8,4.58983428346417,-9.51508285826792)) ;
#107581 = CARTESIAN_POINT('Ctrl Pts',(-1.79961031187958,4.57931684908058,
-9.52034231614199)) ;
#107582 = CARTESIAN_POINT('Ctrl Pts',(-1.79783411578236,4.55695733471976,
-9.53153205028064)) ;
#107583 = CARTESIAN_POINT('Ctrl Pts',(-1.79635217950656,4.54508672740121,
-9.53747723820505)) ;
#107584 = CARTESIAN_POINT('Ctrl Pts',(-1.7923143911688,4.52228383738083,-9.54889323960384)) ;
#107585 = CARTESIAN_POINT('Ctrl Pts',(-1.7898218067518,4.51133748165105,-9.55437013869168)) ;
#107586 = CARTESIAN_POINT('Ctrl Pts',(-1.7864553793346,4.49954994288596,-9.56025930396041)) ;
#107587 = CARTESIAN_POINT('Ctrl Pts',(-1.78608665347809,4.49829071894599,
-9.56088831723382)) ;
#107588 = CARTESIAN_POINT('Ctrl Pts',(-1.78243308776746,4.48611922973275,
-9.56696724864823)) ;
#107589 = CARTESIAN_POINT('Ctrl Pts',(-1.7785996913974,4.47570691736247,-9.57215776157089)) ;
#107590 = CARTESIAN_POINT('Ctrl Pts',(-1.77312881451531,4.46354511002723,
-9.57822881303571)) ;
#107591 = CARTESIAN_POINT('Ctrl Pts',(-1.77193602330144,4.46102933412832,
-9.57948533293587)) ;
#107592 = CARTESIAN_POINT('Ctrl Pts',(-1.77071067811864,4.45857864376272,
-9.58071067811867)) ;
#107593 = CARTESIAN_POINT('Origin',(-1.69700925663781,4.61428005430337,-9.50285789574935)) ;
#107594 = CARTESIAN_POINT('Origin',(-1.7,0.3,-9.51)) ;
#107595 = CARTESIAN_POINT('Origin',(-1.9,-4.11004745125224E-16,-11.56)) ;
#107596 = CARTESIAN_POINT('',(-1.9,6.9,-11.66)) ;
#107597 = CARTESIAN_POINT('Origin',(-1.9,6.9,-11.56)) ;
#107598 = CARTESIAN_POINT('',(-1.9,7.,-11.66)) ;
#107599 = CARTESIAN_POINT('Origin',(-2.,0.1,-11.76)) ;
#107600 = CARTESIAN_POINT('Origin',(-1.89999999999984,0.100000000000157,-11.7600000000001)) ;
#107601 = CARTESIAN_POINT('Origin',(0.899999999999999,0.1,-11.76)) ;
#107602 = CARTESIAN_POINT('Origin',(0.899999999999999,0.1,-11.56)) ;
#107603 = CARTESIAN_POINT('Origin',(1.1,0.1,-11.56)) ;
#107604 = CARTESIAN_POINT('Origin',(0.899999999999999,0.1,-10.16)) ;
#107605 = CARTESIAN_POINT('',(0.999999999999999,0.1,-8.76)) ;
#107606 = CARTESIAN_POINT('',(0.999999999999999,0.1,-11.66)) ;
#107607 = CARTESIAN_POINT('Origin',(0.899999999999999,0.1,-8.76)) ;
#107608 = CARTESIAN_POINT('Origin',(-1.7,0.3,-9.51)) ;
#107609 = CARTESIAN_POINT('Origin',(-1.7,0.3,-9.51)) ;
#107610 = CARTESIAN_POINT('Origin',(-1.9,6.9,-11.56)) ;
#107611 = CARTESIAN_POINT('',(-1.9,7.,-11.56)) ;
#107612 = CARTESIAN_POINT('Origin',(-1.9,6.9,-11.56)) ;
#107613 = CARTESIAN_POINT('Origin',(-1.9,6.9,-11.56)) ;
#107614 = CARTESIAN_POINT('Origin',(-1.9,7.,-11.76)) ;
#107615 = CARTESIAN_POINT('Origin',(-1.9,6.9,-11.76)) ;
#107616 = CARTESIAN_POINT('Origin',(1.1,0.1,-8.66)) ;
#107617 = CARTESIAN_POINT('Origin',(1.1,0.1,-8.76)) ;
#107618 = CARTESIAN_POINT('Origin',(0.899999999999999,0.1,-8.76)) ;
#107619 = CARTESIAN_POINT('',(0.899999999999999,0.1,-8.66)) ;
#107620 = CARTESIAN_POINT('Origin',(0.899999999999999,0.1,-8.76)) ;
#107621 = CARTESIAN_POINT('Origin',(0.899999999999999,0.1,-8.76)) ;
#107622 = CARTESIAN_POINT('Origin',(-1.7,0.3,-10.16)) ;
#107623 = CARTESIAN_POINT('Origin',(-1.7,0.3,-8.76)) ;
#107624 = CARTESIAN_POINT('Origin',(-1.9,6.9,-10.16)) ;
#107625 = CARTESIAN_POINT('',(-1.9,7.,-8.76)) ;
#107626 = CARTESIAN_POINT('Origin',(-1.9,6.9,-8.76)) ;
#107627 = CARTESIAN_POINT('',(-1.9,7.,-11.66)) ;
#107628 = CARTESIAN_POINT('Origin',(-1.9,6.9,-11.56)) ;
#107629 = CARTESIAN_POINT('Origin',(-1.9,7.1,-11.56)) ;
#107630 = CARTESIAN_POINT('Origin',(0.899999999999999,0.1,-8.76)) ;
#107631 = CARTESIAN_POINT('Origin',(0.899999999999999,0.1,-8.56)) ;
#107632 = CARTESIAN_POINT('Origin',(-1.9668402209837E-32,0.1,-8.76)) ;
#107633 = CARTESIAN_POINT('',(0.999999999999999,0.1,-8.66)) ;
#107634 = CARTESIAN_POINT('Origin',(-1.7,0.1,-8.76)) ;
#107635 = CARTESIAN_POINT('Origin',(-1.7,0.3,-8.76)) ;
#107636 = CARTESIAN_POINT('Origin',(-1.9,0.3,-8.76)) ;
#107637 = CARTESIAN_POINT('Origin',(-1.9,6.9,-8.76)) ;
#107638 = CARTESIAN_POINT('',(-1.9,6.9,-8.66)) ;
#107639 = CARTESIAN_POINT('Origin',(-1.9,6.9,-8.76)) ;
#107640 = CARTESIAN_POINT('Origin',(-1.9,6.9,-8.76)) ;
#107641 = CARTESIAN_POINT('Origin',(-1.9,7.1,-11.66)) ;
#107642 = CARTESIAN_POINT('Origin',(-1.9,7.1,-8.76)) ;
#107643 = CARTESIAN_POINT('Origin',(-1.8,0.1,-8.56)) ;
#107644 = CARTESIAN_POINT('Origin',(-1.90000000000002,0.0999999999999822,
-8.56000000000002)) ;
#107645 = CARTESIAN_POINT('Origin',(-1.9,-6.40600499298624E-17,-8.76)) ;
#107646 = CARTESIAN_POINT('',(-1.9,7.,-8.66)) ;
#107647 = CARTESIAN_POINT('Origin',(-1.9,6.9,-8.76)) ;
#107648 = CARTESIAN_POINT('Origin',(-1.9,6.9,-8.56)) ;
#107649 = CARTESIAN_POINT('Origin',(-1.9,7.,-8.56)) ;
#107650 = CARTESIAN_POINT('Origin',(-0.900000000000002,2.95,-10.16)) ;
#107651 = CARTESIAN_POINT('Origin',(-0.900000000000001,2.95,-11.8031676725155)) ;
#107652 = CARTESIAN_POINT('Origin',(-0.900000000000002,2.95,-11.8031676725155)) ;
#107653 = CARTESIAN_POINT('Origin',(-0.900000000000001,2.95,-11.8031676725155)) ;
#107654 = CARTESIAN_POINT('Origin',(-0.900000000000002,2.95,-11.8031676725155)) ;
#107655 = CARTESIAN_POINT('Origin',(1.15,3.15,-12.71)) ;
#107656 = CARTESIAN_POINT('Origin',(1.15,3.15,-11.8031676725155)) ;
#107657 = CARTESIAN_POINT('Origin',(-1.,2.95,-11.8031676725155)) ;
#107658 = CARTESIAN_POINT('Origin',(1.15,2.95,-11.8031676725155)) ;
#107659 = CARTESIAN_POINT('Origin',(-0.900000000000001,3.8,-10.16)) ;
#107660 = CARTESIAN_POINT('Origin',(-0.900000000000002,2.1568323274845,-11.01)) ;
#107661 = CARTESIAN_POINT('Origin',(-0.900000000000002,1.6,-10.16)) ;
#107662 = CARTESIAN_POINT('Origin',(-0.900000000000002,1.6,-12.1221416870349)) ;
#107663 = CARTESIAN_POINT('Origin',(13.9153543900904,1.4,-12.1221416870349)) ;
#107664 = CARTESIAN_POINT('Origin',(8.49172374697002,1.4,-12.1221416870349)) ;
#107665 = CARTESIAN_POINT('Origin',(-0.900000000000001,1.40000000000001,-12.1221416870349)) ;
#107666 = CARTESIAN_POINT('Origin',(1.15,2.95,-11.8031676725155)) ;
#107667 = CARTESIAN_POINT('Origin',(1.15,3.04189189189189,-11.6255279241354)) ;
#107668 = CARTESIAN_POINT('Origin',(-0.900000000000002,2.1568323274845,-11.01)) ;
#107669 = CARTESIAN_POINT('Origin',(-0.900000000000002,2.1568323274845,-11.01)) ;
#107670 = CARTESIAN_POINT('Origin',(-0.900000000000002,2.1568323274845,-11.01)) ;
#107671 = CARTESIAN_POINT('Origin',(-0.900000000000001,1.40000000000001,-12.1221416870349)) ;
#107672 = CARTESIAN_POINT('Origin',(-0.900000000000002,1.55483870967742,-11.9955519007746)) ;
#107673 = CARTESIAN_POINT('Origin',(1.15,3.8,-10.16)) ;
#107674 = CARTESIAN_POINT('Origin',(1.15,2.33447207586456,-10.9181081081081)) ;
#107675 = CARTESIAN_POINT('Origin',(-1.,2.1568323274845,-11.01)) ;
#107676 = CARTESIAN_POINT('Origin',(1.15,2.1568323274845,-11.01)) ;
#107677 = CARTESIAN_POINT('Origin',(-0.900000000000001,3.8,-11.01)) ;
#107678 = CARTESIAN_POINT('Origin',(-0.900000000000002,1.02736587339765,-11.01)) ;
#107679 = CARTESIAN_POINT('Origin',(-0.900000000000001,3.8,-10.16)) ;
#107680 = CARTESIAN_POINT('Origin',(-0.900000000000002,1.02736587339765,-11.01)) ;
#107681 = CARTESIAN_POINT('Origin',(13.9153543900904,1.4,-8.19785831296513)) ;
#107682 = CARTESIAN_POINT('Origin',(8.49172374697002,1.4,-8.19785831296513)) ;
#107683 = CARTESIAN_POINT('Origin',(-0.900000000000001,1.40000000000001,-8.19785831296513)) ;
#107684 = CARTESIAN_POINT('Origin',(-0.900000000000002,1.6,-10.16)) ;
#107685 = CARTESIAN_POINT('Origin',(-0.900000000000002,1.6,-8.19785831296513)) ;
#107686 = CARTESIAN_POINT('Origin',(-0.900000000000002,2.95,-10.16)) ;
#107687 = CARTESIAN_POINT('Origin',(-0.900000000000002,2.95,-8.5168323274845)) ;
#107688 = CARTESIAN_POINT('Origin',(1.15,2.1568323274845,-11.01)) ;
#107689 = CARTESIAN_POINT('Origin',(1.15,2.1568323274845,-10.81)) ;
#107690 = CARTESIAN_POINT('Origin',(-0.900000000000002,1.02736587339765,-11.01)) ;
#107691 = CARTESIAN_POINT('Origin',(-0.900000000000001,1.40000000000001,-8.19785831296513)) ;
#107692 = CARTESIAN_POINT('Origin',(-0.900000000000002,1.55483870967743,-8.32444809922545)) ;
#107693 = CARTESIAN_POINT('Origin',(-0.900000000000002,2.95,-8.5168323274845)) ;
#107694 = CARTESIAN_POINT('Origin',(-0.900000000000002,2.95,-8.5168323274845)) ;
#107695 = CARTESIAN_POINT('Origin',(-0.900000000000001,2.95,-8.5168323274845)) ;
#107696 = CARTESIAN_POINT('Origin',(1.15,2.21886116991581,-10.81)) ;
#107697 = CARTESIAN_POINT('Ctrl Pts',(1.15,1.02736587339765,-10.91)) ;
#107698 = CARTESIAN_POINT('Ctrl Pts',(1.1608920328805,1.02736587339765,-10.91)) ;
#107699 = CARTESIAN_POINT('Ctrl Pts',(1.17195716626105,1.02622125393927,-10.908143843926)) ;
#107700 = CARTESIAN_POINT('Ctrl Pts',(1.1820844490224,1.02414637334385,-10.9047131887908)) ;
#107701 = CARTESIAN_POINT('Ctrl Pts',(1.19245005921088,1.02202266415684,-10.9012017993431)) ;
#107702 = CARTESIAN_POINT('Ctrl Pts',(1.20216743701154,1.01888103823701,-10.8959601980703)) ;
#107703 = CARTESIAN_POINT('Ctrl Pts',(1.21053792402812,1.01518120925307,-10.8895937168021)) ;
#107704 = CARTESIAN_POINT('Ctrl Pts',(1.219343173684,1.01128921135341,-10.8828965608439)) ;
#107705 = CARTESIAN_POINT('Ctrl Pts',(1.22692289939014,1.00668521903338,-10.8747851615315)) ;
#107706 = CARTESIAN_POINT('Ctrl Pts',(1.23290049538659,1.00186003905466,-10.8659241259624)) ;
#107707 = CARTESIAN_POINT('Ctrl Pts',(1.23922345568944,0.9967560772818,-10.85655113117)) ;
#107708 = CARTESIAN_POINT('Ctrl Pts',(1.24392209779927,0.991279542094837,
-10.8461045599897)) ;
#107709 = CARTESIAN_POINT('Ctrl Pts',(1.24674870216524,0.985895902333124,
-10.8352920665297)) ;
#107710 = CARTESIAN_POINT('Ctrl Pts',(1.24889292215336,0.981811953364218,
-10.8270898699727)) ;
#107711 = CARTESIAN_POINT('Ctrl Pts',(1.25,0.977715885027402,-10.8185491686292)) ;
#107712 = CARTESIAN_POINT('Ctrl Pts',(1.25,0.973783447787483,-10.81)) ;
#107713 = CARTESIAN_POINT('Origin',(-0.900000000000001,3.8,-10.16)) ;
#107714 = CARTESIAN_POINT('Origin',(-0.900000000000002,1.02736587339765,-9.31)) ;
#107715 = CARTESIAN_POINT('Origin',(-0.900000000000001,3.8,-9.31)) ;
#107716 = CARTESIAN_POINT('Origin',(-0.900000000000002,2.1568323274845,-9.31)) ;
#107717 = CARTESIAN_POINT('Origin',(-0.900000000000002,1.02736587339765,-9.31)) ;
#107718 = CARTESIAN_POINT('Origin',(-0.900000000000001,3.8,-10.16)) ;
#107719 = CARTESIAN_POINT('Origin',(-0.900000000000002,2.1568323274845,-9.31)) ;
#107720 = CARTESIAN_POINT('Origin',(-1.,2.95,-8.5168323274845)) ;
#107721 = CARTESIAN_POINT('Origin',(1.15,2.95,-8.5168323274845)) ;
#107722 = CARTESIAN_POINT('Origin',(1.15,3.15,-7.61)) ;
#107723 = CARTESIAN_POINT('Origin',(1.15,3.15,-8.5168323274845)) ;
#107724 = CARTESIAN_POINT('Ctrl Pts',(1.11028558574894,0.930383836951429,
-11.034994283658)) ;
#107725 = CARTESIAN_POINT('Ctrl Pts',(1.14039000477529,0.892136466137752,
-10.909969718594)) ;
#107726 = CARTESIAN_POINT('Ctrl Pts',(1.13015013463564,1.02610337426265,-10.9078511248828)) ;
#107727 = CARTESIAN_POINT('Ctrl Pts',(1.1763969065272,0.935225109827845,-11.0501257399473)) ;
#107728 = CARTESIAN_POINT('Ctrl Pts',(1.15491086542921,0.891146666106505,
-10.9092760504016)) ;
#107729 = CARTESIAN_POINT('Ctrl Pts',(1.16319405445819,1.03078047702075,-10.9151648742452)) ;
#107730 = CARTESIAN_POINT('Ctrl Pts',(1.24701363206619,0.927145283841869,
-11.0255522038252)) ;
#107731 = CARTESIAN_POINT('Ctrl Pts',(1.1775998083145,0.893467326853714,-10.9126373120313)) ;
#107732 = CARTESIAN_POINT('Ctrl Pts',(1.19848758201044,1.022974674531,-10.903287122555)) ;
#107733 = CARTESIAN_POINT('Ctrl Pts',(1.33816236560078,0.900022463714239,
-10.929808850615)) ;
#107734 = CARTESIAN_POINT('Ctrl Pts',(1.22862786282603,0.888037626603791,
-10.8831539643241)) ;
#107735 = CARTESIAN_POINT('Ctrl Pts',(1.244032885045,0.996768276947704,-10.8570266594133)) ;
#107736 = CARTESIAN_POINT('Ctrl Pts',(1.35959492575617,0.881455895025387,
-10.8585323412291)) ;
#107737 = CARTESIAN_POINT('Ctrl Pts',(1.2532051975069,0.880428099081518,-10.8510649378273)) ;
#107738 = CARTESIAN_POINT('Ctrl Pts',(1.25473603279823,0.978811277328879,
-10.8225574871508)) ;
#107739 = CARTESIAN_POINT('Ctrl Pts',(1.34615355831638,0.867571605181199,
-10.7927925825334)) ;
#107740 = CARTESIAN_POINT('Ctrl Pts',(1.25176090202798,0.87095013062452,-10.8094490170578)) ;
#107741 = CARTESIAN_POINT('Ctrl Pts',(1.24801589497572,0.965423101361769,
-10.7908695481641)) ;
#107742 = CARTESIAN_POINT('Origin',(1.35,0.973783447787483,-10.81)) ;
#107743 = CARTESIAN_POINT('Origin',(-0.900000000000002,1.02736587339765,-9.31)) ;
#107744 = CARTESIAN_POINT('',(-0.957735026918965,0.969630846478687,-9.36773502691896)) ;
#107745 = CARTESIAN_POINT('Origin',(-0.900000000000002,1.02736587339765,-9.31)) ;
#107746 = CARTESIAN_POINT('Origin',(-0.900000000000002,2.1568323274845,-9.31)) ;
#107747 = CARTESIAN_POINT('Origin',(-0.900000000000002,2.1568323274845,-9.31)) ;
#107748 = CARTESIAN_POINT('Origin',(1.15,2.95,-8.5168323274845)) ;
#107749 = CARTESIAN_POINT('Origin',(1.15,3.04189189189189,-8.69447207586456)) ;
#107750 = CARTESIAN_POINT('Origin',(1.35,3.8,-10.16)) ;
#107751 = CARTESIAN_POINT('Origin',(1.35,0.973783447787484,-9.51)) ;
#107752 = CARTESIAN_POINT('Origin',(-1.,2.1568323274845,-9.31)) ;
#107753 = CARTESIAN_POINT('Origin',(1.15,2.1568323274845,-9.31)) ;
#107754 = CARTESIAN_POINT('Origin',(1.15,3.8,-10.16)) ;
#107755 = CARTESIAN_POINT('Origin',(1.15,2.33447207586456,-9.40189189189189)) ;
#107756 = CARTESIAN_POINT('Ctrl Pts',(1.34754079198594,0.86915957129316,-9.51974853478551)) ;
#107757 = CARTESIAN_POINT('Ctrl Pts',(1.25183398383324,0.871999770424347,
-9.5059986517603)) ;
#107758 = CARTESIAN_POINT('Ctrl Pts',(1.24871534599026,0.966951450593918,
-9.52553571307356)) ;
#107759 = CARTESIAN_POINT('Ctrl Pts',(1.3578897130187,0.882932151572339,-9.45577742826812)) ;
#107760 = CARTESIAN_POINT('Ctrl Pts',(1.25138796519085,0.881019151005395,
-9.46648728142377)) ;
#107761 = CARTESIAN_POINT('Ctrl Pts',(1.25389076424432,0.980237216252331,
-9.49468863425941)) ;
#107762 = CARTESIAN_POINT('Ctrl Pts',(1.33642796493171,0.90055164307479,-9.3883167189688)) ;
#107763 = CARTESIAN_POINT('Ctrl Pts',(1.22773025960893,0.888154519889375,
-9.43630235415234)) ;
#107764 = CARTESIAN_POINT('Ctrl Pts',(1.24317203399028,0.99727835245108,-9.46206445828307)) ;
#107765 = CARTESIAN_POINT('Ctrl Pts',(1.24851212064762,0.926675670999743,
-9.29611185418657)) ;
#107766 = CARTESIAN_POINT('Ctrl Pts',(1.17855408504652,0.893378082604349,
-9.40793584540021)) ;
#107767 = CARTESIAN_POINT('Ctrl Pts',(1.19923947710882,1.02252144543593,-9.41751118406066)) ;
#107768 = CARTESIAN_POINT('Ctrl Pts',(1.18212686068543,0.93456788869825,-9.27189225990077)) ;
#107769 = CARTESIAN_POINT('Ctrl Pts',(1.1569094747617,0.891342319659306,-9.41050130223919)) ;
#107770 = CARTESIAN_POINT('Ctrl Pts',(1.1660589236879,1.03014681530415,-9.40580412352038)) ;
#107771 = CARTESIAN_POINT('Ctrl Pts',(1.11776263740947,0.930888708579174,
-9.28342358191601)) ;
#107772 = CARTESIAN_POINT('Ctrl Pts',(1.14197710563592,0.892059806626676,
-9.41008229965539)) ;
#107773 = CARTESIAN_POINT('Ctrl Pts',(1.13388624958144,1.02659206201255,-9.41137785610126)) ;
#107774 = CARTESIAN_POINT('Ctrl Pts',(1.15,1.02736587339764,-9.41)) ;
#107775 = CARTESIAN_POINT('Ctrl Pts',(1.15623005440502,1.02736587339759,-9.40999999999987)) ;
#107776 = CARTESIAN_POINT('Ctrl Pts',(1.16249579431471,1.02700282517053,-9.41059086606898)) ;
#107777 = CARTESIAN_POINT('Ctrl Pts',(1.16857840195431,1.02630083270769,-9.41174093944667)) ;
#107778 = CARTESIAN_POINT('Ctrl Pts',(1.1798885498395,1.02499553092934,-9.41387941372467)) ;
#107779 = CARTESIAN_POINT('Ctrl Pts',(1.19084787809767,1.02245621903271,-9.41805069661522)) ;
#107780 = CARTESIAN_POINT('Ctrl Pts',(1.20043335385463,1.01914369852331,-9.4236491064379)) ;
#107781 = CARTESIAN_POINT('Ctrl Pts',(1.21063893018497,1.01561688548223,-9.42960968682249)) ;
#107782 = CARTESIAN_POINT('Ctrl Pts',(1.21965078109605,1.01112191387731,-9.43735485110186)) ;
#107783 = CARTESIAN_POINT('Ctrl Pts',(1.226898722009,1.00626683908294,-9.44607358485429)) ;
#107784 = CARTESIAN_POINT('Ctrl Pts',(1.23435386869391,1.0012729663137,-9.45504157173658)) ;
#107785 = CARTESIAN_POINT('Ctrl Pts',(1.24017476602864,0.995763540409855,
-9.46528702640693)) ;
#107786 = CARTESIAN_POINT('Ctrl Pts',(1.24405759382605,0.990267693778535,
-9.47604165723046)) ;
#107787 = CARTESIAN_POINT('Ctrl Pts',(1.24795610732226,0.9847496452368,-9.48683973419908)) ;
#107788 = CARTESIAN_POINT('Ctrl Pts',(1.25,0.97910634898267,-9.49842794502798)) ;
#107789 = CARTESIAN_POINT('Ctrl Pts',(1.25,0.973783447787483,-9.51)) ;
#107790 = CARTESIAN_POINT('Origin',(1.15,2.1568323274845,-9.31)) ;
#107791 = CARTESIAN_POINT('Origin',(1.15,2.1568323274845,-9.51)) ;
#107792 = CARTESIAN_POINT('Origin',(1.15,2.21886116991581,-9.51)) ;
#107793 = CARTESIAN_POINT('Origin',(1.5,2.3,-10.56)) ;
#107794 = CARTESIAN_POINT('Ctrl Pts',(0.549999999999999,4.04473197180486,
-10.61)) ;
#107795 = CARTESIAN_POINT('Ctrl Pts',(0.549999999999999,4.04340510574359,
-10.6120183916746)) ;
#107796 = CARTESIAN_POINT('Ctrl Pts',(0.54993891248805,4.04197482121863,-10.6139799093559)) ;
#107797 = CARTESIAN_POINT('Ctrl Pts',(0.549362579613717,4.03414945156058,
-10.623763201697)) ;
#107798 = CARTESIAN_POINT('Ctrl Pts',(0.548040652125095,4.02633974827553,
-10.6305458262272)) ;
#107799 = CARTESIAN_POINT('Ctrl Pts',(0.544205267183616,4.00519499286844,
-10.6446839427889)) ;
#107800 = CARTESIAN_POINT('Ctrl Pts',(0.541221332378489,3.99011995637975,
-10.6512251154482)) ;
#107801 = CARTESIAN_POINT('Ctrl Pts',(0.537814556431586,3.96385893187673,
-10.65793059224)) ;
#107802 = CARTESIAN_POINT('Ctrl Pts',(0.536602540378443,3.9513239070287,-10.66)) ;
#107803 = CARTESIAN_POINT('Ctrl Pts',(0.536602540378443,3.93764017256378,
-10.66)) ;
#107804 = CARTESIAN_POINT('Origin',(-0.4,2.3,-10.56)) ;
#107805 = CARTESIAN_POINT('Origin',(-0.4,-3.4,-10.56)) ;
#107806 = CARTESIAN_POINT('Origin',(-0.4,-3.36847777691809,-10.56)) ;
#107807 = CARTESIAN_POINT('Origin',(1.5,2.3,-10.56)) ;
#107808 = CARTESIAN_POINT('Ctrl Pts',(0.536602540378442,2.83090991212703,
-10.66)) ;
#107809 = CARTESIAN_POINT('Ctrl Pts',(0.536602540378442,2.80627146475495,
-10.66)) ;
#107810 = CARTESIAN_POINT('Ctrl Pts',(0.538106903229178,2.77742679387655,
-10.6579527908126)) ;
#107811 = CARTESIAN_POINT('Ctrl Pts',(0.545186976568879,2.71156844363324,
-10.64208398098)) ;
#107812 = CARTESIAN_POINT('Ctrl Pts',(0.549999999999999,2.68282906082667,
-10.6281020558136)) ;
#107813 = CARTESIAN_POINT('Ctrl Pts',(0.549999999999999,2.65280931275608,
-10.61)) ;
#107814 = CARTESIAN_POINT('Origin',(0.400000000000001,2.29999999999999,-10.56)) ;
#107815 = CARTESIAN_POINT('Origin',(0.0725078566451197,-4.04348900069683,
-10.0874921433549)) ;
#107816 = CARTESIAN_POINT('Origin',(-0.4,-3.36847777691809,-10.56)) ;
#107817 = CARTESIAN_POINT('Origin',(-0.0979344438426628,-3.8,-10.2579344438427)) ;
#107818 = CARTESIAN_POINT('Origin',(1.5,2.3,-9.76)) ;
#107819 = CARTESIAN_POINT('Ctrl Pts',(0.536602540378443,3.93764017256378,
-9.66)) ;
#107820 = CARTESIAN_POINT('Ctrl Pts',(0.536602540378443,3.93925361219649,
-9.66)) ;
#107821 = CARTESIAN_POINT('Ctrl Pts',(0.536619300889432,3.94087098263986,
-9.66002899725778)) ;
#107822 = CARTESIAN_POINT('Ctrl Pts',(0.536997639747691,3.95938954612056,
-9.66068581289572)) ;
#107823 = CARTESIAN_POINT('Ctrl Pts',(0.53914231517103,3.97567120869872,-9.66431206156154)) ;
#107824 = CARTESIAN_POINT('Ctrl Pts',(0.544035197036615,4.00535605098064,
-9.67539939166588)) ;
#107825 = CARTESIAN_POINT('Ctrl Pts',(0.546989816174385,4.01946236900589,
-9.68356994463487)) ;
#107826 = CARTESIAN_POINT('Ctrl Pts',(0.549463062495682,4.03595536007394,
-9.69854738169706)) ;
#107827 = CARTESIAN_POINT('Ctrl Pts',(0.550000000000879,4.04078397701433,
-9.70399442034631)) ;
#107828 = CARTESIAN_POINT('Ctrl Pts',(0.549999999999999,4.04473197181449,
-9.71000000001465)) ;
#107829 = CARTESIAN_POINT('Origin',(-0.4,2.3,-9.76)) ;
#107830 = CARTESIAN_POINT('Origin',(0.4,2.29999999999999,-10.56)) ;
#107831 = CARTESIAN_POINT('Origin',(0.4,-3.36847777691809,-10.56)) ;
#107832 = CARTESIAN_POINT('Origin',(-0.0979344438426628,-3.8,-10.2579344438427)) ;
#107833 = CARTESIAN_POINT('Origin',(-0.0979344438426628,-3.8,-10.2579344438427)) ;
#107834 = CARTESIAN_POINT('Origin',(-0.0979344438426627,-3.8,-10.2579344438427)) ;
#107835 = CARTESIAN_POINT('Origin',(-0.4,2.3,-9.76)) ;
#107836 = CARTESIAN_POINT('Origin',(-0.4,-3.36847777691809,-9.76)) ;
#107837 = CARTESIAN_POINT('Origin',(0.190875981738719,-3.6672263744342,-10.3508759817387)) ;
#107838 = CARTESIAN_POINT('Origin',(0.400000000000001,-3.36847777691809,-10.56)) ;
#107839 = CARTESIAN_POINT('Origin',(0.0979344438426626,-3.8,-10.2579344438427)) ;
#107840 = CARTESIAN_POINT('Origin',(0.15,-3.8,-10.2579344438427)) ;
#107841 = CARTESIAN_POINT('Origin',(0.0979344438426627,-3.8,-10.2579344438427)) ;
#107842 = CARTESIAN_POINT('Origin',(-0.0979344438426628,-3.8,-9.66)) ;
#107843 = CARTESIAN_POINT('Origin',(-0.0979344438426628,-3.8,-10.0620655561573)) ;
#107844 = CARTESIAN_POINT('Origin',(-0.174966890829628,-3.68995364716148,
-9.98503310917037)) ;
#107845 = CARTESIAN_POINT('Origin',(-0.400000000000001,-3.36847777691809,
-9.76)) ;
#107846 = CARTESIAN_POINT('Origin',(-0.0979344438426627,-3.8,-10.0620655561573)) ;
#107847 = CARTESIAN_POINT('Origin',(0.0979344438426627,-3.8,-10.2579344438427)) ;
#107848 = CARTESIAN_POINT('Origin',(0.0979344438426628,-3.8,-10.2579344438427)) ;
#107849 = CARTESIAN_POINT('Origin',(-0.0979344438426628,-3.8,-10.0620655561573)) ;
#107850 = CARTESIAN_POINT('Origin',(-0.0979344438426628,-3.8,-10.0620655561573)) ;
#107851 = CARTESIAN_POINT('Origin',(0.0979344438426627,-3.8,-9.66)) ;
#107852 = CARTESIAN_POINT('Origin',(0.0979344438426627,-3.8,-10.0620655561573)) ;
#107853 = CARTESIAN_POINT('Origin',(-1.11032778078669,-3.8,-10.0620655561573)) ;
#107854 = CARTESIAN_POINT('Origin',(0.0979344438426626,-3.8,-10.0620655561573)) ;
#107855 = CARTESIAN_POINT('Origin',(0.0979344438426627,-3.8,-10.0620655561573)) ;
#107856 = CARTESIAN_POINT('Origin',(0.0979344438426627,-3.8,-10.0620655561573)) ;
#107857 = CARTESIAN_POINT('Origin',(0.438350729213467,-3.31369102089885,-9.72164927078653)) ;
#107858 = CARTESIAN_POINT('Origin',(0.399999999999999,-3.36847777691809,-9.76)) ;
#107859 = CARTESIAN_POINT('Origin',(0.4,2.3,-9.76)) ;
#107860 = CARTESIAN_POINT('Origin',(0.4,-3.36847777691809,-9.76)) ;
#107861 = CARTESIAN_POINT('Origin',(0.4,2.29999999999999,-9.76)) ;
#107862 = CARTESIAN_POINT('Origin',(1.5,2.3,-9.76)) ;
#107863 = CARTESIAN_POINT('Ctrl Pts',(0.55,2.65280931275594,-9.71000000000009)) ;
#107864 = CARTESIAN_POINT('Ctrl Pts',(0.550000000000012,2.67648433237897,
-9.69572384666271)) ;
#107865 = CARTESIAN_POINT('Ctrl Pts',(0.54690886425279,2.69988533923261,-9.68352570084763)) ;
#107866 = CARTESIAN_POINT('Ctrl Pts',(0.539540151921448,2.76165254733705,
-9.66409159819012)) ;
#107867 = CARTESIAN_POINT('Ctrl Pts',(0.536602540378443,2.79600904778111,
-9.66)) ;
#107868 = CARTESIAN_POINT('Ctrl Pts',(0.536602540378443,2.83090991212703,
-9.66)) ;
#107869 = CARTESIAN_POINT('Origin',(8.,3.4,-10.56)) ;
#107870 = CARTESIAN_POINT('Origin',(7.96847777691809,3.4,-10.56)) ;
#107871 = CARTESIAN_POINT('Origin',(1.5,4.2,-10.56)) ;
#107872 = CARTESIAN_POINT('Origin',(7.96847777691809,4.2,-10.56)) ;
#107873 = CARTESIAN_POINT('Origin',(8.64348900069683,3.87250785664512,-10.0874921433549)) ;
#107874 = CARTESIAN_POINT('Origin',(7.96847777691809,3.4,-10.56)) ;
#107875 = CARTESIAN_POINT('Origin',(8.4,3.70206555615734,-10.2579344438427)) ;
#107876 = CARTESIAN_POINT('Origin',(8.26722637443421,3.99087598173872,-10.3508759817387)) ;
#107877 = CARTESIAN_POINT('Origin',(7.96847777691809,4.2,-10.56)) ;
#107878 = CARTESIAN_POINT('Origin',(8.4,3.89793444384266,-10.2579344438427)) ;
#107879 = CARTESIAN_POINT('Origin',(8.4,3.95,-10.2579344438427)) ;
#107880 = CARTESIAN_POINT('Origin',(8.4,3.70206555615734,-10.2579344438427)) ;
#107881 = CARTESIAN_POINT('Origin',(8.4,3.89793444384266,-10.2579344438427)) ;
#107882 = CARTESIAN_POINT('Origin',(8.4,3.70206555615734,-10.2579344438427)) ;
#107883 = CARTESIAN_POINT('Origin',(8.4,3.70206555615734,-10.2579344438427)) ;
#107884 = CARTESIAN_POINT('Origin',(1.5,3.4,-9.76)) ;
#107885 = CARTESIAN_POINT('Origin',(7.96847777691809,3.4,-9.76)) ;
#107886 = CARTESIAN_POINT('Origin',(1.5,4.2,-9.76)) ;
#107887 = CARTESIAN_POINT('Origin',(7.96847777691809,4.2,-9.76)) ;
#107888 = CARTESIAN_POINT('Origin',(8.4,3.89793444384266,-10.2579344438427)) ;
#107889 = CARTESIAN_POINT('Origin',(8.4,3.89793444384266,-10.2579344438427)) ;
#107890 = CARTESIAN_POINT('Origin',(8.4,3.70206555615734,-9.66)) ;
#107891 = CARTESIAN_POINT('Origin',(8.4,3.70206555615734,-10.0620655561573)) ;
#107892 = CARTESIAN_POINT('Origin',(8.28995364716148,3.62503310917037,-9.98503310917037)) ;
#107893 = CARTESIAN_POINT('Origin',(7.96847777691809,3.4,-9.76)) ;
#107894 = CARTESIAN_POINT('Origin',(8.4,3.70206555615734,-10.0620655561573)) ;
#107895 = CARTESIAN_POINT('Origin',(7.91369102089885,4.23835072921347,-9.72164927078653)) ;
#107896 = CARTESIAN_POINT('Origin',(7.96847777691809,4.2,-9.76)) ;
#107897 = CARTESIAN_POINT('Origin',(8.4,3.89793444384266,-10.0620655561573)) ;
#107898 = CARTESIAN_POINT('Origin',(8.4,3.89793444384266,-9.66)) ;
#107899 = CARTESIAN_POINT('Origin',(8.4,3.89793444384266,-10.0620655561573)) ;
#107900 = CARTESIAN_POINT('Origin',(8.4,3.70206555615734,-10.0620655561573)) ;
#107901 = CARTESIAN_POINT('Origin',(8.4,3.70206555615734,-10.0620655561573)) ;
#107902 = CARTESIAN_POINT('Origin',(8.4,3.89793444384266,-10.0620655561573)) ;
#107903 = CARTESIAN_POINT('Origin',(8.4,3.89793444384266,-10.0620655561573)) ;
#107904 = CARTESIAN_POINT('Origin',(8.4,2.68967221921331,-10.0620655561573)) ;
#107905 = CARTESIAN_POINT('Origin',(9.9,6.8847127088383,-12.7)) ;
#107906 = CARTESIAN_POINT('Origin',(9.9,6.8847127088383,-11.1197127088383)) ;
#107907 = CARTESIAN_POINT('Origin',(8.77035388141948,6.69643835574155,-10.9314383557415)) ;
#107908 = CARTESIAN_POINT('Ctrl Pts',(8.58356010126947,6.66256607592813,-10.7989266835449)) ;
#107909 = CARTESIAN_POINT('Ctrl Pts',(8.58266714977879,6.65676189123867,-10.7987778582964)) ;
#107910 = CARTESIAN_POINT('Ctrl Pts',(8.58182526931896,6.6507714222091,-10.799114171474)) ;
#107911 = CARTESIAN_POINT('Ctrl Pts',(8.58032528754337,6.63886560514819,-10.8009127350996)) ;
#107912 = CARTESIAN_POINT('Ctrl Pts',(8.57966270906111,6.6329537021218,-10.8023448243328)) ;
#107913 = CARTESIAN_POINT('Ctrl Pts',(8.57906641006222,6.62681909302514,-10.8044771744937)) ;
#107914 = CARTESIAN_POINT('Ctrl Pts',(8.5790337515733,6.62647998752502,-10.8045971697284)) ;
#107915 = CARTESIAN_POINT('Ctrl Pts',(8.57846569624187,6.62052582174809,-10.8067417316811)) ;
#107916 = CARTESIAN_POINT('Ctrl Pts',(8.57802501793955,6.61503168015118,-10.8093142858563)) ;
#107917 = CARTESIAN_POINT('Ctrl Pts',(8.57766199200563,6.60925146760179,-10.8127462133241)) ;
#107918 = CARTESIAN_POINT('Ctrl Pts',(8.57762821177171,6.60869602779036,-10.813083835165)) ;
#107919 = CARTESIAN_POINT('Ctrl Pts',(8.57728522755447,6.60286036001416,-10.8167147989574)) ;
#107920 = CARTESIAN_POINT('Ctrl Pts',(8.57709550103272,6.59788070192258,-10.8205482210568)) ;
#107921 = CARTESIAN_POINT('Ctrl Pts',(8.57703980289281,6.59299711069327,-10.8251723373554)) ;
#107922 = CARTESIAN_POINT('Ctrl Pts',(8.57703670271024,6.59265952430004,-10.8254968925423)) ;
#107923 = CARTESIAN_POINT('Ctrl Pts',(8.57701334129172,6.58927432516123,-10.8288013815953)) ;
#107924 = CARTESIAN_POINT('Ctrl Pts',(8.57705699426438,6.58642971201546,-10.8319917444087)) ;
#107925 = CARTESIAN_POINT('Ctrl Pts',(8.57735031225524,6.57961409340218,-10.8407954417554)) ;
#107926 = CARTESIAN_POINT('Ctrl Pts',(8.5777085651344,6.5760438318291,-10.8466682455398)) ;
#107927 = CARTESIAN_POINT('Ctrl Pts',(8.57865704971093,6.57055741297637,-10.8583322193387)) ;
#107928 = CARTESIAN_POINT('Ctrl Pts',(8.57922107378969,6.56851476050451,-10.8640736349075)) ;
#107929 = CARTESIAN_POINT('Ctrl Pts',(8.57993695782543,6.56687610193756,-10.8704559348161)) ;
#107930 = CARTESIAN_POINT('Ctrl Pts',(8.58000419042984,6.56673001682056,-10.8710478351838)) ;
#107931 = CARTESIAN_POINT('Ctrl Pts',(8.58074399738019,6.56520526212525,-10.8774812517351)) ;
#107932 = CARTESIAN_POINT('Ctrl Pts',(8.58149993293344,6.5643813478578,-10.8833541800931)) ;
#107933 = CARTESIAN_POINT('Ctrl Pts',(8.58236768178473,6.56403389662203,-10.8894987578229)) ;
#107934 = CARTESIAN_POINT('Ctrl Pts',(8.58242358604546,6.56401394107886,-10.8898921736314)) ;
#107935 = CARTESIAN_POINT('Ctrl Pts',(8.58283067264383,6.56388592662945,-10.8927394234264)) ;
#107936 = CARTESIAN_POINT('Ctrl Pts',(8.58319156240649,6.56386525642004,-10.8951699505828)) ;
#107937 = CARTESIAN_POINT('Ctrl Pts',(8.58356019967707,6.56392669994633,-10.8975662650647)) ;
#107938 = CARTESIAN_POINT('Origin',(9.9,6.8847127088383,-11.1197127088383)) ;
#107939 = CARTESIAN_POINT('Origin',(9.9,6.8847127088383,-11.1197127088383)) ;
#107940 = CARTESIAN_POINT('Origin',(9.9,6.8847127088383,-11.1197127088383)) ;
#107941 = CARTESIAN_POINT('Origin',(9.9,7.72792407799439,-12.7)) ;
#107942 = CARTESIAN_POINT('Origin',(9.9,7.72792407799439,-11.1197127088383)) ;
#107943 = CARTESIAN_POINT('Origin',(9.90000000000001,4.35421736843756,-11.1197127088383)) ;
#107944 = CARTESIAN_POINT('Origin',(9.9,7.72792407799439,-11.1197127088383)) ;
#107945 = CARTESIAN_POINT('Origin',(9.9,7.72792407799439,-11.1197127088383)) ;
#107946 = CARTESIAN_POINT('Origin',(9.9,7.72792407799439,-11.1197127088383)) ;
#107947 = CARTESIAN_POINT('Origin',(10.9628342502842,7.37364599456632,-11.2968517505523)) ;
#107948 = CARTESIAN_POINT('Ctrl Pts',(8.56837732530586,8.2772075582313,-10.8925052537977)) ;
#107949 = CARTESIAN_POINT('Ctrl Pts',(8.56753565030797,8.2774881236726,-10.8866129921974)) ;
#107950 = CARTESIAN_POINT('Ctrl Pts',(8.56682045541689,8.2772118066791,-10.8805412944396)) ;
#107951 = CARTESIAN_POINT('Ctrl Pts',(8.56575413148015,8.27538624160206,-10.8687284721175)) ;
#107952 = CARTESIAN_POINT('Ctrl Pts',(8.56538426077853,8.27391165896469,-10.8629905624275)) ;
#107953 = CARTESIAN_POINT('Ctrl Pts',(8.56517777855933,8.27166501362502,-10.857014775447)) ;
#107954 = CARTESIAN_POINT('Ctrl Pts',(8.56516523451684,8.27151619608592,-10.8566276382837)) ;
#107955 = CARTESIAN_POINT('Ctrl Pts',(8.56497390811217,8.26902793125449,-10.8502953359912)) ;
#107956 = CARTESIAN_POINT('Ctrl Pts',(8.56499903025538,8.26597630129449,-10.8445357784659)) ;
#107957 = CARTESIAN_POINT('Ctrl Pts',(8.56538588200261,8.26046191593053,-10.8365906723681)) ;
#107958 = CARTESIAN_POINT('Ctrl Pts',(8.56556309332511,8.25853771611456,-10.8341212364558)) ;
#107959 = CARTESIAN_POINT('Ctrl Pts',(8.56628156514553,8.25214511987157,-10.8268017566891)) ;
#107960 = CARTESIAN_POINT('Ctrl Pts',(8.56700742874797,8.24720216256268,-10.822305445231)) ;
#107961 = CARTESIAN_POINT('Ctrl Pts',(8.56880713798128,8.23661566152168,-10.81462449488)) ;
#107962 = CARTESIAN_POINT('Ctrl Pts',(8.5698603939132,8.23102391526974,-10.8113848807256)) ;
#107963 = CARTESIAN_POINT('Ctrl Pts',(8.57116255171754,8.22459552194135,-10.808446774527)) ;
#107964 = CARTESIAN_POINT('Ctrl Pts',(8.5712749581022,8.22404408343789,-10.8082006607902)) ;
#107965 = CARTESIAN_POINT('Ctrl Pts',(8.57260511146314,8.2175590131258,-10.8053749153055)) ;
#107966 = CARTESIAN_POINT('Ctrl Pts',(8.57395629672842,8.2113575973091,-10.8033463864276)) ;
#107967 = CARTESIAN_POINT('Ctrl Pts',(8.57552311082418,8.20452945286286,-10.8017495443173)) ;
#107968 = CARTESIAN_POINT('Ctrl Pts',(8.57564505123014,8.20400026307087,-10.801629826956)) ;
#107969 = CARTESIAN_POINT('Ctrl Pts',(8.57731301559526,8.19679193622634,-10.800053462537)) ;
#107970 = CARTESIAN_POINT('Ctrl Pts',(8.57896065127871,8.19002168485358,-10.799210969344)) ;
#107971 = CARTESIAN_POINT('Ctrl Pts',(8.58161366784368,8.17959769015476,-10.7987553172771)) ;
#107972 = CARTESIAN_POINT('Ctrl Pts',(8.5825836286427,8.17587911616512,-10.7987639381071)) ;
#107973 = CARTESIAN_POINT('Ctrl Pts',(8.58356010126947,8.17221734381475,-10.7989266835449)) ;
#107974 = CARTESIAN_POINT('Origin',(7.96824861826159,6.56275414521524,-9.52224585478477)) ;
#107975 = CARTESIAN_POINT('Origin',(8.59688370202626,6.66156024040307,-9.43124347526404)) ;
#107976 = CARTESIAN_POINT('Origin',(9.9,6.8847127088383,-9.2002872911617)) ;
#107977 = CARTESIAN_POINT('Origin',(9.9,6.8847127088383,-12.7)) ;
#107978 = CARTESIAN_POINT('Origin',(9.9,6.8847127088383,-9.2002872911617)) ;
#107979 = CARTESIAN_POINT('Origin',(9.9,6.8847127088383,-9.2002872911617)) ;
#107980 = CARTESIAN_POINT('Origin',(9.9,6.8847127088383,-9.2002872911617)) ;
#107981 = CARTESIAN_POINT('Origin',(9.9,6.8,-9.2002872911617)) ;
#107982 = CARTESIAN_POINT('Origin',(9.9,7.72792407799439,-9.2002872911617)) ;
#107983 = CARTESIAN_POINT('Origin',(9.9,7.72792407799439,-12.7)) ;
#107984 = CARTESIAN_POINT('Origin',(9.9,7.72792407799439,-9.2002872911617)) ;
#107985 = CARTESIAN_POINT('Origin',(9.9,7.72792407799439,-9.2002872911617)) ;
#107986 = CARTESIAN_POINT('Origin',(9.9,7.72792407799439,-9.2002872911617)) ;
#107987 = CARTESIAN_POINT('Origin',(9.60917571369883,7.82486550676144,-9.24875800554523)) ;
#107988 = CARTESIAN_POINT('Origin',(8.59099001846081,8.18966234086565,-9.42516097389812)) ;
#107989 = CARTESIAN_POINT('Origin',(0.45,4.4,-10.16)) ;
#107990 = CARTESIAN_POINT('Origin',(0.45,4.4,-10.61)) ;
#107991 = CARTESIAN_POINT('Origin',(0.45,4.4,-9.71)) ;
#107992 = CARTESIAN_POINT('Origin',(-1.9,7.55,-12.7)) ;
#107993 = CARTESIAN_POINT('Origin',(6.9,7.75,-12.7)) ;
#107994 = CARTESIAN_POINT('Origin',(7.1,8.2,-12.7)) ;
#107995 = CARTESIAN_POINT('Origin',(9.9,0.1,-12.7)) ;
#107996 = CARTESIAN_POINT('Origin',(9.9,1.16528729116168,-12.7)) ;
#107997 = CARTESIAN_POINT('Origin',(9.9,1.16528729116168,-12.2041618801782)) ;
#107998 = CARTESIAN_POINT('Origin',(9.9,3.8,-10.16)) ;
#107999 = CARTESIAN_POINT('Origin',(9.9,1.16528729116168,-8.1158381198218)) ;
#108000 = CARTESIAN_POINT('Origin',(9.9,1.16528729116168,-12.2041618801782)) ;
#108001 = CARTESIAN_POINT('Origin',(9.9,1.16528729116168,-12.7)) ;
#108002 = CARTESIAN_POINT('Origin',(9.9,1.16528729116168,-8.1158381198218)) ;
#108003 = CARTESIAN_POINT('Ctrl Pts',(0.55,0.3,-10.61)) ;
#108004 = CARTESIAN_POINT('Ctrl Pts',(0.55,0.3,-10.71)) ;
#108005 = CARTESIAN_POINT('Ctrl Pts',(0.45,0.3,-10.71)) ;
#108006 = CARTESIAN_POINT('Ctrl Pts',(0.55,0.28690770353672,-10.6100000008183)) ;
#108007 = CARTESIAN_POINT('Ctrl Pts',(0.549992696056779,0.300543498480462,
-10.7099926960868)) ;
#108008 = CARTESIAN_POINT('Ctrl Pts',(0.450000000818259,0.286907703536723,
-10.71)) ;
#108009 = CARTESIAN_POINT('Ctrl Pts',(0.552602750539093,0.273825167611082,
-10.6152055010782)) ;
#108010 = CARTESIAN_POINT('Ctrl Pts',(0.546703256435901,0.299059401315789,
-10.7067032564359)) ;
#108011 = CARTESIAN_POINT('Ctrl Pts',(0.455205501078185,0.273825167611078,
-10.7126027505391)) ;
#108012 = CARTESIAN_POINT('Ctrl Pts',(0.56262134295865,0.249638145915901,
-10.6352426859173)) ;
#108013 = CARTESIAN_POINT('Ctrl Pts',(0.544986924117067,0.282072776439536,
-10.7049869241171)) ;
#108014 = CARTESIAN_POINT('Ctrl Pts',(0.4752426859173,0.249638145915905,-10.7226213429587)) ;
#108015 = CARTESIAN_POINT('Ctrl Pts',(0.570033341471288,0.238545302291403,
-10.6500666829426)) ;
#108016 = CARTESIAN_POINT('Ctrl Pts',(0.547116196858403,0.267914459835259,
-10.7071161968584)) ;
#108017 = CARTESIAN_POINT('Ctrl Pts',(0.490066682942577,0.238545302291388,
-10.7300333414713)) ;
#108018 = CARTESIAN_POINT('Ctrl Pts',(0.597801282701459,0.210777361061231,
-10.7056025654029)) ;
#108019 = CARTESIAN_POINT('Ctrl Pts',(0.570853448890168,0.22637471385926,
-10.7308534488902)) ;
#108020 = CARTESIAN_POINT('Ctrl Pts',(0.545602565402917,0.210777361061261,
-10.7578012827014)) ;
#108021 = CARTESIAN_POINT('Ctrl Pts',(0.62374656717361,0.2,-10.7574931343473)) ;
#108022 = CARTESIAN_POINT('Ctrl Pts',(0.610458667315072,0.2,-10.7704586673159)) ;
#108023 = CARTESIAN_POINT('Ctrl Pts',(0.59749313434724,0.2,-10.7837465671738)) ;
#108024 = CARTESIAN_POINT('Ctrl Pts',(0.65,0.2,-10.81)) ;
#108025 = CARTESIAN_POINT('Ctrl Pts',(0.65,0.2,-10.81)) ;
#108026 = CARTESIAN_POINT('Ctrl Pts',(0.65,0.2,-10.81)) ;
#108027 = CARTESIAN_POINT('Origin',(0.45,0.3,-10.61)) ;
#108028 = CARTESIAN_POINT('Origin',(0.45,1.24941393210234E-16,-10.61)) ;
#108029 = CARTESIAN_POINT('Origin',(0.45,4.4,-10.61)) ;
#108030 = CARTESIAN_POINT('Origin',(0.45,4.4,-10.61)) ;
#108031 = CARTESIAN_POINT('Origin',(0.45,4.4,-10.61)) ;
#108032 = CARTESIAN_POINT('Origin',(0.549999999999999,4.4,-10.61)) ;
#108033 = CARTESIAN_POINT('Origin',(-1.7,4.4,-10.61)) ;
#108034 = CARTESIAN_POINT('Ctrl Pts',(-1.8,4.6,-10.81)) ;
#108035 = CARTESIAN_POINT('Ctrl Pts',(-1.8,4.6,-10.81)) ;
#108036 = CARTESIAN_POINT('Ctrl Pts',(-1.8,4.6,-10.81)) ;
#108037 = CARTESIAN_POINT('Ctrl Pts',(-1.8,4.57374656717364,-10.7574931343473)) ;
#108038 = CARTESIAN_POINT('Ctrl Pts',(-1.8,4.56045866731614,-10.7704586673162)) ;
#108039 = CARTESIAN_POINT('Ctrl Pts',(-1.8,4.5474931343473,-10.7837465671736)) ;
#108040 = CARTESIAN_POINT('Ctrl Pts',(-1.78922263893876,4.54780128270145,
-10.7056025654029)) ;
#108041 = CARTESIAN_POINT('Ctrl Pts',(-1.77362528614074,4.52085344889012,
-10.7308534488902)) ;
#108042 = CARTESIAN_POINT('Ctrl Pts',(-1.78922263893877,4.49560256540291,
-10.7578012827015)) ;
#108043 = CARTESIAN_POINT('Ctrl Pts',(-1.7614546977086,4.5200333414713,-10.6500666829426)) ;
#108044 = CARTESIAN_POINT('Ctrl Pts',(-1.73208554016475,4.49711619685843,
-10.7071161968584)) ;
#108045 = CARTESIAN_POINT('Ctrl Pts',(-1.7614546977086,4.44006668294258,-10.7300333414713)) ;
#108046 = CARTESIAN_POINT('Ctrl Pts',(-1.7503618540841,4.51262134295865,-10.6352426859173)) ;
#108047 = CARTESIAN_POINT('Ctrl Pts',(-1.71792722356046,4.49498692411707,
-10.704986924117)) ;
#108048 = CARTESIAN_POINT('Ctrl Pts',(-1.75036185408409,4.42524268591729,
-10.7226213429587)) ;
#108049 = CARTESIAN_POINT('Ctrl Pts',(-1.72617483238892,4.50260275053909,
-10.6152055010782)) ;
#108050 = CARTESIAN_POINT('Ctrl Pts',(-1.70094059868421,4.4967032564359,-10.7067032564359)) ;
#108051 = CARTESIAN_POINT('Ctrl Pts',(-1.72617483238892,4.4052055010782,-10.7126027505391)) ;
#108052 = CARTESIAN_POINT('Ctrl Pts',(-1.71309229646328,4.5,-10.6100000008183)) ;
#108053 = CARTESIAN_POINT('Ctrl Pts',(-1.69945650151111,4.49999269607724,
-10.7099926960867)) ;
#108054 = CARTESIAN_POINT('Ctrl Pts',(-1.71309229646328,4.40000000081823,
-10.71)) ;
#108055 = CARTESIAN_POINT('Ctrl Pts',(-1.7,4.5,-10.61)) ;
#108056 = CARTESIAN_POINT('Ctrl Pts',(-1.7,4.5,-10.71)) ;
#108057 = CARTESIAN_POINT('Ctrl Pts',(-1.7,4.4,-10.71)) ;
#108058 = CARTESIAN_POINT('Ctrl Pts',(-1.8,4.6,-9.51)) ;
#108059 = CARTESIAN_POINT('Ctrl Pts',(-1.8,4.6,-9.51)) ;
#108060 = CARTESIAN_POINT('Ctrl Pts',(-1.8,4.6,-9.51)) ;
#108061 = CARTESIAN_POINT('Ctrl Pts',(-1.8,4.5474931343473,-9.53625343282638)) ;
#108062 = CARTESIAN_POINT('Ctrl Pts',(-1.8,4.56045866731616,-9.54954133268381)) ;
#108063 = CARTESIAN_POINT('Ctrl Pts',(-1.8,4.57374656717364,-9.56250686565271)) ;
#108064 = CARTESIAN_POINT('Ctrl Pts',(-1.78922263893877,4.49560256540291,
-9.56219871729854)) ;
#108065 = CARTESIAN_POINT('Ctrl Pts',(-1.77362528614073,4.52085344889015,
-9.58914655110983)) ;
#108066 = CARTESIAN_POINT('Ctrl Pts',(-1.78922263893876,4.54780128270145,
-9.61439743459709)) ;
#108067 = CARTESIAN_POINT('Ctrl Pts',(-1.7614546977086,4.44006668294258,-9.58996665852871)) ;
#108068 = CARTESIAN_POINT('Ctrl Pts',(-1.73208554016475,4.49711619685842,
-9.6128838031416)) ;
#108069 = CARTESIAN_POINT('Ctrl Pts',(-1.7614546977086,4.5200333414713,-9.66993331705742)) ;
#108070 = CARTESIAN_POINT('Ctrl Pts',(-1.75036185408409,4.42524268591729,
-9.59737865704135)) ;
#108071 = CARTESIAN_POINT('Ctrl Pts',(-1.71792722356046,4.49498692411707,
-9.61501307588296)) ;
#108072 = CARTESIAN_POINT('Ctrl Pts',(-1.7503618540841,4.51262134295865,-9.68475731408271)) ;
#108073 = CARTESIAN_POINT('Ctrl Pts',(-1.72617483238892,4.4052055010782,-9.60739724946091)) ;
#108074 = CARTESIAN_POINT('Ctrl Pts',(-1.70094059868421,4.4967032564359,-9.61329674356408)) ;
#108075 = CARTESIAN_POINT('Ctrl Pts',(-1.72617483238892,4.50260275053909,
-9.70479449892181)) ;
#108076 = CARTESIAN_POINT('Ctrl Pts',(-1.71309229646328,4.40000000081823,
-9.61)) ;
#108077 = CARTESIAN_POINT('Ctrl Pts',(-1.69945650152659,4.49999269603973,
-9.61000730391312)) ;
#108078 = CARTESIAN_POINT('Ctrl Pts',(-1.71309229646328,4.5,-9.70999999918169)) ;
#108079 = CARTESIAN_POINT('Ctrl Pts',(-1.7,4.4,-9.61)) ;
#108080 = CARTESIAN_POINT('Ctrl Pts',(-1.7,4.5,-9.61)) ;
#108081 = CARTESIAN_POINT('Ctrl Pts',(-1.7,4.5,-9.71)) ;
#108082 = CARTESIAN_POINT('Origin',(-1.7,4.4,-9.71)) ;
#108083 = CARTESIAN_POINT('Origin',(0.549999999999999,4.4,-9.71)) ;
#108084 = CARTESIAN_POINT('Origin',(0.45,4.4,-9.71)) ;
#108085 = CARTESIAN_POINT('Origin',(0.45,4.4,-9.71)) ;
#108086 = CARTESIAN_POINT('Origin',(0.45,4.4,-9.71)) ;
#108087 = CARTESIAN_POINT('Origin',(0.45,4.9047241136249E-17,-9.71)) ;
#108088 = CARTESIAN_POINT('Origin',(0.45,0.3,-9.71)) ;
#108089 = CARTESIAN_POINT('Ctrl Pts',(0.45,0.3,-9.61)) ;
#108090 = CARTESIAN_POINT('Ctrl Pts',(0.55,0.3,-9.61)) ;
#108091 = CARTESIAN_POINT('Ctrl Pts',(0.55,0.3,-9.71)) ;
#108092 = CARTESIAN_POINT('Ctrl Pts',(0.450000000818259,0.286907703536723,
-9.61)) ;
#108093 = CARTESIAN_POINT('Ctrl Pts',(0.549992696056779,0.300543498480462,
-9.61000730391316)) ;
#108094 = CARTESIAN_POINT('Ctrl Pts',(0.55,0.28690770353672,-9.70999999918169)) ;
#108095 = CARTESIAN_POINT('Ctrl Pts',(0.455205501078185,0.273825167611078,
-9.60739724946091)) ;
#108096 = CARTESIAN_POINT('Ctrl Pts',(0.5467032564359,0.299059401315789,-9.6132967435641)) ;
#108097 = CARTESIAN_POINT('Ctrl Pts',(0.552602750539093,0.273825167611082,
-9.7047944989218)) ;
#108098 = CARTESIAN_POINT('Ctrl Pts',(0.4752426859173,0.249638145915905,-9.59737865704135)) ;
#108099 = CARTESIAN_POINT('Ctrl Pts',(0.544986924117068,0.282072776439536,
-9.61501307588293)) ;
#108100 = CARTESIAN_POINT('Ctrl Pts',(0.56262134295865,0.249638145915901,
-9.68475731408271)) ;
#108101 = CARTESIAN_POINT('Ctrl Pts',(0.490066682942577,0.238545302291388,
-9.5899666585287)) ;
#108102 = CARTESIAN_POINT('Ctrl Pts',(0.547116196858391,0.26791445983525,
-9.61288380314157)) ;
#108103 = CARTESIAN_POINT('Ctrl Pts',(0.570033341471288,0.238545302291403,
-9.66993331705742)) ;
#108104 = CARTESIAN_POINT('Ctrl Pts',(0.545602565402917,0.210777361061261,
-9.56219871729857)) ;
#108105 = CARTESIAN_POINT('Ctrl Pts',(0.570853448890192,0.226374713859273,
-9.58914655110988)) ;
#108106 = CARTESIAN_POINT('Ctrl Pts',(0.597801282701459,0.210777361061231,
-9.61439743459709)) ;
#108107 = CARTESIAN_POINT('Ctrl Pts',(0.59749313434724,0.2,-9.53625343282625)) ;
#108108 = CARTESIAN_POINT('Ctrl Pts',(0.61045866731604,0.2,-9.54954133268394)) ;
#108109 = CARTESIAN_POINT('Ctrl Pts',(0.623746567173607,0.2,-9.56250686565271)) ;
#108110 = CARTESIAN_POINT('Ctrl Pts',(0.65,0.2,-9.51)) ;
#108111 = CARTESIAN_POINT('Ctrl Pts',(0.65,0.2,-9.51)) ;
#108112 = CARTESIAN_POINT('Ctrl Pts',(0.65,0.2,-9.51)) ;
#108113 = CARTESIAN_POINT('Ctrl Pts',(8.5,8.17221734381475,-10.7002872911617)) ;
#108114 = CARTESIAN_POINT('Ctrl Pts',(8.5,8.17221734381475,-10.785)) ;
#108115 = CARTESIAN_POINT('Ctrl Pts',(8.58356010126947,8.17221734381475,-10.7989266835449)) ;
#108116 = CARTESIAN_POINT('Ctrl Pts',(8.5,8.23335379241386,-10.700287292739)) ;
#108117 = CARTESIAN_POINT('Ctrl Pts',(8.5,8.2084742596065,-10.7774575674216)) ;
#108118 = CARTESIAN_POINT('Ctrl Pts',(8.57460439031228,8.20580126077887,-10.797434065052)) ;
#108119 = CARTESIAN_POINT('Ctrl Pts',(8.5,8.29192178062155,-10.7271741150785)) ;
#108120 = CARTESIAN_POINT('Ctrl Pts',(8.5,8.25010493984403,-10.7892546083117)) ;
#108121 = CARTESIAN_POINT('Ctrl Pts',(8.56800970738924,8.23725302684489,-10.8097783631899)) ;
#108122 = CARTESIAN_POINT('Ctrl Pts',(8.5,8.36583651094027,-10.8165506232914)) ;
#108123 = CARTESIAN_POINT('Ctrl Pts',(8.5,8.29925403146167,-10.8433614370366)) ;
#108124 = CARTESIAN_POINT('Ctrl Pts',(8.56373266208983,8.27563607377072,-10.8537537764131)) ;
#108125 = CARTESIAN_POINT('Ctrl Pts',(8.5,8.38029241321775,-10.8779552056997)) ;
#108126 = CARTESIAN_POINT('Ctrl Pts',(8.5,8.30669116589131,-10.8848088499411)) ;
#108127 = CARTESIAN_POINT('Ctrl Pts',(8.5661012385937,8.28208399509957,-10.884808702407)) ;
#108128 = CARTESIAN_POINT('Ctrl Pts',(8.5,8.36719795478507,-10.9360547234799)) ;
#108129 = CARTESIAN_POINT('Ctrl Pts',(8.5,8.29381262650623,-10.9195151496718)) ;
#108130 = CARTESIAN_POINT('Ctrl Pts',(8.57227762885807,8.27346847343705,-10.9149299876354)) ;
#108131 = CARTESIAN_POINT('Ctrl Pts',(8.5485213309235,8.28383177029354,-10.9159865327337)) ;
#108132 = CARTESIAN_POINT('Ctrl Pts',(8.54913757890789,8.28625057716298,-10.902921659184)) ;
#108133 = CARTESIAN_POINT('Ctrl Pts',(8.549146361399,8.28675781111762,-10.8892647894026)) ;
#108134 = CARTESIAN_POINT('Ctrl Pts',(8.54883414737369,8.28489376483071,-10.876098869425)) ;
#108135 = CARTESIAN_POINT('Ctrl Pts',(8.54852072231757,8.28302248819127,-10.8628818808428)) ;
#108136 = CARTESIAN_POINT('Ctrl Pts',(8.54791723678494,8.27865742078997,-10.8498312958117)) ;
#108137 = CARTESIAN_POINT('Ctrl Pts',(8.54677696932927,8.27237937104781,-10.8381020767297)) ;
#108138 = CARTESIAN_POINT('Ctrl Pts',(8.5454465495755,8.26505438658866,-10.8244168797302)) ;
#108139 = CARTESIAN_POINT('Ctrl Pts',(8.54324462275112,8.25487237915563,-10.8122537533388)) ;
#108140 = CARTESIAN_POINT('Ctrl Pts',(8.53884071267076,8.24480815719263,-10.8012071681992)) ;
#108141 = CARTESIAN_POINT('Ctrl Pts',(8.5342440055524,8.23430333763594,-10.7896769789768)) ;
#108142 = CARTESIAN_POINT('Ctrl Pts',(8.52670159721618,8.22420330618022,-10.778704260243)) ;
#108143 = CARTESIAN_POINT('Ctrl Pts',(8.51928858688475,8.21729138318396,-10.7659881754653)) ;
#108144 = CARTESIAN_POINT('Ctrl Pts',(8.51327528614099,8.21168455548023,-10.755673116045)) ;
#108145 = CARTESIAN_POINT('Ctrl Pts',(8.50759525524367,8.20778929846109,-10.7439849430828)) ;
#108146 = CARTESIAN_POINT('Ctrl Pts',(8.50412058850191,8.20498026622232,-10.7315739486628)) ;
#108147 = CARTESIAN_POINT('Ctrl Pts',(8.50147164778345,8.20283877743224,-10.7221123251694)) ;
#108148 = CARTESIAN_POINT('Ctrl Pts',(8.50000317248551,8.2012555848359,-10.712083357655)) ;
#108149 = CARTESIAN_POINT('Ctrl Pts',(8.50000000513446,8.20000405629318,-10.7021052387284)) ;
#108150 = CARTESIAN_POINT('Origin',(8.6,8.17221734381475,-10.7002872911617)) ;
#108151 = CARTESIAN_POINT('Origin',(8.6,4.35421736843756,-10.7002872911617)) ;
#108152 = CARTESIAN_POINT('Origin',(8.6,6.66256607592813,-10.7002872911617)) ;
#108153 = CARTESIAN_POINT('Ctrl Pts',(8.5,6.47083593368087,-10.9448081099244)) ;
#108154 = CARTESIAN_POINT('Ctrl Pts',(8.5,6.55684090505321,-10.9243877386952)) ;
#108155 = CARTESIAN_POINT('Ctrl Pts',(8.58772778625753,6.56739561896918,-10.921881707091)) ;
#108156 = CARTESIAN_POINT('Ctrl Pts',(8.5,6.45680686388585,-10.8857215297177)) ;
#108157 = CARTESIAN_POINT('Ctrl Pts',(8.49999999999995,6.54406229478603,-10.8925101654037)) ;
#108158 = CARTESIAN_POINT('Ctrl Pts',(8.58195196310351,6.55941415012443,-10.8913576868779)) ;
#108159 = CARTESIAN_POINT('Ctrl Pts',(8.5,6.47061556584389,-10.8219524568049)) ;
#108160 = CARTESIAN_POINT('Ctrl Pts',(8.5,6.54836369988887,-10.8523987274071)) ;
#108161 = CARTESIAN_POINT('Ctrl Pts',(8.57801125828726,6.56566601372231,-10.8588344592028)) ;
#108162 = CARTESIAN_POINT('Ctrl Pts',(8.5,6.54379299301796,-10.7286264716581)) ;
#108163 = CARTESIAN_POINT('Ctrl Pts',(8.5,6.59071789516225,-10.7962265152922)) ;
#108164 = CARTESIAN_POINT('Ctrl Pts',(8.57642058265786,6.60198961470444,-10.8119063540245)) ;
#108165 = CARTESIAN_POINT('Ctrl Pts',(8.5,6.60220518075381,-10.7002872929747)) ;
#108166 = CARTESIAN_POINT('Ctrl Pts',(8.4999999999998,6.62800697860326,-10.7809176707627)) ;
#108167 = CARTESIAN_POINT('Ctrl Pts',(8.57879135173927,6.63156920211804,-10.7981318919565)) ;
#108168 = CARTESIAN_POINT('Ctrl Pts',(8.5,6.66256607592813,-10.7002872911617)) ;
#108169 = CARTESIAN_POINT('Ctrl Pts',(8.5,6.66256607592813,-10.785)) ;
#108170 = CARTESIAN_POINT('Ctrl Pts',(8.58356010126947,6.66256607592813,-10.7989266835449)) ;
#108171 = CARTESIAN_POINT('',(8.54565366748546,6.6165071194701,-10.7939653182916)) ;
#108172 = CARTESIAN_POINT('Ctrl Pts',(8.54565366716096,6.61650712004144,-10.7939653178134)) ;
#108173 = CARTESIAN_POINT('Ctrl Pts',(8.54527684775561,6.61717057264373,-10.7934100008636)) ;
#108174 = CARTESIAN_POINT('Ctrl Pts',(8.54488909343999,6.61782772231442,-10.7928554298996)) ;
#108175 = CARTESIAN_POINT('Ctrl Pts',(8.54449064961557,6.61847724592624,-10.7923008713851)) ;
#108176 = CARTESIAN_POINT('Ctrl Pts',(8.54445329550703,6.61853813876485,-10.7922488815243)) ;
#108177 = CARTESIAN_POINT('Ctrl Pts',(8.5444158475797,6.61859896452238,-10.7921968917916)) ;
#108178 = CARTESIAN_POINT('Ctrl Pts',(8.54437830610593,6.61865972207475,-10.7921449015858)) ;
#108179 = CARTESIAN_POINT('Ctrl Pts',(8.54363538409139,6.61986207559674,-10.7911160483067)) ;
#108180 = CARTESIAN_POINT('Ctrl Pts',(8.54285495000579,6.62104203503548,-10.7900848621745)) ;
#108181 = CARTESIAN_POINT('Ctrl Pts',(8.54204093171137,6.62218056960146,-10.789051115167)) ;
#108182 = CARTESIAN_POINT('Ctrl Pts',(8.54157979215428,6.62282554690612,-10.7884654997817)) ;
#108183 = CARTESIAN_POINT('Ctrl Pts',(8.54110770812182,6.62345780120153,-10.7878786499066)) ;
#108184 = CARTESIAN_POINT('Ctrl Pts',(8.54062344907117,6.62407892448169,-10.7872869541397)) ;
#108185 = CARTESIAN_POINT('Ctrl Pts',(8.54011932596481,6.62472552591745,-10.7866709873185)) ;
#108186 = CARTESIAN_POINT('Ctrl Pts',(8.53960207832255,6.62535666566134,-10.7860509905891)) ;
#108187 = CARTESIAN_POINT('Ctrl Pts',(8.53907286520403,6.62597244099098,-10.785425228811)) ;
#108188 = CARTESIAN_POINT('Ctrl Pts',(8.53887441028459,6.6262033567396,-10.7851905681443)) ;
#108189 = CARTESIAN_POINT('Ctrl Pts',(8.53867427664141,6.6264321129994,-10.7849550998211)) ;
#108190 = CARTESIAN_POINT('Ctrl Pts',(8.53847256319997,6.62665871795109,-10.7847187642184)) ;
#108191 = CARTESIAN_POINT('Ctrl Pts',(8.53842843838465,6.62670828778427,-10.7846670658053)) ;
#108192 = CARTESIAN_POINT('Ctrl Pts',(8.53838423811747,6.62675775467668,-10.7846153260175)) ;
#108193 = CARTESIAN_POINT('Ctrl Pts',(8.53833996369343,6.62680711871688,-10.7845635444601)) ;
#108194 = CARTESIAN_POINT('Ctrl Pts',(8.53829707284513,6.62685494013082,-10.7845133810765)) ;
#108195 = CARTESIAN_POINT('Ctrl Pts',(8.53825411240223,6.62690266502019,-10.7844631784931)) ;
#108196 = CARTESIAN_POINT('Ctrl Pts',(8.53821108363804,6.62695029346534,-10.7844129364377)) ;
#108197 = CARTESIAN_POINT('Ctrl Pts',(8.53803571435326,6.62714440934378,-10.7842081684534)) ;
#108198 = CARTESIAN_POINT('Ctrl Pts',(8.53785876035506,6.62733753498029,-10.7840021836648)) ;
#108199 = CARTESIAN_POINT('Ctrl Pts',(8.53767995296703,6.62753033615257,-10.7837944665652)) ;
#108200 = CARTESIAN_POINT('Ctrl Pts',(8.53649871780653,6.62880401687798,-10.7824222484251)) ;
#108201 = CARTESIAN_POINT('Ctrl Pts',(8.53528300832264,6.62998038079528,-10.7810380760596)) ;
#108202 = CARTESIAN_POINT('Ctrl Pts',(8.53403203676336,6.63110281535145,-10.7796044865649)) ;
#108203 = CARTESIAN_POINT('Ctrl Pts',(8.5334687038968,6.63160826591215,-10.7789589178679)) ;
#108204 = CARTESIAN_POINT('Ctrl Pts',(8.5328995953692,6.63209979040223,-10.7783054256595)) ;
#108205 = CARTESIAN_POINT('Ctrl Pts',(8.53232661340319,6.63257735344031,-10.7776437014439)) ;
#108206 = CARTESIAN_POINT('Ctrl Pts',(8.53206474273904,6.63279561467255,-10.7773412727985)) ;
#108207 = CARTESIAN_POINT('Ctrl Pts',(8.53180206199565,6.63301096017663,-10.7770371260807)) ;
#108208 = CARTESIAN_POINT('Ctrl Pts',(8.53153874718657,6.63322338883724,-10.7767312388807)) ;
#108209 = CARTESIAN_POINT('Ctrl Pts',(8.53007363658218,6.63440536369244,-10.7750292511271)) ;
#108210 = CARTESIAN_POINT('Ctrl Pts',(8.52858926277506,6.63549697414123,-10.7732730839131)) ;
#108211 = CARTESIAN_POINT('Ctrl Pts',(8.52711342564664,6.6364985663511,-10.7714611393064)) ;
#108212 = CARTESIAN_POINT('Ctrl Pts',(8.52634316954117,6.63702130866458,-10.7705154649028)) ;
#108213 = CARTESIAN_POINT('Ctrl Pts',(8.52557615349969,6.63751985710295,-10.7695557193112)) ;
#108214 = CARTESIAN_POINT('Ctrl Pts',(8.5248140182343,6.63799287689813,-10.7685803261613)) ;
#108215 = CARTESIAN_POINT('Ctrl Pts',(8.52460710835822,6.63812129566006,-10.7683155195253)) ;
#108216 = CARTESIAN_POINT('Ctrl Pts',(8.52440075574004,6.63824801482191,-10.7680497539023)) ;
#108217 = CARTESIAN_POINT('Ctrl Pts',(8.52419502810871,6.63837284070829,-10.7677830860811)) ;
#108218 = CARTESIAN_POINT('Ctrl Pts',(8.52404824365685,6.63846190263541,-10.7675928214593)) ;
#108219 = CARTESIAN_POINT('Ctrl Pts',(8.52390173612803,6.63855002749203,-10.7674020437347)) ;
#108220 = CARTESIAN_POINT('Ctrl Pts',(8.52375553261475,6.63863721305423,-10.7672107628049)) ;
#108221 = CARTESIAN_POINT('Ctrl Pts',(8.52294204127159,6.63912232246441,-10.7661464560925)) ;
#108222 = CARTESIAN_POINT('Ctrl Pts',(8.52213801365705,6.63957834748689,-10.7650665375564)) ;
#108223 = CARTESIAN_POINT('Ctrl Pts',(8.5213477449051,6.64000494097979,-10.7639729614464)) ;
#108224 = CARTESIAN_POINT('Ctrl Pts',(8.51876608595596,6.64139854145543,-10.7604004545695)) ;
#108225 = CARTESIAN_POINT('Ctrl Pts',(8.51630176076717,6.64256282842069,-10.7566245667844)) ;
#108226 = CARTESIAN_POINT('Ctrl Pts',(8.5140473780102,6.64354662431173,-10.7526687582287)) ;
#108227 = CARTESIAN_POINT('Ctrl Pts',(8.51174271377016,6.64455236266853,-10.7486247197926)) ;
#108228 = CARTESIAN_POINT('Ctrl Pts',(8.50965863261299,6.64536892721963,-10.7443937780696)) ;
#108229 = CARTESIAN_POINT('Ctrl Pts',(8.50786496313904,6.64606338785377,-10.740044165486)) ;
#108230 = CARTESIAN_POINT('Ctrl Pts',(8.50767015284865,6.64613881316471,-10.7395717544299)) ;
#108231 = CARTESIAN_POINT('Ctrl Pts',(8.50747873128295,6.64621281334901,-10.7390979736876)) ;
#108232 = CARTESIAN_POINT('Ctrl Pts',(8.50729076020858,6.64628549377757,-10.7386229301939)) ;
#108233 = CARTESIAN_POINT('Ctrl Pts',(8.5072202710557,6.64631274893828,-10.7384447888838)) ;
#108234 = CARTESIAN_POINT('Ctrl Pts',(8.50715026706479,6.64633981850992,-10.7382664700193)) ;
#108235 = CARTESIAN_POINT('Ctrl Pts',(8.50708075128543,6.64636670806329,-10.7380879793595)) ;
#108236 = CARTESIAN_POINT('Ctrl Pts',(8.50659414082986,6.6465549349369,-10.736838544741)) ;
#108237 = CARTESIAN_POINT('Ctrl Pts',(8.5061314759289,6.64673434010344,-10.735580683755)) ;
#108238 = CARTESIAN_POINT('Ctrl Pts',(8.50569363751093,6.64690683932496,-10.7343164275023)) ;
#108239 = CARTESIAN_POINT('Ctrl Pts',(8.50395436040313,6.64759207829622,-10.7292942735102)) ;
#108240 = CARTESIAN_POINT('Ctrl Pts',(8.50258205288462,6.64816393978853,-10.724091559621)) ;
#108241 = CARTESIAN_POINT('Ctrl Pts',(8.50162662717307,6.64864720987411,-10.7188041247526)) ;
#108242 = CARTESIAN_POINT('Ctrl Pts',(8.50156399248323,6.64867889153345,-10.7184574972346)) ;
#108243 = CARTESIAN_POINT('Ctrl Pts',(8.50150313499629,6.6487101993589,-10.718110507519)) ;
#108244 = CARTESIAN_POINT('Ctrl Pts',(8.50144406283923,6.64874114271681,-10.717763183502)) ;
#108245 = CARTESIAN_POINT('Ctrl Pts',(8.50057491246565,6.64919642372272,-10.7126528774934)) ;
#108246 = CARTESIAN_POINT('Ctrl Pts',(8.50009537300572,6.64957062705852,-10.7074713290505)) ;
#108247 = CARTESIAN_POINT('Ctrl Pts',(8.50001293997569,6.64989933182553,-10.7023144435397)) ;
#108248 = CARTESIAN_POINT('Ctrl Pts',(8.50000430878269,6.64993374902796,-10.7017744891782)) ;
#108249 = CARTESIAN_POINT('Ctrl Pts',(8.5,6.64996765698298,-10.7012348144279)) ;
#108250 = CARTESIAN_POINT('Ctrl Pts',(8.5,6.65000108682384,-10.7006955361059)) ;
#108251 = CARTESIAN_POINT('',(8.55245136877624,6.6009799437261,-10.8067801193796)) ;
#108252 = CARTESIAN_POINT('Ctrl Pts',(8.55238056475493,6.60105295171775,-10.8068886154986)) ;
#108253 = CARTESIAN_POINT('Ctrl Pts',(8.55170523171899,6.60308542368598,-10.8051022656145)) ;
#108254 = CARTESIAN_POINT('Ctrl Pts',(8.55095829520335,6.60513808680204,-10.8033627348215)) ;
#108255 = CARTESIAN_POINT('Ctrl Pts',(8.55012599030478,6.6071915298049,-10.8016544441805)) ;
#108256 = CARTESIAN_POINT('Ctrl Pts',(8.54968322947846,6.60828389886617,-10.8007456856509)) ;
#108257 = CARTESIAN_POINT('Ctrl Pts',(8.54921644930851,6.60937569995309,-10.7998462491231)) ;
#108258 = CARTESIAN_POINT('Ctrl Pts',(8.54872481267394,6.61045954913298,-10.7989557465495)) ;
#108259 = CARTESIAN_POINT('Ctrl Pts',(8.54779539897816,6.61250851009549,-10.7972722973719)) ;
#108260 = CARTESIAN_POINT('Ctrl Pts',(8.54677348694547,6.61453549290076,-10.7956155908862)) ;
#108261 = CARTESIAN_POINT('Ctrl Pts',(8.54565366748546,6.6165071194701,-10.7939653182916)) ;
#108262 = CARTESIAN_POINT('',(8.55735473176743,6.58264207262467,-10.8249557973614)) ;
#108263 = CARTESIAN_POINT('Ctrl Pts',(8.55735473168698,6.58264207302803,-10.8249557968439)) ;
#108264 = CARTESIAN_POINT('Ctrl Pts',(8.55706916598051,6.58397660851281,-10.8232296933712)) ;
#108265 = CARTESIAN_POINT('Ctrl Pts',(8.55678088122702,6.58528501693267,-10.8216621009602)) ;
#108266 = CARTESIAN_POINT('Ctrl Pts',(8.5564740809182,6.58661569125897,-10.8201718232514)) ;
#108267 = CARTESIAN_POINT('Ctrl Pts',(8.55614409617578,6.5880469226241,-10.8185689275185)) ;
#108268 = CARTESIAN_POINT('Ctrl Pts',(8.55579261555188,6.58950524590115,-10.8170567950172)) ;
#108269 = CARTESIAN_POINT('Ctrl Pts',(8.55539993844504,6.59102291080536,-10.8155875677793)) ;
#108270 = CARTESIAN_POINT('Ctrl Pts',(8.55517214917306,6.59190329771265,-10.8147352792269)) ;
#108271 = CARTESIAN_POINT('Ctrl Pts',(8.5549304988196,6.59280308289164,-10.8138983977538)) ;
#108272 = CARTESIAN_POINT('Ctrl Pts',(8.55467134659044,6.59372113732161,-10.8130707946418)) ;
#108273 = CARTESIAN_POINT('Ctrl Pts',(8.55434805237167,6.59486641664526,-10.8120383539701)) ;
#108274 = CARTESIAN_POINT('Ctrl Pts',(8.55400737519029,6.59602723165038,-10.8110361981957)) ;
#108275 = CARTESIAN_POINT('Ctrl Pts',(8.55365328858767,6.59718920061513,-10.8100452155133)) ;
#108276 = CARTESIAN_POINT('Ctrl Pts',(8.5532816788869,6.59840867329807,-10.809005190911)) ;
#108277 = CARTESIAN_POINT('Ctrl Pts',(8.55289390107691,6.59963546460033,-10.8079736796762)) ;
#108278 = CARTESIAN_POINT('Ctrl Pts',(8.55249886556663,6.60083562835463,-10.8069081494348)) ;
#108279 = CARTESIAN_POINT('Ctrl Pts',(8.5524830476332,6.60088368507326,-10.8068654836845)) ;
#108280 = CARTESIAN_POINT('Ctrl Pts',(8.55246721522814,6.6009317901722,-10.806822806733)) ;
#108281 = CARTESIAN_POINT('Ctrl Pts',(8.55245136877624,6.6009799437261,-10.8067801193796)) ;
#108282 = CARTESIAN_POINT('Ctrl Pts',(8.56107669735261,6.5600938800009,-10.9223838472224)) ;
#108283 = CARTESIAN_POINT('Ctrl Pts',(8.56115635543005,6.55978170524809,-10.9208207343832)) ;
#108284 = CARTESIAN_POINT('Ctrl Pts',(8.56122592915386,6.55950119162287,-10.9192507129806)) ;
#108285 = CARTESIAN_POINT('Ctrl Pts',(8.56128584055879,6.55925348717443,-10.9176933919486)) ;
#108286 = CARTESIAN_POINT('Ctrl Pts',(8.56142626445294,6.55867290283843,-10.9140432508109)) ;
#108287 = CARTESIAN_POINT('Ctrl Pts',(8.56152217534693,6.55825854507367,-10.910375633877)) ;
#108288 = CARTESIAN_POINT('Ctrl Pts',(8.5615808174699,6.55798577878935,-10.9066701354254)) ;
#108289 = CARTESIAN_POINT('Ctrl Pts',(8.56158917845351,6.55794688875061,-10.9061418187433)) ;
#108290 = CARTESIAN_POINT('Ctrl Pts',(8.56159677639836,6.55791088241229,-10.9056126452595)) ;
#108291 = CARTESIAN_POINT('Ctrl Pts',(8.56160362608008,6.55787769947531,-10.9050824674717)) ;
#108292 = CARTESIAN_POINT('Ctrl Pts',(8.56164117305277,6.55769580506315,-10.902176263686)) ;
#108293 = CARTESIAN_POINT('Ctrl Pts',(8.56164095204358,6.55766773657216,-10.8992640119966)) ;
#108294 = CARTESIAN_POINT('Ctrl Pts',(8.5616130623009,6.55774920537472,-10.8963655672583)) ;
#108295 = CARTESIAN_POINT('Ctrl Pts',(8.56157759693123,6.55785280336171,-10.8926798246079)) ;
#108296 = CARTESIAN_POINT('Ctrl Pts',(8.56150275624661,6.55813669070951,-10.889004928021)) ;
#108297 = CARTESIAN_POINT('Ctrl Pts',(8.56141108129146,6.55856506509338,-10.8853632925482)) ;
#108298 = CARTESIAN_POINT('Ctrl Pts',(8.56136615997221,6.55877497130414,-10.883578867681)) ;
#108299 = CARTESIAN_POINT('Ctrl Pts',(8.56131707129298,6.55902016312284,-10.8818016709684)) ;
#108300 = CARTESIAN_POINT('Ctrl Pts',(8.56126585691692,6.55929956116446,-10.8800315254682)) ;
#108301 = CARTESIAN_POINT('Ctrl Pts',(8.56116752027493,6.55983603289967,-10.8766326719095)) ;
#108302 = CARTESIAN_POINT('Ctrl Pts',(8.56104954130216,6.56049109659203,-10.8732540075756)) ;
#108303 = CARTESIAN_POINT('Ctrl Pts',(8.56091150449775,6.56129147625802,-10.8698304710248)) ;
#108304 = CARTESIAN_POINT('Ctrl Pts',(8.56080235670743,6.56192434857305,-10.8671234288616)) ;
#108305 = CARTESIAN_POINT('Ctrl Pts',(8.56068045333715,6.56264902401855,-10.8643872666893)) ;
#108306 = CARTESIAN_POINT('Ctrl Pts',(8.56054379825318,6.56349285586902,-10.8616234877211)) ;
#108307 = CARTESIAN_POINT('Ctrl Pts',(8.56050762866484,6.56371619955871,-10.860891976352)) ;
#108308 = CARTESIAN_POINT('Ctrl Pts',(8.56047042218818,6.56394794674724,-10.8601587916983)) ;
#108309 = CARTESIAN_POINT('Ctrl Pts',(8.56043213901761,6.56418871538695,-10.8594246234709)) ;
#108310 = CARTESIAN_POINT('Ctrl Pts',(8.56026887460239,6.56521550994376,-10.8562936511792)) ;
#108311 = CARTESIAN_POINT('Ctrl Pts',(8.56008532870545,6.56636514336274,-10.8532612149347)) ;
#108312 = CARTESIAN_POINT('Ctrl Pts',(8.5598891591871,6.56762686151827,-10.8504713276669)) ;
#108313 = CARTESIAN_POINT('Ctrl Pts',(8.55964574654527,6.5691924368027,-10.8470095572757)) ;
#108314 = CARTESIAN_POINT('Ctrl Pts',(8.55938661160132,6.57080906160866,-10.843732634051)) ;
#108315 = CARTESIAN_POINT('Ctrl Pts',(8.55911582090257,6.57246439798289,-10.840667212428)) ;
#108316 = CARTESIAN_POINT('Ctrl Pts',(8.55888928658551,6.5738491962672,-10.8381027846354)) ;
#108317 = CARTESIAN_POINT('Ctrl Pts',(8.5586381350289,6.57544444689329,-10.8353653454312)) ;
#108318 = CARTESIAN_POINT('Ctrl Pts',(8.55834707044208,6.57718152485395,-10.832668125823)) ;
#108319 = CARTESIAN_POINT('Ctrl Pts',(8.55828762047112,6.57753632320108,-10.8321172184483)) ;
#108320 = CARTESIAN_POINT('Ctrl Pts',(8.55822651695171,6.57789694345782,-10.8315678465791)) ;
#108321 = CARTESIAN_POINT('Ctrl Pts',(8.55816364958868,6.57826264684155,-10.8310215710793)) ;
#108322 = CARTESIAN_POINT('Ctrl Pts',(8.55792499569721,6.57965091145842,-10.828947827764)) ;
#108323 = CARTESIAN_POINT('Ctrl Pts',(8.5576603261423,6.58110993502793,-10.8269213132876)) ;
#108324 = CARTESIAN_POINT('Ctrl Pts',(8.55735473176743,6.58264207262467,-10.8249557973614)) ;
#108325 = CARTESIAN_POINT('Origin',(8.49172374697018,6.65,-12.7)) ;
#108326 = CARTESIAN_POINT('Origin',(8.49226931255791,6.63793757615624,-10.9329882716319)) ;
#108327 = CARTESIAN_POINT('Ctrl Pts',(8.40188506081778,6.5500005341705,-10.6715458308154)) ;
#108328 = CARTESIAN_POINT('Ctrl Pts',(8.50280744587441,6.54966497091139,-10.6851950407542)) ;
#108329 = CARTESIAN_POINT('Ctrl Pts',(8.50109204799973,6.65199687180763,-10.6856804549399)) ;
#108330 = CARTESIAN_POINT('Ctrl Pts',(8.39296932930807,6.55000052027914,-10.7296758024219)) ;
#108331 = CARTESIAN_POINT('Ctrl Pts',(8.49725036372766,6.54968051003383,-10.7169136026831)) ;
#108332 = CARTESIAN_POINT('Ctrl Pts',(8.4966529651636,6.649356723178,-10.7160247114635)) ;
#108333 = CARTESIAN_POINT('Ctrl Pts',(8.4114607955856,6.55000052635931,-10.7896088846459)) ;
#108334 = CARTESIAN_POINT('Ctrl Pts',(8.50278789772746,6.54967384197898,-10.7410143519806)) ;
#108335 = CARTESIAN_POINT('Ctrl Pts',(8.50590954255551,6.65051247736746,-10.7444272120936)) ;
#108336 = CARTESIAN_POINT('Ctrl Pts',(8.45744515914182,6.55000045243508,-10.8428021918821)) ;
#108337 = CARTESIAN_POINT('Ctrl Pts',(8.52023811680809,6.54973725194868,-10.781633015821)) ;
#108338 = CARTESIAN_POINT('Ctrl Pts',(8.5289172307313,6.63643009777376,-10.7734751630783)) ;
#108339 = CARTESIAN_POINT('Ctrl Pts',(8.46608867121689,6.55000043643008,-10.8511950991747)) ;
#108340 = CARTESIAN_POINT('Ctrl Pts',(8.52334270167617,6.54974993059837,-10.7884702400789)) ;
#108341 = CARTESIAN_POINT('Ctrl Pts',(8.53324349789231,6.63337968978886,-10.7782208913001)) ;
#108342 = CARTESIAN_POINT('Ctrl Pts',(8.48465388181691,6.55000038323734,-10.8665763138744)) ;
#108343 = CARTESIAN_POINT('Ctrl Pts',(8.53001210036428,6.5497893864682,-10.8051245951232)) ;
#108344 = CARTESIAN_POINT('Ctrl Pts',(8.54253954944034,6.6232371034799,-10.788863146269)) ;
#108345 = CARTESIAN_POINT('Ctrl Pts',(8.49467048074917,6.55000035131511,-10.8734884944613)) ;
#108346 = CARTESIAN_POINT('Ctrl Pts',(8.53347884787438,6.54981166882502,-10.8130590311501)) ;
#108347 = CARTESIAN_POINT('Ctrl Pts',(8.54755337534731,6.61714793548855,-10.7928676881263)) ;
#108348 = CARTESIAN_POINT('Ctrl Pts',(8.50997930894009,6.55000022766094,-10.8833889027857)) ;
#108349 = CARTESIAN_POINT('Ctrl Pts',(8.5386903515922,6.54988741100168,-10.8387742327548)) ;
#108350 = CARTESIAN_POINT('Ctrl Pts',(8.55523846583761,6.59353839814627,-10.8135278831083)) ;
#108351 = CARTESIAN_POINT('Ctrl Pts',(8.51532901080107,6.55000016113069,-10.8863389673192)) ;
#108352 = CARTESIAN_POINT('Ctrl Pts',(8.54023459682689,6.54992340374046,-10.848489748387)) ;
#108353 = CARTESIAN_POINT('Ctrl Pts',(8.55790835982308,6.58082417519551,-10.8215823085726)) ;
#108354 = CARTESIAN_POINT('Ctrl Pts',(8.52186010906347,6.55000005932357,-10.8927927598772)) ;
#108355 = CARTESIAN_POINT('Ctrl Pts',(8.54265823247977,6.5499732773141,-10.8779316441153)) ;
#108356 = CARTESIAN_POINT('Ctrl Pts',(8.56121746518601,6.56135337205744,-10.8645883700756)) ;
#108357 = CARTESIAN_POINT('Ctrl Pts',(8.52354993939972,6.55000003603139,-10.8958242622279)) ;
#108358 = CARTESIAN_POINT('Ctrl Pts',(8.54350769968241,6.54998394755847,-10.8914238732007)) ;
#108359 = CARTESIAN_POINT('Ctrl Pts',(8.5621431061544,6.55689632415131,-10.8874501335625)) ;
#108360 = CARTESIAN_POINT('Ctrl Pts',(8.52268461318112,6.55000004733863,-10.9017875304158)) ;
#108361 = CARTESIAN_POINT('Ctrl Pts',(8.54305517585924,6.54997881410037,-10.91281341214)) ;
#108362 = CARTESIAN_POINT('Ctrl Pts',(8.5615325917139,6.55906016573919,-10.9227901815805)) ;
#108363 = CARTESIAN_POINT('Ctrl Pts',(8.52060566253928,6.55000006807331,-10.9044138065497)) ;
#108364 = CARTESIAN_POINT('Ctrl Pts',(8.54195943530538,6.54996919659463,-10.9204945748859)) ;
#108365 = CARTESIAN_POINT('Ctrl Pts',(8.56058441628599,6.56302742363386,-10.9345079215137)) ;
#108366 = CARTESIAN_POINT('Ctrl Pts',(8.51445291480387,6.55000012130567,-10.9112328149553)) ;
#108367 = CARTESIAN_POINT('Ctrl Pts',(8.53868948987838,6.54994355920611,-10.9394191817675)) ;
#108368 = CARTESIAN_POINT('Ctrl Pts',(8.55750149922673,6.57320954252653,-10.9611844353068)) ;
#108369 = CARTESIAN_POINT('Ctrl Pts',(8.50953280296017,6.55000015625148,-10.9150479464373)) ;
#108370 = CARTESIAN_POINT('Ctrl Pts',(8.53616288920968,6.54992588038507,-10.9477647485266)) ;
#108371 = CARTESIAN_POINT('Ctrl Pts',(8.55504783006515,6.57989127253964,-10.9706993167928)) ;
#108372 = CARTESIAN_POINT('Ctrl Pts',(8.49261655785715,6.55000026291039,-10.928492606569)) ;
#108373 = CARTESIAN_POINT('Ctrl Pts',(8.52778251455091,6.5498671840875,-10.9757691608948)) ;
#108374 = CARTESIAN_POINT('Ctrl Pts',(8.54658667616929,6.60027178071329,-10.9993533757438)) ;
#108375 = CARTESIAN_POINT('Ctrl Pts',(8.48022165824505,6.55000031608562,-10.9377685341603)) ;
#108376 = CARTESIAN_POINT('Ctrl Pts',(8.52288681814155,6.54983437262023,-10.987455948929)) ;
#108377 = CARTESIAN_POINT('Ctrl Pts',(8.5404533945046,6.61042388759274,-11.0063019909605)) ;
#108378 = CARTESIAN_POINT('Ctrl Pts',(8.46952991654832,6.55000035836672,-10.9490954462194)) ;
#108379 = CARTESIAN_POINT('Ctrl Pts',(8.51900842894258,6.54980714069637,-11.0033676846771)) ;
#108380 = CARTESIAN_POINT('Ctrl Pts',(8.53471369258706,6.61849392543723,-11.021383368443)) ;
#108381 = CARTESIAN_POINT('Origin',(8.4,6.65,-10.7006780018997)) ;
#108382 = CARTESIAN_POINT('Ctrl Pts',(8.54848814460234,8.28374914930622,-9.40353717477989)) ;
#108383 = CARTESIAN_POINT('Ctrl Pts',(8.55964225199693,8.27720012980426,-9.40496794832229)) ;
#108384 = CARTESIAN_POINT('Ctrl Pts',(8.572140519951,8.27365818248462,-9.40574176255693)) ;
#108385 = CARTESIAN_POINT('Ctrl Pts',(8.54519582228985,8.29111303851996,-9.4279603788076)) ;
#108386 = CARTESIAN_POINT('Ctrl Pts',(8.55569959891137,8.28406912459881,-9.42803761744086)) ;
#108387 = CARTESIAN_POINT('Ctrl Pts',(8.56757951573628,8.27991709749371,-9.42819163391183)) ;
#108388 = CARTESIAN_POINT('Ctrl Pts',(8.54340782920288,8.28927570119136,-9.45382299312326)) ;
#108389 = CARTESIAN_POINT('Ctrl Pts',(8.55355053837511,8.282326185643,-9.45215464428979)) ;
#108390 = CARTESIAN_POINT('Ctrl Pts',(8.56507848568421,8.27803412520746,-9.45113214305331)) ;
#108391 = CARTESIAN_POINT('Ctrl Pts',(8.54340835145922,8.27841951799441,-9.47553501116171)) ;
#108392 = CARTESIAN_POINT('Ctrl Pts',(8.55355093564017,8.27219257320284,-9.47242153876592)) ;
#108393 = CARTESIAN_POINT('Ctrl Pts',(8.56507848521152,8.26835005667905,-9.47050028050403)) ;
#108394 = CARTESIAN_POINT('Ctrl Pts',(8.54742026180265,8.27608084857565,-9.4743656412486)) ;
#108395 = CARTESIAN_POINT('Ctrl Pts',(8.54754672558908,8.27683897030433,-9.47267457303652)) ;
#108396 = CARTESIAN_POINT('Ctrl Pts',(8.54766225486891,8.27755642830997,-9.47096549730836)) ;
#108397 = CARTESIAN_POINT('Ctrl Pts',(8.54776713596766,8.27823455672264,-9.46923501677752)) ;
#108398 = CARTESIAN_POINT('Ctrl Pts',(8.54791712013336,8.27920430747293,-9.46676036041189)) ;
#108399 = CARTESIAN_POINT('Ctrl Pts',(8.54806168001142,8.28008011045348,-9.46424633726765)) ;
#108400 = CARTESIAN_POINT('Ctrl Pts',(8.54818998754192,8.28086237513953,-9.461718683859)) ;
#108401 = CARTESIAN_POINT('Ctrl Pts',(8.5482419492675,8.28117917511833,-9.46069503986669)) ;
#108402 = CARTESIAN_POINT('Ctrl Pts',(8.54829140719363,8.28148078264968,-9.45966867429037)) ;
#108403 = CARTESIAN_POINT('Ctrl Pts',(8.54833813644415,8.28176759858573,-9.45863962997721)) ;
#108404 = CARTESIAN_POINT('Ctrl Pts',(8.54850061324771,8.28276485268195,-9.4550616605289)) ;
#108405 = CARTESIAN_POINT('Ctrl Pts',(8.54863339756397,8.28360845633787,-9.45135012352872)) ;
#108406 = CARTESIAN_POINT('Ctrl Pts',(8.54873421749658,8.28426438239348,-9.44761308675746)) ;
#108407 = CARTESIAN_POINT('Ctrl Pts',(8.54878752953697,8.28461122607277,-9.445636998794)) ;
#108408 = CARTESIAN_POINT('Ctrl Pts',(8.54883168679926,8.2849064071404,-9.44365408207379)) ;
#108409 = CARTESIAN_POINT('Ctrl Pts',(8.54886500248132,8.28515040605084,-9.44168185902952)) ;
#108410 = CARTESIAN_POINT('Ctrl Pts',(8.5488738542235,8.28521523484357,-9.44115785325128)) ;
#108411 = CARTESIAN_POINT('Ctrl Pts',(8.54888411330031,8.285275121517,-9.44063500919221)) ;
#108412 = CARTESIAN_POINT('Ctrl Pts',(8.54889386083023,8.2853314308609,-9.44011208678616)) ;
#108413 = CARTESIAN_POINT('Ctrl Pts',(8.54894969070931,8.28565394783543,-9.43711700034693)) ;
#108414 = CARTESIAN_POINT('Ctrl Pts',(8.5489793513821,8.28586680424119,-9.43409863638302)) ;
#108415 = CARTESIAN_POINT('Ctrl Pts',(8.54899968230028,8.28595875954336,-9.43106757780142)) ;
#108416 = CARTESIAN_POINT('Ctrl Pts',(8.54900356561227,8.28597632348829,-9.43048862971749)) ;
#108417 = CARTESIAN_POINT('Ctrl Pts',(8.54900713937599,8.28598945835116,-9.42990930880417)) ;
#108418 = CARTESIAN_POINT('Ctrl Pts',(8.54901057288909,8.28599806377619,-9.42932984021849)) ;
#108419 = CARTESIAN_POINT('Ctrl Pts',(8.54902784271198,8.28604134718934,-9.42641523947596)) ;
#108420 = CARTESIAN_POINT('Ctrl Pts',(8.54901619593281,8.28598556136223,-9.4235157757218)) ;
#108421 = CARTESIAN_POINT('Ctrl Pts',(8.5489843126011,8.28582669412323,-9.42060642867561)) ;
#108422 = CARTESIAN_POINT('Ctrl Pts',(8.54893914418925,8.28560163041442,-9.41648482096991)) ;
#108423 = CARTESIAN_POINT('Ctrl Pts',(8.54884805310403,8.28517290646448,-9.41237709996714)) ;
#108424 = CARTESIAN_POINT('Ctrl Pts',(8.54869940582915,8.28455561418431,-9.40830707741439)) ;
#108425 = CARTESIAN_POINT('Ctrl Pts',(8.54864697316337,8.28433787538059,-9.40687144980293)) ;
#108426 = CARTESIAN_POINT('Ctrl Pts',(8.54858736435355,8.2840967659742,-9.40544083959257)) ;
#108427 = CARTESIAN_POINT('Ctrl Pts',(8.54851996240544,8.28383343043592,-9.40401720308528)) ;
#108428 = CARTESIAN_POINT('Origin',(8.4,6.65,-12.7)) ;
#108429 = CARTESIAN_POINT('Origin',(8.4,6.65,-9.6193219981003)) ;
#108430 = CARTESIAN_POINT('Origin',(8.49172374697018,6.65,-12.7)) ;
#108431 = CARTESIAN_POINT('Origin',(8.4922548564967,6.63809817877304,-9.38700862834994)) ;
#108432 = CARTESIAN_POINT('Origin',(8.6,4.35421736843756,-9.61971270883831)) ;
#108433 = CARTESIAN_POINT('Origin',(8.6,6.66256607592813,-9.61971270883831)) ;
#108434 = CARTESIAN_POINT('Ctrl Pts',(8.50134874936241,6.65217253603383,-9.63598525608075)) ;
#108435 = CARTESIAN_POINT('Ctrl Pts',(8.50315244876583,6.5499712757702,-9.63658636925848)) ;
#108436 = CARTESIAN_POINT('Ctrl Pts',(8.40269444133659,6.55000000392137,-9.6515964965758)) ;
#108437 = CARTESIAN_POINT('Ctrl Pts',(8.4963175378395,6.6493370187709,-9.60501565239566)) ;
#108438 = CARTESIAN_POINT('Ctrl Pts',(8.49707874924871,6.54997270174421,-9.60396122349838)) ;
#108439 = CARTESIAN_POINT('Ctrl Pts',(8.39261127161985,6.55000000381175,-9.59255502081079)) ;
#108440 = CARTESIAN_POINT('Ctrl Pts',(8.50556246021205,6.65075235208957,-9.57601104550147)) ;
#108441 = CARTESIAN_POINT('Ctrl Pts',(8.50253957946704,6.54997202229482,-9.57964413045453)) ;
#108442 = CARTESIAN_POINT('Ctrl Pts',(8.41103525938988,6.55000000386643,-9.53133834963448)) ;
#108443 = CARTESIAN_POINT('Ctrl Pts',(8.52891970071471,6.63645479210457,-9.54652715848278)) ;
#108444 = CARTESIAN_POINT('Ctrl Pts',(8.52027792490147,6.54997752826668,-9.53840493996115)) ;
#108445 = CARTESIAN_POINT('Ctrl Pts',(8.4576425585103,6.5500000033157,-9.47739010158303)) ;
#108446 = CARTESIAN_POINT('Ctrl Pts',(8.53324635448929,6.63340383613804,-9.54178206573817)) ;
#108447 = CARTESIAN_POINT('Ctrl Pts',(8.52338394863782,6.54997861189313,-9.53157331389089)) ;
#108448 = CARTESIAN_POINT('Ctrl Pts',(8.46627109069292,6.55000000319827,-9.4690047485327)) ;
#108449 = CARTESIAN_POINT('Ctrl Pts',(8.54254332011239,6.62325922024831,-9.53114174821779)) ;
#108450 = CARTESIAN_POINT('Ctrl Pts',(8.53005572430512,6.54998198465676,-9.51493264246807)) ;
#108451 = CARTESIAN_POINT('Ctrl Pts',(8.48480454940901,6.55000000280808,-9.45362780882311)) ;
#108452 = CARTESIAN_POINT('Ctrl Pts',(8.54755771953123,6.61716872587379,-9.52713854387739)) ;
#108453 = CARTESIAN_POINT('Ctrl Pts',(8.53352383957155,6.54998388968238,-9.5070066149148)) ;
#108454 = CARTESIAN_POINT('Ctrl Pts',(8.49480263348501,6.55000000257396,-9.44671727629916)) ;
#108455 = CARTESIAN_POINT('Ctrl Pts',(8.55524400651032,6.59355301617583,-9.50648056989544)) ;
#108456 = CARTESIAN_POINT('Ctrl Pts',(8.53873552501328,6.54999036710749,-9.48129485880943)) ;
#108457 = CARTESIAN_POINT('Ctrl Pts',(8.51008526949052,6.55000000166752,-9.43677574941853)) ;
#108458 = CARTESIAN_POINT('Ctrl Pts',(8.55791451833573,6.58083494429021,-9.49842706746385)) ;
#108459 = CARTESIAN_POINT('Ctrl Pts',(8.54027978136636,6.54999344602542,-9.47157902883428)) ;
#108460 = CARTESIAN_POINT('Ctrl Pts',(8.51542462880457,6.55000000118004,-9.43380634433862)) ;
#108461 = CARTESIAN_POINT('Ctrl Pts',(8.56122429319342,6.56135755929237,-9.45541653896343)) ;
#108462 = CARTESIAN_POINT('Ctrl Pts',(8.54270214007071,6.54999771321876,-9.44209990564423)) ;
#108463 = CARTESIAN_POINT('Ctrl Pts',(8.52194436340203,6.55000000043437,-9.42726744367389)) ;
#108464 = CARTESIAN_POINT('Ctrl Pts',(8.56215003896757,6.55689889598544,-9.43255134475621)) ;
#108465 = CARTESIAN_POINT('Ctrl Pts',(8.54355112280984,6.54999862629018,-9.42858541402148)) ;
#108466 = CARTESIAN_POINT('Ctrl Pts',(8.52363168464777,6.55000000026381,-9.42419376079454)) ;
#108467 = CARTESIAN_POINT('Ctrl Pts',(8.56153943432817,6.55906352913392,-9.39720612379093)) ;
#108468 = CARTESIAN_POINT('Ctrl Pts',(8.54309854033144,6.5499981870035,-9.40716316826849)) ;
#108469 = CARTESIAN_POINT('Ctrl Pts',(8.52276767133746,6.5500000003466,-9.41816751318002)) ;
#108470 = CARTESIAN_POINT('Ctrl Pts',(8.56059123720042,6.56303220640812,-9.38548694646253)) ;
#108471 = CARTESIAN_POINT('Ctrl Pts',(8.54200379397878,6.54999736403672,-9.39947204706566)) ;
#108472 = CARTESIAN_POINT('Ctrl Pts',(8.52069177703237,6.55000000049844,-9.41552134373608)) ;
#108473 = CARTESIAN_POINT('Ctrl Pts',(8.55750819780173,6.57321782814891,-9.35880781453251)) ;
#108474 = CARTESIAN_POINT('Ctrl Pts',(8.53873610184734,6.54999517041881,-9.38052685964291)) ;
#108475 = CARTESIAN_POINT('Ctrl Pts',(8.51454797734041,6.55000000088831,-9.40865663082411)) ;
#108476 = CARTESIAN_POINT('Ctrl Pts',(8.55505442469282,6.57990173798309,-9.34929267446123)) ;
#108477 = CARTESIAN_POINT('Ctrl Pts',(8.53621107118182,6.54999365791211,-9.37217666040664)) ;
#108478 = CARTESIAN_POINT('Ctrl Pts',(8.50963525726155,6.55000000114429,-9.40482618291573)) ;
#108479 = CARTESIAN_POINT('Ctrl Pts',(8.55022399280474,6.59153973477787,-9.33293520591855)) ;
#108480 = CARTESIAN_POINT('Ctrl Pts',(8.53156015545169,6.54999086985382,-9.35662116717933)) ;
#108481 = CARTESIAN_POINT('Ctrl Pts',(8.49999539447558,6.55000000159032,-9.3971278236794)) ;
#108482 = CARTESIAN_POINT('Ctrl Pts',(8.54779538881609,6.59665349532941,-9.32691619169829)) ;
#108483 = CARTESIAN_POINT('Ctrl Pts',(8.5293657515114,6.54998957391998,-9.34999554735591)) ;
#108484 = CARTESIAN_POINT('Ctrl Pts',(8.49512741158075,6.55000000178643,-9.39333641589862)) ;
#108485 = CARTESIAN_POINT('Ctrl Pts',(8.54538355337156,6.60121171185029,-9.32167517448425)) ;
#108486 = CARTESIAN_POINT('Ctrl Pts',(8.52733415536172,6.54998837980797,-9.34389835720993)) ;
#108487 = CARTESIAN_POINT('Ctrl Pts',(8.49033880598513,6.55000000196131,-9.38944859709871)) ;
#108488 = CARTESIAN_POINT('',(8.54582344182381,6.61635369861669,-9.52606365157295)) ;
#108489 = CARTESIAN_POINT('Ctrl Pts',(8.54582344182381,6.61635369861669,-9.52606365157295)) ;
#108490 = CARTESIAN_POINT('Ctrl Pts',(8.54493595163519,6.61793460914654,-9.52739407620991)) ;
#108491 = CARTESIAN_POINT('Ctrl Pts',(8.5439844817107,6.61948114927954,-9.52871739283071)) ;
#108492 = CARTESIAN_POINT('Ctrl Pts',(8.54296332801272,6.6209780844369,-9.53004073677983)) ;
#108493 = CARTESIAN_POINT('Ctrl Pts',(8.53827263106763,6.62785429629763,-9.53611955276191)) ;
#108494 = CARTESIAN_POINT('Ctrl Pts',(8.53198779426187,6.63349037496299,-9.54261156852439)) ;
#108495 = CARTESIAN_POINT('Ctrl Pts',(8.5259873730411,6.63731070037229,-9.5500705892422)) ;
#108496 = CARTESIAN_POINT('Ctrl Pts',(8.52000560405467,6.64111915034781,-9.55750642368737)) ;
#108497 = CARTESIAN_POINT('Ctrl Pts',(8.51430181273566,6.64349626850742,-9.56603764730141)) ;
#108498 = CARTESIAN_POINT('Ctrl Pts',(8.50998586672548,6.64522349213896,-9.57520098697005)) ;
#108499 = CARTESIAN_POINT('Ctrl Pts',(8.50534188065424,6.64708199603772,-9.58506080025014)) ;
#108500 = CARTESIAN_POINT('Ctrl Pts',(8.50212992821339,6.64824261275105,-9.59588754367484)) ;
#108501 = CARTESIAN_POINT('Ctrl Pts',(8.50077314609738,6.64911992656046,-9.60682491191675)) ;
#108502 = CARTESIAN_POINT('Ctrl Pts',(8.50025986706873,6.64945181977648,-9.61096258566769)) ;
#108503 = CARTESIAN_POINT('Ctrl Pts',(8.50000017127792,6.64974165917873,-9.61514325510124)) ;
#108504 = CARTESIAN_POINT('Ctrl Pts',(8.5000000000847,6.64999974464544,-9.61931786749562)) ;
#108505 = CARTESIAN_POINT('',(8.55242393572493,6.60106172182543,-9.51324209871612)) ;
#108506 = CARTESIAN_POINT('Ctrl Pts',(8.55241775170034,6.60106807917178,-9.51323281615444)) ;
#108507 = CARTESIAN_POINT('Ctrl Pts',(8.55072388788561,6.6061902674336,-9.51772147695244)) ;
#108508 = CARTESIAN_POINT('Ctrl Pts',(8.5485829404857,6.61143812822774,-9.52192692414486)) ;
#108509 = CARTESIAN_POINT('Ctrl Pts',(8.54582344182381,6.61635369861669,-9.52606365157295)) ;
#108510 = CARTESIAN_POINT('Ctrl Pts',(8.55635360773813,6.58637108369506,-9.49863239073381)) ;
#108511 = CARTESIAN_POINT('Ctrl Pts',(8.55606387390184,6.58765239867384,-9.50011238280753)) ;
#108512 = CARTESIAN_POINT('Ctrl Pts',(8.55575324501783,6.5889682390236,-9.5015659413336)) ;
#108513 = CARTESIAN_POINT('Ctrl Pts',(8.55541196992769,6.59037241127503,-9.50304320494036)) ;
#108514 = CARTESIAN_POINT('Ctrl Pts',(8.5552429000838,6.59106804711314,-9.50377505069942)) ;
#108515 = CARTESIAN_POINT('Ctrl Pts',(8.5550663125072,6.59178496983021,-9.50451195883767)) ;
#108516 = CARTESIAN_POINT('Ctrl Pts',(8.55488049708425,6.59252693597571,-9.50525627761903)) ;
#108517 = CARTESIAN_POINT('Ctrl Pts',(8.55445908016384,6.59420966544519,-9.50694434270892)) ;
#108518 = CARTESIAN_POINT('Ctrl Pts',(8.55403589309456,6.59584037906531,-9.50848837772247)) ;
#108519 = CARTESIAN_POINT('Ctrl Pts',(8.55359592981646,6.59737680581849,-9.50990315623324)) ;
#108520 = CARTESIAN_POINT('Ctrl Pts',(8.55324292160433,6.59860957066092,-9.51103831559199)) ;
#108521 = CARTESIAN_POINT('Ctrl Pts',(8.55287861047124,6.59978201473818,-9.51209104250713)) ;
#108522 = CARTESIAN_POINT('Ctrl Pts',(8.55248933155914,6.60087815532545,-9.51307712698674)) ;
#108523 = CARTESIAN_POINT('Ctrl Pts',(8.55246754857564,6.6009394923555,-9.51313230557793)) ;
#108524 = CARTESIAN_POINT('Ctrl Pts',(8.55244574956029,6.60100068203153,-9.51318729627853)) ;
#108525 = CARTESIAN_POINT('Ctrl Pts',(8.55242393572493,6.60106172182543,-9.51324209871612)) ;
#108526 = CARTESIAN_POINT('Ctrl Pts',(8.5,6.66256607592813,-9.61971270883831)) ;
#108527 = CARTESIAN_POINT('Ctrl Pts',(8.5,6.66256607592813,-9.535)) ;
#108528 = CARTESIAN_POINT('Ctrl Pts',(8.58356010126947,6.66256607592813,-9.52107331645509)) ;
#108529 = CARTESIAN_POINT('Ctrl Pts',(8.5,6.61011302719829,-9.61971270726284)) ;
#108530 = CARTESIAN_POINT('Ctrl Pts',(8.5,6.63245216822978,-9.53855723659927)) ;
#108531 = CARTESIAN_POINT('Ctrl Pts',(8.5794176004298,6.63563981885128,-9.5217637332617)) ;
#108532 = CARTESIAN_POINT('Ctrl Pts',(8.5,6.55934573373317,-9.59884690994277)) ;
#108533 = CARTESIAN_POINT('Ctrl Pts',(8.5,6.60054351783575,-9.5280813958278)) ;
#108534 = CARTESIAN_POINT('Ctrl Pts',(8.57705842698407,6.60987578993432,-9.51172752804771)) ;
#108535 = CARTESIAN_POINT('Ctrl Pts',(8.5,6.52274941072028,-9.56225058927972)) ;
#108536 = CARTESIAN_POINT('Ctrl Pts',(8.5,6.57873105977929,-9.50626894022071)) ;
#108537 = CARTESIAN_POINT('Ctrl Pts',(8.57705842661295,6.59157413088145,-9.49342586911855)) ;
#108538 = CARTESIAN_POINT('Origin',(8.49172374697003,1.4,-12.7)) ;
#108539 = CARTESIAN_POINT('Origin',(8.49172374697003,1.4,-8.19785831296513)) ;
#108540 = CARTESIAN_POINT('Origin',(8.49172374697002,1.4,-8.19785831296513)) ;
#108541 = CARTESIAN_POINT('Origin',(8.49172374697003,1.4,-8.19785831296514)) ;
#108542 = CARTESIAN_POINT('Ctrl Pts',(8.50816364570057,1.49863939238321,-8.19785831296512)) ;
#108543 = CARTESIAN_POINT('Ctrl Pts',(8.51019246767907,1.4983012553868,-8.23292758407099)) ;
#108544 = CARTESIAN_POINT('Ctrl Pts',(8.50816364570057,1.47636598119991,-8.26029201095831)) ;
#108545 = CARTESIAN_POINT('Ctrl Pts',(8.97755831131126,1.42040694811477,-8.16994865115435)) ;
#108546 = CARTESIAN_POINT('Ctrl Pts',(8.9787999739868,1.42020000433582,-8.20456667318447)) ;
#108547 = CARTESIAN_POINT('Ctrl Pts',(8.97755831689146,1.39869563385688,-8.23169481695199)) ;
#108548 = CARTESIAN_POINT('Ctrl Pts',(9.44698496305968,1.34216917282337,-8.14263137063053)) ;
#108549 = CARTESIAN_POINT('Ctrl Pts',(9.44827639615869,1.34195393397321,-8.17677752860714)) ;
#108550 = CARTESIAN_POINT('Ctrl Pts',(9.4469849688788,1.32097764915795,-8.20372298471039)) ;
#108551 = CARTESIAN_POINT('Ctrl Pts',(9.91643989873053,1.26392668354489,-8.11583811982177)) ;
#108552 = CARTESIAN_POINT('Ctrl Pts',(9.91830968165731,1.26361505305709,-8.14950934419701)) ;
#108553 = CARTESIAN_POINT('Ctrl Pts',(9.91643989873053,1.24322097942674,-8.17630356419402)) ;
#108554 = CARTESIAN_POINT('Origin',(9.9,1.16528729116168,-8.1158381198218)) ;
#108555 = CARTESIAN_POINT('Origin',(9.9,1.16528729116168,-8.1158381198218)) ;
#108556 = CARTESIAN_POINT('Origin',(-0.4,-3.36847777691809,-10.56)) ;
#108557 = CARTESIAN_POINT('Origin',(-0.400000000000001,-3.36847777691809,
-10.56)) ;
#108558 = CARTESIAN_POINT('Origin',(-0.4,-3.36847777691809,-10.56)) ;
#108559 = CARTESIAN_POINT('Origin',(-0.400000000000001,-3.36847777691809,
-9.66)) ;
#108560 = CARTESIAN_POINT('Origin',(-0.4,-3.36847777691809,-9.76)) ;
#108561 = CARTESIAN_POINT('Origin',(-1.11032778078669,-3.36847777691809,-10.56)) ;
#108562 = CARTESIAN_POINT('Origin',(0.4,-3.36847777691809,-10.56)) ;
#108563 = CARTESIAN_POINT('Origin',(-0.400000000000001,-3.36847777691809,
-9.76)) ;
#108564 = CARTESIAN_POINT('Origin',(-0.4,-3.36847777691809,-9.76)) ;
#108565 = CARTESIAN_POINT('Origin',(0.400000000000001,-3.36847777691809,-10.56)) ;
#108566 = CARTESIAN_POINT('Origin',(0.400000000000001,-3.36847777691809,-10.56)) ;
#108567 = CARTESIAN_POINT('Origin',(1.5,-3.36847777691809,-9.76)) ;
#108568 = CARTESIAN_POINT('Origin',(0.4,-3.36847777691809,-9.76)) ;
#108569 = CARTESIAN_POINT('Origin',(0.4,-3.36847777691809,-9.66)) ;
#108570 = CARTESIAN_POINT('Origin',(0.4,-3.36847777691809,-9.76)) ;
#108571 = CARTESIAN_POINT('Origin',(0.4,-3.36847777691809,-9.76)) ;
#108572 = CARTESIAN_POINT('Origin',(7.96847777691809,3.4,-10.56)) ;
#108573 = CARTESIAN_POINT('Origin',(7.96847777691809,3.4,-10.56)) ;
#108574 = CARTESIAN_POINT('Origin',(7.96847777691809,3.4,-10.56)) ;
#108575 = CARTESIAN_POINT('Origin',(7.96847777691809,3.4,-9.66)) ;
#108576 = CARTESIAN_POINT('Origin',(7.96847777691809,3.4,-9.76)) ;
#108577 = CARTESIAN_POINT('Origin',(7.96847777691809,2.68967221921331,-10.56)) ;
#108578 = CARTESIAN_POINT('Origin',(7.96847777691809,4.2,-10.56)) ;
#108579 = CARTESIAN_POINT('Origin',(7.96847777691809,3.4,-9.76)) ;
#108580 = CARTESIAN_POINT('Origin',(7.96847777691809,3.4,-9.76)) ;
#108581 = CARTESIAN_POINT('Origin',(7.96847777691809,4.2,-10.56)) ;
#108582 = CARTESIAN_POINT('Origin',(7.96847777691809,4.2,-10.56)) ;
#108583 = CARTESIAN_POINT('Origin',(7.96847777691809,2.3,-9.76)) ;
#108584 = CARTESIAN_POINT('Origin',(7.96847777691809,4.2,-9.76)) ;
#108585 = CARTESIAN_POINT('Origin',(7.96847777691809,4.2,-9.66)) ;
#108586 = CARTESIAN_POINT('Origin',(7.96847777691809,4.2,-9.76)) ;
#108587 = CARTESIAN_POINT('Origin',(7.96847777691809,4.2,-9.76)) ;
#108588 = CARTESIAN_POINT('Origin',(8.49172374697003,1.4,-12.7)) ;
#108589 = CARTESIAN_POINT('Origin',(8.49172374697003,1.4,-12.1221416870349)) ;
#108590 = CARTESIAN_POINT('Origin',(8.49172374697002,1.4,-12.1221416870349)) ;
#108591 = CARTESIAN_POINT('Origin',(8.49172374697003,1.39999999999989,-12.1221416870347)) ;
#108592 = CARTESIAN_POINT('Ctrl Pts',(8.50816364570058,1.47636598119991,-12.0597079890417)) ;
#108593 = CARTESIAN_POINT('Ctrl Pts',(8.51019246767908,1.4983012553868,-12.087072415929)) ;
#108594 = CARTESIAN_POINT('Ctrl Pts',(8.50816364570058,1.49863939238321,-12.1221416870349)) ;
#108595 = CARTESIAN_POINT('Ctrl Pts',(8.97755831689155,1.39869563385768,-12.088305183049)) ;
#108596 = CARTESIAN_POINT('Ctrl Pts',(8.97879997398666,1.42020000433619,-12.1154333268189)) ;
#108597 = CARTESIAN_POINT('Ctrl Pts',(8.97755831131117,1.42040694811478,-12.1500513488473)) ;
#108598 = CARTESIAN_POINT('Ctrl Pts',(9.44698496887881,1.32097764915819,-12.1162770152899)) ;
#108599 = CARTESIAN_POINT('Ctrl Pts',(9.44827639615871,1.34195393397346,-12.1432224713932)) ;
#108600 = CARTESIAN_POINT('Ctrl Pts',(9.44698496305967,1.34216917282337,-12.1773686293698)) ;
#108601 = CARTESIAN_POINT('Ctrl Pts',(9.91643989873053,1.24322097942674,-12.143696435806)) ;
#108602 = CARTESIAN_POINT('Ctrl Pts',(9.91830968165732,1.26361505305709,-12.170490655803)) ;
#108603 = CARTESIAN_POINT('Ctrl Pts',(9.91643989873053,1.26392668354489,-12.2041618801782)) ;
#108604 = CARTESIAN_POINT('Origin',(9.9,1.16528729116168,-12.2041618801782)) ;
#108605 = CARTESIAN_POINT('Origin',(9.9,1.16528729116168,-12.2041618801782)) ;
#108606 = CARTESIAN_POINT('Origin',(8.48377223398316,8.2,-12.7)) ;
#108607 = CARTESIAN_POINT('Origin',(8.48238054867516,8.20007133354354,-9.41317893123556)) ;
#108608 = CARTESIAN_POINT('Ctrl Pts',(8.40201662970151,8.3,-9.64597597792138)) ;
#108609 = CARTESIAN_POINT('Ctrl Pts',(8.50299337454951,8.3,-9.63267481126358)) ;
#108610 = CARTESIAN_POINT('Ctrl Pts',(8.50100123624933,8.19773961376461,-9.63268884611774)) ;
#108611 = CARTESIAN_POINT('Ctrl Pts',(8.39454129798956,8.3,-9.59449818135068)) ;
#108612 = CARTESIAN_POINT('Ctrl Pts',(8.49697875237678,8.3,-9.60537411133466)) ;
#108613 = CARTESIAN_POINT('Ctrl Pts',(8.49727262260755,8.20135231978528,-9.60506706396228)) ;
#108614 = CARTESIAN_POINT('Ctrl Pts',(8.40820218948348,8.3,-9.54202536352426)) ;
#108615 = CARTESIAN_POINT('Ctrl Pts',(8.49818669687004,8.3,-9.58247172780125)) ;
#108616 = CARTESIAN_POINT('Ctrl Pts',(8.50412619268403,8.20300739730715,-9.58038841002482)) ;
#108617 = CARTESIAN_POINT('Ctrl Pts',(8.4430413476632,8.3,-9.49099693308713)) ;
#108618 = CARTESIAN_POINT('Ctrl Pts',(8.50894174387209,8.3,-9.54085505538057)) ;
#108619 = CARTESIAN_POINT('Ctrl Pts',(8.52157716465942,8.21896555381603,-9.55016612665033)) ;
#108620 = CARTESIAN_POINT('Ctrl Pts',(8.44963266995283,8.3,-9.48266783197822)) ;
#108621 = CARTESIAN_POINT('Ctrl Pts',(8.51095981317518,8.3,-9.5337494404835)) ;
#108622 = CARTESIAN_POINT('Ctrl Pts',(8.52487915500778,8.22226238914487,-9.54495161805188)) ;
#108623 = CARTESIAN_POINT('Ctrl Pts',(8.46372306360152,8.3,-9.46695472631993)) ;
#108624 = CARTESIAN_POINT('Ctrl Pts',(8.51547368264944,8.3,-9.51763279105592)) ;
#108625 = CARTESIAN_POINT('Ctrl Pts',(8.53193863144478,8.23129792829965,-9.53331747838551)) ;
#108626 = CARTESIAN_POINT('Ctrl Pts',(8.47128983770084,8.3,-9.45955862714639)) ;
#108627 = CARTESIAN_POINT('Ctrl Pts',(8.51796237042372,8.3,-9.50924649491276)) ;
#108628 = CARTESIAN_POINT('Ctrl Pts',(8.53572833262714,8.23677343862357,-9.52742958850775)) ;
#108629 = CARTESIAN_POINT('Ctrl Pts',(8.48287565264707,8.3,-9.44873079483315)) ;
#108630 = CARTESIAN_POINT('Ctrl Pts',(8.52168214469875,8.3,-9.49074351942998)) ;
#108631 = CARTESIAN_POINT('Ctrl Pts',(8.54153766811346,8.25077321967988,-9.51204498710733)) ;
#108632 = CARTESIAN_POINT('Ctrl Pts',(8.48680760428678,8.3,-9.445187297402)) ;
#108633 = CARTESIAN_POINT('Ctrl Pts',(8.52287759291299,8.3,-9.48414350493172)) ;
#108634 = CARTESIAN_POINT('Ctrl Pts',(8.54350322705385,8.25646917637536,-9.50626226660349)) ;
#108635 = CARTESIAN_POINT('Ctrl Pts',(8.49230810302881,8.3,-9.4394953499955)) ;
#108636 = CARTESIAN_POINT('Ctrl Pts',(8.52426411271138,8.3,-9.46856652463357)) ;
#108637 = CARTESIAN_POINT('Ctrl Pts',(8.54627296401924,8.268663848689,-9.48855256936155)) ;
#108638 = CARTESIAN_POINT('Ctrl Pts',(8.49410170711668,8.3,-9.437526518934)) ;
#108639 = CARTESIAN_POINT('Ctrl Pts',(8.52463604790915,8.3,-9.46240552536514)) ;
#108640 = CARTESIAN_POINT('Ctrl Pts',(8.54716490137965,8.27360757863442,-9.48079595948253)) ;
#108641 = CARTESIAN_POINT('Ctrl Pts',(8.49698869685299,8.3,-9.43307327880953)) ;
#108642 = CARTESIAN_POINT('Ctrl Pts',(8.52523118911551,8.3,-9.4465929344383)) ;
#108643 = CARTESIAN_POINT('Ctrl Pts',(8.54862931231184,8.28262305001772,-9.45784134927038)) ;
#108644 = CARTESIAN_POINT('Ctrl Pts',(8.4979868777125,8.3,-9.43051652115658)) ;
#108645 = CARTESIAN_POINT('Ctrl Pts',(8.52551930315387,8.3,-9.43690627604376)) ;
#108646 = CARTESIAN_POINT('Ctrl Pts',(8.54912969489065,8.28574379441723,-9.44238189749318)) ;
#108647 = CARTESIAN_POINT('Ctrl Pts',(8.49821791151747,8.3,-9.42257957093737)) ;
#108648 = CARTESIAN_POINT('Ctrl Pts',(8.52559423327562,8.3,-9.41218912470487)) ;
#108649 = CARTESIAN_POINT('Ctrl Pts',(8.54922875625408,8.28635135062006,-9.40323867004693)) ;
#108650 = CARTESIAN_POINT('Ctrl Pts',(8.49537847603513,8.3,-9.41764691084576)) ;
#108651 = CARTESIAN_POINT('Ctrl Pts',(8.52439331053439,8.3,-9.40147327498213)) ;
#108652 = CARTESIAN_POINT('Ctrl Pts',(8.54781890418529,8.28040548672881,-9.38847179337203)) ;
#108653 = CARTESIAN_POINT('Ctrl Pts',(8.48955273785443,8.3,-9.40891140345694)) ;
#108654 = CARTESIAN_POINT('Ctrl Pts',(8.52168703568127,8.3,-9.38405258512814)) ;
#108655 = CARTESIAN_POINT('Ctrl Pts',(8.54489815533717,8.2719421259912,-9.36616700770703)) ;
#108656 = CARTESIAN_POINT('Ctrl Pts',(8.48620077197359,8.3,-9.40482630750476)) ;
#108657 = CARTESIAN_POINT('Ctrl Pts',(8.52012703453235,8.3,-9.37710733289327)) ;
#108658 = CARTESIAN_POINT('Ctrl Pts',(8.54324008387895,8.26788967346964,-9.35831423563837)) ;
#108659 = CARTESIAN_POINT('Ctrl Pts',(8.48280151347419,8.3,-9.40079110964071)) ;
#108660 = CARTESIAN_POINT('Ctrl Pts',(8.51858761497412,8.3,-9.3706520257852)) ;
#108661 = CARTESIAN_POINT('Ctrl Pts',(8.54152015125555,8.26408224232382,-9.35133822503473)) ;
#108662 = CARTESIAN_POINT('Origin',(8.4,8.2,-9.61792711014902)) ;
#108663 = CARTESIAN_POINT('Origin',(8.4,8.2,-10.785)) ;
#108664 = CARTESIAN_POINT('Origin',(8.4,8.2,-10.702072889851)) ;
#108665 = CARTESIAN_POINT('Ctrl Pts',(8.50101530037394,8.19768718256761,-10.6872017745814)) ;
#108666 = CARTESIAN_POINT('Ctrl Pts',(8.50305639000874,8.3,-10.6872198113573)) ;
#108667 = CARTESIAN_POINT('Ctrl Pts',(8.40204633857704,8.3,-10.6738202021253)) ;
#108668 = CARTESIAN_POINT('Ctrl Pts',(8.4972546444163,8.20131038948433,-10.7148679119095)) ;
#108669 = CARTESIAN_POINT('Ctrl Pts',(8.49701391805271,8.3,-10.7145609423403)) ;
#108670 = CARTESIAN_POINT('Ctrl Pts',(8.39450526457597,8.3,-10.725363291071)) ;
#108671 = CARTESIAN_POINT('Ctrl Pts',(8.50410935041312,8.20295267265886,-10.7395792968115)) ;
#108672 = CARTESIAN_POINT('Ctrl Pts',(8.49820749521502,8.3,-10.7374643378907)) ;
#108673 = CARTESIAN_POINT('Ctrl Pts',(8.40816401923485,8.3,-10.7779187290435)) ;
#108674 = CARTESIAN_POINT('Ctrl Pts',(8.52158236570989,8.21893216789647,-10.7698300407758)) ;
#108675 = CARTESIAN_POINT('Ctrl Pts',(8.50896456566522,8.3,-10.779127678384)) ;
#108676 = CARTESIAN_POINT('Ctrl Pts',(8.4430413476632,8.3,-10.8290030669129)) ;
#108677 = CARTESIAN_POINT('Ctrl Pts',(8.5248849650705,8.222229916312,-10.7750437061782)) ;
#108678 = CARTESIAN_POINT('Ctrl Pts',(8.51098076140208,8.3,-10.7862331109763)) ;
#108679 = CARTESIAN_POINT('Ctrl Pts',(8.44963266995284,8.3,-10.8373321680218)) ;
#108680 = CARTESIAN_POINT('Ctrl Pts',(8.53194575580938,8.23126818558571,-10.7866757349666)) ;
#108681 = CARTESIAN_POINT('Ctrl Pts',(8.51549074202138,8.3,-10.8023505031351)) ;
#108682 = CARTESIAN_POINT('Ctrl Pts',(8.4637230636015,8.3,-10.8530452736801)) ;
#108683 = CARTESIAN_POINT('Ctrl Pts',(8.53573618291037,8.23674548871787,-10.7925623770273)) ;
#108684 = CARTESIAN_POINT('Ctrl Pts',(8.51797743940284,8.3,-10.8107374625586)) ;
#108685 = CARTESIAN_POINT('Ctrl Pts',(8.47128983770083,8.3,-10.8604413728536)) ;
#108686 = CARTESIAN_POINT('Ctrl Pts',(8.54154687836689,8.25075037830458,-10.8079451319455)) ;
#108687 = CARTESIAN_POINT('Ctrl Pts',(8.52169408444524,8.3,-10.8292435543493)) ;
#108688 = CARTESIAN_POINT('Ctrl Pts',(8.48287565264706,8.3,-10.8712692051668)) ;
#108689 = CARTESIAN_POINT('Ctrl Pts',(8.54351297666181,8.2564485941942,-10.8137272780162)) ;
#108690 = CARTESIAN_POINT('Ctrl Pts',(8.52288848488737,8.3,-10.8358447315488)) ;
#108691 = CARTESIAN_POINT('Ctrl Pts',(8.48680760428676,8.3,-10.874812702598)) ;
#108692 = CARTESIAN_POINT('Ctrl Pts',(8.54628376412585,8.26864846827403,-10.8314376231601)) ;
#108693 = CARTESIAN_POINT('Ctrl Pts',(8.52427341038692,8.3,-10.8514250170404)) ;
#108694 = CARTESIAN_POINT('Ctrl Pts',(8.49230810302881,8.3,-10.8805046500045)) ;
#108695 = CARTESIAN_POINT('Ctrl Pts',(8.54717611873857,8.27359443500942,-10.8391948837188)) ;
#108696 = CARTESIAN_POINT('Ctrl Pts',(8.5246448044482,8.3,-10.8575873399142)) ;
#108697 = CARTESIAN_POINT('Ctrl Pts',(8.49410170711667,8.3,-10.882473481066)) ;
#108698 = CARTESIAN_POINT('Ctrl Pts',(8.54864126180654,8.28261417405718,-10.8621529061247)) ;
#108699 = CARTESIAN_POINT('Ctrl Pts',(8.52523908688554,8.3,-10.8734032849062)) ;
#108700 = CARTESIAN_POINT('Ctrl Pts',(8.49698869685298,8.3,-10.8869267211905)) ;
#108701 = CARTESIAN_POINT('Ctrl Pts',(8.5491418548716,8.28573645090424,-10.877615282416)) ;
#108702 = CARTESIAN_POINT('Ctrl Pts',(8.52552693815803,8.3,-10.8830919520162)) ;
#108703 = CARTESIAN_POINT('Ctrl Pts',(8.4979868777125,8.3,-10.8894834788434)) ;
#108704 = CARTESIAN_POINT('Ctrl Pts',(8.54924094958848,8.28634430798886,-10.9167659475987)) ;
#108705 = CARTESIAN_POINT('Ctrl Pts',(8.52560181204939,8.3,-10.9078137517533)) ;
#108706 = CARTESIAN_POINT('Ctrl Pts',(8.49821791151748,8.3,-10.8974204290626)) ;
#108707 = CARTESIAN_POINT('Ctrl Pts',(8.54783079466743,8.28039553911294,-10.9315348059812)) ;
#108708 = CARTESIAN_POINT('Ctrl Pts',(8.52440147378976,8.3,-10.9185312754322)) ;
#108709 = CARTESIAN_POINT('Ctrl Pts',(8.49537847603513,8.3,-10.9023530891542)) ;
#108710 = CARTESIAN_POINT('Ctrl Pts',(8.54465883986931,8.27120119512637,-10.9557571947032)) ;
#108711 = CARTESIAN_POINT('Ctrl Pts',(8.52145785975947,8.3,-10.93749027833)) ;
#108712 = CARTESIAN_POINT('Ctrl Pts',(8.48905244827038,8.3,-10.9118387647145)) ;
#108713 = CARTESIAN_POINT('Ctrl Pts',(8.54267599402784,8.26648669506703,-10.9642949904304)) ;
#108714 = CARTESIAN_POINT('Ctrl Pts',(8.5195878469242,8.3,-10.9452641321446)) ;
#108715 = CARTESIAN_POINT('Ctrl Pts',(8.48503640902804,8.3,-10.9165685970659)) ;
#108716 = CARTESIAN_POINT('Ctrl Pts',(8.54064021294345,8.26212437554839,-10.9722000298238)) ;
#108717 = CARTESIAN_POINT('Ctrl Pts',(8.51779796763703,8.3,-10.9526895170151)) ;
#108718 = CARTESIAN_POINT('Ctrl Pts',(8.48104783026778,8.3,-10.9212848074951)) ;
#108719 = CARTESIAN_POINT('Origin',(8.48238054716045,8.20007132581614,-10.9068210673796)) ;
#108720 = CARTESIAN_POINT('Origin',(8.48377223398316,8.2,-12.7)) ;
#108721 = CARTESIAN_POINT('Ctrl Pts',(8.55305389383868,6.58518362856711,-14.5798163714329)) ;
#108722 = CARTESIAN_POINT('Ctrl Pts',(8.56447181517253,6.58947636230805,-14.575523637692)) ;
#108723 = CARTESIAN_POINT('Ctrl Pts',(8.57705842661295,6.59157413088145,-14.5734258691185)) ;
#108724 = CARTESIAN_POINT('Ctrl Pts',(8.553051025152,6.55898702014118,-14.5536204597775)) ;
#108725 = CARTESIAN_POINT('Ctrl Pts',(8.56446969712854,6.56479854221785,-14.5508465230912)) ;
#108726 = CARTESIAN_POINT('Ctrl Pts',(8.5770584270977,6.56766897765924,-14.5495207157348)) ;
#108727 = CARTESIAN_POINT('Ctrl Pts',(8.55608440539073,6.54967077654144,-14.5134724260347)) ;
#108728 = CARTESIAN_POINT('Ctrl Pts',(8.56803673427363,6.55578248257735,-14.5131311242349)) ;
#108729 = CARTESIAN_POINT('Ctrl Pts',(8.58110225049763,6.55837193275,-14.5132648466504)) ;
#108730 = CARTESIAN_POINT('Ctrl Pts',(8.56106007075016,6.56033186051354,-14.4769784615962)) ;
#108731 = CARTESIAN_POINT('Ctrl Pts',(8.57385418571953,6.56560017282096,-14.4782038837617)) ;
#108732 = CARTESIAN_POINT('Ctrl Pts',(8.58763814880121,6.56727264871055,-14.4785929056926)) ;
#108733 = CARTESIAN_POINT('',(8.56104219912065,6.56017369985344,-14.4776338509444)) ;
#108734 = CARTESIAN_POINT('',(8.55704445183395,6.58320973295709,-14.5748316411921)) ;
#108735 = CARTESIAN_POINT('Ctrl Pts',(8.56104219912065,6.56017369985344,-14.4776338509444)) ;
#108736 = CARTESIAN_POINT('Ctrl Pts',(8.56172006948825,6.55755272988493,-14.4905099834262)) ;
#108737 = CARTESIAN_POINT('Ctrl Pts',(8.56178854742204,6.55691761311389,-14.5040188634591)) ;
#108738 = CARTESIAN_POINT('Ctrl Pts',(8.56147572200372,6.55855061087387,-14.5170710371545)) ;
#108739 = CARTESIAN_POINT('Ctrl Pts',(8.56116227470662,6.56018685493861,-14.5301491578135)) ;
#108740 = CARTESIAN_POINT('Ctrl Pts',(8.5604843297899,6.56417103596015,-14.5431290791339)) ;
#108741 = CARTESIAN_POINT('Ctrl Pts',(8.55945615587251,6.57017322470283,-14.5548222126965)) ;
#108742 = CARTESIAN_POINT('Ctrl Pts',(8.55883284154061,6.5738119576086,-14.5619109917552)) ;
#108743 = CARTESIAN_POINT('Ctrl Pts',(8.55807185541709,6.57823677723142,-14.5686350483953)) ;
#108744 = CARTESIAN_POINT('Ctrl Pts',(8.55704487707427,6.58320791316496,-14.5748324621195)) ;
#108745 = CARTESIAN_POINT('',(8.55635403291171,6.58636921675995,-14.5786302321744)) ;
#108746 = CARTESIAN_POINT('Origin',(8.54420290656139,6.62817328946518,-14.541941136554)) ;
#108747 = CARTESIAN_POINT('',(8.57705842661295,6.59157413088145,-14.5734258691185)) ;
#108748 = CARTESIAN_POINT('Origin',(8.6,6.52274941072028,-14.6422505892797)) ;
#108749 = CARTESIAN_POINT('',(8.58355189313842,6.56397635572685,-14.502433776426)) ;
#108750 = CARTESIAN_POINT('Origin',(8.59777129281801,6.65641294722147,-14.5008822359315)) ;
#108751 = CARTESIAN_POINT('Ctrl Pts',(8.56104311409705,6.56017375480329,-14.4776348093723)) ;
#108752 = CARTESIAN_POINT('Ctrl Pts',(8.56569547918964,6.5609490208508,-14.4831223861694)) ;
#108753 = CARTESIAN_POINT('Ctrl Pts',(8.57049938306329,6.56176641478978,-14.4885092513474)) ;
#108754 = CARTESIAN_POINT('Ctrl Pts',(8.57538893105709,6.56259599225627,-14.4937862661384)) ;
#108755 = CARTESIAN_POINT('Ctrl Pts',(8.57808773793831,6.5630538810791,-14.4966989369719)) ;
#108756 = CARTESIAN_POINT('Ctrl Pts',(8.58081254036864,6.56351521010419,-14.4995793793676)) ;
#108757 = CARTESIAN_POINT('Ctrl Pts',(8.58355195315297,6.56397636517831,-14.5024336197205)) ;
#108758 = CARTESIAN_POINT('Ctrl Pts',(8.5,8.35216169217141,-14.5924060982502)) ;
#108759 = CARTESIAN_POINT('Ctrl Pts',(8.5,8.2900428850829,-14.561346694706)) ;
#108760 = CARTESIAN_POINT('Ctrl Pts',(8.56507848521152,8.26835005667906,-14.550500280504)) ;
#108761 = CARTESIAN_POINT('Ctrl Pts',(8.5,8.31945293993511,-14.6578235972685)) ;
#108762 = CARTESIAN_POINT('Ctrl Pts',(8.5,8.26922013491168,-14.6029921887963)) ;
#108763 = CARTESIAN_POINT('Ctrl Pts',(8.56507848601002,8.25199117628906,-14.5832180406186)) ;
#108764 = CARTESIAN_POINT('Ctrl Pts',(8.5,8.24922766844411,-14.6997127068514)) ;
#108765 = CARTESIAN_POINT('Ctrl Pts',(8.50000000000007,8.21777561643102,-14.6244773698228)) ;
#108766 = CARTESIAN_POINT('Ctrl Pts',(8.57228151929421,8.21451202732351,-14.6029530801176)) ;
#108767 = CARTESIAN_POINT('Ctrl Pts',(8.5,8.17221734381475,-14.6997127088383)) ;
#108768 = CARTESIAN_POINT('Ctrl Pts',(8.5,8.17221734381475,-14.615)) ;
#108769 = CARTESIAN_POINT('Ctrl Pts',(8.58356010126947,8.17221734381475,-14.6010733164551)) ;
#108770 = CARTESIAN_POINT('',(8.50000000249538,8.20000280433619,-14.6979047436384)) ;
#108771 = CARTESIAN_POINT('',(8.54742025481395,8.27608084305204,-14.5543656619559)) ;
#108772 = CARTESIAN_POINT('Ctrl Pts',(8.50000000249538,8.20000280433619,-14.6979047436384)) ;
#108773 = CARTESIAN_POINT('Ctrl Pts',(8.50000274011724,8.20154143765779,-14.6856354484511)) ;
#108774 = CARTESIAN_POINT('Ctrl Pts',(8.50225788919788,8.20358050335012,-14.6732664749796)) ;
#108775 = CARTESIAN_POINT('Ctrl Pts',(8.50614710304112,8.20657022673326,-14.6619159810139)) ;
#108776 = CARTESIAN_POINT('Ctrl Pts',(8.51002595055128,8.20955198129041,-14.6505957407205)) ;
#108777 = CARTESIAN_POINT('Ctrl Pts',(8.51564213392183,8.21362262975068,-14.6400461335207)) ;
#108778 = CARTESIAN_POINT('Ctrl Pts',(8.52129493663065,8.21921832196825,-14.630621792234)) ;
#108779 = CARTESIAN_POINT('Ctrl Pts',(8.52933132065201,8.22717351408127,-14.6172235489855)) ;
#108780 = CARTESIAN_POINT('Ctrl Pts',(8.53683691159804,8.23885362788864,-14.6056624434434)) ;
#108781 = CARTESIAN_POINT('Ctrl Pts',(8.54097226482464,8.25011947738646,-14.5928811696171)) ;
#108782 = CARTESIAN_POINT('Ctrl Pts',(8.54447125915462,8.25965170869904,-14.5820667114082)) ;
#108783 = CARTESIAN_POINT('Ctrl Pts',(8.54617119150717,8.26873789958222,-14.5699396101896)) ;
#108784 = CARTESIAN_POINT('Ctrl Pts',(8.54724932284106,8.27506683274844,-14.5565664602513)) ;
#108785 = CARTESIAN_POINT('Ctrl Pts',(8.54730817192851,8.27541229338911,-14.5558364956863)) ;
#108786 = CARTESIAN_POINT('Ctrl Pts',(8.5473651061662,8.27575037116516,-14.555102832606)) ;
#108787 = CARTESIAN_POINT('Ctrl Pts',(8.54742024083733,8.27608084608571,-14.5543656752073)) ;
#108788 = CARTESIAN_POINT('',(8.56507848521152,8.26835005667905,-14.550500280504)) ;
#108789 = CARTESIAN_POINT('Origin',(8.6,8.3521616921714,-14.5924060982502)) ;
#108790 = CARTESIAN_POINT('',(8.58356010126947,8.17221734381475,-14.6010733164551)) ;
#108791 = CARTESIAN_POINT('Origin',(8.59670327708558,8.16883734299686,-14.5070689695193)) ;
#108792 = CARTESIAN_POINT('',(8.5,8.17221734381475,-14.6997127088383)) ;
#108793 = CARTESIAN_POINT('Origin',(8.6,8.17221734381475,-14.6997127088383)) ;
#108794 = CARTESIAN_POINT('Origin',(8.5,8.1664264877529,-14.4771077523706)) ;
#108795 = CARTESIAN_POINT('Origin',(2.9,3.8,-15.24)) ;
#108796 = CARTESIAN_POINT('',(3.,2.4,-15.24)) ;
#108797 = CARTESIAN_POINT('Origin',(3.,3.8,-15.24)) ;
#108798 = CARTESIAN_POINT('',(2.9,2.3,-15.24)) ;
#108799 = CARTESIAN_POINT('Origin',(2.9,2.4,-15.24)) ;
#108800 = CARTESIAN_POINT('Origin',(2.9,3.8,-15.24)) ;
#108801 = CARTESIAN_POINT('Origin',(1.35,3.8,-15.24)) ;
#108802 = CARTESIAN_POINT('',(1.35,2.3,-15.24)) ;
#108803 = CARTESIAN_POINT('Origin',(1.35,3.8,-15.24)) ;
#108804 = CARTESIAN_POINT('',(1.25,2.2,-15.24)) ;
#108805 = CARTESIAN_POINT('Origin',(1.35,2.2,-15.24)) ;
#108806 = CARTESIAN_POINT('Origin',(1.25,3.8,-15.24)) ;
#108807 = CARTESIAN_POINT('Origin',(13.9153543900904,1.02736587339764,-14.39)) ;
#108808 = CARTESIAN_POINT('',(1.15,1.02736587339764,-14.49)) ;
#108809 = CARTESIAN_POINT('',(1.15,0.931757800066529,-14.3606896551724)) ;
#108810 = CARTESIAN_POINT('Origin',(1.15,1.02736587339764,-14.39)) ;
#108811 = CARTESIAN_POINT('',(-0.900000000000002,1.02736587339765,-14.49)) ;
#108812 = CARTESIAN_POINT('',(-1.,1.02736587339765,-14.49)) ;
#108813 = CARTESIAN_POINT('',(-0.900000000000002,0.982644513847654,-14.4794427191)) ;
#108814 = CARTESIAN_POINT('Origin',(-0.900000000000002,1.02736587339765,-14.39)) ;
#108815 = CARTESIAN_POINT('',(-0.900000000000002,0.93175780006653,-14.3606896551724)) ;
#108816 = CARTESIAN_POINT('Origin',(-0.900000000000002,1.02736587339765,-14.39)) ;
#108817 = CARTESIAN_POINT('',(13.9153543900904,0.931757800066525,-14.3606896551724)) ;
#108818 = CARTESIAN_POINT('Origin',(13.9153543900904,1.02736587339764,-16.09)) ;
#108819 = CARTESIAN_POINT('',(1.15,0.93175780006653,-16.1193103448276)) ;
#108820 = CARTESIAN_POINT('',(1.15,1.02736587339765,-15.99)) ;
#108821 = CARTESIAN_POINT('Origin',(1.15,1.02736587339765,-16.09)) ;
#108822 = CARTESIAN_POINT('',(-0.900000000000002,0.931757800066531,-16.1193103448276)) ;
#108823 = CARTESIAN_POINT('',(13.9153543900904,0.931757800066525,-16.1193103448276)) ;
#108824 = CARTESIAN_POINT('',(-0.900000000000002,1.02736587339765,-15.99)) ;
#108825 = CARTESIAN_POINT('Origin',(-0.900000000000002,1.02736587339765,-16.09)) ;
#108826 = CARTESIAN_POINT('',(-1.,1.02736587339765,-15.99)) ;
#108827 = CARTESIAN_POINT('Origin',(8.49172374697003,3.8,-15.24)) ;
#108828 = CARTESIAN_POINT('',(8.49172374697003,1.47741935483871,-13.3411532060953)) ;
#108829 = CARTESIAN_POINT('',(8.49172374697003,1.47741935483871,-17.1388467939047)) ;
#108830 = CARTESIAN_POINT('Origin',(8.49172374697003,3.8,-15.24)) ;
#108831 = CARTESIAN_POINT('',(8.50816364570057,1.47636598119991,-13.3402920109583)) ;
#108832 = CARTESIAN_POINT('Origin',(8.49172374697003,1.4,-13.2778583129651)) ;
#108833 = CARTESIAN_POINT('',(8.50816364570057,1.47636598119991,-17.1397079890417)) ;
#108834 = CARTESIAN_POINT('Origin',(8.50816364570057,3.8,-15.24)) ;
#108835 = CARTESIAN_POINT('Origin',(8.49172374697003,1.4,-17.2021416870349)) ;
#108836 = CARTESIAN_POINT('Origin',(1.25,3.8,-15.24)) ;
#108837 = CARTESIAN_POINT('',(1.25,2.3,-15.24)) ;
#108838 = CARTESIAN_POINT('Origin',(13.9153543900904,3.8,-15.24)) ;
#108839 = CARTESIAN_POINT('',(-0.900000000000002,1.47741935483872,-17.1388467939047)) ;
#108840 = CARTESIAN_POINT('',(13.9153543900904,1.47741935483871,-17.1388467939047)) ;
#108841 = CARTESIAN_POINT('Origin',(-0.900000000000001,3.8,-15.24)) ;
#108842 = CARTESIAN_POINT('',(1.35,0.876327704607742,-15.9124137931035)) ;
#108843 = CARTESIAN_POINT('Ctrl Pts',(1.35,0.876327704607742,-15.9124137931035)) ;
#108844 = CARTESIAN_POINT('Ctrl Pts',(1.35,0.888571289407569,-15.9656492115953)) ;
#108845 = CARTESIAN_POINT('Ctrl Pts',(1.32969623836296,0.902340613578954,
-16.0179295970213)) ;
#108846 = CARTESIAN_POINT('Ctrl Pts',(1.25741074236298,0.924142973728496,
-16.0950150537158)) ;
#108847 = CARTESIAN_POINT('Ctrl Pts',(1.20472523187106,0.93175780006653,-16.1193103448276)) ;
#108848 = CARTESIAN_POINT('Ctrl Pts',(1.15,0.93175780006653,-16.1193103448276)) ;
#108849 = CARTESIAN_POINT('',(1.35,0.876327704607742,-14.5675862068966)) ;
#108850 = CARTESIAN_POINT('Origin',(1.35,3.8,-15.24)) ;
#108851 = CARTESIAN_POINT('Ctrl Pts',(1.15,0.931757800066529,-14.3606896551724)) ;
#108852 = CARTESIAN_POINT('Ctrl Pts',(1.20475877631964,0.931757800066529,
-14.3606896551724)) ;
#108853 = CARTESIAN_POINT('Ctrl Pts',(1.2574100247738,0.924155896380522,-14.3849343608884)) ;
#108854 = CARTESIAN_POINT('Ctrl Pts',(1.32987646938161,0.9022735155524,-14.4623125455279)) ;
#108855 = CARTESIAN_POINT('Ctrl Pts',(1.35,0.888577265820266,-14.5143248028101)) ;
#108856 = CARTESIAN_POINT('Ctrl Pts',(1.35,0.876327704607742,-14.5675862068966)) ;
#108857 = CARTESIAN_POINT('',(-0.900000000000002,1.47741935483872,-13.3411532060953)) ;
#108858 = CARTESIAN_POINT('Origin',(-0.900000000000001,3.8,-15.24)) ;
#108859 = CARTESIAN_POINT('',(13.9153543900904,1.47741935483871,-13.3411532060953)) ;
#108860 = CARTESIAN_POINT('Origin',(0.55,3.09772049281573E-17,-15.24)) ;
#108861 = CARTESIAN_POINT('',(0.549999999999999,4.4,-14.79)) ;
#108862 = CARTESIAN_POINT('',(0.549999999999999,4.4,-15.69)) ;
#108863 = CARTESIAN_POINT('',(0.549999999999999,4.4,-15.24)) ;
#108864 = CARTESIAN_POINT('',(0.55,4.04473197180486,-15.69)) ;
#108865 = CARTESIAN_POINT('',(0.55,1.39397422176708E-16,-15.69)) ;
#108866 = CARTESIAN_POINT('',(0.55,4.05997159067981,-15.64)) ;
#108867 = CARTESIAN_POINT('Ctrl Pts',(0.549999999999999,4.04473197180486,
-15.69)) ;
#108868 = CARTESIAN_POINT('Ctrl Pts',(0.549999999999999,4.04764757798806,
-15.6855648611277)) ;
#108869 = CARTESIAN_POINT('Ctrl Pts',(0.549999999999999,4.05014503921306,
-15.6809481448659)) ;
#108870 = CARTESIAN_POINT('Ctrl Pts',(0.549999999999999,4.0569489863933,-15.6656814456903)) ;
#108871 = CARTESIAN_POINT('Ctrl Pts',(0.549999999999999,4.0599715906798,-15.6518214564414)) ;
#108872 = CARTESIAN_POINT('Ctrl Pts',(0.549999999999999,4.0599715906798,-15.64)) ;
#108873 = CARTESIAN_POINT('',(0.55,4.05997159067981,-14.84)) ;
#108874 = CARTESIAN_POINT('',(0.55,4.05997159067981,-14.74)) ;
#108875 = CARTESIAN_POINT('',(0.55,4.04473197181449,-14.7900000000146)) ;
#108876 = CARTESIAN_POINT('Origin',(0.55003450380264,3.938694577917,-14.8424160296945)) ;
#108877 = CARTESIAN_POINT('',(0.55,6.35032701027224E-17,-14.79)) ;
#108878 = CARTESIAN_POINT('Origin',(10.,7.8,-17.78)) ;
#108879 = CARTESIAN_POINT('',(9.93162277660169,7.82279240779944,-17.78)) ;
#108880 = CARTESIAN_POINT('',(8.51539501058484,8.29486832980505,-17.78)) ;
#108881 = CARTESIAN_POINT('',(10.,7.8,-17.78)) ;
#108882 = CARTESIAN_POINT('',(8.51540095511711,8.29487265903615,-16.0090607599342)) ;
#108883 = CARTESIAN_POINT('',(8.51539501058484,8.29486832980505,-17.78)) ;
#108884 = CARTESIAN_POINT('',(8.54856023413467,8.2839858620311,-15.9960080665656)) ;
#108885 = CARTESIAN_POINT('Ctrl Pts',(8.51540095511711,8.29487265903615,-16.0090607599342)) ;
#108886 = CARTESIAN_POINT('Ctrl Pts',(8.51716444659958,8.29428466923189,-16.0096424828188)) ;
#108887 = CARTESIAN_POINT('Ctrl Pts',(8.51901954868166,8.29366521079575,-16.0099704508582)) ;
#108888 = CARTESIAN_POINT('Ctrl Pts',(8.52087614409667,8.2930450194617,-16.0100725025784)) ;
#108889 = CARTESIAN_POINT('Ctrl Pts',(8.52171779595218,8.29276386763785,-16.0101187657647)) ;
#108890 = CARTESIAN_POINT('Ctrl Pts',(8.52256005861364,8.29248252453828,-16.010119087778)) ;
#108891 = CARTESIAN_POINT('Ctrl Pts',(8.52339613191994,8.29220315552769,-16.0100794460141)) ;
#108892 = CARTESIAN_POINT('Ctrl Pts',(8.52456316579569,8.29181319797645,-16.0100241120128)) ;
#108893 = CARTESIAN_POINT('Ctrl Pts',(8.52573147766846,8.29142195356397,-16.0098930049957)) ;
#108894 = CARTESIAN_POINT('Ctrl Pts',(8.52689074379087,8.29103442649366,-16.009691327086)) ;
#108895 = CARTESIAN_POINT('Ctrl Pts',(8.52858695132689,8.2904674071317,-16.0093962373015)) ;
#108896 = CARTESIAN_POINT('Ctrl Pts',(8.53026630212624,8.2899212363328,-16.0089439218143)) ;
#108897 = CARTESIAN_POINT('Ctrl Pts',(8.53190117913116,8.28939883282069,-16.0083683729162)) ;
#108898 = CARTESIAN_POINT('Ctrl Pts',(8.53241671440274,8.28923410028383,-16.0081868817357)) ;
#108899 = CARTESIAN_POINT('Ctrl Pts',(8.53292790037786,8.28907155799428,-16.0079933975174)) ;
#108900 = CARTESIAN_POINT('Ctrl Pts',(8.53343404910735,8.28891083250768,-16.0077898379553)) ;
#108901 = CARTESIAN_POINT('Ctrl Pts',(8.53529681408172,8.28831931900685,-16.0070406834076)) ;
#108902 = CARTESIAN_POINT('Ctrl Pts',(8.53711612169876,8.28774836357888,-16.0061310088335)) ;
#108903 = CARTESIAN_POINT('Ctrl Pts',(8.53885192161986,8.28720494689874,-16.005061264748)) ;
#108904 = CARTESIAN_POINT('Ctrl Pts',(8.54015925159111,8.28679566878771,-16.0042555794339)) ;
#108905 = CARTESIAN_POINT('Ctrl Pts',(8.54141951580282,8.28640152775899,-16.0033597461918)) ;
#108906 = CARTESIAN_POINT('Ctrl Pts',(8.54261761299016,8.2860217121528,-16.0023927107854)) ;
#108907 = CARTESIAN_POINT('Ctrl Pts',(8.54427390694792,8.28549664098141,-16.0010558451977)) ;
#108908 = CARTESIAN_POINT('Ctrl Pts',(8.54582756795265,8.2849959222079,-15.9995574336961)) ;
#108909 = CARTESIAN_POINT('Ctrl Pts',(8.54719190273363,8.28456181678108,-15.9979139760521)) ;
#108910 = CARTESIAN_POINT('Ctrl Pts',(8.547685057547,8.2844049042815,-15.9973199290052)) ;
#108911 = CARTESIAN_POINT('Ctrl Pts',(8.54815358395157,8.28425671205375,-15.9967074323075)) ;
#108912 = CARTESIAN_POINT('Ctrl Pts',(8.54859369700691,8.28411936587097,-15.9960788545618)) ;
#108913 = CARTESIAN_POINT('',(8.56837597005345,8.27720399148459,-15.9725054212675)) ;
#108914 = CARTESIAN_POINT('Ctrl Pts',(8.5485198670553,8.28382649282421,-15.9960140527758)) ;
#108915 = CARTESIAN_POINT('Ctrl Pts',(8.55267891820632,8.28243778061538,-15.9905631273053)) ;
#108916 = CARTESIAN_POINT('Ctrl Pts',(8.55701747195682,8.28096933708255,-15.9852590577816)) ;
#108917 = CARTESIAN_POINT('Ctrl Pts',(8.56150853123443,8.27945301063656,-15.9801132102135)) ;
#108918 = CARTESIAN_POINT('Ctrl Pts',(8.56331520072586,8.27884302075229,-15.9780431315898)) ;
#108919 = CARTESIAN_POINT('Ctrl Pts',(8.5651466343553,8.27822544298233,-15.9759980022295)) ;
#108920 = CARTESIAN_POINT('Ctrl Pts',(8.56700126712394,8.27760232477898,-15.9739757856585)) ;
#108921 = CARTESIAN_POINT('Ctrl Pts',(8.56745273479656,8.27745064099026,-15.9734835235653)) ;
#108922 = CARTESIAN_POINT('Ctrl Pts',(8.56790562999349,8.27729861980367,-15.9729951953627)) ;
#108923 = CARTESIAN_POINT('Ctrl Pts',(8.56835731300612,8.27714712982918,-15.9725055965825)) ;
#108924 = CARTESIAN_POINT('',(9.93162277660169,7.82279240779944,-16.1997127088383)) ;
#108925 = CARTESIAN_POINT('',(9.98593528106273,7.80468823964576,-16.2087647929151)) ;
#108926 = CARTESIAN_POINT('',(9.93162277660169,7.82279240779944,-17.78)) ;
#108927 = CARTESIAN_POINT('Origin',(10.,6.8,-17.78)) ;
#108928 = CARTESIAN_POINT('',(10.,6.8847127088383,-17.78)) ;
#108929 = CARTESIAN_POINT('',(10.,7.72792407799439,-17.78)) ;
#108930 = CARTESIAN_POINT('',(10.,6.8,-17.78)) ;
#108931 = CARTESIAN_POINT('',(10.,7.72792407799439,-16.1997127088383)) ;
#108932 = CARTESIAN_POINT('',(10.,7.72792407799439,-17.78)) ;
#108933 = CARTESIAN_POINT('',(10.,6.8847127088383,-16.1997127088383)) ;
#108934 = CARTESIAN_POINT('',(10.,6.8,-16.1997127088383)) ;
#108935 = CARTESIAN_POINT('',(10.,6.8847127088383,-17.78)) ;
#108936 = CARTESIAN_POINT('Origin',(8.5,6.55,-17.78)) ;
#108937 = CARTESIAN_POINT('',(9.91643989873054,6.78607331645509,-16.1997127088383)) ;
#108938 = CARTESIAN_POINT('',(8.58355805979355,6.56393854759965,-15.9775665415707)) ;
#108939 = CARTESIAN_POINT('',(8.48442535909739,6.54740422651623,-15.9610436188994)) ;
#108940 = CARTESIAN_POINT('',(8.56107669735261,6.5600938800009,-16.0023838472224)) ;
#108941 = CARTESIAN_POINT('Ctrl Pts',(8.58354728038624,6.56400494118525,-15.9775667486351)) ;
#108942 = CARTESIAN_POINT('Ctrl Pts',(8.57838853885689,6.56313097816976,-15.9829365696478)) ;
#108943 = CARTESIAN_POINT('Ctrl Pts',(8.5733012794654,6.56225500583436,-15.9883881686568)) ;
#108944 = CARTESIAN_POINT('Ctrl Pts',(8.56834297134786,6.5614089984296,-15.9939607837898)) ;
#108945 = CARTESIAN_POINT('Ctrl Pts',(8.56587587079858,6.56098805134775,-15.9967335444835)) ;
#108946 = CARTESIAN_POINT('Ctrl Pts',(8.56344049907307,6.56057499921402,-15.9995353033204)) ;
#108947 = CARTESIAN_POINT('Ctrl Pts',(8.56104288133097,6.56017406260212,-16.0023650362459)) ;
#108948 = CARTESIAN_POINT('',(8.50816305748499,6.55136011924236,-16.0173726221053)) ;
#108949 = CARTESIAN_POINT('Ctrl Pts',(8.56125813732196,6.56020968955366,-16.0025506353537)) ;
#108950 = CARTESIAN_POINT('Ctrl Pts',(8.55737139916531,6.55956189986088,-16.007208599473)) ;
#108951 = CARTESIAN_POINT('Ctrl Pts',(8.5530633519033,6.55884389198388,-16.0099674660867)) ;
#108952 = CARTESIAN_POINT('Ctrl Pts',(8.54121332232538,6.55686888705423,-16.0165237407849)) ;
#108953 = CARTESIAN_POINT('Ctrl Pts',(8.53496267038054,6.55582711173009,-16.0179613606699)) ;
#108954 = CARTESIAN_POINT('Ctrl Pts',(8.52888665185221,6.55481444197537,-16.0192795539313)) ;
#108955 = CARTESIAN_POINT('Ctrl Pts',(8.52471102104758,6.55411850350793,-16.0195977494013)) ;
#108956 = CARTESIAN_POINT('Ctrl Pts',(8.52011475164549,6.55335245860758,-16.0197029599352)) ;
#108957 = CARTESIAN_POINT('Ctrl Pts',(8.51754797133905,6.55292466188984,-16.019718645943)) ;
#108958 = CARTESIAN_POINT('Ctrl Pts',(8.51248317870103,6.55208052978351,-16.0189638228623)) ;
#108959 = CARTESIAN_POINT('Ctrl Pts',(8.51021540604925,6.55170256767487,-16.0183708961116)) ;
#108960 = CARTESIAN_POINT('Ctrl Pts',(8.50816120922221,6.55136020153704,-16.0173764115261)) ;
#108961 = CARTESIAN_POINT('',(8.50816364570071,6.55136060761679,-17.78)) ;
#108962 = CARTESIAN_POINT('',(8.50816364570071,6.55136060761679,-17.78)) ;
#108963 = CARTESIAN_POINT('',(9.91643989873054,6.78607331645509,-17.78)) ;
#108964 = CARTESIAN_POINT('',(8.5,6.55,-17.78)) ;
#108965 = CARTESIAN_POINT('',(9.91643989873054,6.78607331645509,-17.78)) ;
#108966 = CARTESIAN_POINT('Origin',(10.,1.5,-17.78)) ;
#108967 = CARTESIAN_POINT('',(-0.900000000000002,1.5,-17.2021416870349)) ;
#108968 = CARTESIAN_POINT('',(8.49172374697003,1.5,-17.2021416870349)) ;
#108969 = CARTESIAN_POINT('',(10.,1.5,-17.2021416870349)) ;
#108970 = CARTESIAN_POINT('',(8.49172374697003,1.5,-17.78)) ;
#108971 = CARTESIAN_POINT('',(8.49172374697003,1.5,-17.78)) ;
#108972 = CARTESIAN_POINT('',(-0.900000000000001,1.5,-17.78)) ;
#108973 = CARTESIAN_POINT('',(10.,1.5,-17.78)) ;
#108974 = CARTESIAN_POINT('',(-0.900000000000002,1.5,-17.1661360284258)) ;
#108975 = CARTESIAN_POINT('Origin',(10.,1.5,-17.78)) ;
#108976 = CARTESIAN_POINT('',(8.49172374697003,1.5,-12.7)) ;
#108977 = CARTESIAN_POINT('',(-0.900000000000001,1.5,-12.7)) ;
#108978 = CARTESIAN_POINT('',(10.,1.5,-12.7)) ;
#108979 = CARTESIAN_POINT('',(8.49172374697003,1.5,-13.2778583129651)) ;
#108980 = CARTESIAN_POINT('',(8.49172374697003,1.5,-17.78)) ;
#108981 = CARTESIAN_POINT('',(-0.900000000000002,1.5,-13.2778583129651)) ;
#108982 = CARTESIAN_POINT('',(10.,1.5,-13.2778583129651)) ;
#108983 = CARTESIAN_POINT('',(-0.900000000000001,1.5,-17.78)) ;
#108984 = CARTESIAN_POINT('Origin',(10.,0.,-17.78)) ;
#108985 = CARTESIAN_POINT('',(10.,0.1,-12.7)) ;
#108986 = CARTESIAN_POINT('',(10.,1.16528729116168,-12.7)) ;
#108987 = CARTESIAN_POINT('',(10.,0.,-12.7)) ;
#108988 = CARTESIAN_POINT('',(10.,0.1,-17.78)) ;
#108989 = CARTESIAN_POINT('',(10.,0.1,-17.78)) ;
#108990 = CARTESIAN_POINT('',(10.,1.16528729116168,-17.78)) ;
#108991 = CARTESIAN_POINT('',(10.,0.,-17.78)) ;
#108992 = CARTESIAN_POINT('',(10.,1.16528729116168,-17.2841618801782)) ;
#108993 = CARTESIAN_POINT('',(10.,1.16528729116168,-17.78)) ;
#108994 = CARTESIAN_POINT('',(10.,1.16528729116168,-13.1958381198218)) ;
#108995 = CARTESIAN_POINT('Origin',(10.,3.8,-15.24)) ;
#108996 = CARTESIAN_POINT('',(10.,1.16528729116168,-17.78)) ;
#108997 = CARTESIAN_POINT('Origin',(0.,0.,-17.78)) ;
#108998 = CARTESIAN_POINT('',(8.48377223398316,8.3,-17.78)) ;
#108999 = CARTESIAN_POINT('',(7.1,8.3,-17.78)) ;
#109000 = CARTESIAN_POINT('',(8.5,8.3,-17.78)) ;
#109001 = CARTESIAN_POINT('Origin',(8.48377223398316,8.2,-17.78)) ;
#109002 = CARTESIAN_POINT('Origin',(9.9,7.72792407799439,-17.78)) ;
#109003 = CARTESIAN_POINT('Origin',(9.9,6.8847127088383,-17.78)) ;
#109004 = CARTESIAN_POINT('',(8.49172374697018,6.55,-17.78)) ;
#109005 = CARTESIAN_POINT('Origin',(8.49172374697018,6.65,-17.78)) ;
#109006 = CARTESIAN_POINT('',(-0.900000000000001,6.55,-17.78)) ;
#109007 = CARTESIAN_POINT('',(1.25,6.55,-17.78)) ;
#109008 = CARTESIAN_POINT('',(-1.,6.45,-17.78)) ;
#109009 = CARTESIAN_POINT('Origin',(-0.9,6.45,-17.78)) ;
#109010 = CARTESIAN_POINT('',(-1.,4.65,-17.78)) ;
#109011 = CARTESIAN_POINT('',(-1.,3.46944695195362E-16,-17.78)) ;
#109012 = CARTESIAN_POINT('',(-0.900000000000001,4.55,-17.78)) ;
#109013 = CARTESIAN_POINT('Origin',(-0.900000000000001,4.65,-17.78)) ;
#109014 = CARTESIAN_POINT('',(1.15,4.55,-17.78)) ;
#109015 = CARTESIAN_POINT('',(1.57859836313889E-15,4.55,-17.78)) ;
#109016 = CARTESIAN_POINT('',(1.25,4.45,-17.78)) ;
#109017 = CARTESIAN_POINT('Origin',(1.15,4.45,-17.78)) ;
#109018 = CARTESIAN_POINT('',(1.25,3.15,-17.78)) ;
#109019 = CARTESIAN_POINT('',(1.25,1.5,-17.78)) ;
#109020 = CARTESIAN_POINT('',(1.15,3.05,-17.78)) ;
#109021 = CARTESIAN_POINT('Origin',(1.15,3.15,-17.78)) ;
#109022 = CARTESIAN_POINT('',(-0.900000000000002,3.05,-17.78)) ;
#109023 = CARTESIAN_POINT('',(1.05818132034585E-15,3.05,-17.78)) ;
#109024 = CARTESIAN_POINT('',(-1.,2.95,-17.78)) ;
#109025 = CARTESIAN_POINT('Origin',(-0.900000000000002,2.95,-17.78)) ;
#109026 = CARTESIAN_POINT('',(-1.,1.6,-17.78)) ;
#109027 = CARTESIAN_POINT('',(-1.,3.46944695195362E-16,-17.78)) ;
#109028 = CARTESIAN_POINT('Origin',(-0.900000000000002,1.6,-17.78)) ;
#109029 = CARTESIAN_POINT('',(8.50816364570057,1.49863939238321,-17.78)) ;
#109030 = CARTESIAN_POINT('Origin',(8.49172374697003,1.4,-17.78)) ;
#109031 = CARTESIAN_POINT('',(9.91643989873054,1.26392668354489,-17.78)) ;
#109032 = CARTESIAN_POINT('',(10.,1.24999999999998,-17.78)) ;
#109033 = CARTESIAN_POINT('Origin',(9.9,1.16528729116168,-17.78)) ;
#109034 = CARTESIAN_POINT('',(9.9,0.,-17.78)) ;
#109035 = CARTESIAN_POINT('Origin',(9.9,0.1,-17.78)) ;
#109036 = CARTESIAN_POINT('',(-2.,0.,-17.78)) ;
#109037 = CARTESIAN_POINT('',(-2.,0.,-17.78)) ;
#109038 = CARTESIAN_POINT('',(-2.,7.55,-17.78)) ;
#109039 = CARTESIAN_POINT('',(-2.,7.65,-17.78)) ;
#109040 = CARTESIAN_POINT('',(-1.9,7.65,-17.78)) ;
#109041 = CARTESIAN_POINT('Origin',(-1.9,7.55,-17.78)) ;
#109042 = CARTESIAN_POINT('',(6.9,7.65,-17.78)) ;
#109043 = CARTESIAN_POINT('',(7.,7.65,-17.78)) ;
#109044 = CARTESIAN_POINT('',(7.,7.75,-17.78)) ;
#109045 = CARTESIAN_POINT('Origin',(6.9,7.75,-17.78)) ;
#109046 = CARTESIAN_POINT('',(7.,8.2,-17.78)) ;
#109047 = CARTESIAN_POINT('',(7.,8.3,-17.78)) ;
#109048 = CARTESIAN_POINT('Origin',(7.1,8.2,-17.78)) ;
#109049 = CARTESIAN_POINT('Origin',(0.,0.,-12.7)) ;
#109050 = CARTESIAN_POINT('',(9.93162277660169,7.82279240779944,-12.7)) ;
#109051 = CARTESIAN_POINT('',(8.51539501058484,8.29486832980505,-12.7)) ;
#109052 = CARTESIAN_POINT('',(10.,7.8,-12.7)) ;
#109053 = CARTESIAN_POINT('',(8.48377223398316,8.3,-12.7)) ;
#109054 = CARTESIAN_POINT('Origin',(8.48377223398316,8.2,-12.7)) ;
#109055 = CARTESIAN_POINT('',(7.1,8.3,-12.7)) ;
#109056 = CARTESIAN_POINT('',(8.5,8.3,-12.7)) ;
#109057 = CARTESIAN_POINT('',(7.,8.2,-12.7)) ;
#109058 = CARTESIAN_POINT('Origin',(7.1,8.2,-12.7)) ;
#109059 = CARTESIAN_POINT('',(7.,7.75,-12.7)) ;
#109060 = CARTESIAN_POINT('',(7.,8.3,-12.7)) ;
#109061 = CARTESIAN_POINT('',(6.9,7.65,-12.7)) ;
#109062 = CARTESIAN_POINT('Origin',(6.9,7.75,-12.7)) ;
#109063 = CARTESIAN_POINT('',(-1.9,7.65,-12.7)) ;
#109064 = CARTESIAN_POINT('',(7.,7.65,-12.7)) ;
#109065 = CARTESIAN_POINT('',(-2.,7.55,-12.7)) ;
#109066 = CARTESIAN_POINT('Origin',(-1.9,7.55,-12.7)) ;
#109067 = CARTESIAN_POINT('',(-2.,0.,-12.7)) ;
#109068 = CARTESIAN_POINT('',(-2.,7.65,-12.7)) ;
#109069 = CARTESIAN_POINT('',(9.9,0.,-12.7)) ;
#109070 = CARTESIAN_POINT('',(-2.,0.,-12.7)) ;
#109071 = CARTESIAN_POINT('Origin',(9.9,0.1,-12.7)) ;
#109072 = CARTESIAN_POINT('',(9.91643989873054,1.26392668354489,-12.7)) ;
#109073 = CARTESIAN_POINT('Origin',(9.9,1.16528729116168,-12.7)) ;
#109074 = CARTESIAN_POINT('',(8.50816364570057,1.49863939238321,-12.7)) ;
#109075 = CARTESIAN_POINT('',(0.472972972972955,2.83783783783779,-12.7)) ;
#109076 = CARTESIAN_POINT('Origin',(8.49172374697003,1.4,-12.7)) ;
#109077 = CARTESIAN_POINT('',(-1.,1.6,-12.7)) ;
#109078 = CARTESIAN_POINT('Origin',(-0.900000000000002,1.6,-12.7)) ;
#109079 = CARTESIAN_POINT('',(-1.,2.95,-12.7)) ;
#109080 = CARTESIAN_POINT('',(-1.,3.46944695195362E-16,-12.7)) ;
#109081 = CARTESIAN_POINT('',(-0.900000000000002,3.05,-12.7)) ;
#109082 = CARTESIAN_POINT('Origin',(-0.900000000000002,2.95,-12.7)) ;
#109083 = CARTESIAN_POINT('',(1.15,3.05,-12.7)) ;
#109084 = CARTESIAN_POINT('',(1.05818132034585E-15,3.05,-12.7)) ;
#109085 = CARTESIAN_POINT('',(1.25,3.15,-12.7)) ;
#109086 = CARTESIAN_POINT('Origin',(1.15,3.15,-12.7)) ;
#109087 = CARTESIAN_POINT('',(1.25,4.45,-12.7)) ;
#109088 = CARTESIAN_POINT('',(1.25,5.3,-12.7)) ;
#109089 = CARTESIAN_POINT('',(1.15,4.55,-12.7)) ;
#109090 = CARTESIAN_POINT('Origin',(1.15,4.45,-12.7)) ;
#109091 = CARTESIAN_POINT('',(-0.900000000000001,4.55,-12.7)) ;
#109092 = CARTESIAN_POINT('',(1.57859836313889E-15,4.55,-12.7)) ;
#109093 = CARTESIAN_POINT('',(-1.,4.65,-12.7)) ;
#109094 = CARTESIAN_POINT('Origin',(-0.900000000000001,4.65,-12.7)) ;
#109095 = CARTESIAN_POINT('',(-1.,6.45,-12.7)) ;
#109096 = CARTESIAN_POINT('',(-1.,3.46944695195362E-16,-12.7)) ;
#109097 = CARTESIAN_POINT('',(-0.900000000000001,6.55,-12.7)) ;
#109098 = CARTESIAN_POINT('Origin',(-0.9,6.45,-12.7)) ;
#109099 = CARTESIAN_POINT('',(8.49172374697018,6.55,-12.7)) ;
#109100 = CARTESIAN_POINT('',(1.25,6.55,-12.7)) ;
#109101 = CARTESIAN_POINT('',(8.50816364570071,6.55136060761679,-12.7)) ;
#109102 = CARTESIAN_POINT('Origin',(8.49172374697018,6.65,-12.7)) ;
#109103 = CARTESIAN_POINT('',(9.91643989873054,6.78607331645509,-12.7)) ;
#109104 = CARTESIAN_POINT('',(8.5,6.55,-12.7)) ;
#109105 = CARTESIAN_POINT('',(10.,6.8847127088383,-12.7)) ;
#109106 = CARTESIAN_POINT('Origin',(9.9,6.8847127088383,-12.7)) ;
#109107 = CARTESIAN_POINT('',(10.,7.72792407799439,-12.7)) ;
#109108 = CARTESIAN_POINT('',(10.,6.8,-12.7)) ;
#109109 = CARTESIAN_POINT('Origin',(9.9,7.72792407799439,-12.7)) ;
#109110 = CARTESIAN_POINT('Origin',(7.,7.65,-17.78)) ;
#109111 = CARTESIAN_POINT('',(-1.9,7.65,-17.78)) ;
#109112 = CARTESIAN_POINT('',(6.9,7.65,-17.78)) ;
#109113 = CARTESIAN_POINT('Origin',(7.,8.3,-17.78)) ;
#109114 = CARTESIAN_POINT('',(7.,7.75,-12.7)) ;
#109115 = CARTESIAN_POINT('',(7.,8.2,-17.78)) ;
#109116 = CARTESIAN_POINT('Origin',(8.5,8.3,-17.78)) ;
#109117 = CARTESIAN_POINT('',(8.4,8.3,-15.782072889851)) ;
#109118 = CARTESIAN_POINT('',(8.48377267093845,8.29999999999968,-15.9980525450042)) ;
#109119 = CARTESIAN_POINT('Ctrl Pts',(8.4,8.3,-15.782072889851)) ;
#109120 = CARTESIAN_POINT('Ctrl Pts',(8.40000007660113,8.3,-15.7992296501961)) ;
#109121 = CARTESIAN_POINT('Ctrl Pts',(8.40222537906653,8.3,-15.8161962391188)) ;
#109122 = CARTESIAN_POINT('Ctrl Pts',(8.40642689896248,8.3,-15.8326162565066)) ;
#109123 = CARTESIAN_POINT('Ctrl Pts',(8.41084238024591,8.3,-15.84987245932)) ;
#109124 = CARTESIAN_POINT('Ctrl Pts',(8.41744096861416,8.3,-15.866526744374)) ;
#109125 = CARTESIAN_POINT('Ctrl Pts',(8.42598957610855,8.3,-15.8821622007355)) ;
#109126 = CARTESIAN_POINT('Ctrl Pts',(8.42927578126156,8.3,-15.8881726904321)) ;
#109127 = CARTESIAN_POINT('Ctrl Pts',(8.43285067318742,8.3,-15.8940324469635)) ;
#109128 = CARTESIAN_POINT('Ctrl Pts',(8.43670279785319,8.3,-15.8997167867855)) ;
#109129 = CARTESIAN_POINT('Ctrl Pts',(8.43684245837179,8.3,-15.8999228750916)) ;
#109130 = CARTESIAN_POINT('Ctrl Pts',(8.43698247939112,8.3,-15.9001287268225)) ;
#109131 = CARTESIAN_POINT('Ctrl Pts',(8.43712286024714,8.3,-15.9003343406941)) ;
#109132 = CARTESIAN_POINT('Ctrl Pts',(8.44304092798571,8.3,-15.9090024515356)) ;
#109133 = CARTESIAN_POINT('Ctrl Pts',(8.44963232699549,8.300000000002,-15.9173317313645)) ;
#109134 = CARTESIAN_POINT('Ctrl Pts',(8.45667836512367,8.29999999999776,-15.9251882739642)) ;
#109135 = CARTESIAN_POINT('Ctrl Pts',(8.46347186896914,8.29999999999367,-15.9327632333091)) ;
#109136 = CARTESIAN_POINT('Ctrl Pts',(8.47075094334181,8.29999999998296,-15.9399098655154)) ;
#109137 = CARTESIAN_POINT('Ctrl Pts',(8.47818849074308,8.29999999991001,-15.9468816128285)) ;
#109138 = CARTESIAN_POINT('Ctrl Pts',(8.47846436286148,8.2999999999073,-15.9471402075771)) ;
#109139 = CARTESIAN_POINT('Ctrl Pts',(8.47874045306876,8.29999999990447,-15.9473985605991)) ;
#109140 = CARTESIAN_POINT('Ctrl Pts',(8.47901674447045,8.29999999990152,-15.9476566852)) ;
#109141 = CARTESIAN_POINT('Ctrl Pts',(8.48287938578322,8.29999999986032,-15.9512653488833)) ;
#109142 = CARTESIAN_POINT('Ctrl Pts',(8.48681205529409,8.29999999978803,-15.9548079367278)) ;
#109143 = CARTESIAN_POINT('Ctrl Pts',(8.49047938959116,8.29999999977836,-15.9586027060218)) ;
#109144 = CARTESIAN_POINT('Ctrl Pts',(8.49231307405274,8.29999999977353,-15.9605001085834)) ;
#109145 = CARTESIAN_POINT('Ctrl Pts',(8.49410676862313,8.29999999978935,-15.962469327125)) ;
#109146 = CARTESIAN_POINT('Ctrl Pts',(8.49555027122445,8.29999999981726,-15.9646968070099)) ;
#109147 = CARTESIAN_POINT('Ctrl Pts',(8.49675259850851,8.2999999998405,-15.9665521274215)) ;
#109148 = CARTESIAN_POINT('Ctrl Pts',(8.49764594203227,8.29999999986456,-15.9686368157432)) ;
#109149 = CARTESIAN_POINT('Ctrl Pts',(8.49795530287013,8.29999999987615,-15.9708110374494)) ;
#109150 = CARTESIAN_POINT('Ctrl Pts',(8.49801735255452,8.29999999987847,-15.9712471293982)) ;
#109151 = CARTESIAN_POINT('Ctrl Pts',(8.49805590844334,8.29999999988033,-15.971686822978)) ;
#109152 = CARTESIAN_POINT('Ctrl Pts',(8.49806875158486,8.29999999988168,-15.9721289896614)) ;
#109153 = CARTESIAN_POINT('Ctrl Pts',(8.49822249685462,8.2999999998978,-15.9774221678068)) ;
#109154 = CARTESIAN_POINT('Ctrl Pts',(8.49538250015675,8.29999999989889,-15.9823553442684)) ;
#109155 = CARTESIAN_POINT('Ctrl Pts',(8.49246863081132,8.29999999993393,-15.986722860551)) ;
#109156 = CARTESIAN_POINT('Ctrl Pts',(8.48983292606215,8.29999999996562,-15.9906734437939)) ;
#109157 = CARTESIAN_POINT('Ctrl Pts',(8.48683766317129,8.3,-15.9943922110698)) ;
#109158 = CARTESIAN_POINT('Ctrl Pts',(8.48377316486175,8.3,-15.9980519562975)) ;
#109159 = CARTESIAN_POINT('',(8.48377223398316,8.3,-17.78)) ;
#109160 = CARTESIAN_POINT('',(7.1,8.3,-17.78)) ;
#109161 = CARTESIAN_POINT('',(8.48377267093845,8.29999999999968,-14.4819474549958)) ;
#109162 = CARTESIAN_POINT('',(8.48377223398316,8.3,-17.78)) ;
#109163 = CARTESIAN_POINT('',(8.4,8.3,-14.697927110149)) ;
#109164 = CARTESIAN_POINT('Ctrl Pts',(8.48377316486179,8.3,-14.4819480437025)) ;
#109165 = CARTESIAN_POINT('Ctrl Pts',(8.48683766317135,8.3,-14.4856077889302)) ;
#109166 = CARTESIAN_POINT('Ctrl Pts',(8.48983292606214,8.29999999996562,-14.4893265562061)) ;
#109167 = CARTESIAN_POINT('Ctrl Pts',(8.49246863081131,8.29999999993393,-14.493277139449)) ;
#109168 = CARTESIAN_POINT('Ctrl Pts',(8.49538250015675,8.29999999989889,-14.4976446557316)) ;
#109169 = CARTESIAN_POINT('Ctrl Pts',(8.49822249685463,8.2999999998978,-14.5025778321932)) ;
#109170 = CARTESIAN_POINT('Ctrl Pts',(8.49806875158486,8.29999999988168,-14.5078710103386)) ;
#109171 = CARTESIAN_POINT('Ctrl Pts',(8.49805590844334,8.29999999988033,-14.508313177022)) ;
#109172 = CARTESIAN_POINT('Ctrl Pts',(8.49801735255452,8.29999999987847,-14.5087528706018)) ;
#109173 = CARTESIAN_POINT('Ctrl Pts',(8.49795530287013,8.29999999987615,-14.5091889625506)) ;
#109174 = CARTESIAN_POINT('Ctrl Pts',(8.49764594190815,8.29999999986456,-14.5113631851291)) ;
#109175 = CARTESIAN_POINT('Ctrl Pts',(8.49675259754384,8.2999999998405,-14.5134478740673)) ;
#109176 = CARTESIAN_POINT('Ctrl Pts',(8.49555027122431,8.29999999981726,-14.51530319299)) ;
#109177 = CARTESIAN_POINT('Ctrl Pts',(8.4941067657021,8.29999999978935,-14.5175306773816)) ;
#109178 = CARTESIAN_POINT('Ctrl Pts',(8.49231306928119,8.29999999977353,-14.519499896352)) ;
#109179 = CARTESIAN_POINT('Ctrl Pts',(8.49047938958767,8.29999999977836,-14.5213972939748)) ;
#109180 = CARTESIAN_POINT('Ctrl Pts',(8.48681202348066,8.29999999978803,-14.5251920961739)) ;
#109181 = CARTESIAN_POINT('Ctrl Pts',(8.48287934332708,8.29999999986032,-14.5287346907302)) ;
#109182 = CARTESIAN_POINT('Ctrl Pts',(8.47901674443308,8.29999999990152,-14.53234331476)) ;
#109183 = CARTESIAN_POINT('Ctrl Pts',(8.47874052296043,8.29999999990447,-14.5326013740281)) ;
#109184 = CARTESIAN_POINT('Ctrl Pts',(8.47846450284309,8.2999999999073,-14.5328596613565)) ;
#109185 = CARTESIAN_POINT('Ctrl Pts',(8.47818870097126,8.29999999991001,-14.5331181900299)) ;
#109186 = CARTESIAN_POINT('Ctrl Pts',(8.47075185325581,8.29999999998296,-14.540089275328)) ;
#109187 = CARTESIAN_POINT('Ctrl Pts',(8.46347271757076,8.29999999998104,-14.547236821007)) ;
#109188 = CARTESIAN_POINT('Ctrl Pts',(8.45667934899942,8.29999999998018,-14.5548126083154)) ;
#109189 = CARTESIAN_POINT('Ctrl Pts',(8.44963335392745,8.2999999999793,-14.5626701181032)) ;
#109190 = CARTESIAN_POINT('Ctrl Pts',(8.44304226791565,8.29999999996634,-14.571000256345)) ;
#109191 = CARTESIAN_POINT('Ctrl Pts',(8.43712466127421,8.29999999997622,-14.579666888942)) ;
#109192 = CARTESIAN_POINT('Ctrl Pts',(8.43698358608697,8.29999999997646,-14.5798735006502)) ;
#109193 = CARTESIAN_POINT('Ctrl Pts',(8.43684287437574,8.29999999997671,-14.5800803512793)) ;
#109194 = CARTESIAN_POINT('Ctrl Pts',(8.43670252680326,8.29999999997696,-14.5802874394955)) ;
#109195 = CARTESIAN_POINT('Ctrl Pts',(8.42665365624143,8.29999999999548,-14.5951149327151)) ;
#109196 = CARTESIAN_POINT('Ctrl Pts',(8.41848789916211,8.29999999999779,-14.611134863194)) ;
#109197 = CARTESIAN_POINT('Ctrl Pts',(8.4124226058228,8.29999999999911,-14.6279180514005)) ;
#109198 = CARTESIAN_POINT('Ctrl Pts',(8.40662497274065,8.30000000000037,-14.6439606006601)) ;
#109199 = CARTESIAN_POINT('Ctrl Pts',(8.4027459894583,8.3,-14.660702193922)) ;
#109200 = CARTESIAN_POINT('Ctrl Pts',(8.40101973895655,8.3,-14.6777797883442)) ;
#109201 = CARTESIAN_POINT('Ctrl Pts',(8.40034533497793,8.3,-14.6844515880696)) ;
#109202 = CARTESIAN_POINT('Ctrl Pts',(8.40000003014814,8.3,-14.6911746730409)) ;
#109203 = CARTESIAN_POINT('Ctrl Pts',(8.4,8.3,-14.697927110149)) ;
#109204 = CARTESIAN_POINT('',(8.4,8.3,-15.8236545563009)) ;
#109205 = CARTESIAN_POINT('Origin',(10.,7.8,-17.78)) ;
#109206 = CARTESIAN_POINT('',(8.56837722373804,8.27720759208727,-14.5074948832495)) ;
#109207 = CARTESIAN_POINT('',(8.54843785958925,8.28385404680358,-14.4839803122607)) ;
#109208 = CARTESIAN_POINT('Ctrl Pts',(8.56837722339832,8.27720759220056,-14.5074948833623)) ;
#109209 = CARTESIAN_POINT('Ctrl Pts',(8.56792584473107,8.27735805175631,-14.5070046902277)) ;
#109210 = CARTESIAN_POINT('Ctrl Pts',(8.56747319573485,8.27750893475505,-14.5065157932638)) ;
#109211 = CARTESIAN_POINT('Ctrl Pts',(8.56702308739659,8.2776589708678,-14.5060243039587)) ;
#109212 = CARTESIAN_POINT('Ctrl Pts',(8.56055949575605,8.27981350141465,-14.4989664783343)) ;
#109213 = CARTESIAN_POINT('Ctrl Pts',(8.5543545977397,8.28188180075344,-14.4916283954692)) ;
#109214 = CARTESIAN_POINT('Ctrl Pts',(8.54852002808959,8.28382665730347,-14.4839858663514)) ;
#109215 = CARTESIAN_POINT('',(8.51539953939799,8.29486682020067,-14.4709403301229)) ;
#109216 = CARTESIAN_POINT('Origin',(8.52916905055884,8.29027698314705,-14.490734470481)) ;
#109217 = CARTESIAN_POINT('',(8.51539501058484,8.29486832980505,-17.78)) ;
#109218 = CARTESIAN_POINT('',(9.93162277660169,7.82279240779944,-14.2802872911617)) ;
#109219 = CARTESIAN_POINT('',(9.93162277660169,7.82279240779944,-17.78)) ;
#109220 = CARTESIAN_POINT('',(8.48593528106273,8.30468823964576,-14.5212352070849)) ;
#109221 = CARTESIAN_POINT('Origin',(10.,6.8,-17.78)) ;
#109222 = CARTESIAN_POINT('',(10.,6.8847127088383,-14.2802872911617)) ;
#109223 = CARTESIAN_POINT('',(10.,7.72792407799439,-14.2802872911617)) ;
#109224 = CARTESIAN_POINT('',(10.,7.8,-14.2802872911617)) ;
#109225 = CARTESIAN_POINT('',(10.,7.72792407799439,-17.78)) ;
#109226 = CARTESIAN_POINT('',(10.,6.8847127088383,-17.78)) ;
#109227 = CARTESIAN_POINT('Origin',(8.5,6.55,-17.78)) ;
#109228 = CARTESIAN_POINT('',(8.50816305748851,6.55136011924293,-14.4626273778919)) ;
#109229 = CARTESIAN_POINT('Ctrl Pts',(8.50816120922618,6.5513602015377,-14.462623588472)) ;
#109230 = CARTESIAN_POINT('Ctrl Pts',(8.50982330775197,6.55163721795866,-14.4618189278179)) ;
#109231 = CARTESIAN_POINT('Ctrl Pts',(8.51162127657709,6.55193687942951,-14.4612790284411)) ;
#109232 = CARTESIAN_POINT('Ctrl Pts',(8.51523682141417,6.5525394702357,-14.4605710923352)) ;
#109233 = CARTESIAN_POINT('Ctrl Pts',(8.51710259142354,6.55285043190392,-14.4603934679393)) ;
#109234 = CARTESIAN_POINT('Ctrl Pts',(8.52217030373185,6.55369505062198,-14.4602356911265)) ;
#109235 = CARTESIAN_POINT('Ctrl Pts',(8.52587381749838,6.5543123029164,-14.4604838833944)) ;
#109236 = CARTESIAN_POINT('Ctrl Pts',(8.5348242152787,6.55580403587979,-14.4617298501839)) ;
#109237 = CARTESIAN_POINT('Ctrl Pts',(8.53952102462535,6.5565868367346,-14.4632204474233)) ;
#109238 = CARTESIAN_POINT('Ctrl Pts',(8.54640674065696,6.5577344560732,-14.4663682122454)) ;
#109239 = CARTESIAN_POINT('Ctrl Pts',(8.55013419152133,6.55835569858689,-14.4682367302301)) ;
#109240 = CARTESIAN_POINT('Ctrl Pts',(8.55581906875145,6.55930317812524,-14.4720433754295)) ;
#109241 = CARTESIAN_POINT('Ctrl Pts',(8.55861150732132,6.55976858455355,-14.4742775555629)) ;
#109242 = CARTESIAN_POINT('Ctrl Pts',(8.56125821409731,6.56020970234955,-14.4774494566561)) ;
#109243 = CARTESIAN_POINT('',(9.91643989873054,6.78607331645509,-14.2802872911617)) ;
#109244 = CARTESIAN_POINT('',(9.98442535909739,6.79740422651623,-14.2689563811006)) ;
#109245 = CARTESIAN_POINT('',(9.91643989873054,6.78607331645509,-17.78)) ;
#109246 = CARTESIAN_POINT('',(8.50816364570071,6.55136060761679,-17.78)) ;
#109247 = CARTESIAN_POINT('Origin',(1.25,6.55,-17.78)) ;
#109248 = CARTESIAN_POINT('',(8.49172372711481,6.55000000000007,-16.0094558427306)) ;
#109249 = CARTESIAN_POINT('',(8.49172374697018,6.55,-17.78)) ;
#109250 = CARTESIAN_POINT('',(8.4,6.55,-15.7806780018997)) ;
#109251 = CARTESIAN_POINT('Ctrl Pts',(8.49172374697018,6.55000000000104,-16.0094557456557)) ;
#109252 = CARTESIAN_POINT('Ctrl Pts',(8.49606803673629,6.55000000001052,-16.0059505863269)) ;
#109253 = CARTESIAN_POINT('Ctrl Pts',(8.50046735944504,6.54999999990301,-16.0025119042493)) ;
#109254 = CARTESIAN_POINT('Ctrl Pts',(8.50920280475194,6.55000000136501,-15.995516026702)) ;
#109255 = CARTESIAN_POINT('Ctrl Pts',(8.51365366733368,6.55000000372466,-15.9920189182923)) ;
#109256 = CARTESIAN_POINT('Ctrl Pts',(8.51786969589109,6.55000000840872,-15.9875740514917)) ;
#109257 = CARTESIAN_POINT('Ctrl Pts',(8.5182483557534,6.5500000088438,-15.9871628343557)) ;
#109258 = CARTESIAN_POINT('Ctrl Pts',(8.51893753951069,6.55000000964298,-15.9863894122641)) ;
#109259 = CARTESIAN_POINT('Ctrl Pts',(8.51925555226624,6.55000001000021,-15.9860246830609)) ;
#109260 = CARTESIAN_POINT('Ctrl Pts',(8.52125362518915,6.55000001218547,-15.9836369664008)) ;
#109261 = CARTESIAN_POINT('Ctrl Pts',(8.52280131776514,6.55000000862054,-15.9813625215737)) ;
#109262 = CARTESIAN_POINT('Ctrl Pts',(8.52354796988915,6.55000000490364,-15.9762172682012)) ;
#109263 = CARTESIAN_POINT('Ctrl Pts',(8.52233587755862,6.5500000056078,-15.9735629178234)) ;
#109264 = CARTESIAN_POINT('Ctrl Pts',(8.52032554216563,6.55000000470579,-15.9711610105706)) ;
#109265 = CARTESIAN_POINT('Ctrl Pts',(8.52004618744964,6.55000000456892,-15.9708554672246)) ;
#109266 = CARTESIAN_POINT('Ctrl Pts',(8.51943244221705,6.55000000425259,-15.9702375575506)) ;
#109267 = CARTESIAN_POINT('Ctrl Pts',(8.51910103101854,6.55000000405877,-15.9699172773213)) ;
#109268 = CARTESIAN_POINT('Ctrl Pts',(8.51460799223803,6.55000000141241,-15.9657349310042)) ;
#109269 = CARTESIAN_POINT('Ctrl Pts',(8.50969722522558,6.55000000036127,-15.962960241153)) ;
#109270 = CARTESIAN_POINT('Ctrl Pts',(8.50463600502757,6.55000000021577,-15.9596634748388)) ;
#109271 = CARTESIAN_POINT('Ctrl Pts',(8.50427412871943,6.55000000020764,-15.9594272801265)) ;
#109272 = CARTESIAN_POINT('Ctrl Pts',(8.49410349041848,6.55000000002643,-15.9527743312814)) ;
#109273 = CARTESIAN_POINT('Ctrl Pts',(8.48448997361521,6.54999999999179,-15.9460809389623)) ;
#109274 = CARTESIAN_POINT('Ctrl Pts',(8.46629237463075,6.55000000001684,-15.9309770243887)) ;
#109275 = CARTESIAN_POINT('Ctrl Pts',(8.45766562693769,6.55000000000151,-15.9225939316618)) ;
#109276 = CARTESIAN_POINT('Ctrl Pts',(8.44955830666689,6.54999999999999,-15.9132123342681)) ;
#109277 = CARTESIAN_POINT('Ctrl Pts',(8.44937081015215,6.54999999999999,-15.9129944283117)) ;
#109278 = CARTESIAN_POINT('Ctrl Pts',(8.43720071044432,6.5500000000026,-15.8987892740219)) ;
#109279 = CARTESIAN_POINT('Ctrl Pts',(8.42721384365784,6.55000000009148,-15.8832566681901)) ;
#109280 = CARTESIAN_POINT('Ctrl Pts',(8.41184903642351,6.55000000007035,-15.8505950553188)) ;
#109281 = CARTESIAN_POINT('Ctrl Pts',(8.40635547808308,6.5500000000232,-15.8335173325289)) ;
#109282 = CARTESIAN_POINT('Ctrl Pts',(8.40108598764573,6.5499999999995,-15.8043588087541)) ;
#109283 = CARTESIAN_POINT('Ctrl Pts',(8.4,6.55,-15.7925595279378)) ;
#109284 = CARTESIAN_POINT('Ctrl Pts',(8.4,6.55,-15.7806780018997)) ;
#109285 = CARTESIAN_POINT('',(8.4,6.55,-14.6993219981003)) ;
#109286 = CARTESIAN_POINT('',(8.4,6.55,-14.5163606076168)) ;
#109287 = CARTESIAN_POINT('',(8.4917237271148,6.5500000000004,-14.4705441572684)) ;
#109288 = CARTESIAN_POINT('Ctrl Pts',(8.4,6.55,-14.6993219981003)) ;
#109289 = CARTESIAN_POINT('Ctrl Pts',(8.4,6.55,-14.6814603515949)) ;
#109290 = CARTESIAN_POINT('Ctrl Pts',(8.40245177849651,6.55000000000111,-14.6637850580908)) ;
#109291 = CARTESIAN_POINT('Ctrl Pts',(8.40709634751497,6.55000000003438,-14.6467518487573)) ;
#109292 = CARTESIAN_POINT('Ctrl Pts',(8.41193897064573,6.55000000006908,-14.6289923078436)) ;
#109293 = CARTESIAN_POINT('Ctrl Pts',(8.41916594308082,6.55000000013771,-14.6119288881443)) ;
#109294 = CARTESIAN_POINT('Ctrl Pts',(8.42853896333557,6.55000000013582,-14.5960812673187)) ;
#109295 = CARTESIAN_POINT('Ctrl Pts',(8.43455058705845,6.55000000013461,-14.5859169946812)) ;
#109296 = CARTESIAN_POINT('Ctrl Pts',(8.44144611055244,6.55000000009672,-14.5762530007228)) ;
#109297 = CARTESIAN_POINT('Ctrl Pts',(8.44917210140206,6.55000000005186,-14.5672326831017)) ;
#109298 = CARTESIAN_POINT('Ctrl Pts',(8.44936219523639,6.55000000005076,-14.5670107430558)) ;
#109299 = CARTESIAN_POINT('Ctrl Pts',(8.44955278293315,6.55000000004969,-14.5667892022863)) ;
#109300 = CARTESIAN_POINT('Ctrl Pts',(8.44974386351696,6.55000000004865,-14.5665680630168)) ;
#109301 = CARTESIAN_POINT('Ctrl Pts',(8.45766118910685,6.55000000000559,-14.5574052712634)) ;
#109302 = CARTESIAN_POINT('Ctrl Pts',(8.46628870646478,6.54999999999864,-14.5490215515033)) ;
#109303 = CARTESIAN_POINT('Ctrl Pts',(8.47555348469884,6.55000000000007,-14.5413352759491)) ;
#109304 = CARTESIAN_POINT('Ctrl Pts',(8.48448851770303,6.55000000000144,-14.5339225647086)) ;
#109305 = CARTESIAN_POINT('Ctrl Pts',(8.49410273695376,6.5500000000304,-14.5272346929705)) ;
#109306 = CARTESIAN_POINT('Ctrl Pts',(8.50391213313781,6.55000000016212,-14.5208238957712)) ;
#109307 = CARTESIAN_POINT('Ctrl Pts',(8.50409415224108,6.55000000016456,-14.5207049396667)) ;
#109308 = CARTESIAN_POINT('Ctrl Pts',(8.50427622716234,6.55000000016576,-14.5205860597931)) ;
#109309 = CARTESIAN_POINT('Ctrl Pts',(8.50445835579895,6.55000000016577,-14.520467254632)) ;
#109310 = CARTESIAN_POINT('Ctrl Pts',(8.50464048443556,6.55000000016577,-14.5203484494708)) ;
#109311 = CARTESIAN_POINT('Ctrl Pts',(8.50482266678753,6.55000000016459,-14.5202297190221)) ;
#109312 = CARTESIAN_POINT('Ctrl Pts',(8.50500490075221,6.55000000016234,-14.5201110617675)) ;
#109313 = CARTESIAN_POINT('Ctrl Pts',(8.50970297364421,6.55000000010443,-14.5170520248173)) ;
#109314 = CARTESIAN_POINT('Ctrl Pts',(8.51460443926437,6.55000000028677,-14.5142756540706)) ;
#109315 = CARTESIAN_POINT('Ctrl Pts',(8.5187483092633,6.55000000038295,-14.5104369847284)) ;
#109316 = CARTESIAN_POINT('Ctrl Pts',(8.51909542442957,6.55000000039101,-14.5101154349821)) ;
#109317 = CARTESIAN_POINT('Ctrl Pts',(8.51943721516332,6.55000000039358,-14.5097864145015)) ;
#109318 = CARTESIAN_POINT('Ctrl Pts',(8.51977310187181,6.55000000039099,-14.5094491161473)) ;
#109319 = CARTESIAN_POINT('Ctrl Pts',(8.52085916897635,6.55000000038261,-14.5083584845811)) ;
#109320 = CARTESIAN_POINT('Ctrl Pts',(8.52182399801738,6.55000000033868,-14.507044620882)) ;
#109321 = CARTESIAN_POINT('Ctrl Pts',(8.5224633406346,6.55000000029842,-14.5056267666597)) ;
#109322 = CARTESIAN_POINT('Ctrl Pts',(8.52278301194321,6.55000000027829,-14.5049178395485)) ;
#109323 = CARTESIAN_POINT('Ctrl Pts',(8.52302131164586,6.55000000025926,-14.5041829148066)) ;
#109324 = CARTESIAN_POINT('Ctrl Pts',(8.52315270869753,6.55000000024662,-14.503436897635)) ;
#109325 = CARTESIAN_POINT('Ctrl Pts',(8.52328410574919,6.55000000023398,-14.5026908804635)) ;
#109326 = CARTESIAN_POINT('Ctrl Pts',(8.52330860014986,6.55000000022778,-14.5019337708624)) ;
#109327 = CARTESIAN_POINT('Ctrl Pts',(8.52320066085451,6.55000000023233,-14.5011804740329)) ;
#109328 = CARTESIAN_POINT('Ctrl Pts',(8.52284031330749,6.55000000024754,-14.4986656469369)) ;
#109329 = CARTESIAN_POINT('Ctrl Pts',(8.52133564423351,6.55000000029586,-14.4964067380131)) ;
#109330 = CARTESIAN_POINT('Ctrl Pts',(8.5196587899188,6.55000000031744,-14.4943986514954)) ;
#109331 = CARTESIAN_POINT('Ctrl Pts',(8.51932554032813,6.55000000032173,-14.4939995744831)) ;
#109332 = CARTESIAN_POINT('Ctrl Pts',(8.51898545723479,6.55000000032523,-14.4936103757649)) ;
#109333 = CARTESIAN_POINT('Ctrl Pts',(8.51864615038492,6.5500000003277,-14.4932310123194)) ;
#109334 = CARTESIAN_POINT('Ctrl Pts',(8.51455081658662,6.55000000035749,-14.4886522072033)) ;
#109335 = CARTESIAN_POINT('Ctrl Pts',(8.50963987409779,6.55000000028079,-14.4848202086187)) ;
#109336 = CARTESIAN_POINT('Ctrl Pts',(8.5048217738226,6.55000000018959,-14.4809688701254)) ;
#109337 = CARTESIAN_POINT('Ctrl Pts',(8.5004640292375,6.5500000001071,-14.4774855160012)) ;
#109338 = CARTESIAN_POINT('Ctrl Pts',(8.49606692679175,6.55000000001227,-14.4740490105462)) ;
#109339 = CARTESIAN_POINT('Ctrl Pts',(8.49172374697017,6.55000000000105,-14.4705442543438)) ;
#109340 = CARTESIAN_POINT('',(8.49172374697018,6.55,-17.78)) ;
#109341 = CARTESIAN_POINT('',(-0.9,6.55,-14.39)) ;
#109342 = CARTESIAN_POINT('',(-0.900000000000001,6.55,-17.78)) ;
#109343 = CARTESIAN_POINT('',(1.15,6.55,-14.39)) ;
#109344 = CARTESIAN_POINT('',(1.25,6.55,-14.39)) ;
#109345 = CARTESIAN_POINT('',(1.35,6.55,-14.59)) ;
#109346 = CARTESIAN_POINT('Origin',(1.15,6.55,-14.59)) ;
#109347 = CARTESIAN_POINT('',(1.35,6.55,-15.89)) ;
#109348 = CARTESIAN_POINT('',(1.35,6.55,-15.99)) ;
#109349 = CARTESIAN_POINT('',(1.15,6.55,-16.09)) ;
#109350 = CARTESIAN_POINT('Origin',(1.15,6.55,-15.89)) ;
#109351 = CARTESIAN_POINT('',(-0.9,6.55,-16.09)) ;
#109352 = CARTESIAN_POINT('',(1.25,6.55,-16.09)) ;
#109353 = CARTESIAN_POINT('',(-0.9,6.55,-17.78)) ;
#109354 = CARTESIAN_POINT('Origin',(1.25,5.3,-17.78)) ;
#109355 = CARTESIAN_POINT('',(1.25,3.15,-16.8831676725155)) ;
#109356 = CARTESIAN_POINT('',(1.25,3.04189189189189,-16.7055279241354)) ;
#109357 = CARTESIAN_POINT('Origin',(1.25,2.95,-16.8831676725155)) ;
#109358 = CARTESIAN_POINT('',(1.25,3.15,-17.78)) ;
#109359 = CARTESIAN_POINT('',(1.25,4.45,-16.8831676725155)) ;
#109360 = CARTESIAN_POINT('',(1.25,4.45,-16.8211388300842)) ;
#109361 = CARTESIAN_POINT('',(1.25,4.55810810810811,-16.7055279241354)) ;
#109362 = CARTESIAN_POINT('Origin',(1.25,4.65,-16.8831676725155)) ;
#109363 = CARTESIAN_POINT('',(1.25,5.26552792413544,-15.9981081081081)) ;
#109364 = CARTESIAN_POINT('Origin',(1.25,3.8,-15.24)) ;
#109365 = CARTESIAN_POINT('',(1.25,5.4431676725155,-15.89)) ;
#109366 = CARTESIAN_POINT('Origin',(1.25,5.4431676725155,-16.09)) ;
#109367 = CARTESIAN_POINT('',(1.25,6.45,-15.89)) ;
#109368 = CARTESIAN_POINT('',(1.25,6.55,-15.89)) ;
#109369 = CARTESIAN_POINT('',(1.25,6.45,-14.59)) ;
#109370 = CARTESIAN_POINT('',(1.25,6.45,-14.49)) ;
#109371 = CARTESIAN_POINT('',(1.25,5.4431676725155,-14.59)) ;
#109372 = CARTESIAN_POINT('',(1.25,5.38113883008419,-14.59)) ;
#109373 = CARTESIAN_POINT('',(1.25,5.26552792413544,-14.4818918918919)) ;
#109374 = CARTESIAN_POINT('Origin',(1.25,5.4431676725155,-14.39)) ;
#109375 = CARTESIAN_POINT('',(1.25,4.55810810810811,-13.7744720758646)) ;
#109376 = CARTESIAN_POINT('Origin',(1.25,3.8,-15.24)) ;
#109377 = CARTESIAN_POINT('',(1.25,4.45,-13.5968323274845)) ;
#109378 = CARTESIAN_POINT('Origin',(1.25,4.65,-13.5968323274845)) ;
#109379 = CARTESIAN_POINT('',(1.25,4.45,-12.7)) ;
#109380 = CARTESIAN_POINT('',(1.25,3.15,-13.5968323274845)) ;
#109381 = CARTESIAN_POINT('',(1.25,3.15,-13.6588611699158)) ;
#109382 = CARTESIAN_POINT('',(1.25,3.04189189189189,-13.7744720758646)) ;
#109383 = CARTESIAN_POINT('Origin',(1.25,2.95,-13.5968323274845)) ;
#109384 = CARTESIAN_POINT('',(1.25,2.33447207586456,-14.4818918918919)) ;
#109385 = CARTESIAN_POINT('Origin',(1.25,3.8,-15.24)) ;
#109386 = CARTESIAN_POINT('',(1.25,2.1568323274845,-14.59)) ;
#109387 = CARTESIAN_POINT('Origin',(1.25,2.1568323274845,-14.39)) ;
#109388 = CARTESIAN_POINT('',(1.25,0.973783447787483,-14.59)) ;
#109389 = CARTESIAN_POINT('',(1.25,0.895262490344437,-14.59)) ;
#109390 = CARTESIAN_POINT('',(1.25,0.973783447787483,-15.89)) ;
#109391 = CARTESIAN_POINT('Origin',(1.25,3.8,-15.24)) ;
#109392 = CARTESIAN_POINT('',(1.25,2.1568323274845,-15.89)) ;
#109393 = CARTESIAN_POINT('',(1.25,2.21886116991581,-15.89)) ;
#109394 = CARTESIAN_POINT('',(1.25,2.33447207586456,-15.9981081081081)) ;
#109395 = CARTESIAN_POINT('Origin',(1.25,2.1568323274845,-16.09)) ;
#109396 = CARTESIAN_POINT('Origin',(1.25,3.8,-15.24)) ;
#109397 = CARTESIAN_POINT('Origin',(-2.,0.,-17.78)) ;
#109398 = CARTESIAN_POINT('',(0.899999999999999,0.,-16.84)) ;
#109399 = CARTESIAN_POINT('',(1.1,0.,-16.64)) ;
#109400 = CARTESIAN_POINT('Origin',(0.899999999999999,0.,-16.64)) ;
#109401 = CARTESIAN_POINT('',(-2.,0.,-16.84)) ;
#109402 = CARTESIAN_POINT('',(-2.,0.,-16.84)) ;
#109403 = CARTESIAN_POINT('',(-2.,0.,-17.78)) ;
#109404 = CARTESIAN_POINT('',(9.9,0.,-17.78)) ;
#109405 = CARTESIAN_POINT('',(-2.,0.,-13.64)) ;
#109406 = CARTESIAN_POINT('',(-2.,0.,-17.78)) ;
#109407 = CARTESIAN_POINT('',(0.899999999999999,0.,-13.64)) ;
#109408 = CARTESIAN_POINT('',(0.999999999999999,0.,-13.64)) ;
#109409 = CARTESIAN_POINT('',(1.1,0.,-13.84)) ;
#109410 = CARTESIAN_POINT('Origin',(0.899999999999999,0.,-13.84)) ;
#109411 = CARTESIAN_POINT('',(1.1,0.,-16.74)) ;
#109412 = CARTESIAN_POINT('Origin',(-2.,7.65,-17.78)) ;
#109413 = CARTESIAN_POINT('',(-2.,6.9,-13.64)) ;
#109414 = CARTESIAN_POINT('',(-2.,7.1,-13.84)) ;
#109415 = CARTESIAN_POINT('Origin',(-2.,6.9,-13.84)) ;
#109416 = CARTESIAN_POINT('',(-2.,-1.13380619344889E-17,-13.64)) ;
#109417 = CARTESIAN_POINT('',(-2.,7.55,-17.78)) ;
#109418 = CARTESIAN_POINT('',(-2.,6.9,-16.84)) ;
#109419 = CARTESIAN_POINT('',(-2.,7.,-16.84)) ;
#109420 = CARTESIAN_POINT('',(-2.,7.1,-16.64)) ;
#109421 = CARTESIAN_POINT('Origin',(-2.,6.9,-16.64)) ;
#109422 = CARTESIAN_POINT('',(-2.,7.1,-13.74)) ;
#109423 = CARTESIAN_POINT('Origin',(-1.8,7.,-13.74)) ;
#109424 = CARTESIAN_POINT('',(-1.7,0.1,-13.74)) ;
#109425 = CARTESIAN_POINT('',(-1.9,0.1,-13.74)) ;
#109426 = CARTESIAN_POINT('',(-2.,0.1,-13.74)) ;
#109427 = CARTESIAN_POINT('',(-1.9,0.3,-13.74)) ;
#109428 = CARTESIAN_POINT('',(-1.9,7.,-13.74)) ;
#109429 = CARTESIAN_POINT('Origin',(-1.7,0.3,-13.74)) ;
#109430 = CARTESIAN_POINT('Origin',(-1.8,7.,-16.74)) ;
#109431 = CARTESIAN_POINT('',(-1.9,0.3,-16.74)) ;
#109432 = CARTESIAN_POINT('',(-1.7,0.1,-16.74)) ;
#109433 = CARTESIAN_POINT('Origin',(-1.7,0.3,-16.74)) ;
#109434 = CARTESIAN_POINT('',(-1.9,0.1,-16.74)) ;
#109435 = CARTESIAN_POINT('',(-1.9,1.23908819712629E-17,-16.74)) ;
#109436 = CARTESIAN_POINT('',(0.999999999999999,0.1,-16.74)) ;
#109437 = CARTESIAN_POINT('Origin',(-1.8,-2.2514151555628E-16,-15.24)) ;
#109438 = CARTESIAN_POINT('',(-1.8,4.6,-15.89)) ;
#109439 = CARTESIAN_POINT('',(-1.8,4.6,-14.59)) ;
#109440 = CARTESIAN_POINT('',(-1.8,4.6,-14.69)) ;
#109441 = CARTESIAN_POINT('',(-1.8,0.3,-14.59)) ;
#109442 = CARTESIAN_POINT('',(-1.8,0.2,-14.59)) ;
#109443 = CARTESIAN_POINT('',(-1.8,0.3,-13.84)) ;
#109444 = CARTESIAN_POINT('',(-1.8,0.3,-13.74)) ;
#109445 = CARTESIAN_POINT('',(-1.8,6.9,-13.84)) ;
#109446 = CARTESIAN_POINT('',(-1.8,-5.16691679585995E-17,-13.84)) ;
#109447 = CARTESIAN_POINT('',(-1.8,6.9,-16.64)) ;
#109448 = CARTESIAN_POINT('',(-1.8,6.9,-15.24)) ;
#109449 = CARTESIAN_POINT('',(-1.8,0.3,-16.64)) ;
#109450 = CARTESIAN_POINT('',(-1.8,-3.98613863153961E-16,-16.64)) ;
#109451 = CARTESIAN_POINT('',(-1.8,0.3,-15.89)) ;
#109452 = CARTESIAN_POINT('',(-1.8,0.3,-15.79)) ;
#109453 = CARTESIAN_POINT('',(-1.8,4.5,-15.89)) ;
#109454 = CARTESIAN_POINT('Origin',(0.549999999999999,4.5,-14.69)) ;
#109455 = CARTESIAN_POINT('',(-1.7,0.3,-14.69)) ;
#109456 = CARTESIAN_POINT('',(-1.7,4.4,-14.69)) ;
#109457 = CARTESIAN_POINT('',(-1.7,4.5,-14.69)) ;
#109458 = CARTESIAN_POINT('',(0.45,4.4,-14.69)) ;
#109459 = CARTESIAN_POINT('',(0.45,4.4,-14.69)) ;
#109460 = CARTESIAN_POINT('',(0.45,0.3,-14.69)) ;
#109461 = CARTESIAN_POINT('',(0.45,4.5,-14.69)) ;
#109462 = CARTESIAN_POINT('',(0.549999999999999,0.3,-14.69)) ;
#109463 = CARTESIAN_POINT('Origin',(0.549999999999999,4.5,-15.79)) ;
#109464 = CARTESIAN_POINT('',(0.45,0.3,-15.79)) ;
#109465 = CARTESIAN_POINT('',(0.45,4.4,-15.79)) ;
#109466 = CARTESIAN_POINT('',(0.45,4.5,-15.79)) ;
#109467 = CARTESIAN_POINT('',(-1.7,4.4,-15.79)) ;
#109468 = CARTESIAN_POINT('',(-1.7,4.4,-15.79)) ;
#109469 = CARTESIAN_POINT('',(-1.7,0.3,-15.79)) ;
#109470 = CARTESIAN_POINT('',(-1.7,0.2,-15.79)) ;
#109471 = CARTESIAN_POINT('',(0.549999999999999,0.3,-15.79)) ;
#109472 = CARTESIAN_POINT('Origin',(0.549999999999999,4.5,-15.79)) ;
#109473 = CARTESIAN_POINT('',(-1.7,4.5,-14.79)) ;
#109474 = CARTESIAN_POINT('',(-1.7,4.5,-15.69)) ;
#109475 = CARTESIAN_POINT('',(-1.7,4.5,-15.79)) ;
#109476 = CARTESIAN_POINT('',(0.45,4.5,-15.69)) ;
#109477 = CARTESIAN_POINT('',(0.45,4.5,-15.69)) ;
#109478 = CARTESIAN_POINT('',(0.45,4.5,-14.79)) ;
#109479 = CARTESIAN_POINT('',(0.45,4.5,-15.79)) ;
#109480 = CARTESIAN_POINT('',(-1.7,4.5,-14.79)) ;
#109481 = CARTESIAN_POINT('Origin',(0.55,3.09772049281573E-17,-15.24)) ;
#109482 = CARTESIAN_POINT('',(0.55,2.61224989991992,-15.64)) ;
#109483 = CARTESIAN_POINT('',(0.55,2.65280931275608,-15.69)) ;
#109484 = CARTESIAN_POINT('Ctrl Pts',(0.55,2.61224989991992,-15.64)) ;
#109485 = CARTESIAN_POINT('Ctrl Pts',(0.55,2.61224989991992,-15.643869744162)) ;
#109486 = CARTESIAN_POINT('Ctrl Pts',(0.55,2.61317624258758,-15.6484201039157)) ;
#109487 = CARTESIAN_POINT('Ctrl Pts',(0.55,2.61634258087509,-15.6566330008589)) ;
#109488 = CARTESIAN_POINT('Ctrl Pts',(0.55,2.61951410407877,-15.6616304286453)) ;
#109489 = CARTESIAN_POINT('Ctrl Pts',(0.55,2.63040394024853,-15.6749387190701)) ;
#109490 = CARTESIAN_POINT('Ctrl Pts',(0.55,2.6414836688106,-15.6831705809674)) ;
#109491 = CARTESIAN_POINT('Ctrl Pts',(0.55,2.65280931275608,-15.69)) ;
#109492 = CARTESIAN_POINT('',(0.55,0.3,-15.69)) ;
#109493 = CARTESIAN_POINT('',(0.55,1.39397422176708E-16,-15.69)) ;
#109494 = CARTESIAN_POINT('',(0.55,0.3,-14.79)) ;
#109495 = CARTESIAN_POINT('',(0.55,0.3,-14.69)) ;
#109496 = CARTESIAN_POINT('',(0.55,2.65280931275594,-14.7900000000001)) ;
#109497 = CARTESIAN_POINT('',(0.55,6.35032701027224E-17,-14.79)) ;
#109498 = CARTESIAN_POINT('',(0.55,2.61224989991992,-14.84)) ;
#109499 = CARTESIAN_POINT('Ctrl Pts',(0.55,2.65280931275593,-14.7900000000001)) ;
#109500 = CARTESIAN_POINT('Ctrl Pts',(0.55,2.64148366881051,-14.7968294190327)) ;
#109501 = CARTESIAN_POINT('Ctrl Pts',(0.55,2.6304039402485,-14.8050612809299)) ;
#109502 = CARTESIAN_POINT('Ctrl Pts',(0.55,2.61951410407877,-14.8183695713547)) ;
#109503 = CARTESIAN_POINT('Ctrl Pts',(0.55,2.61634258087509,-14.8233669991411)) ;
#109504 = CARTESIAN_POINT('Ctrl Pts',(0.55,2.61317624258758,-14.8315798960843)) ;
#109505 = CARTESIAN_POINT('Ctrl Pts',(0.55,2.61224989991992,-14.836130255838)) ;
#109506 = CARTESIAN_POINT('Ctrl Pts',(0.55,2.61224989991992,-14.84)) ;
#109507 = CARTESIAN_POINT('',(0.55,2.61224989991992,-14.74)) ;
#109508 = CARTESIAN_POINT('Origin',(0.,0.2,-15.24)) ;
#109509 = CARTESIAN_POINT('',(-1.7,0.2,-15.89)) ;
#109510 = CARTESIAN_POINT('',(-1.7,0.2,-16.64)) ;
#109511 = CARTESIAN_POINT('',(-1.7,0.2,-16.74)) ;
#109512 = CARTESIAN_POINT('',(0.899999999999999,0.2,-16.64)) ;
#109513 = CARTESIAN_POINT('',(0.999999999999999,0.2,-16.64)) ;
#109514 = CARTESIAN_POINT('',(0.899999999999999,0.2,-13.84)) ;
#109515 = CARTESIAN_POINT('',(0.899999999999999,0.2,-13.74)) ;
#109516 = CARTESIAN_POINT('',(-1.7,0.2,-13.84)) ;
#109517 = CARTESIAN_POINT('',(-1.8,0.2,-13.84)) ;
#109518 = CARTESIAN_POINT('',(-1.7,0.2,-14.59)) ;
#109519 = CARTESIAN_POINT('',(-1.7,0.2,-14.69)) ;
#109520 = CARTESIAN_POINT('',(0.65,0.2,-14.59)) ;
#109521 = CARTESIAN_POINT('',(-1.16429916652874E-32,0.2,-14.59)) ;
#109522 = CARTESIAN_POINT('',(0.65,0.2,-15.89)) ;
#109523 = CARTESIAN_POINT('',(0.65,0.2,-15.79)) ;
#109524 = CARTESIAN_POINT('',(-1.35834902761687E-32,0.2,-15.89)) ;
#109525 = CARTESIAN_POINT('Origin',(3.,2.3,-17.78)) ;
#109526 = CARTESIAN_POINT('',(3.,4.2,-14.74)) ;
#109527 = CARTESIAN_POINT('',(3.,3.4,-14.74)) ;
#109528 = CARTESIAN_POINT('',(3.,2.3,-14.74)) ;
#109529 = CARTESIAN_POINT('',(3.,4.3,-14.84)) ;
#109530 = CARTESIAN_POINT('Origin',(3.,4.2,-14.84)) ;
#109531 = CARTESIAN_POINT('',(3.,4.3,-15.64)) ;
#109532 = CARTESIAN_POINT('',(3.,4.3,-17.78)) ;
#109533 = CARTESIAN_POINT('',(3.,4.2,-15.74)) ;
#109534 = CARTESIAN_POINT('Origin',(3.,4.2,-15.64)) ;
#109535 = CARTESIAN_POINT('',(3.,3.4,-15.74)) ;
#109536 = CARTESIAN_POINT('',(3.,2.3,-15.74)) ;
#109537 = CARTESIAN_POINT('',(3.,3.3,-15.64)) ;
#109538 = CARTESIAN_POINT('Origin',(3.,3.4,-15.64)) ;
#109539 = CARTESIAN_POINT('',(3.,3.3,-14.84)) ;
#109540 = CARTESIAN_POINT('',(3.,3.3,-17.78)) ;
#109541 = CARTESIAN_POINT('Origin',(3.,3.4,-14.84)) ;
#109542 = CARTESIAN_POINT('Origin',(-1.,3.8,-15.24)) ;
#109543 = CARTESIAN_POINT('',(-1.,1.6,-17.2021416870349)) ;
#109544 = CARTESIAN_POINT('',(-1.,1.55483870967742,-17.0755519007745)) ;
#109545 = CARTESIAN_POINT('Origin',(-1.,1.40000000000001,-17.2021416870349)) ;
#109546 = CARTESIAN_POINT('',(-1.,1.6,-17.78)) ;
#109547 = CARTESIAN_POINT('',(-1.,2.95,-16.8831676725155)) ;
#109548 = CARTESIAN_POINT('',(-1.,2.95,-15.24)) ;
#109549 = CARTESIAN_POINT('',(-1.,2.1568323274845,-16.09)) ;
#109550 = CARTESIAN_POINT('Origin',(-1.,3.8,-15.24)) ;
#109551 = CARTESIAN_POINT('',(-1.,1.02736587339765,-16.09)) ;
#109552 = CARTESIAN_POINT('',(-1.,3.8,-16.09)) ;
#109553 = CARTESIAN_POINT('Origin',(-1.,3.8,-15.24)) ;
#109554 = CARTESIAN_POINT('Origin',(-1.,3.05,-17.79)) ;
#109555 = CARTESIAN_POINT('',(1.15,3.05,-16.8831676725155)) ;
#109556 = CARTESIAN_POINT('',(1.15,3.05,-16.8211388300842)) ;
#109557 = CARTESIAN_POINT('',(-0.900000000000002,3.05,-16.8831676725155)) ;
#109558 = CARTESIAN_POINT('',(-1.,3.05,-16.8831676725155)) ;
#109559 = CARTESIAN_POINT('',(-0.900000000000002,3.05,-17.79)) ;
#109560 = CARTESIAN_POINT('Origin',(-1.,2.21886116991581,-15.99)) ;
#109561 = CARTESIAN_POINT('',(-0.900000000000002,2.1568323274845,-15.99)) ;
#109562 = CARTESIAN_POINT('',(1.15,2.1568323274845,-15.99)) ;
#109563 = CARTESIAN_POINT('',(1.25,2.1568323274845,-15.99)) ;
#109564 = CARTESIAN_POINT('',(1.15,0.895262490344437,-15.99)) ;
#109565 = CARTESIAN_POINT('',(-0.900000000000002,2.21886116991581,-15.99)) ;
#109566 = CARTESIAN_POINT('Origin',(-1.,3.8,-15.24)) ;
#109567 = CARTESIAN_POINT('',(-0.900000000000002,2.24565220167453,-16.0440540540541)) ;
#109568 = CARTESIAN_POINT('',(-0.900000000000001,2.99594594594595,-16.7943477983255)) ;
#109569 = CARTESIAN_POINT('Origin',(-0.900000000000001,3.8,-15.24)) ;
#109570 = CARTESIAN_POINT('',(1.15,2.99594594594595,-16.7943477983255)) ;
#109571 = CARTESIAN_POINT('',(-1.,2.99594594594595,-16.7943477983255)) ;
#109572 = CARTESIAN_POINT('',(1.15,2.24565220167453,-16.0440540540541)) ;
#109573 = CARTESIAN_POINT('Origin',(1.15,3.8,-15.24)) ;
#109574 = CARTESIAN_POINT('',(-1.,2.24565220167453,-16.0440540540541)) ;
#109575 = CARTESIAN_POINT('Origin',(-1.,3.8,-15.24)) ;
#109576 = CARTESIAN_POINT('',(-0.900000000000002,2.99594594594594,-13.6856522016745)) ;
#109577 = CARTESIAN_POINT('',(-0.900000000000002,2.24565220167453,-14.4359459459459)) ;
#109578 = CARTESIAN_POINT('Origin',(-0.900000000000001,3.8,-15.24)) ;
#109579 = CARTESIAN_POINT('',(1.15,2.24565220167453,-14.4359459459459)) ;
#109580 = CARTESIAN_POINT('',(-1.,2.24565220167453,-14.4359459459459)) ;
#109581 = CARTESIAN_POINT('',(1.15,2.99594594594594,-13.6856522016745)) ;
#109582 = CARTESIAN_POINT('Origin',(1.15,3.8,-15.24)) ;
#109583 = CARTESIAN_POINT('',(-1.,2.99594594594594,-13.6856522016745)) ;
#109584 = CARTESIAN_POINT('Origin',(-1.,2.21886116991581,-14.49)) ;
#109585 = CARTESIAN_POINT('',(1.15,2.1568323274845,-14.49)) ;
#109586 = CARTESIAN_POINT('',(1.15,2.21886116991581,-14.49)) ;
#109587 = CARTESIAN_POINT('',(-0.900000000000002,2.1568323274845,-14.49)) ;
#109588 = CARTESIAN_POINT('',(-1.,2.1568323274845,-14.49)) ;
#109589 = CARTESIAN_POINT('',(-0.900000000000002,0.895262490344437,-14.49)) ;
#109590 = CARTESIAN_POINT('Origin',(-1.,3.05,-12.69)) ;
#109591 = CARTESIAN_POINT('',(-0.900000000000002,3.05,-13.5968323274845)) ;
#109592 = CARTESIAN_POINT('',(1.15,3.05,-13.5968323274845)) ;
#109593 = CARTESIAN_POINT('',(1.25,3.05,-13.5968323274845)) ;
#109594 = CARTESIAN_POINT('',(1.15,3.05,-12.7)) ;
#109595 = CARTESIAN_POINT('',(-0.900000000000002,3.05,-13.6588611699158)) ;
#109596 = CARTESIAN_POINT('Origin',(-1.,3.8,-15.24)) ;
#109597 = CARTESIAN_POINT('',(-1.,2.1568323274845,-14.39)) ;
#109598 = CARTESIAN_POINT('',(-1.,2.95,-13.5968323274845)) ;
#109599 = CARTESIAN_POINT('Origin',(-1.,3.8,-15.24)) ;
#109600 = CARTESIAN_POINT('',(-1.,2.95,-12.7)) ;
#109601 = CARTESIAN_POINT('',(-1.,1.6,-13.2778583129651)) ;
#109602 = CARTESIAN_POINT('',(-1.,1.6,-15.24)) ;
#109603 = CARTESIAN_POINT('',(-1.,1.55483870967743,-13.4044480992254)) ;
#109604 = CARTESIAN_POINT('Origin',(-1.,1.40000000000001,-13.2778583129651)) ;
#109605 = CARTESIAN_POINT('',(-1.,1.02736587339765,-14.39)) ;
#109606 = CARTESIAN_POINT('Origin',(-1.,3.8,-15.24)) ;
#109607 = CARTESIAN_POINT('',(-1.,2.21886116991581,-14.39)) ;
#109608 = CARTESIAN_POINT('Origin',(-1.,3.8,-15.24)) ;
#109609 = CARTESIAN_POINT('',(-1.,5.4431676725155,-16.09)) ;
#109610 = CARTESIAN_POINT('',(-1.,4.65,-16.8831676725155)) ;
#109611 = CARTESIAN_POINT('Origin',(-1.,3.8,-15.24)) ;
#109612 = CARTESIAN_POINT('',(-1.,4.65,-15.24)) ;
#109613 = CARTESIAN_POINT('',(-1.,6.45,-16.09)) ;
#109614 = CARTESIAN_POINT('',(-1.,6.45,-15.99)) ;
#109615 = CARTESIAN_POINT('',(-1.,3.8,-16.09)) ;
#109616 = CARTESIAN_POINT('Origin',(-1.,4.55,-16.8211388300842)) ;
#109617 = CARTESIAN_POINT('',(-0.900000000000001,4.55,-16.8831676725155)) ;
#109618 = CARTESIAN_POINT('',(1.15,4.55,-16.8831676725155)) ;
#109619 = CARTESIAN_POINT('',(1.25,4.55,-16.8831676725155)) ;
#109620 = CARTESIAN_POINT('',(1.15,4.55,-17.78)) ;
#109621 = CARTESIAN_POINT('',(-0.900000000000001,4.55,-16.8211388300842)) ;
#109622 = CARTESIAN_POINT('Origin',(-1.,3.8,-15.24)) ;
#109623 = CARTESIAN_POINT('',(-0.900000000000001,4.60405405405406,-16.7943477983255)) ;
#109624 = CARTESIAN_POINT('',(-0.900000000000001,5.35434779832547,-16.0440540540541)) ;
#109625 = CARTESIAN_POINT('Origin',(-0.900000000000001,3.8,-15.24)) ;
#109626 = CARTESIAN_POINT('',(1.15,5.35434779832547,-16.0440540540541)) ;
#109627 = CARTESIAN_POINT('',(-1.,5.35434779832547,-16.0440540540541)) ;
#109628 = CARTESIAN_POINT('',(1.15,4.60405405405405,-16.7943477983255)) ;
#109629 = CARTESIAN_POINT('Origin',(1.15,3.8,-15.24)) ;
#109630 = CARTESIAN_POINT('',(-1.,4.60405405405406,-16.7943477983255)) ;
#109631 = CARTESIAN_POINT('Origin',(-1.,6.55,-15.99)) ;
#109632 = CARTESIAN_POINT('',(-0.900000000000001,5.4431676725155,-15.99)) ;
#109633 = CARTESIAN_POINT('',(-0.9,6.45,-15.99)) ;
#109634 = CARTESIAN_POINT('',(-0.9,6.55,-15.99)) ;
#109635 = CARTESIAN_POINT('',(1.15,6.45,-15.99)) ;
#109636 = CARTESIAN_POINT('',(-1.,6.45,-15.99)) ;
#109637 = CARTESIAN_POINT('',(1.15,5.4431676725155,-15.99)) ;
#109638 = CARTESIAN_POINT('',(1.15,5.38113883008419,-15.99)) ;
#109639 = CARTESIAN_POINT('',(-1.,5.4431676725155,-15.99)) ;
#109640 = CARTESIAN_POINT('Origin',(-1.,3.8,-15.24)) ;
#109641 = CARTESIAN_POINT('',(-0.900000000000001,5.35434779832547,-14.4359459459459)) ;
#109642 = CARTESIAN_POINT('',(-0.900000000000001,4.60405405405405,-13.6856522016745)) ;
#109643 = CARTESIAN_POINT('Origin',(-0.900000000000001,3.8,-15.24)) ;
#109644 = CARTESIAN_POINT('',(1.15,4.60405405405405,-13.6856522016745)) ;
#109645 = CARTESIAN_POINT('',(-1.,4.60405405405405,-13.6856522016745)) ;
#109646 = CARTESIAN_POINT('',(1.15,5.35434779832547,-14.4359459459459)) ;
#109647 = CARTESIAN_POINT('Origin',(1.15,3.8,-15.24)) ;
#109648 = CARTESIAN_POINT('',(-1.,5.35434779832547,-14.4359459459459)) ;
#109649 = CARTESIAN_POINT('Origin',(-1.,4.55,-13.6588611699158)) ;
#109650 = CARTESIAN_POINT('',(1.15,4.55,-13.5968323274845)) ;
#109651 = CARTESIAN_POINT('',(1.15,4.55,-13.6588611699158)) ;
#109652 = CARTESIAN_POINT('',(-0.900000000000001,4.55,-13.5968323274845)) ;
#109653 = CARTESIAN_POINT('',(-1.,4.55,-13.5968323274845)) ;
#109654 = CARTESIAN_POINT('',(-0.900000000000001,4.55,-12.7)) ;
#109655 = CARTESIAN_POINT('Origin',(-1.,6.55,-14.49)) ;
#109656 = CARTESIAN_POINT('',(1.15,5.4431676725155,-14.49)) ;
#109657 = CARTESIAN_POINT('',(1.15,6.45,-14.49)) ;
#109658 = CARTESIAN_POINT('',(1.15,6.55,-14.49)) ;
#109659 = CARTESIAN_POINT('',(-0.9,6.45,-14.49)) ;
#109660 = CARTESIAN_POINT('',(-1.,6.45,-14.49)) ;
#109661 = CARTESIAN_POINT('',(-0.900000000000001,5.4431676725155,-14.49)) ;
#109662 = CARTESIAN_POINT('',(-0.900000000000001,5.38113883008419,-14.49)) ;
#109663 = CARTESIAN_POINT('',(1.25,5.4431676725155,-14.49)) ;
#109664 = CARTESIAN_POINT('Origin',(-1.,3.8,-15.24)) ;
#109665 = CARTESIAN_POINT('',(-1.,5.4431676725155,-14.39)) ;
#109666 = CARTESIAN_POINT('',(-1.,6.45,-14.39)) ;
#109667 = CARTESIAN_POINT('',(-1.,6.55,-14.39)) ;
#109668 = CARTESIAN_POINT('',(-1.,6.45,-15.24)) ;
#109669 = CARTESIAN_POINT('',(-1.,4.65,-13.5968323274845)) ;
#109670 = CARTESIAN_POINT('',(-1.,4.65,-13.6588611699158)) ;
#109671 = CARTESIAN_POINT('Origin',(-1.,3.8,-15.24)) ;
#109672 = CARTESIAN_POINT('Origin',(10.,4.35421736843756,-16.115)) ;
#109673 = CARTESIAN_POINT('',(9.91643989873054,7.72792407799439,-16.1010733164551)) ;
#109674 = CARTESIAN_POINT('',(8.58356010126947,8.17221734381475,-15.8789266835449)) ;
#109675 = CARTESIAN_POINT('',(8.47075240319158,8.20981990984071,-15.8601254005319)) ;
#109676 = CARTESIAN_POINT('',(8.58356010126947,6.66256607592813,-15.8789266835449)) ;
#109677 = CARTESIAN_POINT('',(8.58356010126947,6.64863939238321,-15.8789266835449)) ;
#109678 = CARTESIAN_POINT('',(9.91643989873054,6.8847127088383,-16.1010733164551)) ;
#109679 = CARTESIAN_POINT('',(9.98442535909739,6.89604361889945,-16.1124042265162)) ;
#109680 = CARTESIAN_POINT('',(9.91643989873054,7.8,-16.1010733164551)) ;
#109681 = CARTESIAN_POINT('Origin',(8.5,4.35421736843756,-15.865)) ;
#109682 = CARTESIAN_POINT('',(8.5,8.17221734381475,-15.7802872911617)) ;
#109683 = CARTESIAN_POINT('',(8.50000000129681,8.20000000266559,-15.782105625353)) ;
#109684 = CARTESIAN_POINT('Origin',(8.5,8.17870774547598,-15.9690376376839)) ;
#109685 = CARTESIAN_POINT('',(8.5,8.2,-14.6563454436991)) ;
#109686 = CARTESIAN_POINT('',(8.5,6.66256607592813,-14.6997127088383)) ;
#109687 = CARTESIAN_POINT('',(8.5,6.64863939238321,-14.6997127088383)) ;
#109688 = CARTESIAN_POINT('',(8.50000000002143,6.64999999935441,-14.6993178443262)) ;
#109689 = CARTESIAN_POINT('Origin',(8.5,6.65811550062454,-14.503188522499)) ;
#109690 = CARTESIAN_POINT('',(8.49999999999933,6.65000073218972,-15.7806896909636)) ;
#109691 = CARTESIAN_POINT('',(8.5,6.65,-15.9636393923832)) ;
#109692 = CARTESIAN_POINT('',(8.5,6.66256607592813,-15.7802872911617)) ;
#109693 = CARTESIAN_POINT('Origin',(8.5,6.65133313712442,-15.9770100835082)) ;
#109694 = CARTESIAN_POINT('',(8.5,8.20007071090457,-15.7802872911617)) ;
#109695 = CARTESIAN_POINT('Origin',(8.5,4.35421736843756,-14.615)) ;
#109696 = CARTESIAN_POINT('',(9.91643989873054,6.8847127088383,-14.3789266835449)) ;
#109697 = CARTESIAN_POINT('',(8.58356010126947,6.66256607592813,-14.6010733164551)) ;
#109698 = CARTESIAN_POINT('',(8.48442535909739,6.64604361889945,-14.6175957734838)) ;
#109699 = CARTESIAN_POINT('',(8.58356010126947,8.20007071090456,-14.6010733164551)) ;
#109700 = CARTESIAN_POINT('',(9.91643989873054,7.72792407799439,-14.3789266835449)) ;
#109701 = CARTESIAN_POINT('',(9.97075240319158,7.70981990984071,-14.3698745994681)) ;
#109702 = CARTESIAN_POINT('',(9.91643989873054,6.8,-14.3789266835449)) ;
#109703 = CARTESIAN_POINT('Origin',(8.5,3.65,-14.74)) ;
#109704 = CARTESIAN_POINT('',(8.45734623443633,3.62014236410543,-15.1420655561573)) ;
#109705 = CARTESIAN_POINT('',(8.02582401135442,3.3180768079481,-14.84)) ;
#109706 = CARTESIAN_POINT('',(8.34729988159781,3.54310991711847,-15.0650331091704)) ;
#109707 = CARTESIAN_POINT('',(8.02582401135442,3.31807680794809,-15.64)) ;
#109708 = CARTESIAN_POINT('',(8.02582401135442,3.3180768079481,-14.74)) ;
#109709 = CARTESIAN_POINT('',(8.45734623443633,3.62014236410543,-15.3379344438427)) ;
#109710 = CARTESIAN_POINT('',(8.70083523513316,3.79058466459322,-15.1674921433549)) ;
#109711 = CARTESIAN_POINT('',(8.45734623443633,3.62014236410543,-14.74)) ;
#109712 = CARTESIAN_POINT('Origin',(8.5,3.95,-14.74)) ;
#109713 = CARTESIAN_POINT('',(8.5,3.89793444384266,-15.3379344438427)) ;
#109714 = CARTESIAN_POINT('',(8.5,3.89793444384266,-15.1420655561573)) ;
#109715 = CARTESIAN_POINT('',(8.5,3.89793444384266,-14.74)) ;
#109716 = CARTESIAN_POINT('',(8.5,3.70206555615734,-15.1420655561573)) ;
#109717 = CARTESIAN_POINT('',(8.5,3.95,-15.1420655561573)) ;
#109718 = CARTESIAN_POINT('',(8.5,3.70206555615734,-15.3379344438427)) ;
#109719 = CARTESIAN_POINT('',(8.5,3.70206555615734,-14.74)) ;
#109720 = CARTESIAN_POINT('',(8.5,3.95,-15.3379344438427)) ;
#109721 = CARTESIAN_POINT('Origin',(8.,4.3,-14.74)) ;
#109722 = CARTESIAN_POINT('',(8.45734623443633,3.97985763589457,-15.3379344438427)) ;
#109723 = CARTESIAN_POINT('',(8.02582401135442,4.2819231920519,-15.64)) ;
#109724 = CARTESIAN_POINT('',(8.32457260887054,4.07279917379062,-15.4308759817387)) ;
#109725 = CARTESIAN_POINT('',(8.02582401135442,4.2819231920519,-14.84)) ;
#109726 = CARTESIAN_POINT('',(8.02582401135442,4.2819231920519,-14.74)) ;
#109727 = CARTESIAN_POINT('',(8.45734623443633,3.97985763589457,-15.1420655561573)) ;
#109728 = CARTESIAN_POINT('',(7.97103725533518,4.32027392126537,-14.8016492707865)) ;
#109729 = CARTESIAN_POINT('',(8.45734623443633,3.97985763589457,-14.74)) ;
#109730 = CARTESIAN_POINT('Origin',(1.5,2.3,-14.74)) ;
#109731 = CARTESIAN_POINT('',(7.96847777691809,3.4,-14.74)) ;
#109732 = CARTESIAN_POINT('',(8.,3.4,-14.74)) ;
#109733 = CARTESIAN_POINT('',(7.96847777691809,4.2,-14.74)) ;
#109734 = CARTESIAN_POINT('',(7.96847777691809,4.2,-14.74)) ;
#109735 = CARTESIAN_POINT('',(3.,4.2,-14.74)) ;
#109736 = CARTESIAN_POINT('Origin',(1.5,2.3,-15.74)) ;
#109737 = CARTESIAN_POINT('',(7.96847777691809,4.2,-15.74)) ;
#109738 = CARTESIAN_POINT('',(1.5,4.2,-15.74)) ;
#109739 = CARTESIAN_POINT('',(7.96847777691809,3.4,-15.74)) ;
#109740 = CARTESIAN_POINT('',(7.96847777691809,2.3,-15.74)) ;
#109741 = CARTESIAN_POINT('',(1.5,3.4,-15.74)) ;
#109742 = CARTESIAN_POINT('Origin',(8.,3.3,-14.74)) ;
#109743 = CARTESIAN_POINT('',(7.96847777691809,3.3,-15.64)) ;
#109744 = CARTESIAN_POINT('',(8.,3.3,-15.64)) ;
#109745 = CARTESIAN_POINT('',(7.96847777691809,3.3,-14.84)) ;
#109746 = CARTESIAN_POINT('',(7.96847777691809,3.3,-14.74)) ;
#109747 = CARTESIAN_POINT('',(3.,3.3,-14.84)) ;
#109748 = CARTESIAN_POINT('Origin',(1.5,4.3,-14.74)) ;
#109749 = CARTESIAN_POINT('',(7.96847777691809,4.3,-14.84)) ;
#109750 = CARTESIAN_POINT('',(8.,4.3,-14.84)) ;
#109751 = CARTESIAN_POINT('',(7.96847777691809,4.3,-15.64)) ;
#109752 = CARTESIAN_POINT('',(7.96847777691809,4.3,-14.74)) ;
#109753 = CARTESIAN_POINT('',(1.5,4.3,-15.64)) ;
#109754 = CARTESIAN_POINT('Origin',(1.5,2.3,-14.74)) ;
#109755 = CARTESIAN_POINT('',(-0.4,2.3,-14.74)) ;
#109756 = CARTESIAN_POINT('',(-0.4,-3.36847777691809,-14.74)) ;
#109757 = CARTESIAN_POINT('',(-0.4,-3.4,-14.74)) ;
#109758 = CARTESIAN_POINT('',(0.4,-3.36847777691809,-14.74)) ;
#109759 = CARTESIAN_POINT('',(0.4,-3.36847777691809,-14.74)) ;
#109760 = CARTESIAN_POINT('',(0.4,2.29999999999999,-14.74)) ;
#109761 = CARTESIAN_POINT('',(0.4,2.29999999999999,-14.74)) ;
#109762 = CARTESIAN_POINT('',(0.536602540378444,2.83090991212703,-14.74)) ;
#109763 = CARTESIAN_POINT('Origin',(1.5,2.3,-14.74)) ;
#109764 = CARTESIAN_POINT('',(0.536602540378444,3.93764017256378,-14.74)) ;
#109765 = CARTESIAN_POINT('',(0.536602540378444,2.83090991212703,-14.74)) ;
#109766 = CARTESIAN_POINT('Origin',(1.5,2.3,-14.74)) ;
#109767 = CARTESIAN_POINT('Origin',(1.5,2.3,-15.74)) ;
#109768 = CARTESIAN_POINT('',(0.4,2.29999999999999,-15.74)) ;
#109769 = CARTESIAN_POINT('',(0.4,-3.36847777691809,-15.74)) ;
#109770 = CARTESIAN_POINT('',(0.4,2.3,-15.74)) ;
#109771 = CARTESIAN_POINT('',(-0.4,-3.36847777691809,-15.74)) ;
#109772 = CARTESIAN_POINT('',(1.5,-3.36847777691809,-15.74)) ;
#109773 = CARTESIAN_POINT('',(-0.4,2.3,-15.74)) ;
#109774 = CARTESIAN_POINT('',(-0.4,2.3,-15.74)) ;
#109775 = CARTESIAN_POINT('',(0.536602540378444,3.93764017256378,-15.74)) ;
#109776 = CARTESIAN_POINT('Origin',(1.5,2.3,-15.74)) ;
#109777 = CARTESIAN_POINT('',(0.536602540378444,2.83090991212703,-15.74)) ;
#109778 = CARTESIAN_POINT('',(0.536602540378444,3.93764017256378,-15.74)) ;
#109779 = CARTESIAN_POINT('Origin',(1.5,2.3,-15.74)) ;
#109780 = CARTESIAN_POINT('Origin',(1.5,2.3,-14.74)) ;
#109781 = CARTESIAN_POINT('',(-0.5,2.3,-14.84)) ;
#109782 = CARTESIAN_POINT('',(-0.5,2.3,-15.64)) ;
#109783 = CARTESIAN_POINT('',(-0.5,2.3,-14.74)) ;
#109784 = CARTESIAN_POINT('Origin',(1.5,2.3,-14.84)) ;
#109785 = CARTESIAN_POINT('Origin',(1.5,2.3,-15.64)) ;
#109786 = CARTESIAN_POINT('Origin',(-0.5,-3.4,-14.74)) ;
#109787 = CARTESIAN_POINT('',(-0.5,-3.36847777691809,-15.64)) ;
#109788 = CARTESIAN_POINT('',(-0.5,-3.4,-15.64)) ;
#109789 = CARTESIAN_POINT('',(-0.5,-3.36847777691809,-14.84)) ;
#109790 = CARTESIAN_POINT('',(-0.5,-3.36847777691809,-14.74)) ;
#109791 = CARTESIAN_POINT('',(-0.5,2.3,-14.84)) ;
#109792 = CARTESIAN_POINT('Origin',(-0.15,-3.9,-14.74)) ;
#109793 = CARTESIAN_POINT('',(-0.179857635894567,-3.85734623443633,-15.1420655561573)) ;
#109794 = CARTESIAN_POINT('',(-0.481923192051905,-3.42582401135442,-14.84)) ;
#109795 = CARTESIAN_POINT('',(-0.256890082881532,-3.74729988159781,-15.0650331091704)) ;
#109796 = CARTESIAN_POINT('',(-0.481923192051905,-3.42582401135442,-15.64)) ;
#109797 = CARTESIAN_POINT('',(-0.481923192051905,-3.42582401135442,-14.74)) ;
#109798 = CARTESIAN_POINT('',(-0.179857635894567,-3.85734623443633,-15.3379344438427)) ;
#109799 = CARTESIAN_POINT('',(-0.00941533540678435,-4.10083523513317,-15.1674921433549)) ;
#109800 = CARTESIAN_POINT('',(-0.179857635894567,-3.85734623443633,-14.74)) ;
#109801 = CARTESIAN_POINT('Origin',(0.15,-3.9,-14.74)) ;
#109802 = CARTESIAN_POINT('',(0.0979344438426627,-3.9,-15.3379344438427)) ;
#109803 = CARTESIAN_POINT('',(0.0979344438426627,-3.9,-15.1420655561573)) ;
#109804 = CARTESIAN_POINT('',(0.0979344438426627,-3.9,-14.74)) ;
#109805 = CARTESIAN_POINT('',(-0.0979344438426628,-3.9,-15.1420655561573)) ;
#109806 = CARTESIAN_POINT('',(0.15,-3.9,-15.1420655561573)) ;
#109807 = CARTESIAN_POINT('',(-0.0979344438426628,-3.9,-15.3379344438427)) ;
#109808 = CARTESIAN_POINT('',(-0.0979344438426628,-3.9,-14.74)) ;
#109809 = CARTESIAN_POINT('',(0.15,-3.9,-15.3379344438427)) ;
#109810 = CARTESIAN_POINT('Origin',(0.5,-3.4,-14.74)) ;
#109811 = CARTESIAN_POINT('',(0.179857635894567,-3.85734623443633,-15.3379344438427)) ;
#109812 = CARTESIAN_POINT('',(0.481923192051904,-3.42582401135442,-15.64)) ;
#109813 = CARTESIAN_POINT('',(0.272799173790623,-3.72457260887054,-15.4308759817387)) ;
#109814 = CARTESIAN_POINT('',(0.481923192051904,-3.42582401135442,-14.84)) ;
#109815 = CARTESIAN_POINT('',(0.481923192051904,-3.42582401135442,-14.74)) ;
#109816 = CARTESIAN_POINT('',(0.179857635894567,-3.85734623443633,-15.1420655561573)) ;
#109817 = CARTESIAN_POINT('',(0.520273921265371,-3.37103725533519,-14.8016492707865)) ;
#109818 = CARTESIAN_POINT('',(0.179857635894567,-3.85734623443633,-14.74)) ;
#109819 = CARTESIAN_POINT('Origin',(0.5,2.29999999999999,-14.74)) ;
#109820 = CARTESIAN_POINT('',(0.500000000000001,2.29999999999999,-14.84)) ;
#109821 = CARTESIAN_POINT('',(0.5,-3.36847777691809,-14.84)) ;
#109822 = CARTESIAN_POINT('',(0.5,-3.4,-14.84)) ;
#109823 = CARTESIAN_POINT('',(0.5,-3.36847777691809,-15.64)) ;
#109824 = CARTESIAN_POINT('',(0.5,-3.36847777691809,-14.74)) ;
#109825 = CARTESIAN_POINT('',(0.500000000000001,2.29999999999999,-15.64)) ;
#109826 = CARTESIAN_POINT('',(0.5,2.29999999999999,-15.64)) ;
#109827 = CARTESIAN_POINT('',(0.500000000000001,2.29999999999999,-14.74)) ;
#109828 = CARTESIAN_POINT('Origin',(1.5,2.3,-14.74)) ;
#109829 = CARTESIAN_POINT('Origin',(1.5,2.3,-14.84)) ;
#109830 = CARTESIAN_POINT('Origin',(1.5,2.3,-15.64)) ;
#109831 = CARTESIAN_POINT('Origin',(8.,2.68967221921331,-15.74)) ;
#109832 = CARTESIAN_POINT('',(8.45734623443633,3.70206555615734,-15.4198576358946)) ;
#109833 = CARTESIAN_POINT('',(8.02582401135442,3.4,-15.7219231920519)) ;
#109834 = CARTESIAN_POINT('',(7.75526480758232,3.21060855735952,-15.9113146346924)) ;
#109835 = CARTESIAN_POINT('',(8.02582401135442,4.2,-15.7219231920519)) ;
#109836 = CARTESIAN_POINT('',(8.02582401135442,2.68967221921331,-15.7219231920519)) ;
#109837 = CARTESIAN_POINT('',(8.45734623443633,3.89793444384266,-15.4198576358946)) ;
#109838 = CARTESIAN_POINT('',(8.54034505662341,3.83983526831171,-15.3617584603636)) ;
#109839 = CARTESIAN_POINT('',(8.45734623443633,2.68967221921331,-15.4198576358946)) ;
#109840 = CARTESIAN_POINT('Origin',(8.,2.68967221921331,-14.74)) ;
#109841 = CARTESIAN_POINT('',(8.45734623443633,3.89793444384266,-15.0601423641054)) ;
#109842 = CARTESIAN_POINT('',(8.02582401135442,4.2,-14.7580768079481)) ;
#109843 = CARTESIAN_POINT('',(8.54034505662341,3.83983526831171,-15.1182415396364)) ;
#109844 = CARTESIAN_POINT('',(8.02582401135442,3.4,-14.7580768079481)) ;
#109845 = CARTESIAN_POINT('',(8.02582401135442,3.4,-14.7580768079481)) ;
#109846 = CARTESIAN_POINT('',(8.45734623443633,3.70206555615734,-15.0601423641054)) ;
#109847 = CARTESIAN_POINT('',(7.75526480758232,3.21060855735952,-14.5686853653076)) ;
#109848 = CARTESIAN_POINT('',(8.45734623443633,2.68967221921331,-15.0601423641054)) ;
#109849 = CARTESIAN_POINT('Origin',(-1.11032778078669,-3.9,-15.09)) ;
#109850 = CARTESIAN_POINT('',(0.0979344438426626,-3.85734623443633,-15.0601423641054)) ;
#109851 = CARTESIAN_POINT('',(0.4,-3.42582401135442,-14.7580768079481)) ;
#109852 = CARTESIAN_POINT('',(-0.223548570072128,-4.31660768288603,-15.3816253780202)) ;
#109853 = CARTESIAN_POINT('',(-0.400000000000001,-3.42582401135442,-14.7580768079481)) ;
#109854 = CARTESIAN_POINT('',(-0.400000000000001,-3.42582401135442,-14.7580768079481)) ;
#109855 = CARTESIAN_POINT('',(-0.0979344438426627,-3.85734623443633,-15.0601423641054)) ;
#109856 = CARTESIAN_POINT('',(-0.326007604256636,-3.53152743384494,-14.8320692036915)) ;
#109857 = CARTESIAN_POINT('',(-1.11032778078669,-3.85734623443633,-15.0601423641054)) ;
#109858 = CARTESIAN_POINT('Origin',(-1.11032778078669,-3.4,-15.74)) ;
#109859 = CARTESIAN_POINT('',(-0.0979344438426627,-3.85734623443633,-15.4198576358946)) ;
#109860 = CARTESIAN_POINT('',(-0.4,-3.42582401135442,-15.7219231920519)) ;
#109861 = CARTESIAN_POINT('',(-0.589391442640475,-3.15526480758232,-15.9113146346924)) ;
#109862 = CARTESIAN_POINT('',(0.400000000000001,-3.42582401135442,-15.7219231920519)) ;
#109863 = CARTESIAN_POINT('',(-1.11032778078669,-3.42582401135442,-15.7219231920519)) ;
#109864 = CARTESIAN_POINT('',(0.0979344438426626,-3.85734623443633,-15.4198576358946)) ;
#109865 = CARTESIAN_POINT('',(0.0398352683117103,-3.94034505662341,-15.3617584603636)) ;
#109866 = CARTESIAN_POINT('',(-1.11032778078669,-3.85734623443633,-15.4198576358946)) ;
#109867 = CARTESIAN_POINT('Origin',(10.,1.24999999999998,-17.78)) ;
#109868 = CARTESIAN_POINT('',(9.91643989873054,1.26392668354489,-13.1958381198218)) ;
#109869 = CARTESIAN_POINT('',(9.91643989873054,1.26392668354489,-17.78)) ;
#109870 = CARTESIAN_POINT('',(8.50816364570057,1.49863939238321,-13.2778583129651)) ;
#109871 = CARTESIAN_POINT('Origin',(43.7052916800694,-4.36754861267736,-621.928202370209)) ;
#109872 = CARTESIAN_POINT('',(8.50816364570057,1.49863939238321,-17.78)) ;
#109873 = CARTESIAN_POINT('Origin',(8.49999999999985,3.8,-15.24)) ;
#109874 = CARTESIAN_POINT('',(9.91643989873053,1.24322097942674,-13.2563035641941)) ;
#109875 = CARTESIAN_POINT('',(9.91643989873053,1.24322097942648,-17.2236964358056)) ;
#109876 = CARTESIAN_POINT('Origin',(9.91643989873053,3.8,-15.24)) ;
#109877 = CARTESIAN_POINT('Origin',(36.548065341889,-40.3802616891523,557.037655188902)) ;
#109878 = CARTESIAN_POINT('Origin',(36.5480653700872,-40.3802615697373,-587.517655338219)) ;
#109879 = CARTESIAN_POINT('Origin',(10.,1.24999999999998,-17.78)) ;
#109880 = CARTESIAN_POINT('',(8.50816364570059,1.49863939238321,-17.2021416870347)) ;
#109881 = CARTESIAN_POINT('',(8.50816364570057,1.49863939238321,-17.78)) ;
#109882 = CARTESIAN_POINT('',(9.91643989873054,1.26392668354489,-17.2841618801782)) ;
#109883 = CARTESIAN_POINT('Origin',(43.7052917204119,-4.36754862113872,591.448203083967)) ;
#109884 = CARTESIAN_POINT('',(9.91643989873054,1.26392668354489,-17.78)) ;
#109885 = CARTESIAN_POINT('Origin',(-0.900000000000001,4.65,-15.24)) ;
#109886 = CARTESIAN_POINT('Origin',(-0.900000000000001,4.65,-13.5968323274845)) ;
#109887 = CARTESIAN_POINT('Origin',(-0.900000000000001,4.65,-13.5968323274845)) ;
#109888 = CARTESIAN_POINT('Origin',(-0.900000000000001,4.65,-13.5968323274845)) ;
#109889 = CARTESIAN_POINT('Origin',(-0.900000000000001,4.65,-13.5968323274845)) ;
#109890 = CARTESIAN_POINT('Origin',(1.15,4.45,-13.6588611699158)) ;
#109891 = CARTESIAN_POINT('Origin',(1.15,4.45,-13.5968323274845)) ;
#109892 = CARTESIAN_POINT('Origin',(-1.,4.65,-13.5968323274845)) ;
#109893 = CARTESIAN_POINT('Origin',(1.15,4.65,-13.5968323274845)) ;
#109894 = CARTESIAN_POINT('Origin',(-0.900000000000001,3.8,-15.24)) ;
#109895 = CARTESIAN_POINT('Origin',(-0.900000000000001,5.4431676725155,-14.39)) ;
#109896 = CARTESIAN_POINT('Origin',(1.15,4.65,-13.5968323274845)) ;
#109897 = CARTESIAN_POINT('Origin',(1.15,4.55810810810811,-13.7744720758646)) ;
#109898 = CARTESIAN_POINT('Origin',(-0.900000000000001,5.4431676725155,-14.39)) ;
#109899 = CARTESIAN_POINT('Origin',(-0.900000000000001,5.4431676725155,-14.39)) ;
#109900 = CARTESIAN_POINT('Origin',(-0.900000000000001,5.4431676725155,-14.39)) ;
#109901 = CARTESIAN_POINT('Origin',(-0.900000000000001,4.65,-15.24)) ;
#109902 = CARTESIAN_POINT('Origin',(-0.900000000000001,4.65,-16.8831676725155)) ;
#109903 = CARTESIAN_POINT('Origin',(-1.,4.65,-16.8831676725155)) ;
#109904 = CARTESIAN_POINT('Origin',(1.15,4.65,-16.8831676725155)) ;
#109905 = CARTESIAN_POINT('Origin',(-0.900000000000001,4.65,-16.8831676725155)) ;
#109906 = CARTESIAN_POINT('Origin',(1.15,4.45,-16.8211388300842)) ;
#109907 = CARTESIAN_POINT('Origin',(1.15,4.45,-16.8831676725155)) ;
#109908 = CARTESIAN_POINT('Origin',(1.15,3.8,-15.24)) ;
#109909 = CARTESIAN_POINT('Origin',(1.15,5.26552792413544,-14.4818918918919)) ;
#109910 = CARTESIAN_POINT('Origin',(-1.,5.4431676725155,-14.39)) ;
#109911 = CARTESIAN_POINT('Origin',(1.15,5.4431676725155,-14.39)) ;
#109912 = CARTESIAN_POINT('Origin',(-0.900000000000001,3.8,-14.39)) ;
#109913 = CARTESIAN_POINT('Origin',(-0.9,6.45,-14.39)) ;
#109914 = CARTESIAN_POINT('Origin',(-0.9,6.45,-15.24)) ;
#109915 = CARTESIAN_POINT('Origin',(-0.9,6.45,-14.39)) ;
#109916 = CARTESIAN_POINT('Origin',(-0.900000000000001,4.65,-16.8831676725155)) ;
#109917 = CARTESIAN_POINT('Origin',(-0.900000000000001,4.65,-16.8831676725155)) ;
#109918 = CARTESIAN_POINT('Origin',(1.15,4.65,-16.8831676725155)) ;
#109919 = CARTESIAN_POINT('Origin',(1.15,4.55810810810811,-16.7055279241354)) ;
#109920 = CARTESIAN_POINT('Origin',(1.15,5.4431676725155,-14.39)) ;
#109921 = CARTESIAN_POINT('Origin',(1.15,5.4431676725155,-14.59)) ;
#109922 = CARTESIAN_POINT('Origin',(-0.9,6.45,-14.39)) ;
#109923 = CARTESIAN_POINT('Origin',(-0.9,6.45,-14.39)) ;
#109924 = CARTESIAN_POINT('Origin',(-0.900000000000001,3.8,-15.24)) ;
#109925 = CARTESIAN_POINT('Origin',(-0.900000000000001,5.4431676725155,-16.09)) ;
#109926 = CARTESIAN_POINT('Origin',(-1.,5.4431676725155,-16.09)) ;
#109927 = CARTESIAN_POINT('Origin',(1.15,5.4431676725155,-16.09)) ;
#109928 = CARTESIAN_POINT('Origin',(-0.900000000000001,5.4431676725155,-16.09)) ;
#109929 = CARTESIAN_POINT('Origin',(1.15,3.8,-15.24)) ;
#109930 = CARTESIAN_POINT('Origin',(1.15,5.26552792413544,-15.9981081081081)) ;
#109931 = CARTESIAN_POINT('Origin',(1.15,6.55,-14.59)) ;
#109932 = CARTESIAN_POINT('Origin',(1.15,6.45,-14.59)) ;
#109933 = CARTESIAN_POINT('Origin',(1.25,6.45,-14.39)) ;
#109934 = CARTESIAN_POINT('Origin',(1.15,6.45,-14.39)) ;
#109935 = CARTESIAN_POINT('Origin',(-0.900000000000001,5.4431676725155,-16.09)) ;
#109936 = CARTESIAN_POINT('Origin',(-0.900000000000001,5.4431676725155,-16.09)) ;
#109937 = CARTESIAN_POINT('Origin',(1.15,5.4431676725155,-16.09)) ;
#109938 = CARTESIAN_POINT('Origin',(1.15,5.4431676725155,-15.89)) ;
#109939 = CARTESIAN_POINT('Origin',(1.15,6.45,-14.59)) ;
#109940 = CARTESIAN_POINT('Origin',(1.35,6.45,-14.59)) ;
#109941 = CARTESIAN_POINT('Origin',(-0.9,6.45,-15.24)) ;
#109942 = CARTESIAN_POINT('Origin',(-0.9,6.45,-16.09)) ;
#109943 = CARTESIAN_POINT('Origin',(-0.900000000000001,3.8,-16.09)) ;
#109944 = CARTESIAN_POINT('Origin',(-0.9,6.45,-16.09)) ;
#109945 = CARTESIAN_POINT('Origin',(1.15,6.55,-15.89)) ;
#109946 = CARTESIAN_POINT('Origin',(1.15,6.45,-15.89)) ;
#109947 = CARTESIAN_POINT('Origin',(1.35,6.45,-17.78)) ;
#109948 = CARTESIAN_POINT('Origin',(1.35,6.45,-15.89)) ;
#109949 = CARTESIAN_POINT('Origin',(-0.9,6.45,-16.09)) ;
#109950 = CARTESIAN_POINT('Origin',(-0.9,6.45,-16.09)) ;
#109951 = CARTESIAN_POINT('Origin',(1.15,6.45,-15.89)) ;
#109952 = CARTESIAN_POINT('Origin',(1.15,6.45,-16.09)) ;
#109953 = CARTESIAN_POINT('Origin',(-1.,6.45,-16.09)) ;
#109954 = CARTESIAN_POINT('Origin',(-1.7,0.3,-15.89)) ;
#109955 = CARTESIAN_POINT('Origin',(-1.7,0.3,-15.89)) ;
#109956 = CARTESIAN_POINT('Origin',(-1.7,0.3,-15.89)) ;
#109957 = CARTESIAN_POINT('Origin',(-1.7,0.3,-15.89)) ;
#109958 = CARTESIAN_POINT('Origin',(0.549999999999999,0.3,-15.89)) ;
#109959 = CARTESIAN_POINT('',(0.508578643762786,0.229289321881393,-15.8192893218813)) ;
#109960 = CARTESIAN_POINT('Ctrl Pts',(0.65,0.200000000000001,-15.89)) ;
#109961 = CARTESIAN_POINT('Ctrl Pts',(0.639834283464216,0.200000000000001,
-15.8849171417321)) ;
#109962 = CARTESIAN_POINT('Ctrl Pts',(0.629316849080668,0.200389688120421,
-15.879657683858)) ;
#109963 = CARTESIAN_POINT('Ctrl Pts',(0.606957334719987,0.202165884217636,
-15.8684679497194)) ;
#109964 = CARTESIAN_POINT('Ctrl Pts',(0.595086727401534,0.203647820493406,
-15.8625227617951)) ;
#109965 = CARTESIAN_POINT('Ctrl Pts',(0.572283837383803,0.207685608830691,
-15.8511067603976)) ;
#109966 = CARTESIAN_POINT('Ctrl Pts',(0.561337481656533,0.210178193246995,
-15.845629861311)) ;
#109967 = CARTESIAN_POINT('Ctrl Pts',(0.549549942891241,0.21354462066391,
-15.8397406960421)) ;
#109968 = CARTESIAN_POINT('Ctrl Pts',(0.548290718948854,0.213913346521105,
-15.8391116827675)) ;
#109969 = CARTESIAN_POINT('Ctrl Pts',(0.536119229733182,0.217566912232434,
-15.8330327513519)) ;
#109970 = CARTESIAN_POINT('Ctrl Pts',(0.525706917362863,0.221400308602525,
-15.8278422384292)) ;
#109971 = CARTESIAN_POINT('Ctrl Pts',(0.513545110027474,0.226871185484662,
-15.8217711869643)) ;
#109972 = CARTESIAN_POINT('Ctrl Pts',(0.511029334128474,0.228063976698571,
-15.8205146670641)) ;
#109973 = CARTESIAN_POINT('Ctrl Pts',(0.508578643762786,0.229289321881393,
-15.8192893218813)) ;
#109974 = CARTESIAN_POINT('Origin',(0.664280054284628,0.302990743358677,-15.8971421042412)) ;
#109975 = CARTESIAN_POINT('Origin',(-1.7,4.5,-15.89)) ;
#109976 = CARTESIAN_POINT('',(-1.77071067811866,4.45857864376269,-15.8192893218813)) ;
#109977 = CARTESIAN_POINT('Origin',(-1.69703459697991,4.61417009502528,-15.8970866853669)) ;
#109978 = CARTESIAN_POINT('Ctrl Pts',(-1.77071067811863,4.45857864376269,
-15.8192893218813)) ;
#109979 = CARTESIAN_POINT('Ctrl Pts',(-1.77521675558369,4.46759079869274,
-15.8237953993464)) ;
#109980 = CARTESIAN_POINT('Ctrl Pts',(-1.77928079264421,4.47748625817285,
-15.8287264816716)) ;
#109981 = CARTESIAN_POINT('Ctrl Pts',(-1.78624680748596,4.49811277056786,
-15.8390208825473)) ;
#109982 = CARTESIAN_POINT('Ctrl Pts',(-1.78918030781743,4.50880509433296,
-15.8443639841482)) ;
#109983 = CARTESIAN_POINT('Ctrl Pts',(-1.79185985500253,4.52101859321847,
-15.8504747545319)) ;
#109984 = CARTESIAN_POINT('Ctrl Pts',(-1.79213045061208,4.52228751722605,
-15.8511097099085)) ;
#109985 = CARTESIAN_POINT('Ctrl Pts',(-1.7947746790983,4.53504937002851,-15.8574962891339)) ;
#109986 = CARTESIAN_POINT('Ctrl Pts',(-1.79657370273652,4.54677936428193,
-15.8633715724062)) ;
#109987 = CARTESIAN_POINT('Ctrl Pts',(-1.79896007643135,4.56920025888384,
-15.8745957747611)) ;
#109988 = CARTESIAN_POINT('Ctrl Pts',(-1.79963010255187,4.57990192168146,
-15.8799500759449)) ;
#109989 = CARTESIAN_POINT('Ctrl Pts',(-1.79996164986962,4.59357116034291,
-15.886785573817)) ;
#109990 = CARTESIAN_POINT('Ctrl Pts',(-1.8,4.59680282631912,-15.8884014131596)) ;
#109991 = CARTESIAN_POINT('Ctrl Pts',(-1.8,4.6,-15.89)) ;
#109992 = CARTESIAN_POINT('Origin',(-1.7,0.3,-15.24)) ;
#109993 = CARTESIAN_POINT('Origin',(-1.7,0.3,-16.64)) ;
#109994 = CARTESIAN_POINT('Origin',(0.65,0.3,-15.24)) ;
#109995 = CARTESIAN_POINT('',(0.579289321881345,0.229289321881345,-15.7485786437627)) ;
#109996 = CARTESIAN_POINT('Origin',(0.65708668537483,0.30296540302241,-15.9041700950407)) ;
#109997 = CARTESIAN_POINT('Ctrl Pts',(0.579289321881345,0.229289321881345,
-15.7485786437627)) ;
#109998 = CARTESIAN_POINT('Ctrl Pts',(0.583795399346368,0.224783244416322,
-15.7575907986927)) ;
#109999 = CARTESIAN_POINT('Ctrl Pts',(0.588726481671644,0.220719207355776,
-15.7674862581729)) ;
#110000 = CARTESIAN_POINT('Ctrl Pts',(0.599020882547771,0.213753192513755,
-15.7881127705687)) ;
#110001 = CARTESIAN_POINT('Ctrl Pts',(0.604363984149059,0.210819692182103,
-15.7988050943346)) ;
#110002 = CARTESIAN_POINT('Ctrl Pts',(0.610474754532788,0.2081401449971,-15.8110185932201)) ;
#110003 = CARTESIAN_POINT('Ctrl Pts',(0.611109709908931,0.207869549387732,
-15.8122875172269)) ;
#110004 = CARTESIAN_POINT('Ctrl Pts',(0.617496289133965,0.205225320901699,
-15.8250493700286)) ;
#110005 = CARTESIAN_POINT('Ctrl Pts',(0.623371572406214,0.203426297263465,
-15.836779364282)) ;
#110006 = CARTESIAN_POINT('Ctrl Pts',(0.634595774761229,0.201039923568636,
-15.859200258884)) ;
#110007 = CARTESIAN_POINT('Ctrl Pts',(0.639950075945052,0.200369897448118,
-15.8699019216816)) ;
#110008 = CARTESIAN_POINT('Ctrl Pts',(0.646785573817061,0.200038350130375,
-15.883571160343)) ;
#110009 = CARTESIAN_POINT('Ctrl Pts',(0.64840141315959,0.2,-15.8868028263192)) ;
#110010 = CARTESIAN_POINT('Ctrl Pts',(0.65,0.2,-15.89)) ;
#110011 = CARTESIAN_POINT('',(0.579289321881328,0.229289321881363,-14.7314213562373)) ;
#110012 = CARTESIAN_POINT('Ctrl Pts',(0.65,0.2,-14.59)) ;
#110013 = CARTESIAN_POINT('Ctrl Pts',(0.644917141732081,0.2,-14.6001657165358)) ;
#110014 = CARTESIAN_POINT('Ctrl Pts',(0.639657683858012,0.200389688120423,
-14.6106831509194)) ;
#110015 = CARTESIAN_POINT('Ctrl Pts',(0.628467949719366,0.202165884217642,
-14.6330426652802)) ;
#110016 = CARTESIAN_POINT('Ctrl Pts',(0.622522761794963,0.203647820493433,
-14.6449132725987)) ;
#110017 = CARTESIAN_POINT('Ctrl Pts',(0.611106760396033,0.207685608831249,
-14.6677161626194)) ;
#110018 = CARTESIAN_POINT('Ctrl Pts',(0.605629861308049,0.210178193248326,
-14.6786625183495)) ;
#110019 = CARTESIAN_POINT('Ctrl Pts',(0.599740696039329,0.213544620665554,
-14.6904500571145)) ;
#110020 = CARTESIAN_POINT('Ctrl Pts',(0.599111682766062,0.213913346521981,
-14.6917092810542)) ;
#110021 = CARTESIAN_POINT('Ctrl Pts',(0.593032751351783,0.217566912232526,
-14.7038807702672)) ;
#110022 = CARTESIAN_POINT('Ctrl Pts',(0.587842238429121,0.221400308602596,
-14.7142930826375)) ;
#110023 = CARTESIAN_POINT('Ctrl Pts',(0.581771186964291,0.226871185484691,
-14.7264548899728)) ;
#110024 = CARTESIAN_POINT('Ctrl Pts',(0.58051466706413,0.22806397669856,-14.7289706658717)) ;
#110025 = CARTESIAN_POINT('Ctrl Pts',(0.579289321881328,0.229289321881363,
-14.7314213562373)) ;
#110026 = CARTESIAN_POINT('Origin',(0.657142104261918,0.302990743367277,-14.5757199456745)) ;
#110027 = CARTESIAN_POINT('Origin',(-1.7,4.6,-15.79)) ;
#110028 = CARTESIAN_POINT('',(-1.77071067811866,4.52928932188135,-15.7485786437627)) ;
#110029 = CARTESIAN_POINT('Ctrl Pts',(-1.8,4.6,-15.89)) ;
#110030 = CARTESIAN_POINT('Ctrl Pts',(-1.8,4.5949171417321,-15.8798342834642)) ;
#110031 = CARTESIAN_POINT('Ctrl Pts',(-1.79961031187958,4.58965768385803,
-15.8693168490805)) ;
#110032 = CARTESIAN_POINT('Ctrl Pts',(-1.79783411578236,4.57846794971939,
-15.8469573347197)) ;
#110033 = CARTESIAN_POINT('Ctrl Pts',(-1.79635217950657,4.57252276179498,
-15.8350867274011)) ;
#110034 = CARTESIAN_POINT('Ctrl Pts',(-1.79231439116877,4.5611067603961,-15.8122838373806)) ;
#110035 = CARTESIAN_POINT('Ctrl Pts',(-1.78982180675173,4.55562986130817,
-15.8013374816506)) ;
#110036 = CARTESIAN_POINT('Ctrl Pts',(-1.78645537933451,4.54974069603944,
-15.7895499428856)) ;
#110037 = CARTESIAN_POINT('Ctrl Pts',(-1.78608665347804,4.5491116827661,-15.7882907189457)) ;
#110038 = CARTESIAN_POINT('Ctrl Pts',(-1.78243308776746,4.54303275135176,
-15.7761192297327)) ;
#110039 = CARTESIAN_POINT('Ctrl Pts',(-1.7785996913974,4.53784223842911,-15.7657069173624)) ;
#110040 = CARTESIAN_POINT('Ctrl Pts',(-1.77312881451532,4.5317711869643,-15.7535451100272)) ;
#110041 = CARTESIAN_POINT('Ctrl Pts',(-1.77193602330145,4.53051466706415,
-15.7510293341283)) ;
#110042 = CARTESIAN_POINT('Ctrl Pts',(-1.77071067811866,4.52928932188135,
-15.7485786437627)) ;
#110043 = CARTESIAN_POINT('Origin',(-1.69700925664399,4.60714210423621,-15.9042800542741)) ;
#110044 = CARTESIAN_POINT('',(-1.77071067811866,4.52928932188135,-14.7314213562373)) ;
#110045 = CARTESIAN_POINT('Origin',(-1.69703459697175,4.60708668538575,-14.5758299049368)) ;
#110046 = CARTESIAN_POINT('Ctrl Pts',(-1.77071067811866,4.52928932188135,
-14.7314213562373)) ;
#110047 = CARTESIAN_POINT('Ctrl Pts',(-1.77521675558368,4.53379539934637,
-14.7224092013072)) ;
#110048 = CARTESIAN_POINT('Ctrl Pts',(-1.77928079264423,4.53872648167164,
-14.7125137418271)) ;
#110049 = CARTESIAN_POINT('Ctrl Pts',(-1.78624680748634,4.54902088254791,
-14.6918872294311)) ;
#110050 = CARTESIAN_POINT('Ctrl Pts',(-1.78918030781805,4.55436398414935,
-14.6811949056648)) ;
#110051 = CARTESIAN_POINT('Ctrl Pts',(-1.79185985500302,4.56047475453307,
-14.6689814067792)) ;
#110052 = CARTESIAN_POINT('Ctrl Pts',(-1.79213045061232,4.56110970990906,
-14.6677124827727)) ;
#110053 = CARTESIAN_POINT('Ctrl Pts',(-1.7947746790983,4.56749628913395,-14.6549506299714)) ;
#110054 = CARTESIAN_POINT('Ctrl Pts',(-1.79657370273653,4.5733715724062,-14.643220635718)) ;
#110055 = CARTESIAN_POINT('Ctrl Pts',(-1.79896007643137,4.58459577476124,
-14.620799741116)) ;
#110056 = CARTESIAN_POINT('Ctrl Pts',(-1.79963010255189,4.58995007594508,
-14.6100980783183)) ;
#110057 = CARTESIAN_POINT('Ctrl Pts',(-1.79996164986963,4.59678557381709,
-14.5964288396569)) ;
#110058 = CARTESIAN_POINT('Ctrl Pts',(-1.8,4.5984014131596,-14.5931971736808)) ;
#110059 = CARTESIAN_POINT('Ctrl Pts',(-1.8,4.6,-14.59)) ;
#110060 = CARTESIAN_POINT('Origin',(-1.7,0.3,-16.64)) ;
#110061 = CARTESIAN_POINT('Origin',(-1.7,0.1,-16.64)) ;
#110062 = CARTESIAN_POINT('Origin',(-1.9,0.3,-16.64)) ;
#110063 = CARTESIAN_POINT('Origin',(1.9668402209837E-32,0.1,-16.64)) ;
#110064 = CARTESIAN_POINT('',(0.899999999999999,0.1,-16.74)) ;
#110065 = CARTESIAN_POINT('',(-1.8,0.1,-16.74)) ;
#110066 = CARTESIAN_POINT('Origin',(0.899999999999999,0.1,-16.64)) ;
#110067 = CARTESIAN_POINT('Origin',(0.899999999999999,0.1,-16.64)) ;
#110068 = CARTESIAN_POINT('',(0.999999999999999,0.1,-16.64)) ;
#110069 = CARTESIAN_POINT('Origin',(0.899999999999999,0.1,-16.64)) ;
#110070 = CARTESIAN_POINT('Origin',(0.899999999999999,0.1,-16.64)) ;
#110071 = CARTESIAN_POINT('Origin',(0.549999999999999,0.3,-14.59)) ;
#110072 = CARTESIAN_POINT('',(0.50857864376269,0.229289321881346,-14.6607106781187)) ;
#110073 = CARTESIAN_POINT('Origin',(0.664170095063304,0.30296540302746,-14.5829133146142)) ;
#110074 = CARTESIAN_POINT('Ctrl Pts',(0.50857864376269,0.229289321881369,
-14.6607106781187)) ;
#110075 = CARTESIAN_POINT('Ctrl Pts',(0.517590798692736,0.224783244416307,
-14.6562046006536)) ;
#110076 = CARTESIAN_POINT('Ctrl Pts',(0.52748625817285,0.22071920735579,-14.6512735183284)) ;
#110077 = CARTESIAN_POINT('Ctrl Pts',(0.548112770567762,0.21375319251403,
-14.6409791174526)) ;
#110078 = CARTESIAN_POINT('Ctrl Pts',(0.558805094332743,0.210819692182585,
-14.6356360158518)) ;
#110079 = CARTESIAN_POINT('Ctrl Pts',(0.571018593218257,0.208140144997491,
-14.6295252454681)) ;
#110080 = CARTESIAN_POINT('Ctrl Pts',(0.572287517225956,0.207869549387918,
-14.6288902900915)) ;
#110081 = CARTESIAN_POINT('Ctrl Pts',(0.585049370028551,0.205225320901704,
-14.622503710866)) ;
#110082 = CARTESIAN_POINT('Ctrl Pts',(0.596779364281985,0.20342629726345,
-14.6166284275937)) ;
#110083 = CARTESIAN_POINT('Ctrl Pts',(0.619200258883932,0.201039923568639,
-14.6054042252388)) ;
#110084 = CARTESIAN_POINT('Ctrl Pts',(0.629901921681571,0.200369897448121,
-14.600049924055)) ;
#110085 = CARTESIAN_POINT('Ctrl Pts',(0.643571160343008,0.200038350130376,
-14.593214426183)) ;
#110086 = CARTESIAN_POINT('Ctrl Pts',(0.646802826319167,0.200000000000001,
-14.5915985868404)) ;
#110087 = CARTESIAN_POINT('Ctrl Pts',(0.65,0.200000000000001,-14.59)) ;
#110088 = CARTESIAN_POINT('Origin',(-1.7,0.3,-14.59)) ;
#110089 = CARTESIAN_POINT('Origin',(-1.7,4.5,-14.59)) ;
#110090 = CARTESIAN_POINT('',(-1.77071067811864,4.45857864376273,-14.6607106781187)) ;
#110091 = CARTESIAN_POINT('Ctrl Pts',(-1.8,4.6,-14.59)) ;
#110092 = CARTESIAN_POINT('Ctrl Pts',(-1.8,4.58983428346416,-14.5950828582679)) ;
#110093 = CARTESIAN_POINT('Ctrl Pts',(-1.79961031187958,4.57931684908054,
-14.600342316142)) ;
#110094 = CARTESIAN_POINT('Ctrl Pts',(-1.79783411578235,4.5569573347197,-14.6115320502807)) ;
#110095 = CARTESIAN_POINT('Ctrl Pts',(-1.79635217950654,4.54508672740115,
-14.6174772382051)) ;
#110096 = CARTESIAN_POINT('Ctrl Pts',(-1.79231439116922,4.52228383738327,
-14.6288932396026)) ;
#110097 = CARTESIAN_POINT('Ctrl Pts',(-1.7898218067529,4.51133748165596,-14.6343701386892)) ;
#110098 = CARTESIAN_POINT('Ctrl Pts',(-1.78645537933596,4.49954994289065,
-14.6402593039581)) ;
#110099 = CARTESIAN_POINT('Ctrl Pts',(-1.78608665347877,4.49829071894828,
-14.6408883172327)) ;
#110100 = CARTESIAN_POINT('Ctrl Pts',(-1.78243308776744,4.48611922973267,
-14.6469672486483)) ;
#110101 = CARTESIAN_POINT('Ctrl Pts',(-1.77859969139738,4.4757069173624,-14.6521577615709)) ;
#110102 = CARTESIAN_POINT('Ctrl Pts',(-1.7731288145153,4.46354511002718,-14.6582288130357)) ;
#110103 = CARTESIAN_POINT('Ctrl Pts',(-1.77193602330142,4.4610293341283,-14.6594853329359)) ;
#110104 = CARTESIAN_POINT('Ctrl Pts',(-1.77071067811862,4.45857864376273,
-14.6607106781187)) ;
#110105 = CARTESIAN_POINT('Origin',(-1.69700925663777,4.6142800543045,-14.5828578957488)) ;
#110106 = CARTESIAN_POINT('Origin',(-1.7,0.3,-14.59)) ;
#110107 = CARTESIAN_POINT('Origin',(-1.9,-4.11004745125224E-16,-16.64)) ;
#110108 = CARTESIAN_POINT('',(-1.9,6.9,-16.74)) ;
#110109 = CARTESIAN_POINT('Origin',(-1.9,6.9,-16.64)) ;
#110110 = CARTESIAN_POINT('',(-1.9,7.,-16.74)) ;
#110111 = CARTESIAN_POINT('Origin',(-2.,0.1,-16.84)) ;
#110112 = CARTESIAN_POINT('Origin',(-1.89999999999978,0.100000000000219,-16.8400000000002)) ;
#110113 = CARTESIAN_POINT('Origin',(0.899999999999999,0.1,-16.84)) ;
#110114 = CARTESIAN_POINT('Origin',(0.899999999999999,0.1,-16.64)) ;
#110115 = CARTESIAN_POINT('Origin',(1.1,0.1,-16.64)) ;
#110116 = CARTESIAN_POINT('Origin',(0.899999999999999,0.1,-15.24)) ;
#110117 = CARTESIAN_POINT('',(0.999999999999999,0.1,-13.84)) ;
#110118 = CARTESIAN_POINT('',(0.999999999999999,0.1,-16.74)) ;
#110119 = CARTESIAN_POINT('Origin',(0.899999999999999,0.1,-13.84)) ;
#110120 = CARTESIAN_POINT('Origin',(-1.7,0.3,-14.59)) ;
#110121 = CARTESIAN_POINT('Origin',(-1.7,0.3,-14.59)) ;
#110122 = CARTESIAN_POINT('Origin',(-1.9,6.9,-16.64)) ;
#110123 = CARTESIAN_POINT('',(-1.9,7.,-16.64)) ;
#110124 = CARTESIAN_POINT('Origin',(-1.9,6.9,-16.64)) ;
#110125 = CARTESIAN_POINT('Origin',(-1.9,6.9,-16.64)) ;
#110126 = CARTESIAN_POINT('Origin',(-1.9,7.,-16.84)) ;
#110127 = CARTESIAN_POINT('Origin',(-1.9,6.9,-16.84)) ;
#110128 = CARTESIAN_POINT('Origin',(1.1,0.1,-13.74)) ;
#110129 = CARTESIAN_POINT('Origin',(1.1,0.1,-13.84)) ;
#110130 = CARTESIAN_POINT('Origin',(0.899999999999999,0.1,-13.84)) ;
#110131 = CARTESIAN_POINT('',(0.899999999999999,0.1,-13.74)) ;
#110132 = CARTESIAN_POINT('Origin',(0.899999999999999,0.1,-13.84)) ;
#110133 = CARTESIAN_POINT('Origin',(0.899999999999999,0.1,-13.84)) ;
#110134 = CARTESIAN_POINT('Origin',(-1.7,0.3,-15.24)) ;
#110135 = CARTESIAN_POINT('Origin',(-1.7,0.3,-13.84)) ;
#110136 = CARTESIAN_POINT('Origin',(-1.9,6.9,-15.24)) ;
#110137 = CARTESIAN_POINT('',(-1.9,7.,-13.84)) ;
#110138 = CARTESIAN_POINT('Origin',(-1.9,6.9,-13.84)) ;
#110139 = CARTESIAN_POINT('',(-1.9,7.,-16.74)) ;
#110140 = CARTESIAN_POINT('Origin',(-1.9,6.9,-16.64)) ;
#110141 = CARTESIAN_POINT('Origin',(-1.9,7.1,-16.64)) ;
#110142 = CARTESIAN_POINT('Origin',(0.899999999999999,0.1,-13.84)) ;
#110143 = CARTESIAN_POINT('Origin',(0.899999999999999,0.1,-13.64)) ;
#110144 = CARTESIAN_POINT('Origin',(-1.9668402209837E-32,0.1,-13.84)) ;
#110145 = CARTESIAN_POINT('',(0.999999999999999,0.1,-13.74)) ;
#110146 = CARTESIAN_POINT('Origin',(-1.7,0.1,-13.84)) ;
#110147 = CARTESIAN_POINT('Origin',(-1.7,0.3,-13.84)) ;
#110148 = CARTESIAN_POINT('Origin',(-1.9,0.3,-13.84)) ;
#110149 = CARTESIAN_POINT('Origin',(-1.9,6.9,-13.84)) ;
#110150 = CARTESIAN_POINT('',(-1.9,6.9,-13.74)) ;
#110151 = CARTESIAN_POINT('Origin',(-1.9,6.9,-13.84)) ;
#110152 = CARTESIAN_POINT('Origin',(-1.9,6.9,-13.84)) ;
#110153 = CARTESIAN_POINT('Origin',(-1.9,7.1,-16.74)) ;
#110154 = CARTESIAN_POINT('Origin',(-1.9,7.1,-13.84)) ;
#110155 = CARTESIAN_POINT('Origin',(-1.8,0.1,-13.64)) ;
#110156 = CARTESIAN_POINT('Origin',(-1.90000000000006,0.0999999999999441,
-13.6400000000001)) ;
#110157 = CARTESIAN_POINT('Origin',(-1.9,-6.40600499298624E-17,-13.84)) ;
#110158 = CARTESIAN_POINT('',(-1.9,7.,-13.74)) ;
#110159 = CARTESIAN_POINT('Origin',(-1.9,6.9,-13.84)) ;
#110160 = CARTESIAN_POINT('Origin',(-1.9,6.9,-13.64)) ;
#110161 = CARTESIAN_POINT('Origin',(-1.9,7.,-13.64)) ;
#110162 = CARTESIAN_POINT('Origin',(-0.900000000000002,2.95,-15.24)) ;
#110163 = CARTESIAN_POINT('Origin',(-0.900000000000001,2.95,-16.8831676725155)) ;
#110164 = CARTESIAN_POINT('Origin',(-0.900000000000002,2.95,-16.8831676725155)) ;
#110165 = CARTESIAN_POINT('Origin',(-0.900000000000001,2.95,-16.8831676725155)) ;
#110166 = CARTESIAN_POINT('Origin',(-0.900000000000002,2.95,-16.8831676725155)) ;
#110167 = CARTESIAN_POINT('Origin',(1.15,3.15,-17.79)) ;
#110168 = CARTESIAN_POINT('Origin',(1.15,3.15,-16.8831676725155)) ;
#110169 = CARTESIAN_POINT('Origin',(-1.,2.95,-16.8831676725155)) ;
#110170 = CARTESIAN_POINT('Origin',(1.15,2.95,-16.8831676725155)) ;
#110171 = CARTESIAN_POINT('Origin',(-0.900000000000001,3.8,-15.24)) ;
#110172 = CARTESIAN_POINT('Origin',(-0.900000000000002,2.1568323274845,-16.09)) ;
#110173 = CARTESIAN_POINT('Origin',(-0.900000000000002,1.6,-15.24)) ;
#110174 = CARTESIAN_POINT('Origin',(-0.900000000000002,1.6,-17.2021416870349)) ;
#110175 = CARTESIAN_POINT('Origin',(13.9153543900904,1.4,-17.2021416870349)) ;
#110176 = CARTESIAN_POINT('Origin',(8.49172374697002,1.4,-17.2021416870349)) ;
#110177 = CARTESIAN_POINT('Origin',(-0.900000000000001,1.40000000000001,-17.2021416870349)) ;
#110178 = CARTESIAN_POINT('Origin',(1.15,2.95,-16.8831676725155)) ;
#110179 = CARTESIAN_POINT('Origin',(1.15,3.04189189189189,-16.7055279241354)) ;
#110180 = CARTESIAN_POINT('Origin',(-0.900000000000002,2.1568323274845,-16.09)) ;
#110181 = CARTESIAN_POINT('Origin',(-0.900000000000002,2.1568323274845,-16.09)) ;
#110182 = CARTESIAN_POINT('Origin',(-0.900000000000002,2.1568323274845,-16.09)) ;
#110183 = CARTESIAN_POINT('Origin',(-0.900000000000001,1.40000000000001,-17.2021416870349)) ;
#110184 = CARTESIAN_POINT('Origin',(-0.900000000000002,1.55483870967742,-17.0755519007745)) ;
#110185 = CARTESIAN_POINT('Origin',(1.15,3.8,-15.24)) ;
#110186 = CARTESIAN_POINT('Origin',(1.15,2.33447207586456,-15.9981081081081)) ;
#110187 = CARTESIAN_POINT('Origin',(-1.,2.1568323274845,-16.09)) ;
#110188 = CARTESIAN_POINT('Origin',(1.15,2.1568323274845,-16.09)) ;
#110189 = CARTESIAN_POINT('Origin',(-0.900000000000001,3.8,-16.09)) ;
#110190 = CARTESIAN_POINT('Origin',(-0.900000000000002,1.02736587339765,-16.09)) ;
#110191 = CARTESIAN_POINT('Origin',(-0.900000000000001,3.8,-15.24)) ;
#110192 = CARTESIAN_POINT('Origin',(-0.900000000000002,1.02736587339765,-16.09)) ;
#110193 = CARTESIAN_POINT('Origin',(13.9153543900904,1.4,-13.2778583129651)) ;
#110194 = CARTESIAN_POINT('Origin',(8.49172374697002,1.4,-13.2778583129651)) ;
#110195 = CARTESIAN_POINT('Origin',(-0.900000000000001,1.40000000000001,-13.2778583129651)) ;
#110196 = CARTESIAN_POINT('Origin',(-0.900000000000002,1.6,-15.24)) ;
#110197 = CARTESIAN_POINT('Origin',(-0.900000000000002,1.6,-13.2778583129651)) ;
#110198 = CARTESIAN_POINT('Origin',(-0.900000000000002,2.95,-15.24)) ;
#110199 = CARTESIAN_POINT('Origin',(-0.900000000000002,2.95,-13.5968323274845)) ;
#110200 = CARTESIAN_POINT('Origin',(1.15,2.1568323274845,-16.09)) ;
#110201 = CARTESIAN_POINT('Origin',(1.15,2.1568323274845,-15.89)) ;
#110202 = CARTESIAN_POINT('Origin',(-0.900000000000002,1.02736587339765,-16.09)) ;
#110203 = CARTESIAN_POINT('Origin',(-0.900000000000001,1.40000000000001,-13.2778583129651)) ;
#110204 = CARTESIAN_POINT('Origin',(-0.900000000000002,1.55483870967743,-13.4044480992254)) ;
#110205 = CARTESIAN_POINT('Origin',(-0.900000000000002,2.95,-13.5968323274845)) ;
#110206 = CARTESIAN_POINT('Origin',(-0.900000000000002,2.95,-13.5968323274845)) ;
#110207 = CARTESIAN_POINT('Origin',(-0.900000000000001,2.95,-13.5968323274845)) ;
#110208 = CARTESIAN_POINT('Origin',(1.15,2.21886116991581,-15.89)) ;
#110209 = CARTESIAN_POINT('Ctrl Pts',(1.15,1.02736587339765,-15.99)) ;
#110210 = CARTESIAN_POINT('Ctrl Pts',(1.1608920328805,1.02736587339765,-15.99)) ;
#110211 = CARTESIAN_POINT('Ctrl Pts',(1.17195716626105,1.02622125393927,-15.988143843926)) ;
#110212 = CARTESIAN_POINT('Ctrl Pts',(1.1820844490224,1.02414637334385,-15.9847131887908)) ;
#110213 = CARTESIAN_POINT('Ctrl Pts',(1.19245005921088,1.02202266415684,-15.9812017993431)) ;
#110214 = CARTESIAN_POINT('Ctrl Pts',(1.20216743701154,1.01888103823701,-15.9759601980703)) ;
#110215 = CARTESIAN_POINT('Ctrl Pts',(1.21053792402812,1.01518120925307,-15.969593716802)) ;
#110216 = CARTESIAN_POINT('Ctrl Pts',(1.219343173684,1.01128921135341,-15.9628965608439)) ;
#110217 = CARTESIAN_POINT('Ctrl Pts',(1.22692289939014,1.00668521903338,-15.9547851615315)) ;
#110218 = CARTESIAN_POINT('Ctrl Pts',(1.23290049538659,1.00186003905466,-15.9459241259624)) ;
#110219 = CARTESIAN_POINT('Ctrl Pts',(1.23922345568944,0.9967560772818,-15.93655113117)) ;
#110220 = CARTESIAN_POINT('Ctrl Pts',(1.24392209779927,0.991279542094837,
-15.9261045599897)) ;
#110221 = CARTESIAN_POINT('Ctrl Pts',(1.24674870216524,0.985895902333124,
-15.9152920665297)) ;
#110222 = CARTESIAN_POINT('Ctrl Pts',(1.24889292215336,0.981811953364218,
-15.9070898699727)) ;
#110223 = CARTESIAN_POINT('Ctrl Pts',(1.25,0.977715885027402,-15.8985491686292)) ;
#110224 = CARTESIAN_POINT('Ctrl Pts',(1.25,0.973783447787483,-15.89)) ;
#110225 = CARTESIAN_POINT('Origin',(-0.900000000000001,3.8,-15.24)) ;
#110226 = CARTESIAN_POINT('Origin',(-0.900000000000002,1.02736587339765,-14.39)) ;
#110227 = CARTESIAN_POINT('Origin',(-0.900000000000001,3.8,-14.39)) ;
#110228 = CARTESIAN_POINT('Origin',(-0.900000000000002,2.1568323274845,-14.39)) ;
#110229 = CARTESIAN_POINT('Origin',(-0.900000000000002,1.02736587339765,-14.39)) ;
#110230 = CARTESIAN_POINT('Origin',(-0.900000000000001,3.8,-15.24)) ;
#110231 = CARTESIAN_POINT('Origin',(-0.900000000000002,2.1568323274845,-14.39)) ;
#110232 = CARTESIAN_POINT('Origin',(-1.,2.95,-13.5968323274845)) ;
#110233 = CARTESIAN_POINT('Origin',(1.15,2.95,-13.5968323274845)) ;
#110234 = CARTESIAN_POINT('Origin',(1.15,3.15,-12.69)) ;
#110235 = CARTESIAN_POINT('Origin',(1.15,3.15,-13.5968323274845)) ;
#110236 = CARTESIAN_POINT('Ctrl Pts',(1.11028558574901,0.930383836951479,
-16.1149942836582)) ;
#110237 = CARTESIAN_POINT('Ctrl Pts',(1.14039000477524,0.89213646613791,-15.989969718594)) ;
#110238 = CARTESIAN_POINT('Ctrl Pts',(1.13015013463564,1.02610337426268,-15.9878511248827)) ;
#110239 = CARTESIAN_POINT('Ctrl Pts',(1.17639690652713,0.93522510982765,-16.1301257399467)) ;
#110240 = CARTESIAN_POINT('Ctrl Pts',(1.15491086542928,0.891146666106907,
-15.9892760504014)) ;
#110241 = CARTESIAN_POINT('Ctrl Pts',(1.16319405445819,1.03078047702079,-15.9951648742452)) ;
#110242 = CARTESIAN_POINT('Ctrl Pts',(1.24701363206612,0.927145283841805,
-16.1055522038251)) ;
#110243 = CARTESIAN_POINT('Ctrl Pts',(1.17759980831447,0.893467326853923,
-15.9926373120314)) ;
#110244 = CARTESIAN_POINT('Ctrl Pts',(1.19848758201044,1.02297467453101,-15.983287122555)) ;
#110245 = CARTESIAN_POINT('Ctrl Pts',(1.33816236560056,0.900022463714239,
-16.0098088506149)) ;
#110246 = CARTESIAN_POINT('Ctrl Pts',(1.22862786282606,0.888037626604014,
-15.963153964324)) ;
#110247 = CARTESIAN_POINT('Ctrl Pts',(1.24403288504499,0.996768276947748,
-15.9370266594133)) ;
#110248 = CARTESIAN_POINT('Ctrl Pts',(1.35959492575597,0.881455895025368,
-15.938532341229)) ;
#110249 = CARTESIAN_POINT('Ctrl Pts',(1.25320519750665,0.88042809908173,-15.9310649378274)) ;
#110250 = CARTESIAN_POINT('Ctrl Pts',(1.25473603279823,0.978811277328846,
-15.9025574871508)) ;
#110251 = CARTESIAN_POINT('Ctrl Pts',(1.34615355831624,0.867571605181224,
-15.8727925825335)) ;
#110252 = CARTESIAN_POINT('Ctrl Pts',(1.2517609020281,0.870950130624643,-15.8894490170578)) ;
#110253 = CARTESIAN_POINT('Ctrl Pts',(1.24801589497573,0.965423101361847,
-15.8708695481641)) ;
#110254 = CARTESIAN_POINT('Origin',(1.35,0.973783447787483,-15.89)) ;
#110255 = CARTESIAN_POINT('Origin',(-0.900000000000002,1.02736587339765,-14.39)) ;
#110256 = CARTESIAN_POINT('',(-0.957735026918965,0.969630846478687,-14.447735026919)) ;
#110257 = CARTESIAN_POINT('Origin',(-0.900000000000002,1.02736587339765,-14.39)) ;
#110258 = CARTESIAN_POINT('Origin',(-0.900000000000002,2.1568323274845,-14.39)) ;
#110259 = CARTESIAN_POINT('Origin',(-0.900000000000002,2.1568323274845,-14.39)) ;
#110260 = CARTESIAN_POINT('Origin',(1.15,2.95,-13.5968323274845)) ;
#110261 = CARTESIAN_POINT('Origin',(1.15,3.04189189189189,-13.7744720758646)) ;
#110262 = CARTESIAN_POINT('Origin',(1.35,3.8,-15.24)) ;
#110263 = CARTESIAN_POINT('Origin',(1.35,0.973783447787484,-14.59)) ;
#110264 = CARTESIAN_POINT('Origin',(-1.,2.1568323274845,-14.39)) ;
#110265 = CARTESIAN_POINT('Origin',(1.15,2.1568323274845,-14.39)) ;
#110266 = CARTESIAN_POINT('Origin',(1.15,3.8,-15.24)) ;
#110267 = CARTESIAN_POINT('Origin',(1.15,2.33447207586456,-14.4818918918919)) ;
#110268 = CARTESIAN_POINT('Ctrl Pts',(1.34754079198594,0.869159571293157,
-14.5997485347855)) ;
#110269 = CARTESIAN_POINT('Ctrl Pts',(1.25183398383325,0.87199977042434,-14.5859986517604)) ;
#110270 = CARTESIAN_POINT('Ctrl Pts',(1.24871534599026,0.966951450593922,
-14.6055357130736)) ;
#110271 = CARTESIAN_POINT('Ctrl Pts',(1.3578897130187,0.882932151572343,-14.5357774282681)) ;
#110272 = CARTESIAN_POINT('Ctrl Pts',(1.25138796519083,0.881019151005405,
-14.5464872814236)) ;
#110273 = CARTESIAN_POINT('Ctrl Pts',(1.25389076424432,0.980237216252324,
-14.5746886342594)) ;
#110274 = CARTESIAN_POINT('Ctrl Pts',(1.33642796493171,0.90055164307479,-14.4683167189688)) ;
#110275 = CARTESIAN_POINT('Ctrl Pts',(1.22773025960896,0.888154519889406,
-14.5163023541524)) ;
#110276 = CARTESIAN_POINT('Ctrl Pts',(1.24317203399028,0.99727835245108,-14.5420644582831)) ;
#110277 = CARTESIAN_POINT('Ctrl Pts',(1.24851212064762,0.926675670999743,
-14.3761118541866)) ;
#110278 = CARTESIAN_POINT('Ctrl Pts',(1.17855408504648,0.893378082604318,
-14.4879358454001)) ;
#110279 = CARTESIAN_POINT('Ctrl Pts',(1.19923947710882,1.02252144543593,-14.4975111840607)) ;
#110280 = CARTESIAN_POINT('Ctrl Pts',(1.18212686068543,0.934567888698249,
-14.3518922599008)) ;
#110281 = CARTESIAN_POINT('Ctrl Pts',(1.15690947476175,0.891342319659322,
-14.4905013022392)) ;
#110282 = CARTESIAN_POINT('Ctrl Pts',(1.1660589236879,1.03014681530415,-14.4858041235204)) ;
#110283 = CARTESIAN_POINT('Ctrl Pts',(1.11776263740948,0.930888708579174,
-14.363423581916)) ;
#110284 = CARTESIAN_POINT('Ctrl Pts',(1.1419771056359,0.892059806626674,-14.4900822996554)) ;
#110285 = CARTESIAN_POINT('Ctrl Pts',(1.13388624958143,1.02659206201255,-14.4913778561013)) ;
#110286 = CARTESIAN_POINT('Ctrl Pts',(1.15,1.02736587339764,-14.49)) ;
#110287 = CARTESIAN_POINT('Ctrl Pts',(1.15623005440502,1.02736587339759,-14.4899999999999)) ;
#110288 = CARTESIAN_POINT('Ctrl Pts',(1.16249579431471,1.02700282517053,-14.490590866069)) ;
#110289 = CARTESIAN_POINT('Ctrl Pts',(1.16857840195431,1.02630083270769,-14.4917409394467)) ;
#110290 = CARTESIAN_POINT('Ctrl Pts',(1.1798885498395,1.02499553092934,-14.4938794137247)) ;
#110291 = CARTESIAN_POINT('Ctrl Pts',(1.19084787809767,1.02245621903271,-14.4980506966152)) ;
#110292 = CARTESIAN_POINT('Ctrl Pts',(1.20043335385463,1.01914369852331,-14.5036491064379)) ;
#110293 = CARTESIAN_POINT('Ctrl Pts',(1.21063893018497,1.01561688548223,-14.5096096868225)) ;
#110294 = CARTESIAN_POINT('Ctrl Pts',(1.21965078109605,1.01112191387731,-14.5173548511019)) ;
#110295 = CARTESIAN_POINT('Ctrl Pts',(1.226898722009,1.00626683908294,-14.5260735848543)) ;
#110296 = CARTESIAN_POINT('Ctrl Pts',(1.23435386869391,1.0012729663137,-14.5350415717366)) ;
#110297 = CARTESIAN_POINT('Ctrl Pts',(1.24017476602864,0.995763540409855,
-14.5452870264069)) ;
#110298 = CARTESIAN_POINT('Ctrl Pts',(1.24405759382605,0.990267693778535,
-14.5560416572305)) ;
#110299 = CARTESIAN_POINT('Ctrl Pts',(1.24795610732226,0.9847496452368,-14.5668397341991)) ;
#110300 = CARTESIAN_POINT('Ctrl Pts',(1.25,0.97910634898267,-14.578427945028)) ;
#110301 = CARTESIAN_POINT('Ctrl Pts',(1.25,0.973783447787483,-14.59)) ;
#110302 = CARTESIAN_POINT('Origin',(1.15,2.1568323274845,-14.39)) ;
#110303 = CARTESIAN_POINT('Origin',(1.15,2.1568323274845,-14.59)) ;
#110304 = CARTESIAN_POINT('Origin',(1.15,2.21886116991581,-14.59)) ;
#110305 = CARTESIAN_POINT('Origin',(1.5,2.3,-15.64)) ;
#110306 = CARTESIAN_POINT('Ctrl Pts',(0.549999999999999,4.04473197180487,
-15.69)) ;
#110307 = CARTESIAN_POINT('Ctrl Pts',(0.549999999999999,4.04340510574362,
-15.6920183916746)) ;
#110308 = CARTESIAN_POINT('Ctrl Pts',(0.549938912488053,4.04197482121869,
-15.6939799093558)) ;
#110309 = CARTESIAN_POINT('Ctrl Pts',(0.549362579613731,4.03414945156067,
-15.7037632016969)) ;
#110310 = CARTESIAN_POINT('Ctrl Pts',(0.548040652125111,4.02633974827563,
-15.7105458262271)) ;
#110311 = CARTESIAN_POINT('Ctrl Pts',(0.544205267183641,4.00519499286858,
-15.7246839427888)) ;
#110312 = CARTESIAN_POINT('Ctrl Pts',(0.541221332378522,3.99011995637991,
-15.7312251154481)) ;
#110313 = CARTESIAN_POINT('Ctrl Pts',(0.537814556431575,3.96385893187674,
-15.73793059224)) ;
#110314 = CARTESIAN_POINT('Ctrl Pts',(0.536602540378442,3.95132390702861,
-15.74)) ;
#110315 = CARTESIAN_POINT('Ctrl Pts',(0.536602540378442,3.93764017256378,
-15.74)) ;
#110316 = CARTESIAN_POINT('Origin',(-0.4,2.3,-15.64)) ;
#110317 = CARTESIAN_POINT('Origin',(-0.4,-3.4,-15.64)) ;
#110318 = CARTESIAN_POINT('Origin',(-0.4,-3.36847777691809,-15.64)) ;
#110319 = CARTESIAN_POINT('Origin',(1.5,2.3,-15.64)) ;
#110320 = CARTESIAN_POINT('Ctrl Pts',(0.536602540378442,2.83090991212703,
-15.74)) ;
#110321 = CARTESIAN_POINT('Ctrl Pts',(0.536602540378442,2.80627146475495,
-15.74)) ;
#110322 = CARTESIAN_POINT('Ctrl Pts',(0.538106903229178,2.77742679387655,
-15.7379527908126)) ;
#110323 = CARTESIAN_POINT('Ctrl Pts',(0.545186976568879,2.71156844363324,
-15.72208398098)) ;
#110324 = CARTESIAN_POINT('Ctrl Pts',(0.549999999999999,2.68282906082667,
-15.7081020558136)) ;
#110325 = CARTESIAN_POINT('Ctrl Pts',(0.549999999999999,2.65280931275608,
-15.69)) ;
#110326 = CARTESIAN_POINT('Origin',(0.400000000000001,2.29999999999999,-15.64)) ;
#110327 = CARTESIAN_POINT('Origin',(0.0725078566451197,-4.04348900069683,
-15.1674921433549)) ;
#110328 = CARTESIAN_POINT('Origin',(-0.4,-3.36847777691809,-15.64)) ;
#110329 = CARTESIAN_POINT('Origin',(-0.0979344438426628,-3.8,-15.3379344438427)) ;
#110330 = CARTESIAN_POINT('Origin',(1.5,2.3,-14.84)) ;
#110331 = CARTESIAN_POINT('Ctrl Pts',(0.536602540378443,3.93764017256378,
-14.74)) ;
#110332 = CARTESIAN_POINT('Ctrl Pts',(0.536602540378443,3.93925361219667,
-14.74)) ;
#110333 = CARTESIAN_POINT('Ctrl Pts',(0.536619300889436,3.94087098264022,
-14.7400289972578)) ;
#110334 = CARTESIAN_POINT('Ctrl Pts',(0.536997639747737,3.95938954612103,
-14.7406858128958)) ;
#110335 = CARTESIAN_POINT('Ctrl Pts',(0.539142315171097,3.97567120869923,
-14.7443120615617)) ;
#110336 = CARTESIAN_POINT('Ctrl Pts',(0.544035197036717,4.00535605098116,
-14.7553993916662)) ;
#110337 = CARTESIAN_POINT('Ctrl Pts',(0.546989816174457,4.01946236900627,
-14.7635699446351)) ;
#110338 = CARTESIAN_POINT('Ctrl Pts',(0.549463062495699,4.0359553600741,-14.7785473816972)) ;
#110339 = CARTESIAN_POINT('Ctrl Pts',(0.550000000000877,4.04078397701437,
-14.7839944203464)) ;
#110340 = CARTESIAN_POINT('Ctrl Pts',(0.549999999999999,4.04473197181447,
-14.7900000000146)) ;
#110341 = CARTESIAN_POINT('Origin',(-0.4,2.3,-14.84)) ;
#110342 = CARTESIAN_POINT('Origin',(0.4,2.29999999999999,-15.64)) ;
#110343 = CARTESIAN_POINT('Origin',(0.4,-3.36847777691809,-15.64)) ;
#110344 = CARTESIAN_POINT('Origin',(-0.0979344438426628,-3.8,-15.3379344438427)) ;
#110345 = CARTESIAN_POINT('Origin',(-0.0979344438426628,-3.8,-15.3379344438427)) ;
#110346 = CARTESIAN_POINT('Origin',(-0.0979344438426627,-3.8,-15.3379344438427)) ;
#110347 = CARTESIAN_POINT('Origin',(-0.4,2.3,-14.84)) ;
#110348 = CARTESIAN_POINT('Origin',(-0.4,-3.36847777691809,-14.84)) ;
#110349 = CARTESIAN_POINT('Origin',(0.190875981738719,-3.6672263744342,-15.4308759817387)) ;
#110350 = CARTESIAN_POINT('Origin',(0.400000000000001,-3.36847777691809,-15.64)) ;
#110351 = CARTESIAN_POINT('Origin',(0.0979344438426626,-3.8,-15.3379344438427)) ;
#110352 = CARTESIAN_POINT('Origin',(0.15,-3.8,-15.3379344438427)) ;
#110353 = CARTESIAN_POINT('Origin',(0.0979344438426627,-3.8,-15.3379344438427)) ;
#110354 = CARTESIAN_POINT('Origin',(-0.0979344438426628,-3.8,-14.74)) ;
#110355 = CARTESIAN_POINT('Origin',(-0.0979344438426628,-3.8,-15.1420655561573)) ;
#110356 = CARTESIAN_POINT('Origin',(-0.174966890829628,-3.68995364716148,
-15.0650331091704)) ;
#110357 = CARTESIAN_POINT('Origin',(-0.400000000000001,-3.36847777691809,
-14.84)) ;
#110358 = CARTESIAN_POINT('Origin',(-0.0979344438426627,-3.8,-15.1420655561573)) ;
#110359 = CARTESIAN_POINT('Origin',(0.0979344438426627,-3.8,-15.3379344438427)) ;
#110360 = CARTESIAN_POINT('Origin',(0.0979344438426628,-3.8,-15.3379344438427)) ;
#110361 = CARTESIAN_POINT('Origin',(-0.0979344438426628,-3.8,-15.1420655561573)) ;
#110362 = CARTESIAN_POINT('Origin',(-0.0979344438426628,-3.8,-15.1420655561573)) ;
#110363 = CARTESIAN_POINT('Origin',(0.0979344438426627,-3.8,-14.74)) ;
#110364 = CARTESIAN_POINT('Origin',(0.0979344438426627,-3.8,-15.1420655561573)) ;
#110365 = CARTESIAN_POINT('Origin',(-1.11032778078669,-3.8,-15.1420655561573)) ;
#110366 = CARTESIAN_POINT('Origin',(0.0979344438426626,-3.8,-15.1420655561573)) ;
#110367 = CARTESIAN_POINT('Origin',(0.0979344438426627,-3.8,-15.1420655561573)) ;
#110368 = CARTESIAN_POINT('Origin',(0.0979344438426627,-3.8,-15.1420655561573)) ;
#110369 = CARTESIAN_POINT('Origin',(0.438350729213467,-3.31369102089885,-14.8016492707865)) ;
#110370 = CARTESIAN_POINT('Origin',(0.399999999999999,-3.36847777691809,-14.84)) ;
#110371 = CARTESIAN_POINT('Origin',(0.4,2.3,-14.84)) ;
#110372 = CARTESIAN_POINT('Origin',(0.4,-3.36847777691809,-14.84)) ;
#110373 = CARTESIAN_POINT('Origin',(0.4,2.29999999999999,-14.84)) ;
#110374 = CARTESIAN_POINT('Origin',(1.5,2.3,-14.84)) ;
#110375 = CARTESIAN_POINT('Ctrl Pts',(0.55,2.65280931275593,-14.7900000000001)) ;
#110376 = CARTESIAN_POINT('Ctrl Pts',(0.550000000000012,2.67648433237896,
-14.7757238466627)) ;
#110377 = CARTESIAN_POINT('Ctrl Pts',(0.546908864252792,2.69988533923259,
-14.7635257008476)) ;
#110378 = CARTESIAN_POINT('Ctrl Pts',(0.539540151921449,2.76165254733703,
-14.7440915981901)) ;
#110379 = CARTESIAN_POINT('Ctrl Pts',(0.536602540378443,2.79600904778111,
-14.74)) ;
#110380 = CARTESIAN_POINT('Ctrl Pts',(0.536602540378443,2.83090991212703,
-14.74)) ;
#110381 = CARTESIAN_POINT('Origin',(8.,3.4,-15.64)) ;
#110382 = CARTESIAN_POINT('Origin',(7.96847777691809,3.4,-15.64)) ;
#110383 = CARTESIAN_POINT('Origin',(1.5,4.2,-15.64)) ;
#110384 = CARTESIAN_POINT('Origin',(7.96847777691809,4.2,-15.64)) ;
#110385 = CARTESIAN_POINT('Origin',(8.64348900069683,3.87250785664512,-15.1674921433549)) ;
#110386 = CARTESIAN_POINT('Origin',(7.96847777691809,3.4,-15.64)) ;
#110387 = CARTESIAN_POINT('Origin',(8.4,3.70206555615734,-15.3379344438427)) ;
#110388 = CARTESIAN_POINT('Origin',(8.26722637443421,3.99087598173872,-15.4308759817387)) ;
#110389 = CARTESIAN_POINT('Origin',(7.96847777691809,4.2,-15.64)) ;
#110390 = CARTESIAN_POINT('Origin',(8.4,3.89793444384266,-15.3379344438427)) ;
#110391 = CARTESIAN_POINT('Origin',(8.4,3.95,-15.3379344438427)) ;
#110392 = CARTESIAN_POINT('Origin',(8.4,3.70206555615734,-15.3379344438427)) ;
#110393 = CARTESIAN_POINT('Origin',(8.4,3.89793444384266,-15.3379344438427)) ;
#110394 = CARTESIAN_POINT('Origin',(8.4,3.70206555615734,-15.3379344438427)) ;
#110395 = CARTESIAN_POINT('Origin',(8.4,3.70206555615734,-15.3379344438427)) ;
#110396 = CARTESIAN_POINT('Origin',(1.5,3.4,-14.84)) ;
#110397 = CARTESIAN_POINT('Origin',(7.96847777691809,3.4,-14.84)) ;
#110398 = CARTESIAN_POINT('Origin',(1.5,4.2,-14.84)) ;
#110399 = CARTESIAN_POINT('Origin',(7.96847777691809,4.2,-14.84)) ;
#110400 = CARTESIAN_POINT('Origin',(8.4,3.89793444384266,-15.3379344438427)) ;
#110401 = CARTESIAN_POINT('Origin',(8.4,3.89793444384266,-15.3379344438427)) ;
#110402 = CARTESIAN_POINT('Origin',(8.4,3.70206555615734,-14.74)) ;
#110403 = CARTESIAN_POINT('Origin',(8.4,3.70206555615734,-15.1420655561573)) ;
#110404 = CARTESIAN_POINT('Origin',(8.28995364716148,3.62503310917037,-15.0650331091704)) ;
#110405 = CARTESIAN_POINT('Origin',(7.96847777691809,3.4,-14.84)) ;
#110406 = CARTESIAN_POINT('Origin',(8.4,3.70206555615734,-15.1420655561573)) ;
#110407 = CARTESIAN_POINT('Origin',(7.91369102089885,4.23835072921347,-14.8016492707865)) ;
#110408 = CARTESIAN_POINT('Origin',(7.96847777691809,4.2,-14.84)) ;
#110409 = CARTESIAN_POINT('Origin',(8.4,3.89793444384266,-15.1420655561573)) ;
#110410 = CARTESIAN_POINT('Origin',(8.4,3.89793444384266,-14.74)) ;
#110411 = CARTESIAN_POINT('Origin',(8.4,3.89793444384266,-15.1420655561573)) ;
#110412 = CARTESIAN_POINT('Origin',(8.4,3.70206555615734,-15.1420655561573)) ;
#110413 = CARTESIAN_POINT('Origin',(8.4,3.70206555615734,-15.1420655561573)) ;
#110414 = CARTESIAN_POINT('Origin',(8.4,3.89793444384266,-15.1420655561573)) ;
#110415 = CARTESIAN_POINT('Origin',(8.4,3.89793444384266,-15.1420655561573)) ;
#110416 = CARTESIAN_POINT('Origin',(8.4,2.68967221921331,-15.1420655561573)) ;
#110417 = CARTESIAN_POINT('Origin',(9.9,6.8847127088383,-17.78)) ;
#110418 = CARTESIAN_POINT('Origin',(9.9,6.8847127088383,-16.1997127088383)) ;
#110419 = CARTESIAN_POINT('Origin',(8.77035388141948,6.69643835574155,-16.0114383557416)) ;
#110420 = CARTESIAN_POINT('Ctrl Pts',(8.58356010126946,6.66256607592812,-15.878926683545)) ;
#110421 = CARTESIAN_POINT('Ctrl Pts',(8.58266714977878,6.65676189123867,-15.8787778582965)) ;
#110422 = CARTESIAN_POINT('Ctrl Pts',(8.58182526931893,6.65077142220909,-15.8791141714741)) ;
#110423 = CARTESIAN_POINT('Ctrl Pts',(8.58032528754329,6.63886560514777,-15.8809127350998)) ;
#110424 = CARTESIAN_POINT('Ctrl Pts',(8.57966270906098,6.63295370212097,-15.8823448243331)) ;
#110425 = CARTESIAN_POINT('Ctrl Pts',(8.57906641006212,6.62681909302431,-15.8844771744941)) ;
#110426 = CARTESIAN_POINT('Ctrl Pts',(8.57903375157323,6.6264799875246,-15.8845971697286)) ;
#110427 = CARTESIAN_POINT('Ctrl Pts',(8.57846569624192,6.6205258217488,-15.886741731681)) ;
#110428 = CARTESIAN_POINT('Ctrl Pts',(8.57802501793965,6.61503168015257,-15.8893142858557)) ;
#110429 = CARTESIAN_POINT('Ctrl Pts',(8.57766199200568,6.60925146760312,-15.8927462133234)) ;
#110430 = CARTESIAN_POINT('Ctrl Pts',(8.57762821177172,6.60869602779103,-15.8930838351647)) ;
#110431 = CARTESIAN_POINT('Ctrl Pts',(8.57728522755446,6.60286036001455,-15.8967147989572)) ;
#110432 = CARTESIAN_POINT('Ctrl Pts',(8.57709550103271,6.59788070192331,-15.9005482210564)) ;
#110433 = CARTESIAN_POINT('Ctrl Pts',(8.57703980289278,6.59299711069393,-15.9051723373549)) ;
#110434 = CARTESIAN_POINT('Ctrl Pts',(8.57703670271021,6.59265952430039,-15.9054968925421)) ;
#110435 = CARTESIAN_POINT('Ctrl Pts',(8.57701334129169,6.58927432516127,-15.9088013815953)) ;
#110436 = CARTESIAN_POINT('Ctrl Pts',(8.57705699426434,6.5864297120155,-15.9119917444088)) ;
#110437 = CARTESIAN_POINT('Ctrl Pts',(8.57735031225521,6.57961409340222,-15.9207954417554)) ;
#110438 = CARTESIAN_POINT('Ctrl Pts',(8.57770856513437,6.57604383182914,-15.9266682455399)) ;
#110439 = CARTESIAN_POINT('Ctrl Pts',(8.57865704971091,6.57055741297636,-15.9383322193388)) ;
#110440 = CARTESIAN_POINT('Ctrl Pts',(8.57922107378969,6.56851476050447,-15.9440736349076)) ;
#110441 = CARTESIAN_POINT('Ctrl Pts',(8.57993695782543,6.56687610193754,-15.9504559348163)) ;
#110442 = CARTESIAN_POINT('Ctrl Pts',(8.58000419042984,6.56673001682056,-15.9510478351839)) ;
#110443 = CARTESIAN_POINT('Ctrl Pts',(8.58074399738019,6.56520526212522,-15.9574812517353)) ;
#110444 = CARTESIAN_POINT('Ctrl Pts',(8.58149993293348,6.56438134785777,-15.9633541800934)) ;
#110445 = CARTESIAN_POINT('Ctrl Pts',(8.58236768178477,6.56403389662202,-15.9694987578232)) ;
#110446 = CARTESIAN_POINT('Ctrl Pts',(8.58242358604549,6.56401394107886,-15.9698921736316)) ;
#110447 = CARTESIAN_POINT('Ctrl Pts',(8.58283067264383,6.56388592662946,-15.9727394234264)) ;
#110448 = CARTESIAN_POINT('Ctrl Pts',(8.58319156240649,6.56386525642005,-15.9751699505828)) ;
#110449 = CARTESIAN_POINT('Ctrl Pts',(8.58356019967707,6.56392669994633,-15.9775662650647)) ;
#110450 = CARTESIAN_POINT('Origin',(9.9,6.8847127088383,-16.1997127088383)) ;
#110451 = CARTESIAN_POINT('Origin',(9.9,6.8847127088383,-16.1997127088383)) ;
#110452 = CARTESIAN_POINT('Origin',(9.9,6.8847127088383,-16.1997127088383)) ;
#110453 = CARTESIAN_POINT('Origin',(9.9,7.72792407799439,-17.78)) ;
#110454 = CARTESIAN_POINT('Origin',(9.9,7.72792407799439,-16.1997127088383)) ;
#110455 = CARTESIAN_POINT('Origin',(9.90000000000001,4.35421736843756,-16.1997127088383)) ;
#110456 = CARTESIAN_POINT('Origin',(9.9,7.72792407799439,-16.1997127088383)) ;
#110457 = CARTESIAN_POINT('Origin',(9.9,7.72792407799439,-16.1997127088383)) ;
#110458 = CARTESIAN_POINT('Origin',(9.9,7.72792407799439,-16.1997127088383)) ;
#110459 = CARTESIAN_POINT('Origin',(10.9628342502842,7.37364599456632,-16.3768517505523)) ;
#110460 = CARTESIAN_POINT('Ctrl Pts',(8.56837732530591,8.27720755823129,-15.972505253798)) ;
#110461 = CARTESIAN_POINT('Ctrl Pts',(8.56753565030799,8.27748812367261,-15.9666129921977)) ;
#110462 = CARTESIAN_POINT('Ctrl Pts',(8.5668204554169,8.27721180667912,-15.9605412944397)) ;
#110463 = CARTESIAN_POINT('Ctrl Pts',(8.56575413148011,8.27538624160202,-15.9487284721173)) ;
#110464 = CARTESIAN_POINT('Ctrl Pts',(8.56538426077847,8.27391165896455,-15.9429905624269)) ;
#110465 = CARTESIAN_POINT('Ctrl Pts',(8.56517777855929,8.27166501362482,-15.9370147754464)) ;
#110466 = CARTESIAN_POINT('Ctrl Pts',(8.56516523451681,8.27151619608583,-15.9366276382834)) ;
#110467 = CARTESIAN_POINT('Ctrl Pts',(8.56497390811214,8.26902793125451,-15.9302953359912)) ;
#110468 = CARTESIAN_POINT('Ctrl Pts',(8.56499903025534,8.2659763012945,-15.9245357784659)) ;
#110469 = CARTESIAN_POINT('Ctrl Pts',(8.56538588200257,8.26046191593055,-15.9165906723681)) ;
#110470 = CARTESIAN_POINT('Ctrl Pts',(8.56556309332507,8.25853771611458,-15.9141212364558)) ;
#110471 = CARTESIAN_POINT('Ctrl Pts',(8.56628156514548,8.25214511987158,-15.9068017566891)) ;
#110472 = CARTESIAN_POINT('Ctrl Pts',(8.56700742874793,8.2472021625627,-15.902305445231)) ;
#110473 = CARTESIAN_POINT('Ctrl Pts',(8.56880713798126,8.23661566152159,-15.8946244948799)) ;
#110474 = CARTESIAN_POINT('Ctrl Pts',(8.56986039391321,8.23102391526953,-15.8913848807254)) ;
#110475 = CARTESIAN_POINT('Ctrl Pts',(8.57116255171756,8.22459552194113,-15.8884467745269)) ;
#110476 = CARTESIAN_POINT('Ctrl Pts',(8.57127495810218,8.22404408343781,-15.8882006607901)) ;
#110477 = CARTESIAN_POINT('Ctrl Pts',(8.57260511146311,8.21755901312583,-15.8853749153055)) ;
#110478 = CARTESIAN_POINT('Ctrl Pts',(8.57395629672839,8.2113575973091,-15.8833463864276)) ;
#110479 = CARTESIAN_POINT('Ctrl Pts',(8.57552311082417,8.20452945286286,-15.8817495443173)) ;
#110480 = CARTESIAN_POINT('Ctrl Pts',(8.57564505123012,8.2040002630709,-15.881629826956)) ;
#110481 = CARTESIAN_POINT('Ctrl Pts',(8.57731301559523,8.1967919362264,-15.880053462537)) ;
#110482 = CARTESIAN_POINT('Ctrl Pts',(8.57896065127869,8.19002168485366,-15.879210969344)) ;
#110483 = CARTESIAN_POINT('Ctrl Pts',(8.58161366784366,8.17959769015482,-15.8787553172771)) ;
#110484 = CARTESIAN_POINT('Ctrl Pts',(8.58258362864269,8.17587911616515,-15.8787639381071)) ;
#110485 = CARTESIAN_POINT('Ctrl Pts',(8.58356010126947,8.17221734381475,-15.8789266835449)) ;
#110486 = CARTESIAN_POINT('Origin',(7.96824861826159,6.56275414521524,-14.6022458547848)) ;
#110487 = CARTESIAN_POINT('Origin',(8.59688370202597,6.66156024040237,-14.5112434752653)) ;
#110488 = CARTESIAN_POINT('Origin',(9.9,6.8847127088383,-14.2802872911617)) ;
#110489 = CARTESIAN_POINT('Origin',(9.9,6.8847127088383,-17.78)) ;
#110490 = CARTESIAN_POINT('Origin',(9.9,6.8847127088383,-14.2802872911617)) ;
#110491 = CARTESIAN_POINT('Origin',(9.9,6.8847127088383,-14.2802872911617)) ;
#110492 = CARTESIAN_POINT('Origin',(9.9,6.8847127088383,-14.2802872911617)) ;
#110493 = CARTESIAN_POINT('Origin',(9.9,6.8,-14.2802872911617)) ;
#110494 = CARTESIAN_POINT('Origin',(9.9,7.72792407799439,-14.2802872911617)) ;
#110495 = CARTESIAN_POINT('Origin',(9.9,7.72792407799439,-17.78)) ;
#110496 = CARTESIAN_POINT('Origin',(9.9,7.72792407799439,-14.2802872911617)) ;
#110497 = CARTESIAN_POINT('Origin',(9.9,7.72792407799439,-14.2802872911617)) ;
#110498 = CARTESIAN_POINT('Origin',(9.9,7.72792407799439,-14.2802872911617)) ;
#110499 = CARTESIAN_POINT('Origin',(9.60917571369883,7.82486550676144,-14.3287580055452)) ;
#110500 = CARTESIAN_POINT('Origin',(8.59099001846147,8.18966234086349,-14.5051609738971)) ;
#110501 = CARTESIAN_POINT('Origin',(0.45,4.4,-15.24)) ;
#110502 = CARTESIAN_POINT('Origin',(0.45,4.4,-15.69)) ;
#110503 = CARTESIAN_POINT('Origin',(0.45,4.4,-14.79)) ;
#110504 = CARTESIAN_POINT('Origin',(-1.9,7.55,-17.78)) ;
#110505 = CARTESIAN_POINT('Origin',(6.9,7.75,-17.78)) ;
#110506 = CARTESIAN_POINT('Origin',(7.1,8.2,-17.78)) ;
#110507 = CARTESIAN_POINT('Origin',(9.9,0.1,-17.78)) ;
#110508 = CARTESIAN_POINT('Origin',(9.9,1.16528729116168,-17.78)) ;
#110509 = CARTESIAN_POINT('Origin',(9.9,1.16528729116168,-17.2841618801782)) ;
#110510 = CARTESIAN_POINT('Origin',(9.9,3.8,-15.24)) ;
#110511 = CARTESIAN_POINT('Origin',(9.9,1.16528729116168,-13.1958381198218)) ;
#110512 = CARTESIAN_POINT('Origin',(9.9,1.16528729116168,-17.2841618801782)) ;
#110513 = CARTESIAN_POINT('Origin',(9.9,1.16528729116168,-17.78)) ;
#110514 = CARTESIAN_POINT('Origin',(9.9,1.16528729116168,-13.1958381198218)) ;
#110515 = CARTESIAN_POINT('Ctrl Pts',(0.55,0.3,-15.69)) ;
#110516 = CARTESIAN_POINT('Ctrl Pts',(0.55,0.3,-15.79)) ;
#110517 = CARTESIAN_POINT('Ctrl Pts',(0.45,0.3,-15.79)) ;
#110518 = CARTESIAN_POINT('Ctrl Pts',(0.55,0.28690770353672,-15.6900000008182)) ;
#110519 = CARTESIAN_POINT('Ctrl Pts',(0.549992696056738,0.300543498484345,
-15.7899926960962)) ;
#110520 = CARTESIAN_POINT('Ctrl Pts',(0.450000000818259,0.286907703536713,
-15.79)) ;
#110521 = CARTESIAN_POINT('Ctrl Pts',(0.552602750539093,0.273825167611082,
-15.6952055010782)) ;
#110522 = CARTESIAN_POINT('Ctrl Pts',(0.546703256435903,0.299059401315785,
-15.7867032564359)) ;
#110523 = CARTESIAN_POINT('Ctrl Pts',(0.455205501078185,0.273825167611091,
-15.7926027505391)) ;
#110524 = CARTESIAN_POINT('Ctrl Pts',(0.56262134295865,0.249638145915901,
-15.7152426859173)) ;
#110525 = CARTESIAN_POINT('Ctrl Pts',(0.544986924117065,0.28207277643954,
-15.7849869241171)) ;
#110526 = CARTESIAN_POINT('Ctrl Pts',(0.4752426859173,0.249638145915891,-15.8026213429587)) ;
#110527 = CARTESIAN_POINT('Ctrl Pts',(0.570033341471288,0.238545302291403,
-15.7300666829426)) ;
#110528 = CARTESIAN_POINT('Ctrl Pts',(0.54711619685839,0.267914459835251,
-15.7871161968584)) ;
#110529 = CARTESIAN_POINT('Ctrl Pts',(0.490066682942577,0.238545302291388,
-15.8100333414713)) ;
#110530 = CARTESIAN_POINT('Ctrl Pts',(0.597801282701459,0.210777361061231,
-15.7856025654029)) ;
#110531 = CARTESIAN_POINT('Ctrl Pts',(0.570853448890191,0.226374713859272,
-15.8108534488901)) ;
#110532 = CARTESIAN_POINT('Ctrl Pts',(0.545602565402917,0.21077736106126,
-15.8378012827014)) ;
#110533 = CARTESIAN_POINT('Ctrl Pts',(0.623746567173686,0.2,-15.8374931343473)) ;
#110534 = CARTESIAN_POINT('Ctrl Pts',(0.610458667316253,0.2,-15.8504586673162)) ;
#110535 = CARTESIAN_POINT('Ctrl Pts',(0.59749313434734,0.2,-15.8637465671735)) ;
#110536 = CARTESIAN_POINT('Ctrl Pts',(0.65,0.2,-15.89)) ;
#110537 = CARTESIAN_POINT('Ctrl Pts',(0.65,0.2,-15.89)) ;
#110538 = CARTESIAN_POINT('Ctrl Pts',(0.65,0.2,-15.89)) ;
#110539 = CARTESIAN_POINT('Origin',(0.45,0.3,-15.69)) ;
#110540 = CARTESIAN_POINT('Origin',(0.45,1.24941393210234E-16,-15.69)) ;
#110541 = CARTESIAN_POINT('Origin',(0.45,4.4,-15.69)) ;
#110542 = CARTESIAN_POINT('Origin',(0.45,4.4,-15.69)) ;
#110543 = CARTESIAN_POINT('Origin',(0.45,4.4,-15.69)) ;
#110544 = CARTESIAN_POINT('Origin',(0.549999999999999,4.4,-15.69)) ;
#110545 = CARTESIAN_POINT('Origin',(-1.7,4.4,-15.69)) ;
#110546 = CARTESIAN_POINT('Ctrl Pts',(-1.8,4.6,-15.89)) ;
#110547 = CARTESIAN_POINT('Ctrl Pts',(-1.8,4.6,-15.89)) ;
#110548 = CARTESIAN_POINT('Ctrl Pts',(-1.8,4.6,-15.89)) ;
#110549 = CARTESIAN_POINT('Ctrl Pts',(-1.8,4.57374656717372,-15.8374931343473)) ;
#110550 = CARTESIAN_POINT('Ctrl Pts',(-1.8,4.56045866731429,-15.8504586673144)) ;
#110551 = CARTESIAN_POINT('Ctrl Pts',(-1.8,4.54749313434728,-15.8637465671737)) ;
#110552 = CARTESIAN_POINT('Ctrl Pts',(-1.78922263893876,4.54780128270145,
-15.7856025654029)) ;
#110553 = CARTESIAN_POINT('Ctrl Pts',(-1.77362528614074,4.52085344889015,
-15.8108534488901)) ;
#110554 = CARTESIAN_POINT('Ctrl Pts',(-1.78922263893874,4.49560256540291,
-15.8378012827014)) ;
#110555 = CARTESIAN_POINT('Ctrl Pts',(-1.7614546977086,4.5200333414713,-15.7300666829426)) ;
#110556 = CARTESIAN_POINT('Ctrl Pts',(-1.73208554016474,4.49711619685842,
-15.7871161968584)) ;
#110557 = CARTESIAN_POINT('Ctrl Pts',(-1.76145469770861,4.44006668294258,
-15.8100333414713)) ;
#110558 = CARTESIAN_POINT('Ctrl Pts',(-1.7503618540841,4.51262134295865,-15.7152426859173)) ;
#110559 = CARTESIAN_POINT('Ctrl Pts',(-1.71792722356046,4.49498692411707,
-15.7849869241171)) ;
#110560 = CARTESIAN_POINT('Ctrl Pts',(-1.75036185408411,4.42524268591729,
-15.8026213429587)) ;
#110561 = CARTESIAN_POINT('Ctrl Pts',(-1.72617483238892,4.50260275053909,
-15.6952055010782)) ;
#110562 = CARTESIAN_POINT('Ctrl Pts',(-1.70094059868422,4.4967032564359,-15.7867032564359)) ;
#110563 = CARTESIAN_POINT('Ctrl Pts',(-1.72617483238891,4.4052055010782,-15.7926027505391)) ;
#110564 = CARTESIAN_POINT('Ctrl Pts',(-1.71309229646328,4.5,-15.6900000008182)) ;
#110565 = CARTESIAN_POINT('Ctrl Pts',(-1.69945650152272,4.49999269603968,
-15.7899926960963)) ;
#110566 = CARTESIAN_POINT('Ctrl Pts',(-1.71309229646329,4.40000000081823,
-15.79)) ;
#110567 = CARTESIAN_POINT('Ctrl Pts',(-1.7,4.5,-15.69)) ;
#110568 = CARTESIAN_POINT('Ctrl Pts',(-1.7,4.5,-15.79)) ;
#110569 = CARTESIAN_POINT('Ctrl Pts',(-1.7,4.4,-15.79)) ;
#110570 = CARTESIAN_POINT('Ctrl Pts',(-1.8,4.6,-14.59)) ;
#110571 = CARTESIAN_POINT('Ctrl Pts',(-1.8,4.6,-14.59)) ;
#110572 = CARTESIAN_POINT('Ctrl Pts',(-1.8,4.6,-14.59)) ;
#110573 = CARTESIAN_POINT('Ctrl Pts',(-1.8,4.54749313434729,-14.6162534328264)) ;
#110574 = CARTESIAN_POINT('Ctrl Pts',(-1.8,4.56045866731616,-14.6295413326839)) ;
#110575 = CARTESIAN_POINT('Ctrl Pts',(-1.8,4.57374656717362,-14.6425068656528)) ;
#110576 = CARTESIAN_POINT('Ctrl Pts',(-1.78922263893879,4.49560256540291,
-14.6421987172985)) ;
#110577 = CARTESIAN_POINT('Ctrl Pts',(-1.77362528614072,4.52085344889015,
-14.6691465511098)) ;
#110578 = CARTESIAN_POINT('Ctrl Pts',(-1.78922263893876,4.54780128270145,
-14.694397434597)) ;
#110579 = CARTESIAN_POINT('Ctrl Pts',(-1.76145469770859,4.44006668294258,
-14.6699666585287)) ;
#110580 = CARTESIAN_POINT('Ctrl Pts',(-1.73208554016476,4.49711619685842,
-14.6928838031416)) ;
#110581 = CARTESIAN_POINT('Ctrl Pts',(-1.7614546977086,4.5200333414713,-14.7499333170575)) ;
#110582 = CARTESIAN_POINT('Ctrl Pts',(-1.75036185408409,4.42524268591729,
-14.6773786570414)) ;
#110583 = CARTESIAN_POINT('Ctrl Pts',(-1.71792722356047,4.49498692411705,
-14.695013075883)) ;
#110584 = CARTESIAN_POINT('Ctrl Pts',(-1.7503618540841,4.51262134295865,-14.7647573140827)) ;
#110585 = CARTESIAN_POINT('Ctrl Pts',(-1.72617483238892,4.4052055010782,-14.6873972494609)) ;
#110586 = CARTESIAN_POINT('Ctrl Pts',(-1.7009405986842,4.49670325643591,-14.6932967435641)) ;
#110587 = CARTESIAN_POINT('Ctrl Pts',(-1.72617483238892,4.50260275053909,
-14.7847944989218)) ;
#110588 = CARTESIAN_POINT('Ctrl Pts',(-1.71309229646328,4.40000000081823,
-14.69)) ;
#110589 = CARTESIAN_POINT('Ctrl Pts',(-1.69945650151499,4.49999269606786,
-14.6900073039133)) ;
#110590 = CARTESIAN_POINT('Ctrl Pts',(-1.71309229646328,4.5,-14.7899999991817)) ;
#110591 = CARTESIAN_POINT('Ctrl Pts',(-1.7,4.4,-14.69)) ;
#110592 = CARTESIAN_POINT('Ctrl Pts',(-1.7,4.5,-14.69)) ;
#110593 = CARTESIAN_POINT('Ctrl Pts',(-1.7,4.5,-14.79)) ;
#110594 = CARTESIAN_POINT('Origin',(-1.7,4.4,-14.79)) ;
#110595 = CARTESIAN_POINT('Origin',(0.549999999999999,4.4,-14.79)) ;
#110596 = CARTESIAN_POINT('Origin',(0.45,4.4,-14.79)) ;
#110597 = CARTESIAN_POINT('Origin',(0.45,4.4,-14.79)) ;
#110598 = CARTESIAN_POINT('Origin',(0.45,4.4,-14.79)) ;
#110599 = CARTESIAN_POINT('Origin',(0.45,4.9047241136249E-17,-14.79)) ;
#110600 = CARTESIAN_POINT('Origin',(0.45,0.3,-14.79)) ;
#110601 = CARTESIAN_POINT('Ctrl Pts',(0.45,0.3,-14.69)) ;
#110602 = CARTESIAN_POINT('Ctrl Pts',(0.55,0.3,-14.69)) ;
#110603 = CARTESIAN_POINT('Ctrl Pts',(0.55,0.3,-14.79)) ;
#110604 = CARTESIAN_POINT('Ctrl Pts',(0.450000000818259,0.286907703536723,
-14.69)) ;
#110605 = CARTESIAN_POINT('Ctrl Pts',(0.549992696019264,0.300543498464983,
-14.690007303913)) ;
#110606 = CARTESIAN_POINT('Ctrl Pts',(0.55,0.28690770353672,-14.7899999991817)) ;
#110607 = CARTESIAN_POINT('Ctrl Pts',(0.455205501078185,0.273825167611078,
-14.6873972494609)) ;
#110608 = CARTESIAN_POINT('Ctrl Pts',(0.546703256435899,0.299059401315789,
-14.6932967435641)) ;
#110609 = CARTESIAN_POINT('Ctrl Pts',(0.552602750539093,0.273825167611082,
-14.7847944989218)) ;
#110610 = CARTESIAN_POINT('Ctrl Pts',(0.4752426859173,0.249638145915905,-14.6773786570414)) ;
#110611 = CARTESIAN_POINT('Ctrl Pts',(0.544986924117067,0.282072776439535,
-14.6950130758829)) ;
#110612 = CARTESIAN_POINT('Ctrl Pts',(0.56262134295865,0.249638145915901,
-14.7647573140827)) ;
#110613 = CARTESIAN_POINT('Ctrl Pts',(0.490066682942577,0.238545302291402,
-14.6699666585287)) ;
#110614 = CARTESIAN_POINT('Ctrl Pts',(0.547116196858397,0.267914459835244,
-14.6928838031416)) ;
#110615 = CARTESIAN_POINT('Ctrl Pts',(0.570033341471288,0.238545302291403,
-14.7499333170574)) ;
#110616 = CARTESIAN_POINT('Ctrl Pts',(0.545602565402917,0.210777361061233,
-14.6421987172985)) ;
#110617 = CARTESIAN_POINT('Ctrl Pts',(0.570853448890184,0.226374713859283,
-14.6691465511098)) ;
#110618 = CARTESIAN_POINT('Ctrl Pts',(0.597801282701459,0.210777361061231,
-14.6943974345971)) ;
#110619 = CARTESIAN_POINT('Ctrl Pts',(0.59749313434723,0.2,-14.6162534328263)) ;
#110620 = CARTESIAN_POINT('Ctrl Pts',(0.610458667316026,0.2,-14.629541332684)) ;
#110621 = CARTESIAN_POINT('Ctrl Pts',(0.623746567173609,0.2,-14.6425068656527)) ;
#110622 = CARTESIAN_POINT('Ctrl Pts',(0.65,0.2,-14.59)) ;
#110623 = CARTESIAN_POINT('Ctrl Pts',(0.65,0.2,-14.59)) ;
#110624 = CARTESIAN_POINT('Ctrl Pts',(0.65,0.2,-14.59)) ;
#110625 = CARTESIAN_POINT('Ctrl Pts',(8.5,8.17221734381475,-15.7802872911617)) ;
#110626 = CARTESIAN_POINT('Ctrl Pts',(8.5,8.17221734381475,-15.865)) ;
#110627 = CARTESIAN_POINT('Ctrl Pts',(8.58356010126947,8.17221734381475,-15.8789266835449)) ;
#110628 = CARTESIAN_POINT('Ctrl Pts',(8.5,8.23335379241386,-15.7802872927391)) ;
#110629 = CARTESIAN_POINT('Ctrl Pts',(8.5,8.20847425960662,-15.8574575674223)) ;
#110630 = CARTESIAN_POINT('Ctrl Pts',(8.57460439031233,8.20580126077889,-15.8774340650521)) ;
#110631 = CARTESIAN_POINT('Ctrl Pts',(8.5,8.29192178062155,-15.8071741150785)) ;
#110632 = CARTESIAN_POINT('Ctrl Pts',(8.5,8.25010493984403,-15.8692546083117)) ;
#110633 = CARTESIAN_POINT('Ctrl Pts',(8.56800970738924,8.23725302684489,-15.8897783631899)) ;
#110634 = CARTESIAN_POINT('Ctrl Pts',(8.5,8.36583651094027,-15.8965506232914)) ;
#110635 = CARTESIAN_POINT('Ctrl Pts',(8.5,8.29925403146167,-15.9233614370366)) ;
#110636 = CARTESIAN_POINT('Ctrl Pts',(8.56373266208983,8.27563607377072,-15.9337537764131)) ;
#110637 = CARTESIAN_POINT('Ctrl Pts',(8.5,8.38029241321759,-15.9579552056996)) ;
#110638 = CARTESIAN_POINT('Ctrl Pts',(8.5,8.30669116589121,-15.9648088499411)) ;
#110639 = CARTESIAN_POINT('Ctrl Pts',(8.56610123859376,8.28208399509955,-15.964808702407)) ;
#110640 = CARTESIAN_POINT('Ctrl Pts',(8.5,8.36719795478508,-16.0160547234799)) ;
#110641 = CARTESIAN_POINT('Ctrl Pts',(8.5,8.29381262650623,-15.9995151496718)) ;
#110642 = CARTESIAN_POINT('Ctrl Pts',(8.57227762885807,8.27346847343705,-15.9949299876354)) ;
#110643 = CARTESIAN_POINT('Ctrl Pts',(8.5485213309235,8.28383177029354,-15.9959865327337)) ;
#110644 = CARTESIAN_POINT('Ctrl Pts',(8.54913757890789,8.28625057716298,-15.982921659184)) ;
#110645 = CARTESIAN_POINT('Ctrl Pts',(8.549146361399,8.28675781111762,-15.9692647894026)) ;
#110646 = CARTESIAN_POINT('Ctrl Pts',(8.54883414737369,8.28489376483071,-15.956098869425)) ;
#110647 = CARTESIAN_POINT('Ctrl Pts',(8.54852072231757,8.28302248819127,-15.9428818808428)) ;
#110648 = CARTESIAN_POINT('Ctrl Pts',(8.54791723678494,8.27865742078997,-15.9298312958117)) ;
#110649 = CARTESIAN_POINT('Ctrl Pts',(8.54677696932927,8.27237937104781,-15.9181020767297)) ;
#110650 = CARTESIAN_POINT('Ctrl Pts',(8.5454465495755,8.26505438658866,-15.9044168797302)) ;
#110651 = CARTESIAN_POINT('Ctrl Pts',(8.54324462275112,8.25487237915563,-15.8922537533388)) ;
#110652 = CARTESIAN_POINT('Ctrl Pts',(8.53884071267076,8.24480815719263,-15.8812071681992)) ;
#110653 = CARTESIAN_POINT('Ctrl Pts',(8.5342440055524,8.23430333763594,-15.8696769789768)) ;
#110654 = CARTESIAN_POINT('Ctrl Pts',(8.52670159721618,8.22420330618022,-15.858704260243)) ;
#110655 = CARTESIAN_POINT('Ctrl Pts',(8.51928858688475,8.21729138318396,-15.8459881754653)) ;
#110656 = CARTESIAN_POINT('Ctrl Pts',(8.51327528614099,8.21168455548023,-15.835673116045)) ;
#110657 = CARTESIAN_POINT('Ctrl Pts',(8.50759525524367,8.20778929846109,-15.8239849430828)) ;
#110658 = CARTESIAN_POINT('Ctrl Pts',(8.50412058850191,8.20498026622232,-15.8115739486628)) ;
#110659 = CARTESIAN_POINT('Ctrl Pts',(8.50147164778345,8.20283877743224,-15.8021123251694)) ;
#110660 = CARTESIAN_POINT('Ctrl Pts',(8.50000317248551,8.2012555848359,-15.792083357655)) ;
#110661 = CARTESIAN_POINT('Ctrl Pts',(8.50000000513446,8.20000405629318,-15.7821052387284)) ;
#110662 = CARTESIAN_POINT('Origin',(8.6,8.17221734381475,-15.7802872911617)) ;
#110663 = CARTESIAN_POINT('Origin',(8.6,4.35421736843756,-15.7802872911617)) ;
#110664 = CARTESIAN_POINT('Origin',(8.6,6.66256607592813,-15.7802872911617)) ;
#110665 = CARTESIAN_POINT('Ctrl Pts',(8.5,6.47083593368087,-16.0248081099244)) ;
#110666 = CARTESIAN_POINT('Ctrl Pts',(8.5,6.55684090505321,-16.0043877386952)) ;
#110667 = CARTESIAN_POINT('Ctrl Pts',(8.58772778625753,6.56739561896918,-16.001881707091)) ;
#110668 = CARTESIAN_POINT('Ctrl Pts',(8.5,6.45680686388577,-15.9657215297177)) ;
#110669 = CARTESIAN_POINT('Ctrl Pts',(8.5,6.544062294786,-15.9725101654037)) ;
#110670 = CARTESIAN_POINT('Ctrl Pts',(8.58195196310359,6.55941415012443,-15.9713576868778)) ;
#110671 = CARTESIAN_POINT('Ctrl Pts',(8.5,6.47061556584392,-15.9019524568048)) ;
#110672 = CARTESIAN_POINT('Ctrl Pts',(8.5,6.54836369988892,-15.9323987274072)) ;
#110673 = CARTESIAN_POINT('Ctrl Pts',(8.57801125828727,6.5656660137223,-15.9388344592028)) ;
#110674 = CARTESIAN_POINT('Ctrl Pts',(8.5,6.54379299301794,-15.8086264716581)) ;
#110675 = CARTESIAN_POINT('Ctrl Pts',(8.5,6.5907178951622,-15.8762265152921)) ;
#110676 = CARTESIAN_POINT('Ctrl Pts',(8.57642058265785,6.60198961470446,-15.8919063540245)) ;
#110677 = CARTESIAN_POINT('Ctrl Pts',(8.5,6.60220518075383,-15.7802872929745)) ;
#110678 = CARTESIAN_POINT('Ctrl Pts',(8.5,6.62800697860329,-15.8609176707628)) ;
#110679 = CARTESIAN_POINT('Ctrl Pts',(8.57879135173924,6.63156920211803,-15.8781318919565)) ;
#110680 = CARTESIAN_POINT('Ctrl Pts',(8.5,6.66256607592813,-15.7802872911617)) ;
#110681 = CARTESIAN_POINT('Ctrl Pts',(8.5,6.66256607592813,-15.865)) ;
#110682 = CARTESIAN_POINT('Ctrl Pts',(8.58356010126947,6.66256607592813,-15.8789266835449)) ;
#110683 = CARTESIAN_POINT('',(8.54565366748552,6.61650711946997,-15.8739653182917)) ;
#110684 = CARTESIAN_POINT('Ctrl Pts',(8.54565366716102,6.61650712004131,-15.8739653178135)) ;
#110685 = CARTESIAN_POINT('Ctrl Pts',(8.54527684775567,6.61717057264361,-15.8734100008637)) ;
#110686 = CARTESIAN_POINT('Ctrl Pts',(8.54488909344006,6.61782772231432,-15.8728554298997)) ;
#110687 = CARTESIAN_POINT('Ctrl Pts',(8.54449064961563,6.61847724592616,-15.8723008713851)) ;
#110688 = CARTESIAN_POINT('Ctrl Pts',(8.54445329550709,6.61853813876477,-15.8722488815244)) ;
#110689 = CARTESIAN_POINT('Ctrl Pts',(8.54441584757976,6.6185989645223,-15.8721968917916)) ;
#110690 = CARTESIAN_POINT('Ctrl Pts',(8.54437830610599,6.61865972207468,-15.8721449015859)) ;
#110691 = CARTESIAN_POINT('Ctrl Pts',(8.54363538409151,6.61986207559658,-15.8711160483068)) ;
#110692 = CARTESIAN_POINT('Ctrl Pts',(8.54285495000594,6.62104203503528,-15.8700848621747)) ;
#110693 = CARTESIAN_POINT('Ctrl Pts',(8.54204093171157,6.6221805696012,-15.8690511151673)) ;
#110694 = CARTESIAN_POINT('Ctrl Pts',(8.54157979215442,6.62282554690595,-15.8684654997818)) ;
#110695 = CARTESIAN_POINT('Ctrl Pts',(8.5411077081219,6.62345780120144,-15.8678786499067)) ;
#110696 = CARTESIAN_POINT('Ctrl Pts',(8.54062344907118,6.62407892448169,-15.8672869541396)) ;
#110697 = CARTESIAN_POINT('Ctrl Pts',(8.54011932596482,6.62472552591744,-15.8666709873185)) ;
#110698 = CARTESIAN_POINT('Ctrl Pts',(8.53960207832256,6.62535666566134,-15.866050990589)) ;
#110699 = CARTESIAN_POINT('Ctrl Pts',(8.53907286520408,6.62597244099096,-15.8654252288111)) ;
#110700 = CARTESIAN_POINT('Ctrl Pts',(8.53887441028465,6.62620335673957,-15.8651905681443)) ;
#110701 = CARTESIAN_POINT('Ctrl Pts',(8.53867427664143,6.6264321129994,-15.8649550998211)) ;
#110702 = CARTESIAN_POINT('Ctrl Pts',(8.53847256319998,6.62665871795108,-15.8647187642184)) ;
#110703 = CARTESIAN_POINT('Ctrl Pts',(8.53842843838466,6.62670828778426,-15.8646670658053)) ;
#110704 = CARTESIAN_POINT('Ctrl Pts',(8.53838423811749,6.62675775467668,-15.8646153260174)) ;
#110705 = CARTESIAN_POINT('Ctrl Pts',(8.53833996369345,6.62680711871688,-15.8645635444601)) ;
#110706 = CARTESIAN_POINT('Ctrl Pts',(8.53829707284515,6.62685494013081,-15.8645133810765)) ;
#110707 = CARTESIAN_POINT('Ctrl Pts',(8.53825411240224,6.62690266502018,-15.8644631784931)) ;
#110708 = CARTESIAN_POINT('Ctrl Pts',(8.53821108363806,6.62695029346532,-15.8644129364377)) ;
#110709 = CARTESIAN_POINT('Ctrl Pts',(8.53803571435332,6.62714440934376,-15.8642081684534)) ;
#110710 = CARTESIAN_POINT('Ctrl Pts',(8.53785876035507,6.62733753498028,-15.8640021836648)) ;
#110711 = CARTESIAN_POINT('Ctrl Pts',(8.53767995296704,6.62753033615257,-15.8637944665652)) ;
#110712 = CARTESIAN_POINT('Ctrl Pts',(8.53649871780655,6.62880401687797,-15.862422248425)) ;
#110713 = CARTESIAN_POINT('Ctrl Pts',(8.53528300832266,6.62998038079526,-15.8610380760596)) ;
#110714 = CARTESIAN_POINT('Ctrl Pts',(8.53403203676338,6.63110281535143,-15.8596044865649)) ;
#110715 = CARTESIAN_POINT('Ctrl Pts',(8.53346870389682,6.63160826591213,-15.8589589178679)) ;
#110716 = CARTESIAN_POINT('Ctrl Pts',(8.53289959536922,6.63209979040222,-15.8583054256595)) ;
#110717 = CARTESIAN_POINT('Ctrl Pts',(8.53232661340321,6.63257735344029,-15.8576437014439)) ;
#110718 = CARTESIAN_POINT('Ctrl Pts',(8.53206474273906,6.63279561467254,-15.8573412727985)) ;
#110719 = CARTESIAN_POINT('Ctrl Pts',(8.53180206199568,6.63301096017662,-15.8570371260807)) ;
#110720 = CARTESIAN_POINT('Ctrl Pts',(8.53153874718659,6.63322338883723,-15.8567312388807)) ;
#110721 = CARTESIAN_POINT('Ctrl Pts',(8.5300736365822,6.63440536369243,-15.8550292511271)) ;
#110722 = CARTESIAN_POINT('Ctrl Pts',(8.52858926277509,6.63549697414123,-15.8532730839131)) ;
#110723 = CARTESIAN_POINT('Ctrl Pts',(8.52711342564667,6.63649856635108,-15.8514611393064)) ;
#110724 = CARTESIAN_POINT('Ctrl Pts',(8.5263431695412,6.63702130866457,-15.8505154649028)) ;
#110725 = CARTESIAN_POINT('Ctrl Pts',(8.52557615349971,6.63751985710294,-15.8495557193112)) ;
#110726 = CARTESIAN_POINT('Ctrl Pts',(8.52481401823432,6.63799287689813,-15.8485803261613)) ;
#110727 = CARTESIAN_POINT('Ctrl Pts',(8.52460710835824,6.63812129566006,-15.8483155195253)) ;
#110728 = CARTESIAN_POINT('Ctrl Pts',(8.52440075574006,6.63824801482191,-15.8480497539023)) ;
#110729 = CARTESIAN_POINT('Ctrl Pts',(8.52419502810873,6.63837284070828,-15.8477830860811)) ;
#110730 = CARTESIAN_POINT('Ctrl Pts',(8.52404824365687,6.63846190263541,-15.8475928214593)) ;
#110731 = CARTESIAN_POINT('Ctrl Pts',(8.52390173612806,6.63855002749202,-15.8474020437347)) ;
#110732 = CARTESIAN_POINT('Ctrl Pts',(8.52375553261478,6.63863721305422,-15.8472107628049)) ;
#110733 = CARTESIAN_POINT('Ctrl Pts',(8.52294204127162,6.63912232246439,-15.8461464560924)) ;
#110734 = CARTESIAN_POINT('Ctrl Pts',(8.52213801365707,6.63957834748689,-15.8450665375564)) ;
#110735 = CARTESIAN_POINT('Ctrl Pts',(8.52134774490512,6.64000494097979,-15.8439729614464)) ;
#110736 = CARTESIAN_POINT('Ctrl Pts',(8.51876608595598,6.64139854145541,-15.8404004545695)) ;
#110737 = CARTESIAN_POINT('Ctrl Pts',(8.51630176076719,6.64256282842068,-15.8366245667844)) ;
#110738 = CARTESIAN_POINT('Ctrl Pts',(8.51404737801022,6.64354662431173,-15.8326687582286)) ;
#110739 = CARTESIAN_POINT('Ctrl Pts',(8.51174271377018,6.64455236266853,-15.8286247197926)) ;
#110740 = CARTESIAN_POINT('Ctrl Pts',(8.50965863261302,6.64536892721963,-15.8243937780696)) ;
#110741 = CARTESIAN_POINT('Ctrl Pts',(8.50786496313903,6.64606338785378,-15.8200441654859)) ;
#110742 = CARTESIAN_POINT('Ctrl Pts',(8.50767015284864,6.64613881316472,-15.8195717544298)) ;
#110743 = CARTESIAN_POINT('Ctrl Pts',(8.50747873128293,6.64621281334902,-15.8190979736875)) ;
#110744 = CARTESIAN_POINT('Ctrl Pts',(8.50729076020857,6.64628549377757,-15.8186229301938)) ;
#110745 = CARTESIAN_POINT('Ctrl Pts',(8.50722027105568,6.64631274893828,-15.8184447888837)) ;
#110746 = CARTESIAN_POINT('Ctrl Pts',(8.50715026706478,6.64633981850992,-15.8182664700192)) ;
#110747 = CARTESIAN_POINT('Ctrl Pts',(8.50708075128542,6.6463667080633,-15.8180879793594)) ;
#110748 = CARTESIAN_POINT('Ctrl Pts',(8.50659414082988,6.6465549349369,-15.816838544741)) ;
#110749 = CARTESIAN_POINT('Ctrl Pts',(8.50613147592892,6.64673434010344,-15.815580683755)) ;
#110750 = CARTESIAN_POINT('Ctrl Pts',(8.50569363751095,6.64690683932496,-15.8143164275023)) ;
#110751 = CARTESIAN_POINT('Ctrl Pts',(8.50395436040201,6.64759207829665,-15.8092942735069)) ;
#110752 = CARTESIAN_POINT('Ctrl Pts',(8.50258205288293,6.64816393978924,-15.8040915596145)) ;
#110753 = CARTESIAN_POINT('Ctrl Pts',(8.50162662717129,6.64864720987501,-15.7988041247427)) ;
#110754 = CARTESIAN_POINT('Ctrl Pts',(8.50156399248209,6.64867889153404,-15.798457497228)) ;
#110755 = CARTESIAN_POINT('Ctrl Pts',(8.50150313499575,6.64871019935918,-15.7981105075157)) ;
#110756 = CARTESIAN_POINT('Ctrl Pts',(8.50144406283925,6.6487411427168,-15.797763183502)) ;
#110757 = CARTESIAN_POINT('Ctrl Pts',(8.50057491246561,6.64919642372274,-15.7926528774931)) ;
#110758 = CARTESIAN_POINT('Ctrl Pts',(8.50009537300568,6.64957062705855,-15.78747132905)) ;
#110759 = CARTESIAN_POINT('Ctrl Pts',(8.50001293997568,6.64989933182557,-15.782314443539)) ;
#110760 = CARTESIAN_POINT('Ctrl Pts',(8.50000430878269,6.64993374902799,-15.7817744891777)) ;
#110761 = CARTESIAN_POINT('Ctrl Pts',(8.5,6.649967656983,-15.7812348144276)) ;
#110762 = CARTESIAN_POINT('Ctrl Pts',(8.5,6.65000108682384,-15.7806955361059)) ;
#110763 = CARTESIAN_POINT('',(8.55245136877618,6.60097994372616,-15.8867801193795)) ;
#110764 = CARTESIAN_POINT('Ctrl Pts',(8.5523805647549,6.60105295171781,-15.8868886154986)) ;
#110765 = CARTESIAN_POINT('Ctrl Pts',(8.55170523171907,6.6030854236856,-15.8851022656148)) ;
#110766 = CARTESIAN_POINT('Ctrl Pts',(8.55095829520368,6.60513808680113,-15.8833627348222)) ;
#110767 = CARTESIAN_POINT('Ctrl Pts',(8.55012599030534,6.60719152980351,-15.8816544441816)) ;
#110768 = CARTESIAN_POINT('Ctrl Pts',(8.54968322947886,6.60828389886524,-15.8807456856517)) ;
#110769 = CARTESIAN_POINT('Ctrl Pts',(8.54921644930871,6.60937569995262,-15.8798462491235)) ;
#110770 = CARTESIAN_POINT('Ctrl Pts',(8.54872481267394,6.61045954913298,-15.8789557465494)) ;
#110771 = CARTESIAN_POINT('Ctrl Pts',(8.54779539897816,6.61250851009546,-15.8772722973719)) ;
#110772 = CARTESIAN_POINT('Ctrl Pts',(8.54677348694555,6.61453549290065,-15.8756155908862)) ;
#110773 = CARTESIAN_POINT('Ctrl Pts',(8.54565366748552,6.61650711946997,-15.8739653182917)) ;
#110774 = CARTESIAN_POINT('',(8.55735473176745,6.58264207262453,-15.9049557973616)) ;
#110775 = CARTESIAN_POINT('Ctrl Pts',(8.557354731687,6.58264207302789,-15.9049557968441)) ;
#110776 = CARTESIAN_POINT('Ctrl Pts',(8.55706916598052,6.58397660851271,-15.9032296933714)) ;
#110777 = CARTESIAN_POINT('Ctrl Pts',(8.55678088122702,6.58528501693262,-15.9016621009603)) ;
#110778 = CARTESIAN_POINT('Ctrl Pts',(8.55647408091819,6.58661569125896,-15.9001718232515)) ;
#110779 = CARTESIAN_POINT('Ctrl Pts',(8.55614409617577,6.58804692262413,-15.8985689275185)) ;
#110780 = CARTESIAN_POINT('Ctrl Pts',(8.55579261555186,6.5895052459012,-15.8970567950172)) ;
#110781 = CARTESIAN_POINT('Ctrl Pts',(8.55539993844502,6.59102291080544,-15.8955875677792)) ;
#110782 = CARTESIAN_POINT('Ctrl Pts',(8.55517214917305,6.59190329771266,-15.894735279227)) ;
#110783 = CARTESIAN_POINT('Ctrl Pts',(8.55493049881961,6.59280308289159,-15.8938983977538)) ;
#110784 = CARTESIAN_POINT('Ctrl Pts',(8.55467134659048,6.59372113732149,-15.8930707946419)) ;
#110785 = CARTESIAN_POINT('Ctrl Pts',(8.5543480523717,6.59486641664517,-15.8920383539702)) ;
#110786 = CARTESIAN_POINT('Ctrl Pts',(8.55400737519029,6.59602723165037,-15.8910361981957)) ;
#110787 = CARTESIAN_POINT('Ctrl Pts',(8.55365328858766,6.59718920061514,-15.8900452155133)) ;
#110788 = CARTESIAN_POINT('Ctrl Pts',(8.55328167888691,6.59840867329803,-15.889005190911)) ;
#110789 = CARTESIAN_POINT('Ctrl Pts',(8.55289390107693,6.59963546460028,-15.8879736796763)) ;
#110790 = CARTESIAN_POINT('Ctrl Pts',(8.55249886556661,6.60083562835457,-15.8869081494348)) ;
#110791 = CARTESIAN_POINT('Ctrl Pts',(8.55248304763317,6.60088368507324,-15.8868654836845)) ;
#110792 = CARTESIAN_POINT('Ctrl Pts',(8.55246721522809,6.60093179017222,-15.886822806733)) ;
#110793 = CARTESIAN_POINT('Ctrl Pts',(8.55245136877618,6.60097994372616,-15.8867801193795)) ;
#110794 = CARTESIAN_POINT('Ctrl Pts',(8.56107669735261,6.5600938800009,-16.0023838472224)) ;
#110795 = CARTESIAN_POINT('Ctrl Pts',(8.56115635543005,6.55978170524809,-16.0008207343832)) ;
#110796 = CARTESIAN_POINT('Ctrl Pts',(8.56122592915387,6.55950119162288,-15.9992507129806)) ;
#110797 = CARTESIAN_POINT('Ctrl Pts',(8.56128584055879,6.55925348717443,-15.9976933919487)) ;
#110798 = CARTESIAN_POINT('Ctrl Pts',(8.56142626445294,6.55867290283842,-15.9940432508109)) ;
#110799 = CARTESIAN_POINT('Ctrl Pts',(8.56152217534693,6.55825854507366,-15.9903756338769)) ;
#110800 = CARTESIAN_POINT('Ctrl Pts',(8.5615808174699,6.55798577878933,-15.9866701354253)) ;
#110801 = CARTESIAN_POINT('Ctrl Pts',(8.56158917845351,6.5579468887506,-15.9861418187432)) ;
#110802 = CARTESIAN_POINT('Ctrl Pts',(8.56159677639836,6.55791088241228,-15.9856126452595)) ;
#110803 = CARTESIAN_POINT('Ctrl Pts',(8.56160362608007,6.55787769947531,-15.9850824674717)) ;
#110804 = CARTESIAN_POINT('Ctrl Pts',(8.56164117305277,6.55769580506315,-15.982176263686)) ;
#110805 = CARTESIAN_POINT('Ctrl Pts',(8.56164095204357,6.55766773657216,-15.9792640119966)) ;
#110806 = CARTESIAN_POINT('Ctrl Pts',(8.56161306230089,6.55774920537472,-15.9763655672583)) ;
#110807 = CARTESIAN_POINT('Ctrl Pts',(8.56157759693122,6.55785280336172,-15.9726798246079)) ;
#110808 = CARTESIAN_POINT('Ctrl Pts',(8.5615027562466,6.55813669070952,-15.969004928021)) ;
#110809 = CARTESIAN_POINT('Ctrl Pts',(8.56141108129145,6.55856506509339,-15.9653632925482)) ;
#110810 = CARTESIAN_POINT('Ctrl Pts',(8.5613661599722,6.55877497130414,-15.963578867681)) ;
#110811 = CARTESIAN_POINT('Ctrl Pts',(8.56131707129297,6.55902016312284,-15.9618016709685)) ;
#110812 = CARTESIAN_POINT('Ctrl Pts',(8.56126585691691,6.55929956116447,-15.9600315254682)) ;
#110813 = CARTESIAN_POINT('Ctrl Pts',(8.56116752027492,6.55983603289968,-15.9566326719095)) ;
#110814 = CARTESIAN_POINT('Ctrl Pts',(8.56104954130216,6.56049109659204,-15.9532540075756)) ;
#110815 = CARTESIAN_POINT('Ctrl Pts',(8.56091150449775,6.56129147625803,-15.9498304710248)) ;
#110816 = CARTESIAN_POINT('Ctrl Pts',(8.56080235670743,6.56192434857304,-15.9471234288616)) ;
#110817 = CARTESIAN_POINT('Ctrl Pts',(8.56068045333715,6.56264902401852,-15.9443872666894)) ;
#110818 = CARTESIAN_POINT('Ctrl Pts',(8.56054379825319,6.56349285586897,-15.9416234877212)) ;
#110819 = CARTESIAN_POINT('Ctrl Pts',(8.56050762866484,6.56371619955867,-15.9408919763521)) ;
#110820 = CARTESIAN_POINT('Ctrl Pts',(8.56047042218818,6.56394794674722,-15.9401587916983)) ;
#110821 = CARTESIAN_POINT('Ctrl Pts',(8.5604321390176,6.56418871538696,-15.9394246234709)) ;
#110822 = CARTESIAN_POINT('Ctrl Pts',(8.56026887460239,6.56521550994376,-15.9362936511792)) ;
#110823 = CARTESIAN_POINT('Ctrl Pts',(8.56008532870545,6.56636514336275,-15.9332612149346)) ;
#110824 = CARTESIAN_POINT('Ctrl Pts',(8.5598891591871,6.56762686151827,-15.9304713276669)) ;
#110825 = CARTESIAN_POINT('Ctrl Pts',(8.55964574654527,6.56919243680269,-15.9270095572757)) ;
#110826 = CARTESIAN_POINT('Ctrl Pts',(8.55938661160132,6.57080906160865,-15.923732634051)) ;
#110827 = CARTESIAN_POINT('Ctrl Pts',(8.55911582090257,6.57246439798288,-15.920667212428)) ;
#110828 = CARTESIAN_POINT('Ctrl Pts',(8.55888928658553,6.5738491962671,-15.9181027846356)) ;
#110829 = CARTESIAN_POINT('Ctrl Pts',(8.55863813502893,6.57544444689309,-15.9153653454316)) ;
#110830 = CARTESIAN_POINT('Ctrl Pts',(8.55834707044213,6.57718152485361,-15.9126681258235)) ;
#110831 = CARTESIAN_POINT('Ctrl Pts',(8.55828762047115,6.57753632320085,-15.9121172184487)) ;
#110832 = CARTESIAN_POINT('Ctrl Pts',(8.55822651695173,6.5778969434577,-15.9115678465793)) ;
#110833 = CARTESIAN_POINT('Ctrl Pts',(8.55816364958867,6.57826264684155,-15.9110215710793)) ;
#110834 = CARTESIAN_POINT('Ctrl Pts',(8.55792499569721,6.57965091145837,-15.9089478277641)) ;
#110835 = CARTESIAN_POINT('Ctrl Pts',(8.5576603261423,6.58110993502786,-15.9069213132877)) ;
#110836 = CARTESIAN_POINT('Ctrl Pts',(8.55735473176745,6.58264207262453,-15.9049557973616)) ;
#110837 = CARTESIAN_POINT('Origin',(8.49172374697018,6.65,-17.78)) ;
#110838 = CARTESIAN_POINT('Origin',(8.4922693126432,6.63793757512217,-16.0129882716364)) ;
#110839 = CARTESIAN_POINT('Ctrl Pts',(8.40188506081761,6.5500005341705,-15.7515458308153)) ;
#110840 = CARTESIAN_POINT('Ctrl Pts',(8.5028074458744,6.54966497091121,-15.7651950407541)) ;
#110841 = CARTESIAN_POINT('Ctrl Pts',(8.50109204799972,6.65199687180764,-15.7656804549399)) ;
#110842 = CARTESIAN_POINT('Ctrl Pts',(8.3929693293079,6.55000052027914,-15.809675802422)) ;
#110843 = CARTESIAN_POINT('Ctrl Pts',(8.49725036372771,6.54968051003366,-15.7969136026831)) ;
#110844 = CARTESIAN_POINT('Ctrl Pts',(8.49665296516362,6.64935672317804,-15.7960247114635)) ;
#110845 = CARTESIAN_POINT('Ctrl Pts',(8.41146079558545,6.55000052635931,-15.869608884646)) ;
#110846 = CARTESIAN_POINT('Ctrl Pts',(8.50278789772742,6.54967384197881,-15.8210143519806)) ;
#110847 = CARTESIAN_POINT('Ctrl Pts',(8.50590954255545,6.65051247736746,-15.8244272120935)) ;
#110848 = CARTESIAN_POINT('Ctrl Pts',(8.4574451591417,6.55000045243508,-15.9228021918822)) ;
#110849 = CARTESIAN_POINT('Ctrl Pts',(8.5202381168081,6.54973725194854,-15.861633015821)) ;
#110850 = CARTESIAN_POINT('Ctrl Pts',(8.52891723073131,6.63643009777378,-15.8534751630783)) ;
#110851 = CARTESIAN_POINT('Ctrl Pts',(8.46608867121678,6.55000043643008,-15.9311950991748)) ;
#110852 = CARTESIAN_POINT('Ctrl Pts',(8.52334270167613,6.54974993059824,-15.868470240079)) ;
#110853 = CARTESIAN_POINT('Ctrl Pts',(8.53324349789231,6.63337968978884,-15.8582208913001)) ;
#110854 = CARTESIAN_POINT('Ctrl Pts',(8.48465388181683,6.55000038323734,-15.9465763138745)) ;
#110855 = CARTESIAN_POINT('Ctrl Pts',(8.53001210036429,6.54978938646809,-15.8851245951232)) ;
#110856 = CARTESIAN_POINT('Ctrl Pts',(8.54253954944034,6.62323710347996,-15.868863146269)) ;
#110857 = CARTESIAN_POINT('Ctrl Pts',(8.49467048074911,6.55000035131511,-15.9534884944614)) ;
#110858 = CARTESIAN_POINT('Ctrl Pts',(8.53347884787437,6.54981166882492,-15.89305903115)) ;
#110859 = CARTESIAN_POINT('Ctrl Pts',(8.5475533753473,6.6171479354886,-15.8728676881263)) ;
#110860 = CARTESIAN_POINT('Ctrl Pts',(8.50997930894003,6.55000022766094,-15.9633889027859)) ;
#110861 = CARTESIAN_POINT('Ctrl Pts',(8.53869035159217,6.54988741100163,-15.9187742327549)) ;
#110862 = CARTESIAN_POINT('Ctrl Pts',(8.55523846583762,6.59353839814627,-15.8935278831083)) ;
#110863 = CARTESIAN_POINT('Ctrl Pts',(8.51532901080101,6.5500001611307,-15.9663389673193)) ;
#110864 = CARTESIAN_POINT('Ctrl Pts',(8.54023459682686,6.54992340374042,-15.9284897483873)) ;
#110865 = CARTESIAN_POINT('Ctrl Pts',(8.55790835982308,6.58082417519535,-15.9015823085729)) ;
#110866 = CARTESIAN_POINT('Ctrl Pts',(8.52186010906342,6.55000005932357,-15.9727927598773)) ;
#110867 = CARTESIAN_POINT('Ctrl Pts',(8.54265823247975,6.54997327731409,-15.9579316441152)) ;
#110868 = CARTESIAN_POINT('Ctrl Pts',(8.56121746518601,6.56135337205752,-15.9445883700754)) ;
#110869 = CARTESIAN_POINT('Ctrl Pts',(8.52354993939967,6.55000003603139,-15.9758242622279)) ;
#110870 = CARTESIAN_POINT('Ctrl Pts',(8.54350769968238,6.54998394755847,-15.9714238732007)) ;
#110871 = CARTESIAN_POINT('Ctrl Pts',(8.5621431061544,6.55689632415131,-15.9674501335625)) ;
#110872 = CARTESIAN_POINT('Ctrl Pts',(8.52268461318107,6.55000004733862,-15.9817875304157)) ;
#110873 = CARTESIAN_POINT('Ctrl Pts',(8.54305517585921,6.54997881410036,-15.99281341214)) ;
#110874 = CARTESIAN_POINT('Ctrl Pts',(8.5615325917139,6.55906016573919,-16.0027901815805)) ;
#110875 = CARTESIAN_POINT('Ctrl Pts',(8.52060566253923,6.55000006807331,-15.9844138065496)) ;
#110876 = CARTESIAN_POINT('Ctrl Pts',(8.54195943530535,6.54996919659462,-16.0004945748859)) ;
#110877 = CARTESIAN_POINT('Ctrl Pts',(8.56058441628599,6.56302742363386,-16.0145079215137)) ;
#110878 = CARTESIAN_POINT('Ctrl Pts',(8.51445291480382,6.55000012130567,-15.9912328149552)) ;
#110879 = CARTESIAN_POINT('Ctrl Pts',(8.53868948987836,6.54994355920607,-16.0194191817675)) ;
#110880 = CARTESIAN_POINT('Ctrl Pts',(8.55750149922673,6.57320954252654,-16.0411844353069)) ;
#110881 = CARTESIAN_POINT('Ctrl Pts',(8.50953280296012,6.55000015625148,-15.9950479464372)) ;
#110882 = CARTESIAN_POINT('Ctrl Pts',(8.53616288920967,6.54992588038503,-16.0277647485266)) ;
#110883 = CARTESIAN_POINT('Ctrl Pts',(8.55504783006516,6.57989127253965,-16.0506993167928)) ;
#110884 = CARTESIAN_POINT('Ctrl Pts',(8.49261655785707,6.55000026291038,-16.0084926065689)) ;
#110885 = CARTESIAN_POINT('Ctrl Pts',(8.52778251455087,6.54986718408742,-16.0557691608947)) ;
#110886 = CARTESIAN_POINT('Ctrl Pts',(8.54658667616929,6.60027178071326,-16.0793533757438)) ;
#110887 = CARTESIAN_POINT('Ctrl Pts',(8.48022165824516,6.55000031608562,-16.0177685341604)) ;
#110888 = CARTESIAN_POINT('Ctrl Pts',(8.52288681814154,6.54983437262021,-16.0674559489292)) ;
#110889 = CARTESIAN_POINT('Ctrl Pts',(8.54045339450462,6.610423887593,-16.0863019909606)) ;
#110890 = CARTESIAN_POINT('Ctrl Pts',(8.46952991654744,6.55000035836673,-16.0290954462183)) ;
#110891 = CARTESIAN_POINT('Ctrl Pts',(8.51900842894269,6.54980714069599,-16.0833676846763)) ;
#110892 = CARTESIAN_POINT('Ctrl Pts',(8.53471369258699,6.61849392543639,-16.1013833684425)) ;
#110893 = CARTESIAN_POINT('Origin',(8.4,6.65,-15.7806780018997)) ;
#110894 = CARTESIAN_POINT('Ctrl Pts',(8.54848814460235,8.28374914930622,-14.4835371747799)) ;
#110895 = CARTESIAN_POINT('Ctrl Pts',(8.55964225199693,8.27720012980426,-14.4849679483223)) ;
#110896 = CARTESIAN_POINT('Ctrl Pts',(8.572140519951,8.27365818248462,-14.4857417625569)) ;
#110897 = CARTESIAN_POINT('Ctrl Pts',(8.54519582228985,8.29111303851996,-14.5079603788076)) ;
#110898 = CARTESIAN_POINT('Ctrl Pts',(8.55569959891137,8.28406912459881,-14.5080376174409)) ;
#110899 = CARTESIAN_POINT('Ctrl Pts',(8.56757951573628,8.27991709749371,-14.5081916339118)) ;
#110900 = CARTESIAN_POINT('Ctrl Pts',(8.54340782920288,8.28927570119136,-14.5338229931233)) ;
#110901 = CARTESIAN_POINT('Ctrl Pts',(8.55355053837511,8.28232618564301,-14.5321546442898)) ;
#110902 = CARTESIAN_POINT('Ctrl Pts',(8.56507848568421,8.27803412520747,-14.5311321430533)) ;
#110903 = CARTESIAN_POINT('Ctrl Pts',(8.54340835145922,8.27841951799441,-14.5555350111617)) ;
#110904 = CARTESIAN_POINT('Ctrl Pts',(8.55355093564017,8.27219257320284,-14.5524215387659)) ;
#110905 = CARTESIAN_POINT('Ctrl Pts',(8.56507848521152,8.26835005667905,-14.550500280504)) ;
#110906 = CARTESIAN_POINT('Ctrl Pts',(8.54742026180266,8.27608084857564,-14.5543656412486)) ;
#110907 = CARTESIAN_POINT('Ctrl Pts',(8.54754672558908,8.27683897030432,-14.5526745730365)) ;
#110908 = CARTESIAN_POINT('Ctrl Pts',(8.54766225486891,8.27755642830995,-14.5509654973084)) ;
#110909 = CARTESIAN_POINT('Ctrl Pts',(8.54776713596767,8.27823455672262,-14.5492350167776)) ;
#110910 = CARTESIAN_POINT('Ctrl Pts',(8.54791712013338,8.27920430747298,-14.5467603604118)) ;
#110911 = CARTESIAN_POINT('Ctrl Pts',(8.54806168001143,8.28008011045357,-14.5442463372674)) ;
#110912 = CARTESIAN_POINT('Ctrl Pts',(8.54818998754194,8.28086237513967,-14.5417186838585)) ;
#110913 = CARTESIAN_POINT('Ctrl Pts',(8.54824194926751,8.28117917511843,-14.5406950398664)) ;
#110914 = CARTESIAN_POINT('Ctrl Pts',(8.54829140719363,8.28148078264973,-14.5396686742902)) ;
#110915 = CARTESIAN_POINT('Ctrl Pts',(8.54833813644415,8.28176759858575,-14.5386396299772)) ;
#110916 = CARTESIAN_POINT('Ctrl Pts',(8.5485006132477,8.28276485268188,-14.5350616605292)) ;
#110917 = CARTESIAN_POINT('Ctrl Pts',(8.54863339756394,8.28360845633773,-14.5313501235293)) ;
#110918 = CARTESIAN_POINT('Ctrl Pts',(8.54873421749655,8.28426438239332,-14.5276130867584)) ;
#110919 = CARTESIAN_POINT('Ctrl Pts',(8.54878752953696,8.28461122607269,-14.5256369987946)) ;
#110920 = CARTESIAN_POINT('Ctrl Pts',(8.54883168679926,8.28490640714037,-14.523654082074)) ;
#110921 = CARTESIAN_POINT('Ctrl Pts',(8.54886500248133,8.28515040605085,-14.5216818590294)) ;
#110922 = CARTESIAN_POINT('Ctrl Pts',(8.54887385422351,8.28521523484358,-14.5211578532513)) ;
#110923 = CARTESIAN_POINT('Ctrl Pts',(8.54888411330031,8.285275121517,-14.5206350091922)) ;
#110924 = CARTESIAN_POINT('Ctrl Pts',(8.54889386083023,8.2853314308609,-14.5201120867862)) ;
#110925 = CARTESIAN_POINT('Ctrl Pts',(8.54894969070932,8.28565394783543,-14.5171170003469)) ;
#110926 = CARTESIAN_POINT('Ctrl Pts',(8.5489793513821,8.28586680424119,-14.514098636383)) ;
#110927 = CARTESIAN_POINT('Ctrl Pts',(8.54899968230029,8.28595875954336,-14.5110675778014)) ;
#110928 = CARTESIAN_POINT('Ctrl Pts',(8.54900356561227,8.28597632348829,-14.5104886297175)) ;
#110929 = CARTESIAN_POINT('Ctrl Pts',(8.54900713937599,8.28598945835116,-14.5099093088042)) ;
#110930 = CARTESIAN_POINT('Ctrl Pts',(8.54901057288909,8.2859980637762,-14.5093298402185)) ;
#110931 = CARTESIAN_POINT('Ctrl Pts',(8.54902784271198,8.28604134718934,-14.5064152394759)) ;
#110932 = CARTESIAN_POINT('Ctrl Pts',(8.54901619593281,8.28598556136223,-14.5035157757219)) ;
#110933 = CARTESIAN_POINT('Ctrl Pts',(8.54898431260111,8.28582669412323,-14.5006064286757)) ;
#110934 = CARTESIAN_POINT('Ctrl Pts',(8.54893914418925,8.2856016304144,-14.4964848209696)) ;
#110935 = CARTESIAN_POINT('Ctrl Pts',(8.54884805310402,8.28517290646441,-14.4923770999664)) ;
#110936 = CARTESIAN_POINT('Ctrl Pts',(8.54869940582912,8.28455561418415,-14.4883070774133)) ;
#110937 = CARTESIAN_POINT('Ctrl Pts',(8.54864697316335,8.28433787538047,-14.4868714498022)) ;
#110938 = CARTESIAN_POINT('Ctrl Pts',(8.54858736435354,8.28409676597413,-14.4854408395922)) ;
#110939 = CARTESIAN_POINT('Ctrl Pts',(8.54851996240545,8.28383343043592,-14.4840172030853)) ;
#110940 = CARTESIAN_POINT('Origin',(8.4,6.65,-17.78)) ;
#110941 = CARTESIAN_POINT('Origin',(8.4,6.65,-14.6993219981003)) ;
#110942 = CARTESIAN_POINT('Origin',(8.49172374697018,6.65,-17.78)) ;
#110943 = CARTESIAN_POINT('Origin',(8.49225485644025,6.63809817934705,-14.4670086283546)) ;
#110944 = CARTESIAN_POINT('Origin',(8.6,4.35421736843756,-14.6997127088383)) ;
#110945 = CARTESIAN_POINT('Origin',(8.6,6.66256607592813,-14.6997127088383)) ;
#110946 = CARTESIAN_POINT('Ctrl Pts',(8.5013487493624,6.65217253603386,-14.7159852560807)) ;
#110947 = CARTESIAN_POINT('Ctrl Pts',(8.50315244876585,6.54997127577019,-14.7165863692585)) ;
#110948 = CARTESIAN_POINT('Ctrl Pts',(8.4026944413366,6.55000000392136,-14.7315964965758)) ;
#110949 = CARTESIAN_POINT('Ctrl Pts',(8.49631753783951,6.64933701877093,-14.6850156523956)) ;
#110950 = CARTESIAN_POINT('Ctrl Pts',(8.49707874924869,6.54997270174421,-14.6839612234984)) ;
#110951 = CARTESIAN_POINT('Ctrl Pts',(8.39261127161985,6.55000000381175,-14.6725550208108)) ;
#110952 = CARTESIAN_POINT('Ctrl Pts',(8.50556246021206,6.65075235208957,-14.6560110455015)) ;
#110953 = CARTESIAN_POINT('Ctrl Pts',(8.50253957946711,6.54997202229479,-14.6596441304545)) ;
#110954 = CARTESIAN_POINT('Ctrl Pts',(8.41103525938989,6.55000000386643,-14.6113383496345)) ;
#110955 = CARTESIAN_POINT('Ctrl Pts',(8.52891970071471,6.63645479210458,-14.6265271584828)) ;
#110956 = CARTESIAN_POINT('Ctrl Pts',(8.52027792490147,6.54997752826669,-14.6184049399612)) ;
#110957 = CARTESIAN_POINT('Ctrl Pts',(8.4576425585103,6.5500000033157,-14.557390101583)) ;
#110958 = CARTESIAN_POINT('Ctrl Pts',(8.53324635448929,6.63340383613806,-14.6217820657382)) ;
#110959 = CARTESIAN_POINT('Ctrl Pts',(8.52338394863781,6.54997861189312,-14.6115733138909)) ;
#110960 = CARTESIAN_POINT('Ctrl Pts',(8.46627109069291,6.55000000319827,-14.5490047485327)) ;
#110961 = CARTESIAN_POINT('Ctrl Pts',(8.5425433201124,6.62325922024832,-14.6111417482178)) ;
#110962 = CARTESIAN_POINT('Ctrl Pts',(8.53005572430513,6.54998198465677,-14.5949326424681)) ;
#110963 = CARTESIAN_POINT('Ctrl Pts',(8.48480454940903,6.55000000280808,-14.5336278088231)) ;
#110964 = CARTESIAN_POINT('Ctrl Pts',(8.54755771953123,6.61716872587381,-14.6071385438774)) ;
#110965 = CARTESIAN_POINT('Ctrl Pts',(8.53352383957156,6.54998388968237,-14.5870066149148)) ;
#110966 = CARTESIAN_POINT('Ctrl Pts',(8.49480263348501,6.55000000257396,-14.5267172762992)) ;
#110967 = CARTESIAN_POINT('Ctrl Pts',(8.55524400651032,6.59355301617583,-14.5864805698954)) ;
#110968 = CARTESIAN_POINT('Ctrl Pts',(8.53873552501328,6.54999036710749,-14.5612948588094)) ;
#110969 = CARTESIAN_POINT('Ctrl Pts',(8.51008526949052,6.55000000166752,-14.5167757494185)) ;
#110970 = CARTESIAN_POINT('Ctrl Pts',(8.55791451833573,6.58083494429022,-14.5784270674639)) ;
#110971 = CARTESIAN_POINT('Ctrl Pts',(8.54027978136636,6.54999344602542,-14.5515790288343)) ;
#110972 = CARTESIAN_POINT('Ctrl Pts',(8.51542462880457,6.55000000118004,-14.5138063443386)) ;
#110973 = CARTESIAN_POINT('Ctrl Pts',(8.56122429319342,6.56135755929237,-14.5354165389634)) ;
#110974 = CARTESIAN_POINT('Ctrl Pts',(8.54270214007071,6.54999771321876,-14.5220999056442)) ;
#110975 = CARTESIAN_POINT('Ctrl Pts',(8.52194436340203,6.55000000043437,-14.5072674436739)) ;
#110976 = CARTESIAN_POINT('Ctrl Pts',(8.56215003896757,6.55689889598544,-14.5125513447562)) ;
#110977 = CARTESIAN_POINT('Ctrl Pts',(8.54355112280985,6.54999862629018,-14.5085854140215)) ;
#110978 = CARTESIAN_POINT('Ctrl Pts',(8.52363168464777,6.55000000026381,-14.5041937607945)) ;
#110979 = CARTESIAN_POINT('Ctrl Pts',(8.56153943432818,6.55906352913393,-14.4772061237909)) ;
#110980 = CARTESIAN_POINT('Ctrl Pts',(8.54309854033144,6.5499981870035,-14.4871631682685)) ;
#110981 = CARTESIAN_POINT('Ctrl Pts',(8.52276767133745,6.5500000003466,-14.49816751318)) ;
#110982 = CARTESIAN_POINT('Ctrl Pts',(8.56059123720043,6.56303220640812,-14.4654869464625)) ;
#110983 = CARTESIAN_POINT('Ctrl Pts',(8.54200379397878,6.54999736403672,-14.4794720470657)) ;
#110984 = CARTESIAN_POINT('Ctrl Pts',(8.52069177703238,6.55000000049844,-14.4955213437361)) ;
#110985 = CARTESIAN_POINT('Ctrl Pts',(8.55750819780173,6.57321782814892,-14.4388078145325)) ;
#110986 = CARTESIAN_POINT('Ctrl Pts',(8.53873610184734,6.54999517041881,-14.4605268596429)) ;
#110987 = CARTESIAN_POINT('Ctrl Pts',(8.51454797734041,6.55000000088831,-14.4886566308241)) ;
#110988 = CARTESIAN_POINT('Ctrl Pts',(8.55505442469283,6.5799017379831,-14.4292926744612)) ;
#110989 = CARTESIAN_POINT('Ctrl Pts',(8.53621107118182,6.54999365791211,-14.4521766604066)) ;
#110990 = CARTESIAN_POINT('Ctrl Pts',(8.50963525726155,6.5500000011443,-14.4848261829157)) ;
#110991 = CARTESIAN_POINT('Ctrl Pts',(8.55022399280474,6.59153973477788,-14.4129352059185)) ;
#110992 = CARTESIAN_POINT('Ctrl Pts',(8.53156015545169,6.54999086985382,-14.4366211671793)) ;
#110993 = CARTESIAN_POINT('Ctrl Pts',(8.49999539447557,6.55000000159032,-14.4771278236794)) ;
#110994 = CARTESIAN_POINT('Ctrl Pts',(8.54779538881609,6.59665349532942,-14.4069161916983)) ;
#110995 = CARTESIAN_POINT('Ctrl Pts',(8.5293657515114,6.54998957391999,-14.4299955473559)) ;
#110996 = CARTESIAN_POINT('Ctrl Pts',(8.49512741158075,6.55000000178643,-14.4733364158986)) ;
#110997 = CARTESIAN_POINT('Ctrl Pts',(8.54538355337156,6.6012117118503,-14.4016751744842)) ;
#110998 = CARTESIAN_POINT('Ctrl Pts',(8.52733415536173,6.54998837980797,-14.4238983572099)) ;
#110999 = CARTESIAN_POINT('Ctrl Pts',(8.49033880598513,6.55000000196131,-14.4694485970987)) ;
#111000 = CARTESIAN_POINT('',(8.54582344182381,6.6163536986167,-14.606063651573)) ;
#111001 = CARTESIAN_POINT('Ctrl Pts',(8.54582344182381,6.6163536986167,-14.606063651573)) ;
#111002 = CARTESIAN_POINT('Ctrl Pts',(8.54493595163518,6.61793460914655,-14.6073940762099)) ;
#111003 = CARTESIAN_POINT('Ctrl Pts',(8.5439844817107,6.61948114927954,-14.6087173928307)) ;
#111004 = CARTESIAN_POINT('Ctrl Pts',(8.54296332801272,6.6209780844369,-14.6100407367798)) ;
#111005 = CARTESIAN_POINT('Ctrl Pts',(8.53827263106763,6.62785429629763,-14.6161195527619)) ;
#111006 = CARTESIAN_POINT('Ctrl Pts',(8.53198779426187,6.63349037496299,-14.6226115685244)) ;
#111007 = CARTESIAN_POINT('Ctrl Pts',(8.5259873730411,6.63731070037229,-14.6300705892422)) ;
#111008 = CARTESIAN_POINT('Ctrl Pts',(8.52000560405467,6.64111915034781,-14.6375064236874)) ;
#111009 = CARTESIAN_POINT('Ctrl Pts',(8.51430181273566,6.64349626850742,-14.6460376473014)) ;
#111010 = CARTESIAN_POINT('Ctrl Pts',(8.50998586672548,6.64522349213896,-14.6552009869701)) ;
#111011 = CARTESIAN_POINT('Ctrl Pts',(8.50534188065424,6.64708199603772,-14.6650608002501)) ;
#111012 = CARTESIAN_POINT('Ctrl Pts',(8.50212992821339,6.64824261275105,-14.6758875436748)) ;
#111013 = CARTESIAN_POINT('Ctrl Pts',(8.50077314609738,6.64911992656046,-14.6868249119168)) ;
#111014 = CARTESIAN_POINT('Ctrl Pts',(8.50025986706873,6.64945181977648,-14.6909625856677)) ;
#111015 = CARTESIAN_POINT('Ctrl Pts',(8.50000017127793,6.64974165917873,-14.6951432551012)) ;
#111016 = CARTESIAN_POINT('Ctrl Pts',(8.5000000000847,6.64999974464545,-14.6993178674956)) ;
#111017 = CARTESIAN_POINT('',(8.55242393572493,6.60106172182544,-14.5932420987161)) ;
#111018 = CARTESIAN_POINT('Ctrl Pts',(8.55241775170034,6.60106807917178,-14.5932328161544)) ;
#111019 = CARTESIAN_POINT('Ctrl Pts',(8.55072388788561,6.6061902674336,-14.5977214769524)) ;
#111020 = CARTESIAN_POINT('Ctrl Pts',(8.5485829404857,6.61143812822775,-14.6019269241449)) ;
#111021 = CARTESIAN_POINT('Ctrl Pts',(8.54582344182381,6.6163536986167,-14.606063651573)) ;
#111022 = CARTESIAN_POINT('Ctrl Pts',(8.55635360773813,6.58637108369505,-14.5786323907338)) ;
#111023 = CARTESIAN_POINT('Ctrl Pts',(8.55606387390182,6.58765239867387,-14.5801123828075)) ;
#111024 = CARTESIAN_POINT('Ctrl Pts',(8.55575324501782,6.58896823902364,-14.5815659413336)) ;
#111025 = CARTESIAN_POINT('Ctrl Pts',(8.55541196992766,6.59037241127512,-14.5830432049404)) ;
#111026 = CARTESIAN_POINT('Ctrl Pts',(8.55524290008377,6.59106804711321,-14.5837750506995)) ;
#111027 = CARTESIAN_POINT('Ctrl Pts',(8.55506631250718,6.59178496983026,-14.5845119588377)) ;
#111028 = CARTESIAN_POINT('Ctrl Pts',(8.55488049708424,6.59252693597572,-14.585256277619)) ;
#111029 = CARTESIAN_POINT('Ctrl Pts',(8.55445908016381,6.59420966544528,-14.586944342709)) ;
#111030 = CARTESIAN_POINT('Ctrl Pts',(8.55403589309454,6.59584037906542,-14.5884883777225)) ;
#111031 = CARTESIAN_POINT('Ctrl Pts',(8.55359592981642,6.59737680581864,-14.5899031562334)) ;
#111032 = CARTESIAN_POINT('Ctrl Pts',(8.55324292160432,6.59860957066101,-14.591038315592)) ;
#111033 = CARTESIAN_POINT('Ctrl Pts',(8.55287861047121,6.59978201473825,-14.5920910425072)) ;
#111034 = CARTESIAN_POINT('Ctrl Pts',(8.55248933155914,6.60087815532547,-14.5930771269867)) ;
#111035 = CARTESIAN_POINT('Ctrl Pts',(8.55246754857564,6.60093949235551,-14.5931323055779)) ;
#111036 = CARTESIAN_POINT('Ctrl Pts',(8.55244574956029,6.60100068203154,-14.5931872962785)) ;
#111037 = CARTESIAN_POINT('Ctrl Pts',(8.55242393572493,6.60106172182544,-14.5932420987161)) ;
#111038 = CARTESIAN_POINT('Ctrl Pts',(8.5,6.66256607592813,-14.6997127088383)) ;
#111039 = CARTESIAN_POINT('Ctrl Pts',(8.5,6.66256607592813,-14.615)) ;
#111040 = CARTESIAN_POINT('Ctrl Pts',(8.58356010126947,6.66256607592813,-14.6010733164551)) ;
#111041 = CARTESIAN_POINT('Ctrl Pts',(8.5,6.61011302719822,-14.6997127072628)) ;
#111042 = CARTESIAN_POINT('Ctrl Pts',(8.50000000000005,6.63245216822976,-14.6185572365992)) ;
#111043 = CARTESIAN_POINT('Ctrl Pts',(8.57941760042981,6.63563981885127,-14.6017637332617)) ;
#111044 = CARTESIAN_POINT('Ctrl Pts',(8.5,6.55934573373326,-14.6788469099428)) ;
#111045 = CARTESIAN_POINT('Ctrl Pts',(8.5,6.60054351783578,-14.6080813958278)) ;
#111046 = CARTESIAN_POINT('Ctrl Pts',(8.57705842698407,6.60987578993433,-14.5917275280477)) ;
#111047 = CARTESIAN_POINT('Ctrl Pts',(8.5,6.52274941072028,-14.6422505892797)) ;
#111048 = CARTESIAN_POINT('Ctrl Pts',(8.5,6.57873105977929,-14.5862689402207)) ;
#111049 = CARTESIAN_POINT('Ctrl Pts',(8.57705842661295,6.59157413088145,-14.5734258691185)) ;
#111050 = CARTESIAN_POINT('Origin',(8.49172374697003,1.4,-17.78)) ;
#111051 = CARTESIAN_POINT('Origin',(8.49172374697003,1.4,-13.2778583129651)) ;
#111052 = CARTESIAN_POINT('Origin',(8.49172374697002,1.4,-13.2778583129651)) ;
#111053 = CARTESIAN_POINT('Origin',(8.49172374697003,1.4,-13.2778583129651)) ;
#111054 = CARTESIAN_POINT('Ctrl Pts',(8.50816364570057,1.49863939238321,-13.2778583129651)) ;
#111055 = CARTESIAN_POINT('Ctrl Pts',(8.51019246767907,1.4983012553868,-13.312927584071)) ;
#111056 = CARTESIAN_POINT('Ctrl Pts',(8.50816364570057,1.47636598119991,-13.3402920109583)) ;
#111057 = CARTESIAN_POINT('Ctrl Pts',(8.97755831131125,1.42040694811477,-13.2499486511544)) ;
#111058 = CARTESIAN_POINT('Ctrl Pts',(8.97879997398683,1.42020000433581,-13.2845666731845)) ;
#111059 = CARTESIAN_POINT('Ctrl Pts',(8.97755831689146,1.39869563385688,-13.311694816952)) ;
#111060 = CARTESIAN_POINT('Ctrl Pts',(9.44698496305968,1.34216917282337,-13.2226313706305)) ;
#111061 = CARTESIAN_POINT('Ctrl Pts',(9.44827639615881,1.3419539339721,-13.2567775286129)) ;
#111062 = CARTESIAN_POINT('Ctrl Pts',(9.44698496887879,1.32097764915795,-13.2837229847104)) ;
#111063 = CARTESIAN_POINT('Ctrl Pts',(9.91643989873053,1.26392668354489,-13.1958381198218)) ;
#111064 = CARTESIAN_POINT('Ctrl Pts',(9.91830968165731,1.2636150530571,-13.229509344197)) ;
#111065 = CARTESIAN_POINT('Ctrl Pts',(9.91643989873053,1.24322097942674,-13.256303564194)) ;
#111066 = CARTESIAN_POINT('Origin',(9.9,1.16528729116168,-13.1958381198218)) ;
#111067 = CARTESIAN_POINT('Origin',(9.9,1.16528729116168,-13.1958381198218)) ;
#111068 = CARTESIAN_POINT('Origin',(-0.4,-3.36847777691809,-15.64)) ;
#111069 = CARTESIAN_POINT('Origin',(-0.400000000000001,-3.36847777691809,
-15.64)) ;
#111070 = CARTESIAN_POINT('Origin',(-0.4,-3.36847777691809,-15.64)) ;
#111071 = CARTESIAN_POINT('Origin',(-0.400000000000001,-3.36847777691809,
-14.74)) ;
#111072 = CARTESIAN_POINT('Origin',(-0.4,-3.36847777691809,-14.84)) ;
#111073 = CARTESIAN_POINT('Origin',(-1.11032778078669,-3.36847777691809,-15.64)) ;
#111074 = CARTESIAN_POINT('Origin',(0.4,-3.36847777691809,-15.64)) ;
#111075 = CARTESIAN_POINT('Origin',(-0.400000000000001,-3.36847777691809,
-14.84)) ;
#111076 = CARTESIAN_POINT('Origin',(-0.4,-3.36847777691809,-14.84)) ;
#111077 = CARTESIAN_POINT('Origin',(0.400000000000001,-3.36847777691809,-15.64)) ;
#111078 = CARTESIAN_POINT('Origin',(0.400000000000001,-3.36847777691809,-15.64)) ;
#111079 = CARTESIAN_POINT('Origin',(1.5,-3.36847777691809,-14.84)) ;
#111080 = CARTESIAN_POINT('Origin',(0.4,-3.36847777691809,-14.84)) ;
#111081 = CARTESIAN_POINT('Origin',(0.4,-3.36847777691809,-14.74)) ;
#111082 = CARTESIAN_POINT('Origin',(0.4,-3.36847777691809,-14.84)) ;
#111083 = CARTESIAN_POINT('Origin',(0.4,-3.36847777691809,-14.84)) ;
#111084 = CARTESIAN_POINT('Origin',(7.96847777691809,3.4,-15.64)) ;
#111085 = CARTESIAN_POINT('Origin',(7.96847777691809,3.4,-15.64)) ;
#111086 = CARTESIAN_POINT('Origin',(7.96847777691809,3.4,-15.64)) ;
#111087 = CARTESIAN_POINT('Origin',(7.96847777691809,3.4,-14.74)) ;
#111088 = CARTESIAN_POINT('Origin',(7.96847777691809,3.4,-14.84)) ;
#111089 = CARTESIAN_POINT('Origin',(7.96847777691809,2.68967221921331,-15.64)) ;
#111090 = CARTESIAN_POINT('Origin',(7.96847777691809,4.2,-15.64)) ;
#111091 = CARTESIAN_POINT('Origin',(7.96847777691809,3.4,-14.84)) ;
#111092 = CARTESIAN_POINT('Origin',(7.96847777691809,3.4,-14.84)) ;
#111093 = CARTESIAN_POINT('Origin',(7.96847777691809,4.2,-15.64)) ;
#111094 = CARTESIAN_POINT('Origin',(7.96847777691809,4.2,-15.64)) ;
#111095 = CARTESIAN_POINT('Origin',(7.96847777691809,2.3,-14.84)) ;
#111096 = CARTESIAN_POINT('Origin',(7.96847777691809,4.2,-14.84)) ;
#111097 = CARTESIAN_POINT('Origin',(7.96847777691809,4.2,-14.74)) ;
#111098 = CARTESIAN_POINT('Origin',(7.96847777691809,4.2,-14.84)) ;
#111099 = CARTESIAN_POINT('Origin',(7.96847777691809,4.2,-14.84)) ;
#111100 = CARTESIAN_POINT('Origin',(8.49172374697003,1.4,-17.78)) ;
#111101 = CARTESIAN_POINT('Origin',(8.49172374697003,1.4,-17.2021416870349)) ;
#111102 = CARTESIAN_POINT('Origin',(8.49172374697002,1.4,-17.2021416870349)) ;
#111103 = CARTESIAN_POINT('Origin',(8.49172374697003,1.39999999999989,-17.2021416870347)) ;
#111104 = CARTESIAN_POINT('Ctrl Pts',(8.50816364570058,1.47636598119991,-17.1397079890417)) ;
#111105 = CARTESIAN_POINT('Ctrl Pts',(8.51019246767908,1.4983012553868,-17.167072415929)) ;
#111106 = CARTESIAN_POINT('Ctrl Pts',(8.50816364570058,1.49863939238321,-17.2021416870349)) ;
#111107 = CARTESIAN_POINT('Ctrl Pts',(8.9775583168915,1.39869563385713,-17.1683051830483)) ;
#111108 = CARTESIAN_POINT('Ctrl Pts',(8.97879997398667,1.42020000433563,-17.1954333268176)) ;
#111109 = CARTESIAN_POINT('Ctrl Pts',(8.97755831131135,1.42040694811475,-17.2300513488443)) ;
#111110 = CARTESIAN_POINT('Ctrl Pts',(9.44698496887878,1.32097764915799,-17.1962770152897)) ;
#111111 = CARTESIAN_POINT('Ctrl Pts',(9.4482763961588,1.34195393397339,-17.2232224713911)) ;
#111112 = CARTESIAN_POINT('Ctrl Pts',(9.44698496305964,1.34216917282337,-17.2573686293698)) ;
#111113 = CARTESIAN_POINT('Ctrl Pts',(9.91643989873053,1.24322097942674,-17.223696435806)) ;
#111114 = CARTESIAN_POINT('Ctrl Pts',(9.91830968165732,1.26361505305709,-17.250490655803)) ;
#111115 = CARTESIAN_POINT('Ctrl Pts',(9.91643989873053,1.26392668354489,-17.2841618801782)) ;
#111116 = CARTESIAN_POINT('Origin',(9.9,1.16528729116168,-17.2841618801782)) ;
#111117 = CARTESIAN_POINT('Origin',(9.9,1.16528729116168,-17.2841618801782)) ;
#111118 = CARTESIAN_POINT('Origin',(8.48377223398316,8.2,-17.78)) ;
#111119 = CARTESIAN_POINT('Origin',(8.48238055012102,8.20007134086553,-14.4931789299182)) ;
#111120 = CARTESIAN_POINT('Ctrl Pts',(8.40201662970149,8.3,-14.7259759779213)) ;
#111121 = CARTESIAN_POINT('Ctrl Pts',(8.50299337454948,8.3,-14.7126748112635)) ;
#111122 = CARTESIAN_POINT('Ctrl Pts',(8.50100123624931,8.19773961376461,-14.7126888461177)) ;
#111123 = CARTESIAN_POINT('Ctrl Pts',(8.3945412979896,8.3,-14.6744981813506)) ;
#111124 = CARTESIAN_POINT('Ctrl Pts',(8.4969787523768,8.3,-14.6853741113346)) ;
#111125 = CARTESIAN_POINT('Ctrl Pts',(8.49727262260755,8.20135231978531,-14.6850670639623)) ;
#111126 = CARTESIAN_POINT('Ctrl Pts',(8.40820218948345,8.3,-14.6220253635242)) ;
#111127 = CARTESIAN_POINT('Ctrl Pts',(8.49818669687003,8.3,-14.6624717278012)) ;
#111128 = CARTESIAN_POINT('Ctrl Pts',(8.50412619268405,8.20300739730713,-14.6603884100247)) ;
#111129 = CARTESIAN_POINT('Ctrl Pts',(8.44304134766321,8.3,-14.5709969330871)) ;
#111130 = CARTESIAN_POINT('Ctrl Pts',(8.50894174387209,8.3,-14.6208550553806)) ;
#111131 = CARTESIAN_POINT('Ctrl Pts',(8.52157716465941,8.21896555381605,-14.6301661266503)) ;
#111132 = CARTESIAN_POINT('Ctrl Pts',(8.44963266995283,8.3,-14.5626678319782)) ;
#111133 = CARTESIAN_POINT('Ctrl Pts',(8.51095981317517,8.3,-14.6137494404835)) ;
#111134 = CARTESIAN_POINT('Ctrl Pts',(8.52487915500777,8.22226238914488,-14.6249516180519)) ;
#111135 = CARTESIAN_POINT('Ctrl Pts',(8.46372306360151,8.3,-14.5469547263199)) ;
#111136 = CARTESIAN_POINT('Ctrl Pts',(8.51547368264944,8.3,-14.5976327910559)) ;
#111137 = CARTESIAN_POINT('Ctrl Pts',(8.53193863144478,8.23129792829965,-14.6133174783855)) ;
#111138 = CARTESIAN_POINT('Ctrl Pts',(8.47128983770084,8.3,-14.5395586271464)) ;
#111139 = CARTESIAN_POINT('Ctrl Pts',(8.5179623704237,8.3,-14.5892464949127)) ;
#111140 = CARTESIAN_POINT('Ctrl Pts',(8.53572833262715,8.2367734386236,-14.6074295885077)) ;
#111141 = CARTESIAN_POINT('Ctrl Pts',(8.48287565264706,8.3,-14.5287307948332)) ;
#111142 = CARTESIAN_POINT('Ctrl Pts',(8.52168214469875,8.3,-14.57074351943)) ;
#111143 = CARTESIAN_POINT('Ctrl Pts',(8.54153766811345,8.25077321967987,-14.5920449871074)) ;
#111144 = CARTESIAN_POINT('Ctrl Pts',(8.48680760428677,8.3,-14.525187297402)) ;
#111145 = CARTESIAN_POINT('Ctrl Pts',(8.52287759291297,8.3,-14.5641435049317)) ;
#111146 = CARTESIAN_POINT('Ctrl Pts',(8.54350322705384,8.2564691763754,-14.5862622666034)) ;
#111147 = CARTESIAN_POINT('Ctrl Pts',(8.49230810302881,8.3,-14.5194953499955)) ;
#111148 = CARTESIAN_POINT('Ctrl Pts',(8.52426411271138,8.3,-14.5485665246336)) ;
#111149 = CARTESIAN_POINT('Ctrl Pts',(8.54627296401923,8.26866384868898,-14.5685525693616)) ;
#111150 = CARTESIAN_POINT('Ctrl Pts',(8.49410170711667,8.3,-14.517526518934)) ;
#111151 = CARTESIAN_POINT('Ctrl Pts',(8.52463604790914,8.3,-14.5424055253652)) ;
#111152 = CARTESIAN_POINT('Ctrl Pts',(8.54716490137964,8.27360757863439,-14.5607959594826)) ;
#111153 = CARTESIAN_POINT('Ctrl Pts',(8.49698869685298,8.3,-14.5130732788095)) ;
#111154 = CARTESIAN_POINT('Ctrl Pts',(8.52523118911551,8.3,-14.5265929344383)) ;
#111155 = CARTESIAN_POINT('Ctrl Pts',(8.54862931231184,8.28262305001771,-14.5378413492704)) ;
#111156 = CARTESIAN_POINT('Ctrl Pts',(8.4979868777125,8.3,-14.5105165211566)) ;
#111157 = CARTESIAN_POINT('Ctrl Pts',(8.52551930315386,8.3,-14.5169062760438)) ;
#111158 = CARTESIAN_POINT('Ctrl Pts',(8.54912969489065,8.28574379441723,-14.5223818974932)) ;
#111159 = CARTESIAN_POINT('Ctrl Pts',(8.49821791151748,8.3,-14.5025795709374)) ;
#111160 = CARTESIAN_POINT('Ctrl Pts',(8.52559423327562,8.3,-14.4921891247049)) ;
#111161 = CARTESIAN_POINT('Ctrl Pts',(8.54922875625408,8.28635135062007,-14.4832386700469)) ;
#111162 = CARTESIAN_POINT('Ctrl Pts',(8.49537847603514,8.3,-14.4976469108458)) ;
#111163 = CARTESIAN_POINT('Ctrl Pts',(8.5243933105344,8.3,-14.4814732749821)) ;
#111164 = CARTESIAN_POINT('Ctrl Pts',(8.54781890418529,8.2804054867288,-14.468471793372)) ;
#111165 = CARTESIAN_POINT('Ctrl Pts',(8.48955273785442,8.3,-14.4889114034569)) ;
#111166 = CARTESIAN_POINT('Ctrl Pts',(8.52168703568126,8.29999999999999,-14.4640525851282)) ;
#111167 = CARTESIAN_POINT('Ctrl Pts',(8.54489815533715,8.27194212599122,-14.4461670077071)) ;
#111168 = CARTESIAN_POINT('Ctrl Pts',(8.48620077197361,8.3,-14.4848263075048)) ;
#111169 = CARTESIAN_POINT('Ctrl Pts',(8.52012703453236,8.30000000000001,-14.4571073328933)) ;
#111170 = CARTESIAN_POINT('Ctrl Pts',(8.54324008387895,8.26788967346963,-14.4383142356384)) ;
#111171 = CARTESIAN_POINT('Ctrl Pts',(8.48280151347419,8.3,-14.4807911096407)) ;
#111172 = CARTESIAN_POINT('Ctrl Pts',(8.51858761497412,8.3,-14.4506520257852)) ;
#111173 = CARTESIAN_POINT('Ctrl Pts',(8.54152015125555,8.26408224232382,-14.4313382250347)) ;
#111174 = CARTESIAN_POINT('Origin',(8.4,8.2,-14.697927110149)) ;
#111175 = CARTESIAN_POINT('Origin',(8.4,8.2,-15.865)) ;
#111176 = CARTESIAN_POINT('Origin',(8.4,8.2,-15.782072889851)) ;
#111177 = CARTESIAN_POINT('Ctrl Pts',(8.50101530037395,8.19768718256762,-15.7672017745814)) ;
#111178 = CARTESIAN_POINT('Ctrl Pts',(8.50305639000873,8.3,-15.7672198113572)) ;
#111179 = CARTESIAN_POINT('Ctrl Pts',(8.40204633857705,8.3,-15.7538202021254)) ;
#111180 = CARTESIAN_POINT('Ctrl Pts',(8.49725464441632,8.20131038948436,-15.7948679119096)) ;
#111181 = CARTESIAN_POINT('Ctrl Pts',(8.49701391805272,8.3,-15.7945609423404)) ;
#111182 = CARTESIAN_POINT('Ctrl Pts',(8.39450526457597,8.3,-15.8053632910712)) ;
#111183 = CARTESIAN_POINT('Ctrl Pts',(8.5041093504131,8.20295267265881,-15.8195792968114)) ;
#111184 = CARTESIAN_POINT('Ctrl Pts',(8.498207495215,8.3,-15.8174643378906)) ;
#111185 = CARTESIAN_POINT('Ctrl Pts',(8.40816401923481,8.3,-15.8579187290434)) ;
#111186 = CARTESIAN_POINT('Ctrl Pts',(8.52158236570989,8.21893216789649,-15.8498300407758)) ;
#111187 = CARTESIAN_POINT('Ctrl Pts',(8.50896456566521,8.3,-15.8591276783841)) ;
#111188 = CARTESIAN_POINT('Ctrl Pts',(8.44304134766321,8.3,-15.9090030669129)) ;
#111189 = CARTESIAN_POINT('Ctrl Pts',(8.5248849650705,8.22222991631201,-15.8550437061782)) ;
#111190 = CARTESIAN_POINT('Ctrl Pts',(8.51098076140206,8.3,-15.8662331109763)) ;
#111191 = CARTESIAN_POINT('Ctrl Pts',(8.44963266995282,8.3,-15.9173321680218)) ;
#111192 = CARTESIAN_POINT('Ctrl Pts',(8.53194575580938,8.23126818558572,-15.8666757349666)) ;
#111193 = CARTESIAN_POINT('Ctrl Pts',(8.51549074202138,8.3,-15.8823505031351)) ;
#111194 = CARTESIAN_POINT('Ctrl Pts',(8.46372306360152,8.3,-15.9330452736801)) ;
#111195 = CARTESIAN_POINT('Ctrl Pts',(8.53573618291037,8.23674548871788,-15.8725623770273)) ;
#111196 = CARTESIAN_POINT('Ctrl Pts',(8.51797743940283,8.3,-15.8907374625586)) ;
#111197 = CARTESIAN_POINT('Ctrl Pts',(8.47128983770083,8.3,-15.9404413728536)) ;
#111198 = CARTESIAN_POINT('Ctrl Pts',(8.54154687836688,8.25075037830458,-15.8879451319455)) ;
#111199 = CARTESIAN_POINT('Ctrl Pts',(8.52169408444524,8.3,-15.9092435543493)) ;
#111200 = CARTESIAN_POINT('Ctrl Pts',(8.48287565264706,8.3,-15.9512692051668)) ;
#111201 = CARTESIAN_POINT('Ctrl Pts',(8.54351297666181,8.25644859419422,-15.8937272780162)) ;
#111202 = CARTESIAN_POINT('Ctrl Pts',(8.52288848488736,8.3,-15.9158447315488)) ;
#111203 = CARTESIAN_POINT('Ctrl Pts',(8.48680760428676,8.3,-15.954812702598)) ;
#111204 = CARTESIAN_POINT('Ctrl Pts',(8.54628376412584,8.26864846827403,-15.9114376231601)) ;
#111205 = CARTESIAN_POINT('Ctrl Pts',(8.52427341038692,8.3,-15.9314250170403)) ;
#111206 = CARTESIAN_POINT('Ctrl Pts',(8.4923081030288,8.3,-15.9605046500045)) ;
#111207 = CARTESIAN_POINT('Ctrl Pts',(8.54717611873857,8.27359443500938,-15.9191948837187)) ;
#111208 = CARTESIAN_POINT('Ctrl Pts',(8.52464480444821,8.3,-15.9375873399142)) ;
#111209 = CARTESIAN_POINT('Ctrl Pts',(8.49410170711667,8.3,-15.962473481066)) ;
#111210 = CARTESIAN_POINT('Ctrl Pts',(8.54864126180654,8.28261417405722,-15.9421529061248)) ;
#111211 = CARTESIAN_POINT('Ctrl Pts',(8.52523908688552,8.3,-15.9534032849063)) ;
#111212 = CARTESIAN_POINT('Ctrl Pts',(8.49698869685298,8.3,-15.9669267211905)) ;
#111213 = CARTESIAN_POINT('Ctrl Pts',(8.5491418548716,8.28573645090425,-15.9576152824162)) ;
#111214 = CARTESIAN_POINT('Ctrl Pts',(8.52552693815802,8.3,-15.9630919520163)) ;
#111215 = CARTESIAN_POINT('Ctrl Pts',(8.49798687771249,8.3,-15.9694834788434)) ;
#111216 = CARTESIAN_POINT('Ctrl Pts',(8.54924094958847,8.28634430798885,-15.9967659475983)) ;
#111217 = CARTESIAN_POINT('Ctrl Pts',(8.52560181204939,8.3,-15.9878137517531)) ;
#111218 = CARTESIAN_POINT('Ctrl Pts',(8.49821791151747,8.3,-15.9774204290626)) ;
#111219 = CARTESIAN_POINT('Ctrl Pts',(8.54783079466743,8.28039553911293,-16.0115348059813)) ;
#111220 = CARTESIAN_POINT('Ctrl Pts',(8.52440147378976,8.3,-15.9985312754323)) ;
#111221 = CARTESIAN_POINT('Ctrl Pts',(8.49537847603514,8.3,-15.9823530891542)) ;
#111222 = CARTESIAN_POINT('Ctrl Pts',(8.54465883986931,8.27120119512637,-16.0357571947032)) ;
#111223 = CARTESIAN_POINT('Ctrl Pts',(8.52145785975945,8.3,-16.0174902783301)) ;
#111224 = CARTESIAN_POINT('Ctrl Pts',(8.48905244827038,8.3,-15.9918387647145)) ;
#111225 = CARTESIAN_POINT('Ctrl Pts',(8.54267599402786,8.26648669506697,-16.0442949904305)) ;
#111226 = CARTESIAN_POINT('Ctrl Pts',(8.51958784692425,8.3,-16.0252641321447)) ;
#111227 = CARTESIAN_POINT('Ctrl Pts',(8.48503640902804,8.3,-15.9965685970659)) ;
#111228 = CARTESIAN_POINT('Ctrl Pts',(8.54064021294342,8.26212437554839,-16.0522000298239)) ;
#111229 = CARTESIAN_POINT('Ctrl Pts',(8.51779796763698,8.3,-16.0326895170151)) ;
#111230 = CARTESIAN_POINT('Ctrl Pts',(8.48104783026775,8.3,-16.0012848074951)) ;
#111231 = CARTESIAN_POINT('Origin',(8.4823805486149,8.20007133319196,-15.9868210687046)) ;
#111232 = CARTESIAN_POINT('Origin',(8.48377223398316,8.2,-17.78)) ;
#111233 = CARTESIAN_POINT('Ctrl Pts',(8.55305389383868,6.58518362856711,-19.6598163714329)) ;
#111234 = CARTESIAN_POINT('Ctrl Pts',(8.56447181517253,6.58947636230805,-19.6555236376919)) ;
#111235 = CARTESIAN_POINT('Ctrl Pts',(8.57705842661295,6.59157413088145,-19.6534258691185)) ;
#111236 = CARTESIAN_POINT('Ctrl Pts',(8.55305102515203,6.55898702014122,-19.6336204597774)) ;
#111237 = CARTESIAN_POINT('Ctrl Pts',(8.56446969712857,6.56479854221787,-19.6308465230911)) ;
#111238 = CARTESIAN_POINT('Ctrl Pts',(8.57705842709774,6.56766897765924,-19.6295207157347)) ;
#111239 = CARTESIAN_POINT('Ctrl Pts',(8.55608440539073,6.54967077654141,-19.5934724260347)) ;
#111240 = CARTESIAN_POINT('Ctrl Pts',(8.56803673427362,6.55578248257734,-19.5931311242349)) ;
#111241 = CARTESIAN_POINT('Ctrl Pts',(8.58110225049762,6.55837193275,-19.5932648466505)) ;
#111242 = CARTESIAN_POINT('Ctrl Pts',(8.56106007075016,6.56033186051354,-19.5569784615962)) ;
#111243 = CARTESIAN_POINT('Ctrl Pts',(8.57385418571952,6.56560017282096,-19.5582038837617)) ;
#111244 = CARTESIAN_POINT('Ctrl Pts',(8.58763814880121,6.56727264871055,-19.5585929056925)) ;
#111245 = CARTESIAN_POINT('',(8.56104219912065,6.56017369985344,-19.5576338509444)) ;
#111246 = CARTESIAN_POINT('',(8.55704445183397,6.58320973295693,-19.6548316411919)) ;
#111247 = CARTESIAN_POINT('Ctrl Pts',(8.56104219912065,6.56017369985344,-19.5576338509444)) ;
#111248 = CARTESIAN_POINT('Ctrl Pts',(8.56172006948825,6.55755272988493,-19.5705099834262)) ;
#111249 = CARTESIAN_POINT('Ctrl Pts',(8.56178854742204,6.55691761311389,-19.5840188634591)) ;
#111250 = CARTESIAN_POINT('Ctrl Pts',(8.56147572200372,6.55855061087387,-19.5970710371545)) ;
#111251 = CARTESIAN_POINT('Ctrl Pts',(8.56116227470662,6.56018685493862,-19.6101491578135)) ;
#111252 = CARTESIAN_POINT('Ctrl Pts',(8.5604843297899,6.56417103596015,-19.6231290791339)) ;
#111253 = CARTESIAN_POINT('Ctrl Pts',(8.55945615587251,6.57017322470283,-19.6348222126965)) ;
#111254 = CARTESIAN_POINT('Ctrl Pts',(8.55883284154062,6.57381195760855,-19.6419109917552)) ;
#111255 = CARTESIAN_POINT('Ctrl Pts',(8.55807185541711,6.57823677723133,-19.6486350483951)) ;
#111256 = CARTESIAN_POINT('Ctrl Pts',(8.55704487707431,6.58320791316478,-19.6548324621192)) ;
#111257 = CARTESIAN_POINT('',(8.55635403291171,6.58636921675995,-19.6586302321744)) ;
#111258 = CARTESIAN_POINT('Origin',(8.54420290085246,6.6281733092357,-19.6219411204917)) ;
#111259 = CARTESIAN_POINT('',(8.57705842661295,6.59157413088145,-19.6534258691185)) ;
#111260 = CARTESIAN_POINT('Origin',(8.6,6.52274941072028,-19.7222505892797)) ;
#111261 = CARTESIAN_POINT('',(8.58355189313841,6.56397635572684,-19.582433776426)) ;
#111262 = CARTESIAN_POINT('Origin',(8.59777129281795,6.65641294722127,-19.5808822359315)) ;
#111263 = CARTESIAN_POINT('Ctrl Pts',(8.56104311409705,6.56017375480329,-19.5576348093723)) ;
#111264 = CARTESIAN_POINT('Ctrl Pts',(8.56569547918965,6.56094902085081,-19.5631223861694)) ;
#111265 = CARTESIAN_POINT('Ctrl Pts',(8.57049938306333,6.56176641478979,-19.5685092513474)) ;
#111266 = CARTESIAN_POINT('Ctrl Pts',(8.57538893105716,6.56259599225628,-19.5737862661385)) ;
#111267 = CARTESIAN_POINT('Ctrl Pts',(8.57808773793835,6.56305388107911,-19.576698936972)) ;
#111268 = CARTESIAN_POINT('Ctrl Pts',(8.58081254036867,6.56351521010419,-19.5795793793677)) ;
#111269 = CARTESIAN_POINT('Ctrl Pts',(8.58355195315297,6.56397636517831,-19.5824336197205)) ;
#111270 = CARTESIAN_POINT('Ctrl Pts',(8.5,8.3521616921714,-19.6724060982502)) ;
#111271 = CARTESIAN_POINT('Ctrl Pts',(8.5,8.2900428850829,-19.641346694706)) ;
#111272 = CARTESIAN_POINT('Ctrl Pts',(8.56507848521152,8.26835005667905,-19.630500280504)) ;
#111273 = CARTESIAN_POINT('Ctrl Pts',(8.5,8.31945293993537,-19.7378235972687)) ;
#111274 = CARTESIAN_POINT('Ctrl Pts',(8.5,8.26922013491147,-19.6829921887968)) ;
#111275 = CARTESIAN_POINT('Ctrl Pts',(8.56507848600994,8.25199117628908,-19.6632180406186)) ;
#111276 = CARTESIAN_POINT('Ctrl Pts',(8.5,8.24922766844392,-19.7797127068513)) ;
#111277 = CARTESIAN_POINT('Ctrl Pts',(8.5,8.21777561643124,-19.7044773698221)) ;
#111278 = CARTESIAN_POINT('Ctrl Pts',(8.57228151929428,8.2145120273235,-19.6829530801176)) ;
#111279 = CARTESIAN_POINT('Ctrl Pts',(8.5,8.17221734381475,-19.7797127088383)) ;
#111280 = CARTESIAN_POINT('Ctrl Pts',(8.5,8.17221734381475,-19.695)) ;
#111281 = CARTESIAN_POINT('Ctrl Pts',(8.58356010126947,8.17221734381475,-19.6810733164551)) ;
#111282 = CARTESIAN_POINT('',(8.50000000249538,8.20000280433619,-19.7779047436384)) ;
#111283 = CARTESIAN_POINT('',(8.54742025481395,8.27608084305204,-19.6343656619559)) ;
#111284 = CARTESIAN_POINT('Ctrl Pts',(8.50000000249538,8.20000280433619,-19.7779047436384)) ;
#111285 = CARTESIAN_POINT('Ctrl Pts',(8.50000274011724,8.2015414376578,-19.7656354484511)) ;
#111286 = CARTESIAN_POINT('Ctrl Pts',(8.50225788919789,8.20358050335012,-19.7532664749796)) ;
#111287 = CARTESIAN_POINT('Ctrl Pts',(8.50614710304112,8.20657022673326,-19.7419159810139)) ;
#111288 = CARTESIAN_POINT('Ctrl Pts',(8.51002595055128,8.20955198129041,-19.7305957407205)) ;
#111289 = CARTESIAN_POINT('Ctrl Pts',(8.51564213392183,8.21362262975068,-19.7200461335207)) ;
#111290 = CARTESIAN_POINT('Ctrl Pts',(8.52129493663065,8.21921832196825,-19.710621792234)) ;
#111291 = CARTESIAN_POINT('Ctrl Pts',(8.52933132065201,8.22717351408127,-19.6972235489855)) ;
#111292 = CARTESIAN_POINT('Ctrl Pts',(8.53683691159804,8.23885362788864,-19.6856624434434)) ;
#111293 = CARTESIAN_POINT('Ctrl Pts',(8.54097226482464,8.25011947738646,-19.6728811696171)) ;
#111294 = CARTESIAN_POINT('Ctrl Pts',(8.54447125915462,8.25965170869904,-19.6620667114082)) ;
#111295 = CARTESIAN_POINT('Ctrl Pts',(8.54617119150717,8.26873789958222,-19.6499396101897)) ;
#111296 = CARTESIAN_POINT('Ctrl Pts',(8.54724932284106,8.27506683274844,-19.6365664602513)) ;
#111297 = CARTESIAN_POINT('Ctrl Pts',(8.54730817192851,8.27541229338911,-19.6358364956863)) ;
#111298 = CARTESIAN_POINT('Ctrl Pts',(8.54736510616621,8.27575037116516,-19.635102832606)) ;
#111299 = CARTESIAN_POINT('Ctrl Pts',(8.54742024083733,8.27608084608571,-19.6343656752073)) ;
#111300 = CARTESIAN_POINT('',(8.56507848521152,8.26835005667905,-19.630500280504)) ;
#111301 = CARTESIAN_POINT('Origin',(8.6,8.3521616921714,-19.6724060982502)) ;
#111302 = CARTESIAN_POINT('',(8.58356010126947,8.17221734381475,-19.6810733164551)) ;
#111303 = CARTESIAN_POINT('Origin',(8.59670327708558,8.16883734299673,-19.5870689695193)) ;
#111304 = CARTESIAN_POINT('',(8.5,8.17221734381475,-19.7797127088383)) ;
#111305 = CARTESIAN_POINT('Origin',(8.6,8.17221734381475,-19.7797127088383)) ;
#111306 = CARTESIAN_POINT('Origin',(8.5,8.1664264877272,-19.5571077523216)) ;
#111307 = CARTESIAN_POINT('Origin',(2.9,3.8,-20.32)) ;
#111308 = CARTESIAN_POINT('',(3.,2.4,-20.32)) ;
#111309 = CARTESIAN_POINT('Origin',(3.,3.8,-20.32)) ;
#111310 = CARTESIAN_POINT('',(2.9,2.3,-20.32)) ;
#111311 = CARTESIAN_POINT('Origin',(2.9,2.4,-20.32)) ;
#111312 = CARTESIAN_POINT('Origin',(2.9,3.8,-20.32)) ;
#111313 = CARTESIAN_POINT('Origin',(1.35,3.8,-20.32)) ;
#111314 = CARTESIAN_POINT('',(1.35,2.3,-20.32)) ;
#111315 = CARTESIAN_POINT('Origin',(1.35,3.8,-20.32)) ;
#111316 = CARTESIAN_POINT('',(1.25,2.2,-20.32)) ;
#111317 = CARTESIAN_POINT('Origin',(1.35,2.2,-20.32)) ;
#111318 = CARTESIAN_POINT('Origin',(1.25,3.8,-20.32)) ;
#111319 = CARTESIAN_POINT('Origin',(13.9153543900904,1.02736587339764,-19.47)) ;
#111320 = CARTESIAN_POINT('',(1.15,1.02736587339764,-19.57)) ;
#111321 = CARTESIAN_POINT('',(1.15,0.931757800066529,-19.4406896551724)) ;
#111322 = CARTESIAN_POINT('Origin',(1.15,1.02736587339764,-19.47)) ;
#111323 = CARTESIAN_POINT('',(-0.900000000000002,1.02736587339765,-19.57)) ;
#111324 = CARTESIAN_POINT('',(-1.,1.02736587339765,-19.57)) ;
#111325 = CARTESIAN_POINT('',(-0.900000000000002,0.982644513847654,-19.5594427191)) ;
#111326 = CARTESIAN_POINT('Origin',(-0.900000000000002,1.02736587339765,-19.47)) ;
#111327 = CARTESIAN_POINT('',(-0.900000000000002,0.93175780006653,-19.4406896551724)) ;
#111328 = CARTESIAN_POINT('Origin',(-0.900000000000002,1.02736587339765,-19.47)) ;
#111329 = CARTESIAN_POINT('',(13.9153543900904,0.931757800066525,-19.4406896551724)) ;
#111330 = CARTESIAN_POINT('Origin',(13.9153543900904,1.02736587339764,-21.17)) ;
#111331 = CARTESIAN_POINT('',(1.15,0.93175780006653,-21.1993103448276)) ;
#111332 = CARTESIAN_POINT('',(1.15,1.02736587339765,-21.07)) ;
#111333 = CARTESIAN_POINT('Origin',(1.15,1.02736587339765,-21.17)) ;
#111334 = CARTESIAN_POINT('',(-0.900000000000002,0.931757800066531,-21.1993103448276)) ;
#111335 = CARTESIAN_POINT('',(13.9153543900904,0.931757800066525,-21.1993103448276)) ;
#111336 = CARTESIAN_POINT('',(-0.900000000000002,1.02736587339765,-21.07)) ;
#111337 = CARTESIAN_POINT('Origin',(-0.900000000000002,1.02736587339765,-21.17)) ;
#111338 = CARTESIAN_POINT('',(-1.,1.02736587339765,-21.07)) ;
#111339 = CARTESIAN_POINT('Origin',(8.49172374697003,3.8,-20.32)) ;
#111340 = CARTESIAN_POINT('',(8.49172374697003,1.47741935483871,-18.4211532060953)) ;
#111341 = CARTESIAN_POINT('',(8.49172374697003,1.47741935483871,-22.2188467939047)) ;
#111342 = CARTESIAN_POINT('Origin',(8.49172374697003,3.8,-20.32)) ;
#111343 = CARTESIAN_POINT('',(8.50816364570057,1.47636598119991,-18.4202920109583)) ;
#111344 = CARTESIAN_POINT('Origin',(8.49172374697003,1.4,-18.3578583129651)) ;
#111345 = CARTESIAN_POINT('',(8.50816364570057,1.47636598119991,-22.2197079890417)) ;
#111346 = CARTESIAN_POINT('Origin',(8.50816364570057,3.8,-20.32)) ;
#111347 = CARTESIAN_POINT('Origin',(8.49172374697003,1.4,-22.2821416870349)) ;
#111348 = CARTESIAN_POINT('Origin',(1.25,3.8,-20.32)) ;
#111349 = CARTESIAN_POINT('',(1.25,2.3,-20.32)) ;
#111350 = CARTESIAN_POINT('Origin',(13.9153543900904,3.8,-20.32)) ;
#111351 = CARTESIAN_POINT('',(-0.900000000000002,1.47741935483872,-22.2188467939047)) ;
#111352 = CARTESIAN_POINT('',(13.9153543900904,1.47741935483871,-22.2188467939047)) ;
#111353 = CARTESIAN_POINT('Origin',(-0.900000000000001,3.8,-20.32)) ;
#111354 = CARTESIAN_POINT('',(1.35,0.876327704607742,-20.9924137931035)) ;
#111355 = CARTESIAN_POINT('Ctrl Pts',(1.35,0.876327704607742,-20.9924137931035)) ;
#111356 = CARTESIAN_POINT('Ctrl Pts',(1.35,0.888571289407569,-21.0456492115953)) ;
#111357 = CARTESIAN_POINT('Ctrl Pts',(1.32969623836296,0.902340613578954,
-21.0979295970213)) ;
#111358 = CARTESIAN_POINT('Ctrl Pts',(1.25741074236298,0.924142973728496,
-21.1750150537158)) ;
#111359 = CARTESIAN_POINT('Ctrl Pts',(1.20472523187106,0.93175780006653,-21.1993103448276)) ;
#111360 = CARTESIAN_POINT('Ctrl Pts',(1.15,0.93175780006653,-21.1993103448276)) ;
#111361 = CARTESIAN_POINT('',(1.35,0.876327704607742,-19.6475862068966)) ;
#111362 = CARTESIAN_POINT('Origin',(1.35,3.8,-20.32)) ;
#111363 = CARTESIAN_POINT('Ctrl Pts',(1.15,0.931757800066529,-19.4406896551724)) ;
#111364 = CARTESIAN_POINT('Ctrl Pts',(1.20475877631964,0.931757800066529,
-19.4406896551724)) ;
#111365 = CARTESIAN_POINT('Ctrl Pts',(1.2574100247738,0.924155896380523,-19.4649343608884)) ;
#111366 = CARTESIAN_POINT('Ctrl Pts',(1.32987646938161,0.9022735155524,-19.5423125455279)) ;
#111367 = CARTESIAN_POINT('Ctrl Pts',(1.35,0.888577265820266,-19.5943248028101)) ;
#111368 = CARTESIAN_POINT('Ctrl Pts',(1.35,0.876327704607742,-19.6475862068966)) ;
#111369 = CARTESIAN_POINT('',(-0.900000000000002,1.47741935483872,-18.4211532060953)) ;
#111370 = CARTESIAN_POINT('Origin',(-0.900000000000001,3.8,-20.32)) ;
#111371 = CARTESIAN_POINT('',(13.9153543900904,1.47741935483871,-18.4211532060953)) ;
#111372 = CARTESIAN_POINT('Origin',(0.55,3.09772049281573E-17,-20.32)) ;
#111373 = CARTESIAN_POINT('',(0.549999999999999,4.4,-19.87)) ;
#111374 = CARTESIAN_POINT('',(0.549999999999999,4.4,-20.77)) ;
#111375 = CARTESIAN_POINT('',(0.549999999999999,4.4,-20.32)) ;
#111376 = CARTESIAN_POINT('',(0.55,4.04473197180486,-20.77)) ;
#111377 = CARTESIAN_POINT('',(0.55,1.39397422176708E-16,-20.77)) ;
#111378 = CARTESIAN_POINT('',(0.55,4.05997159067981,-20.72)) ;
#111379 = CARTESIAN_POINT('Ctrl Pts',(0.549999999999999,4.04473197180486,
-20.77)) ;
#111380 = CARTESIAN_POINT('Ctrl Pts',(0.549999999999999,4.04764757798806,
-20.7655648611277)) ;
#111381 = CARTESIAN_POINT('Ctrl Pts',(0.549999999999999,4.05014503921306,
-20.7609481448659)) ;
#111382 = CARTESIAN_POINT('Ctrl Pts',(0.549999999999999,4.0569489863933,-20.7456814456903)) ;
#111383 = CARTESIAN_POINT('Ctrl Pts',(0.549999999999999,4.0599715906798,-20.7318214564414)) ;
#111384 = CARTESIAN_POINT('Ctrl Pts',(0.549999999999999,4.0599715906798,-20.72)) ;
#111385 = CARTESIAN_POINT('',(0.55,4.05997159067981,-19.92)) ;
#111386 = CARTESIAN_POINT('',(0.55,4.05997159067981,-19.82)) ;
#111387 = CARTESIAN_POINT('',(0.55,4.04473197181449,-19.8700000000146)) ;
#111388 = CARTESIAN_POINT('Origin',(0.550034503802634,3.93869457791706,-19.9224160296946)) ;
#111389 = CARTESIAN_POINT('',(0.55,6.35032701027224E-17,-19.87)) ;
#111390 = CARTESIAN_POINT('Origin',(10.,7.8,-22.86)) ;
#111391 = CARTESIAN_POINT('',(9.93162277660169,7.82279240779944,-22.86)) ;
#111392 = CARTESIAN_POINT('',(8.51539501058484,8.29486832980505,-22.86)) ;
#111393 = CARTESIAN_POINT('',(10.,7.8,-22.86)) ;
#111394 = CARTESIAN_POINT('',(8.51540095511711,8.29487265903615,-21.0890607599342)) ;
#111395 = CARTESIAN_POINT('',(8.51539501058484,8.29486832980505,-22.86)) ;
#111396 = CARTESIAN_POINT('',(8.54856023413467,8.2839858620311,-21.0760080665656)) ;
#111397 = CARTESIAN_POINT('Ctrl Pts',(8.51540095511711,8.29487265903615,-21.0890607599342)) ;
#111398 = CARTESIAN_POINT('Ctrl Pts',(8.51716444659961,8.29428466923188,-21.0896424828188)) ;
#111399 = CARTESIAN_POINT('Ctrl Pts',(8.5190195486817,8.29366521079574,-21.0899704508582)) ;
#111400 = CARTESIAN_POINT('Ctrl Pts',(8.52087614409674,8.29304501946167,-21.0900725025784)) ;
#111401 = CARTESIAN_POINT('Ctrl Pts',(8.52171779595222,8.29276386763783,-21.0901187657647)) ;
#111402 = CARTESIAN_POINT('Ctrl Pts',(8.52256005861366,8.29248252453827,-21.090119087778)) ;
#111403 = CARTESIAN_POINT('Ctrl Pts',(8.52339613191994,8.29220315552769,-21.0900794460141)) ;
#111404 = CARTESIAN_POINT('Ctrl Pts',(8.52456316579569,8.29181319797645,-21.0900241120128)) ;
#111405 = CARTESIAN_POINT('Ctrl Pts',(8.52573147766847,8.29142195356397,-21.0898930049957)) ;
#111406 = CARTESIAN_POINT('Ctrl Pts',(8.52689074379087,8.29103442649366,-21.089691327086)) ;
#111407 = CARTESIAN_POINT('Ctrl Pts',(8.52858695132689,8.2904674071317,-21.0893962373015)) ;
#111408 = CARTESIAN_POINT('Ctrl Pts',(8.53026630212623,8.2899212363328,-21.0889439218143)) ;
#111409 = CARTESIAN_POINT('Ctrl Pts',(8.53190117913114,8.28939883282068,-21.0883683729163)) ;
#111410 = CARTESIAN_POINT('Ctrl Pts',(8.53241671440272,8.28923410028381,-21.0881868817358)) ;
#111411 = CARTESIAN_POINT('Ctrl Pts',(8.53292790037785,8.28907155799427,-21.0879933975174)) ;
#111412 = CARTESIAN_POINT('Ctrl Pts',(8.53343404910735,8.28891083250767,-21.0877898379553)) ;
#111413 = CARTESIAN_POINT('Ctrl Pts',(8.53529681408171,8.28831931900685,-21.0870406834076)) ;
#111414 = CARTESIAN_POINT('Ctrl Pts',(8.53711612169875,8.28774836357889,-21.0861310088335)) ;
#111415 = CARTESIAN_POINT('Ctrl Pts',(8.53885192161983,8.28720494689875,-21.085061264748)) ;
#111416 = CARTESIAN_POINT('Ctrl Pts',(8.54015925159109,8.28679566878772,-21.0842555794339)) ;
#111417 = CARTESIAN_POINT('Ctrl Pts',(8.54141951580282,8.28640152775899,-21.0833597461918)) ;
#111418 = CARTESIAN_POINT('Ctrl Pts',(8.54261761299017,8.2860217121528,-21.0823927107854)) ;
#111419 = CARTESIAN_POINT('Ctrl Pts',(8.54427390694791,8.28549664098141,-21.0810558451977)) ;
#111420 = CARTESIAN_POINT('Ctrl Pts',(8.54582756795261,8.28499592220789,-21.0795574336962)) ;
#111421 = CARTESIAN_POINT('Ctrl Pts',(8.54719190273359,8.28456181678109,-21.0779139760522)) ;
#111422 = CARTESIAN_POINT('Ctrl Pts',(8.54768505754697,8.28440490428151,-21.0773199290052)) ;
#111423 = CARTESIAN_POINT('Ctrl Pts',(8.54815358395156,8.28425671205374,-21.0767074323075)) ;
#111424 = CARTESIAN_POINT('Ctrl Pts',(8.54859369700691,8.28411936587097,-21.0760788545618)) ;
#111425 = CARTESIAN_POINT('',(8.56837597005374,8.27720399148448,-21.0525054212669)) ;
#111426 = CARTESIAN_POINT('Ctrl Pts',(8.5485198670553,8.28382649282421,-21.0760140527758)) ;
#111427 = CARTESIAN_POINT('Ctrl Pts',(8.55267891820627,8.28243778061541,-21.0705631273053)) ;
#111428 = CARTESIAN_POINT('Ctrl Pts',(8.5570174719567,8.2809693370826,-21.0652590577817)) ;
#111429 = CARTESIAN_POINT('Ctrl Pts',(8.56150853123423,8.27945301063663,-21.0601132102137)) ;
#111430 = CARTESIAN_POINT('Ctrl Pts',(8.56331520072572,8.27884302075234,-21.0580431315899)) ;
#111431 = CARTESIAN_POINT('Ctrl Pts',(8.56514663435523,8.27822544298235,-21.0559980022296)) ;
#111432 = CARTESIAN_POINT('Ctrl Pts',(8.56700126712394,8.27760232477898,-21.0539757856585)) ;
#111433 = CARTESIAN_POINT('Ctrl Pts',(8.56745273479657,8.27745064099025,-21.0534835235653)) ;
#111434 = CARTESIAN_POINT('Ctrl Pts',(8.56790562999349,8.27729861980367,-21.0529951953627)) ;
#111435 = CARTESIAN_POINT('Ctrl Pts',(8.56835731300612,8.27714712982918,-21.0525055965825)) ;
#111436 = CARTESIAN_POINT('',(9.93162277660169,7.82279240779944,-21.2797127088383)) ;
#111437 = CARTESIAN_POINT('',(9.98593528106273,7.80468823964576,-21.2887647929151)) ;
#111438 = CARTESIAN_POINT('',(9.93162277660169,7.82279240779944,-22.86)) ;
#111439 = CARTESIAN_POINT('Origin',(10.,6.8,-22.86)) ;
#111440 = CARTESIAN_POINT('',(10.,6.8847127088383,-22.86)) ;
#111441 = CARTESIAN_POINT('',(10.,7.72792407799439,-22.86)) ;
#111442 = CARTESIAN_POINT('',(10.,6.8,-22.86)) ;
#111443 = CARTESIAN_POINT('',(10.,7.72792407799439,-21.2797127088383)) ;
#111444 = CARTESIAN_POINT('',(10.,7.72792407799439,-22.86)) ;
#111445 = CARTESIAN_POINT('',(10.,6.8847127088383,-21.2797127088383)) ;
#111446 = CARTESIAN_POINT('',(10.,6.8,-21.2797127088383)) ;
#111447 = CARTESIAN_POINT('',(10.,6.8847127088383,-22.86)) ;
#111448 = CARTESIAN_POINT('Origin',(8.5,6.55,-22.86)) ;
#111449 = CARTESIAN_POINT('',(9.91643989873054,6.78607331645509,-21.2797127088383)) ;
#111450 = CARTESIAN_POINT('',(8.58355805979354,6.56393854759965,-21.0575665415707)) ;
#111451 = CARTESIAN_POINT('',(8.48442535909739,6.54740422651623,-21.0410436188994)) ;
#111452 = CARTESIAN_POINT('',(8.56107669735261,6.56009388000089,-21.0823838472224)) ;
#111453 = CARTESIAN_POINT('Ctrl Pts',(8.58354728038625,6.56400494118525,-21.0575667486351)) ;
#111454 = CARTESIAN_POINT('Ctrl Pts',(8.57838853885694,6.56313097816977,-21.0629365696477)) ;
#111455 = CARTESIAN_POINT('Ctrl Pts',(8.5733012794655,6.56225500583438,-21.0683881686567)) ;
#111456 = CARTESIAN_POINT('Ctrl Pts',(8.56834297134802,6.56140899842962,-21.0739607837897)) ;
#111457 = CARTESIAN_POINT('Ctrl Pts',(8.5658758707987,6.56098805134777,-21.0767335444834)) ;
#111458 = CARTESIAN_POINT('Ctrl Pts',(8.56344049907312,6.56057499921404,-21.0795353033204)) ;
#111459 = CARTESIAN_POINT('Ctrl Pts',(8.56104288133098,6.56017406260212,-21.0823650362459)) ;
#111460 = CARTESIAN_POINT('',(8.50816305748501,6.55136011924236,-21.0973726221052)) ;
#111461 = CARTESIAN_POINT('Ctrl Pts',(8.56125813732196,6.56020968955366,-21.0825506353537)) ;
#111462 = CARTESIAN_POINT('Ctrl Pts',(8.5573713991649,6.55956189986082,-21.0872085994735)) ;
#111463 = CARTESIAN_POINT('Ctrl Pts',(8.55306335190238,6.55884389198373,-21.0899674660873)) ;
#111464 = CARTESIAN_POINT('Ctrl Pts',(8.54121332232612,6.55686888705435,-21.0965237407842)) ;
#111465 = CARTESIAN_POINT('Ctrl Pts',(8.53496267038448,6.55582711173075,-21.0979613606691)) ;
#111466 = CARTESIAN_POINT('Ctrl Pts',(8.5288866518513,6.55481444197522,-21.0992795539314)) ;
#111467 = CARTESIAN_POINT('Ctrl Pts',(8.52471102104674,6.55411850350779,-21.0995977494013)) ;
#111468 = CARTESIAN_POINT('Ctrl Pts',(8.52011475164502,6.5533524586075,-21.0997029599352)) ;
#111469 = CARTESIAN_POINT('Ctrl Pts',(8.51754797133869,6.55292466188978,-21.0997186459429)) ;
#111470 = CARTESIAN_POINT('Ctrl Pts',(8.51248317870076,6.55208052978346,-21.0989638228622)) ;
#111471 = CARTESIAN_POINT('Ctrl Pts',(8.51021540604917,6.55170256767486,-21.0983708961115)) ;
#111472 = CARTESIAN_POINT('Ctrl Pts',(8.50816120922225,6.55136020153704,-21.097376411526)) ;
#111473 = CARTESIAN_POINT('',(8.50816364570071,6.55136060761679,-22.86)) ;
#111474 = CARTESIAN_POINT('',(8.50816364570071,6.55136060761679,-22.86)) ;
#111475 = CARTESIAN_POINT('',(9.91643989873054,6.78607331645509,-22.86)) ;
#111476 = CARTESIAN_POINT('',(8.5,6.55,-22.86)) ;
#111477 = CARTESIAN_POINT('',(9.91643989873054,6.78607331645509,-22.86)) ;
#111478 = CARTESIAN_POINT('Origin',(10.,1.5,-22.86)) ;
#111479 = CARTESIAN_POINT('',(-0.900000000000002,1.5,-22.2821416870349)) ;
#111480 = CARTESIAN_POINT('',(8.49172374697003,1.5,-22.2821416870349)) ;
#111481 = CARTESIAN_POINT('',(10.,1.5,-22.2821416870349)) ;
#111482 = CARTESIAN_POINT('',(8.49172374697003,1.5,-22.86)) ;
#111483 = CARTESIAN_POINT('',(8.49172374697003,1.5,-22.86)) ;
#111484 = CARTESIAN_POINT('',(-0.900000000000001,1.5,-22.86)) ;
#111485 = CARTESIAN_POINT('',(10.,1.5,-22.86)) ;
#111486 = CARTESIAN_POINT('',(-0.900000000000002,1.5,-22.2461360284258)) ;
#111487 = CARTESIAN_POINT('Origin',(10.,1.5,-22.86)) ;
#111488 = CARTESIAN_POINT('',(8.49172374697003,1.5,-17.78)) ;
#111489 = CARTESIAN_POINT('',(-0.900000000000001,1.5,-17.78)) ;
#111490 = CARTESIAN_POINT('',(10.,1.5,-17.78)) ;
#111491 = CARTESIAN_POINT('',(8.49172374697003,1.5,-18.3578583129651)) ;
#111492 = CARTESIAN_POINT('',(8.49172374697003,1.5,-22.86)) ;
#111493 = CARTESIAN_POINT('',(-0.900000000000002,1.5,-18.3578583129651)) ;
#111494 = CARTESIAN_POINT('',(10.,1.5,-18.3578583129651)) ;
#111495 = CARTESIAN_POINT('',(-0.900000000000001,1.5,-22.86)) ;
#111496 = CARTESIAN_POINT('Origin',(10.,0.,-22.86)) ;
#111497 = CARTESIAN_POINT('',(10.,0.1,-17.78)) ;
#111498 = CARTESIAN_POINT('',(10.,1.16528729116168,-17.78)) ;
#111499 = CARTESIAN_POINT('',(10.,0.,-17.78)) ;
#111500 = CARTESIAN_POINT('',(10.,0.1,-22.86)) ;
#111501 = CARTESIAN_POINT('',(10.,0.1,-22.86)) ;
#111502 = CARTESIAN_POINT('',(10.,1.16528729116168,-22.86)) ;
#111503 = CARTESIAN_POINT('',(10.,0.,-22.86)) ;
#111504 = CARTESIAN_POINT('',(10.,1.16528729116168,-22.3641618801782)) ;
#111505 = CARTESIAN_POINT('',(10.,1.16528729116168,-22.86)) ;
#111506 = CARTESIAN_POINT('',(10.,1.16528729116168,-18.2758381198218)) ;
#111507 = CARTESIAN_POINT('Origin',(10.,3.8,-20.32)) ;
#111508 = CARTESIAN_POINT('',(10.,1.16528729116168,-22.86)) ;
#111509 = CARTESIAN_POINT('Origin',(0.,0.,-22.86)) ;
#111510 = CARTESIAN_POINT('',(8.48377223398316,8.3,-22.86)) ;
#111511 = CARTESIAN_POINT('',(7.1,8.3,-22.86)) ;
#111512 = CARTESIAN_POINT('',(8.5,8.3,-22.86)) ;
#111513 = CARTESIAN_POINT('Origin',(8.48377223398316,8.2,-22.86)) ;
#111514 = CARTESIAN_POINT('Origin',(9.9,7.72792407799439,-22.86)) ;
#111515 = CARTESIAN_POINT('Origin',(9.9,6.8847127088383,-22.86)) ;
#111516 = CARTESIAN_POINT('',(8.49172374697018,6.55,-22.86)) ;
#111517 = CARTESIAN_POINT('Origin',(8.49172374697018,6.65,-22.86)) ;
#111518 = CARTESIAN_POINT('',(-0.900000000000001,6.55,-22.86)) ;
#111519 = CARTESIAN_POINT('',(1.25,6.55,-22.86)) ;
#111520 = CARTESIAN_POINT('',(-1.,6.45,-22.86)) ;
#111521 = CARTESIAN_POINT('Origin',(-0.9,6.45,-22.86)) ;
#111522 = CARTESIAN_POINT('',(-1.,4.65,-22.86)) ;
#111523 = CARTESIAN_POINT('',(-1.,3.46944695195362E-16,-22.86)) ;
#111524 = CARTESIAN_POINT('',(-0.900000000000001,4.55,-22.86)) ;
#111525 = CARTESIAN_POINT('Origin',(-0.900000000000001,4.65,-22.86)) ;
#111526 = CARTESIAN_POINT('',(1.15,4.55,-22.86)) ;
#111527 = CARTESIAN_POINT('',(1.57859836313889E-15,4.55,-22.86)) ;
#111528 = CARTESIAN_POINT('',(1.25,4.45,-22.86)) ;
#111529 = CARTESIAN_POINT('Origin',(1.15,4.45,-22.86)) ;
#111530 = CARTESIAN_POINT('',(1.25,3.15,-22.86)) ;
#111531 = CARTESIAN_POINT('',(1.25,1.5,-22.86)) ;
#111532 = CARTESIAN_POINT('',(1.15,3.05,-22.86)) ;
#111533 = CARTESIAN_POINT('Origin',(1.15,3.15,-22.86)) ;
#111534 = CARTESIAN_POINT('',(-0.900000000000002,3.05,-22.86)) ;
#111535 = CARTESIAN_POINT('',(1.05818132034585E-15,3.05,-22.86)) ;
#111536 = CARTESIAN_POINT('',(-1.,2.95,-22.86)) ;
#111537 = CARTESIAN_POINT('Origin',(-0.900000000000002,2.95,-22.86)) ;
#111538 = CARTESIAN_POINT('',(-1.,1.6,-22.86)) ;
#111539 = CARTESIAN_POINT('',(-1.,3.46944695195362E-16,-22.86)) ;
#111540 = CARTESIAN_POINT('Origin',(-0.900000000000002,1.6,-22.86)) ;
#111541 = CARTESIAN_POINT('',(8.50816364570057,1.49863939238321,-22.86)) ;
#111542 = CARTESIAN_POINT('Origin',(8.49172374697003,1.4,-22.86)) ;
#111543 = CARTESIAN_POINT('',(9.91643989873054,1.26392668354489,-22.86)) ;
#111544 = CARTESIAN_POINT('',(10.,1.24999999999998,-22.86)) ;
#111545 = CARTESIAN_POINT('Origin',(9.9,1.16528729116168,-22.86)) ;
#111546 = CARTESIAN_POINT('',(9.9,0.,-22.86)) ;
#111547 = CARTESIAN_POINT('Origin',(9.9,0.1,-22.86)) ;
#111548 = CARTESIAN_POINT('',(-2.,0.,-22.86)) ;
#111549 = CARTESIAN_POINT('',(-2.,0.,-22.86)) ;
#111550 = CARTESIAN_POINT('',(-2.,7.55,-22.86)) ;
#111551 = CARTESIAN_POINT('',(-2.,7.65,-22.86)) ;
#111552 = CARTESIAN_POINT('',(-1.9,7.65,-22.86)) ;
#111553 = CARTESIAN_POINT('Origin',(-1.9,7.55,-22.86)) ;
#111554 = CARTESIAN_POINT('',(6.9,7.65,-22.86)) ;
#111555 = CARTESIAN_POINT('',(7.,7.65,-22.86)) ;
#111556 = CARTESIAN_POINT('',(7.,7.75,-22.86)) ;
#111557 = CARTESIAN_POINT('Origin',(6.9,7.75,-22.86)) ;
#111558 = CARTESIAN_POINT('',(7.,8.2,-22.86)) ;
#111559 = CARTESIAN_POINT('',(7.,8.3,-22.86)) ;
#111560 = CARTESIAN_POINT('Origin',(7.1,8.2,-22.86)) ;
#111561 = CARTESIAN_POINT('Origin',(0.,0.,-17.78)) ;
#111562 = CARTESIAN_POINT('',(9.93162277660169,7.82279240779944,-17.78)) ;
#111563 = CARTESIAN_POINT('',(8.51539501058484,8.29486832980505,-17.78)) ;
#111564 = CARTESIAN_POINT('',(10.,7.8,-17.78)) ;
#111565 = CARTESIAN_POINT('',(8.48377223398316,8.3,-17.78)) ;
#111566 = CARTESIAN_POINT('Origin',(8.48377223398316,8.2,-17.78)) ;
#111567 = CARTESIAN_POINT('',(7.1,8.3,-17.78)) ;
#111568 = CARTESIAN_POINT('',(8.5,8.3,-17.78)) ;
#111569 = CARTESIAN_POINT('',(7.,8.2,-17.78)) ;
#111570 = CARTESIAN_POINT('Origin',(7.1,8.2,-17.78)) ;
#111571 = CARTESIAN_POINT('',(7.,7.75,-17.78)) ;
#111572 = CARTESIAN_POINT('',(7.,8.3,-17.78)) ;
#111573 = CARTESIAN_POINT('',(6.9,7.65,-17.78)) ;
#111574 = CARTESIAN_POINT('Origin',(6.9,7.75,-17.78)) ;
#111575 = CARTESIAN_POINT('',(-1.9,7.65,-17.78)) ;
#111576 = CARTESIAN_POINT('',(7.,7.65,-17.78)) ;
#111577 = CARTESIAN_POINT('',(-2.,7.55,-17.78)) ;
#111578 = CARTESIAN_POINT('Origin',(-1.9,7.55,-17.78)) ;
#111579 = CARTESIAN_POINT('',(-2.,0.,-17.78)) ;
#111580 = CARTESIAN_POINT('',(-2.,7.65,-17.78)) ;
#111581 = CARTESIAN_POINT('',(9.9,0.,-17.78)) ;
#111582 = CARTESIAN_POINT('',(-2.,0.,-17.78)) ;
#111583 = CARTESIAN_POINT('Origin',(9.9,0.1,-17.78)) ;
#111584 = CARTESIAN_POINT('',(9.91643989873054,1.26392668354489,-17.78)) ;
#111585 = CARTESIAN_POINT('Origin',(9.9,1.16528729116168,-17.78)) ;
#111586 = CARTESIAN_POINT('',(8.50816364570057,1.49863939238321,-17.78)) ;
#111587 = CARTESIAN_POINT('',(0.472972972972955,2.83783783783779,-17.78)) ;
#111588 = CARTESIAN_POINT('Origin',(8.49172374697003,1.4,-17.78)) ;
#111589 = CARTESIAN_POINT('',(-1.,1.6,-17.78)) ;
#111590 = CARTESIAN_POINT('Origin',(-0.900000000000002,1.6,-17.78)) ;
#111591 = CARTESIAN_POINT('',(-1.,2.95,-17.78)) ;
#111592 = CARTESIAN_POINT('',(-1.,3.46944695195362E-16,-17.78)) ;
#111593 = CARTESIAN_POINT('',(-0.900000000000002,3.05,-17.78)) ;
#111594 = CARTESIAN_POINT('Origin',(-0.900000000000002,2.95,-17.78)) ;
#111595 = CARTESIAN_POINT('',(1.15,3.05,-17.78)) ;
#111596 = CARTESIAN_POINT('',(1.05818132034585E-15,3.05,-17.78)) ;
#111597 = CARTESIAN_POINT('',(1.25,3.15,-17.78)) ;
#111598 = CARTESIAN_POINT('Origin',(1.15,3.15,-17.78)) ;
#111599 = CARTESIAN_POINT('',(1.25,4.45,-17.78)) ;
#111600 = CARTESIAN_POINT('',(1.25,5.3,-17.78)) ;
#111601 = CARTESIAN_POINT('',(1.15,4.55,-17.78)) ;
#111602 = CARTESIAN_POINT('Origin',(1.15,4.45,-17.78)) ;
#111603 = CARTESIAN_POINT('',(-0.900000000000001,4.55,-17.78)) ;
#111604 = CARTESIAN_POINT('',(1.57859836313889E-15,4.55,-17.78)) ;
#111605 = CARTESIAN_POINT('',(-1.,4.65,-17.78)) ;
#111606 = CARTESIAN_POINT('Origin',(-0.900000000000001,4.65,-17.78)) ;
#111607 = CARTESIAN_POINT('',(-1.,6.45,-17.78)) ;
#111608 = CARTESIAN_POINT('',(-1.,3.46944695195362E-16,-17.78)) ;
#111609 = CARTESIAN_POINT('',(-0.900000000000001,6.55,-17.78)) ;
#111610 = CARTESIAN_POINT('Origin',(-0.9,6.45,-17.78)) ;
#111611 = CARTESIAN_POINT('',(8.49172374697018,6.55,-17.78)) ;
#111612 = CARTESIAN_POINT('',(1.25,6.55,-17.78)) ;
#111613 = CARTESIAN_POINT('',(8.50816364570071,6.55136060761679,-17.78)) ;
#111614 = CARTESIAN_POINT('Origin',(8.49172374697018,6.65,-17.78)) ;
#111615 = CARTESIAN_POINT('',(9.91643989873054,6.78607331645509,-17.78)) ;
#111616 = CARTESIAN_POINT('',(8.5,6.55,-17.78)) ;
#111617 = CARTESIAN_POINT('',(10.,6.8847127088383,-17.78)) ;
#111618 = CARTESIAN_POINT('Origin',(9.9,6.8847127088383,-17.78)) ;
#111619 = CARTESIAN_POINT('',(10.,7.72792407799439,-17.78)) ;
#111620 = CARTESIAN_POINT('',(10.,6.8,-17.78)) ;
#111621 = CARTESIAN_POINT('Origin',(9.9,7.72792407799439,-17.78)) ;
#111622 = CARTESIAN_POINT('Origin',(7.,7.65,-22.86)) ;
#111623 = CARTESIAN_POINT('',(-1.9,7.65,-22.86)) ;
#111624 = CARTESIAN_POINT('',(6.9,7.65,-22.86)) ;
#111625 = CARTESIAN_POINT('Origin',(7.,8.3,-22.86)) ;
#111626 = CARTESIAN_POINT('',(7.,7.75,-17.78)) ;
#111627 = CARTESIAN_POINT('',(7.,8.2,-22.86)) ;
#111628 = CARTESIAN_POINT('Origin',(8.5,8.3,-22.86)) ;
#111629 = CARTESIAN_POINT('',(8.4,8.3,-20.862072889851)) ;
#111630 = CARTESIAN_POINT('',(8.48377267093844,8.29999999999968,-21.0780525450042)) ;
#111631 = CARTESIAN_POINT('Ctrl Pts',(8.40000000000001,8.3,-20.862072889851)) ;
#111632 = CARTESIAN_POINT('Ctrl Pts',(8.40000007660114,8.3,-20.8792296501961)) ;
#111633 = CARTESIAN_POINT('Ctrl Pts',(8.40222537906653,8.3,-20.8961962391188)) ;
#111634 = CARTESIAN_POINT('Ctrl Pts',(8.40642689896248,8.3,-20.9126162565066)) ;
#111635 = CARTESIAN_POINT('Ctrl Pts',(8.4108423802459,8.3,-20.92987245932)) ;
#111636 = CARTESIAN_POINT('Ctrl Pts',(8.41744096861416,8.3,-20.946526744374)) ;
#111637 = CARTESIAN_POINT('Ctrl Pts',(8.42598957610854,8.3,-20.9621622007355)) ;
#111638 = CARTESIAN_POINT('Ctrl Pts',(8.42927578126155,8.3,-20.9681726904321)) ;
#111639 = CARTESIAN_POINT('Ctrl Pts',(8.43285067318742,8.3,-20.9740324469635)) ;
#111640 = CARTESIAN_POINT('Ctrl Pts',(8.43670279785319,8.3,-20.9797167867854)) ;
#111641 = CARTESIAN_POINT('Ctrl Pts',(8.43684245837179,8.3,-20.9799228750916)) ;
#111642 = CARTESIAN_POINT('Ctrl Pts',(8.43698247939113,8.3,-20.9801287268225)) ;
#111643 = CARTESIAN_POINT('Ctrl Pts',(8.43712286024715,8.3,-20.9803343406941)) ;
#111644 = CARTESIAN_POINT('Ctrl Pts',(8.44304092798571,8.3,-20.9890024515356)) ;
#111645 = CARTESIAN_POINT('Ctrl Pts',(8.44963232699549,8.300000000002,-20.9973317313645)) ;
#111646 = CARTESIAN_POINT('Ctrl Pts',(8.45667836512367,8.29999999999776,-21.0051882739642)) ;
#111647 = CARTESIAN_POINT('Ctrl Pts',(8.46347186896914,8.29999999999368,-21.0127632333091)) ;
#111648 = CARTESIAN_POINT('Ctrl Pts',(8.47075094334181,8.29999999998296,-21.0199098655154)) ;
#111649 = CARTESIAN_POINT('Ctrl Pts',(8.47818849074308,8.29999999991001,-21.0268816128285)) ;
#111650 = CARTESIAN_POINT('Ctrl Pts',(8.47846436286148,8.2999999999073,-21.0271402075771)) ;
#111651 = CARTESIAN_POINT('Ctrl Pts',(8.47874045306876,8.29999999990447,-21.0273985605991)) ;
#111652 = CARTESIAN_POINT('Ctrl Pts',(8.47901674447045,8.29999999990152,-21.0276566852)) ;
#111653 = CARTESIAN_POINT('Ctrl Pts',(8.48287938578321,8.29999999986032,-21.0312653488833)) ;
#111654 = CARTESIAN_POINT('Ctrl Pts',(8.48681205529409,8.29999999978803,-21.0348079367278)) ;
#111655 = CARTESIAN_POINT('Ctrl Pts',(8.49047938959116,8.29999999977836,-21.0386027060218)) ;
#111656 = CARTESIAN_POINT('Ctrl Pts',(8.49231307405274,8.29999999977353,-21.0405001085834)) ;
#111657 = CARTESIAN_POINT('Ctrl Pts',(8.49410676862313,8.29999999978935,-21.042469327125)) ;
#111658 = CARTESIAN_POINT('Ctrl Pts',(8.49555027122445,8.29999999981726,-21.0446968070099)) ;
#111659 = CARTESIAN_POINT('Ctrl Pts',(8.49675259850851,8.2999999998405,-21.0465521274215)) ;
#111660 = CARTESIAN_POINT('Ctrl Pts',(8.49764594203226,8.29999999986456,-21.0486368157432)) ;
#111661 = CARTESIAN_POINT('Ctrl Pts',(8.49795530287013,8.29999999987615,-21.0508110374494)) ;
#111662 = CARTESIAN_POINT('Ctrl Pts',(8.49801735255452,8.29999999987847,-21.0512471293982)) ;
#111663 = CARTESIAN_POINT('Ctrl Pts',(8.49805590844334,8.29999999988033,-21.051686822978)) ;
#111664 = CARTESIAN_POINT('Ctrl Pts',(8.49806875158486,8.29999999988168,-21.0521289896614)) ;
#111665 = CARTESIAN_POINT('Ctrl Pts',(8.49822249685463,8.2999999998978,-21.0574221678068)) ;
#111666 = CARTESIAN_POINT('Ctrl Pts',(8.49538250015676,8.29999999989889,-21.0623553442684)) ;
#111667 = CARTESIAN_POINT('Ctrl Pts',(8.49246863081133,8.29999999993393,-21.066722860551)) ;
#111668 = CARTESIAN_POINT('Ctrl Pts',(8.48983292606215,8.29999999996562,-21.0706734437939)) ;
#111669 = CARTESIAN_POINT('Ctrl Pts',(8.48683766317129,8.3,-21.0743922110698)) ;
#111670 = CARTESIAN_POINT('Ctrl Pts',(8.48377316486175,8.3,-21.0780519562975)) ;
#111671 = CARTESIAN_POINT('',(8.48377223398316,8.3,-22.86)) ;
#111672 = CARTESIAN_POINT('',(7.1,8.3,-22.86)) ;
#111673 = CARTESIAN_POINT('',(8.48377267093845,8.29999999999968,-19.5619474549958)) ;
#111674 = CARTESIAN_POINT('',(8.48377223398316,8.3,-22.86)) ;
#111675 = CARTESIAN_POINT('',(8.4,8.3,-19.777927110149)) ;
#111676 = CARTESIAN_POINT('Ctrl Pts',(8.48377316486178,8.3,-19.5619480437025)) ;
#111677 = CARTESIAN_POINT('Ctrl Pts',(8.48683766317132,8.3,-19.5656077889302)) ;
#111678 = CARTESIAN_POINT('Ctrl Pts',(8.48983292606215,8.29999999996562,-19.5693265562061)) ;
#111679 = CARTESIAN_POINT('Ctrl Pts',(8.49246863081132,8.29999999993393,-19.573277139449)) ;
#111680 = CARTESIAN_POINT('Ctrl Pts',(8.49538250015675,8.29999999989889,-19.5776446557316)) ;
#111681 = CARTESIAN_POINT('Ctrl Pts',(8.49822249685464,8.2999999998978,-19.5825778321932)) ;
#111682 = CARTESIAN_POINT('Ctrl Pts',(8.49806875158487,8.29999999988168,-19.5878710103386)) ;
#111683 = CARTESIAN_POINT('Ctrl Pts',(8.49805590844335,8.29999999988033,-19.588313177022)) ;
#111684 = CARTESIAN_POINT('Ctrl Pts',(8.49801735255452,8.29999999987847,-19.5887528706018)) ;
#111685 = CARTESIAN_POINT('Ctrl Pts',(8.49795530287013,8.29999999987615,-19.5891889625506)) ;
#111686 = CARTESIAN_POINT('Ctrl Pts',(8.49764594190814,8.29999999986456,-19.5913631851291)) ;
#111687 = CARTESIAN_POINT('Ctrl Pts',(8.49675259754384,8.2999999998405,-19.5934478740673)) ;
#111688 = CARTESIAN_POINT('Ctrl Pts',(8.49555027122431,8.29999999981726,-19.59530319299)) ;
#111689 = CARTESIAN_POINT('Ctrl Pts',(8.4941067657021,8.29999999978935,-19.5975306773816)) ;
#111690 = CARTESIAN_POINT('Ctrl Pts',(8.49231306928119,8.29999999977353,-19.599499896352)) ;
#111691 = CARTESIAN_POINT('Ctrl Pts',(8.49047938958767,8.29999999977837,-19.6013972939748)) ;
#111692 = CARTESIAN_POINT('Ctrl Pts',(8.48681202348066,8.29999999978803,-19.6051920961739)) ;
#111693 = CARTESIAN_POINT('Ctrl Pts',(8.48287934332709,8.29999999986032,-19.6087346907302)) ;
#111694 = CARTESIAN_POINT('Ctrl Pts',(8.47901674443309,8.29999999990152,-19.6123433147599)) ;
#111695 = CARTESIAN_POINT('Ctrl Pts',(8.47874052296043,8.29999999990447,-19.6126013740281)) ;
#111696 = CARTESIAN_POINT('Ctrl Pts',(8.47846450284309,8.2999999999073,-19.6128596613565)) ;
#111697 = CARTESIAN_POINT('Ctrl Pts',(8.47818870097127,8.29999999991001,-19.6131181900299)) ;
#111698 = CARTESIAN_POINT('Ctrl Pts',(8.4707518532558,8.29999999998296,-19.620089275328)) ;
#111699 = CARTESIAN_POINT('Ctrl Pts',(8.46347271757077,8.29999999998104,-19.627236821007)) ;
#111700 = CARTESIAN_POINT('Ctrl Pts',(8.45667934899943,8.29999999998018,-19.6348126083154)) ;
#111701 = CARTESIAN_POINT('Ctrl Pts',(8.44963335392747,8.29999999997929,-19.6426701181032)) ;
#111702 = CARTESIAN_POINT('Ctrl Pts',(8.44304226791566,8.29999999996634,-19.651000256345)) ;
#111703 = CARTESIAN_POINT('Ctrl Pts',(8.43712466127423,8.29999999997622,-19.659666888942)) ;
#111704 = CARTESIAN_POINT('Ctrl Pts',(8.43698358608699,8.29999999997646,-19.6598735006502)) ;
#111705 = CARTESIAN_POINT('Ctrl Pts',(8.43684287437576,8.2999999999767,-19.6600803512793)) ;
#111706 = CARTESIAN_POINT('Ctrl Pts',(8.43670252680328,8.29999999997696,-19.6602874394955)) ;
#111707 = CARTESIAN_POINT('Ctrl Pts',(8.42665365624043,8.29999999999548,-19.6751149327167)) ;
#111708 = CARTESIAN_POINT('Ctrl Pts',(8.41848789916046,8.29999999999779,-19.6911348631973)) ;
#111709 = CARTESIAN_POINT('Ctrl Pts',(8.41242260582095,8.29999999999911,-19.7079180514057)) ;
#111710 = CARTESIAN_POINT('Ctrl Pts',(8.40662497273872,8.30000000000037,-19.7239606006668)) ;
#111711 = CARTESIAN_POINT('Ctrl Pts',(8.40274598945664,8.3,-19.7407021939303)) ;
#111712 = CARTESIAN_POINT('Ctrl Pts',(8.40101973895557,8.3,-19.757779788354)) ;
#111713 = CARTESIAN_POINT('Ctrl Pts',(8.4003453349776,8.3,-19.7644515880762)) ;
#111714 = CARTESIAN_POINT('Ctrl Pts',(8.40000003014814,8.3,-19.7711746730442)) ;
#111715 = CARTESIAN_POINT('Ctrl Pts',(8.4,8.3,-19.777927110149)) ;
#111716 = CARTESIAN_POINT('',(8.4,8.3,-20.9036545563009)) ;
#111717 = CARTESIAN_POINT('Origin',(10.,7.8,-22.86)) ;
#111718 = CARTESIAN_POINT('',(8.56837722373804,8.27720759208727,-19.5874948832496)) ;
#111719 = CARTESIAN_POINT('',(8.54843785958922,8.2838540468036,-19.5639803122607)) ;
#111720 = CARTESIAN_POINT('Ctrl Pts',(8.56837722339832,8.27720759220056,-19.5874948833623)) ;
#111721 = CARTESIAN_POINT('Ctrl Pts',(8.56792584473107,8.27735805175631,-19.5870046902277)) ;
#111722 = CARTESIAN_POINT('Ctrl Pts',(8.56747319573485,8.27750893475505,-19.5865157932638)) ;
#111723 = CARTESIAN_POINT('Ctrl Pts',(8.56702308739659,8.2776589708678,-19.5860243039587)) ;
#111724 = CARTESIAN_POINT('Ctrl Pts',(8.56055949575605,8.27981350141465,-19.5789664783343)) ;
#111725 = CARTESIAN_POINT('Ctrl Pts',(8.55435459773969,8.28188180075344,-19.5716283954692)) ;
#111726 = CARTESIAN_POINT('Ctrl Pts',(8.54852002808959,8.28382665730347,-19.5639858663514)) ;
#111727 = CARTESIAN_POINT('',(8.51539953939803,8.29486682020066,-19.550940330123)) ;
#111728 = CARTESIAN_POINT('Origin',(8.52916905055879,8.29027698314707,-19.5707344704815)) ;
#111729 = CARTESIAN_POINT('',(8.51539501058484,8.29486832980505,-22.86)) ;
#111730 = CARTESIAN_POINT('',(9.93162277660169,7.82279240779944,-19.3602872911617)) ;
#111731 = CARTESIAN_POINT('',(9.93162277660169,7.82279240779944,-22.86)) ;
#111732 = CARTESIAN_POINT('',(8.48593528106273,8.30468823964576,-19.6012352070849)) ;
#111733 = CARTESIAN_POINT('Origin',(10.,6.8,-22.86)) ;
#111734 = CARTESIAN_POINT('',(10.,6.8847127088383,-19.3602872911617)) ;
#111735 = CARTESIAN_POINT('',(10.,7.72792407799439,-19.3602872911617)) ;
#111736 = CARTESIAN_POINT('',(10.,7.8,-19.3602872911617)) ;
#111737 = CARTESIAN_POINT('',(10.,7.72792407799439,-22.86)) ;
#111738 = CARTESIAN_POINT('',(10.,6.8847127088383,-22.86)) ;
#111739 = CARTESIAN_POINT('Origin',(8.5,6.55,-22.86)) ;
#111740 = CARTESIAN_POINT('',(8.50816305748852,6.55136011924294,-19.5426273778919)) ;
#111741 = CARTESIAN_POINT('Ctrl Pts',(8.50816120922619,6.5513602015377,-19.542623588472)) ;
#111742 = CARTESIAN_POINT('Ctrl Pts',(8.50982330775214,6.55163721795869,-19.5418189278179)) ;
#111743 = CARTESIAN_POINT('Ctrl Pts',(8.51162127657743,6.55193687942957,-19.541279028441)) ;
#111744 = CARTESIAN_POINT('Ctrl Pts',(8.51523682141501,6.55253947023584,-19.5405710923351)) ;
#111745 = CARTESIAN_POINT('Ctrl Pts',(8.51710259142463,6.5528504319041,-19.5403934679392)) ;
#111746 = CARTESIAN_POINT('Ctrl Pts',(8.52217030373324,6.55369505062221,-19.5402356911266)) ;
#111747 = CARTESIAN_POINT('Ctrl Pts',(8.52587381750002,6.55431230291667,-19.5404838833945)) ;
#111748 = CARTESIAN_POINT('Ctrl Pts',(8.53482421528023,6.55580403588004,-19.5417298501843)) ;
#111749 = CARTESIAN_POINT('Ctrl Pts',(8.53952102462709,6.55658683673489,-19.5432204474238)) ;
#111750 = CARTESIAN_POINT('Ctrl Pts',(8.54640674065863,6.55773445607348,-19.5463682122463)) ;
#111751 = CARTESIAN_POINT('Ctrl Pts',(8.55013419152287,6.55835569858715,-19.548236730231)) ;
#111752 = CARTESIAN_POINT('Ctrl Pts',(8.55581906875195,6.55930317812533,-19.55204337543)) ;
#111753 = CARTESIAN_POINT('Ctrl Pts',(8.5586115073215,6.55976858455358,-19.5542775555632)) ;
#111754 = CARTESIAN_POINT('Ctrl Pts',(8.56125821409731,6.56020970234955,-19.5574494566561)) ;
#111755 = CARTESIAN_POINT('',(9.91643989873054,6.78607331645509,-19.3602872911617)) ;
#111756 = CARTESIAN_POINT('',(9.98442535909739,6.79740422651623,-19.3489563811006)) ;
#111757 = CARTESIAN_POINT('',(9.91643989873054,6.78607331645509,-22.86)) ;
#111758 = CARTESIAN_POINT('',(8.50816364570071,6.55136060761679,-22.86)) ;
#111759 = CARTESIAN_POINT('Origin',(1.25,6.55,-22.86)) ;
#111760 = CARTESIAN_POINT('',(8.49172372711481,6.55000000000007,-21.0894558427306)) ;
#111761 = CARTESIAN_POINT('',(8.49172374697018,6.55,-22.86)) ;
#111762 = CARTESIAN_POINT('',(8.4,6.55,-20.8606780018997)) ;
#111763 = CARTESIAN_POINT('Ctrl Pts',(8.49172374697018,6.55000000000105,-21.0894557456557)) ;
#111764 = CARTESIAN_POINT('Ctrl Pts',(8.4960680367363,6.55000000001052,-21.0859505863269)) ;
#111765 = CARTESIAN_POINT('Ctrl Pts',(8.50046735944504,6.54999999990302,-21.0825119042492)) ;
#111766 = CARTESIAN_POINT('Ctrl Pts',(8.5092028047519,6.55000000136502,-21.075516026702)) ;
#111767 = CARTESIAN_POINT('Ctrl Pts',(8.51365366733359,6.55000000372466,-21.0720189182924)) ;
#111768 = CARTESIAN_POINT('Ctrl Pts',(8.51786969589101,6.55000000840872,-21.0675740514918)) ;
#111769 = CARTESIAN_POINT('Ctrl Pts',(8.51824835575336,6.5500000088438,-21.0671628343558)) ;
#111770 = CARTESIAN_POINT('Ctrl Pts',(8.51893753951069,6.55000000964297,-21.0663894122641)) ;
#111771 = CARTESIAN_POINT('Ctrl Pts',(8.51925555226624,6.55000001000021,-21.0660246830609)) ;
#111772 = CARTESIAN_POINT('Ctrl Pts',(8.52125362518915,6.55000001218547,-21.0636369664008)) ;
#111773 = CARTESIAN_POINT('Ctrl Pts',(8.52280131776514,6.55000000862054,-21.0613625215737)) ;
#111774 = CARTESIAN_POINT('Ctrl Pts',(8.52354796988915,6.55000000490364,-21.0562172682012)) ;
#111775 = CARTESIAN_POINT('Ctrl Pts',(8.52233587755859,6.5500000056078,-21.0535629178234)) ;
#111776 = CARTESIAN_POINT('Ctrl Pts',(8.52032554216559,6.55000000470579,-21.0511610105705)) ;
#111777 = CARTESIAN_POINT('Ctrl Pts',(8.52004618744962,6.55000000456892,-21.0508554672246)) ;
#111778 = CARTESIAN_POINT('Ctrl Pts',(8.51943244221704,6.55000000425258,-21.0502375575506)) ;
#111779 = CARTESIAN_POINT('Ctrl Pts',(8.51910103101854,6.55000000405877,-21.0499172773213)) ;
#111780 = CARTESIAN_POINT('Ctrl Pts',(8.51460799223803,6.5500000014124,-21.0457349310042)) ;
#111781 = CARTESIAN_POINT('Ctrl Pts',(8.50969722522557,6.55000000036127,-21.042960241153)) ;
#111782 = CARTESIAN_POINT('Ctrl Pts',(8.50463600502756,6.55000000021577,-21.0396634748388)) ;
#111783 = CARTESIAN_POINT('Ctrl Pts',(8.50427412871943,6.55000000020764,-21.0394272801265)) ;
#111784 = CARTESIAN_POINT('Ctrl Pts',(8.49410349041849,6.55000000002642,-21.0327743312814)) ;
#111785 = CARTESIAN_POINT('Ctrl Pts',(8.48448997361522,6.54999999999179,-21.0260809389623)) ;
#111786 = CARTESIAN_POINT('Ctrl Pts',(8.46629237463078,6.55000000001684,-21.0109770243886)) ;
#111787 = CARTESIAN_POINT('Ctrl Pts',(8.45766562693774,6.55000000000152,-21.0025939316619)) ;
#111788 = CARTESIAN_POINT('Ctrl Pts',(8.44955830666692,6.55,-20.9932123342682)) ;
#111789 = CARTESIAN_POINT('Ctrl Pts',(8.44937081015217,6.55,-20.9929944283117)) ;
#111790 = CARTESIAN_POINT('Ctrl Pts',(8.43720071044388,6.5500000000026,-20.9787892740214)) ;
#111791 = CARTESIAN_POINT('Ctrl Pts',(8.42721384365712,6.55000000009149,-20.963256668189)) ;
#111792 = CARTESIAN_POINT('Ctrl Pts',(8.4118490364227,6.55000000007035,-20.9305950553166)) ;
#111793 = CARTESIAN_POINT('Ctrl Pts',(8.40635547808238,6.5500000000232,-20.9135173325265)) ;
#111794 = CARTESIAN_POINT('Ctrl Pts',(8.40108598764556,6.5499999999995,-20.8843588087523)) ;
#111795 = CARTESIAN_POINT('Ctrl Pts',(8.4,6.55,-20.8725595279368)) ;
#111796 = CARTESIAN_POINT('Ctrl Pts',(8.4,6.55,-20.8606780018997)) ;
#111797 = CARTESIAN_POINT('',(8.4,6.55,-19.7793219981003)) ;
#111798 = CARTESIAN_POINT('',(8.4,6.55,-19.5963606076168)) ;
#111799 = CARTESIAN_POINT('',(8.4917237271148,6.5500000000004,-19.5505441572684)) ;
#111800 = CARTESIAN_POINT('Ctrl Pts',(8.4,6.55000000000001,-19.7793219981003)) ;
#111801 = CARTESIAN_POINT('Ctrl Pts',(8.4,6.55,-19.7614603515919)) ;
#111802 = CARTESIAN_POINT('Ctrl Pts',(8.4024517784973,6.55000000000111,-19.7437850580849)) ;
#111803 = CARTESIAN_POINT('Ctrl Pts',(8.40709634751727,6.55000000003439,-19.7267518487488)) ;
#111804 = CARTESIAN_POINT('Ctrl Pts',(8.41193897064973,6.55000000006908,-19.708992307832)) ;
#111805 = CARTESIAN_POINT('Ctrl Pts',(8.41916594308737,6.55000000013771,-19.6919288881297)) ;
#111806 = CARTESIAN_POINT('Ctrl Pts',(8.42853896334544,6.55000000013582,-19.676081267302)) ;
#111807 = CARTESIAN_POINT('Ctrl Pts',(8.43455058706601,6.55000000013461,-19.6659169946706)) ;
#111808 = CARTESIAN_POINT('Ctrl Pts',(8.4414461105567,6.55000000009671,-19.6562530007178)) ;
#111809 = CARTESIAN_POINT('Ctrl Pts',(8.44917210140209,6.55000000005186,-19.6472326831015)) ;
#111810 = CARTESIAN_POINT('Ctrl Pts',(8.44936219523642,6.55000000005075,-19.6470107430557)) ;
#111811 = CARTESIAN_POINT('Ctrl Pts',(8.44955278293318,6.55000000004968,-19.6467892022862)) ;
#111812 = CARTESIAN_POINT('Ctrl Pts',(8.44974386351698,6.55000000004864,-19.6465680630167)) ;
#111813 = CARTESIAN_POINT('Ctrl Pts',(8.45766118910687,6.55000000000559,-19.6374052712633)) ;
#111814 = CARTESIAN_POINT('Ctrl Pts',(8.46628870646482,6.54999999999864,-19.6290215515032)) ;
#111815 = CARTESIAN_POINT('Ctrl Pts',(8.47555348469889,6.55000000000007,-19.621335275949)) ;
#111816 = CARTESIAN_POINT('Ctrl Pts',(8.48448851770308,6.55000000000144,-19.6139225647086)) ;
#111817 = CARTESIAN_POINT('Ctrl Pts',(8.4941027369538,6.5500000000304,-19.6072346929705)) ;
#111818 = CARTESIAN_POINT('Ctrl Pts',(8.50391213313786,6.55000000016212,-19.6008238957712)) ;
#111819 = CARTESIAN_POINT('Ctrl Pts',(8.50409415224113,6.55000000016456,-19.6007049396667)) ;
#111820 = CARTESIAN_POINT('Ctrl Pts',(8.50427622716239,6.55000000016576,-19.6005860597931)) ;
#111821 = CARTESIAN_POINT('Ctrl Pts',(8.504458355799,6.55000000016576,-19.600467254632)) ;
#111822 = CARTESIAN_POINT('Ctrl Pts',(8.50464048443561,6.55000000016577,-19.6003484494708)) ;
#111823 = CARTESIAN_POINT('Ctrl Pts',(8.50482266678758,6.55000000016458,-19.6002297190221)) ;
#111824 = CARTESIAN_POINT('Ctrl Pts',(8.50500490075226,6.55000000016234,-19.6001110617675)) ;
#111825 = CARTESIAN_POINT('Ctrl Pts',(8.50970297364428,6.55000000010443,-19.5970520248173)) ;
#111826 = CARTESIAN_POINT('Ctrl Pts',(8.51460443926445,6.55000000028677,-19.5942756540706)) ;
#111827 = CARTESIAN_POINT('Ctrl Pts',(8.51874830926338,6.55000000038295,-19.5904369847284)) ;
#111828 = CARTESIAN_POINT('Ctrl Pts',(8.51909542442965,6.550000000391,-19.5901154349821)) ;
#111829 = CARTESIAN_POINT('Ctrl Pts',(8.51943721516341,6.55000000039357,-19.5897864145015)) ;
#111830 = CARTESIAN_POINT('Ctrl Pts',(8.5197731018719,6.55000000039098,-19.5894491161473)) ;
#111831 = CARTESIAN_POINT('Ctrl Pts',(8.52085916897642,6.5500000003826,-19.5883584845811)) ;
#111832 = CARTESIAN_POINT('Ctrl Pts',(8.52182399801745,6.55000000033868,-19.5870446208819)) ;
#111833 = CARTESIAN_POINT('Ctrl Pts',(8.52246334063467,6.55000000029842,-19.5856267666595)) ;
#111834 = CARTESIAN_POINT('Ctrl Pts',(8.52278301194328,6.55000000027829,-19.5849178395483)) ;
#111835 = CARTESIAN_POINT('Ctrl Pts',(8.52302131164593,6.55000000025926,-19.5841829148064)) ;
#111836 = CARTESIAN_POINT('Ctrl Pts',(8.52315270869759,6.55000000024662,-19.5834368976348)) ;
#111837 = CARTESIAN_POINT('Ctrl Pts',(8.52328410574924,6.55000000023398,-19.5826908804633)) ;
#111838 = CARTESIAN_POINT('Ctrl Pts',(8.52330860014991,6.55000000022778,-19.5819337708622)) ;
#111839 = CARTESIAN_POINT('Ctrl Pts',(8.52320066085453,6.55000000023233,-19.5811804740327)) ;
#111840 = CARTESIAN_POINT('Ctrl Pts',(8.52284031330747,6.55000000024754,-19.5786656469369)) ;
#111841 = CARTESIAN_POINT('Ctrl Pts',(8.52133564423349,6.55000000029586,-19.5764067380131)) ;
#111842 = CARTESIAN_POINT('Ctrl Pts',(8.51965878991878,6.55000000031744,-19.5743986514954)) ;
#111843 = CARTESIAN_POINT('Ctrl Pts',(8.51932554032811,6.55000000032172,-19.573999574483)) ;
#111844 = CARTESIAN_POINT('Ctrl Pts',(8.51898545723477,6.55000000032522,-19.5736103757648)) ;
#111845 = CARTESIAN_POINT('Ctrl Pts',(8.5186461503849,6.55000000032769,-19.5732310123193)) ;
#111846 = CARTESIAN_POINT('Ctrl Pts',(8.51455081658658,6.55000000035749,-19.5686522072032)) ;
#111847 = CARTESIAN_POINT('Ctrl Pts',(8.50963987409776,6.55000000028078,-19.5648202086186)) ;
#111848 = CARTESIAN_POINT('Ctrl Pts',(8.50482177382259,6.55000000018959,-19.5609688701254)) ;
#111849 = CARTESIAN_POINT('Ctrl Pts',(8.5004640292375,6.5500000001071,-19.5574855160012)) ;
#111850 = CARTESIAN_POINT('Ctrl Pts',(8.49606692679174,6.55000000001227,-19.5540490105462)) ;
#111851 = CARTESIAN_POINT('Ctrl Pts',(8.49172374697017,6.55000000000105,-19.5505442543438)) ;
#111852 = CARTESIAN_POINT('',(8.49172374697018,6.55,-22.86)) ;
#111853 = CARTESIAN_POINT('',(-0.9,6.55,-19.47)) ;
#111854 = CARTESIAN_POINT('',(-0.900000000000001,6.55,-22.86)) ;
#111855 = CARTESIAN_POINT('',(1.15,6.55,-19.47)) ;
#111856 = CARTESIAN_POINT('',(1.25,6.55,-19.47)) ;
#111857 = CARTESIAN_POINT('',(1.35,6.55,-19.67)) ;
#111858 = CARTESIAN_POINT('Origin',(1.15,6.55,-19.67)) ;
#111859 = CARTESIAN_POINT('',(1.35,6.55,-20.97)) ;
#111860 = CARTESIAN_POINT('',(1.35,6.55,-21.07)) ;
#111861 = CARTESIAN_POINT('',(1.15,6.55,-21.17)) ;
#111862 = CARTESIAN_POINT('Origin',(1.15,6.55,-20.97)) ;
#111863 = CARTESIAN_POINT('',(-0.9,6.55,-21.17)) ;
#111864 = CARTESIAN_POINT('',(1.25,6.55,-21.17)) ;
#111865 = CARTESIAN_POINT('',(-0.9,6.55,-22.86)) ;
#111866 = CARTESIAN_POINT('Origin',(1.25,5.3,-22.86)) ;
#111867 = CARTESIAN_POINT('',(1.25,3.15,-21.9631676725155)) ;
#111868 = CARTESIAN_POINT('',(1.25,3.04189189189189,-21.7855279241354)) ;
#111869 = CARTESIAN_POINT('Origin',(1.25,2.95,-21.9631676725155)) ;
#111870 = CARTESIAN_POINT('',(1.25,3.15,-22.86)) ;
#111871 = CARTESIAN_POINT('',(1.25,4.45,-21.9631676725155)) ;
#111872 = CARTESIAN_POINT('',(1.25,4.45,-21.9011388300842)) ;
#111873 = CARTESIAN_POINT('',(1.25,4.55810810810811,-21.7855279241354)) ;
#111874 = CARTESIAN_POINT('Origin',(1.25,4.65,-21.9631676725155)) ;
#111875 = CARTESIAN_POINT('',(1.25,5.26552792413544,-21.0781081081081)) ;
#111876 = CARTESIAN_POINT('Origin',(1.25,3.8,-20.32)) ;
#111877 = CARTESIAN_POINT('',(1.25,5.4431676725155,-20.97)) ;
#111878 = CARTESIAN_POINT('Origin',(1.25,5.4431676725155,-21.17)) ;
#111879 = CARTESIAN_POINT('',(1.25,6.45,-20.97)) ;
#111880 = CARTESIAN_POINT('',(1.25,6.55,-20.97)) ;
#111881 = CARTESIAN_POINT('',(1.25,6.45,-19.67)) ;
#111882 = CARTESIAN_POINT('',(1.25,6.45,-19.57)) ;
#111883 = CARTESIAN_POINT('',(1.25,5.4431676725155,-19.67)) ;
#111884 = CARTESIAN_POINT('',(1.25,5.38113883008419,-19.67)) ;
#111885 = CARTESIAN_POINT('',(1.25,5.26552792413544,-19.5618918918919)) ;
#111886 = CARTESIAN_POINT('Origin',(1.25,5.4431676725155,-19.47)) ;
#111887 = CARTESIAN_POINT('',(1.25,4.55810810810811,-18.8544720758646)) ;
#111888 = CARTESIAN_POINT('Origin',(1.25,3.8,-20.32)) ;
#111889 = CARTESIAN_POINT('',(1.25,4.45,-18.6768323274845)) ;
#111890 = CARTESIAN_POINT('Origin',(1.25,4.65,-18.6768323274845)) ;
#111891 = CARTESIAN_POINT('',(1.25,4.45,-17.78)) ;
#111892 = CARTESIAN_POINT('',(1.25,3.15,-18.6768323274845)) ;
#111893 = CARTESIAN_POINT('',(1.25,3.15,-18.7388611699158)) ;
#111894 = CARTESIAN_POINT('',(1.25,3.04189189189189,-18.8544720758646)) ;
#111895 = CARTESIAN_POINT('Origin',(1.25,2.95,-18.6768323274845)) ;
#111896 = CARTESIAN_POINT('',(1.25,2.33447207586456,-19.5618918918919)) ;
#111897 = CARTESIAN_POINT('Origin',(1.25,3.8,-20.32)) ;
#111898 = CARTESIAN_POINT('',(1.25,2.1568323274845,-19.67)) ;
#111899 = CARTESIAN_POINT('Origin',(1.25,2.1568323274845,-19.47)) ;
#111900 = CARTESIAN_POINT('',(1.25,0.973783447787483,-19.67)) ;
#111901 = CARTESIAN_POINT('',(1.25,0.895262490344437,-19.67)) ;
#111902 = CARTESIAN_POINT('',(1.25,0.973783447787483,-20.97)) ;
#111903 = CARTESIAN_POINT('Origin',(1.25,3.8,-20.32)) ;
#111904 = CARTESIAN_POINT('',(1.25,2.1568323274845,-20.97)) ;
#111905 = CARTESIAN_POINT('',(1.25,2.21886116991581,-20.97)) ;
#111906 = CARTESIAN_POINT('',(1.25,2.33447207586456,-21.0781081081081)) ;
#111907 = CARTESIAN_POINT('Origin',(1.25,2.1568323274845,-21.17)) ;
#111908 = CARTESIAN_POINT('Origin',(1.25,3.8,-20.32)) ;
#111909 = CARTESIAN_POINT('Origin',(-2.,0.,-22.86)) ;
#111910 = CARTESIAN_POINT('',(0.899999999999999,0.,-21.92)) ;
#111911 = CARTESIAN_POINT('',(1.1,0.,-21.72)) ;
#111912 = CARTESIAN_POINT('Origin',(0.899999999999999,0.,-21.72)) ;
#111913 = CARTESIAN_POINT('',(-2.,0.,-21.92)) ;
#111914 = CARTESIAN_POINT('',(-2.,0.,-21.92)) ;
#111915 = CARTESIAN_POINT('',(-2.,0.,-22.86)) ;
#111916 = CARTESIAN_POINT('',(9.9,0.,-22.86)) ;
#111917 = CARTESIAN_POINT('',(-2.,0.,-18.72)) ;
#111918 = CARTESIAN_POINT('',(-2.,0.,-22.86)) ;
#111919 = CARTESIAN_POINT('',(0.899999999999999,0.,-18.72)) ;
#111920 = CARTESIAN_POINT('',(0.999999999999999,0.,-18.72)) ;
#111921 = CARTESIAN_POINT('',(1.1,0.,-18.92)) ;
#111922 = CARTESIAN_POINT('Origin',(0.899999999999999,0.,-18.92)) ;
#111923 = CARTESIAN_POINT('',(1.1,0.,-21.82)) ;
#111924 = CARTESIAN_POINT('Origin',(-2.,7.65,-22.86)) ;
#111925 = CARTESIAN_POINT('',(-2.,6.9,-18.72)) ;
#111926 = CARTESIAN_POINT('',(-2.,7.1,-18.92)) ;
#111927 = CARTESIAN_POINT('Origin',(-2.,6.9,-18.92)) ;
#111928 = CARTESIAN_POINT('',(-2.,-1.13380619344889E-17,-18.72)) ;
#111929 = CARTESIAN_POINT('',(-2.,7.55,-22.86)) ;
#111930 = CARTESIAN_POINT('',(-2.,6.9,-21.92)) ;
#111931 = CARTESIAN_POINT('',(-2.,7.,-21.92)) ;
#111932 = CARTESIAN_POINT('',(-2.,7.1,-21.72)) ;
#111933 = CARTESIAN_POINT('Origin',(-2.,6.9,-21.72)) ;
#111934 = CARTESIAN_POINT('',(-2.,7.1,-18.82)) ;
#111935 = CARTESIAN_POINT('Origin',(-1.8,7.,-18.82)) ;
#111936 = CARTESIAN_POINT('',(-1.7,0.1,-18.82)) ;
#111937 = CARTESIAN_POINT('',(-1.9,0.1,-18.82)) ;
#111938 = CARTESIAN_POINT('',(-2.,0.1,-18.82)) ;
#111939 = CARTESIAN_POINT('',(-1.9,0.3,-18.82)) ;
#111940 = CARTESIAN_POINT('',(-1.9,7.,-18.82)) ;
#111941 = CARTESIAN_POINT('Origin',(-1.7,0.3,-18.82)) ;
#111942 = CARTESIAN_POINT('Origin',(-1.8,7.,-21.82)) ;
#111943 = CARTESIAN_POINT('',(-1.9,0.3,-21.82)) ;
#111944 = CARTESIAN_POINT('',(-1.7,0.1,-21.82)) ;
#111945 = CARTESIAN_POINT('Origin',(-1.7,0.3,-21.82)) ;
#111946 = CARTESIAN_POINT('',(-1.9,0.1,-21.82)) ;
#111947 = CARTESIAN_POINT('',(-1.9,1.23908819712629E-17,-21.82)) ;
#111948 = CARTESIAN_POINT('',(0.999999999999999,0.1,-21.82)) ;
#111949 = CARTESIAN_POINT('Origin',(-1.8,-2.2514151555628E-16,-20.32)) ;
#111950 = CARTESIAN_POINT('',(-1.8,4.6,-20.97)) ;
#111951 = CARTESIAN_POINT('',(-1.8,4.6,-19.67)) ;
#111952 = CARTESIAN_POINT('',(-1.8,4.6,-19.77)) ;
#111953 = CARTESIAN_POINT('',(-1.8,0.3,-19.67)) ;
#111954 = CARTESIAN_POINT('',(-1.8,0.2,-19.67)) ;
#111955 = CARTESIAN_POINT('',(-1.8,0.3,-18.92)) ;
#111956 = CARTESIAN_POINT('',(-1.8,0.3,-18.82)) ;
#111957 = CARTESIAN_POINT('',(-1.8,6.9,-18.92)) ;
#111958 = CARTESIAN_POINT('',(-1.8,-5.16691679585995E-17,-18.92)) ;
#111959 = CARTESIAN_POINT('',(-1.8,6.9,-21.72)) ;
#111960 = CARTESIAN_POINT('',(-1.8,6.9,-20.32)) ;
#111961 = CARTESIAN_POINT('',(-1.8,0.3,-21.72)) ;
#111962 = CARTESIAN_POINT('',(-1.8,-3.98613863153961E-16,-21.72)) ;
#111963 = CARTESIAN_POINT('',(-1.8,0.3,-20.97)) ;
#111964 = CARTESIAN_POINT('',(-1.8,0.3,-20.87)) ;
#111965 = CARTESIAN_POINT('',(-1.8,4.5,-20.97)) ;
#111966 = CARTESIAN_POINT('Origin',(0.549999999999999,4.5,-19.77)) ;
#111967 = CARTESIAN_POINT('',(-1.7,0.3,-19.77)) ;
#111968 = CARTESIAN_POINT('',(-1.7,4.4,-19.77)) ;
#111969 = CARTESIAN_POINT('',(-1.7,4.5,-19.77)) ;
#111970 = CARTESIAN_POINT('',(0.45,4.4,-19.77)) ;
#111971 = CARTESIAN_POINT('',(0.45,4.4,-19.77)) ;
#111972 = CARTESIAN_POINT('',(0.45,0.3,-19.77)) ;
#111973 = CARTESIAN_POINT('',(0.45,4.5,-19.77)) ;
#111974 = CARTESIAN_POINT('',(0.549999999999999,0.3,-19.77)) ;
#111975 = CARTESIAN_POINT('Origin',(0.549999999999999,4.5,-20.87)) ;
#111976 = CARTESIAN_POINT('',(0.45,0.3,-20.87)) ;
#111977 = CARTESIAN_POINT('',(0.45,4.4,-20.87)) ;
#111978 = CARTESIAN_POINT('',(0.45,4.5,-20.87)) ;
#111979 = CARTESIAN_POINT('',(-1.7,4.4,-20.87)) ;
#111980 = CARTESIAN_POINT('',(-1.7,4.4,-20.87)) ;
#111981 = CARTESIAN_POINT('',(-1.7,0.3,-20.87)) ;
#111982 = CARTESIAN_POINT('',(-1.7,0.2,-20.87)) ;
#111983 = CARTESIAN_POINT('',(0.549999999999999,0.3,-20.87)) ;
#111984 = CARTESIAN_POINT('Origin',(0.549999999999999,4.5,-20.87)) ;
#111985 = CARTESIAN_POINT('',(-1.7,4.5,-19.87)) ;
#111986 = CARTESIAN_POINT('',(-1.7,4.5,-20.77)) ;
#111987 = CARTESIAN_POINT('',(-1.7,4.5,-20.87)) ;
#111988 = CARTESIAN_POINT('',(0.45,4.5,-20.77)) ;
#111989 = CARTESIAN_POINT('',(0.45,4.5,-20.77)) ;
#111990 = CARTESIAN_POINT('',(0.45,4.5,-19.87)) ;
#111991 = CARTESIAN_POINT('',(0.45,4.5,-20.87)) ;
#111992 = CARTESIAN_POINT('',(-1.7,4.5,-19.87)) ;
#111993 = CARTESIAN_POINT('Origin',(0.55,3.09772049281573E-17,-20.32)) ;
#111994 = CARTESIAN_POINT('',(0.55,2.61224989991992,-20.72)) ;
#111995 = CARTESIAN_POINT('',(0.55,2.65280931275608,-20.77)) ;
#111996 = CARTESIAN_POINT('Ctrl Pts',(0.55,2.61224989991992,-20.72)) ;
#111997 = CARTESIAN_POINT('Ctrl Pts',(0.55,2.61224989991992,-20.723869744162)) ;
#111998 = CARTESIAN_POINT('Ctrl Pts',(0.55,2.61317624258758,-20.7284201039157)) ;
#111999 = CARTESIAN_POINT('Ctrl Pts',(0.55,2.61634258087509,-20.7366330008589)) ;
#112000 = CARTESIAN_POINT('Ctrl Pts',(0.55,2.61951410407877,-20.7416304286453)) ;
#112001 = CARTESIAN_POINT('Ctrl Pts',(0.55,2.63040394024853,-20.7549387190702)) ;
#112002 = CARTESIAN_POINT('Ctrl Pts',(0.55,2.64148366881061,-20.7631705809674)) ;
#112003 = CARTESIAN_POINT('Ctrl Pts',(0.55,2.65280931275608,-20.77)) ;
#112004 = CARTESIAN_POINT('',(0.55,0.3,-20.77)) ;
#112005 = CARTESIAN_POINT('',(0.55,1.39397422176708E-16,-20.77)) ;
#112006 = CARTESIAN_POINT('',(0.55,0.3,-19.87)) ;
#112007 = CARTESIAN_POINT('',(0.55,0.3,-19.77)) ;
#112008 = CARTESIAN_POINT('',(0.55,2.65280931275594,-19.8700000000001)) ;
#112009 = CARTESIAN_POINT('',(0.55,6.35032701027224E-17,-19.87)) ;
#112010 = CARTESIAN_POINT('',(0.55,2.61224989991992,-19.92)) ;
#112011 = CARTESIAN_POINT('Ctrl Pts',(0.55,2.65280931275593,-19.8700000000001)) ;
#112012 = CARTESIAN_POINT('Ctrl Pts',(0.55,2.64148366881051,-19.8768294190327)) ;
#112013 = CARTESIAN_POINT('Ctrl Pts',(0.55,2.63040394024849,-19.8850612809299)) ;
#112014 = CARTESIAN_POINT('Ctrl Pts',(0.55,2.61951410407877,-19.8983695713547)) ;
#112015 = CARTESIAN_POINT('Ctrl Pts',(0.55,2.61634258087509,-19.9033669991411)) ;
#112016 = CARTESIAN_POINT('Ctrl Pts',(0.55,2.61317624258758,-19.9115798960843)) ;
#112017 = CARTESIAN_POINT('Ctrl Pts',(0.55,2.61224989991992,-19.916130255838)) ;
#112018 = CARTESIAN_POINT('Ctrl Pts',(0.55,2.61224989991992,-19.92)) ;
#112019 = CARTESIAN_POINT('',(0.55,2.61224989991992,-19.82)) ;
#112020 = CARTESIAN_POINT('Origin',(0.,0.2,-20.32)) ;
#112021 = CARTESIAN_POINT('',(-1.7,0.2,-20.97)) ;
#112022 = CARTESIAN_POINT('',(-1.7,0.2,-21.72)) ;
#112023 = CARTESIAN_POINT('',(-1.7,0.2,-21.82)) ;
#112024 = CARTESIAN_POINT('',(0.899999999999999,0.2,-21.72)) ;
#112025 = CARTESIAN_POINT('',(0.999999999999999,0.2,-21.72)) ;
#112026 = CARTESIAN_POINT('',(0.899999999999999,0.2,-18.92)) ;
#112027 = CARTESIAN_POINT('',(0.899999999999999,0.2,-18.82)) ;
#112028 = CARTESIAN_POINT('',(-1.7,0.2,-18.92)) ;
#112029 = CARTESIAN_POINT('',(-1.8,0.2,-18.92)) ;
#112030 = CARTESIAN_POINT('',(-1.7,0.2,-19.67)) ;
#112031 = CARTESIAN_POINT('',(-1.7,0.2,-19.77)) ;
#112032 = CARTESIAN_POINT('',(0.65,0.2,-19.67)) ;
#112033 = CARTESIAN_POINT('',(-1.16429916652874E-32,0.2,-19.67)) ;
#112034 = CARTESIAN_POINT('',(0.65,0.2,-20.97)) ;
#112035 = CARTESIAN_POINT('',(0.65,0.2,-20.87)) ;
#112036 = CARTESIAN_POINT('',(-1.35834902761687E-32,0.2,-20.97)) ;
#112037 = CARTESIAN_POINT('Origin',(3.,2.3,-22.86)) ;
#112038 = CARTESIAN_POINT('',(3.,4.2,-19.82)) ;
#112039 = CARTESIAN_POINT('',(3.,3.4,-19.82)) ;
#112040 = CARTESIAN_POINT('',(3.,2.3,-19.82)) ;
#112041 = CARTESIAN_POINT('',(3.,4.3,-19.92)) ;
#112042 = CARTESIAN_POINT('Origin',(3.,4.2,-19.92)) ;
#112043 = CARTESIAN_POINT('',(3.,4.3,-20.72)) ;
#112044 = CARTESIAN_POINT('',(3.,4.3,-22.86)) ;
#112045 = CARTESIAN_POINT('',(3.,4.2,-20.82)) ;
#112046 = CARTESIAN_POINT('Origin',(3.,4.2,-20.72)) ;
#112047 = CARTESIAN_POINT('',(3.,3.4,-20.82)) ;
#112048 = CARTESIAN_POINT('',(3.,2.3,-20.82)) ;
#112049 = CARTESIAN_POINT('',(3.,3.3,-20.72)) ;
#112050 = CARTESIAN_POINT('Origin',(3.,3.4,-20.72)) ;
#112051 = CARTESIAN_POINT('',(3.,3.3,-19.92)) ;
#112052 = CARTESIAN_POINT('',(3.,3.3,-22.86)) ;
#112053 = CARTESIAN_POINT('Origin',(3.,3.4,-19.92)) ;
#112054 = CARTESIAN_POINT('Origin',(-1.,3.8,-20.32)) ;
#112055 = CARTESIAN_POINT('',(-1.,1.6,-22.2821416870349)) ;
#112056 = CARTESIAN_POINT('',(-1.,1.55483870967742,-22.1555519007746)) ;
#112057 = CARTESIAN_POINT('Origin',(-1.,1.40000000000001,-22.2821416870349)) ;
#112058 = CARTESIAN_POINT('',(-1.,1.6,-22.86)) ;
#112059 = CARTESIAN_POINT('',(-1.,2.95,-21.9631676725155)) ;
#112060 = CARTESIAN_POINT('',(-1.,2.95,-20.32)) ;
#112061 = CARTESIAN_POINT('',(-1.,2.1568323274845,-21.17)) ;
#112062 = CARTESIAN_POINT('Origin',(-1.,3.8,-20.32)) ;
#112063 = CARTESIAN_POINT('',(-1.,1.02736587339765,-21.17)) ;
#112064 = CARTESIAN_POINT('',(-1.,3.8,-21.17)) ;
#112065 = CARTESIAN_POINT('Origin',(-1.,3.8,-20.32)) ;
#112066 = CARTESIAN_POINT('Origin',(-1.,3.05,-22.87)) ;
#112067 = CARTESIAN_POINT('',(1.15,3.05,-21.9631676725155)) ;
#112068 = CARTESIAN_POINT('',(1.15,3.05,-21.9011388300842)) ;
#112069 = CARTESIAN_POINT('',(-0.900000000000002,3.05,-21.9631676725155)) ;
#112070 = CARTESIAN_POINT('',(-1.,3.05,-21.9631676725155)) ;
#112071 = CARTESIAN_POINT('',(-0.900000000000002,3.05,-22.87)) ;
#112072 = CARTESIAN_POINT('Origin',(-1.,2.21886116991581,-21.07)) ;
#112073 = CARTESIAN_POINT('',(-0.900000000000002,2.1568323274845,-21.07)) ;
#112074 = CARTESIAN_POINT('',(1.15,2.1568323274845,-21.07)) ;
#112075 = CARTESIAN_POINT('',(1.25,2.1568323274845,-21.07)) ;
#112076 = CARTESIAN_POINT('',(1.15,0.895262490344437,-21.07)) ;
#112077 = CARTESIAN_POINT('',(-0.900000000000002,2.21886116991581,-21.07)) ;
#112078 = CARTESIAN_POINT('Origin',(-1.,3.8,-20.32)) ;
#112079 = CARTESIAN_POINT('',(-0.900000000000002,2.24565220167453,-21.1240540540541)) ;
#112080 = CARTESIAN_POINT('',(-0.900000000000001,2.99594594594595,-21.8743477983255)) ;
#112081 = CARTESIAN_POINT('Origin',(-0.900000000000001,3.8,-20.32)) ;
#112082 = CARTESIAN_POINT('',(1.15,2.99594594594595,-21.8743477983255)) ;
#112083 = CARTESIAN_POINT('',(-1.,2.99594594594595,-21.8743477983255)) ;
#112084 = CARTESIAN_POINT('',(1.15,2.24565220167453,-21.1240540540541)) ;
#112085 = CARTESIAN_POINT('Origin',(1.15,3.8,-20.32)) ;
#112086 = CARTESIAN_POINT('',(-1.,2.24565220167453,-21.1240540540541)) ;
#112087 = CARTESIAN_POINT('Origin',(-1.,3.8,-20.32)) ;
#112088 = CARTESIAN_POINT('',(-0.900000000000002,2.99594594594594,-18.7656522016745)) ;
#112089 = CARTESIAN_POINT('',(-0.900000000000002,2.24565220167453,-19.515945945946)) ;
#112090 = CARTESIAN_POINT('Origin',(-0.900000000000001,3.8,-20.32)) ;
#112091 = CARTESIAN_POINT('',(1.15,2.24565220167453,-19.515945945946)) ;
#112092 = CARTESIAN_POINT('',(-1.,2.24565220167453,-19.515945945946)) ;
#112093 = CARTESIAN_POINT('',(1.15,2.99594594594594,-18.7656522016745)) ;
#112094 = CARTESIAN_POINT('Origin',(1.15,3.8,-20.32)) ;
#112095 = CARTESIAN_POINT('',(-1.,2.99594594594594,-18.7656522016745)) ;
#112096 = CARTESIAN_POINT('Origin',(-1.,2.21886116991581,-19.57)) ;
#112097 = CARTESIAN_POINT('',(1.15,2.1568323274845,-19.57)) ;
#112098 = CARTESIAN_POINT('',(1.15,2.21886116991581,-19.57)) ;
#112099 = CARTESIAN_POINT('',(-0.900000000000002,2.1568323274845,-19.57)) ;
#112100 = CARTESIAN_POINT('',(-1.,2.1568323274845,-19.57)) ;
#112101 = CARTESIAN_POINT('',(-0.900000000000002,0.895262490344437,-19.57)) ;
#112102 = CARTESIAN_POINT('Origin',(-1.,3.05,-17.77)) ;
#112103 = CARTESIAN_POINT('',(-0.900000000000002,3.05,-18.6768323274845)) ;
#112104 = CARTESIAN_POINT('',(1.15,3.05,-18.6768323274845)) ;
#112105 = CARTESIAN_POINT('',(1.25,3.05,-18.6768323274845)) ;
#112106 = CARTESIAN_POINT('',(1.15,3.05,-17.78)) ;
#112107 = CARTESIAN_POINT('',(-0.900000000000002,3.05,-18.7388611699158)) ;
#112108 = CARTESIAN_POINT('Origin',(-1.,3.8,-20.32)) ;
#112109 = CARTESIAN_POINT('',(-1.,2.1568323274845,-19.47)) ;
#112110 = CARTESIAN_POINT('',(-1.,2.95,-18.6768323274845)) ;
#112111 = CARTESIAN_POINT('Origin',(-1.,3.8,-20.32)) ;
#112112 = CARTESIAN_POINT('',(-1.,2.95,-17.78)) ;
#112113 = CARTESIAN_POINT('',(-1.,1.6,-18.3578583129651)) ;
#112114 = CARTESIAN_POINT('',(-1.,1.6,-20.32)) ;
#112115 = CARTESIAN_POINT('',(-1.,1.55483870967743,-18.4844480992254)) ;
#112116 = CARTESIAN_POINT('Origin',(-1.,1.40000000000001,-18.3578583129651)) ;
#112117 = CARTESIAN_POINT('',(-1.,1.02736587339765,-19.47)) ;
#112118 = CARTESIAN_POINT('Origin',(-1.,3.8,-20.32)) ;
#112119 = CARTESIAN_POINT('',(-1.,2.21886116991581,-19.47)) ;
#112120 = CARTESIAN_POINT('Origin',(-1.,3.8,-20.32)) ;
#112121 = CARTESIAN_POINT('',(-1.,5.4431676725155,-21.17)) ;
#112122 = CARTESIAN_POINT('',(-1.,4.65,-21.9631676725155)) ;
#112123 = CARTESIAN_POINT('Origin',(-1.,3.8,-20.32)) ;
#112124 = CARTESIAN_POINT('',(-1.,4.65,-20.32)) ;
#112125 = CARTESIAN_POINT('',(-1.,6.45,-21.17)) ;
#112126 = CARTESIAN_POINT('',(-1.,6.45,-21.07)) ;
#112127 = CARTESIAN_POINT('',(-1.,3.8,-21.17)) ;
#112128 = CARTESIAN_POINT('Origin',(-1.,4.55,-21.9011388300842)) ;
#112129 = CARTESIAN_POINT('',(-0.900000000000001,4.55,-21.9631676725155)) ;
#112130 = CARTESIAN_POINT('',(1.15,4.55,-21.9631676725155)) ;
#112131 = CARTESIAN_POINT('',(1.25,4.55,-21.9631676725155)) ;
#112132 = CARTESIAN_POINT('',(1.15,4.55,-22.86)) ;
#112133 = CARTESIAN_POINT('',(-0.900000000000001,4.55,-21.9011388300842)) ;
#112134 = CARTESIAN_POINT('Origin',(-1.,3.8,-20.32)) ;
#112135 = CARTESIAN_POINT('',(-0.900000000000001,4.60405405405406,-21.8743477983255)) ;
#112136 = CARTESIAN_POINT('',(-0.900000000000001,5.35434779832547,-21.1240540540541)) ;
#112137 = CARTESIAN_POINT('Origin',(-0.900000000000001,3.8,-20.32)) ;
#112138 = CARTESIAN_POINT('',(1.15,5.35434779832547,-21.1240540540541)) ;
#112139 = CARTESIAN_POINT('',(-1.,5.35434779832547,-21.1240540540541)) ;
#112140 = CARTESIAN_POINT('',(1.15,4.60405405405405,-21.8743477983255)) ;
#112141 = CARTESIAN_POINT('Origin',(1.15,3.8,-20.32)) ;
#112142 = CARTESIAN_POINT('',(-1.,4.60405405405406,-21.8743477983255)) ;
#112143 = CARTESIAN_POINT('Origin',(-1.,6.55,-21.07)) ;
#112144 = CARTESIAN_POINT('',(-0.900000000000001,5.4431676725155,-21.07)) ;
#112145 = CARTESIAN_POINT('',(-0.9,6.45,-21.07)) ;
#112146 = CARTESIAN_POINT('',(-0.9,6.55,-21.07)) ;
#112147 = CARTESIAN_POINT('',(1.15,6.45,-21.07)) ;
#112148 = CARTESIAN_POINT('',(-1.,6.45,-21.07)) ;
#112149 = CARTESIAN_POINT('',(1.15,5.4431676725155,-21.07)) ;
#112150 = CARTESIAN_POINT('',(1.15,5.38113883008419,-21.07)) ;
#112151 = CARTESIAN_POINT('',(-1.,5.4431676725155,-21.07)) ;
#112152 = CARTESIAN_POINT('Origin',(-1.,3.8,-20.32)) ;
#112153 = CARTESIAN_POINT('',(-0.900000000000001,5.35434779832547,-19.515945945946)) ;
#112154 = CARTESIAN_POINT('',(-0.900000000000001,4.60405405405405,-18.7656522016745)) ;
#112155 = CARTESIAN_POINT('Origin',(-0.900000000000001,3.8,-20.32)) ;
#112156 = CARTESIAN_POINT('',(1.15,4.60405405405405,-18.7656522016745)) ;
#112157 = CARTESIAN_POINT('',(-1.,4.60405405405405,-18.7656522016745)) ;
#112158 = CARTESIAN_POINT('',(1.15,5.35434779832547,-19.515945945946)) ;
#112159 = CARTESIAN_POINT('Origin',(1.15,3.8,-20.32)) ;
#112160 = CARTESIAN_POINT('',(-1.,5.35434779832547,-19.515945945946)) ;
#112161 = CARTESIAN_POINT('Origin',(-1.,4.55,-18.7388611699158)) ;
#112162 = CARTESIAN_POINT('',(1.15,4.55,-18.6768323274845)) ;
#112163 = CARTESIAN_POINT('',(1.15,4.55,-18.7388611699158)) ;
#112164 = CARTESIAN_POINT('',(-0.900000000000001,4.55,-18.6768323274845)) ;
#112165 = CARTESIAN_POINT('',(-1.,4.55,-18.6768323274845)) ;
#112166 = CARTESIAN_POINT('',(-0.900000000000001,4.55,-17.78)) ;
#112167 = CARTESIAN_POINT('Origin',(-1.,6.55,-19.57)) ;
#112168 = CARTESIAN_POINT('',(1.15,5.4431676725155,-19.57)) ;
#112169 = CARTESIAN_POINT('',(1.15,6.45,-19.57)) ;
#112170 = CARTESIAN_POINT('',(1.15,6.55,-19.57)) ;
#112171 = CARTESIAN_POINT('',(-0.9,6.45,-19.57)) ;
#112172 = CARTESIAN_POINT('',(-1.,6.45,-19.57)) ;
#112173 = CARTESIAN_POINT('',(-0.900000000000001,5.4431676725155,-19.57)) ;
#112174 = CARTESIAN_POINT('',(-0.900000000000001,5.38113883008419,-19.57)) ;
#112175 = CARTESIAN_POINT('',(1.25,5.4431676725155,-19.57)) ;
#112176 = CARTESIAN_POINT('Origin',(-1.,3.8,-20.32)) ;
#112177 = CARTESIAN_POINT('',(-1.,5.4431676725155,-19.47)) ;
#112178 = CARTESIAN_POINT('',(-1.,6.45,-19.47)) ;
#112179 = CARTESIAN_POINT('',(-1.,6.55,-19.47)) ;
#112180 = CARTESIAN_POINT('',(-1.,6.45,-20.32)) ;
#112181 = CARTESIAN_POINT('',(-1.,4.65,-18.6768323274845)) ;
#112182 = CARTESIAN_POINT('',(-1.,4.65,-18.7388611699158)) ;
#112183 = CARTESIAN_POINT('Origin',(-1.,3.8,-20.32)) ;
#112184 = CARTESIAN_POINT('Origin',(10.,4.35421736843756,-21.195)) ;
#112185 = CARTESIAN_POINT('',(9.91643989873054,7.72792407799439,-21.1810733164551)) ;
#112186 = CARTESIAN_POINT('',(8.58356010126947,8.17221734381475,-20.9589266835449)) ;
#112187 = CARTESIAN_POINT('',(8.47075240319158,8.20981990984071,-20.9401254005319)) ;
#112188 = CARTESIAN_POINT('',(8.58356010126947,6.66256607592813,-20.9589266835449)) ;
#112189 = CARTESIAN_POINT('',(8.58356010126947,6.64863939238321,-20.9589266835449)) ;
#112190 = CARTESIAN_POINT('',(9.91643989873054,6.8847127088383,-21.1810733164551)) ;
#112191 = CARTESIAN_POINT('',(9.98442535909739,6.89604361889945,-21.1924042265162)) ;
#112192 = CARTESIAN_POINT('',(9.91643989873054,7.8,-21.1810733164551)) ;
#112193 = CARTESIAN_POINT('Origin',(8.5,4.35421736843756,-20.945)) ;
#112194 = CARTESIAN_POINT('',(8.5,8.17221734381475,-20.8602872911617)) ;
#112195 = CARTESIAN_POINT('',(8.50000000129681,8.20000000266559,-20.862105625353)) ;
#112196 = CARTESIAN_POINT('Origin',(8.5,8.1787077453077,-21.0490376414923)) ;
#112197 = CARTESIAN_POINT('',(8.5,8.2,-19.7363454436991)) ;
#112198 = CARTESIAN_POINT('',(8.5,6.66256607592813,-19.7797127088383)) ;
#112199 = CARTESIAN_POINT('',(8.5,6.64863939238321,-19.7797127088383)) ;
#112200 = CARTESIAN_POINT('',(8.50000000002143,6.64999999935441,-19.7793178443263)) ;
#112201 = CARTESIAN_POINT('Origin',(8.5,6.65811550064505,-19.5831885106307)) ;
#112202 = CARTESIAN_POINT('',(8.49999999999933,6.65000073218972,-20.8606896909637)) ;
#112203 = CARTESIAN_POINT('',(8.5,6.65,-21.0436393923832)) ;
#112204 = CARTESIAN_POINT('',(8.5,6.66256607592813,-20.8602872911617)) ;
#112205 = CARTESIAN_POINT('Origin',(8.5,6.65133313842863,-21.0570100177546)) ;
#112206 = CARTESIAN_POINT('',(8.5,8.20007071090457,-20.8602872911617)) ;
#112207 = CARTESIAN_POINT('Origin',(8.5,4.35421736843756,-19.695)) ;
#112208 = CARTESIAN_POINT('',(9.91643989873054,6.8847127088383,-19.4589266835449)) ;
#112209 = CARTESIAN_POINT('',(8.58356010126947,6.66256607592813,-19.6810733164551)) ;
#112210 = CARTESIAN_POINT('',(8.48442535909739,6.64604361889945,-19.6975957734838)) ;
#112211 = CARTESIAN_POINT('',(8.58356010126947,8.20007071090456,-19.6810733164551)) ;
#112212 = CARTESIAN_POINT('',(9.91643989873054,7.72792407799439,-19.4589266835449)) ;
#112213 = CARTESIAN_POINT('',(9.97075240319158,7.70981990984071,-19.4498745994681)) ;
#112214 = CARTESIAN_POINT('',(9.91643989873054,6.8,-19.4589266835449)) ;
#112215 = CARTESIAN_POINT('Origin',(8.5,3.65,-19.82)) ;
#112216 = CARTESIAN_POINT('',(8.45734623443633,3.62014236410543,-20.2220655561573)) ;
#112217 = CARTESIAN_POINT('',(8.02582401135442,3.3180768079481,-19.92)) ;
#112218 = CARTESIAN_POINT('',(8.34729988159781,3.54310991711847,-20.1450331091704)) ;
#112219 = CARTESIAN_POINT('',(8.02582401135442,3.31807680794809,-20.72)) ;
#112220 = CARTESIAN_POINT('',(8.02582401135442,3.3180768079481,-19.82)) ;
#112221 = CARTESIAN_POINT('',(8.45734623443633,3.62014236410543,-20.4179344438427)) ;
#112222 = CARTESIAN_POINT('',(8.70083523513316,3.79058466459322,-20.2474921433549)) ;
#112223 = CARTESIAN_POINT('',(8.45734623443633,3.62014236410543,-19.82)) ;
#112224 = CARTESIAN_POINT('Origin',(8.5,3.95,-19.82)) ;
#112225 = CARTESIAN_POINT('',(8.5,3.89793444384266,-20.4179344438427)) ;
#112226 = CARTESIAN_POINT('',(8.5,3.89793444384266,-20.2220655561573)) ;
#112227 = CARTESIAN_POINT('',(8.5,3.89793444384266,-19.82)) ;
#112228 = CARTESIAN_POINT('',(8.5,3.70206555615734,-20.2220655561573)) ;
#112229 = CARTESIAN_POINT('',(8.5,3.95,-20.2220655561573)) ;
#112230 = CARTESIAN_POINT('',(8.5,3.70206555615734,-20.4179344438427)) ;
#112231 = CARTESIAN_POINT('',(8.5,3.70206555615734,-19.82)) ;
#112232 = CARTESIAN_POINT('',(8.5,3.95,-20.4179344438427)) ;
#112233 = CARTESIAN_POINT('Origin',(8.,4.3,-19.82)) ;
#112234 = CARTESIAN_POINT('',(8.45734623443633,3.97985763589457,-20.4179344438427)) ;
#112235 = CARTESIAN_POINT('',(8.02582401135442,4.2819231920519,-20.72)) ;
#112236 = CARTESIAN_POINT('',(8.32457260887054,4.07279917379062,-20.5108759817387)) ;
#112237 = CARTESIAN_POINT('',(8.02582401135442,4.2819231920519,-19.92)) ;
#112238 = CARTESIAN_POINT('',(8.02582401135442,4.2819231920519,-19.82)) ;
#112239 = CARTESIAN_POINT('',(8.45734623443633,3.97985763589457,-20.2220655561573)) ;
#112240 = CARTESIAN_POINT('',(7.97103725533518,4.32027392126537,-19.8816492707865)) ;
#112241 = CARTESIAN_POINT('',(8.45734623443633,3.97985763589457,-19.82)) ;
#112242 = CARTESIAN_POINT('Origin',(1.5,2.3,-19.82)) ;
#112243 = CARTESIAN_POINT('',(7.96847777691809,3.4,-19.82)) ;
#112244 = CARTESIAN_POINT('',(8.,3.4,-19.82)) ;
#112245 = CARTESIAN_POINT('',(7.96847777691809,4.2,-19.82)) ;
#112246 = CARTESIAN_POINT('',(7.96847777691809,4.2,-19.82)) ;
#112247 = CARTESIAN_POINT('',(3.,4.2,-19.82)) ;
#112248 = CARTESIAN_POINT('Origin',(1.5,2.3,-20.82)) ;
#112249 = CARTESIAN_POINT('',(7.96847777691809,4.2,-20.82)) ;
#112250 = CARTESIAN_POINT('',(1.5,4.2,-20.82)) ;
#112251 = CARTESIAN_POINT('',(7.96847777691809,3.4,-20.82)) ;
#112252 = CARTESIAN_POINT('',(7.96847777691809,2.3,-20.82)) ;
#112253 = CARTESIAN_POINT('',(1.5,3.4,-20.82)) ;
#112254 = CARTESIAN_POINT('Origin',(8.,3.3,-19.82)) ;
#112255 = CARTESIAN_POINT('',(7.96847777691809,3.3,-20.72)) ;
#112256 = CARTESIAN_POINT('',(8.,3.3,-20.72)) ;
#112257 = CARTESIAN_POINT('',(7.96847777691809,3.3,-19.92)) ;
#112258 = CARTESIAN_POINT('',(7.96847777691809,3.3,-19.82)) ;
#112259 = CARTESIAN_POINT('',(3.,3.3,-19.92)) ;
#112260 = CARTESIAN_POINT('Origin',(1.5,4.3,-19.82)) ;
#112261 = CARTESIAN_POINT('',(7.96847777691809,4.3,-19.92)) ;
#112262 = CARTESIAN_POINT('',(8.,4.3,-19.92)) ;
#112263 = CARTESIAN_POINT('',(7.96847777691809,4.3,-20.72)) ;
#112264 = CARTESIAN_POINT('',(7.96847777691809,4.3,-19.82)) ;
#112265 = CARTESIAN_POINT('',(1.5,4.3,-20.72)) ;
#112266 = CARTESIAN_POINT('Origin',(1.5,2.3,-19.82)) ;
#112267 = CARTESIAN_POINT('',(-0.4,2.3,-19.82)) ;
#112268 = CARTESIAN_POINT('',(-0.4,-3.36847777691809,-19.82)) ;
#112269 = CARTESIAN_POINT('',(-0.4,-3.4,-19.82)) ;
#112270 = CARTESIAN_POINT('',(0.4,-3.36847777691809,-19.82)) ;
#112271 = CARTESIAN_POINT('',(0.4,-3.36847777691809,-19.82)) ;
#112272 = CARTESIAN_POINT('',(0.4,2.29999999999999,-19.82)) ;
#112273 = CARTESIAN_POINT('',(0.4,2.29999999999999,-19.82)) ;
#112274 = CARTESIAN_POINT('',(0.536602540378444,2.83090991212703,-19.82)) ;
#112275 = CARTESIAN_POINT('Origin',(1.5,2.3,-19.82)) ;
#112276 = CARTESIAN_POINT('',(0.536602540378444,3.93764017256378,-19.82)) ;
#112277 = CARTESIAN_POINT('',(0.536602540378444,2.83090991212703,-19.82)) ;
#112278 = CARTESIAN_POINT('Origin',(1.5,2.3,-19.82)) ;
#112279 = CARTESIAN_POINT('Origin',(1.5,2.3,-20.82)) ;
#112280 = CARTESIAN_POINT('',(0.4,2.29999999999999,-20.82)) ;
#112281 = CARTESIAN_POINT('',(0.4,-3.36847777691809,-20.82)) ;
#112282 = CARTESIAN_POINT('',(0.4,2.3,-20.82)) ;
#112283 = CARTESIAN_POINT('',(-0.4,-3.36847777691809,-20.82)) ;
#112284 = CARTESIAN_POINT('',(1.5,-3.36847777691809,-20.82)) ;
#112285 = CARTESIAN_POINT('',(-0.4,2.3,-20.82)) ;
#112286 = CARTESIAN_POINT('',(-0.4,2.3,-20.82)) ;
#112287 = CARTESIAN_POINT('',(0.536602540378444,3.93764017256378,-20.82)) ;
#112288 = CARTESIAN_POINT('Origin',(1.5,2.3,-20.82)) ;
#112289 = CARTESIAN_POINT('',(0.536602540378444,2.83090991212703,-20.82)) ;
#112290 = CARTESIAN_POINT('',(0.536602540378444,3.93764017256378,-20.82)) ;
#112291 = CARTESIAN_POINT('Origin',(1.5,2.3,-20.82)) ;
#112292 = CARTESIAN_POINT('Origin',(1.5,2.3,-19.82)) ;
#112293 = CARTESIAN_POINT('',(-0.5,2.3,-19.92)) ;
#112294 = CARTESIAN_POINT('',(-0.5,2.3,-20.72)) ;
#112295 = CARTESIAN_POINT('',(-0.5,2.3,-19.82)) ;
#112296 = CARTESIAN_POINT('Origin',(1.5,2.3,-19.92)) ;
#112297 = CARTESIAN_POINT('Origin',(1.5,2.3,-20.72)) ;
#112298 = CARTESIAN_POINT('Origin',(-0.5,-3.4,-19.82)) ;
#112299 = CARTESIAN_POINT('',(-0.5,-3.36847777691809,-20.72)) ;
#112300 = CARTESIAN_POINT('',(-0.5,-3.4,-20.72)) ;
#112301 = CARTESIAN_POINT('',(-0.5,-3.36847777691809,-19.92)) ;
#112302 = CARTESIAN_POINT('',(-0.5,-3.36847777691809,-19.82)) ;
#112303 = CARTESIAN_POINT('',(-0.5,2.3,-19.92)) ;
#112304 = CARTESIAN_POINT('Origin',(-0.15,-3.9,-19.82)) ;
#112305 = CARTESIAN_POINT('',(-0.179857635894567,-3.85734623443633,-20.2220655561573)) ;
#112306 = CARTESIAN_POINT('',(-0.481923192051905,-3.42582401135442,-19.92)) ;
#112307 = CARTESIAN_POINT('',(-0.256890082881532,-3.74729988159781,-20.1450331091704)) ;
#112308 = CARTESIAN_POINT('',(-0.481923192051905,-3.42582401135442,-20.72)) ;
#112309 = CARTESIAN_POINT('',(-0.481923192051905,-3.42582401135442,-19.82)) ;
#112310 = CARTESIAN_POINT('',(-0.179857635894567,-3.85734623443633,-20.4179344438427)) ;
#112311 = CARTESIAN_POINT('',(-0.00941533540678435,-4.10083523513317,-20.2474921433549)) ;
#112312 = CARTESIAN_POINT('',(-0.179857635894567,-3.85734623443633,-19.82)) ;
#112313 = CARTESIAN_POINT('Origin',(0.15,-3.9,-19.82)) ;
#112314 = CARTESIAN_POINT('',(0.0979344438426627,-3.9,-20.4179344438427)) ;
#112315 = CARTESIAN_POINT('',(0.0979344438426627,-3.9,-20.2220655561573)) ;
#112316 = CARTESIAN_POINT('',(0.0979344438426627,-3.9,-19.82)) ;
#112317 = CARTESIAN_POINT('',(-0.0979344438426628,-3.9,-20.2220655561573)) ;
#112318 = CARTESIAN_POINT('',(0.15,-3.9,-20.2220655561573)) ;
#112319 = CARTESIAN_POINT('',(-0.0979344438426628,-3.9,-20.4179344438427)) ;
#112320 = CARTESIAN_POINT('',(-0.0979344438426628,-3.9,-19.82)) ;
#112321 = CARTESIAN_POINT('',(0.15,-3.9,-20.4179344438427)) ;
#112322 = CARTESIAN_POINT('Origin',(0.5,-3.4,-19.82)) ;
#112323 = CARTESIAN_POINT('',(0.179857635894567,-3.85734623443633,-20.4179344438427)) ;
#112324 = CARTESIAN_POINT('',(0.481923192051904,-3.42582401135442,-20.72)) ;
#112325 = CARTESIAN_POINT('',(0.272799173790623,-3.72457260887054,-20.5108759817387)) ;
#112326 = CARTESIAN_POINT('',(0.481923192051904,-3.42582401135442,-19.92)) ;
#112327 = CARTESIAN_POINT('',(0.481923192051904,-3.42582401135442,-19.82)) ;
#112328 = CARTESIAN_POINT('',(0.179857635894567,-3.85734623443633,-20.2220655561573)) ;
#112329 = CARTESIAN_POINT('',(0.520273921265371,-3.37103725533519,-19.8816492707865)) ;
#112330 = CARTESIAN_POINT('',(0.179857635894567,-3.85734623443633,-19.82)) ;
#112331 = CARTESIAN_POINT('Origin',(0.5,2.29999999999999,-19.82)) ;
#112332 = CARTESIAN_POINT('',(0.500000000000001,2.29999999999999,-19.92)) ;
#112333 = CARTESIAN_POINT('',(0.5,-3.36847777691809,-19.92)) ;
#112334 = CARTESIAN_POINT('',(0.5,-3.4,-19.92)) ;
#112335 = CARTESIAN_POINT('',(0.5,-3.36847777691809,-20.72)) ;
#112336 = CARTESIAN_POINT('',(0.5,-3.36847777691809,-19.82)) ;
#112337 = CARTESIAN_POINT('',(0.500000000000001,2.29999999999999,-20.72)) ;
#112338 = CARTESIAN_POINT('',(0.5,2.29999999999999,-20.72)) ;
#112339 = CARTESIAN_POINT('',(0.500000000000001,2.29999999999999,-19.82)) ;
#112340 = CARTESIAN_POINT('Origin',(1.5,2.3,-19.82)) ;
#112341 = CARTESIAN_POINT('Origin',(1.5,2.3,-19.92)) ;
#112342 = CARTESIAN_POINT('Origin',(1.5,2.3,-20.72)) ;
#112343 = CARTESIAN_POINT('Origin',(8.,2.68967221921331,-20.82)) ;
#112344 = CARTESIAN_POINT('',(8.45734623443633,3.70206555615734,-20.4998576358946)) ;
#112345 = CARTESIAN_POINT('',(8.02582401135442,3.4,-20.8019231920519)) ;
#112346 = CARTESIAN_POINT('',(7.75526480758232,3.21060855735952,-20.9913146346924)) ;
#112347 = CARTESIAN_POINT('',(8.02582401135442,4.2,-20.8019231920519)) ;
#112348 = CARTESIAN_POINT('',(8.02582401135442,2.68967221921331,-20.8019231920519)) ;
#112349 = CARTESIAN_POINT('',(8.45734623443633,3.89793444384266,-20.4998576358946)) ;
#112350 = CARTESIAN_POINT('',(8.54034505662341,3.83983526831171,-20.4417584603636)) ;
#112351 = CARTESIAN_POINT('',(8.45734623443633,2.68967221921331,-20.4998576358946)) ;
#112352 = CARTESIAN_POINT('Origin',(8.,2.68967221921331,-19.82)) ;
#112353 = CARTESIAN_POINT('',(8.45734623443633,3.89793444384266,-20.1401423641054)) ;
#112354 = CARTESIAN_POINT('',(8.02582401135442,4.2,-19.8380768079481)) ;
#112355 = CARTESIAN_POINT('',(8.54034505662341,3.83983526831171,-20.1982415396364)) ;
#112356 = CARTESIAN_POINT('',(8.02582401135442,3.4,-19.8380768079481)) ;
#112357 = CARTESIAN_POINT('',(8.02582401135442,3.4,-19.8380768079481)) ;
#112358 = CARTESIAN_POINT('',(8.45734623443633,3.70206555615734,-20.1401423641054)) ;
#112359 = CARTESIAN_POINT('',(7.75526480758232,3.21060855735952,-19.6486853653076)) ;
#112360 = CARTESIAN_POINT('',(8.45734623443633,2.68967221921331,-20.1401423641054)) ;
#112361 = CARTESIAN_POINT('Origin',(-1.11032778078669,-3.9,-20.17)) ;
#112362 = CARTESIAN_POINT('',(0.0979344438426626,-3.85734623443633,-20.1401423641054)) ;
#112363 = CARTESIAN_POINT('',(0.4,-3.42582401135442,-19.8380768079481)) ;
#112364 = CARTESIAN_POINT('',(-0.223548570072128,-4.31660768288603,-20.4616253780202)) ;
#112365 = CARTESIAN_POINT('',(-0.400000000000001,-3.42582401135442,-19.8380768079481)) ;
#112366 = CARTESIAN_POINT('',(-0.400000000000001,-3.42582401135442,-19.8380768079481)) ;
#112367 = CARTESIAN_POINT('',(-0.0979344438426627,-3.85734623443633,-20.1401423641054)) ;
#112368 = CARTESIAN_POINT('',(-0.326007604256636,-3.53152743384494,-19.9120692036915)) ;
#112369 = CARTESIAN_POINT('',(-1.11032778078669,-3.85734623443633,-20.1401423641054)) ;
#112370 = CARTESIAN_POINT('Origin',(-1.11032778078669,-3.4,-20.82)) ;
#112371 = CARTESIAN_POINT('',(-0.0979344438426627,-3.85734623443633,-20.4998576358946)) ;
#112372 = CARTESIAN_POINT('',(-0.4,-3.42582401135442,-20.8019231920519)) ;
#112373 = CARTESIAN_POINT('',(-0.589391442640475,-3.15526480758232,-20.9913146346924)) ;
#112374 = CARTESIAN_POINT('',(0.400000000000001,-3.42582401135442,-20.8019231920519)) ;
#112375 = CARTESIAN_POINT('',(-1.11032778078669,-3.42582401135442,-20.8019231920519)) ;
#112376 = CARTESIAN_POINT('',(0.0979344438426626,-3.85734623443633,-20.4998576358946)) ;
#112377 = CARTESIAN_POINT('',(0.0398352683117103,-3.94034505662341,-20.4417584603636)) ;
#112378 = CARTESIAN_POINT('',(-1.11032778078669,-3.85734623443633,-20.4998576358946)) ;
#112379 = CARTESIAN_POINT('Origin',(10.,1.24999999999998,-22.86)) ;
#112380 = CARTESIAN_POINT('',(9.91643989873054,1.26392668354489,-18.2758381198218)) ;
#112381 = CARTESIAN_POINT('',(9.91643989873054,1.26392668354489,-22.86)) ;
#112382 = CARTESIAN_POINT('',(8.50816364570057,1.49863939238321,-18.3578583129651)) ;
#112383 = CARTESIAN_POINT('Origin',(43.7052916441365,-4.36754860694379,-627.008201735632)) ;
#112384 = CARTESIAN_POINT('',(8.50816364570057,1.49863939238321,-22.86)) ;
#112385 = CARTESIAN_POINT('Origin',(8.49999999999985,3.8,-20.32)) ;
#112386 = CARTESIAN_POINT('',(9.91643989873053,1.24322097942674,-18.3363035641941)) ;
#112387 = CARTESIAN_POINT('',(9.91643989873053,1.24322097942648,-22.3036964358056)) ;
#112388 = CARTESIAN_POINT('Origin',(9.91643989873053,3.8,-20.32)) ;
#112389 = CARTESIAN_POINT('Origin',(36.5480653420491,-40.3802616895407,551.957655191746)) ;
#112390 = CARTESIAN_POINT('Origin',(36.5480652367772,-40.3802620727359,-592.59765448914)) ;
#112391 = CARTESIAN_POINT('Origin',(10.,1.24999999999998,-22.86)) ;
#112392 = CARTESIAN_POINT('',(8.50816364570059,1.49863939238321,-22.2821416870347)) ;
#112393 = CARTESIAN_POINT('',(8.50816364570057,1.49863939238321,-22.86)) ;
#112394 = CARTESIAN_POINT('',(9.91643989873054,1.26392668354489,-22.3641618801782)) ;
#112395 = CARTESIAN_POINT('Origin',(43.705291720328,-4.36754862033938,586.368203082216)) ;
#112396 = CARTESIAN_POINT('',(9.91643989873054,1.26392668354489,-22.86)) ;
#112397 = CARTESIAN_POINT('Origin',(-0.900000000000001,4.65,-20.32)) ;
#112398 = CARTESIAN_POINT('Origin',(-0.900000000000001,4.65,-18.6768323274845)) ;
#112399 = CARTESIAN_POINT('Origin',(-0.900000000000001,4.65,-18.6768323274845)) ;
#112400 = CARTESIAN_POINT('Origin',(-0.900000000000001,4.65,-18.6768323274845)) ;
#112401 = CARTESIAN_POINT('Origin',(-0.900000000000001,4.65,-18.6768323274845)) ;
#112402 = CARTESIAN_POINT('Origin',(1.15,4.45,-18.7388611699158)) ;
#112403 = CARTESIAN_POINT('Origin',(1.15,4.45,-18.6768323274845)) ;
#112404 = CARTESIAN_POINT('Origin',(-1.,4.65,-18.6768323274845)) ;
#112405 = CARTESIAN_POINT('Origin',(1.15,4.65,-18.6768323274845)) ;
#112406 = CARTESIAN_POINT('Origin',(-0.900000000000001,3.8,-20.32)) ;
#112407 = CARTESIAN_POINT('Origin',(-0.900000000000001,5.4431676725155,-19.47)) ;
#112408 = CARTESIAN_POINT('Origin',(1.15,4.65,-18.6768323274845)) ;
#112409 = CARTESIAN_POINT('Origin',(1.15,4.55810810810811,-18.8544720758646)) ;
#112410 = CARTESIAN_POINT('Origin',(-0.900000000000001,5.4431676725155,-19.47)) ;
#112411 = CARTESIAN_POINT('Origin',(-0.900000000000001,5.4431676725155,-19.47)) ;
#112412 = CARTESIAN_POINT('Origin',(-0.900000000000001,5.4431676725155,-19.47)) ;
#112413 = CARTESIAN_POINT('Origin',(-0.900000000000001,4.65,-20.32)) ;
#112414 = CARTESIAN_POINT('Origin',(-0.900000000000001,4.65,-21.9631676725155)) ;
#112415 = CARTESIAN_POINT('Origin',(-1.,4.65,-21.9631676725155)) ;
#112416 = CARTESIAN_POINT('Origin',(1.15,4.65,-21.9631676725155)) ;
#112417 = CARTESIAN_POINT('Origin',(-0.900000000000001,4.65,-21.9631676725155)) ;
#112418 = CARTESIAN_POINT('Origin',(1.15,4.45,-21.9011388300842)) ;
#112419 = CARTESIAN_POINT('Origin',(1.15,4.45,-21.9631676725155)) ;
#112420 = CARTESIAN_POINT('Origin',(1.15,3.8,-20.32)) ;
#112421 = CARTESIAN_POINT('Origin',(1.15,5.26552792413544,-19.5618918918919)) ;
#112422 = CARTESIAN_POINT('Origin',(-1.,5.4431676725155,-19.47)) ;
#112423 = CARTESIAN_POINT('Origin',(1.15,5.4431676725155,-19.47)) ;
#112424 = CARTESIAN_POINT('Origin',(-0.900000000000001,3.8,-19.47)) ;
#112425 = CARTESIAN_POINT('Origin',(-0.9,6.45,-19.47)) ;
#112426 = CARTESIAN_POINT('Origin',(-0.9,6.45,-20.32)) ;
#112427 = CARTESIAN_POINT('Origin',(-0.9,6.45,-19.47)) ;
#112428 = CARTESIAN_POINT('Origin',(-0.900000000000001,4.65,-21.9631676725155)) ;
#112429 = CARTESIAN_POINT('Origin',(-0.900000000000001,4.65,-21.9631676725155)) ;
#112430 = CARTESIAN_POINT('Origin',(1.15,4.65,-21.9631676725155)) ;
#112431 = CARTESIAN_POINT('Origin',(1.15,4.55810810810811,-21.7855279241354)) ;
#112432 = CARTESIAN_POINT('Origin',(1.15,5.4431676725155,-19.47)) ;
#112433 = CARTESIAN_POINT('Origin',(1.15,5.4431676725155,-19.67)) ;
#112434 = CARTESIAN_POINT('Origin',(-0.9,6.45,-19.47)) ;
#112435 = CARTESIAN_POINT('Origin',(-0.9,6.45,-19.47)) ;
#112436 = CARTESIAN_POINT('Origin',(-0.900000000000001,3.8,-20.32)) ;
#112437 = CARTESIAN_POINT('Origin',(-0.900000000000001,5.4431676725155,-21.17)) ;
#112438 = CARTESIAN_POINT('Origin',(-1.,5.4431676725155,-21.17)) ;
#112439 = CARTESIAN_POINT('Origin',(1.15,5.4431676725155,-21.17)) ;
#112440 = CARTESIAN_POINT('Origin',(-0.900000000000001,5.4431676725155,-21.17)) ;
#112441 = CARTESIAN_POINT('Origin',(1.15,3.8,-20.32)) ;
#112442 = CARTESIAN_POINT('Origin',(1.15,5.26552792413544,-21.0781081081081)) ;
#112443 = CARTESIAN_POINT('Origin',(1.15,6.55,-19.67)) ;
#112444 = CARTESIAN_POINT('Origin',(1.15,6.45,-19.67)) ;
#112445 = CARTESIAN_POINT('Origin',(1.25,6.45,-19.47)) ;
#112446 = CARTESIAN_POINT('Origin',(1.15,6.45,-19.47)) ;
#112447 = CARTESIAN_POINT('Origin',(-0.900000000000001,5.4431676725155,-21.17)) ;
#112448 = CARTESIAN_POINT('Origin',(-0.900000000000001,5.4431676725155,-21.17)) ;
#112449 = CARTESIAN_POINT('Origin',(1.15,5.4431676725155,-21.17)) ;
#112450 = CARTESIAN_POINT('Origin',(1.15,5.4431676725155,-20.97)) ;
#112451 = CARTESIAN_POINT('Origin',(1.15,6.45,-19.67)) ;
#112452 = CARTESIAN_POINT('Origin',(1.35,6.45,-19.67)) ;
#112453 = CARTESIAN_POINT('Origin',(-0.9,6.45,-20.32)) ;
#112454 = CARTESIAN_POINT('Origin',(-0.9,6.45,-21.17)) ;
#112455 = CARTESIAN_POINT('Origin',(-0.900000000000001,3.8,-21.17)) ;
#112456 = CARTESIAN_POINT('Origin',(-0.9,6.45,-21.17)) ;
#112457 = CARTESIAN_POINT('Origin',(1.15,6.55,-20.97)) ;
#112458 = CARTESIAN_POINT('Origin',(1.15,6.45,-20.97)) ;
#112459 = CARTESIAN_POINT('Origin',(1.35,6.45,-22.86)) ;
#112460 = CARTESIAN_POINT('Origin',(1.35,6.45,-20.97)) ;
#112461 = CARTESIAN_POINT('Origin',(-0.9,6.45,-21.17)) ;
#112462 = CARTESIAN_POINT('Origin',(-0.9,6.45,-21.17)) ;
#112463 = CARTESIAN_POINT('Origin',(1.15,6.45,-20.97)) ;
#112464 = CARTESIAN_POINT('Origin',(1.15,6.45,-21.17)) ;
#112465 = CARTESIAN_POINT('Origin',(-1.,6.45,-21.17)) ;
#112466 = CARTESIAN_POINT('Origin',(-1.7,0.3,-20.97)) ;
#112467 = CARTESIAN_POINT('Origin',(-1.7,0.3,-20.97)) ;
#112468 = CARTESIAN_POINT('Origin',(-1.7,0.3,-20.97)) ;
#112469 = CARTESIAN_POINT('Origin',(-1.7,0.3,-20.97)) ;
#112470 = CARTESIAN_POINT('Origin',(0.549999999999999,0.3,-20.97)) ;
#112471 = CARTESIAN_POINT('',(0.508578643762789,0.229289321881395,-20.8992893218813)) ;
#112472 = CARTESIAN_POINT('Ctrl Pts',(0.65,0.200000000000001,-20.97)) ;
#112473 = CARTESIAN_POINT('Ctrl Pts',(0.639834283464219,0.200000000000001,
-20.9649171417321)) ;
#112474 = CARTESIAN_POINT('Ctrl Pts',(0.629316849080676,0.200389688120421,
-20.959657683858)) ;
#112475 = CARTESIAN_POINT('Ctrl Pts',(0.606957334720003,0.202165884217635,
-20.9484679497194)) ;
#112476 = CARTESIAN_POINT('Ctrl Pts',(0.595086727401555,0.203647820493405,
-20.9425227617951)) ;
#112477 = CARTESIAN_POINT('Ctrl Pts',(0.572283837383469,0.207685608830753,
-20.9311067603974)) ;
#112478 = CARTESIAN_POINT('Ctrl Pts',(0.561337481655848,0.210178193247152,
-20.9256298613106)) ;
#112479 = CARTESIAN_POINT('Ctrl Pts',(0.549549942890579,0.213544620664103,
-20.9197406960418)) ;
#112480 = CARTESIAN_POINT('Ctrl Pts',(0.548290718948528,0.213913346521202,
-20.9191116827674)) ;
#112481 = CARTESIAN_POINT('Ctrl Pts',(0.536119229733184,0.217566912232432,
-20.9130327513519)) ;
#112482 = CARTESIAN_POINT('Ctrl Pts',(0.52570691736286,0.221400308602526,
-20.9078422384292)) ;
#112483 = CARTESIAN_POINT('Ctrl Pts',(0.513545110027472,0.226871185484663,
-20.9017711869643)) ;
#112484 = CARTESIAN_POINT('Ctrl Pts',(0.511029334128475,0.228063976698571,
-20.9005146670641)) ;
#112485 = CARTESIAN_POINT('Ctrl Pts',(0.508578643762789,0.229289321881392,
-20.8992893218813)) ;
#112486 = CARTESIAN_POINT('Origin',(0.664280054302503,0.302990743361758,-20.9771421042501)) ;
#112487 = CARTESIAN_POINT('Origin',(-1.7,4.5,-20.97)) ;
#112488 = CARTESIAN_POINT('',(-1.77071067811866,4.45857864376269,-20.8992893218813)) ;
#112489 = CARTESIAN_POINT('Origin',(-1.69703459697577,4.61417009504575,-20.977086685377)) ;
#112490 = CARTESIAN_POINT('Ctrl Pts',(-1.77071067811863,4.45857864376269,
-20.8992893218813)) ;
#112491 = CARTESIAN_POINT('Ctrl Pts',(-1.77521675558369,4.46759079869273,
-20.9037953993464)) ;
#112492 = CARTESIAN_POINT('Ctrl Pts',(-1.77928079264421,4.47748625817284,
-20.9087264816716)) ;
#112493 = CARTESIAN_POINT('Ctrl Pts',(-1.78624680748594,4.49811277056781,
-20.9190208825473)) ;
#112494 = CARTESIAN_POINT('Ctrl Pts',(-1.78918030781741,4.50880509433286,
-20.9243639841482)) ;
#112495 = CARTESIAN_POINT('Ctrl Pts',(-1.79185985500252,4.52101859321837,
-20.9304747545319)) ;
#112496 = CARTESIAN_POINT('Ctrl Pts',(-1.79213045061208,4.522287517226,-20.9311097099085)) ;
#112497 = CARTESIAN_POINT('Ctrl Pts',(-1.7947746790983,4.53504937002851,-20.937496289134)) ;
#112498 = CARTESIAN_POINT('Ctrl Pts',(-1.79657370273652,4.54677936428193,
-20.9433715724062)) ;
#112499 = CARTESIAN_POINT('Ctrl Pts',(-1.79896007643135,4.56920025888385,
-20.9545957747611)) ;
#112500 = CARTESIAN_POINT('Ctrl Pts',(-1.79963010255188,4.57990192168147,
-20.959950075945)) ;
#112501 = CARTESIAN_POINT('Ctrl Pts',(-1.79996164986962,4.59357116034293,
-20.966785573817)) ;
#112502 = CARTESIAN_POINT('Ctrl Pts',(-1.8,4.59680282631913,-20.9684014131596)) ;
#112503 = CARTESIAN_POINT('Ctrl Pts',(-1.8,4.6,-20.97)) ;
#112504 = CARTESIAN_POINT('Origin',(-1.7,0.3,-20.32)) ;
#112505 = CARTESIAN_POINT('Origin',(-1.7,0.3,-21.72)) ;
#112506 = CARTESIAN_POINT('Origin',(0.65,0.3,-20.32)) ;
#112507 = CARTESIAN_POINT('',(0.579289321881345,0.229289321881346,-20.8285786437627)) ;
#112508 = CARTESIAN_POINT('Origin',(0.657086685361009,0.302965403016329,-20.9841700950131)) ;
#112509 = CARTESIAN_POINT('Ctrl Pts',(0.579289321881345,0.229289321881345,
-20.8285786437627)) ;
#112510 = CARTESIAN_POINT('Ctrl Pts',(0.583795399346365,0.224783244416326,
-20.8375907986927)) ;
#112511 = CARTESIAN_POINT('Ctrl Pts',(0.588726481671636,0.220719207355781,
-20.8474862581728)) ;
#112512 = CARTESIAN_POINT('Ctrl Pts',(0.599020882547777,0.213753192513749,
-20.8681127705687)) ;
#112513 = CARTESIAN_POINT('Ctrl Pts',(0.604363984149085,0.210819692182088,
-20.8788050943346)) ;
#112514 = CARTESIAN_POINT('Ctrl Pts',(0.610474754532814,0.208140144997089,
-20.8910185932202)) ;
#112515 = CARTESIAN_POINT('Ctrl Pts',(0.611109709908936,0.207869549387731,
-20.8922875172269)) ;
#112516 = CARTESIAN_POINT('Ctrl Pts',(0.617496289133951,0.205225320901704,
-20.9050493700285)) ;
#112517 = CARTESIAN_POINT('Ctrl Pts',(0.623371572406202,0.203426297263468,
-20.916779364282)) ;
#112518 = CARTESIAN_POINT('Ctrl Pts',(0.634595774761219,0.201039923568638,
-20.9392002588839)) ;
#112519 = CARTESIAN_POINT('Ctrl Pts',(0.639950075945042,0.200369897448119,
-20.9499019216816)) ;
#112520 = CARTESIAN_POINT('Ctrl Pts',(0.646785573817055,0.200038350130375,
-20.963571160343)) ;
#112521 = CARTESIAN_POINT('Ctrl Pts',(0.648401413159587,0.2,-20.9668028263192)) ;
#112522 = CARTESIAN_POINT('Ctrl Pts',(0.65,0.2,-20.97)) ;
#112523 = CARTESIAN_POINT('',(0.579289321881345,0.229289321881345,-19.8114213562373)) ;
#112524 = CARTESIAN_POINT('Ctrl Pts',(0.65,0.2,-19.67)) ;
#112525 = CARTESIAN_POINT('Ctrl Pts',(0.64491714173209,0.2,-19.6801657165358)) ;
#112526 = CARTESIAN_POINT('Ctrl Pts',(0.639657683858026,0.200389688120421,
-19.6906831509195)) ;
#112527 = CARTESIAN_POINT('Ctrl Pts',(0.628467949719372,0.20216588421764,
-19.7130426652803)) ;
#112528 = CARTESIAN_POINT('Ctrl Pts',(0.622522761794955,0.203647820493434,
-19.7249132725989)) ;
#112529 = CARTESIAN_POINT('Ctrl Pts',(0.611106760396054,0.207685608831243,
-19.7477161626195)) ;
#112530 = CARTESIAN_POINT('Ctrl Pts',(0.605629861308111,0.210178193248298,
-19.7586625183495)) ;
#112531 = CARTESIAN_POINT('Ctrl Pts',(0.599740696039384,0.213544620665521,
-19.7704500571145)) ;
#112532 = CARTESIAN_POINT('Ctrl Pts',(0.599111682766073,0.213913346521975,
-19.7717092810543)) ;
#112533 = CARTESIAN_POINT('Ctrl Pts',(0.593032751351765,0.21756691223254,
-19.7838807702673)) ;
#112534 = CARTESIAN_POINT('Ctrl Pts',(0.587842238429117,0.221400308602601,
-19.7942930826376)) ;
#112535 = CARTESIAN_POINT('Ctrl Pts',(0.581771186964304,0.226871185484679,
-19.8064548899728)) ;
#112536 = CARTESIAN_POINT('Ctrl Pts',(0.580514667064145,0.228063976698545,
-19.8089706658717)) ;
#112537 = CARTESIAN_POINT('Ctrl Pts',(0.579289321881345,0.229289321881345,
-19.8114213562373)) ;
#112538 = CARTESIAN_POINT('Origin',(0.657142104237265,0.302990743356481,-19.6557199457236)) ;
#112539 = CARTESIAN_POINT('Origin',(-1.7,4.6,-20.87)) ;
#112540 = CARTESIAN_POINT('',(-1.77071067811866,4.52928932188135,-20.8285786437627)) ;
#112541 = CARTESIAN_POINT('Ctrl Pts',(-1.8,4.6,-20.97)) ;
#112542 = CARTESIAN_POINT('Ctrl Pts',(-1.8,4.5949171417321,-20.9598342834642)) ;
#112543 = CARTESIAN_POINT('Ctrl Pts',(-1.79961031187958,4.58965768385804,
-20.9493168490806)) ;
#112544 = CARTESIAN_POINT('Ctrl Pts',(-1.79783411578236,4.57846794971939,
-20.9269573347197)) ;
#112545 = CARTESIAN_POINT('Ctrl Pts',(-1.79635217950657,4.57252276179498,
-20.9150867274011)) ;
#112546 = CARTESIAN_POINT('Ctrl Pts',(-1.79231439116883,4.56110676039624,
-20.8922838373809)) ;
#112547 = CARTESIAN_POINT('Ctrl Pts',(-1.78982180675186,4.55562986130845,
-20.8813374816513)) ;
#112548 = CARTESIAN_POINT('Ctrl Pts',(-1.78645537933467,4.54974069603971,
-20.8695499428861)) ;
#112549 = CARTESIAN_POINT('Ctrl Pts',(-1.78608665347813,4.54911168276625,
-20.8682907189461)) ;
#112550 = CARTESIAN_POINT('Ctrl Pts',(-1.78243308776747,4.54303275135178,
-20.8561192297327)) ;
#112551 = CARTESIAN_POINT('Ctrl Pts',(-1.77859969139741,4.53784223842912,
-20.8457069173624)) ;
#112552 = CARTESIAN_POINT('Ctrl Pts',(-1.77312881451532,4.53177118696431,
-20.8335451100272)) ;
#112553 = CARTESIAN_POINT('Ctrl Pts',(-1.77193602330146,4.53051466706415,
-20.8310293341283)) ;
#112554 = CARTESIAN_POINT('Ctrl Pts',(-1.77071067811866,4.52928932188135,
-20.8285786437627)) ;
#112555 = CARTESIAN_POINT('Origin',(-1.69700925664257,4.60714210423891,-20.9842800542796)) ;
#112556 = CARTESIAN_POINT('',(-1.77071067811866,4.52928932188135,-19.8114213562373)) ;
#112557 = CARTESIAN_POINT('Origin',(-1.69703459698473,4.60708668535819,-19.6558299049927)) ;
#112558 = CARTESIAN_POINT('Ctrl Pts',(-1.77071067811866,4.52928932188135,
-19.8114213562373)) ;
#112559 = CARTESIAN_POINT('Ctrl Pts',(-1.77521675558368,4.53379539934637,
-19.8024092013073)) ;
#112560 = CARTESIAN_POINT('Ctrl Pts',(-1.77928079264423,4.53872648167165,
-19.7925137418271)) ;
#112561 = CARTESIAN_POINT('Ctrl Pts',(-1.78624680748614,4.54902088254762,
-19.7718872294317)) ;
#112562 = CARTESIAN_POINT('Ctrl Pts',(-1.78918030781772,4.55436398414873,
-19.7611949056661)) ;
#112563 = CARTESIAN_POINT('Ctrl Pts',(-1.79185985500276,4.56047475453246,
-19.7489814067805)) ;
#112564 = CARTESIAN_POINT('Ctrl Pts',(-1.7921304506122,4.56110970990877,-19.7477124827734)) ;
#112565 = CARTESIAN_POINT('Ctrl Pts',(-1.7947746790983,4.56749628913397,-19.7349506299714)) ;
#112566 = CARTESIAN_POINT('Ctrl Pts',(-1.79657370273654,4.57337157240623,
-19.723220635718)) ;
#112567 = CARTESIAN_POINT('Ctrl Pts',(-1.79896007643136,4.58459577476124,
-19.7007997411161)) ;
#112568 = CARTESIAN_POINT('Ctrl Pts',(-1.79963010255188,4.58995007594506,
-19.6900980783184)) ;
#112569 = CARTESIAN_POINT('Ctrl Pts',(-1.79996164986962,4.59678557381705,
-19.676428839657)) ;
#112570 = CARTESIAN_POINT('Ctrl Pts',(-1.8,4.59840141315959,-19.6731971736808)) ;
#112571 = CARTESIAN_POINT('Ctrl Pts',(-1.8,4.6,-19.67)) ;
#112572 = CARTESIAN_POINT('Origin',(-1.7,0.3,-21.72)) ;
#112573 = CARTESIAN_POINT('Origin',(-1.7,0.1,-21.72)) ;
#112574 = CARTESIAN_POINT('Origin',(-1.9,0.3,-21.72)) ;
#112575 = CARTESIAN_POINT('Origin',(1.9668402209837E-32,0.1,-21.72)) ;
#112576 = CARTESIAN_POINT('',(0.899999999999999,0.1,-21.82)) ;
#112577 = CARTESIAN_POINT('',(-1.8,0.1,-21.82)) ;
#112578 = CARTESIAN_POINT('Origin',(0.899999999999999,0.1,-21.72)) ;
#112579 = CARTESIAN_POINT('Origin',(0.899999999999999,0.1,-21.72)) ;
#112580 = CARTESIAN_POINT('',(0.999999999999999,0.1,-21.72)) ;
#112581 = CARTESIAN_POINT('Origin',(0.899999999999999,0.1,-21.72)) ;
#112582 = CARTESIAN_POINT('Origin',(0.899999999999999,0.1,-21.72)) ;
#112583 = CARTESIAN_POINT('Origin',(0.549999999999999,0.3,-19.67)) ;
#112584 = CARTESIAN_POINT('',(0.508578643762786,0.229289321881393,-19.7407106781187)) ;
#112585 = CARTESIAN_POINT('Origin',(0.664170095050064,0.302965403024492,-19.6629133146209)) ;
#112586 = CARTESIAN_POINT('Ctrl Pts',(0.508578643762786,0.229289321881391,
-19.7407106781187)) ;
#112587 = CARTESIAN_POINT('Ctrl Pts',(0.517590798692864,0.224783244416372,
-19.7362046006537)) ;
#112588 = CARTESIAN_POINT('Ctrl Pts',(0.527486258173022,0.220719207355799,
-19.7312735183284)) ;
#112589 = CARTESIAN_POINT('Ctrl Pts',(0.548112770567078,0.213753192514375,
-19.7209791174532)) ;
#112590 = CARTESIAN_POINT('Ctrl Pts',(0.558805094331059,0.210819692183137,
-19.7156360158528)) ;
#112591 = CARTESIAN_POINT('Ctrl Pts',(0.571018593216485,0.208140144997932,
-19.7095252454692)) ;
#112592 = CARTESIAN_POINT('Ctrl Pts',(0.572287517225128,0.207869549388149,
-19.7088902900921)) ;
#112593 = CARTESIAN_POINT('Ctrl Pts',(0.585049370028565,0.20522532090174,
-19.7025037108661)) ;
#112594 = CARTESIAN_POINT('Ctrl Pts',(0.596779364281885,0.203426297263527,
-19.696628427594)) ;
#112595 = CARTESIAN_POINT('Ctrl Pts',(0.619200258883654,0.201039923568666,
-19.685404225239)) ;
#112596 = CARTESIAN_POINT('Ctrl Pts',(0.629901921681228,0.20036989744814,
-19.6800499240552)) ;
#112597 = CARTESIAN_POINT('Ctrl Pts',(0.64357116034274,0.200038350130378,
-19.6732144261831)) ;
#112598 = CARTESIAN_POINT('Ctrl Pts',(0.646802826319035,0.200000000000001,
-19.6715985868405)) ;
#112599 = CARTESIAN_POINT('Ctrl Pts',(0.65,0.200000000000001,-19.67)) ;
#112600 = CARTESIAN_POINT('Origin',(-1.7,0.3,-19.67)) ;
#112601 = CARTESIAN_POINT('Origin',(-1.7,4.5,-19.67)) ;
#112602 = CARTESIAN_POINT('',(-1.77071067811866,4.45857864376269,-19.7407106781187)) ;
#112603 = CARTESIAN_POINT('Ctrl Pts',(-1.8,4.6,-19.67)) ;
#112604 = CARTESIAN_POINT('Ctrl Pts',(-1.8,4.58983428346418,-19.6750828582679)) ;
#112605 = CARTESIAN_POINT('Ctrl Pts',(-1.79961031187958,4.57931684908058,
-19.680342316142)) ;
#112606 = CARTESIAN_POINT('Ctrl Pts',(-1.79783411578237,4.55695733471976,
-19.6915320502806)) ;
#112607 = CARTESIAN_POINT('Ctrl Pts',(-1.79635217950657,4.54508672740122,
-19.697477238205)) ;
#112608 = CARTESIAN_POINT('Ctrl Pts',(-1.79231439116924,4.52228383738322,
-19.7088932396026)) ;
#112609 = CARTESIAN_POINT('Ctrl Pts',(-1.78982180675289,4.51133748165579,
-19.7143701386893)) ;
#112610 = CARTESIAN_POINT('Ctrl Pts',(-1.78645537933594,4.49954994289049,
-19.7202593039581)) ;
#112611 = CARTESIAN_POINT('Ctrl Pts',(-1.78608665347879,4.49829071894825,
-19.7208883172327)) ;
#112612 = CARTESIAN_POINT('Ctrl Pts',(-1.7824330877675,4.48611922973279,-19.7269672486482)) ;
#112613 = CARTESIAN_POINT('Ctrl Pts',(-1.77859969139746,4.47570691736254,
-19.7321577615708)) ;
#112614 = CARTESIAN_POINT('Ctrl Pts',(-1.77312881451533,4.46354511002727,
-19.7382288130357)) ;
#112615 = CARTESIAN_POINT('Ctrl Pts',(-1.77193602330149,4.46102933412832,
-19.7394853329358)) ;
#112616 = CARTESIAN_POINT('Ctrl Pts',(-1.77071067811864,4.45857864376269,
-19.7407106781187)) ;
#112617 = CARTESIAN_POINT('Origin',(-1.69700925663949,4.61428005429195,-19.6628578957552)) ;
#112618 = CARTESIAN_POINT('Origin',(-1.7,0.3,-19.67)) ;
#112619 = CARTESIAN_POINT('Origin',(-1.9,-4.11004745125224E-16,-21.72)) ;
#112620 = CARTESIAN_POINT('',(-1.9,6.9,-21.82)) ;
#112621 = CARTESIAN_POINT('Origin',(-1.9,6.9,-21.72)) ;
#112622 = CARTESIAN_POINT('',(-1.9,7.,-21.82)) ;
#112623 = CARTESIAN_POINT('Origin',(-2.,0.1,-21.92)) ;
#112624 = CARTESIAN_POINT('Origin',(-1.89999999999986,0.100000000000145,-21.9200000000001)) ;
#112625 = CARTESIAN_POINT('Origin',(0.899999999999999,0.1,-21.92)) ;
#112626 = CARTESIAN_POINT('Origin',(0.899999999999999,0.1,-21.72)) ;
#112627 = CARTESIAN_POINT('Origin',(1.1,0.1,-21.72)) ;
#112628 = CARTESIAN_POINT('Origin',(0.899999999999999,0.1,-20.32)) ;
#112629 = CARTESIAN_POINT('',(0.999999999999999,0.1,-18.92)) ;
#112630 = CARTESIAN_POINT('',(0.999999999999999,0.1,-21.82)) ;
#112631 = CARTESIAN_POINT('Origin',(0.899999999999999,0.1,-18.92)) ;
#112632 = CARTESIAN_POINT('Origin',(-1.7,0.3,-19.67)) ;
#112633 = CARTESIAN_POINT('Origin',(-1.7,0.3,-19.67)) ;
#112634 = CARTESIAN_POINT('Origin',(-1.9,6.9,-21.72)) ;
#112635 = CARTESIAN_POINT('',(-1.9,7.,-21.72)) ;
#112636 = CARTESIAN_POINT('Origin',(-1.9,6.9,-21.72)) ;
#112637 = CARTESIAN_POINT('Origin',(-1.9,6.9,-21.72)) ;
#112638 = CARTESIAN_POINT('Origin',(-1.9,7.,-21.92)) ;
#112639 = CARTESIAN_POINT('Origin',(-1.9,6.9,-21.92)) ;
#112640 = CARTESIAN_POINT('Origin',(1.1,0.1,-18.82)) ;
#112641 = CARTESIAN_POINT('Origin',(1.1,0.1,-18.92)) ;
#112642 = CARTESIAN_POINT('Origin',(0.899999999999999,0.1,-18.92)) ;
#112643 = CARTESIAN_POINT('',(0.899999999999999,0.1,-18.82)) ;
#112644 = CARTESIAN_POINT('Origin',(0.899999999999999,0.1,-18.92)) ;
#112645 = CARTESIAN_POINT('Origin',(0.899999999999999,0.1,-18.92)) ;
#112646 = CARTESIAN_POINT('Origin',(-1.7,0.3,-20.32)) ;
#112647 = CARTESIAN_POINT('Origin',(-1.7,0.3,-18.92)) ;
#112648 = CARTESIAN_POINT('Origin',(-1.9,6.9,-20.32)) ;
#112649 = CARTESIAN_POINT('',(-1.9,7.,-18.92)) ;
#112650 = CARTESIAN_POINT('Origin',(-1.9,6.9,-18.92)) ;
#112651 = CARTESIAN_POINT('',(-1.9,7.,-21.82)) ;
#112652 = CARTESIAN_POINT('Origin',(-1.9,6.9,-21.72)) ;
#112653 = CARTESIAN_POINT('Origin',(-1.9,7.1,-21.72)) ;
#112654 = CARTESIAN_POINT('Origin',(0.899999999999999,0.1,-18.92)) ;
#112655 = CARTESIAN_POINT('Origin',(0.899999999999999,0.1,-18.72)) ;
#112656 = CARTESIAN_POINT('Origin',(-1.9668402209837E-32,0.1,-18.92)) ;
#112657 = CARTESIAN_POINT('',(0.999999999999999,0.1,-18.82)) ;
#112658 = CARTESIAN_POINT('Origin',(-1.7,0.1,-18.92)) ;
#112659 = CARTESIAN_POINT('Origin',(-1.7,0.3,-18.92)) ;
#112660 = CARTESIAN_POINT('Origin',(-1.9,0.3,-18.92)) ;
#112661 = CARTESIAN_POINT('Origin',(-1.9,6.9,-18.92)) ;
#112662 = CARTESIAN_POINT('',(-1.9,6.9,-18.82)) ;
#112663 = CARTESIAN_POINT('Origin',(-1.9,6.9,-18.92)) ;
#112664 = CARTESIAN_POINT('Origin',(-1.9,6.9,-18.92)) ;
#112665 = CARTESIAN_POINT('Origin',(-1.9,7.1,-21.82)) ;
#112666 = CARTESIAN_POINT('Origin',(-1.9,7.1,-18.92)) ;
#112667 = CARTESIAN_POINT('Origin',(-1.8,0.1,-18.72)) ;
#112668 = CARTESIAN_POINT('Origin',(-1.90000000000013,0.0999999999998694,
-18.7200000000001)) ;
#112669 = CARTESIAN_POINT('Origin',(-1.9,-6.40600499298624E-17,-18.92)) ;
#112670 = CARTESIAN_POINT('',(-1.9,7.,-18.82)) ;
#112671 = CARTESIAN_POINT('Origin',(-1.9,6.9,-18.92)) ;
#112672 = CARTESIAN_POINT('Origin',(-1.9,6.9,-18.72)) ;
#112673 = CARTESIAN_POINT('Origin',(-1.9,7.,-18.72)) ;
#112674 = CARTESIAN_POINT('Origin',(-0.900000000000002,2.95,-20.32)) ;
#112675 = CARTESIAN_POINT('Origin',(-0.900000000000001,2.95,-21.9631676725155)) ;
#112676 = CARTESIAN_POINT('Origin',(-0.900000000000002,2.95,-21.9631676725155)) ;
#112677 = CARTESIAN_POINT('Origin',(-0.900000000000001,2.95,-21.9631676725155)) ;
#112678 = CARTESIAN_POINT('Origin',(-0.900000000000002,2.95,-21.9631676725155)) ;
#112679 = CARTESIAN_POINT('Origin',(1.15,3.15,-22.87)) ;
#112680 = CARTESIAN_POINT('Origin',(1.15,3.15,-21.9631676725155)) ;
#112681 = CARTESIAN_POINT('Origin',(-1.,2.95,-21.9631676725155)) ;
#112682 = CARTESIAN_POINT('Origin',(1.15,2.95,-21.9631676725155)) ;
#112683 = CARTESIAN_POINT('Origin',(-0.900000000000001,3.8,-20.32)) ;
#112684 = CARTESIAN_POINT('Origin',(-0.900000000000002,2.1568323274845,-21.17)) ;
#112685 = CARTESIAN_POINT('Origin',(-0.900000000000002,1.6,-20.32)) ;
#112686 = CARTESIAN_POINT('Origin',(-0.900000000000002,1.6,-22.2821416870349)) ;
#112687 = CARTESIAN_POINT('Origin',(13.9153543900904,1.4,-22.2821416870349)) ;
#112688 = CARTESIAN_POINT('Origin',(8.49172374697002,1.4,-22.2821416870349)) ;
#112689 = CARTESIAN_POINT('Origin',(-0.900000000000001,1.40000000000001,-22.2821416870349)) ;
#112690 = CARTESIAN_POINT('Origin',(1.15,2.95,-21.9631676725155)) ;
#112691 = CARTESIAN_POINT('Origin',(1.15,3.04189189189189,-21.7855279241354)) ;
#112692 = CARTESIAN_POINT('Origin',(-0.900000000000002,2.1568323274845,-21.17)) ;
#112693 = CARTESIAN_POINT('Origin',(-0.900000000000002,2.1568323274845,-21.17)) ;
#112694 = CARTESIAN_POINT('Origin',(-0.900000000000002,2.1568323274845,-21.17)) ;
#112695 = CARTESIAN_POINT('Origin',(-0.900000000000001,1.40000000000001,-22.2821416870349)) ;
#112696 = CARTESIAN_POINT('Origin',(-0.900000000000002,1.55483870967742,-22.1555519007746)) ;
#112697 = CARTESIAN_POINT('Origin',(1.15,3.8,-20.32)) ;
#112698 = CARTESIAN_POINT('Origin',(1.15,2.33447207586456,-21.0781081081081)) ;
#112699 = CARTESIAN_POINT('Origin',(-1.,2.1568323274845,-21.17)) ;
#112700 = CARTESIAN_POINT('Origin',(1.15,2.1568323274845,-21.17)) ;
#112701 = CARTESIAN_POINT('Origin',(-0.900000000000001,3.8,-21.17)) ;
#112702 = CARTESIAN_POINT('Origin',(-0.900000000000002,1.02736587339765,-21.17)) ;
#112703 = CARTESIAN_POINT('Origin',(-0.900000000000001,3.8,-20.32)) ;
#112704 = CARTESIAN_POINT('Origin',(-0.900000000000002,1.02736587339765,-21.17)) ;
#112705 = CARTESIAN_POINT('Origin',(13.9153543900904,1.4,-18.3578583129651)) ;
#112706 = CARTESIAN_POINT('Origin',(8.49172374697002,1.4,-18.3578583129651)) ;
#112707 = CARTESIAN_POINT('Origin',(-0.900000000000001,1.40000000000001,-18.3578583129651)) ;
#112708 = CARTESIAN_POINT('Origin',(-0.900000000000002,1.6,-20.32)) ;
#112709 = CARTESIAN_POINT('Origin',(-0.900000000000002,1.6,-18.3578583129651)) ;
#112710 = CARTESIAN_POINT('Origin',(-0.900000000000002,2.95,-20.32)) ;
#112711 = CARTESIAN_POINT('Origin',(-0.900000000000002,2.95,-18.6768323274845)) ;
#112712 = CARTESIAN_POINT('Origin',(1.15,2.1568323274845,-21.17)) ;
#112713 = CARTESIAN_POINT('Origin',(1.15,2.1568323274845,-20.97)) ;
#112714 = CARTESIAN_POINT('Origin',(-0.900000000000002,1.02736587339765,-21.17)) ;
#112715 = CARTESIAN_POINT('Origin',(-0.900000000000001,1.40000000000001,-18.3578583129651)) ;
#112716 = CARTESIAN_POINT('Origin',(-0.900000000000002,1.55483870967743,-18.4844480992254)) ;
#112717 = CARTESIAN_POINT('Origin',(-0.900000000000002,2.95,-18.6768323274845)) ;
#112718 = CARTESIAN_POINT('Origin',(-0.900000000000002,2.95,-18.6768323274845)) ;
#112719 = CARTESIAN_POINT('Origin',(-0.900000000000001,2.95,-18.6768323274845)) ;
#112720 = CARTESIAN_POINT('Origin',(1.15,2.21886116991581,-20.97)) ;
#112721 = CARTESIAN_POINT('Ctrl Pts',(1.15,1.02736587339765,-21.07)) ;
#112722 = CARTESIAN_POINT('Ctrl Pts',(1.1608920328805,1.02736587339765,-21.07)) ;
#112723 = CARTESIAN_POINT('Ctrl Pts',(1.17195716626105,1.02622125393927,-21.068143843926)) ;
#112724 = CARTESIAN_POINT('Ctrl Pts',(1.1820844490224,1.02414637334385,-21.0647131887908)) ;
#112725 = CARTESIAN_POINT('Ctrl Pts',(1.19245005921088,1.02202266415684,-21.0612017993431)) ;
#112726 = CARTESIAN_POINT('Ctrl Pts',(1.20216743701154,1.01888103823701,-21.0559601980703)) ;
#112727 = CARTESIAN_POINT('Ctrl Pts',(1.21053792402812,1.01518120925307,-21.0495937168021)) ;
#112728 = CARTESIAN_POINT('Ctrl Pts',(1.219343173684,1.01128921135341,-21.0428965608439)) ;
#112729 = CARTESIAN_POINT('Ctrl Pts',(1.22692289939014,1.00668521903338,-21.0347851615315)) ;
#112730 = CARTESIAN_POINT('Ctrl Pts',(1.23290049538659,1.00186003905466,-21.0259241259624)) ;
#112731 = CARTESIAN_POINT('Ctrl Pts',(1.23922345568944,0.9967560772818,-21.01655113117)) ;
#112732 = CARTESIAN_POINT('Ctrl Pts',(1.24392209779927,0.991279542094837,
-21.0061045599897)) ;
#112733 = CARTESIAN_POINT('Ctrl Pts',(1.24674870216524,0.985895902333124,
-20.9952920665297)) ;
#112734 = CARTESIAN_POINT('Ctrl Pts',(1.24889292215336,0.981811953364218,
-20.9870898699727)) ;
#112735 = CARTESIAN_POINT('Ctrl Pts',(1.25,0.977715885027402,-20.9785491686292)) ;
#112736 = CARTESIAN_POINT('Ctrl Pts',(1.25,0.973783447787483,-20.97)) ;
#112737 = CARTESIAN_POINT('Origin',(-0.900000000000001,3.8,-20.32)) ;
#112738 = CARTESIAN_POINT('Origin',(-0.900000000000002,1.02736587339765,-19.47)) ;
#112739 = CARTESIAN_POINT('Origin',(-0.900000000000001,3.8,-19.47)) ;
#112740 = CARTESIAN_POINT('Origin',(-0.900000000000002,2.1568323274845,-19.47)) ;
#112741 = CARTESIAN_POINT('Origin',(-0.900000000000002,1.02736587339765,-19.47)) ;
#112742 = CARTESIAN_POINT('Origin',(-0.900000000000001,3.8,-20.32)) ;
#112743 = CARTESIAN_POINT('Origin',(-0.900000000000002,2.1568323274845,-19.47)) ;
#112744 = CARTESIAN_POINT('Origin',(-1.,2.95,-18.6768323274845)) ;
#112745 = CARTESIAN_POINT('Origin',(1.15,2.95,-18.6768323274845)) ;
#112746 = CARTESIAN_POINT('Origin',(1.15,3.15,-17.77)) ;
#112747 = CARTESIAN_POINT('Origin',(1.15,3.15,-18.6768323274845)) ;
#112748 = CARTESIAN_POINT('Ctrl Pts',(1.11028558574902,0.930383836951476,
-21.1949942836581)) ;
#112749 = CARTESIAN_POINT('Ctrl Pts',(1.14039000477524,0.892136466138335,
-21.0699697185941)) ;
#112750 = CARTESIAN_POINT('Ctrl Pts',(1.13015013463564,1.02610337426265,-21.0678511248828)) ;
#112751 = CARTESIAN_POINT('Ctrl Pts',(1.17639690652712,0.935225109827649,
-21.2101257399467)) ;
#112752 = CARTESIAN_POINT('Ctrl Pts',(1.15491086542929,0.891146666106391,
-21.0692760504014)) ;
#112753 = CARTESIAN_POINT('Ctrl Pts',(1.16319405445819,1.03078047702076,-21.0751648742452)) ;
#112754 = CARTESIAN_POINT('Ctrl Pts',(1.24701363206612,0.927145283841802,
-21.1855522038251)) ;
#112755 = CARTESIAN_POINT('Ctrl Pts',(1.1775998083145,0.893467326853946,-21.0726373120314)) ;
#112756 = CARTESIAN_POINT('Ctrl Pts',(1.19848758201044,1.02297467453099,-21.063287122555)) ;
#112757 = CARTESIAN_POINT('Ctrl Pts',(1.33816236560056,0.900022463714237,
-21.0898088506149)) ;
#112758 = CARTESIAN_POINT('Ctrl Pts',(1.22862786282608,0.888037626604027,
-21.043153964324)) ;
#112759 = CARTESIAN_POINT('Ctrl Pts',(1.24403288504499,0.996768276947721,
-21.0170266594133)) ;
#112760 = CARTESIAN_POINT('Ctrl Pts',(1.35959492575595,0.881455895025368,
-21.018532341229)) ;
#112761 = CARTESIAN_POINT('Ctrl Pts',(1.25320519750646,0.880428099081736,
-21.0110649378273)) ;
#112762 = CARTESIAN_POINT('Ctrl Pts',(1.25473603279823,0.978811277328825,
-20.982557487151)) ;
#112763 = CARTESIAN_POINT('Ctrl Pts',(1.34615355831623,0.867571605181219,
-20.9527925825335)) ;
#112764 = CARTESIAN_POINT('Ctrl Pts',(1.25176090202828,0.870950130624649,
-20.9694490170578)) ;
#112765 = CARTESIAN_POINT('Ctrl Pts',(1.24801589497573,0.965423101361819,
-20.9508695481641)) ;
#112766 = CARTESIAN_POINT('Origin',(1.35,0.973783447787483,-20.97)) ;
#112767 = CARTESIAN_POINT('Origin',(-0.900000000000002,1.02736587339765,-19.47)) ;
#112768 = CARTESIAN_POINT('',(-0.957735026918965,0.969630846478687,-19.527735026919)) ;
#112769 = CARTESIAN_POINT('Origin',(-0.900000000000002,1.02736587339765,-19.47)) ;
#112770 = CARTESIAN_POINT('Origin',(-0.900000000000002,2.1568323274845,-19.47)) ;
#112771 = CARTESIAN_POINT('Origin',(-0.900000000000002,2.1568323274845,-19.47)) ;
#112772 = CARTESIAN_POINT('Origin',(1.15,2.95,-18.6768323274845)) ;
#112773 = CARTESIAN_POINT('Origin',(1.15,3.04189189189189,-18.8544720758646)) ;
#112774 = CARTESIAN_POINT('Origin',(1.35,3.8,-20.32)) ;
#112775 = CARTESIAN_POINT('Origin',(1.35,0.973783447787484,-19.67)) ;
#112776 = CARTESIAN_POINT('Origin',(-1.,2.1568323274845,-19.47)) ;
#112777 = CARTESIAN_POINT('Origin',(1.15,2.1568323274845,-19.47)) ;
#112778 = CARTESIAN_POINT('Origin',(1.15,3.8,-20.32)) ;
#112779 = CARTESIAN_POINT('Origin',(1.15,2.33447207586456,-19.5618918918919)) ;
#112780 = CARTESIAN_POINT('Ctrl Pts',(1.34754079198595,0.869159571293143,
-19.6797485347856)) ;
#112781 = CARTESIAN_POINT('Ctrl Pts',(1.25183398383322,0.871999770424367,
-19.6659986517603)) ;
#112782 = CARTESIAN_POINT('Ctrl Pts',(1.24871534599026,0.966951450593966,
-19.6855357130736)) ;
#112783 = CARTESIAN_POINT('Ctrl Pts',(1.35788971301869,0.882932151572375,
-19.615777428268)) ;
#112784 = CARTESIAN_POINT('Ctrl Pts',(1.25138796519091,0.881019151005352,
-19.6264872814237)) ;
#112785 = CARTESIAN_POINT('Ctrl Pts',(1.25389076424431,0.980237216252235,
-19.6546886342593)) ;
#112786 = CARTESIAN_POINT('Ctrl Pts',(1.33642796493172,0.900551643074762,
-19.5483167189689)) ;
#112787 = CARTESIAN_POINT('Ctrl Pts',(1.22773025960896,0.888154519889412,
-19.5963023541524)) ;
#112788 = CARTESIAN_POINT('Ctrl Pts',(1.2431720339903,0.997278352451067,-19.6220644582831)) ;
#112789 = CARTESIAN_POINT('Ctrl Pts',(1.24851212064762,0.926675670999774,
-19.4561118541865)) ;
#112790 = CARTESIAN_POINT('Ctrl Pts',(1.17855408504649,0.893378082604311,
-19.5679358454001)) ;
#112791 = CARTESIAN_POINT('Ctrl Pts',(1.1992394771088,1.02252144543593,-19.5775111840606)) ;
#112792 = CARTESIAN_POINT('Ctrl Pts',(1.18212686068544,0.934567888698279,
-19.4318922599007)) ;
#112793 = CARTESIAN_POINT('Ctrl Pts',(1.15690947476174,0.891342319658717,
-19.5705013022393)) ;
#112794 = CARTESIAN_POINT('Ctrl Pts',(1.16605892368793,1.03014681530421,-19.5658041235204)) ;
#112795 = CARTESIAN_POINT('Ctrl Pts',(1.11776263740947,0.930888708579155,
-19.4434235819161)) ;
#112796 = CARTESIAN_POINT('Ctrl Pts',(1.1419771056359,0.892059806627037,-19.5700822996553)) ;
#112797 = CARTESIAN_POINT('Ctrl Pts',(1.13388624958142,1.02659206201251,-19.5713778561013)) ;
#112798 = CARTESIAN_POINT('Ctrl Pts',(1.15,1.02736587339764,-19.57)) ;
#112799 = CARTESIAN_POINT('Ctrl Pts',(1.15623005440502,1.02736587339759,-19.5699999999999)) ;
#112800 = CARTESIAN_POINT('Ctrl Pts',(1.16249579431471,1.02700282517053,-19.570590866069)) ;
#112801 = CARTESIAN_POINT('Ctrl Pts',(1.16857840195431,1.02630083270769,-19.5717409394467)) ;
#112802 = CARTESIAN_POINT('Ctrl Pts',(1.1798885498395,1.02499553092934,-19.5738794137247)) ;
#112803 = CARTESIAN_POINT('Ctrl Pts',(1.19084787809767,1.02245621903271,-19.5780506966152)) ;
#112804 = CARTESIAN_POINT('Ctrl Pts',(1.20043335385463,1.01914369852331,-19.5836491064379)) ;
#112805 = CARTESIAN_POINT('Ctrl Pts',(1.21063893018497,1.01561688548223,-19.5896096868225)) ;
#112806 = CARTESIAN_POINT('Ctrl Pts',(1.21965078109605,1.01112191387731,-19.5973548511019)) ;
#112807 = CARTESIAN_POINT('Ctrl Pts',(1.226898722009,1.00626683908294,-19.6060735848543)) ;
#112808 = CARTESIAN_POINT('Ctrl Pts',(1.23435386869391,1.0012729663137,-19.6150415717366)) ;
#112809 = CARTESIAN_POINT('Ctrl Pts',(1.24017476602864,0.995763540409855,
-19.6252870264069)) ;
#112810 = CARTESIAN_POINT('Ctrl Pts',(1.24405759382605,0.990267693778535,
-19.6360416572305)) ;
#112811 = CARTESIAN_POINT('Ctrl Pts',(1.24795610732226,0.9847496452368,-19.6468397341991)) ;
#112812 = CARTESIAN_POINT('Ctrl Pts',(1.25,0.97910634898267,-19.658427945028)) ;
#112813 = CARTESIAN_POINT('Ctrl Pts',(1.25,0.973783447787483,-19.67)) ;
#112814 = CARTESIAN_POINT('Origin',(1.15,2.1568323274845,-19.47)) ;
#112815 = CARTESIAN_POINT('Origin',(1.15,2.1568323274845,-19.67)) ;
#112816 = CARTESIAN_POINT('Origin',(1.15,2.21886116991581,-19.67)) ;
#112817 = CARTESIAN_POINT('Origin',(1.5,2.3,-20.72)) ;
#112818 = CARTESIAN_POINT('Ctrl Pts',(0.549999999999999,4.04473197180487,
-20.77)) ;
#112819 = CARTESIAN_POINT('Ctrl Pts',(0.549999999999999,4.04340510574359,
-20.7720183916746)) ;
#112820 = CARTESIAN_POINT('Ctrl Pts',(0.549938912488049,4.04197482121862,
-20.7739799093559)) ;
#112821 = CARTESIAN_POINT('Ctrl Pts',(0.549362579613713,4.03414945156058,
-20.783763201697)) ;
#112822 = CARTESIAN_POINT('Ctrl Pts',(0.548040652125092,4.02633974827551,
-20.7905458262272)) ;
#112823 = CARTESIAN_POINT('Ctrl Pts',(0.544205267183616,4.00519499286846,
-20.8046839427888)) ;
#112824 = CARTESIAN_POINT('Ctrl Pts',(0.541221332378481,3.99011995637977,
-20.8112251154482)) ;
#112825 = CARTESIAN_POINT('Ctrl Pts',(0.537814556431532,3.96385893187633,
-20.81793059224)) ;
#112826 = CARTESIAN_POINT('Ctrl Pts',(0.53660254037844,3.95132390702842,-20.82)) ;
#112827 = CARTESIAN_POINT('Ctrl Pts',(0.53660254037844,3.93764017256378,-20.82)) ;
#112828 = CARTESIAN_POINT('Origin',(-0.4,2.3,-20.72)) ;
#112829 = CARTESIAN_POINT('Origin',(-0.4,-3.4,-20.72)) ;
#112830 = CARTESIAN_POINT('Origin',(-0.4,-3.36847777691809,-20.72)) ;
#112831 = CARTESIAN_POINT('Origin',(1.5,2.3,-20.72)) ;
#112832 = CARTESIAN_POINT('Ctrl Pts',(0.536602540378443,2.83090991212703,
-20.82)) ;
#112833 = CARTESIAN_POINT('Ctrl Pts',(0.536602540378443,2.80627146475521,
-20.82)) ;
#112834 = CARTESIAN_POINT('Ctrl Pts',(0.538106903229136,2.77742679387696,
-20.8179527908127)) ;
#112835 = CARTESIAN_POINT('Ctrl Pts',(0.54518697656879,2.71156844363407,-20.8020839809802)) ;
#112836 = CARTESIAN_POINT('Ctrl Pts',(0.55,2.68282906082737,-20.7881020558141)) ;
#112837 = CARTESIAN_POINT('Ctrl Pts',(0.549999999999999,2.65280931275608,
-20.77)) ;
#112838 = CARTESIAN_POINT('Origin',(0.400000000000001,2.29999999999999,-20.72)) ;
#112839 = CARTESIAN_POINT('Origin',(0.0725078566451197,-4.04348900069683,
-20.2474921433549)) ;
#112840 = CARTESIAN_POINT('Origin',(-0.4,-3.36847777691809,-20.72)) ;
#112841 = CARTESIAN_POINT('Origin',(-0.0979344438426628,-3.8,-20.4179344438427)) ;
#112842 = CARTESIAN_POINT('Origin',(1.5,2.3,-19.92)) ;
#112843 = CARTESIAN_POINT('Ctrl Pts',(0.536602540378444,3.93764017256378,
-19.82)) ;
#112844 = CARTESIAN_POINT('Ctrl Pts',(0.536602540378444,3.93925361219679,
-19.82)) ;
#112845 = CARTESIAN_POINT('Ctrl Pts',(0.536619300889441,3.94087098264046,
-19.8200289972578)) ;
#112846 = CARTESIAN_POINT('Ctrl Pts',(0.536997639747773,3.95938954612139,
-19.8206858128959)) ;
#112847 = CARTESIAN_POINT('Ctrl Pts',(0.539142315171152,3.97567120869963,
-19.8243120615618)) ;
#112848 = CARTESIAN_POINT('Ctrl Pts',(0.544035197036784,4.00535605098148,
-19.8353993916663)) ;
#112849 = CARTESIAN_POINT('Ctrl Pts',(0.546989816174504,4.01946236900651,
-19.8435699446353)) ;
#112850 = CARTESIAN_POINT('Ctrl Pts',(0.549463062495712,4.03595536007421,
-19.8585473816974)) ;
#112851 = CARTESIAN_POINT('Ctrl Pts',(0.550000000000877,4.04078397701442,
-19.8639944203465)) ;
#112852 = CARTESIAN_POINT('Ctrl Pts',(0.549999999999999,4.04473197181447,
-19.8700000000146)) ;
#112853 = CARTESIAN_POINT('Origin',(-0.4,2.3,-19.92)) ;
#112854 = CARTESIAN_POINT('Origin',(0.4,2.29999999999999,-20.72)) ;
#112855 = CARTESIAN_POINT('Origin',(0.4,-3.36847777691809,-20.72)) ;
#112856 = CARTESIAN_POINT('Origin',(-0.0979344438426628,-3.8,-20.4179344438427)) ;
#112857 = CARTESIAN_POINT('Origin',(-0.0979344438426628,-3.8,-20.4179344438427)) ;
#112858 = CARTESIAN_POINT('Origin',(-0.0979344438426627,-3.8,-20.4179344438427)) ;
#112859 = CARTESIAN_POINT('Origin',(-0.4,2.3,-19.92)) ;
#112860 = CARTESIAN_POINT('Origin',(-0.4,-3.36847777691809,-19.92)) ;
#112861 = CARTESIAN_POINT('Origin',(0.190875981738719,-3.6672263744342,-20.5108759817387)) ;
#112862 = CARTESIAN_POINT('Origin',(0.400000000000001,-3.36847777691809,-20.72)) ;
#112863 = CARTESIAN_POINT('Origin',(0.0979344438426626,-3.8,-20.4179344438427)) ;
#112864 = CARTESIAN_POINT('Origin',(0.15,-3.8,-20.4179344438427)) ;
#112865 = CARTESIAN_POINT('Origin',(0.0979344438426627,-3.8,-20.4179344438427)) ;
#112866 = CARTESIAN_POINT('Origin',(-0.0979344438426628,-3.8,-19.82)) ;
#112867 = CARTESIAN_POINT('Origin',(-0.0979344438426628,-3.8,-20.2220655561573)) ;
#112868 = CARTESIAN_POINT('Origin',(-0.174966890829628,-3.68995364716148,
-20.1450331091704)) ;
#112869 = CARTESIAN_POINT('Origin',(-0.400000000000001,-3.36847777691809,
-19.92)) ;
#112870 = CARTESIAN_POINT('Origin',(-0.0979344438426627,-3.8,-20.2220655561573)) ;
#112871 = CARTESIAN_POINT('Origin',(0.0979344438426627,-3.8,-20.4179344438427)) ;
#112872 = CARTESIAN_POINT('Origin',(0.0979344438426628,-3.8,-20.4179344438427)) ;
#112873 = CARTESIAN_POINT('Origin',(-0.0979344438426628,-3.8,-20.2220655561573)) ;
#112874 = CARTESIAN_POINT('Origin',(-0.0979344438426628,-3.8,-20.2220655561573)) ;
#112875 = CARTESIAN_POINT('Origin',(0.0979344438426627,-3.8,-19.82)) ;
#112876 = CARTESIAN_POINT('Origin',(0.0979344438426627,-3.8,-20.2220655561573)) ;
#112877 = CARTESIAN_POINT('Origin',(-1.11032778078669,-3.8,-20.2220655561573)) ;
#112878 = CARTESIAN_POINT('Origin',(0.0979344438426626,-3.8,-20.2220655561573)) ;
#112879 = CARTESIAN_POINT('Origin',(0.0979344438426627,-3.8,-20.2220655561573)) ;
#112880 = CARTESIAN_POINT('Origin',(0.0979344438426627,-3.8,-20.2220655561573)) ;
#112881 = CARTESIAN_POINT('Origin',(0.438350729213467,-3.31369102089885,-19.8816492707865)) ;
#112882 = CARTESIAN_POINT('Origin',(0.399999999999999,-3.36847777691809,-19.92)) ;
#112883 = CARTESIAN_POINT('Origin',(0.4,2.3,-19.92)) ;
#112884 = CARTESIAN_POINT('Origin',(0.4,-3.36847777691809,-19.92)) ;
#112885 = CARTESIAN_POINT('Origin',(0.4,2.29999999999999,-19.92)) ;
#112886 = CARTESIAN_POINT('Origin',(1.5,2.3,-19.92)) ;
#112887 = CARTESIAN_POINT('Ctrl Pts',(0.55,2.65280931275593,-19.8700000000001)) ;
#112888 = CARTESIAN_POINT('Ctrl Pts',(0.550000000000013,2.67648433237897,
-19.8557238466627)) ;
#112889 = CARTESIAN_POINT('Ctrl Pts',(0.546908864252789,2.69988533923261,
-19.8435257008476)) ;
#112890 = CARTESIAN_POINT('Ctrl Pts',(0.539540151921447,2.76165254733706,
-19.8240915981901)) ;
#112891 = CARTESIAN_POINT('Ctrl Pts',(0.536602540378444,2.79600904778111,
-19.82)) ;
#112892 = CARTESIAN_POINT('Ctrl Pts',(0.536602540378444,2.83090991212703,
-19.82)) ;
#112893 = CARTESIAN_POINT('Origin',(8.,3.4,-20.72)) ;
#112894 = CARTESIAN_POINT('Origin',(7.96847777691809,3.4,-20.72)) ;
#112895 = CARTESIAN_POINT('Origin',(1.5,4.2,-20.72)) ;
#112896 = CARTESIAN_POINT('Origin',(7.96847777691809,4.2,-20.72)) ;
#112897 = CARTESIAN_POINT('Origin',(8.64348900069683,3.87250785664512,-20.2474921433549)) ;
#112898 = CARTESIAN_POINT('Origin',(7.96847777691809,3.4,-20.72)) ;
#112899 = CARTESIAN_POINT('Origin',(8.4,3.70206555615734,-20.4179344438427)) ;
#112900 = CARTESIAN_POINT('Origin',(8.26722637443421,3.99087598173872,-20.5108759817387)) ;
#112901 = CARTESIAN_POINT('Origin',(7.96847777691809,4.2,-20.72)) ;
#112902 = CARTESIAN_POINT('Origin',(8.4,3.89793444384266,-20.4179344438427)) ;
#112903 = CARTESIAN_POINT('Origin',(8.4,3.95,-20.4179344438427)) ;
#112904 = CARTESIAN_POINT('Origin',(8.4,3.70206555615734,-20.4179344438427)) ;
#112905 = CARTESIAN_POINT('Origin',(8.4,3.89793444384266,-20.4179344438427)) ;
#112906 = CARTESIAN_POINT('Origin',(8.4,3.70206555615734,-20.4179344438427)) ;
#112907 = CARTESIAN_POINT('Origin',(8.4,3.70206555615734,-20.4179344438427)) ;
#112908 = CARTESIAN_POINT('Origin',(1.5,3.4,-19.92)) ;
#112909 = CARTESIAN_POINT('Origin',(7.96847777691809,3.4,-19.92)) ;
#112910 = CARTESIAN_POINT('Origin',(1.5,4.2,-19.92)) ;
#112911 = CARTESIAN_POINT('Origin',(7.96847777691809,4.2,-19.92)) ;
#112912 = CARTESIAN_POINT('Origin',(8.4,3.89793444384266,-20.4179344438427)) ;
#112913 = CARTESIAN_POINT('Origin',(8.4,3.89793444384266,-20.4179344438427)) ;
#112914 = CARTESIAN_POINT('Origin',(8.4,3.70206555615734,-19.82)) ;
#112915 = CARTESIAN_POINT('Origin',(8.4,3.70206555615734,-20.2220655561573)) ;
#112916 = CARTESIAN_POINT('Origin',(8.28995364716148,3.62503310917037,-20.1450331091704)) ;
#112917 = CARTESIAN_POINT('Origin',(7.96847777691809,3.4,-19.92)) ;
#112918 = CARTESIAN_POINT('Origin',(8.4,3.70206555615734,-20.2220655561573)) ;
#112919 = CARTESIAN_POINT('Origin',(7.91369102089885,4.23835072921347,-19.8816492707865)) ;
#112920 = CARTESIAN_POINT('Origin',(7.96847777691809,4.2,-19.92)) ;
#112921 = CARTESIAN_POINT('Origin',(8.4,3.89793444384266,-20.2220655561573)) ;
#112922 = CARTESIAN_POINT('Origin',(8.4,3.89793444384266,-19.82)) ;
#112923 = CARTESIAN_POINT('Origin',(8.4,3.89793444384266,-20.2220655561573)) ;
#112924 = CARTESIAN_POINT('Origin',(8.4,3.70206555615734,-20.2220655561573)) ;
#112925 = CARTESIAN_POINT('Origin',(8.4,3.70206555615734,-20.2220655561573)) ;
#112926 = CARTESIAN_POINT('Origin',(8.4,3.89793444384266,-20.2220655561573)) ;
#112927 = CARTESIAN_POINT('Origin',(8.4,3.89793444384266,-20.2220655561573)) ;
#112928 = CARTESIAN_POINT('Origin',(8.4,2.68967221921331,-20.2220655561573)) ;
#112929 = CARTESIAN_POINT('Origin',(9.9,6.8847127088383,-22.86)) ;
#112930 = CARTESIAN_POINT('Origin',(9.9,6.8847127088383,-21.2797127088383)) ;
#112931 = CARTESIAN_POINT('Origin',(8.77035388141948,6.69643835574155,-21.0914383557416)) ;
#112932 = CARTESIAN_POINT('Ctrl Pts',(8.58356010126946,6.66256607592812,-20.958926683545)) ;
#112933 = CARTESIAN_POINT('Ctrl Pts',(8.58266714977878,6.65676189123867,-20.9587778582965)) ;
#112934 = CARTESIAN_POINT('Ctrl Pts',(8.58182526931893,6.6507714222091,-20.9591141714741)) ;
#112935 = CARTESIAN_POINT('Ctrl Pts',(8.58032528754329,6.63886560514773,-20.9609127350998)) ;
#112936 = CARTESIAN_POINT('Ctrl Pts',(8.57966270906097,6.63295370212089,-20.9623448243331)) ;
#112937 = CARTESIAN_POINT('Ctrl Pts',(8.57906641006211,6.62681909302424,-20.9644771744941)) ;
#112938 = CARTESIAN_POINT('Ctrl Pts',(8.57903375157323,6.62647998752457,-20.9645971697287)) ;
#112939 = CARTESIAN_POINT('Ctrl Pts',(8.57846569624192,6.6205258217488,-20.966741731681)) ;
#112940 = CARTESIAN_POINT('Ctrl Pts',(8.57802501793965,6.61503168015257,-20.9693142858557)) ;
#112941 = CARTESIAN_POINT('Ctrl Pts',(8.57766199200569,6.60925146760312,-20.9727462133234)) ;
#112942 = CARTESIAN_POINT('Ctrl Pts',(8.57762821177172,6.60869602779103,-20.9730838351647)) ;
#112943 = CARTESIAN_POINT('Ctrl Pts',(8.57728522755447,6.60286036001468,-20.9767147989572)) ;
#112944 = CARTESIAN_POINT('Ctrl Pts',(8.57709550103272,6.59788070192354,-20.9805482210562)) ;
#112945 = CARTESIAN_POINT('Ctrl Pts',(8.57703980289278,6.59299711069415,-20.9851723373547)) ;
#112946 = CARTESIAN_POINT('Ctrl Pts',(8.57703670271021,6.5926595243005,-20.985496892542)) ;
#112947 = CARTESIAN_POINT('Ctrl Pts',(8.57701334129169,6.58927432516128,-20.9888013815953)) ;
#112948 = CARTESIAN_POINT('Ctrl Pts',(8.57705699426434,6.5864297120155,-20.9919917444088)) ;
#112949 = CARTESIAN_POINT('Ctrl Pts',(8.57735031225521,6.57961409340222,-21.0007954417554)) ;
#112950 = CARTESIAN_POINT('Ctrl Pts',(8.57770856513437,6.57604383182914,-21.0066682455399)) ;
#112951 = CARTESIAN_POINT('Ctrl Pts',(8.57865704971091,6.57055741297635,-21.0183322193388)) ;
#112952 = CARTESIAN_POINT('Ctrl Pts',(8.57922107378969,6.56851476050446,-21.0240736349077)) ;
#112953 = CARTESIAN_POINT('Ctrl Pts',(8.57993695782543,6.56687610193753,-21.0304559348163)) ;
#112954 = CARTESIAN_POINT('Ctrl Pts',(8.58000419042984,6.56673001682056,-21.0310478351839)) ;
#112955 = CARTESIAN_POINT('Ctrl Pts',(8.58074399738015,6.56520526212529,-21.037481251735)) ;
#112956 = CARTESIAN_POINT('Ctrl Pts',(8.58149993293339,6.56438134785785,-21.0433541800929)) ;
#112957 = CARTESIAN_POINT('Ctrl Pts',(8.58236768178469,6.56403389662205,-21.0494987578227)) ;
#112958 = CARTESIAN_POINT('Ctrl Pts',(8.58242358604544,6.56401394107887,-21.0498921736313)) ;
#112959 = CARTESIAN_POINT('Ctrl Pts',(8.58283067264383,6.56388592662946,-21.0527394234264)) ;
#112960 = CARTESIAN_POINT('Ctrl Pts',(8.58319156240649,6.56386525642005,-21.0551699505828)) ;
#112961 = CARTESIAN_POINT('Ctrl Pts',(8.58356019967707,6.56392669994633,-21.0575662650647)) ;
#112962 = CARTESIAN_POINT('Origin',(9.9,6.8847127088383,-21.2797127088383)) ;
#112963 = CARTESIAN_POINT('Origin',(9.9,6.8847127088383,-21.2797127088383)) ;
#112964 = CARTESIAN_POINT('Origin',(9.9,6.8847127088383,-21.2797127088383)) ;
#112965 = CARTESIAN_POINT('Origin',(9.9,7.72792407799439,-22.86)) ;
#112966 = CARTESIAN_POINT('Origin',(9.9,7.72792407799439,-21.2797127088383)) ;
#112967 = CARTESIAN_POINT('Origin',(9.90000000000001,4.35421736843756,-21.2797127088383)) ;
#112968 = CARTESIAN_POINT('Origin',(9.9,7.72792407799439,-21.2797127088383)) ;
#112969 = CARTESIAN_POINT('Origin',(9.9,7.72792407799439,-21.2797127088383)) ;
#112970 = CARTESIAN_POINT('Origin',(9.9,7.72792407799439,-21.2797127088383)) ;
#112971 = CARTESIAN_POINT('Origin',(10.9628342502842,7.37364599456632,-21.4568517505523)) ;
#112972 = CARTESIAN_POINT('Ctrl Pts',(8.56837732530586,8.2772075582313,-21.0525052537977)) ;
#112973 = CARTESIAN_POINT('Ctrl Pts',(8.56753565030797,8.2774881236726,-21.0466129921974)) ;
#112974 = CARTESIAN_POINT('Ctrl Pts',(8.56682045541689,8.2772118066791,-21.0405412944396)) ;
#112975 = CARTESIAN_POINT('Ctrl Pts',(8.56575413148015,8.27538624160209,-21.0287284721177)) ;
#112976 = CARTESIAN_POINT('Ctrl Pts',(8.56538426077852,8.27391165896476,-21.0229905624278)) ;
#112977 = CARTESIAN_POINT('Ctrl Pts',(8.56517777855932,8.27166501362512,-21.0170147754472)) ;
#112978 = CARTESIAN_POINT('Ctrl Pts',(8.56516523451682,8.27151619608598,-21.0166276382838)) ;
#112979 = CARTESIAN_POINT('Ctrl Pts',(8.56497390811214,8.26902793125451,-21.0102953359912)) ;
#112980 = CARTESIAN_POINT('Ctrl Pts',(8.56499903025534,8.2659763012945,-21.0045357784659)) ;
#112981 = CARTESIAN_POINT('Ctrl Pts',(8.56538588200257,8.26046191593055,-20.9965906723681)) ;
#112982 = CARTESIAN_POINT('Ctrl Pts',(8.56556309332507,8.25853771611458,-20.9941212364558)) ;
#112983 = CARTESIAN_POINT('Ctrl Pts',(8.56628156514548,8.25214511987158,-20.9868017566891)) ;
#112984 = CARTESIAN_POINT('Ctrl Pts',(8.56700742874793,8.2472021625627,-20.982305445231)) ;
#112985 = CARTESIAN_POINT('Ctrl Pts',(8.56880713798126,8.23661566152161,-20.97462449488)) ;
#112986 = CARTESIAN_POINT('Ctrl Pts',(8.5698603939132,8.23102391526957,-20.9713848807255)) ;
#112987 = CARTESIAN_POINT('Ctrl Pts',(8.57116255171755,8.22459552194118,-20.9684467745269)) ;
#112988 = CARTESIAN_POINT('Ctrl Pts',(8.57127495810218,8.22404408343782,-20.9682006607901)) ;
#112989 = CARTESIAN_POINT('Ctrl Pts',(8.57260511146312,8.21755901312581,-20.9653749153055)) ;
#112990 = CARTESIAN_POINT('Ctrl Pts',(8.5739562967284,8.21135759730909,-20.9633463864276)) ;
#112991 = CARTESIAN_POINT('Ctrl Pts',(8.57552311082417,8.20452945286284,-20.9617495443173)) ;
#112992 = CARTESIAN_POINT('Ctrl Pts',(8.57564505123012,8.20400026307089,-20.961629826956)) ;
#112993 = CARTESIAN_POINT('Ctrl Pts',(8.57731301559524,8.1967919362264,-20.960053462537)) ;
#112994 = CARTESIAN_POINT('Ctrl Pts',(8.57896065127869,8.19002168485366,-20.959210969344)) ;
#112995 = CARTESIAN_POINT('Ctrl Pts',(8.58161366784366,8.17959769015482,-20.9587553172771)) ;
#112996 = CARTESIAN_POINT('Ctrl Pts',(8.58258362864269,8.17587911616515,-20.9587639381071)) ;
#112997 = CARTESIAN_POINT('Ctrl Pts',(8.58356010126947,8.17221734381475,-20.9589266835449)) ;
#112998 = CARTESIAN_POINT('Origin',(7.96824861826159,6.56275414521524,-19.6822458547848)) ;
#112999 = CARTESIAN_POINT('Origin',(8.5968837020256,6.66156024040156,-19.5912434752671)) ;
#113000 = CARTESIAN_POINT('Origin',(9.9,6.8847127088383,-19.3602872911617)) ;
#113001 = CARTESIAN_POINT('Origin',(9.9,6.8847127088383,-22.86)) ;
#113002 = CARTESIAN_POINT('Origin',(9.9,6.8847127088383,-19.3602872911617)) ;
#113003 = CARTESIAN_POINT('Origin',(9.9,6.8847127088383,-19.3602872911617)) ;
#113004 = CARTESIAN_POINT('Origin',(9.9,6.8847127088383,-19.3602872911617)) ;
#113005 = CARTESIAN_POINT('Origin',(9.9,6.8,-19.3602872911617)) ;
#113006 = CARTESIAN_POINT('Origin',(9.9,7.72792407799439,-19.3602872911617)) ;
#113007 = CARTESIAN_POINT('Origin',(9.9,7.72792407799439,-22.86)) ;
#113008 = CARTESIAN_POINT('Origin',(9.9,7.72792407799439,-19.3602872911617)) ;
#113009 = CARTESIAN_POINT('Origin',(9.9,7.72792407799439,-19.3602872911617)) ;
#113010 = CARTESIAN_POINT('Origin',(9.9,7.72792407799439,-19.3602872911617)) ;
#113011 = CARTESIAN_POINT('Origin',(9.60917571369883,7.82486550676144,-19.4087580055452)) ;
#113012 = CARTESIAN_POINT('Origin',(8.59099001845867,8.18966234087289,-19.5851609739002)) ;
#113013 = CARTESIAN_POINT('Origin',(0.45,4.4,-20.32)) ;
#113014 = CARTESIAN_POINT('Origin',(0.45,4.4,-20.77)) ;
#113015 = CARTESIAN_POINT('Origin',(0.45,4.4,-19.87)) ;
#113016 = CARTESIAN_POINT('Origin',(-1.9,7.55,-22.86)) ;
#113017 = CARTESIAN_POINT('Origin',(6.9,7.75,-22.86)) ;
#113018 = CARTESIAN_POINT('Origin',(7.1,8.2,-22.86)) ;
#113019 = CARTESIAN_POINT('Origin',(9.9,0.1,-22.86)) ;
#113020 = CARTESIAN_POINT('Origin',(9.9,1.16528729116168,-22.86)) ;
#113021 = CARTESIAN_POINT('Origin',(9.9,1.16528729116168,-22.3641618801782)) ;
#113022 = CARTESIAN_POINT('Origin',(9.9,3.8,-20.32)) ;
#113023 = CARTESIAN_POINT('Origin',(9.9,1.16528729116168,-18.2758381198218)) ;
#113024 = CARTESIAN_POINT('Origin',(9.9,1.16528729116168,-22.3641618801782)) ;
#113025 = CARTESIAN_POINT('Origin',(9.9,1.16528729116168,-22.86)) ;
#113026 = CARTESIAN_POINT('Origin',(9.9,1.16528729116168,-18.2758381198218)) ;
#113027 = CARTESIAN_POINT('Ctrl Pts',(0.55,0.3,-20.77)) ;
#113028 = CARTESIAN_POINT('Ctrl Pts',(0.55,0.3,-20.87)) ;
#113029 = CARTESIAN_POINT('Ctrl Pts',(0.45,0.3,-20.87)) ;
#113030 = CARTESIAN_POINT('Ctrl Pts',(0.55,0.28690770353672,-20.7700000008182)) ;
#113031 = CARTESIAN_POINT('Ctrl Pts',(0.549992696056738,0.300543498484345,
-20.8699926960962)) ;
#113032 = CARTESIAN_POINT('Ctrl Pts',(0.450000000818259,0.286907703536713,
-20.87)) ;
#113033 = CARTESIAN_POINT('Ctrl Pts',(0.552602750539093,0.273825167611082,
-20.7752055010782)) ;
#113034 = CARTESIAN_POINT('Ctrl Pts',(0.546703256435903,0.299059401315785,
-20.8667032564359)) ;
#113035 = CARTESIAN_POINT('Ctrl Pts',(0.455205501078185,0.273825167611091,
-20.8726027505391)) ;
#113036 = CARTESIAN_POINT('Ctrl Pts',(0.56262134295865,0.249638145915901,
-20.7952426859173)) ;
#113037 = CARTESIAN_POINT('Ctrl Pts',(0.544986924117065,0.28207277643954,
-20.8649869241171)) ;
#113038 = CARTESIAN_POINT('Ctrl Pts',(0.4752426859173,0.249638145915891,-20.8826213429587)) ;
#113039 = CARTESIAN_POINT('Ctrl Pts',(0.570033341471288,0.238545302291403,
-20.8100666829426)) ;
#113040 = CARTESIAN_POINT('Ctrl Pts',(0.54711619685839,0.267914459835251,
-20.8671161968584)) ;
#113041 = CARTESIAN_POINT('Ctrl Pts',(0.490066682942577,0.238545302291388,
-20.8900333414713)) ;
#113042 = CARTESIAN_POINT('Ctrl Pts',(0.597801282701459,0.210777361061231,
-20.8656025654029)) ;
#113043 = CARTESIAN_POINT('Ctrl Pts',(0.570853448890191,0.226374713859272,
-20.8908534488901)) ;
#113044 = CARTESIAN_POINT('Ctrl Pts',(0.545602565402917,0.21077736106126,
-20.9178012827014)) ;
#113045 = CARTESIAN_POINT('Ctrl Pts',(0.623746567173686,0.2,-20.9174931343473)) ;
#113046 = CARTESIAN_POINT('Ctrl Pts',(0.610458667315294,0.2,-20.930458667316)) ;
#113047 = CARTESIAN_POINT('Ctrl Pts',(0.597493134347343,0.2,-20.9437465671735)) ;
#113048 = CARTESIAN_POINT('Ctrl Pts',(0.65,0.2,-20.97)) ;
#113049 = CARTESIAN_POINT('Ctrl Pts',(0.65,0.2,-20.97)) ;
#113050 = CARTESIAN_POINT('Ctrl Pts',(0.65,0.2,-20.97)) ;
#113051 = CARTESIAN_POINT('Origin',(0.45,0.3,-20.77)) ;
#113052 = CARTESIAN_POINT('Origin',(0.45,1.24941393210234E-16,-20.77)) ;
#113053 = CARTESIAN_POINT('Origin',(0.45,4.4,-20.77)) ;
#113054 = CARTESIAN_POINT('Origin',(0.45,4.4,-20.77)) ;
#113055 = CARTESIAN_POINT('Origin',(0.45,4.4,-20.77)) ;
#113056 = CARTESIAN_POINT('Origin',(0.549999999999999,4.4,-20.77)) ;
#113057 = CARTESIAN_POINT('Origin',(-1.7,4.4,-20.77)) ;
#113058 = CARTESIAN_POINT('Ctrl Pts',(-1.8,4.6,-20.97)) ;
#113059 = CARTESIAN_POINT('Ctrl Pts',(-1.8,4.6,-20.97)) ;
#113060 = CARTESIAN_POINT('Ctrl Pts',(-1.8,4.6,-20.97)) ;
#113061 = CARTESIAN_POINT('Ctrl Pts',(-1.8,4.57374656717372,-20.9174931343473)) ;
#113062 = CARTESIAN_POINT('Ctrl Pts',(-1.8,4.56045866731641,-20.930458667317)) ;
#113063 = CARTESIAN_POINT('Ctrl Pts',(-1.8,4.54749313434728,-20.9437465671737)) ;
#113064 = CARTESIAN_POINT('Ctrl Pts',(-1.78922263893876,4.54780128270145,
-20.8656025654029)) ;
#113065 = CARTESIAN_POINT('Ctrl Pts',(-1.77362528614074,4.52085344889015,
-20.8908534488901)) ;
#113066 = CARTESIAN_POINT('Ctrl Pts',(-1.78922263893874,4.49560256540291,
-20.9178012827014)) ;
#113067 = CARTESIAN_POINT('Ctrl Pts',(-1.7614546977086,4.5200333414713,-20.8100666829426)) ;
#113068 = CARTESIAN_POINT('Ctrl Pts',(-1.73208554016474,4.49711619685842,
-20.8671161968584)) ;
#113069 = CARTESIAN_POINT('Ctrl Pts',(-1.76145469770861,4.44006668294258,
-20.8900333414713)) ;
#113070 = CARTESIAN_POINT('Ctrl Pts',(-1.7503618540841,4.51262134295865,-20.7952426859173)) ;
#113071 = CARTESIAN_POINT('Ctrl Pts',(-1.71792722356046,4.49498692411707,
-20.8649869241171)) ;
#113072 = CARTESIAN_POINT('Ctrl Pts',(-1.75036185408411,4.42524268591729,
-20.8826213429587)) ;
#113073 = CARTESIAN_POINT('Ctrl Pts',(-1.72617483238892,4.50260275053909,
-20.7752055010782)) ;
#113074 = CARTESIAN_POINT('Ctrl Pts',(-1.70094059868422,4.4967032564359,-20.8667032564359)) ;
#113075 = CARTESIAN_POINT('Ctrl Pts',(-1.72617483238891,4.4052055010782,-20.8726027505391)) ;
#113076 = CARTESIAN_POINT('Ctrl Pts',(-1.71309229646328,4.5,-20.7700000008182)) ;
#113077 = CARTESIAN_POINT('Ctrl Pts',(-1.69945650152272,4.49999269603968,
-20.8699926960963)) ;
#113078 = CARTESIAN_POINT('Ctrl Pts',(-1.71309229646328,4.40000000081823,
-20.87)) ;
#113079 = CARTESIAN_POINT('Ctrl Pts',(-1.7,4.5,-20.77)) ;
#113080 = CARTESIAN_POINT('Ctrl Pts',(-1.7,4.5,-20.87)) ;
#113081 = CARTESIAN_POINT('Ctrl Pts',(-1.7,4.4,-20.87)) ;
#113082 = CARTESIAN_POINT('Ctrl Pts',(-1.8,4.6,-19.67)) ;
#113083 = CARTESIAN_POINT('Ctrl Pts',(-1.8,4.6,-19.67)) ;
#113084 = CARTESIAN_POINT('Ctrl Pts',(-1.8,4.6,-19.67)) ;
#113085 = CARTESIAN_POINT('Ctrl Pts',(-1.8,4.54749313434728,-19.6962534328263)) ;
#113086 = CARTESIAN_POINT('Ctrl Pts',(-1.8,4.5604586673143,-19.7095413326856)) ;
#113087 = CARTESIAN_POINT('Ctrl Pts',(-1.8,4.57374656717372,-19.7225068656528)) ;
#113088 = CARTESIAN_POINT('Ctrl Pts',(-1.78922263893874,4.49560256540291,
-19.7221987172986)) ;
#113089 = CARTESIAN_POINT('Ctrl Pts',(-1.77362528614074,4.52085344889015,
-19.7491465511099)) ;
#113090 = CARTESIAN_POINT('Ctrl Pts',(-1.78922263893876,4.54780128270145,
-19.7743974345971)) ;
#113091 = CARTESIAN_POINT('Ctrl Pts',(-1.76145469770861,4.44006668294258,
-19.7499666585287)) ;
#113092 = CARTESIAN_POINT('Ctrl Pts',(-1.73208554016474,4.49711619685842,
-19.7728838031416)) ;
#113093 = CARTESIAN_POINT('Ctrl Pts',(-1.7614546977086,4.5200333414713,-19.8299333170574)) ;
#113094 = CARTESIAN_POINT('Ctrl Pts',(-1.75036185408411,4.42524268591729,
-19.7573786570413)) ;
#113095 = CARTESIAN_POINT('Ctrl Pts',(-1.71792722356045,4.49498692411707,
-19.7750130758829)) ;
#113096 = CARTESIAN_POINT('Ctrl Pts',(-1.7503618540841,4.51262134295865,-19.8447573140827)) ;
#113097 = CARTESIAN_POINT('Ctrl Pts',(-1.72617483238891,4.4052055010782,-19.7673972494609)) ;
#113098 = CARTESIAN_POINT('Ctrl Pts',(-1.70094059868422,4.4967032564359,-19.7732967435641)) ;
#113099 = CARTESIAN_POINT('Ctrl Pts',(-1.72617483238892,4.50260275053909,
-19.8647944989218)) ;
#113100 = CARTESIAN_POINT('Ctrl Pts',(-1.71309229646329,4.40000000081823,
-19.77)) ;
#113101 = CARTESIAN_POINT('Ctrl Pts',(-1.69945650152272,4.49999269603968,
-19.7700073039037)) ;
#113102 = CARTESIAN_POINT('Ctrl Pts',(-1.71309229646328,4.5,-19.8699999991818)) ;
#113103 = CARTESIAN_POINT('Ctrl Pts',(-1.7,4.4,-19.77)) ;
#113104 = CARTESIAN_POINT('Ctrl Pts',(-1.7,4.5,-19.77)) ;
#113105 = CARTESIAN_POINT('Ctrl Pts',(-1.7,4.5,-19.87)) ;
#113106 = CARTESIAN_POINT('Origin',(-1.7,4.4,-19.87)) ;
#113107 = CARTESIAN_POINT('Origin',(0.549999999999999,4.4,-19.87)) ;
#113108 = CARTESIAN_POINT('Origin',(0.45,4.4,-19.87)) ;
#113109 = CARTESIAN_POINT('Origin',(0.45,4.4,-19.87)) ;
#113110 = CARTESIAN_POINT('Origin',(0.45,4.4,-19.87)) ;
#113111 = CARTESIAN_POINT('Origin',(0.45,4.9047241136249E-17,-19.87)) ;
#113112 = CARTESIAN_POINT('Origin',(0.45,0.3,-19.87)) ;
#113113 = CARTESIAN_POINT('Ctrl Pts',(0.45,0.3,-19.77)) ;
#113114 = CARTESIAN_POINT('Ctrl Pts',(0.55,0.3,-19.77)) ;
#113115 = CARTESIAN_POINT('Ctrl Pts',(0.55,0.3,-19.87)) ;
#113116 = CARTESIAN_POINT('Ctrl Pts',(0.450000000818259,0.286907703536713,
-19.77)) ;
#113117 = CARTESIAN_POINT('Ctrl Pts',(0.549992696056738,0.300543498484345,
-19.7700073039038)) ;
#113118 = CARTESIAN_POINT('Ctrl Pts',(0.55,0.28690770353672,-19.8699999991818)) ;
#113119 = CARTESIAN_POINT('Ctrl Pts',(0.455205501078185,0.273825167611091,
-19.7673972494609)) ;
#113120 = CARTESIAN_POINT('Ctrl Pts',(0.546703256435901,0.299059401315784,
-19.7732967435641)) ;
#113121 = CARTESIAN_POINT('Ctrl Pts',(0.552602750539093,0.273825167611082,
-19.8647944989218)) ;
#113122 = CARTESIAN_POINT('Ctrl Pts',(0.4752426859173,0.249638145915891,-19.7573786570413)) ;
#113123 = CARTESIAN_POINT('Ctrl Pts',(0.544986924117067,0.282072776439541,
-19.7750130758829)) ;
#113124 = CARTESIAN_POINT('Ctrl Pts',(0.56262134295865,0.249638145915901,
-19.8447573140827)) ;
#113125 = CARTESIAN_POINT('Ctrl Pts',(0.490066682942577,0.238545302291388,
-19.7499666585287)) ;
#113126 = CARTESIAN_POINT('Ctrl Pts',(0.54711619685839,0.267914459835252,
-19.7728838031416)) ;
#113127 = CARTESIAN_POINT('Ctrl Pts',(0.570033341471288,0.238545302291403,
-19.8299333170574)) ;
#113128 = CARTESIAN_POINT('Ctrl Pts',(0.545602565402917,0.21077736106126,
-19.7221987172986)) ;
#113129 = CARTESIAN_POINT('Ctrl Pts',(0.570853448890191,0.22637471385927,
-19.7491465511099)) ;
#113130 = CARTESIAN_POINT('Ctrl Pts',(0.597801282701459,0.210777361061231,
-19.7743974345971)) ;
#113131 = CARTESIAN_POINT('Ctrl Pts',(0.597493134347346,0.2,-19.6962534328265)) ;
#113132 = CARTESIAN_POINT('Ctrl Pts',(0.610458667316253,0.2,-19.7095413326839)) ;
#113133 = CARTESIAN_POINT('Ctrl Pts',(0.623746567173686,0.2,-19.7225068656527)) ;
#113134 = CARTESIAN_POINT('Ctrl Pts',(0.65,0.2,-19.67)) ;
#113135 = CARTESIAN_POINT('Ctrl Pts',(0.65,0.2,-19.67)) ;
#113136 = CARTESIAN_POINT('Ctrl Pts',(0.65,0.2,-19.67)) ;
#113137 = CARTESIAN_POINT('Ctrl Pts',(8.5,8.17221734381475,-20.8602872911617)) ;
#113138 = CARTESIAN_POINT('Ctrl Pts',(8.5,8.17221734381475,-20.945)) ;
#113139 = CARTESIAN_POINT('Ctrl Pts',(8.58356010126947,8.17221734381475,-20.9589266835449)) ;
#113140 = CARTESIAN_POINT('Ctrl Pts',(8.5,8.23335379241385,-20.8602872927391)) ;
#113141 = CARTESIAN_POINT('Ctrl Pts',(8.5,8.2084742596066,-20.9374575674223)) ;
#113142 = CARTESIAN_POINT('Ctrl Pts',(8.57460439031233,8.20580126077889,-20.9574340650521)) ;
#113143 = CARTESIAN_POINT('Ctrl Pts',(8.5,8.29192178062155,-20.8871741150785)) ;
#113144 = CARTESIAN_POINT('Ctrl Pts',(8.49999999999995,8.25010493984403,-20.9492546083116)) ;
#113145 = CARTESIAN_POINT('Ctrl Pts',(8.56800970738924,8.23725302684489,-20.9697783631899)) ;
#113146 = CARTESIAN_POINT('Ctrl Pts',(8.5,8.36583651094027,-20.9765506232914)) ;
#113147 = CARTESIAN_POINT('Ctrl Pts',(8.50000000000005,8.29925403146166,-21.0033614370367)) ;
#113148 = CARTESIAN_POINT('Ctrl Pts',(8.56373266208983,8.27563607377072,-21.0137537764131)) ;
#113149 = CARTESIAN_POINT('Ctrl Pts',(8.5,8.38029241321759,-21.0379552056996)) ;
#113150 = CARTESIAN_POINT('Ctrl Pts',(8.50000000000015,8.30669116589111,-21.044808849941)) ;
#113151 = CARTESIAN_POINT('Ctrl Pts',(8.56610123859376,8.28208399509955,-21.044808702407)) ;
#113152 = CARTESIAN_POINT('Ctrl Pts',(8.5,8.36719795478508,-21.0960547234799)) ;
#113153 = CARTESIAN_POINT('Ctrl Pts',(8.5,8.29381262650623,-21.0795151496718)) ;
#113154 = CARTESIAN_POINT('Ctrl Pts',(8.57227762885807,8.27346847343705,-21.0749299876354)) ;
#113155 = CARTESIAN_POINT('Ctrl Pts',(8.5485213309235,8.28383177029354,-21.0759865327337)) ;
#113156 = CARTESIAN_POINT('Ctrl Pts',(8.54913757890789,8.28625057716299,-21.062921659184)) ;
#113157 = CARTESIAN_POINT('Ctrl Pts',(8.549146361399,8.28675781111762,-21.0492647894026)) ;
#113158 = CARTESIAN_POINT('Ctrl Pts',(8.54883414737369,8.28489376483071,-21.036098869425)) ;
#113159 = CARTESIAN_POINT('Ctrl Pts',(8.54852072231757,8.28302248819127,-21.0228818808428)) ;
#113160 = CARTESIAN_POINT('Ctrl Pts',(8.54791723678494,8.27865742078997,-21.0098312958117)) ;
#113161 = CARTESIAN_POINT('Ctrl Pts',(8.54677696932927,8.27237937104781,-20.9981020767297)) ;
#113162 = CARTESIAN_POINT('Ctrl Pts',(8.5454465495755,8.26505438658866,-20.9844168797302)) ;
#113163 = CARTESIAN_POINT('Ctrl Pts',(8.54324462275112,8.25487237915563,-20.9722537533388)) ;
#113164 = CARTESIAN_POINT('Ctrl Pts',(8.53884071267076,8.24480815719263,-20.9612071681992)) ;
#113165 = CARTESIAN_POINT('Ctrl Pts',(8.5342440055524,8.23430333763594,-20.9496769789768)) ;
#113166 = CARTESIAN_POINT('Ctrl Pts',(8.52670159721618,8.22420330618022,-20.938704260243)) ;
#113167 = CARTESIAN_POINT('Ctrl Pts',(8.51928858688475,8.21729138318396,-20.9259881754653)) ;
#113168 = CARTESIAN_POINT('Ctrl Pts',(8.51327528614099,8.21168455548023,-20.915673116045)) ;
#113169 = CARTESIAN_POINT('Ctrl Pts',(8.50759525524367,8.20778929846109,-20.9039849430828)) ;
#113170 = CARTESIAN_POINT('Ctrl Pts',(8.50412058850191,8.20498026622232,-20.8915739486628)) ;
#113171 = CARTESIAN_POINT('Ctrl Pts',(8.50147164778345,8.20283877743224,-20.8821123251694)) ;
#113172 = CARTESIAN_POINT('Ctrl Pts',(8.50000317248551,8.2012555848359,-20.872083357655)) ;
#113173 = CARTESIAN_POINT('Ctrl Pts',(8.50000000513446,8.20000405629318,-20.8621052387284)) ;
#113174 = CARTESIAN_POINT('Origin',(8.6,8.17221734381475,-20.8602872911617)) ;
#113175 = CARTESIAN_POINT('Origin',(8.6,4.35421736843756,-20.8602872911617)) ;
#113176 = CARTESIAN_POINT('Origin',(8.6,6.66256607592813,-20.8602872911617)) ;
#113177 = CARTESIAN_POINT('Ctrl Pts',(8.5,6.47083593368087,-21.1048081099244)) ;
#113178 = CARTESIAN_POINT('Ctrl Pts',(8.5,6.55684090505321,-21.0843877386952)) ;
#113179 = CARTESIAN_POINT('Ctrl Pts',(8.58772778625753,6.56739561896918,-21.081881707091)) ;
#113180 = CARTESIAN_POINT('Ctrl Pts',(8.5,6.45680686388577,-21.0457215297177)) ;
#113181 = CARTESIAN_POINT('Ctrl Pts',(8.50000000000015,6.54406229478603,-21.0525101654037)) ;
#113182 = CARTESIAN_POINT('Ctrl Pts',(8.58195196310359,6.55941415012443,-21.0513576868779)) ;
#113183 = CARTESIAN_POINT('Ctrl Pts',(8.5,6.47061556584392,-20.9819524568048)) ;
#113184 = CARTESIAN_POINT('Ctrl Pts',(8.5,6.54836369988892,-21.0123987274072)) ;
#113185 = CARTESIAN_POINT('Ctrl Pts',(8.57801125828727,6.5656660137223,-21.0188344592028)) ;
#113186 = CARTESIAN_POINT('Ctrl Pts',(8.5,6.54379299301794,-20.8886264716581)) ;
#113187 = CARTESIAN_POINT('Ctrl Pts',(8.5,6.5907178951622,-20.9562265152921)) ;
#113188 = CARTESIAN_POINT('Ctrl Pts',(8.57642058265785,6.60198961470446,-20.9719063540245)) ;
#113189 = CARTESIAN_POINT('Ctrl Pts',(8.5,6.60220518075382,-20.8602872929745)) ;
#113190 = CARTESIAN_POINT('Ctrl Pts',(8.5,6.62800697860328,-20.9409176707628)) ;
#113191 = CARTESIAN_POINT('Ctrl Pts',(8.57879135173924,6.63156920211803,-20.9581318919565)) ;
#113192 = CARTESIAN_POINT('Ctrl Pts',(8.5,6.66256607592813,-20.8602872911617)) ;
#113193 = CARTESIAN_POINT('Ctrl Pts',(8.5,6.66256607592813,-20.945)) ;
#113194 = CARTESIAN_POINT('Ctrl Pts',(8.58356010126947,6.66256607592813,-20.9589266835449)) ;
#113195 = CARTESIAN_POINT('',(8.54565366748552,6.61650711946997,-20.9539653182917)) ;
#113196 = CARTESIAN_POINT('Ctrl Pts',(8.54565366716102,6.61650712004131,-20.9539653178135)) ;
#113197 = CARTESIAN_POINT('Ctrl Pts',(8.54527684775567,6.61717057264361,-20.9534100008637)) ;
#113198 = CARTESIAN_POINT('Ctrl Pts',(8.54488909344006,6.61782772231432,-20.9528554298997)) ;
#113199 = CARTESIAN_POINT('Ctrl Pts',(8.54449064961563,6.61847724592616,-20.9523008713851)) ;
#113200 = CARTESIAN_POINT('Ctrl Pts',(8.54445329550709,6.61853813876477,-20.9522488815244)) ;
#113201 = CARTESIAN_POINT('Ctrl Pts',(8.54441584757976,6.61859896452229,-20.9521968917916)) ;
#113202 = CARTESIAN_POINT('Ctrl Pts',(8.54437830610599,6.61865972207467,-20.9521449015859)) ;
#113203 = CARTESIAN_POINT('Ctrl Pts',(8.54363538409152,6.61986207559656,-20.9511160483068)) ;
#113204 = CARTESIAN_POINT('Ctrl Pts',(8.54285495000596,6.62104203503525,-20.9500848621747)) ;
#113205 = CARTESIAN_POINT('Ctrl Pts',(8.54204093171159,6.62218056960115,-20.9490511151673)) ;
#113206 = CARTESIAN_POINT('Ctrl Pts',(8.54157979215443,6.62282554690592,-20.9484654997818)) ;
#113207 = CARTESIAN_POINT('Ctrl Pts',(8.54110770812191,6.62345780120142,-20.9478786499067)) ;
#113208 = CARTESIAN_POINT('Ctrl Pts',(8.54062344907117,6.62407892448169,-20.9472869541396)) ;
#113209 = CARTESIAN_POINT('Ctrl Pts',(8.54011932596481,6.62472552591744,-20.9466709873185)) ;
#113210 = CARTESIAN_POINT('Ctrl Pts',(8.53960207832256,6.62535666566135,-20.946050990589)) ;
#113211 = CARTESIAN_POINT('Ctrl Pts',(8.53907286520408,6.62597244099096,-20.9454252288111)) ;
#113212 = CARTESIAN_POINT('Ctrl Pts',(8.53887441028465,6.62620335673957,-20.9451905681443)) ;
#113213 = CARTESIAN_POINT('Ctrl Pts',(8.53867427664143,6.6264321129994,-20.9449550998211)) ;
#113214 = CARTESIAN_POINT('Ctrl Pts',(8.53847256319998,6.62665871795109,-20.9447187642184)) ;
#113215 = CARTESIAN_POINT('Ctrl Pts',(8.53842843838466,6.62670828778427,-20.9446670658053)) ;
#113216 = CARTESIAN_POINT('Ctrl Pts',(8.53838423811749,6.62675775467668,-20.9446153260174)) ;
#113217 = CARTESIAN_POINT('Ctrl Pts',(8.53833996369345,6.62680711871687,-20.9445635444601)) ;
#113218 = CARTESIAN_POINT('Ctrl Pts',(8.53829707284515,6.62685494013081,-20.9445133810765)) ;
#113219 = CARTESIAN_POINT('Ctrl Pts',(8.53825411240225,6.62690266502018,-20.9444631784931)) ;
#113220 = CARTESIAN_POINT('Ctrl Pts',(8.53821108363806,6.62695029346532,-20.9444129364377)) ;
#113221 = CARTESIAN_POINT('Ctrl Pts',(8.53803571435332,6.62714440934376,-20.9442081684534)) ;
#113222 = CARTESIAN_POINT('Ctrl Pts',(8.53785876035507,6.62733753498028,-20.9440021836648)) ;
#113223 = CARTESIAN_POINT('Ctrl Pts',(8.53767995296704,6.62753033615257,-20.9437944665652)) ;
#113224 = CARTESIAN_POINT('Ctrl Pts',(8.53649871780654,6.62880401687797,-20.942422248425)) ;
#113225 = CARTESIAN_POINT('Ctrl Pts',(8.53528300832265,6.62998038079526,-20.9410380760596)) ;
#113226 = CARTESIAN_POINT('Ctrl Pts',(8.53403203676338,6.63110281535143,-20.9396044865649)) ;
#113227 = CARTESIAN_POINT('Ctrl Pts',(8.53346870389682,6.63160826591214,-20.9389589178679)) ;
#113228 = CARTESIAN_POINT('Ctrl Pts',(8.53289959536922,6.63209979040222,-20.9383054256595)) ;
#113229 = CARTESIAN_POINT('Ctrl Pts',(8.53232661340321,6.6325773534403,-20.9376437014439)) ;
#113230 = CARTESIAN_POINT('Ctrl Pts',(8.53206474273906,6.63279561467254,-20.9373412727985)) ;
#113231 = CARTESIAN_POINT('Ctrl Pts',(8.53180206199566,6.63301096017661,-20.9370371260807)) ;
#113232 = CARTESIAN_POINT('Ctrl Pts',(8.53153874718658,6.63322338883723,-20.9367312388807)) ;
#113233 = CARTESIAN_POINT('Ctrl Pts',(8.5300736365822,6.63440536369243,-20.9350292511271)) ;
#113234 = CARTESIAN_POINT('Ctrl Pts',(8.52858926277509,6.63549697414122,-20.9332730839131)) ;
#113235 = CARTESIAN_POINT('Ctrl Pts',(8.52711342564668,6.63649856635108,-20.9314611393064)) ;
#113236 = CARTESIAN_POINT('Ctrl Pts',(8.5263431695412,6.63702130866457,-20.9305154649028)) ;
#113237 = CARTESIAN_POINT('Ctrl Pts',(8.52557615349971,6.63751985710294,-20.9295557193112)) ;
#113238 = CARTESIAN_POINT('Ctrl Pts',(8.52481401823433,6.63799287689813,-20.9285803261613)) ;
#113239 = CARTESIAN_POINT('Ctrl Pts',(8.52460710835824,6.63812129566006,-20.9283155195253)) ;
#113240 = CARTESIAN_POINT('Ctrl Pts',(8.52440075574007,6.63824801482191,-20.9280497539023)) ;
#113241 = CARTESIAN_POINT('Ctrl Pts',(8.52419502810874,6.63837284070829,-20.9277830860811)) ;
#113242 = CARTESIAN_POINT('Ctrl Pts',(8.52404824365687,6.63846190263541,-20.9275928214593)) ;
#113243 = CARTESIAN_POINT('Ctrl Pts',(8.52390173612806,6.63855002749204,-20.9274020437347)) ;
#113244 = CARTESIAN_POINT('Ctrl Pts',(8.52375553261477,6.63863721305423,-20.9272107628049)) ;
#113245 = CARTESIAN_POINT('Ctrl Pts',(8.52294204127161,6.63912232246438,-20.9261464560924)) ;
#113246 = CARTESIAN_POINT('Ctrl Pts',(8.52213801365707,6.63957834748689,-20.9250665375564)) ;
#113247 = CARTESIAN_POINT('Ctrl Pts',(8.52134774490512,6.64000494097979,-20.9239729614464)) ;
#113248 = CARTESIAN_POINT('Ctrl Pts',(8.51876608595599,6.64139854145543,-20.9204004545695)) ;
#113249 = CARTESIAN_POINT('Ctrl Pts',(8.51630176076719,6.64256282842068,-20.9166245667844)) ;
#113250 = CARTESIAN_POINT('Ctrl Pts',(8.51404737801022,6.64354662431173,-20.9126687582286)) ;
#113251 = CARTESIAN_POINT('Ctrl Pts',(8.51174271377019,6.64455236266853,-20.9086247197926)) ;
#113252 = CARTESIAN_POINT('Ctrl Pts',(8.50965863261302,6.64536892721963,-20.9043937780696)) ;
#113253 = CARTESIAN_POINT('Ctrl Pts',(8.50786496313903,6.64606338785379,-20.9000441654859)) ;
#113254 = CARTESIAN_POINT('Ctrl Pts',(8.50767015284864,6.64613881316473,-20.8995717544299)) ;
#113255 = CARTESIAN_POINT('Ctrl Pts',(8.50747873128293,6.64621281334902,-20.8990979736875)) ;
#113256 = CARTESIAN_POINT('Ctrl Pts',(8.50729076020856,6.64628549377757,-20.8986229301938)) ;
#113257 = CARTESIAN_POINT('Ctrl Pts',(8.50722027105568,6.64631274893828,-20.8984447888837)) ;
#113258 = CARTESIAN_POINT('Ctrl Pts',(8.50715026706477,6.64633981850992,-20.8982664700192)) ;
#113259 = CARTESIAN_POINT('Ctrl Pts',(8.50708075128541,6.64636670806329,-20.8980879793594)) ;
#113260 = CARTESIAN_POINT('Ctrl Pts',(8.50659414082988,6.6465549349369,-20.896838544741)) ;
#113261 = CARTESIAN_POINT('Ctrl Pts',(8.50613147592892,6.64673434010345,-20.895580683755)) ;
#113262 = CARTESIAN_POINT('Ctrl Pts',(8.50569363751095,6.64690683932497,-20.8943164275023)) ;
#113263 = CARTESIAN_POINT('Ctrl Pts',(8.50395436040173,6.64759207829676,-20.8892942735061)) ;
#113264 = CARTESIAN_POINT('Ctrl Pts',(8.50258205288248,6.64816393978949,-20.8840915596128)) ;
#113265 = CARTESIAN_POINT('Ctrl Pts',(8.50162662717083,6.64864720987532,-20.8788041247401)) ;
#113266 = CARTESIAN_POINT('Ctrl Pts',(8.50156399248179,6.64867889153427,-20.8784574972263)) ;
#113267 = CARTESIAN_POINT('Ctrl Pts',(8.50150313499559,6.64871019935933,-20.8781105075148)) ;
#113268 = CARTESIAN_POINT('Ctrl Pts',(8.50144406283924,6.64874114271687,-20.8777631835019)) ;
#113269 = CARTESIAN_POINT('Ctrl Pts',(8.50057491246564,6.64919642372279,-20.8726528774933)) ;
#113270 = CARTESIAN_POINT('Ctrl Pts',(8.50009537300571,6.64957062705854,-20.8674713290504)) ;
#113271 = CARTESIAN_POINT('Ctrl Pts',(8.50001293997568,6.64989933182553,-20.8623144435395)) ;
#113272 = CARTESIAN_POINT('Ctrl Pts',(8.50000430878269,6.64993374902796,-20.861774489178)) ;
#113273 = CARTESIAN_POINT('Ctrl Pts',(8.5,6.64996765698299,-20.8612348144278)) ;
#113274 = CARTESIAN_POINT('Ctrl Pts',(8.5,6.65000108682384,-20.8606955361059)) ;
#113275 = CARTESIAN_POINT('',(8.55245136877619,6.60097994372616,-20.9667801193795)) ;
#113276 = CARTESIAN_POINT('Ctrl Pts',(8.55238056475491,6.60105295171781,-20.9668886154986)) ;
#113277 = CARTESIAN_POINT('Ctrl Pts',(8.55170523171908,6.60308542368566,-20.9651022656148)) ;
#113278 = CARTESIAN_POINT('Ctrl Pts',(8.5509582952036,6.60513808680132,-20.9633627348221)) ;
#113279 = CARTESIAN_POINT('Ctrl Pts',(8.55012599030524,6.60719152980376,-20.9616544441814)) ;
#113280 = CARTESIAN_POINT('Ctrl Pts',(8.5496832294788,6.60828389886539,-20.9607456856515)) ;
#113281 = CARTESIAN_POINT('Ctrl Pts',(8.54921644930866,6.60937569995271,-20.9598462491234)) ;
#113282 = CARTESIAN_POINT('Ctrl Pts',(8.54872481267393,6.61045954913299,-20.9589557465494)) ;
#113283 = CARTESIAN_POINT('Ctrl Pts',(8.54779539897816,6.61250851009546,-20.9572722973719)) ;
#113284 = CARTESIAN_POINT('Ctrl Pts',(8.54677348694554,6.61453549290064,-20.9556155908862)) ;
#113285 = CARTESIAN_POINT('Ctrl Pts',(8.54565366748551,6.61650711946996,-20.9539653182917)) ;
#113286 = CARTESIAN_POINT('',(8.55735473176745,6.58264207262453,-20.9849557973616)) ;
#113287 = CARTESIAN_POINT('Ctrl Pts',(8.557354731687,6.58264207302788,-20.9849557968441)) ;
#113288 = CARTESIAN_POINT('Ctrl Pts',(8.55706916598053,6.58397660851271,-20.9832296933714)) ;
#113289 = CARTESIAN_POINT('Ctrl Pts',(8.55678088122702,6.58528501693261,-20.9816621009603)) ;
#113290 = CARTESIAN_POINT('Ctrl Pts',(8.55647408091819,6.58661569125895,-20.9801718232515)) ;
#113291 = CARTESIAN_POINT('Ctrl Pts',(8.55614409617576,6.58804692262413,-20.9785689275185)) ;
#113292 = CARTESIAN_POINT('Ctrl Pts',(8.55579261555185,6.58950524590121,-20.9770567950172)) ;
#113293 = CARTESIAN_POINT('Ctrl Pts',(8.55539993844501,6.59102291080546,-20.9755875677792)) ;
#113294 = CARTESIAN_POINT('Ctrl Pts',(8.55517214917304,6.59190329771267,-20.974735279227)) ;
#113295 = CARTESIAN_POINT('Ctrl Pts',(8.55493049881961,6.59280308289159,-20.9738983977538)) ;
#113296 = CARTESIAN_POINT('Ctrl Pts',(8.55467134659048,6.59372113732148,-20.9730707946419)) ;
#113297 = CARTESIAN_POINT('Ctrl Pts',(8.5543480523717,6.59486641664517,-20.9720383539702)) ;
#113298 = CARTESIAN_POINT('Ctrl Pts',(8.55400737519029,6.59602723165037,-20.9710361981957)) ;
#113299 = CARTESIAN_POINT('Ctrl Pts',(8.55365328858766,6.59718920061514,-20.9700452155133)) ;
#113300 = CARTESIAN_POINT('Ctrl Pts',(8.55328167888691,6.59840867329803,-20.969005190911)) ;
#113301 = CARTESIAN_POINT('Ctrl Pts',(8.55289390107695,6.59963546460028,-20.9679736796763)) ;
#113302 = CARTESIAN_POINT('Ctrl Pts',(8.55249886556662,6.60083562835459,-20.9669081494348)) ;
#113303 = CARTESIAN_POINT('Ctrl Pts',(8.55248304763317,6.60088368507325,-20.9668654836845)) ;
#113304 = CARTESIAN_POINT('Ctrl Pts',(8.5524672152281,6.60093179017222,-20.966822806733)) ;
#113305 = CARTESIAN_POINT('Ctrl Pts',(8.55245136877619,6.60097994372615,-20.9667801193796)) ;
#113306 = CARTESIAN_POINT('Ctrl Pts',(8.56107669735261,6.56009388000089,-21.0823838472224)) ;
#113307 = CARTESIAN_POINT('Ctrl Pts',(8.56115635543005,6.55978170524809,-21.0808207343832)) ;
#113308 = CARTESIAN_POINT('Ctrl Pts',(8.56122592915387,6.55950119162287,-21.0792507129806)) ;
#113309 = CARTESIAN_POINT('Ctrl Pts',(8.56128584055879,6.55925348717442,-21.0776933919486)) ;
#113310 = CARTESIAN_POINT('Ctrl Pts',(8.56142626445294,6.55867290283844,-21.074043250811)) ;
#113311 = CARTESIAN_POINT('Ctrl Pts',(8.56152217534693,6.55825854507369,-21.0703756338773)) ;
#113312 = CARTESIAN_POINT('Ctrl Pts',(8.56158081746989,6.55798577878937,-21.0666701354258)) ;
#113313 = CARTESIAN_POINT('Ctrl Pts',(8.56158917845351,6.55794688875062,-21.0661418187435)) ;
#113314 = CARTESIAN_POINT('Ctrl Pts',(8.56159677639836,6.55791088241229,-21.0656126452596)) ;
#113315 = CARTESIAN_POINT('Ctrl Pts',(8.56160362608008,6.55787769947531,-21.0650824674717)) ;
#113316 = CARTESIAN_POINT('Ctrl Pts',(8.56164117305277,6.55769580506315,-21.0621762636859)) ;
#113317 = CARTESIAN_POINT('Ctrl Pts',(8.56164095204358,6.55766773657216,-21.0592640119965)) ;
#113318 = CARTESIAN_POINT('Ctrl Pts',(8.56161306230089,6.55774920537473,-21.0563655672582)) ;
#113319 = CARTESIAN_POINT('Ctrl Pts',(8.56157759693122,6.55785280336173,-21.0526798246077)) ;
#113320 = CARTESIAN_POINT('Ctrl Pts',(8.56150275624659,6.55813669070955,-21.0490049280206)) ;
#113321 = CARTESIAN_POINT('Ctrl Pts',(8.56141108129143,6.55856506509346,-21.0453632925476)) ;
#113322 = CARTESIAN_POINT('Ctrl Pts',(8.56136615997218,6.5587749713042,-21.0435788676806)) ;
#113323 = CARTESIAN_POINT('Ctrl Pts',(8.56131707129296,6.55902016312288,-21.0418016709682)) ;
#113324 = CARTESIAN_POINT('Ctrl Pts',(8.56126585691691,6.55929956116447,-21.0400315254682)) ;
#113325 = CARTESIAN_POINT('Ctrl Pts',(8.56116752027492,6.55983603289969,-21.0366326719095)) ;
#113326 = CARTESIAN_POINT('Ctrl Pts',(8.56104954130216,6.56049109659205,-21.0332540075755)) ;
#113327 = CARTESIAN_POINT('Ctrl Pts',(8.56091150449775,6.56129147625804,-21.0298304710248)) ;
#113328 = CARTESIAN_POINT('Ctrl Pts',(8.56080235670743,6.56192434857304,-21.0271234288616)) ;
#113329 = CARTESIAN_POINT('Ctrl Pts',(8.56068045333715,6.56264902401852,-21.0243872666894)) ;
#113330 = CARTESIAN_POINT('Ctrl Pts',(8.56054379825319,6.56349285586897,-21.0216234877213)) ;
#113331 = CARTESIAN_POINT('Ctrl Pts',(8.56050762866484,6.56371619955867,-21.0208919763521)) ;
#113332 = CARTESIAN_POINT('Ctrl Pts',(8.56047042218818,6.56394794674722,-21.0201587916983)) ;
#113333 = CARTESIAN_POINT('Ctrl Pts',(8.5604321390176,6.56418871538696,-21.0194246234709)) ;
#113334 = CARTESIAN_POINT('Ctrl Pts',(8.56026887460239,6.56521550994376,-21.0162936511792)) ;
#113335 = CARTESIAN_POINT('Ctrl Pts',(8.56008532870544,6.56636514336274,-21.0132612149346)) ;
#113336 = CARTESIAN_POINT('Ctrl Pts',(8.5598891591871,6.56762686151826,-21.0104713276669)) ;
#113337 = CARTESIAN_POINT('Ctrl Pts',(8.55964574654527,6.56919243680269,-21.0070095572757)) ;
#113338 = CARTESIAN_POINT('Ctrl Pts',(8.55938661160132,6.57080906160864,-21.003732634051)) ;
#113339 = CARTESIAN_POINT('Ctrl Pts',(8.55911582090257,6.57246439798288,-21.000667212428)) ;
#113340 = CARTESIAN_POINT('Ctrl Pts',(8.55888928658553,6.57384919626708,-20.9981027846356)) ;
#113341 = CARTESIAN_POINT('Ctrl Pts',(8.55863813502894,6.57544444689303,-20.9953653454317)) ;
#113342 = CARTESIAN_POINT('Ctrl Pts',(8.55834707044214,6.57718152485352,-20.9926681258236)) ;
#113343 = CARTESIAN_POINT('Ctrl Pts',(8.55828762047116,6.57753632320078,-20.9921172184488)) ;
#113344 = CARTESIAN_POINT('Ctrl Pts',(8.55822651695173,6.57789694345767,-20.9915678465794)) ;
#113345 = CARTESIAN_POINT('Ctrl Pts',(8.55816364958867,6.57826264684155,-20.9910215710793)) ;
#113346 = CARTESIAN_POINT('Ctrl Pts',(8.55792499569721,6.57965091145837,-20.9889478277641)) ;
#113347 = CARTESIAN_POINT('Ctrl Pts',(8.5576603261423,6.58110993502786,-20.9869213132877)) ;
#113348 = CARTESIAN_POINT('Ctrl Pts',(8.55735473176745,6.58264207262453,-20.9849557973616)) ;
#113349 = CARTESIAN_POINT('Origin',(8.49172374697018,6.65,-22.86)) ;
#113350 = CARTESIAN_POINT('Origin',(8.49226931262625,6.63793757533841,-21.0929882716362)) ;
#113351 = CARTESIAN_POINT('Ctrl Pts',(8.40188506081761,6.5500005341705,-20.8315458308153)) ;
#113352 = CARTESIAN_POINT('Ctrl Pts',(8.50280744587441,6.54966497091121,-20.8451950407541)) ;
#113353 = CARTESIAN_POINT('Ctrl Pts',(8.50109204799972,6.65199687180765,-20.8456804549399)) ;
#113354 = CARTESIAN_POINT('Ctrl Pts',(8.3929693293079,6.55000052027914,-20.889675802422)) ;
#113355 = CARTESIAN_POINT('Ctrl Pts',(8.49725036372775,6.54968051003366,-20.8769136026832)) ;
#113356 = CARTESIAN_POINT('Ctrl Pts',(8.49665296516362,6.64935672317805,-20.8760247114635)) ;
#113357 = CARTESIAN_POINT('Ctrl Pts',(8.41146079558545,6.55000052635931,-20.949608884646)) ;
#113358 = CARTESIAN_POINT('Ctrl Pts',(8.50278789772743,6.54967384197881,-20.9010143519806)) ;
#113359 = CARTESIAN_POINT('Ctrl Pts',(8.50590954255545,6.65051247736748,-20.9044272120935)) ;
#113360 = CARTESIAN_POINT('Ctrl Pts',(8.45744515914171,6.55000045243509,-21.0028021918823)) ;
#113361 = CARTESIAN_POINT('Ctrl Pts',(8.5202381168081,6.54973725194854,-20.941633015821)) ;
#113362 = CARTESIAN_POINT('Ctrl Pts',(8.52891723073132,6.63643009777379,-20.9334751630783)) ;
#113363 = CARTESIAN_POINT('Ctrl Pts',(8.46608867121678,6.55000043643008,-21.0111950991748)) ;
#113364 = CARTESIAN_POINT('Ctrl Pts',(8.52334270167615,6.54974993059823,-20.948470240079)) ;
#113365 = CARTESIAN_POINT('Ctrl Pts',(8.53324349789231,6.63337968978884,-20.9382208913)) ;
#113366 = CARTESIAN_POINT('Ctrl Pts',(8.48465388181683,6.55000038323734,-21.0265763138745)) ;
#113367 = CARTESIAN_POINT('Ctrl Pts',(8.53001210036428,6.54978938646811,-20.9651245951232)) ;
#113368 = CARTESIAN_POINT('Ctrl Pts',(8.54253954944034,6.62323710347997,-20.948863146269)) ;
#113369 = CARTESIAN_POINT('Ctrl Pts',(8.49467048074911,6.55000035131511,-21.0334884944614)) ;
#113370 = CARTESIAN_POINT('Ctrl Pts',(8.53347884787438,6.54981166882491,-20.97305903115)) ;
#113371 = CARTESIAN_POINT('Ctrl Pts',(8.5475533753473,6.6171479354886,-20.9528676881263)) ;
#113372 = CARTESIAN_POINT('Ctrl Pts',(8.50997930894002,6.55000022766094,-21.0433889027859)) ;
#113373 = CARTESIAN_POINT('Ctrl Pts',(8.53869035159218,6.54988741100163,-20.9987742327549)) ;
#113374 = CARTESIAN_POINT('Ctrl Pts',(8.55523846583762,6.59353839814627,-20.9735278831083)) ;
#113375 = CARTESIAN_POINT('Ctrl Pts',(8.51532901080101,6.55000016113069,-21.0463389673193)) ;
#113376 = CARTESIAN_POINT('Ctrl Pts',(8.54023459682686,6.54992340374042,-21.0084897483873)) ;
#113377 = CARTESIAN_POINT('Ctrl Pts',(8.55790835982309,6.58082417519535,-20.9815823085729)) ;
#113378 = CARTESIAN_POINT('Ctrl Pts',(8.52186010906342,6.55000005932357,-21.0527927598773)) ;
#113379 = CARTESIAN_POINT('Ctrl Pts',(8.54265823247976,6.5499732773141,-21.0379316441152)) ;
#113380 = CARTESIAN_POINT('Ctrl Pts',(8.56121746518602,6.56135337205753,-21.0245883700754)) ;
#113381 = CARTESIAN_POINT('Ctrl Pts',(8.52354993939967,6.55000003603139,-21.0558242622279)) ;
#113382 = CARTESIAN_POINT('Ctrl Pts',(8.54350769968238,6.54998394755847,-21.0514238732007)) ;
#113383 = CARTESIAN_POINT('Ctrl Pts',(8.5621431061544,6.55689632415131,-21.0474501335625)) ;
#113384 = CARTESIAN_POINT('Ctrl Pts',(8.52268461318107,6.55000004733862,-21.0617875304157)) ;
#113385 = CARTESIAN_POINT('Ctrl Pts',(8.54305517585922,6.54997881410036,-21.07281341214)) ;
#113386 = CARTESIAN_POINT('Ctrl Pts',(8.56153259171391,6.55906016573919,-21.0827901815805)) ;
#113387 = CARTESIAN_POINT('Ctrl Pts',(8.52060566253923,6.55000006807331,-21.0644138065496)) ;
#113388 = CARTESIAN_POINT('Ctrl Pts',(8.54195943530536,6.54996919659462,-21.0804945748859)) ;
#113389 = CARTESIAN_POINT('Ctrl Pts',(8.560584416286,6.56302742363386,-21.0945079215137)) ;
#113390 = CARTESIAN_POINT('Ctrl Pts',(8.51445291480382,6.55000012130567,-21.0712328149552)) ;
#113391 = CARTESIAN_POINT('Ctrl Pts',(8.53868948987836,6.54994355920607,-21.0994191817675)) ;
#113392 = CARTESIAN_POINT('Ctrl Pts',(8.55750149922674,6.57320954252655,-21.1211844353069)) ;
#113393 = CARTESIAN_POINT('Ctrl Pts',(8.50953280296012,6.55000015625149,-21.0750479464372)) ;
#113394 = CARTESIAN_POINT('Ctrl Pts',(8.53616288920967,6.54992588038503,-21.1077647485266)) ;
#113395 = CARTESIAN_POINT('Ctrl Pts',(8.55504783006516,6.57989127253965,-21.1306993167928)) ;
#113396 = CARTESIAN_POINT('Ctrl Pts',(8.49261655785707,6.55000026291039,-21.0884926065688)) ;
#113397 = CARTESIAN_POINT('Ctrl Pts',(8.52778251455086,6.54986718408743,-21.1357691608947)) ;
#113398 = CARTESIAN_POINT('Ctrl Pts',(8.54658667616929,6.60027178071327,-21.1593533757438)) ;
#113399 = CARTESIAN_POINT('Ctrl Pts',(8.48022165824516,6.55000031608561,-21.0977685341604)) ;
#113400 = CARTESIAN_POINT('Ctrl Pts',(8.52288681814163,6.54983437262026,-21.1474559489292)) ;
#113401 = CARTESIAN_POINT('Ctrl Pts',(8.5404533945046,6.61042388759305,-21.1663019909607)) ;
#113402 = CARTESIAN_POINT('Ctrl Pts',(8.46952991654743,6.55000035836673,-21.1090954462182)) ;
#113403 = CARTESIAN_POINT('Ctrl Pts',(8.51900842894227,6.54980714069579,-21.1633676846765)) ;
#113404 = CARTESIAN_POINT('Ctrl Pts',(8.53471369258705,6.61849392543623,-21.1813833684422)) ;
#113405 = CARTESIAN_POINT('Origin',(8.4,6.65,-20.8606780018997)) ;
#113406 = CARTESIAN_POINT('Ctrl Pts',(8.54848814460235,8.28374914930622,-19.5635371747799)) ;
#113407 = CARTESIAN_POINT('Ctrl Pts',(8.55964225199693,8.27720012980425,-19.5649679483223)) ;
#113408 = CARTESIAN_POINT('Ctrl Pts',(8.572140519951,8.27365818248462,-19.5657417625569)) ;
#113409 = CARTESIAN_POINT('Ctrl Pts',(8.54519582228988,8.29111303851998,-19.5879603788076)) ;
#113410 = CARTESIAN_POINT('Ctrl Pts',(8.5556995989114,8.28406912459882,-19.5880376174409)) ;
#113411 = CARTESIAN_POINT('Ctrl Pts',(8.56757951573632,8.2799170974937,-19.5881916339118)) ;
#113412 = CARTESIAN_POINT('Ctrl Pts',(8.54340782920287,8.28927570119136,-19.6138229931233)) ;
#113413 = CARTESIAN_POINT('Ctrl Pts',(8.5535505383751,8.28232618564301,-19.6121546442898)) ;
#113414 = CARTESIAN_POINT('Ctrl Pts',(8.56507848568419,8.27803412520748,-19.6111321430533)) ;
#113415 = CARTESIAN_POINT('Ctrl Pts',(8.54340835145922,8.27841951799441,-19.6355350111617)) ;
#113416 = CARTESIAN_POINT('Ctrl Pts',(8.55355093564017,8.27219257320284,-19.6324215387659)) ;
#113417 = CARTESIAN_POINT('Ctrl Pts',(8.56507848521152,8.26835005667905,-19.630500280504)) ;
#113418 = CARTESIAN_POINT('Ctrl Pts',(8.54742026180265,8.27608084857563,-19.6343656412486)) ;
#113419 = CARTESIAN_POINT('Ctrl Pts',(8.54754672558908,8.27683897030432,-19.6326745730365)) ;
#113420 = CARTESIAN_POINT('Ctrl Pts',(8.54766225486891,8.27755642830994,-19.6309654973084)) ;
#113421 = CARTESIAN_POINT('Ctrl Pts',(8.54776713596767,8.27823455672261,-19.6292350167776)) ;
#113422 = CARTESIAN_POINT('Ctrl Pts',(8.54791712013337,8.27920430747289,-19.626760360412)) ;
#113423 = CARTESIAN_POINT('Ctrl Pts',(8.54806168001141,8.28008011045343,-19.6242463372678)) ;
#113424 = CARTESIAN_POINT('Ctrl Pts',(8.54818998754191,8.28086237513948,-19.6217186838591)) ;
#113425 = CARTESIAN_POINT('Ctrl Pts',(8.54824194926749,8.28117917511831,-19.6206950398668)) ;
#113426 = CARTESIAN_POINT('Ctrl Pts',(8.54829140719363,8.2814807826497,-19.6196686742903)) ;
#113427 = CARTESIAN_POINT('Ctrl Pts',(8.54833813644416,8.28176759858577,-19.6186396299771)) ;
#113428 = CARTESIAN_POINT('Ctrl Pts',(8.54850061324771,8.28276485268192,-19.615061660529)) ;
#113429 = CARTESIAN_POINT('Ctrl Pts',(8.54863339756395,8.28360845633779,-19.6113501235291)) ;
#113430 = CARTESIAN_POINT('Ctrl Pts',(8.54873421749656,8.28426438239338,-19.6076130867581)) ;
#113431 = CARTESIAN_POINT('Ctrl Pts',(8.54878752953696,8.28461122607273,-19.6056369987943)) ;
#113432 = CARTESIAN_POINT('Ctrl Pts',(8.54883168679926,8.28490640714041,-19.6036540820739)) ;
#113433 = CARTESIAN_POINT('Ctrl Pts',(8.54886500248133,8.28515040605088,-19.6016818590293)) ;
#113434 = CARTESIAN_POINT('Ctrl Pts',(8.54887385422351,8.2852152348436,-19.6011578532512)) ;
#113435 = CARTESIAN_POINT('Ctrl Pts',(8.54888411330031,8.28527512151702,-19.6006350091921)) ;
#113436 = CARTESIAN_POINT('Ctrl Pts',(8.54889386083024,8.28533143086091,-19.6001120867861)) ;
#113437 = CARTESIAN_POINT('Ctrl Pts',(8.54894969070932,8.28565394783545,-19.5971170003468)) ;
#113438 = CARTESIAN_POINT('Ctrl Pts',(8.54897935138211,8.28586680424121,-19.5940986363827)) ;
#113439 = CARTESIAN_POINT('Ctrl Pts',(8.54899968230029,8.28595875954339,-19.5910675778011)) ;
#113440 = CARTESIAN_POINT('Ctrl Pts',(8.54900356561227,8.28597632348831,-19.5904886297173)) ;
#113441 = CARTESIAN_POINT('Ctrl Pts',(8.54900713937599,8.28598945835117,-19.5899093088041)) ;
#113442 = CARTESIAN_POINT('Ctrl Pts',(8.5490105728891,8.2859980637762,-19.5893298402186)) ;
#113443 = CARTESIAN_POINT('Ctrl Pts',(8.54902784271198,8.28604134718936,-19.5864152394759)) ;
#113444 = CARTESIAN_POINT('Ctrl Pts',(8.54901619593281,8.28598556136224,-19.5835157757217)) ;
#113445 = CARTESIAN_POINT('Ctrl Pts',(8.54898431260111,8.28582669412323,-19.5806064286754)) ;
#113446 = CARTESIAN_POINT('Ctrl Pts',(8.54893914418924,8.28560163041434,-19.5764848209685)) ;
#113447 = CARTESIAN_POINT('Ctrl Pts',(8.54884805310399,8.2851729064642,-19.5723770999644)) ;
#113448 = CARTESIAN_POINT('Ctrl Pts',(8.54869940582901,8.28455561418372,-19.5683070774105)) ;
#113449 = CARTESIAN_POINT('Ctrl Pts',(8.54864697316327,8.28433787538015,-19.5668714498003)) ;
#113450 = CARTESIAN_POINT('Ctrl Pts',(8.5485873643535,8.28409676597397,-19.5654408395913)) ;
#113451 = CARTESIAN_POINT('Ctrl Pts',(8.54851996240545,8.28383343043593,-19.5640172030853)) ;
#113452 = CARTESIAN_POINT('Origin',(8.4,6.65,-22.86)) ;
#113453 = CARTESIAN_POINT('Origin',(8.4,6.65,-19.7793219981003)) ;
#113454 = CARTESIAN_POINT('Origin',(8.49172374697018,6.65,-22.86)) ;
#113455 = CARTESIAN_POINT('Origin',(8.49225485641684,6.63809817973796,-19.5470086283537)) ;
#113456 = CARTESIAN_POINT('Origin',(8.6,4.35421736843756,-19.7797127088383)) ;
#113457 = CARTESIAN_POINT('Origin',(8.6,6.66256607592813,-19.7797127088383)) ;
#113458 = CARTESIAN_POINT('Ctrl Pts',(8.50134874936238,6.65217253603381,-19.7959852560808)) ;
#113459 = CARTESIAN_POINT('Ctrl Pts',(8.50315244876582,6.5499712757703,-19.7965863692586)) ;
#113460 = CARTESIAN_POINT('Ctrl Pts',(8.40269444133667,6.55000000392137,-19.8115964965758)) ;
#113461 = CARTESIAN_POINT('Ctrl Pts',(8.49631753783953,6.64933701877088,-19.7650156523955)) ;
#113462 = CARTESIAN_POINT('Ctrl Pts',(8.49707874924866,6.54997270174429,-19.7639612234982)) ;
#113463 = CARTESIAN_POINT('Ctrl Pts',(8.39261127161998,6.55000000381176,-19.7525550208105)) ;
#113464 = CARTESIAN_POINT('Ctrl Pts',(8.50556246021202,6.6507523520896,-19.7360110455015)) ;
#113465 = CARTESIAN_POINT('Ctrl Pts',(8.50253957946717,6.54997202229494,-19.7396441304546)) ;
#113466 = CARTESIAN_POINT('Ctrl Pts',(8.41103525938995,6.55000000386643,-19.6913383496346)) ;
#113467 = CARTESIAN_POINT('Ctrl Pts',(8.52891970071474,6.63645479210453,-19.7065271584827)) ;
#113468 = CARTESIAN_POINT('Ctrl Pts',(8.52027792490146,6.54997752826675,-19.6984049399611)) ;
#113469 = CARTESIAN_POINT('Ctrl Pts',(8.4576425585104,6.5500000033157,-19.637390101583)) ;
#113470 = CARTESIAN_POINT('Ctrl Pts',(8.53324635448931,6.63340383613801,-19.7017820657382)) ;
#113471 = CARTESIAN_POINT('Ctrl Pts',(8.52338394863782,6.5499786118932,-19.6915733138909)) ;
#113472 = CARTESIAN_POINT('Ctrl Pts',(8.46627109069301,6.55000000319827,-19.6290047485327)) ;
#113473 = CARTESIAN_POINT('Ctrl Pts',(8.54254332011243,6.62325922024827,-19.6911417482178)) ;
#113474 = CARTESIAN_POINT('Ctrl Pts',(8.53005572430516,6.54998198465682,-19.674932642468)) ;
#113475 = CARTESIAN_POINT('Ctrl Pts',(8.48480454940912,6.55000000280808,-19.6136278088231)) ;
#113476 = CARTESIAN_POINT('Ctrl Pts',(8.54755771953125,6.61716872587347,-19.6871385438772)) ;
#113477 = CARTESIAN_POINT('Ctrl Pts',(8.53352383957151,6.54998388968243,-19.6670066149145)) ;
#113478 = CARTESIAN_POINT('Ctrl Pts',(8.49480263348509,6.55000000257396,-19.6067172762992)) ;
#113479 = CARTESIAN_POINT('Ctrl Pts',(8.55524400651034,6.59355301617587,-19.6664805698954)) ;
#113480 = CARTESIAN_POINT('Ctrl Pts',(8.53873552501335,6.54999036710752,-19.6412948588094)) ;
#113481 = CARTESIAN_POINT('Ctrl Pts',(8.51008526949062,6.55000000166752,-19.5967757494185)) ;
#113482 = CARTESIAN_POINT('Ctrl Pts',(8.55791451833572,6.5808349442897,-19.6584270674629)) ;
#113483 = CARTESIAN_POINT('Ctrl Pts',(8.54027978136633,6.54999344602544,-19.6315790288336)) ;
#113484 = CARTESIAN_POINT('Ctrl Pts',(8.51542462880467,6.55000000118004,-19.5938063443386)) ;
#113485 = CARTESIAN_POINT('Ctrl Pts',(8.56122429319345,6.56135755929253,-19.6154165389637)) ;
#113486 = CARTESIAN_POINT('Ctrl Pts',(8.54270214007079,6.54999771321877,-19.6020999056444)) ;
#113487 = CARTESIAN_POINT('Ctrl Pts',(8.5219443634021,6.55000000043436,-19.5872674436738)) ;
#113488 = CARTESIAN_POINT('Ctrl Pts',(8.56215003896757,6.55689889598542,-19.5925513447558)) ;
#113489 = CARTESIAN_POINT('Ctrl Pts',(8.54355112280986,6.54999862629019,-19.5885854140212)) ;
#113490 = CARTESIAN_POINT('Ctrl Pts',(8.52363168464781,6.55000000026381,-19.5841937607945)) ;
#113491 = CARTESIAN_POINT('Ctrl Pts',(8.56153943432815,6.55906352913399,-19.5572061237906)) ;
#113492 = CARTESIAN_POINT('Ctrl Pts',(8.54309854033143,6.54999818700351,-19.5671631682683)) ;
#113493 = CARTESIAN_POINT('Ctrl Pts',(8.52276767133745,6.5500000003466,-19.5781675131799)) ;
#113494 = CARTESIAN_POINT('Ctrl Pts',(8.5605912372004,6.56303220640817,-19.5454869464624)) ;
#113495 = CARTESIAN_POINT('Ctrl Pts',(8.54200379397878,6.54999736403673,-19.5594720470655)) ;
#113496 = CARTESIAN_POINT('Ctrl Pts',(8.52069177703237,6.55000000049843,-19.575521343736)) ;
#113497 = CARTESIAN_POINT('Ctrl Pts',(8.5575081978017,6.57321782814896,-19.5188078145324)) ;
#113498 = CARTESIAN_POINT('Ctrl Pts',(8.53873610184732,6.54999517041883,-19.5405268596428)) ;
#113499 = CARTESIAN_POINT('Ctrl Pts',(8.5145479773404,6.55000000088831,-19.568656630824)) ;
#113500 = CARTESIAN_POINT('Ctrl Pts',(8.55505442469281,6.57990173798312,-19.5092926744612)) ;
#113501 = CARTESIAN_POINT('Ctrl Pts',(8.53621107118182,6.54999365791213,-19.5321766604066)) ;
#113502 = CARTESIAN_POINT('Ctrl Pts',(8.50963525726155,6.55000000114429,-19.5648261829157)) ;
#113503 = CARTESIAN_POINT('Ctrl Pts',(8.55022399280473,6.59153973477787,-19.4929352059185)) ;
#113504 = CARTESIAN_POINT('Ctrl Pts',(8.5315601554517,6.54999086985385,-19.5166211671793)) ;
#113505 = CARTESIAN_POINT('Ctrl Pts',(8.49999539447561,6.55000000159032,-19.5571278236793)) ;
#113506 = CARTESIAN_POINT('Ctrl Pts',(8.54779538881607,6.5966534953294,-19.4869161916983)) ;
#113507 = CARTESIAN_POINT('Ctrl Pts',(8.52936575151139,6.54998957392002,-19.5099955473559)) ;
#113508 = CARTESIAN_POINT('Ctrl Pts',(8.49512741158077,6.55000000178643,-19.5533364158986)) ;
#113509 = CARTESIAN_POINT('Ctrl Pts',(8.54538355337156,6.60121171185028,-19.4816751744843)) ;
#113510 = CARTESIAN_POINT('Ctrl Pts',(8.52733415536173,6.54998837980801,-19.5038983572099)) ;
#113511 = CARTESIAN_POINT('Ctrl Pts',(8.49033880598518,6.55000000196131,-19.5494485970987)) ;
#113512 = CARTESIAN_POINT('',(8.5458234418239,6.61635369861655,-19.6860636515728)) ;
#113513 = CARTESIAN_POINT('Ctrl Pts',(8.5458234418239,6.61635369861655,-19.6860636515728)) ;
#113514 = CARTESIAN_POINT('Ctrl Pts',(8.54493595163524,6.61793460914645,-19.6873940762098)) ;
#113515 = CARTESIAN_POINT('Ctrl Pts',(8.54398448171073,6.61948114927949,-19.6887173928307)) ;
#113516 = CARTESIAN_POINT('Ctrl Pts',(8.54296332801272,6.6209780844369,-19.6900407367798)) ;
#113517 = CARTESIAN_POINT('Ctrl Pts',(8.53827263106763,6.62785429629763,-19.6961195527619)) ;
#113518 = CARTESIAN_POINT('Ctrl Pts',(8.53198779426187,6.63349037496299,-19.7026115685244)) ;
#113519 = CARTESIAN_POINT('Ctrl Pts',(8.5259873730411,6.63731070037229,-19.7100705892422)) ;
#113520 = CARTESIAN_POINT('Ctrl Pts',(8.52000560405467,6.64111915034781,-19.7175064236874)) ;
#113521 = CARTESIAN_POINT('Ctrl Pts',(8.51430181273566,6.64349626850742,-19.7260376473014)) ;
#113522 = CARTESIAN_POINT('Ctrl Pts',(8.50998586672548,6.64522349213896,-19.7352009869701)) ;
#113523 = CARTESIAN_POINT('Ctrl Pts',(8.50534188065424,6.64708199603772,-19.7450608002501)) ;
#113524 = CARTESIAN_POINT('Ctrl Pts',(8.50212992821339,6.64824261275105,-19.7558875436748)) ;
#113525 = CARTESIAN_POINT('Ctrl Pts',(8.50077314609738,6.64911992656046,-19.7668249119168)) ;
#113526 = CARTESIAN_POINT('Ctrl Pts',(8.50025986706873,6.64945181977648,-19.7709625856677)) ;
#113527 = CARTESIAN_POINT('Ctrl Pts',(8.50000017127792,6.64974165917873,-19.7751432551012)) ;
#113528 = CARTESIAN_POINT('Ctrl Pts',(8.5000000000847,6.64999974464545,-19.7793178674956)) ;
#113529 = CARTESIAN_POINT('',(8.55242393572497,6.60106172182536,-19.673242098716)) ;
#113530 = CARTESIAN_POINT('Ctrl Pts',(8.55241775170037,6.6010680791717,-19.6732328161544)) ;
#113531 = CARTESIAN_POINT('Ctrl Pts',(8.55072388788565,6.60619026743349,-19.6777214769524)) ;
#113532 = CARTESIAN_POINT('Ctrl Pts',(8.54858294048575,6.61143812822761,-19.6819269241448)) ;
#113533 = CARTESIAN_POINT('Ctrl Pts',(8.5458234418239,6.61635369861655,-19.6860636515728)) ;
#113534 = CARTESIAN_POINT('Ctrl Pts',(8.55635360773813,6.58637108369504,-19.6586323907337)) ;
#113535 = CARTESIAN_POINT('Ctrl Pts',(8.55606387390184,6.58765239867375,-19.6601123828074)) ;
#113536 = CARTESIAN_POINT('Ctrl Pts',(8.55575324501786,6.5889682390234,-19.6615659413334)) ;
#113537 = CARTESIAN_POINT('Ctrl Pts',(8.55541196992778,6.5903724112747,-19.66304320494)) ;
#113538 = CARTESIAN_POINT('Ctrl Pts',(8.55524290008387,6.59106804711291,-19.6637750506991)) ;
#113539 = CARTESIAN_POINT('Ctrl Pts',(8.55506631250724,6.59178496983012,-19.6645119588375)) ;
#113540 = CARTESIAN_POINT('Ctrl Pts',(8.55488049708426,6.59252693597574,-19.665256277619)) ;
#113541 = CARTESIAN_POINT('Ctrl Pts',(8.55445908016383,6.59420966544526,-19.666944342709)) ;
#113542 = CARTESIAN_POINT('Ctrl Pts',(8.55403589309453,6.59584037906545,-19.6684883777226)) ;
#113543 = CARTESIAN_POINT('Ctrl Pts',(8.55359592981642,6.59737680581866,-19.6699031562334)) ;
#113544 = CARTESIAN_POINT('Ctrl Pts',(8.55324292160432,6.598609570661,-19.671038315592)) ;
#113545 = CARTESIAN_POINT('Ctrl Pts',(8.55287861047125,6.59978201473819,-19.6720910425071)) ;
#113546 = CARTESIAN_POINT('Ctrl Pts',(8.55248933155918,6.60087815532536,-19.6730771269866)) ;
#113547 = CARTESIAN_POINT('Ctrl Pts',(8.55246754857568,6.60093949235542,-19.6731323055778)) ;
#113548 = CARTESIAN_POINT('Ctrl Pts',(8.55244574956032,6.60100068203144,-19.6731872962784)) ;
#113549 = CARTESIAN_POINT('Ctrl Pts',(8.55242393572497,6.60106172182536,-19.673242098716)) ;
#113550 = CARTESIAN_POINT('Ctrl Pts',(8.5,6.66256607592813,-19.7797127088383)) ;
#113551 = CARTESIAN_POINT('Ctrl Pts',(8.5,6.66256607592813,-19.695)) ;
#113552 = CARTESIAN_POINT('Ctrl Pts',(8.58356010126947,6.66256607592813,-19.6810733164551)) ;
#113553 = CARTESIAN_POINT('Ctrl Pts',(8.5,6.61011302719839,-19.779712707263)) ;
#113554 = CARTESIAN_POINT('Ctrl Pts',(8.5,6.63245216822994,-19.6985572365993)) ;
#113555 = CARTESIAN_POINT('Ctrl Pts',(8.57941760042978,6.6356398188513,-19.6817637332617)) ;
#113556 = CARTESIAN_POINT('Ctrl Pts',(8.5,6.55934573373302,-19.7588469099427)) ;
#113557 = CARTESIAN_POINT('Ctrl Pts',(8.5,6.60054351783555,-19.6880813958278)) ;
#113558 = CARTESIAN_POINT('Ctrl Pts',(8.57705842698403,6.6098757899343,-19.6717275280477)) ;
#113559 = CARTESIAN_POINT('Ctrl Pts',(8.5,6.52274941072028,-19.7222505892797)) ;
#113560 = CARTESIAN_POINT('Ctrl Pts',(8.5,6.57873105977929,-19.6662689402207)) ;
#113561 = CARTESIAN_POINT('Ctrl Pts',(8.57705842661295,6.59157413088145,-19.6534258691185)) ;
#113562 = CARTESIAN_POINT('Origin',(8.49172374697003,1.4,-22.86)) ;
#113563 = CARTESIAN_POINT('Origin',(8.49172374697003,1.4,-18.3578583129651)) ;
#113564 = CARTESIAN_POINT('Origin',(8.49172374697002,1.4,-18.3578583129651)) ;
#113565 = CARTESIAN_POINT('Origin',(8.49172374697003,1.4,-18.3578583129651)) ;
#113566 = CARTESIAN_POINT('Ctrl Pts',(8.50816364570057,1.49863939238321,-18.3578583129651)) ;
#113567 = CARTESIAN_POINT('Ctrl Pts',(8.51019246767907,1.4983012553868,-18.392927584071)) ;
#113568 = CARTESIAN_POINT('Ctrl Pts',(8.50816364570057,1.47636598119991,-18.4202920109583)) ;
#113569 = CARTESIAN_POINT('Ctrl Pts',(8.97755831131121,1.42040694811478,-18.3299486511532)) ;
#113570 = CARTESIAN_POINT('Ctrl Pts',(8.97879997398643,1.42020000433524,-18.3645666731799)) ;
#113571 = CARTESIAN_POINT('Ctrl Pts',(8.97755831689156,1.39869563385813,-18.3916948169504)) ;
#113572 = CARTESIAN_POINT('Ctrl Pts',(9.44698496305965,1.34216917282337,-18.3026313706301)) ;
#113573 = CARTESIAN_POINT('Ctrl Pts',(9.44827639615879,1.34195393397322,-18.3367775286088)) ;
#113574 = CARTESIAN_POINT('Ctrl Pts',(9.44698496887881,1.32097764915797,-18.3637229847104)) ;
#113575 = CARTESIAN_POINT('Ctrl Pts',(9.91643989873053,1.26392668354489,-18.2758381198218)) ;
#113576 = CARTESIAN_POINT('Ctrl Pts',(9.91830968165731,1.26361505305709,-18.309509344197)) ;
#113577 = CARTESIAN_POINT('Ctrl Pts',(9.91643989873053,1.24322097942674,-18.336303564194)) ;
#113578 = CARTESIAN_POINT('Origin',(9.9,1.16528729116168,-18.2758381198218)) ;
#113579 = CARTESIAN_POINT('Origin',(9.9,1.16528729116168,-18.2758381198218)) ;
#113580 = CARTESIAN_POINT('Origin',(-0.4,-3.36847777691809,-20.72)) ;
#113581 = CARTESIAN_POINT('Origin',(-0.400000000000001,-3.36847777691809,
-20.72)) ;
#113582 = CARTESIAN_POINT('Origin',(-0.4,-3.36847777691809,-20.72)) ;
#113583 = CARTESIAN_POINT('Origin',(-0.400000000000001,-3.36847777691809,
-19.82)) ;
#113584 = CARTESIAN_POINT('Origin',(-0.4,-3.36847777691809,-19.92)) ;
#113585 = CARTESIAN_POINT('Origin',(-1.11032778078669,-3.36847777691809,-20.72)) ;
#113586 = CARTESIAN_POINT('Origin',(0.4,-3.36847777691809,-20.72)) ;
#113587 = CARTESIAN_POINT('Origin',(-0.400000000000001,-3.36847777691809,
-19.92)) ;
#113588 = CARTESIAN_POINT('Origin',(-0.4,-3.36847777691809,-19.92)) ;
#113589 = CARTESIAN_POINT('Origin',(0.400000000000001,-3.36847777691809,-20.72)) ;
#113590 = CARTESIAN_POINT('Origin',(0.400000000000001,-3.36847777691809,-20.72)) ;
#113591 = CARTESIAN_POINT('Origin',(1.5,-3.36847777691809,-19.92)) ;
#113592 = CARTESIAN_POINT('Origin',(0.4,-3.36847777691809,-19.92)) ;
#113593 = CARTESIAN_POINT('Origin',(0.4,-3.36847777691809,-19.82)) ;
#113594 = CARTESIAN_POINT('Origin',(0.4,-3.36847777691809,-19.92)) ;
#113595 = CARTESIAN_POINT('Origin',(0.4,-3.36847777691809,-19.92)) ;
#113596 = CARTESIAN_POINT('Origin',(7.96847777691809,3.4,-20.72)) ;
#113597 = CARTESIAN_POINT('Origin',(7.96847777691809,3.4,-20.72)) ;
#113598 = CARTESIAN_POINT('Origin',(7.96847777691809,3.4,-20.72)) ;
#113599 = CARTESIAN_POINT('Origin',(7.96847777691809,3.4,-19.82)) ;
#113600 = CARTESIAN_POINT('Origin',(7.96847777691809,3.4,-19.92)) ;
#113601 = CARTESIAN_POINT('Origin',(7.96847777691809,2.68967221921331,-20.72)) ;
#113602 = CARTESIAN_POINT('Origin',(7.96847777691809,4.2,-20.72)) ;
#113603 = CARTESIAN_POINT('Origin',(7.96847777691809,3.4,-19.92)) ;
#113604 = CARTESIAN_POINT('Origin',(7.96847777691809,3.4,-19.92)) ;
#113605 = CARTESIAN_POINT('Origin',(7.96847777691809,4.2,-20.72)) ;
#113606 = CARTESIAN_POINT('Origin',(7.96847777691809,4.2,-20.72)) ;
#113607 = CARTESIAN_POINT('Origin',(7.96847777691809,2.3,-19.92)) ;
#113608 = CARTESIAN_POINT('Origin',(7.96847777691809,4.2,-19.92)) ;
#113609 = CARTESIAN_POINT('Origin',(7.96847777691809,4.2,-19.82)) ;
#113610 = CARTESIAN_POINT('Origin',(7.96847777691809,4.2,-19.92)) ;
#113611 = CARTESIAN_POINT('Origin',(7.96847777691809,4.2,-19.92)) ;
#113612 = CARTESIAN_POINT('Origin',(8.49172374697003,1.4,-22.86)) ;
#113613 = CARTESIAN_POINT('Origin',(8.49172374697003,1.4,-22.2821416870349)) ;
#113614 = CARTESIAN_POINT('Origin',(8.49172374697002,1.4,-22.2821416870349)) ;
#113615 = CARTESIAN_POINT('Origin',(8.49172374697003,1.39999999999989,-22.2821416870347)) ;
#113616 = CARTESIAN_POINT('Ctrl Pts',(8.50816364570058,1.47636598119991,-22.2197079890417)) ;
#113617 = CARTESIAN_POINT('Ctrl Pts',(8.51019246767907,1.4983012553868,-22.247072415929)) ;
#113618 = CARTESIAN_POINT('Ctrl Pts',(8.50816364570058,1.49863939238321,-22.2821416870349)) ;
#113619 = CARTESIAN_POINT('Ctrl Pts',(8.97755831689149,1.39869563385714,-22.2483051830483)) ;
#113620 = CARTESIAN_POINT('Ctrl Pts',(8.97879997398686,1.42020000433534,-22.2754333268135)) ;
#113621 = CARTESIAN_POINT('Ctrl Pts',(8.97755831131135,1.42040694811475,-22.3100513488443)) ;
#113622 = CARTESIAN_POINT('Ctrl Pts',(9.44698496887879,1.32097764915799,-22.2762770152897)) ;
#113623 = CARTESIAN_POINT('Ctrl Pts',(9.4482763961588,1.34195393397339,-22.3032224713911)) ;
#113624 = CARTESIAN_POINT('Ctrl Pts',(9.44698496305964,1.34216917282337,-22.3373686293698)) ;
#113625 = CARTESIAN_POINT('Ctrl Pts',(9.91643989873053,1.24322097942674,-22.303696435806)) ;
#113626 = CARTESIAN_POINT('Ctrl Pts',(9.91830968165732,1.26361505305709,-22.330490655803)) ;
#113627 = CARTESIAN_POINT('Ctrl Pts',(9.91643989873053,1.26392668354489,-22.3641618801782)) ;
#113628 = CARTESIAN_POINT('Origin',(9.9,1.16528729116168,-22.3641618801782)) ;
#113629 = CARTESIAN_POINT('Origin',(9.9,1.16528729116168,-22.3641618801782)) ;
#113630 = CARTESIAN_POINT('Origin',(8.48377223398316,8.2,-22.86)) ;
#113631 = CARTESIAN_POINT('Origin',(8.48238054866943,8.20007133352095,-19.5731789312376)) ;
#113632 = CARTESIAN_POINT('Ctrl Pts',(8.40201662970151,8.3,-19.8059759779215)) ;
#113633 = CARTESIAN_POINT('Ctrl Pts',(8.50299337454958,8.3,-19.7926748112638)) ;
#113634 = CARTESIAN_POINT('Ctrl Pts',(8.50100123624931,8.19773961376455,-19.7926888461178)) ;
#113635 = CARTESIAN_POINT('Ctrl Pts',(8.39454129798956,8.3,-19.7544981813506)) ;
#113636 = CARTESIAN_POINT('Ctrl Pts',(8.49697875237666,8.3,-19.7653741113344)) ;
#113637 = CARTESIAN_POINT('Ctrl Pts',(8.49727262260757,8.20135231978541,-19.765067063962)) ;
#113638 = CARTESIAN_POINT('Ctrl Pts',(8.40820218948347,8.3,-19.7020253635243)) ;
#113639 = CARTESIAN_POINT('Ctrl Pts',(8.49818669687012,8.3,-19.7424717278015)) ;
#113640 = CARTESIAN_POINT('Ctrl Pts',(8.50412619268399,8.20300739730705,-19.7403884100248)) ;
#113641 = CARTESIAN_POINT('Ctrl Pts',(8.4430413476632,8.3,-19.6509969330871)) ;
#113642 = CARTESIAN_POINT('Ctrl Pts',(8.50894174387208,8.3,-19.7008550553805)) ;
#113643 = CARTESIAN_POINT('Ctrl Pts',(8.52157716465943,8.21896555381606,-19.7101661266503)) ;
#113644 = CARTESIAN_POINT('Ctrl Pts',(8.44963266995283,8.3,-19.6426678319782)) ;
#113645 = CARTESIAN_POINT('Ctrl Pts',(8.51095981317517,8.3,-19.6937494404835)) ;
#113646 = CARTESIAN_POINT('Ctrl Pts',(8.52487915500779,8.22226238914488,-19.7049516180519)) ;
#113647 = CARTESIAN_POINT('Ctrl Pts',(8.46372306360151,8.3,-19.6269547263199)) ;
#113648 = CARTESIAN_POINT('Ctrl Pts',(8.51547368264944,8.3,-19.6776327910559)) ;
#113649 = CARTESIAN_POINT('Ctrl Pts',(8.53193863144477,8.23129792829964,-19.6933174783855)) ;
#113650 = CARTESIAN_POINT('Ctrl Pts',(8.47128983770082,8.3,-19.6195586271464)) ;
#113651 = CARTESIAN_POINT('Ctrl Pts',(8.51796237042371,8.3,-19.6692464949128)) ;
#113652 = CARTESIAN_POINT('Ctrl Pts',(8.53572833262714,8.23677343862355,-19.6874295885078)) ;
#113653 = CARTESIAN_POINT('Ctrl Pts',(8.48287565264707,8.3,-19.6087307948332)) ;
#113654 = CARTESIAN_POINT('Ctrl Pts',(8.52168214469875,8.3,-19.65074351943)) ;
#113655 = CARTESIAN_POINT('Ctrl Pts',(8.54153766811345,8.25077321967989,-19.6720449871073)) ;
#113656 = CARTESIAN_POINT('Ctrl Pts',(8.48680760428676,8.3,-19.605187297402)) ;
#113657 = CARTESIAN_POINT('Ctrl Pts',(8.52287759291296,8.3,-19.6441435049317)) ;
#113658 = CARTESIAN_POINT('Ctrl Pts',(8.54350322705384,8.2564691763754,-19.6662622666034)) ;
#113659 = CARTESIAN_POINT('Ctrl Pts',(8.49230810302881,8.3,-19.5994953499955)) ;
#113660 = CARTESIAN_POINT('Ctrl Pts',(8.52426411271138,8.3,-19.6285665246336)) ;
#113661 = CARTESIAN_POINT('Ctrl Pts',(8.54627296401924,8.26866384868896,-19.6485525693616)) ;
#113662 = CARTESIAN_POINT('Ctrl Pts',(8.49410170711667,8.3,-19.597526518934)) ;
#113663 = CARTESIAN_POINT('Ctrl Pts',(8.52463604790914,8.3,-19.6224055253652)) ;
#113664 = CARTESIAN_POINT('Ctrl Pts',(8.54716490137965,8.27360757863441,-19.6407959594825)) ;
#113665 = CARTESIAN_POINT('Ctrl Pts',(8.49698869685298,8.3,-19.5930732788095)) ;
#113666 = CARTESIAN_POINT('Ctrl Pts',(8.52523118911551,8.3,-19.6065929344384)) ;
#113667 = CARTESIAN_POINT('Ctrl Pts',(8.54862931231183,8.28262305001768,-19.6178413492705)) ;
#113668 = CARTESIAN_POINT('Ctrl Pts',(8.49798687771249,8.3,-19.5905165211566)) ;
#113669 = CARTESIAN_POINT('Ctrl Pts',(8.52551930315386,8.3,-19.5969062760439)) ;
#113670 = CARTESIAN_POINT('Ctrl Pts',(8.54912969489065,8.28574379441722,-19.6023818974934)) ;
#113671 = CARTESIAN_POINT('Ctrl Pts',(8.49821791151749,8.3,-19.5825795709374)) ;
#113672 = CARTESIAN_POINT('Ctrl Pts',(8.52559423327562,8.3,-19.5721891247048)) ;
#113673 = CARTESIAN_POINT('Ctrl Pts',(8.54922875625409,8.28635135062008,-19.5632386700468)) ;
#113674 = CARTESIAN_POINT('Ctrl Pts',(8.49537847603514,8.3,-19.5776469108458)) ;
#113675 = CARTESIAN_POINT('Ctrl Pts',(8.5243933105344,8.3,-19.5614732749821)) ;
#113676 = CARTESIAN_POINT('Ctrl Pts',(8.54781890418529,8.28040548672879,-19.548471793372)) ;
#113677 = CARTESIAN_POINT('Ctrl Pts',(8.48955273785443,8.3,-19.5689114034569)) ;
#113678 = CARTESIAN_POINT('Ctrl Pts',(8.52168703568127,8.3,-19.5440525851282)) ;
#113679 = CARTESIAN_POINT('Ctrl Pts',(8.54489815533716,8.27194212599123,-19.5261670077071)) ;
#113680 = CARTESIAN_POINT('Ctrl Pts',(8.48620077197361,8.3,-19.5648263075048)) ;
#113681 = CARTESIAN_POINT('Ctrl Pts',(8.52012703453235,8.3,-19.5371073328932)) ;
#113682 = CARTESIAN_POINT('Ctrl Pts',(8.54324008387894,8.26788967346962,-19.5183142356383)) ;
#113683 = CARTESIAN_POINT('Ctrl Pts',(8.48280151347419,8.3,-19.5607911096407)) ;
#113684 = CARTESIAN_POINT('Ctrl Pts',(8.51858761497412,8.3,-19.5306520257852)) ;
#113685 = CARTESIAN_POINT('Ctrl Pts',(8.54152015125555,8.26408224232382,-19.5113382250347)) ;
#113686 = CARTESIAN_POINT('Origin',(8.4,8.2,-19.777927110149)) ;
#113687 = CARTESIAN_POINT('Origin',(8.4,8.2,-20.945)) ;
#113688 = CARTESIAN_POINT('Origin',(8.4,8.2,-20.862072889851)) ;
#113689 = CARTESIAN_POINT('Ctrl Pts',(8.50101530037396,8.19768718256762,-20.8472017745814)) ;
#113690 = CARTESIAN_POINT('Ctrl Pts',(8.50305639000874,8.3,-20.8472198113571)) ;
#113691 = CARTESIAN_POINT('Ctrl Pts',(8.40204633857706,8.3,-20.8338202021253)) ;
#113692 = CARTESIAN_POINT('Ctrl Pts',(8.49725464441631,8.20131038948437,-20.8748679119096)) ;
#113693 = CARTESIAN_POINT('Ctrl Pts',(8.4970139180527,8.29999999999998,-20.8745609423402)) ;
#113694 = CARTESIAN_POINT('Ctrl Pts',(8.39450526457596,8.3,-20.8853632910711)) ;
#113695 = CARTESIAN_POINT('Ctrl Pts',(8.50410935041309,8.20295267265882,-20.8995792968114)) ;
#113696 = CARTESIAN_POINT('Ctrl Pts',(8.49820749521504,8.30000000000005,-20.8974643378906)) ;
#113697 = CARTESIAN_POINT('Ctrl Pts',(8.40816401923479,8.3,-20.9379187290433)) ;
#113698 = CARTESIAN_POINT('Ctrl Pts',(8.52158236570989,8.2189321678965,-20.9298300407758)) ;
#113699 = CARTESIAN_POINT('Ctrl Pts',(8.5089645656652,8.29999999999999,-20.9391276783841)) ;
#113700 = CARTESIAN_POINT('Ctrl Pts',(8.44304134766321,8.3,-20.9890030669129)) ;
#113701 = CARTESIAN_POINT('Ctrl Pts',(8.52488496507049,8.22222991631201,-20.9350437061782)) ;
#113702 = CARTESIAN_POINT('Ctrl Pts',(8.51098076140206,8.29999999999999,-20.9462331109763)) ;
#113703 = CARTESIAN_POINT('Ctrl Pts',(8.44963266995282,8.3,-20.9973321680218)) ;
#113704 = CARTESIAN_POINT('Ctrl Pts',(8.53194575580938,8.23126818558572,-20.9466757349666)) ;
#113705 = CARTESIAN_POINT('Ctrl Pts',(8.51549074202138,8.30000000000001,-20.9623505031351)) ;
#113706 = CARTESIAN_POINT('Ctrl Pts',(8.46372306360152,8.3,-21.0130452736801)) ;
#113707 = CARTESIAN_POINT('Ctrl Pts',(8.53573618291037,8.23674548871788,-20.9525623770273)) ;
#113708 = CARTESIAN_POINT('Ctrl Pts',(8.51797743940283,8.3,-20.9707374625586)) ;
#113709 = CARTESIAN_POINT('Ctrl Pts',(8.47128983770083,8.3,-21.0204413728536)) ;
#113710 = CARTESIAN_POINT('Ctrl Pts',(8.54154687836688,8.25075037830458,-20.9679451319455)) ;
#113711 = CARTESIAN_POINT('Ctrl Pts',(8.52169408444524,8.3,-20.9892435543493)) ;
#113712 = CARTESIAN_POINT('Ctrl Pts',(8.48287565264706,8.3,-21.0312692051668)) ;
#113713 = CARTESIAN_POINT('Ctrl Pts',(8.54351297666181,8.25644859419422,-20.9737272780162)) ;
#113714 = CARTESIAN_POINT('Ctrl Pts',(8.52288848488736,8.3,-20.9958447315488)) ;
#113715 = CARTESIAN_POINT('Ctrl Pts',(8.48680760428676,8.3,-21.034812702598)) ;
#113716 = CARTESIAN_POINT('Ctrl Pts',(8.54628376412584,8.26864846827403,-20.9914376231601)) ;
#113717 = CARTESIAN_POINT('Ctrl Pts',(8.52427341038692,8.3,-21.0114250170403)) ;
#113718 = CARTESIAN_POINT('Ctrl Pts',(8.4923081030288,8.3,-21.0405046500045)) ;
#113719 = CARTESIAN_POINT('Ctrl Pts',(8.54717611873857,8.27359443500939,-20.9991948837187)) ;
#113720 = CARTESIAN_POINT('Ctrl Pts',(8.52464480444821,8.3,-21.0175873399142)) ;
#113721 = CARTESIAN_POINT('Ctrl Pts',(8.49410170711667,8.3,-21.042473481066)) ;
#113722 = CARTESIAN_POINT('Ctrl Pts',(8.54864126180654,8.28261417405722,-21.0221529061248)) ;
#113723 = CARTESIAN_POINT('Ctrl Pts',(8.52523908688552,8.3,-21.0334032849063)) ;
#113724 = CARTESIAN_POINT('Ctrl Pts',(8.49698869685298,8.3,-21.0469267211905)) ;
#113725 = CARTESIAN_POINT('Ctrl Pts',(8.5491418548716,8.28573645090425,-21.0376152824162)) ;
#113726 = CARTESIAN_POINT('Ctrl Pts',(8.52552693815802,8.3,-21.0430919520163)) ;
#113727 = CARTESIAN_POINT('Ctrl Pts',(8.49798687771249,8.3,-21.0494834788434)) ;
#113728 = CARTESIAN_POINT('Ctrl Pts',(8.54924094958847,8.28634430798884,-21.0767659475983)) ;
#113729 = CARTESIAN_POINT('Ctrl Pts',(8.52560181204939,8.3,-21.0678137517531)) ;
#113730 = CARTESIAN_POINT('Ctrl Pts',(8.49821791151747,8.3,-21.0574204290626)) ;
#113731 = CARTESIAN_POINT('Ctrl Pts',(8.54783079466743,8.28039553911293,-21.0915348059813)) ;
#113732 = CARTESIAN_POINT('Ctrl Pts',(8.52440147378976,8.3,-21.0785312754323)) ;
#113733 = CARTESIAN_POINT('Ctrl Pts',(8.49537847603514,8.3,-21.0623530891542)) ;
#113734 = CARTESIAN_POINT('Ctrl Pts',(8.5446588398693,8.27120119512636,-21.1157571947032)) ;
#113735 = CARTESIAN_POINT('Ctrl Pts',(8.52145785975945,8.3,-21.0974902783301)) ;
#113736 = CARTESIAN_POINT('Ctrl Pts',(8.48905244827037,8.3,-21.0718387647145)) ;
#113737 = CARTESIAN_POINT('Ctrl Pts',(8.54267599402785,8.26648669506698,-21.1242949904305)) ;
#113738 = CARTESIAN_POINT('Ctrl Pts',(8.51958784692425,8.3,-21.1052641321446)) ;
#113739 = CARTESIAN_POINT('Ctrl Pts',(8.48503640902804,8.3,-21.0765685970659)) ;
#113740 = CARTESIAN_POINT('Ctrl Pts',(8.54064021294341,8.26212437554838,-21.1322000298239)) ;
#113741 = CARTESIAN_POINT('Ctrl Pts',(8.51779796763698,8.3,-21.1126895170151)) ;
#113742 = CARTESIAN_POINT('Ctrl Pts',(8.48104783026774,8.3,-21.0812848074951)) ;
#113743 = CARTESIAN_POINT('Origin',(8.48238055011341,8.20007134081619,-21.0668210700733)) ;
#113744 = CARTESIAN_POINT('Origin',(8.48377223398316,8.2,-22.86)) ;
#113745 = CARTESIAN_POINT('',(0.,0.,0.)) ;
#113746 = CARTESIAN_POINT('Origin',(1.27,5.3848,0.)) ;
#113747 = CARTESIAN_POINT('',(1.27,1.397,1.4986)) ;
#113748 = CARTESIAN_POINT('Origin',(1.27,1.397,0.)) ;
#113749 = CARTESIAN_POINT('',(1.27,3.8862,1.4986)) ;
#113750 = CARTESIAN_POINT('',(1.27,5.3848,1.4986)) ;
#113751 = CARTESIAN_POINT('',(-0.2286,3.8862,1.83525569320222E-16)) ;
#113752 = CARTESIAN_POINT('Origin',(1.27,3.8862,0.)) ;
#113753 = CARTESIAN_POINT('Origin',(1.27,3.8862,0.)) ;
#113754 = CARTESIAN_POINT('Origin',(1.27,1.397,0.)) ;
#113755 = CARTESIAN_POINT('',(2.58523201375271,1.397,1.4986)) ;
#113756 = CARTESIAN_POINT('',(-0.0452320137527065,1.397,1.4986)) ;
#113757 = CARTESIAN_POINT('Origin',(1.27,1.397,0.)) ;
#113758 = CARTESIAN_POINT('',(2.58523201375271,0.381,1.4986)) ;
#113759 = CARTESIAN_POINT('',(2.58523201375271,1.397,1.4986)) ;
#113760 = CARTESIAN_POINT('',(-0.0452320137527065,0.381,1.4986)) ;
#113761 = CARTESIAN_POINT('Origin',(1.27,0.381,0.)) ;
#113762 = CARTESIAN_POINT('',(-0.0452320137527065,1.397,1.4986)) ;
#113763 = CARTESIAN_POINT('Origin',(-0.254,0.381,0.254)) ;
#113764 = CARTESIAN_POINT('',(0.254,-0.254,0.254)) ;
#113765 = CARTESIAN_POINT('',(0.508,0.,0.254)) ;
#113766 = CARTESIAN_POINT('Origin',(0.508,-0.254,0.254)) ;
#113767 = CARTESIAN_POINT('',(0.508,0.381,0.254)) ;
#113768 = CARTESIAN_POINT('',(0.508,0.381,0.254)) ;
#113769 = CARTESIAN_POINT('',(0.,0.381,0.254)) ;
#113770 = CARTESIAN_POINT('',(-0.254,0.381,0.254)) ;
#113771 = CARTESIAN_POINT('',(-0.254,0.127,0.254)) ;
#113772 = CARTESIAN_POINT('Origin',(0.,0.127,0.254)) ;
#113773 = CARTESIAN_POINT('',(-0.254,-3.175,0.254)) ;
#113774 = CARTESIAN_POINT('',(-0.254,0.381,0.254)) ;
#113775 = CARTESIAN_POINT('',(0.254,-3.175,0.254)) ;
#113776 = CARTESIAN_POINT('',(-0.254,-3.175,0.254)) ;
#113777 = CARTESIAN_POINT('',(0.254,-3.175,0.254)) ;
#113778 = CARTESIAN_POINT('Origin',(-0.254,0.381,-0.254)) ;
#113779 = CARTESIAN_POINT('',(0.508,0.381,-0.254)) ;
#113780 = CARTESIAN_POINT('',(-5.42101086242752E-17,0.381,-0.254)) ;
#113781 = CARTESIAN_POINT('',(-0.254,0.381,-0.254)) ;
#113782 = CARTESIAN_POINT('',(0.508,0.,-0.254)) ;
#113783 = CARTESIAN_POINT('',(0.508,0.381,-0.254)) ;
#113784 = CARTESIAN_POINT('',(0.254,-0.254,-0.254)) ;
#113785 = CARTESIAN_POINT('Origin',(0.508,-0.254,-0.254)) ;
#113786 = CARTESIAN_POINT('',(0.254,-3.175,-0.254)) ;
#113787 = CARTESIAN_POINT('',(0.254,-3.175,-0.254)) ;
#113788 = CARTESIAN_POINT('',(-0.254,-3.175,-0.254)) ;
#113789 = CARTESIAN_POINT('',(-0.254,-3.175,-0.254)) ;
#113790 = CARTESIAN_POINT('',(-0.254,0.127,-0.254)) ;
#113791 = CARTESIAN_POINT('',(-0.254,0.381,-0.254)) ;
#113792 = CARTESIAN_POINT('Origin',(-5.42101086242752E-17,0.127,-0.254)) ;
#113793 = CARTESIAN_POINT('Origin',(-0.254,0.381,-0.254)) ;
#113794 = CARTESIAN_POINT('',(-0.254,0.127,-0.254)) ;
#113795 = CARTESIAN_POINT('',(-0.254,-3.175,0.254)) ;
#113796 = CARTESIAN_POINT('Origin',(-0.254,0.381,0.254)) ;
#113797 = CARTESIAN_POINT('',(2.032,0.381,0.254)) ;
#113798 = CARTESIAN_POINT('',(2.54,0.381,0.254)) ;
#113799 = CARTESIAN_POINT('',(-0.254,0.381,0.254)) ;
#113800 = CARTESIAN_POINT('',(2.032,0.,0.254)) ;
#113801 = CARTESIAN_POINT('',(2.032,0.381,0.254)) ;
#113802 = CARTESIAN_POINT('',(2.286,-0.254,0.254)) ;
#113803 = CARTESIAN_POINT('Origin',(2.032,-0.254,0.254)) ;
#113804 = CARTESIAN_POINT('',(2.286,-3.175,0.254)) ;
#113805 = CARTESIAN_POINT('',(2.286,-3.175,0.254)) ;
#113806 = CARTESIAN_POINT('',(2.794,-3.175,0.254)) ;
#113807 = CARTESIAN_POINT('',(2.794,-3.175,0.254)) ;
#113808 = CARTESIAN_POINT('',(2.794,0.127,0.254)) ;
#113809 = CARTESIAN_POINT('',(2.794,0.381,0.254)) ;
#113810 = CARTESIAN_POINT('Origin',(2.54,0.127,0.254)) ;
#113811 = CARTESIAN_POINT('Origin',(2.794,0.381,-0.254)) ;
#113812 = CARTESIAN_POINT('',(2.794,0.127,-0.254)) ;
#113813 = CARTESIAN_POINT('',(2.794,-3.175,-0.254)) ;
#113814 = CARTESIAN_POINT('',(2.794,0.381,-0.254)) ;
#113815 = CARTESIAN_POINT('',(2.794,0.127,0.254)) ;
#113816 = CARTESIAN_POINT('',(2.794,-3.175,0.254)) ;
#113817 = CARTESIAN_POINT('Origin',(-0.254,0.381,-0.254)) ;
#113818 = CARTESIAN_POINT('',(2.286,-0.254,-0.254)) ;
#113819 = CARTESIAN_POINT('',(2.032,0.,-0.254)) ;
#113820 = CARTESIAN_POINT('Origin',(2.032,-0.254,-0.254)) ;
#113821 = CARTESIAN_POINT('',(2.032,0.381,-0.254)) ;
#113822 = CARTESIAN_POINT('',(2.032,0.381,-0.254)) ;
#113823 = CARTESIAN_POINT('',(2.54,0.381,-0.254)) ;
#113824 = CARTESIAN_POINT('',(-0.254,0.381,-0.254)) ;
#113825 = CARTESIAN_POINT('Origin',(2.54,0.127,-0.254)) ;
#113826 = CARTESIAN_POINT('',(2.286,-3.175,-0.254)) ;
#113827 = CARTESIAN_POINT('',(2.794,-3.175,-0.254)) ;
#113828 = CARTESIAN_POINT('',(2.286,-3.175,-0.254)) ;
#113829 = CARTESIAN_POINT('Origin',(0.254,-3.175,0.254)) ;
#113830 = CARTESIAN_POINT('',(0.254,-0.254,0.254)) ;
#113831 = CARTESIAN_POINT('',(0.254,-3.175,0.254)) ;
#113832 = CARTESIAN_POINT('Origin',(-0.254,-3.175,-0.254)) ;
#113833 = CARTESIAN_POINT('Origin',(2.286,-3.175,0.254)) ;
#113834 = CARTESIAN_POINT('',(2.286,-0.254,-0.254)) ;
#113835 = CARTESIAN_POINT('',(2.286,-3.175,0.254)) ;
#113836 = CARTESIAN_POINT('Origin',(2.794,-3.175,-0.254)) ;
#113837 = CARTESIAN_POINT('Origin',(0.,0.127,0.254)) ;
#113838 = CARTESIAN_POINT('',(-2.89245657190524E-33,0.381,0.254)) ;
#113839 = CARTESIAN_POINT('Origin',(2.54,0.127,0.254)) ;
#113840 = CARTESIAN_POINT('',(2.54,0.381,-0.254)) ;
#113841 = CARTESIAN_POINT('Origin',(0.508,-0.254,0.254)) ;
#113842 = CARTESIAN_POINT('',(0.508,0.,-0.254)) ;
#113843 = CARTESIAN_POINT('Origin',(2.032,-0.254,0.254)) ;
#113844 = CARTESIAN_POINT('',(2.032,0.,0.254)) ;
#113845 = CARTESIAN_POINT('Origin',(1.27,0.381,0.)) ;
#113846 = CARTESIAN_POINT('',(2.58523201375271,0.381,1.4986)) ;
#113847 = CARTESIAN_POINT('',(0.508,0.381,-1.9939)) ;
#113848 = CARTESIAN_POINT('',(2.032,0.381,-1.9939)) ;
#113849 = CARTESIAN_POINT('Origin',(2.58523201375271,1.397,1.4986)) ;
#113850 = CARTESIAN_POINT('',(2.58523201375271,1.397,1.4986)) ;
#113851 = CARTESIAN_POINT('',(2.58523201375271,1.397,1.4986)) ;
#113852 = CARTESIAN_POINT('Origin',(1.27,1.397,0.)) ;
#113853 = CARTESIAN_POINT('Origin',(1.27,3.8862,0.)) ;
#113854 = CARTESIAN_POINT('',(1.27,5.3848,1.12377000514853E-32)) ;
#113855 = CARTESIAN_POINT('Origin',(1.27,3.8862,0.)) ;
#113856 = CARTESIAN_POINT('Origin',(0.508,0.381,-1.9939)) ;
#113857 = CARTESIAN_POINT('Origin',(2.032,0.381,-1.9939)) ;
#113858 = CARTESIAN_POINT('',(0.,0.,0.)) ;
#113859 = CARTESIAN_POINT('Origin',(2.3,0.,-34.29)) ;
#113860 = CARTESIAN_POINT('',(2.4,-1.10218211923262E-16,-33.39)) ;
#113861 = CARTESIAN_POINT('Origin',(2.4,0.,-34.29)) ;
#113862 = CARTESIAN_POINT('',(2.3,-1.22464679914735E-16,-33.29)) ;
#113863 = CARTESIAN_POINT('Origin',(2.3,-1.10218211923262E-16,-33.39)) ;
#113864 = CARTESIAN_POINT('',(2.3,1.22464679914735E-16,-35.29)) ;
#113865 = CARTESIAN_POINT('Origin',(2.3,0.,-34.29)) ;
#113866 = CARTESIAN_POINT('Origin',(2.3,0.,-34.29)) ;
#113867 = CARTESIAN_POINT('Origin',(1.5,0.,-34.29)) ;
#113868 = CARTESIAN_POINT('',(1.4,-1.34711147906208E-16,-35.39)) ;
#113869 = CARTESIAN_POINT('Origin',(1.4,0.,-34.29)) ;
#113870 = CARTESIAN_POINT('',(1.5,-1.22464679914735E-16,-35.29)) ;
#113871 = CARTESIAN_POINT('Origin',(1.5,-1.34711147906209E-16,-35.39)) ;
#113872 = CARTESIAN_POINT('Origin',(1.5,0.,-34.29)) ;
#113873 = CARTESIAN_POINT('Origin',(1.5,3.15,-33.0314213562373)) ;
#113874 = CARTESIAN_POINT('',(1.5,3.07928932188135,-32.9607106781187)) ;
#113875 = CARTESIAN_POINT('',(1.5,3.25,-33.0314213562373)) ;
#113876 = CARTESIAN_POINT('Origin',(1.5,3.15,-33.0314213562373)) ;
#113877 = CARTESIAN_POINT('',(1.4,3.15,-33.0314213562373)) ;
#113878 = CARTESIAN_POINT('Origin',(1.5,3.15,-33.0314213562373)) ;
#113879 = CARTESIAN_POINT('Origin',(1.5,3.15,-33.0314213562373)) ;
#113880 = CARTESIAN_POINT('Origin',(0.500000000000001,-4.56640444411537E-17,
-34.69)) ;
#113881 = CARTESIAN_POINT('',(0.600000000000001,0.4,-34.69)) ;
#113882 = CARTESIAN_POINT('',(0.59561299721608,0.370705721320401,-34.6607057213204)) ;
#113883 = CARTESIAN_POINT('Origin',(0.500000000014529,0.399999999998192,-34.6899999999979)) ;
#113884 = CARTESIAN_POINT('',(0.500000000000001,0.4,-34.79)) ;
#113885 = CARTESIAN_POINT('Origin',(0.500000000000001,0.4,-34.69)) ;
#113886 = CARTESIAN_POINT('',(0.500000000000001,-1.9,-34.79)) ;
#113887 = CARTESIAN_POINT('',(0.500000000000001,0.5,-34.79)) ;
#113888 = CARTESIAN_POINT('',(0.600000000000001,-1.9,-34.69)) ;
#113889 = CARTESIAN_POINT('Origin',(0.500000000000001,-1.9,-34.69)) ;
#113890 = CARTESIAN_POINT('',(0.600000000000001,-0.3,-34.69)) ;
#113891 = CARTESIAN_POINT('',(0.600000000000001,-2.39800009914437E-17,-34.69)) ;
#113892 = CARTESIAN_POINT('',(0.600000000000001,0.299999999999999,-34.69)) ;
#113893 = CARTESIAN_POINT('',(0.600000000000001,-2.39800009914437E-17,-34.69)) ;
#113894 = CARTESIAN_POINT('Ctrl Pts',(0.600000000000001,0.300000000000003,
-34.69)) ;
#113895 = CARTESIAN_POINT('Ctrl Pts',(0.600000000000001,0.312243016306297,
-34.69)) ;
#113896 = CARTESIAN_POINT('Ctrl Pts',(0.60006974742297,0.324350425899703,
-34.6877515285214)) ;
#113897 = CARTESIAN_POINT('Ctrl Pts',(0.599517124288205,0.34619696929781,
-34.6793954490601)) ;
#113898 = CARTESIAN_POINT('Ctrl Pts',(0.598927484301131,0.355857825373572,
-34.6736750447227)) ;
#113899 = CARTESIAN_POINT('Ctrl Pts',(0.596766673872563,0.366539012308038,
-34.6647023851096)) ;
#113900 = CARTESIAN_POINT('Ctrl Pts',(0.59623562910414,0.368676603883175,
-34.6627379168092)) ;
#113901 = CARTESIAN_POINT('Ctrl Pts',(0.59561299721608,0.370705721320409,
-34.6607057213204)) ;
#113902 = CARTESIAN_POINT('Origin',(2.3,0.,-30.48)) ;
#113903 = CARTESIAN_POINT('',(2.4,-1.10218211923262E-16,-29.58)) ;
#113904 = CARTESIAN_POINT('Origin',(2.4,0.,-30.48)) ;
#113905 = CARTESIAN_POINT('',(2.3,-1.22464679914735E-16,-29.48)) ;
#113906 = CARTESIAN_POINT('Origin',(2.3,-1.10218211923262E-16,-29.58)) ;
#113907 = CARTESIAN_POINT('',(2.3,1.22464679914735E-16,-31.48)) ;
#113908 = CARTESIAN_POINT('Origin',(2.3,0.,-30.48)) ;
#113909 = CARTESIAN_POINT('Origin',(2.3,0.,-30.48)) ;
#113910 = CARTESIAN_POINT('Origin',(1.5,0.,-30.48)) ;
#113911 = CARTESIAN_POINT('',(1.4,-1.34711147906209E-16,-31.58)) ;
#113912 = CARTESIAN_POINT('Origin',(1.4,0.,-30.48)) ;
#113913 = CARTESIAN_POINT('',(1.5,-1.22464679914735E-16,-31.48)) ;
#113914 = CARTESIAN_POINT('Origin',(1.5,-1.34711147906209E-16,-31.58)) ;
#113915 = CARTESIAN_POINT('Origin',(1.5,0.,-30.48)) ;
#113916 = CARTESIAN_POINT('Origin',(1.5,3.15,-29.2214213562373)) ;
#113917 = CARTESIAN_POINT('',(1.5,3.07928932188135,-29.1507106781187)) ;
#113918 = CARTESIAN_POINT('',(1.5,3.25,-29.2214213562373)) ;
#113919 = CARTESIAN_POINT('Origin',(1.5,3.15,-29.2214213562373)) ;
#113920 = CARTESIAN_POINT('',(1.4,3.15,-29.2214213562373)) ;
#113921 = CARTESIAN_POINT('Origin',(1.5,3.15,-29.2214213562373)) ;
#113922 = CARTESIAN_POINT('Origin',(1.5,3.15,-29.2214213562373)) ;
#113923 = CARTESIAN_POINT('Origin',(0.500000000000001,-4.56640444411542E-17,
-30.88)) ;
#113924 = CARTESIAN_POINT('',(0.600000000000001,0.4,-30.88)) ;
#113925 = CARTESIAN_POINT('',(0.595612997216081,0.370705721320403,-30.8507057213204)) ;
#113926 = CARTESIAN_POINT('Origin',(0.500000000043895,0.399999999994469,-30.8799999999944)) ;
#113927 = CARTESIAN_POINT('',(0.500000000000001,0.4,-30.98)) ;
#113928 = CARTESIAN_POINT('Origin',(0.500000000000001,0.4,-30.88)) ;
#113929 = CARTESIAN_POINT('',(0.500000000000001,-1.9,-30.98)) ;
#113930 = CARTESIAN_POINT('',(0.500000000000001,0.5,-30.98)) ;
#113931 = CARTESIAN_POINT('',(0.600000000000001,-1.9,-30.88)) ;
#113932 = CARTESIAN_POINT('Origin',(0.500000000000001,-1.9,-30.88)) ;
#113933 = CARTESIAN_POINT('',(0.600000000000001,-0.3,-30.88)) ;
#113934 = CARTESIAN_POINT('',(0.600000000000001,-2.39800009914441E-17,-30.88)) ;
#113935 = CARTESIAN_POINT('',(0.600000000000001,0.299999999999999,-30.88)) ;
#113936 = CARTESIAN_POINT('',(0.600000000000001,-2.39800009914441E-17,-30.88)) ;
#113937 = CARTESIAN_POINT('Ctrl Pts',(0.600000000000001,0.300000000000003,
-30.88)) ;
#113938 = CARTESIAN_POINT('Ctrl Pts',(0.600000000000001,0.312243016306059,
-30.88)) ;
#113939 = CARTESIAN_POINT('Ctrl Pts',(0.600069747422976,0.324350425899479,
-30.8777515285215)) ;
#113940 = CARTESIAN_POINT('Ctrl Pts',(0.59951712428821,0.346196969297596,
-30.8693954490601)) ;
#113941 = CARTESIAN_POINT('Ctrl Pts',(0.598927484301166,0.355857825373397,
-30.8636750447228)) ;
#113942 = CARTESIAN_POINT('Ctrl Pts',(0.596766673872565,0.36653901230802,
-30.8547023851096)) ;
#113943 = CARTESIAN_POINT('Ctrl Pts',(0.596235629104145,0.368676603883157,
-30.8527379168092)) ;
#113944 = CARTESIAN_POINT('Ctrl Pts',(0.595612997216081,0.370705721320405,
-30.8507057213204)) ;
#113945 = CARTESIAN_POINT('Origin',(2.3,0.,-26.67)) ;
#113946 = CARTESIAN_POINT('',(2.4,-1.10218211923262E-16,-25.77)) ;
#113947 = CARTESIAN_POINT('Origin',(2.4,0.,-26.67)) ;
#113948 = CARTESIAN_POINT('',(2.3,-1.22464679914735E-16,-25.67)) ;
#113949 = CARTESIAN_POINT('Origin',(2.3,-1.10218211923262E-16,-25.77)) ;
#113950 = CARTESIAN_POINT('',(2.3,1.22464679914735E-16,-27.67)) ;
#113951 = CARTESIAN_POINT('Origin',(2.3,0.,-26.67)) ;
#113952 = CARTESIAN_POINT('Origin',(2.3,0.,-26.67)) ;
#113953 = CARTESIAN_POINT('Origin',(1.5,0.,-26.67)) ;
#113954 = CARTESIAN_POINT('',(1.4,-1.34711147906209E-16,-27.77)) ;
#113955 = CARTESIAN_POINT('Origin',(1.4,0.,-26.67)) ;
#113956 = CARTESIAN_POINT('',(1.5,-1.22464679914735E-16,-27.67)) ;
#113957 = CARTESIAN_POINT('Origin',(1.5,-1.34711147906209E-16,-27.77)) ;
#113958 = CARTESIAN_POINT('Origin',(1.5,0.,-26.67)) ;
#113959 = CARTESIAN_POINT('Origin',(1.5,3.15,-25.4114213562373)) ;
#113960 = CARTESIAN_POINT('',(1.5,3.07928932188135,-25.3407106781187)) ;
#113961 = CARTESIAN_POINT('',(1.5,3.25,-25.4114213562373)) ;
#113962 = CARTESIAN_POINT('Origin',(1.5,3.15,-25.4114213562373)) ;
#113963 = CARTESIAN_POINT('',(1.4,3.15,-25.4114213562373)) ;
#113964 = CARTESIAN_POINT('Origin',(1.5,3.15,-25.4114213562373)) ;
#113965 = CARTESIAN_POINT('Origin',(1.5,3.15,-25.4114213562373)) ;
#113966 = CARTESIAN_POINT('Origin',(0.500000000000001,-4.56640444411542E-17,
-27.07)) ;
#113967 = CARTESIAN_POINT('',(0.600000000000001,0.4,-27.07)) ;
#113968 = CARTESIAN_POINT('',(0.595612997216081,0.370705721320403,-27.0407057213204)) ;
#113969 = CARTESIAN_POINT('Origin',(0.500000000043127,0.39999999999434,-27.0699999999943)) ;
#113970 = CARTESIAN_POINT('',(0.500000000000001,0.4,-27.17)) ;
#113971 = CARTESIAN_POINT('Origin',(0.500000000000001,0.4,-27.07)) ;
#113972 = CARTESIAN_POINT('',(0.500000000000001,-1.9,-27.17)) ;
#113973 = CARTESIAN_POINT('',(0.500000000000001,0.5,-27.17)) ;
#113974 = CARTESIAN_POINT('',(0.600000000000001,-1.9,-27.07)) ;
#113975 = CARTESIAN_POINT('Origin',(0.500000000000001,-1.9,-27.07)) ;
#113976 = CARTESIAN_POINT('',(0.600000000000001,-0.3,-27.07)) ;
#113977 = CARTESIAN_POINT('',(0.600000000000001,-2.39800009914441E-17,-27.07)) ;
#113978 = CARTESIAN_POINT('',(0.600000000000001,0.299999999999999,-27.07)) ;
#113979 = CARTESIAN_POINT('',(0.600000000000001,-2.39800009914441E-17,-27.07)) ;
#113980 = CARTESIAN_POINT('Ctrl Pts',(0.600000000000001,0.300000000000003,
-27.07)) ;
#113981 = CARTESIAN_POINT('Ctrl Pts',(0.600000000000001,0.312243016306037,
-27.07)) ;
#113982 = CARTESIAN_POINT('Ctrl Pts',(0.600069747422976,0.324350425899459,
-27.0677515285215)) ;
#113983 = CARTESIAN_POINT('Ctrl Pts',(0.59951712428821,0.346196969297585,
-27.0593954490602)) ;
#113984 = CARTESIAN_POINT('Ctrl Pts',(0.598927484301167,0.355857825373385,
-27.0536750447229)) ;
#113985 = CARTESIAN_POINT('Ctrl Pts',(0.596766673872565,0.366539012308015,
-27.0447023851096)) ;
#113986 = CARTESIAN_POINT('Ctrl Pts',(0.596235629104144,0.368676603883154,
-27.0427379168092)) ;
#113987 = CARTESIAN_POINT('Ctrl Pts',(0.59561299721608,0.370705721320403,
-27.0407057213204)) ;
#113988 = CARTESIAN_POINT('Origin',(2.3,0.,-22.86)) ;
#113989 = CARTESIAN_POINT('',(2.4,-1.10218211923262E-16,-21.96)) ;
#113990 = CARTESIAN_POINT('Origin',(2.4,0.,-22.86)) ;
#113991 = CARTESIAN_POINT('',(2.3,-1.22464679914735E-16,-21.86)) ;
#113992 = CARTESIAN_POINT('Origin',(2.3,-1.10218211923262E-16,-21.96)) ;
#113993 = CARTESIAN_POINT('',(2.3,1.22464679914735E-16,-23.86)) ;
#113994 = CARTESIAN_POINT('Origin',(2.3,0.,-22.86)) ;
#113995 = CARTESIAN_POINT('Origin',(2.3,0.,-22.86)) ;
#113996 = CARTESIAN_POINT('Origin',(1.5,0.,-22.86)) ;
#113997 = CARTESIAN_POINT('',(1.4,-1.34711147906209E-16,-23.96)) ;
#113998 = CARTESIAN_POINT('Origin',(1.4,0.,-22.86)) ;
#113999 = CARTESIAN_POINT('',(1.5,-1.22464679914735E-16,-23.86)) ;
#114000 = CARTESIAN_POINT('Origin',(1.5,-1.34711147906209E-16,-23.96)) ;
#114001 = CARTESIAN_POINT('Origin',(1.5,0.,-22.86)) ;
#114002 = CARTESIAN_POINT('Origin',(1.5,3.15,-21.6014213562373)) ;
#114003 = CARTESIAN_POINT('',(1.5,3.07928932188135,-21.5307106781187)) ;
#114004 = CARTESIAN_POINT('',(1.5,3.25,-21.6014213562373)) ;
#114005 = CARTESIAN_POINT('Origin',(1.5,3.15,-21.6014213562373)) ;
#114006 = CARTESIAN_POINT('',(1.4,3.15,-21.6014213562373)) ;
#114007 = CARTESIAN_POINT('Origin',(1.5,3.15,-21.6014213562373)) ;
#114008 = CARTESIAN_POINT('Origin',(1.5,3.15,-21.6014213562373)) ;
#114009 = CARTESIAN_POINT('Origin',(0.500000000000001,-4.56640444411542E-17,
-23.26)) ;
#114010 = CARTESIAN_POINT('',(0.600000000000001,0.4,-23.26)) ;
#114011 = CARTESIAN_POINT('',(0.595612997216081,0.370705721320403,-23.2307057213204)) ;
#114012 = CARTESIAN_POINT('Origin',(0.50000000005309,0.399999999992667,-23.2599999999926)) ;
#114013 = CARTESIAN_POINT('',(0.500000000000001,0.4,-23.36)) ;
#114014 = CARTESIAN_POINT('Origin',(0.500000000000001,0.4,-23.26)) ;
#114015 = CARTESIAN_POINT('',(0.500000000000001,-1.9,-23.36)) ;
#114016 = CARTESIAN_POINT('',(0.500000000000001,0.5,-23.36)) ;
#114017 = CARTESIAN_POINT('',(0.600000000000001,-1.9,-23.26)) ;
#114018 = CARTESIAN_POINT('Origin',(0.500000000000001,-1.9,-23.26)) ;
#114019 = CARTESIAN_POINT('',(0.600000000000001,-0.3,-23.26)) ;
#114020 = CARTESIAN_POINT('',(0.600000000000001,-2.39800009914441E-17,-23.26)) ;
#114021 = CARTESIAN_POINT('',(0.600000000000001,0.299999999999999,-23.26)) ;
#114022 = CARTESIAN_POINT('',(0.600000000000001,-2.39800009914441E-17,-23.26)) ;
#114023 = CARTESIAN_POINT('Ctrl Pts',(0.600000000000001,0.300000000000003,
-23.26)) ;
#114024 = CARTESIAN_POINT('Ctrl Pts',(0.600000000000001,0.312243016306061,
-23.26)) ;
#114025 = CARTESIAN_POINT('Ctrl Pts',(0.600069747422976,0.324350425899477,
-23.2577515285215)) ;
#114026 = CARTESIAN_POINT('Ctrl Pts',(0.599517124288211,0.346196969297576,
-23.2493954490602)) ;
#114027 = CARTESIAN_POINT('Ctrl Pts',(0.598927484301166,0.35585782537339,
-23.2436750447229)) ;
#114028 = CARTESIAN_POINT('Ctrl Pts',(0.596766673872565,0.36653901230802,
-23.2347023851096)) ;
#114029 = CARTESIAN_POINT('Ctrl Pts',(0.596235629104145,0.368676603883157,
-23.2327379168092)) ;
#114030 = CARTESIAN_POINT('Ctrl Pts',(0.595612997216081,0.370705721320404,
-23.2307057213204)) ;
#114031 = CARTESIAN_POINT('Origin',(2.3,0.,-19.05)) ;
#114032 = CARTESIAN_POINT('',(2.4,-1.10218211923262E-16,-18.15)) ;
#114033 = CARTESIAN_POINT('Origin',(2.4,0.,-19.05)) ;
#114034 = CARTESIAN_POINT('',(2.3,-1.22464679914735E-16,-18.05)) ;
#114035 = CARTESIAN_POINT('Origin',(2.3,-1.10218211923262E-16,-18.15)) ;
#114036 = CARTESIAN_POINT('',(2.3,1.22464679914735E-16,-20.05)) ;
#114037 = CARTESIAN_POINT('Origin',(2.3,0.,-19.05)) ;
#114038 = CARTESIAN_POINT('Origin',(2.3,0.,-19.05)) ;
#114039 = CARTESIAN_POINT('Origin',(1.5,0.,-19.05)) ;
#114040 = CARTESIAN_POINT('',(1.4,-1.34711147906209E-16,-20.15)) ;
#114041 = CARTESIAN_POINT('Origin',(1.4,0.,-19.05)) ;
#114042 = CARTESIAN_POINT('',(1.5,-1.22464679914735E-16,-20.05)) ;
#114043 = CARTESIAN_POINT('Origin',(1.5,-1.34711147906209E-16,-20.15)) ;
#114044 = CARTESIAN_POINT('Origin',(1.5,0.,-19.05)) ;
#114045 = CARTESIAN_POINT('Origin',(1.5,3.15,-17.7914213562373)) ;
#114046 = CARTESIAN_POINT('',(1.5,3.07928932188135,-17.7207106781187)) ;
#114047 = CARTESIAN_POINT('',(1.5,3.25,-17.7914213562373)) ;
#114048 = CARTESIAN_POINT('Origin',(1.5,3.15,-17.7914213562373)) ;
#114049 = CARTESIAN_POINT('',(1.4,3.15,-17.7914213562373)) ;
#114050 = CARTESIAN_POINT('Origin',(1.5,3.15,-17.7914213562373)) ;
#114051 = CARTESIAN_POINT('Origin',(1.5,3.15,-17.7914213562373)) ;
#114052 = CARTESIAN_POINT('Origin',(0.500000000000001,-4.56640444411542E-17,
-19.45)) ;
#114053 = CARTESIAN_POINT('',(0.600000000000001,0.4,-19.45)) ;
#114054 = CARTESIAN_POINT('',(0.595612997216081,0.370705721320403,-19.4207057213204)) ;
#114055 = CARTESIAN_POINT('Origin',(0.500000000041676,0.399999999994165,-19.4499999999941)) ;
#114056 = CARTESIAN_POINT('',(0.500000000000001,0.4,-19.55)) ;
#114057 = CARTESIAN_POINT('Origin',(0.500000000000001,0.4,-19.45)) ;
#114058 = CARTESIAN_POINT('',(0.500000000000001,-1.9,-19.55)) ;
#114059 = CARTESIAN_POINT('',(0.500000000000001,0.5,-19.55)) ;
#114060 = CARTESIAN_POINT('',(0.600000000000001,-1.9,-19.45)) ;
#114061 = CARTESIAN_POINT('Origin',(0.500000000000001,-1.9,-19.45)) ;
#114062 = CARTESIAN_POINT('',(0.600000000000001,-0.3,-19.45)) ;
#114063 = CARTESIAN_POINT('',(0.600000000000001,-2.39800009914441E-17,-19.45)) ;
#114064 = CARTESIAN_POINT('',(0.600000000000001,0.299999999999999,-19.45)) ;
#114065 = CARTESIAN_POINT('',(0.600000000000001,-2.39800009914441E-17,-19.45)) ;
#114066 = CARTESIAN_POINT('Ctrl Pts',(0.600000000000001,0.300000000000003,
-19.45)) ;
#114067 = CARTESIAN_POINT('Ctrl Pts',(0.600000000000001,0.312243016306433,
-19.45)) ;
#114068 = CARTESIAN_POINT('Ctrl Pts',(0.600069747422966,0.324350425899823,
-19.4477515285214)) ;
#114069 = CARTESIAN_POINT('Ctrl Pts',(0.599517124288202,0.346196969297921,
-19.43939544906)) ;
#114070 = CARTESIAN_POINT('Ctrl Pts',(0.598927484301112,0.355857825373661,
-19.4336750447226)) ;
#114071 = CARTESIAN_POINT('Ctrl Pts',(0.596766673872561,0.366539012308041,
-19.4247023851096)) ;
#114072 = CARTESIAN_POINT('Ctrl Pts',(0.596235629104139,0.368676603883175,
-19.4227379168092)) ;
#114073 = CARTESIAN_POINT('Ctrl Pts',(0.595612997216081,0.370705721320404,
-19.4207057213204)) ;
#114074 = CARTESIAN_POINT('Origin',(2.3,0.,-15.24)) ;
#114075 = CARTESIAN_POINT('',(2.4,-1.10218211923262E-16,-14.34)) ;
#114076 = CARTESIAN_POINT('Origin',(2.4,0.,-15.24)) ;
#114077 = CARTESIAN_POINT('',(2.3,-1.22464679914735E-16,-14.24)) ;
#114078 = CARTESIAN_POINT('Origin',(2.3,-1.10218211923262E-16,-14.34)) ;
#114079 = CARTESIAN_POINT('',(2.3,1.22464679914735E-16,-16.24)) ;
#114080 = CARTESIAN_POINT('Origin',(2.3,0.,-15.24)) ;
#114081 = CARTESIAN_POINT('Origin',(2.3,0.,-15.24)) ;
#114082 = CARTESIAN_POINT('Origin',(1.5,0.,-15.24)) ;
#114083 = CARTESIAN_POINT('',(1.4,-1.34711147906209E-16,-16.34)) ;
#114084 = CARTESIAN_POINT('Origin',(1.4,0.,-15.24)) ;
#114085 = CARTESIAN_POINT('',(1.5,-1.22464679914735E-16,-16.24)) ;
#114086 = CARTESIAN_POINT('Origin',(1.5,-1.34711147906209E-16,-16.34)) ;
#114087 = CARTESIAN_POINT('Origin',(1.5,0.,-15.24)) ;
#114088 = CARTESIAN_POINT('Origin',(1.5,3.15,-13.9814213562373)) ;
#114089 = CARTESIAN_POINT('',(1.5,3.07928932188135,-13.9107106781187)) ;
#114090 = CARTESIAN_POINT('',(1.5,3.25,-13.9814213562373)) ;
#114091 = CARTESIAN_POINT('Origin',(1.5,3.15,-13.9814213562373)) ;
#114092 = CARTESIAN_POINT('',(1.4,3.15,-13.9814213562373)) ;
#114093 = CARTESIAN_POINT('Origin',(1.5,3.15,-13.9814213562373)) ;
#114094 = CARTESIAN_POINT('Origin',(1.5,3.15,-13.9814213562373)) ;
#114095 = CARTESIAN_POINT('Origin',(0.500000000000001,-4.56640444411542E-17,
-15.64)) ;
#114096 = CARTESIAN_POINT('',(0.600000000000001,0.4,-15.64)) ;
#114097 = CARTESIAN_POINT('',(0.595612997216081,0.370705721320403,-15.6107057213204)) ;
#114098 = CARTESIAN_POINT('Origin',(0.499999999962138,0.400000000005185,-15.6400000000051)) ;
#114099 = CARTESIAN_POINT('',(0.500000000000001,0.4,-15.74)) ;
#114100 = CARTESIAN_POINT('Origin',(0.500000000000001,0.4,-15.64)) ;
#114101 = CARTESIAN_POINT('',(0.500000000000001,-1.9,-15.74)) ;
#114102 = CARTESIAN_POINT('',(0.500000000000001,0.5,-15.74)) ;
#114103 = CARTESIAN_POINT('',(0.600000000000001,-1.9,-15.64)) ;
#114104 = CARTESIAN_POINT('Origin',(0.500000000000001,-1.9,-15.64)) ;
#114105 = CARTESIAN_POINT('',(0.600000000000001,-0.3,-15.64)) ;
#114106 = CARTESIAN_POINT('',(0.600000000000001,-2.39800009914441E-17,-15.64)) ;
#114107 = CARTESIAN_POINT('',(0.600000000000001,0.299999999999999,-15.64)) ;
#114108 = CARTESIAN_POINT('',(0.600000000000001,-2.39800009914441E-17,-15.64)) ;
#114109 = CARTESIAN_POINT('Ctrl Pts',(0.600000000000001,0.300000000000003,
-15.64)) ;
#114110 = CARTESIAN_POINT('Ctrl Pts',(0.600000000000001,0.312243016306305,
-15.64)) ;
#114111 = CARTESIAN_POINT('Ctrl Pts',(0.60006974742297,0.324350425899701,
-15.6377515285214)) ;
#114112 = CARTESIAN_POINT('Ctrl Pts',(0.599517124288205,0.346196969297796,
-15.6293954490601)) ;
#114113 = CARTESIAN_POINT('Ctrl Pts',(0.59892748430113,0.355857825373563,
-15.6236750447227)) ;
#114114 = CARTESIAN_POINT('Ctrl Pts',(0.596766673872562,0.366539012308031,
-15.6147023851096)) ;
#114115 = CARTESIAN_POINT('Ctrl Pts',(0.596235629104141,0.368676603883168,
-15.6127379168092)) ;
#114116 = CARTESIAN_POINT('Ctrl Pts',(0.59561299721608,0.370705721320404,
-15.6107057213204)) ;
#114117 = CARTESIAN_POINT('Origin',(2.3,0.,-11.43)) ;
#114118 = CARTESIAN_POINT('',(2.4,-1.10218211923262E-16,-10.53)) ;
#114119 = CARTESIAN_POINT('Origin',(2.4,0.,-11.43)) ;
#114120 = CARTESIAN_POINT('',(2.3,-1.22464679914735E-16,-10.43)) ;
#114121 = CARTESIAN_POINT('Origin',(2.3,-1.10218211923262E-16,-10.53)) ;
#114122 = CARTESIAN_POINT('',(2.3,1.22464679914735E-16,-12.43)) ;
#114123 = CARTESIAN_POINT('Origin',(2.3,0.,-11.43)) ;
#114124 = CARTESIAN_POINT('Origin',(2.3,0.,-11.43)) ;
#114125 = CARTESIAN_POINT('Origin',(1.5,0.,-11.43)) ;
#114126 = CARTESIAN_POINT('',(1.4,-1.34711147906209E-16,-12.53)) ;
#114127 = CARTESIAN_POINT('Origin',(1.4,0.,-11.43)) ;
#114128 = CARTESIAN_POINT('',(1.5,-1.22464679914735E-16,-12.43)) ;
#114129 = CARTESIAN_POINT('Origin',(1.5,-1.34711147906209E-16,-12.53)) ;
#114130 = CARTESIAN_POINT('Origin',(1.5,0.,-11.43)) ;
#114131 = CARTESIAN_POINT('Origin',(1.5,3.15,-10.1714213562373)) ;
#114132 = CARTESIAN_POINT('',(1.5,3.07928932188135,-10.1007106781187)) ;
#114133 = CARTESIAN_POINT('',(1.5,3.25,-10.1714213562373)) ;
#114134 = CARTESIAN_POINT('Origin',(1.5,3.15,-10.1714213562373)) ;
#114135 = CARTESIAN_POINT('',(1.4,3.15,-10.1714213562373)) ;
#114136 = CARTESIAN_POINT('Origin',(1.5,3.15,-10.1714213562373)) ;
#114137 = CARTESIAN_POINT('Origin',(1.5,3.15,-10.1714213562373)) ;
#114138 = CARTESIAN_POINT('Origin',(0.500000000000001,-4.56640444411542E-17,
-11.83)) ;
#114139 = CARTESIAN_POINT('',(0.600000000000001,0.4,-11.83)) ;
#114140 = CARTESIAN_POINT('',(0.59561299721608,0.370705721320402,-11.8007057213204)) ;
#114141 = CARTESIAN_POINT('Origin',(0.500000000002749,0.399999999999878,-11.8299999999996)) ;
#114142 = CARTESIAN_POINT('',(0.500000000000001,0.4,-11.93)) ;
#114143 = CARTESIAN_POINT('Origin',(0.500000000000001,0.4,-11.83)) ;
#114144 = CARTESIAN_POINT('',(0.500000000000001,-1.9,-11.93)) ;
#114145 = CARTESIAN_POINT('',(0.500000000000001,0.5,-11.93)) ;
#114146 = CARTESIAN_POINT('',(0.600000000000001,-1.9,-11.83)) ;
#114147 = CARTESIAN_POINT('Origin',(0.500000000000001,-1.9,-11.83)) ;
#114148 = CARTESIAN_POINT('',(0.600000000000001,-0.3,-11.83)) ;
#114149 = CARTESIAN_POINT('',(0.600000000000001,-2.39800009914441E-17,-11.83)) ;
#114150 = CARTESIAN_POINT('',(0.600000000000001,0.299999999999999,-11.83)) ;
#114151 = CARTESIAN_POINT('',(0.600000000000001,-2.39800009914441E-17,-11.83)) ;
#114152 = CARTESIAN_POINT('Ctrl Pts',(0.600000000000001,0.300000000000003,
-11.83)) ;
#114153 = CARTESIAN_POINT('Ctrl Pts',(0.600000000000001,0.312243016306181,
-11.83)) ;
#114154 = CARTESIAN_POINT('Ctrl Pts',(0.600069747422973,0.324350425899585,
-11.8277515285214)) ;
#114155 = CARTESIAN_POINT('Ctrl Pts',(0.599517124288208,0.346196969297684,
-11.8193954490601)) ;
#114156 = CARTESIAN_POINT('Ctrl Pts',(0.598927484301148,0.355857825373472,
-11.8136750447228)) ;
#114157 = CARTESIAN_POINT('Ctrl Pts',(0.596766673872564,0.366539012308024,
-11.8047023851096)) ;
#114158 = CARTESIAN_POINT('Ctrl Pts',(0.596235629104143,0.368676603883159,
-11.8027379168092)) ;
#114159 = CARTESIAN_POINT('Ctrl Pts',(0.595612997216081,0.370705721320402,
-11.8007057213204)) ;
#114160 = CARTESIAN_POINT('Origin',(2.3,0.,-7.62)) ;
#114161 = CARTESIAN_POINT('',(2.4,-1.10218211923262E-16,-6.72)) ;
#114162 = CARTESIAN_POINT('Origin',(2.4,0.,-7.62)) ;
#114163 = CARTESIAN_POINT('',(2.3,-1.22464679914735E-16,-6.62)) ;
#114164 = CARTESIAN_POINT('Origin',(2.3,-1.10218211923262E-16,-6.72)) ;
#114165 = CARTESIAN_POINT('',(2.3,1.22464679914735E-16,-8.62)) ;
#114166 = CARTESIAN_POINT('Origin',(2.3,0.,-7.62)) ;
#114167 = CARTESIAN_POINT('Origin',(2.3,0.,-7.62)) ;
#114168 = CARTESIAN_POINT('Origin',(1.5,0.,-7.62)) ;
#114169 = CARTESIAN_POINT('',(1.4,-1.34711147906209E-16,-8.72)) ;
#114170 = CARTESIAN_POINT('Origin',(1.4,0.,-7.62)) ;
#114171 = CARTESIAN_POINT('',(1.5,-1.22464679914735E-16,-8.62)) ;
#114172 = CARTESIAN_POINT('Origin',(1.5,-1.34711147906209E-16,-8.72)) ;
#114173 = CARTESIAN_POINT('Origin',(1.5,0.,-7.62)) ;
#114174 = CARTESIAN_POINT('Origin',(1.5,3.15,-6.36142135623731)) ;
#114175 = CARTESIAN_POINT('',(1.5,3.07928932188135,-6.29071067811866)) ;
#114176 = CARTESIAN_POINT('',(1.5,3.25,-6.36142135623731)) ;
#114177 = CARTESIAN_POINT('Origin',(1.5,3.15,-6.36142135623731)) ;
#114178 = CARTESIAN_POINT('',(1.4,3.15,-6.36142135623731)) ;
#114179 = CARTESIAN_POINT('Origin',(1.5,3.15,-6.36142135623731)) ;
#114180 = CARTESIAN_POINT('Origin',(1.5,3.15,-6.36142135623731)) ;
#114181 = CARTESIAN_POINT('Origin',(0.500000000000001,-4.56640444411542E-17,
-8.02)) ;
#114182 = CARTESIAN_POINT('',(0.600000000000001,0.4,-8.02)) ;
#114183 = CARTESIAN_POINT('',(0.59561299721608,0.370705721320402,-7.9907057213204)) ;
#114184 = CARTESIAN_POINT('Origin',(0.499999999996157,0.400000000000788,-8.02000000000056)) ;
#114185 = CARTESIAN_POINT('',(0.500000000000001,0.4,-8.12)) ;
#114186 = CARTESIAN_POINT('Origin',(0.500000000000001,0.4,-8.02)) ;
#114187 = CARTESIAN_POINT('',(0.500000000000001,-1.9,-8.12)) ;
#114188 = CARTESIAN_POINT('',(0.500000000000001,0.5,-8.12)) ;
#114189 = CARTESIAN_POINT('',(0.600000000000001,-1.9,-8.02)) ;
#114190 = CARTESIAN_POINT('Origin',(0.500000000000001,-1.9,-8.02)) ;
#114191 = CARTESIAN_POINT('',(0.600000000000001,-0.3,-8.02)) ;
#114192 = CARTESIAN_POINT('',(0.600000000000001,-2.39800009914441E-17,-8.02)) ;
#114193 = CARTESIAN_POINT('',(0.600000000000001,0.299999999999999,-8.02)) ;
#114194 = CARTESIAN_POINT('',(0.600000000000001,-2.39800009914441E-17,-8.02)) ;
#114195 = CARTESIAN_POINT('Ctrl Pts',(0.600000000000001,0.300000000000003,
-8.02)) ;
#114196 = CARTESIAN_POINT('Ctrl Pts',(0.600000000000001,0.312243016306057,
-8.02)) ;
#114197 = CARTESIAN_POINT('Ctrl Pts',(0.600069747422976,0.32435042589947,
-8.01775152852148)) ;
#114198 = CARTESIAN_POINT('Ctrl Pts',(0.599517124288211,0.346196969297575,
-8.00939544906016)) ;
#114199 = CARTESIAN_POINT('Ctrl Pts',(0.598927484301167,0.355857825373384,
-8.00367504472285)) ;
#114200 = CARTESIAN_POINT('Ctrl Pts',(0.596766673872565,0.366539012308017,
-7.99470238510958)) ;
#114201 = CARTESIAN_POINT('Ctrl Pts',(0.596235629104145,0.368676603883154,
-7.9927379168092)) ;
#114202 = CARTESIAN_POINT('Ctrl Pts',(0.59561299721608,0.370705721320404,
-7.9907057213204)) ;
#114203 = CARTESIAN_POINT('Origin',(2.3,0.,-3.81)) ;
#114204 = CARTESIAN_POINT('',(2.4,-1.10218211923262E-16,-2.91)) ;
#114205 = CARTESIAN_POINT('Origin',(2.4,0.,-3.81)) ;
#114206 = CARTESIAN_POINT('',(2.3,-1.22464679914735E-16,-2.81)) ;
#114207 = CARTESIAN_POINT('Origin',(2.3,-1.10218211923262E-16,-2.91)) ;
#114208 = CARTESIAN_POINT('',(2.3,1.22464679914735E-16,-4.81)) ;
#114209 = CARTESIAN_POINT('Origin',(2.3,0.,-3.81)) ;
#114210 = CARTESIAN_POINT('Origin',(2.3,0.,-3.81)) ;
#114211 = CARTESIAN_POINT('Origin',(7.9,3.15,-5.06857864376269)) ;
#114212 = CARTESIAN_POINT('',(8.,3.35,-5.06857864376269)) ;
#114213 = CARTESIAN_POINT('',(8.,3.00857864376269,-5.21)) ;
#114214 = CARTESIAN_POINT('Origin',(8.,3.15,-5.06857864376269)) ;
#114215 = CARTESIAN_POINT('',(7.9,3.25,-5.06857864376269)) ;
#114216 = CARTESIAN_POINT('Origin',(7.9,3.35,-5.06857864376269)) ;
#114217 = CARTESIAN_POINT('',(7.9,3.07928932188135,-5.13928932188135)) ;
#114218 = CARTESIAN_POINT('Origin',(7.9,3.15,-5.06857864376269)) ;
#114219 = CARTESIAN_POINT('Origin',(7.9,3.00857864376269,-5.21)) ;
#114220 = CARTESIAN_POINT('Origin',(7.9,3.15,-8.87857864376269)) ;
#114221 = CARTESIAN_POINT('',(8.,3.35,-8.87857864376269)) ;
#114222 = CARTESIAN_POINT('',(8.,3.00857864376269,-9.02)) ;
#114223 = CARTESIAN_POINT('Origin',(8.,3.15,-8.87857864376269)) ;
#114224 = CARTESIAN_POINT('',(7.9,3.25,-8.87857864376269)) ;
#114225 = CARTESIAN_POINT('Origin',(7.9,3.35,-8.87857864376269)) ;
#114226 = CARTESIAN_POINT('',(7.9,3.07928932188135,-8.94928932188134)) ;
#114227 = CARTESIAN_POINT('Origin',(7.9,3.15,-8.87857864376269)) ;
#114228 = CARTESIAN_POINT('Origin',(7.9,3.00857864376269,-9.02)) ;
#114229 = CARTESIAN_POINT('Origin',(7.9,3.15,-12.6885786437627)) ;
#114230 = CARTESIAN_POINT('',(8.,3.35,-12.6885786437627)) ;
#114231 = CARTESIAN_POINT('',(8.,3.00857864376269,-12.83)) ;
#114232 = CARTESIAN_POINT('Origin',(8.,3.15,-12.6885786437627)) ;
#114233 = CARTESIAN_POINT('',(7.9,3.25,-12.6885786437627)) ;
#114234 = CARTESIAN_POINT('Origin',(7.9,3.35,-12.6885786437627)) ;
#114235 = CARTESIAN_POINT('',(7.9,3.07928932188135,-12.7592893218813)) ;
#114236 = CARTESIAN_POINT('Origin',(7.9,3.15,-12.6885786437627)) ;
#114237 = CARTESIAN_POINT('Origin',(7.9,3.00857864376269,-12.83)) ;
#114238 = CARTESIAN_POINT('Origin',(7.9,3.15,-16.4985786437627)) ;
#114239 = CARTESIAN_POINT('',(8.,3.35,-16.4985786437627)) ;
#114240 = CARTESIAN_POINT('',(8.,3.00857864376269,-16.64)) ;
#114241 = CARTESIAN_POINT('Origin',(8.,3.15,-16.4985786437627)) ;
#114242 = CARTESIAN_POINT('',(7.9,3.25,-16.4985786437627)) ;
#114243 = CARTESIAN_POINT('Origin',(7.9,3.35,-16.4985786437627)) ;
#114244 = CARTESIAN_POINT('',(7.9,3.07928932188135,-16.5692893218813)) ;
#114245 = CARTESIAN_POINT('Origin',(7.9,3.15,-16.4985786437627)) ;
#114246 = CARTESIAN_POINT('Origin',(7.9,3.00857864376269,-16.64)) ;
#114247 = CARTESIAN_POINT('Origin',(7.9,3.15,-20.3085786437627)) ;
#114248 = CARTESIAN_POINT('',(8.,3.35,-20.3085786437627)) ;
#114249 = CARTESIAN_POINT('',(8.,3.00857864376269,-20.45)) ;
#114250 = CARTESIAN_POINT('Origin',(8.,3.15,-20.3085786437627)) ;
#114251 = CARTESIAN_POINT('',(7.9,3.25,-20.3085786437627)) ;
#114252 = CARTESIAN_POINT('Origin',(7.9,3.35,-20.3085786437627)) ;
#114253 = CARTESIAN_POINT('',(7.9,3.07928932188135,-20.3792893218813)) ;
#114254 = CARTESIAN_POINT('Origin',(7.9,3.15,-20.3085786437627)) ;
#114255 = CARTESIAN_POINT('Origin',(7.9,3.00857864376269,-20.45)) ;
#114256 = CARTESIAN_POINT('Origin',(7.9,3.15,-24.1185786437627)) ;
#114257 = CARTESIAN_POINT('',(8.,3.35,-24.1185786437627)) ;
#114258 = CARTESIAN_POINT('',(8.,3.00857864376269,-24.26)) ;
#114259 = CARTESIAN_POINT('Origin',(8.,3.15,-24.1185786437627)) ;
#114260 = CARTESIAN_POINT('',(7.9,3.25,-24.1185786437627)) ;
#114261 = CARTESIAN_POINT('Origin',(7.9,3.35,-24.1185786437627)) ;
#114262 = CARTESIAN_POINT('',(7.9,3.07928932188135,-24.1892893218813)) ;
#114263 = CARTESIAN_POINT('Origin',(7.9,3.15,-24.1185786437627)) ;
#114264 = CARTESIAN_POINT('Origin',(7.9,3.00857864376269,-24.26)) ;
#114265 = CARTESIAN_POINT('Origin',(7.9,3.15,-27.9285786437627)) ;
#114266 = CARTESIAN_POINT('',(8.,3.35,-27.9285786437627)) ;
#114267 = CARTESIAN_POINT('',(8.,3.00857864376269,-28.07)) ;
#114268 = CARTESIAN_POINT('Origin',(8.,3.15,-27.9285786437627)) ;
#114269 = CARTESIAN_POINT('',(7.9,3.25,-27.9285786437627)) ;
#114270 = CARTESIAN_POINT('Origin',(7.9,3.35,-27.9285786437627)) ;
#114271 = CARTESIAN_POINT('',(7.9,3.07928932188135,-27.9992893218813)) ;
#114272 = CARTESIAN_POINT('Origin',(7.9,3.15,-27.9285786437627)) ;
#114273 = CARTESIAN_POINT('Origin',(7.9,3.00857864376269,-28.07)) ;
#114274 = CARTESIAN_POINT('Origin',(7.9,3.15,-31.7385786437627)) ;
#114275 = CARTESIAN_POINT('',(8.,3.35,-31.7385786437627)) ;
#114276 = CARTESIAN_POINT('',(8.,3.00857864376269,-31.88)) ;
#114277 = CARTESIAN_POINT('Origin',(8.,3.15,-31.7385786437627)) ;
#114278 = CARTESIAN_POINT('',(7.9,3.25,-31.7385786437627)) ;
#114279 = CARTESIAN_POINT('Origin',(7.9,3.35,-31.7385786437627)) ;
#114280 = CARTESIAN_POINT('',(7.9,3.07928932188135,-31.8092893218813)) ;
#114281 = CARTESIAN_POINT('Origin',(7.9,3.15,-31.7385786437627)) ;
#114282 = CARTESIAN_POINT('Origin',(7.9,3.00857864376269,-31.88)) ;
#114283 = CARTESIAN_POINT('Origin',(7.9,3.15,-35.5485786437627)) ;
#114284 = CARTESIAN_POINT('',(8.,3.35,-35.5485786437627)) ;
#114285 = CARTESIAN_POINT('',(8.,3.00857864376269,-35.69)) ;
#114286 = CARTESIAN_POINT('Origin',(8.,3.15,-35.5485786437627)) ;
#114287 = CARTESIAN_POINT('',(7.9,3.25,-35.5485786437627)) ;
#114288 = CARTESIAN_POINT('Origin',(7.9,3.35,-35.5485786437627)) ;
#114289 = CARTESIAN_POINT('',(7.9,3.07928932188135,-35.6192893218813)) ;
#114290 = CARTESIAN_POINT('Origin',(7.9,3.15,-35.5485786437627)) ;
#114291 = CARTESIAN_POINT('Origin',(7.9,3.00857864376269,-35.69)) ;
#114292 = CARTESIAN_POINT('Origin',(1.5,0.,-3.81)) ;
#114293 = CARTESIAN_POINT('',(1.4,-1.34711147906209E-16,-4.91)) ;
#114294 = CARTESIAN_POINT('Origin',(1.4,0.,-3.81)) ;
#114295 = CARTESIAN_POINT('',(1.5,-1.22464679914735E-16,-4.81)) ;
#114296 = CARTESIAN_POINT('Origin',(1.5,-1.34711147906209E-16,-4.91)) ;
#114297 = CARTESIAN_POINT('Origin',(1.5,0.,-3.81)) ;
#114298 = CARTESIAN_POINT('Origin',(1.5,3.15,-2.55142135623731)) ;
#114299 = CARTESIAN_POINT('',(1.5,3.07928932188135,-2.48071067811865)) ;
#114300 = CARTESIAN_POINT('',(1.5,3.25,-2.55142135623731)) ;
#114301 = CARTESIAN_POINT('Origin',(1.5,3.15,-2.55142135623731)) ;
#114302 = CARTESIAN_POINT('',(1.4,3.15,-2.55142135623731)) ;
#114303 = CARTESIAN_POINT('Origin',(1.5,3.15,-2.55142135623731)) ;
#114304 = CARTESIAN_POINT('Origin',(1.5,3.15,-2.55142135623731)) ;
#114305 = CARTESIAN_POINT('Origin',(0.500000000000001,-4.56640444411539E-17,
-4.21)) ;
#114306 = CARTESIAN_POINT('',(0.600000000000001,0.4,-4.21)) ;
#114307 = CARTESIAN_POINT('',(0.595612997216081,0.370705721320403,-4.1807057213204)) ;
#114308 = CARTESIAN_POINT('Origin',(0.499999999992608,0.400000000001211,-4.21000000000122)) ;
#114309 = CARTESIAN_POINT('',(0.500000000000001,0.4,-4.31)) ;
#114310 = CARTESIAN_POINT('Origin',(0.500000000000001,0.4,-4.21)) ;
#114311 = CARTESIAN_POINT('',(0.500000000000001,-1.9,-4.31)) ;
#114312 = CARTESIAN_POINT('',(0.500000000000001,0.5,-4.31)) ;
#114313 = CARTESIAN_POINT('',(0.600000000000001,-1.9,-4.21)) ;
#114314 = CARTESIAN_POINT('Origin',(0.500000000000001,-1.9,-4.21)) ;
#114315 = CARTESIAN_POINT('',(0.600000000000001,-0.3,-4.21)) ;
#114316 = CARTESIAN_POINT('',(0.600000000000001,-2.39800009914439E-17,-4.21)) ;
#114317 = CARTESIAN_POINT('',(0.600000000000001,0.299999999999999,-4.21)) ;
#114318 = CARTESIAN_POINT('',(0.600000000000001,-2.39800009914439E-17,-4.21)) ;
#114319 = CARTESIAN_POINT('Ctrl Pts',(0.600000000000001,0.300000000000003,
-4.21)) ;
#114320 = CARTESIAN_POINT('Ctrl Pts',(0.600000000000001,0.312243016306119,
-4.21)) ;
#114321 = CARTESIAN_POINT('Ctrl Pts',(0.600069747422974,0.324350425899533,
-4.20775152852146)) ;
#114322 = CARTESIAN_POINT('Ctrl Pts',(0.599517124288209,0.346196969297642,
-4.19939544906013)) ;
#114323 = CARTESIAN_POINT('Ctrl Pts',(0.598927484301157,0.355857825373437,
-4.19367504472281)) ;
#114324 = CARTESIAN_POINT('Ctrl Pts',(0.596766673872564,0.366539012308024,
-4.18470238510957)) ;
#114325 = CARTESIAN_POINT('Ctrl Pts',(0.596235629104143,0.36867660388316,
-4.18273791680919)) ;
#114326 = CARTESIAN_POINT('Ctrl Pts',(0.595612997216081,0.370705721320404,
-4.1807057213204)) ;
#114327 = CARTESIAN_POINT('Origin',(2.4,0.,-34.29)) ;
#114328 = CARTESIAN_POINT('',(2.4,-1.22464679914735E-16,-35.29)) ;
#114329 = CARTESIAN_POINT('Origin',(2.4,0.,-30.48)) ;
#114330 = CARTESIAN_POINT('',(2.4,-1.22464679914735E-16,-31.48)) ;
#114331 = CARTESIAN_POINT('Origin',(2.4,0.,-26.67)) ;
#114332 = CARTESIAN_POINT('',(2.4,-1.22464679914735E-16,-27.67)) ;
#114333 = CARTESIAN_POINT('Origin',(2.4,0.,-22.86)) ;
#114334 = CARTESIAN_POINT('',(2.4,-1.22464679914735E-16,-23.86)) ;
#114335 = CARTESIAN_POINT('Origin',(2.4,0.,-19.05)) ;
#114336 = CARTESIAN_POINT('',(2.4,-1.22464679914735E-16,-20.05)) ;
#114337 = CARTESIAN_POINT('Origin',(2.4,0.,-15.24)) ;
#114338 = CARTESIAN_POINT('',(2.4,-1.22464679914735E-16,-16.24)) ;
#114339 = CARTESIAN_POINT('Origin',(2.4,0.,-11.43)) ;
#114340 = CARTESIAN_POINT('',(2.4,-1.22464679914735E-16,-12.43)) ;
#114341 = CARTESIAN_POINT('Origin',(2.4,0.,-7.62)) ;
#114342 = CARTESIAN_POINT('',(2.4,-1.22464679914735E-16,-8.62)) ;
#114343 = CARTESIAN_POINT('Origin',(2.4,0.,-3.81)) ;
#114344 = CARTESIAN_POINT('',(2.4,-1.22464679914735E-16,-4.81)) ;
#114345 = CARTESIAN_POINT('Origin',(1.4,3.15,-5.06857864376269)) ;
#114346 = CARTESIAN_POINT('',(1.5,3.25,-5.06857864376269)) ;
#114347 = CARTESIAN_POINT('',(1.5,3.07928932188135,-5.13928932188135)) ;
#114348 = CARTESIAN_POINT('Origin',(1.5,3.15,-5.06857864376269)) ;
#114349 = CARTESIAN_POINT('',(1.4,3.07928932188135,-5.13928932188135)) ;
#114350 = CARTESIAN_POINT('',(1.4,3.25,-5.06857864376269)) ;
#114351 = CARTESIAN_POINT('Origin',(1.4,3.15,-8.87857864376269)) ;
#114352 = CARTESIAN_POINT('',(1.5,3.25,-8.87857864376269)) ;
#114353 = CARTESIAN_POINT('',(1.5,3.07928932188135,-8.94928932188134)) ;
#114354 = CARTESIAN_POINT('Origin',(1.5,3.15,-8.87857864376269)) ;
#114355 = CARTESIAN_POINT('',(1.4,3.07928932188135,-8.94928932188134)) ;
#114356 = CARTESIAN_POINT('',(1.4,3.25,-8.87857864376269)) ;
#114357 = CARTESIAN_POINT('Origin',(1.4,3.15,-12.6885786437627)) ;
#114358 = CARTESIAN_POINT('',(1.5,3.25,-12.6885786437627)) ;
#114359 = CARTESIAN_POINT('',(1.5,3.07928932188135,-12.7592893218813)) ;
#114360 = CARTESIAN_POINT('Origin',(1.5,3.15,-12.6885786437627)) ;
#114361 = CARTESIAN_POINT('',(1.4,3.07928932188135,-12.7592893218813)) ;
#114362 = CARTESIAN_POINT('',(1.4,3.25,-12.6885786437627)) ;
#114363 = CARTESIAN_POINT('Origin',(1.4,3.15,-16.4985786437627)) ;
#114364 = CARTESIAN_POINT('',(1.5,3.25,-16.4985786437627)) ;
#114365 = CARTESIAN_POINT('',(1.5,3.07928932188135,-16.5692893218813)) ;
#114366 = CARTESIAN_POINT('Origin',(1.5,3.15,-16.4985786437627)) ;
#114367 = CARTESIAN_POINT('',(1.4,3.07928932188135,-16.5692893218813)) ;
#114368 = CARTESIAN_POINT('',(1.4,3.25,-16.4985786437627)) ;
#114369 = CARTESIAN_POINT('Origin',(1.4,3.15,-20.3085786437627)) ;
#114370 = CARTESIAN_POINT('',(1.5,3.25,-20.3085786437627)) ;
#114371 = CARTESIAN_POINT('',(1.5,3.07928932188135,-20.3792893218813)) ;
#114372 = CARTESIAN_POINT('Origin',(1.5,3.15,-20.3085786437627)) ;
#114373 = CARTESIAN_POINT('',(1.4,3.07928932188135,-20.3792893218813)) ;
#114374 = CARTESIAN_POINT('',(1.4,3.25,-20.3085786437627)) ;
#114375 = CARTESIAN_POINT('Origin',(1.4,3.15,-24.1185786437627)) ;
#114376 = CARTESIAN_POINT('',(1.5,3.25,-24.1185786437627)) ;
#114377 = CARTESIAN_POINT('',(1.5,3.07928932188135,-24.1892893218813)) ;
#114378 = CARTESIAN_POINT('Origin',(1.5,3.15,-24.1185786437627)) ;
#114379 = CARTESIAN_POINT('',(1.4,3.07928932188135,-24.1892893218813)) ;
#114380 = CARTESIAN_POINT('',(1.4,3.25,-24.1185786437627)) ;
#114381 = CARTESIAN_POINT('Origin',(1.4,3.15,-27.9285786437627)) ;
#114382 = CARTESIAN_POINT('',(1.5,3.25,-27.9285786437627)) ;
#114383 = CARTESIAN_POINT('',(1.5,3.07928932188135,-27.9992893218813)) ;
#114384 = CARTESIAN_POINT('Origin',(1.5,3.15,-27.9285786437627)) ;
#114385 = CARTESIAN_POINT('',(1.4,3.07928932188135,-27.9992893218813)) ;
#114386 = CARTESIAN_POINT('',(1.4,3.25,-27.9285786437627)) ;
#114387 = CARTESIAN_POINT('Origin',(1.4,3.15,-31.7385786437627)) ;
#114388 = CARTESIAN_POINT('',(1.5,3.25,-31.7385786437627)) ;
#114389 = CARTESIAN_POINT('',(1.5,3.07928932188135,-31.8092893218813)) ;
#114390 = CARTESIAN_POINT('Origin',(1.5,3.15,-31.7385786437627)) ;
#114391 = CARTESIAN_POINT('',(1.4,3.07928932188135,-31.8092893218813)) ;
#114392 = CARTESIAN_POINT('',(1.4,3.25,-31.7385786437627)) ;
#114393 = CARTESIAN_POINT('Origin',(1.4,3.15,-35.5485786437627)) ;
#114394 = CARTESIAN_POINT('',(1.5,3.25,-35.5485786437627)) ;
#114395 = CARTESIAN_POINT('',(1.5,3.07928932188135,-35.6192893218813)) ;
#114396 = CARTESIAN_POINT('Origin',(1.5,3.15,-35.5485786437627)) ;
#114397 = CARTESIAN_POINT('',(1.4,3.07928932188135,-35.6192893218813)) ;
#114398 = CARTESIAN_POINT('',(1.4,3.25,-35.5485786437627)) ;
#114399 = CARTESIAN_POINT('Origin',(2.3,0.,0.)) ;
#114400 = CARTESIAN_POINT('',(2.4,-1.10218211923262E-16,0.9)) ;
#114401 = CARTESIAN_POINT('Origin',(2.4,0.,0.)) ;
#114402 = CARTESIAN_POINT('',(2.3,-1.22464679914735E-16,1.)) ;
#114403 = CARTESIAN_POINT('Origin',(2.3,-1.10218211923262E-16,0.9)) ;
#114404 = CARTESIAN_POINT('',(2.3,1.22464679914735E-16,-1.)) ;
#114405 = CARTESIAN_POINT('Origin',(2.3,0.,0.)) ;
#114406 = CARTESIAN_POINT('Origin',(2.3,0.,0.)) ;
#114407 = CARTESIAN_POINT('Origin',(7.9,3.15,-1.25857864376269)) ;
#114408 = CARTESIAN_POINT('',(8.,3.35,-1.25857864376269)) ;
#114409 = CARTESIAN_POINT('',(8.,3.00857864376269,-1.4)) ;
#114410 = CARTESIAN_POINT('Origin',(8.,3.15,-1.25857864376269)) ;
#114411 = CARTESIAN_POINT('',(7.9,3.25,-1.25857864376269)) ;
#114412 = CARTESIAN_POINT('Origin',(7.9,3.35,-1.25857864376269)) ;
#114413 = CARTESIAN_POINT('',(7.9,3.07928932188135,-1.32928932188135)) ;
#114414 = CARTESIAN_POINT('Origin',(7.9,3.15,-1.25857864376269)) ;
#114415 = CARTESIAN_POINT('Origin',(7.9,3.00857864376269,-1.4)) ;
#114416 = CARTESIAN_POINT('Origin',(1.5,0.,0.)) ;
#114417 = CARTESIAN_POINT('',(1.4,-1.34711147906209E-16,-1.1)) ;
#114418 = CARTESIAN_POINT('Origin',(1.4,0.,0.)) ;
#114419 = CARTESIAN_POINT('',(1.5,-1.22464679914735E-16,-1.)) ;
#114420 = CARTESIAN_POINT('Origin',(1.5,-1.34711147906209E-16,-1.1)) ;
#114421 = CARTESIAN_POINT('Origin',(1.5,0.,0.)) ;
#114422 = CARTESIAN_POINT('Origin',(1.5,3.15,1.25857864376269)) ;
#114423 = CARTESIAN_POINT('',(1.5,3.07928932188135,1.32928932188135)) ;
#114424 = CARTESIAN_POINT('',(1.5,3.25,1.25857864376269)) ;
#114425 = CARTESIAN_POINT('Origin',(1.5,3.15,1.25857864376269)) ;
#114426 = CARTESIAN_POINT('',(1.4,3.15,1.25857864376269)) ;
#114427 = CARTESIAN_POINT('Origin',(1.5,3.15,1.25857864376269)) ;
#114428 = CARTESIAN_POINT('Origin',(1.5,3.15,1.25857864376269)) ;
#114429 = CARTESIAN_POINT('Origin',(0.500000000000001,-4.5664044441154E-17,
-0.4)) ;
#114430 = CARTESIAN_POINT('',(0.600000000000001,0.4,-0.4)) ;
#114431 = CARTESIAN_POINT('',(0.595612997216081,0.370705721320403,-0.370705721320403)) ;
#114432 = CARTESIAN_POINT('Origin',(0.499999999989667,0.400000000001553,-0.400000000001553)) ;
#114433 = CARTESIAN_POINT('',(0.500000000000001,0.4,-0.5)) ;
#114434 = CARTESIAN_POINT('Origin',(0.500000000000001,0.4,-0.4)) ;
#114435 = CARTESIAN_POINT('',(0.500000000000001,-1.9,-0.5)) ;
#114436 = CARTESIAN_POINT('',(0.500000000000001,0.5,-0.5)) ;
#114437 = CARTESIAN_POINT('',(0.600000000000001,-1.9,-0.4)) ;
#114438 = CARTESIAN_POINT('Origin',(0.500000000000001,-1.9,-0.4)) ;
#114439 = CARTESIAN_POINT('',(0.600000000000001,-0.3,-0.4)) ;
#114440 = CARTESIAN_POINT('',(0.600000000000001,-2.3980000991444E-17,-0.4)) ;
#114441 = CARTESIAN_POINT('',(0.600000000000001,0.299999999999999,-0.4)) ;
#114442 = CARTESIAN_POINT('',(0.600000000000001,-2.3980000991444E-17,-0.4)) ;
#114443 = CARTESIAN_POINT('Ctrl Pts',(0.600000000000001,0.300000000000003,
-0.4)) ;
#114444 = CARTESIAN_POINT('Ctrl Pts',(0.600000000000001,0.312243016306053,
-0.4)) ;
#114445 = CARTESIAN_POINT('Ctrl Pts',(0.600069747422976,0.324350425899471,
-0.397751528521482)) ;
#114446 = CARTESIAN_POINT('Ctrl Pts',(0.599517124288211,0.34619696929758,
-0.389395449060154)) ;
#114447 = CARTESIAN_POINT('Ctrl Pts',(0.598927484301167,0.355857825373388,
-0.383675044722851)) ;
#114448 = CARTESIAN_POINT('Ctrl Pts',(0.596766673872565,0.36653901230802,
-0.374702385109574)) ;
#114449 = CARTESIAN_POINT('Ctrl Pts',(0.596235629104145,0.368676603883155,
-0.372737916809195)) ;
#114450 = CARTESIAN_POINT('Ctrl Pts',(0.595612997216081,0.370705721320403,
-0.370705721320403)) ;
#114451 = CARTESIAN_POINT('Origin',(2.4,0.,0.)) ;
#114452 = CARTESIAN_POINT('',(2.4,-1.22464679914735E-16,-1.)) ;
#114453 = CARTESIAN_POINT('Origin',(1.4,3.15,-1.25857864376269)) ;
#114454 = CARTESIAN_POINT('',(1.5,3.25,-1.25857864376269)) ;
#114455 = CARTESIAN_POINT('',(1.5,3.07928932188135,-1.32928932188135)) ;
#114456 = CARTESIAN_POINT('Origin',(1.5,3.15,-1.25857864376269)) ;
#114457 = CARTESIAN_POINT('',(1.4,3.07928932188135,-1.32928932188135)) ;
#114458 = CARTESIAN_POINT('',(1.4,3.25,-1.25857864376269)) ;
#114459 = CARTESIAN_POINT('Origin',(0.600000000000001,2.80617032878603E-17,
-34.29)) ;
#114460 = CARTESIAN_POINT('',(0.600000000000001,-1.9,-33.89)) ;
#114461 = CARTESIAN_POINT('',(0.600000000000001,-0.3,-33.89)) ;
#114462 = CARTESIAN_POINT('',(0.600000000000001,-2.39800009914436E-17,-33.89)) ;
#114463 = CARTESIAN_POINT('',(0.6,-0.4,-33.99)) ;
#114464 = CARTESIAN_POINT('Origin',(0.6,-0.3,-33.99)) ;
#114465 = CARTESIAN_POINT('',(0.6,-0.4,-34.59)) ;
#114466 = CARTESIAN_POINT('',(0.6,-0.4,-33.89)) ;
#114467 = CARTESIAN_POINT('Origin',(0.6,-0.3,-34.59)) ;
#114468 = CARTESIAN_POINT('',(0.600000000000001,-2.1,-34.89)) ;
#114469 = CARTESIAN_POINT('Origin',(0.600000000000001,-1.9,-34.89)) ;
#114470 = CARTESIAN_POINT('',(0.600000000000001,-2.1,-35.565)) ;
#114471 = CARTESIAN_POINT('',(0.600000000000001,-2.1,-34.29)) ;
#114472 = CARTESIAN_POINT('',(0.600000000000001,-2.9,-35.565)) ;
#114473 = CARTESIAN_POINT('',(0.600000000000001,-3.69904270612699E-17,-35.565)) ;
#114474 = CARTESIAN_POINT('',(0.600000000000001,-2.9,-33.015)) ;
#114475 = CARTESIAN_POINT('',(0.600000000000001,-2.9,-34.29)) ;
#114476 = CARTESIAN_POINT('',(0.600000000000001,-2.1,-33.015)) ;
#114477 = CARTESIAN_POINT('',(0.600000000000001,1.58165963986121E-16,-33.015)) ;
#114478 = CARTESIAN_POINT('',(0.600000000000001,-2.1,-33.69)) ;
#114479 = CARTESIAN_POINT('',(0.600000000000001,-2.1,-34.29)) ;
#114480 = CARTESIAN_POINT('Origin',(0.600000000000001,-1.9,-33.69)) ;
#114481 = CARTESIAN_POINT('Origin',(0.600000000000001,2.80617032878603E-17,
-30.48)) ;
#114482 = CARTESIAN_POINT('',(0.600000000000001,-1.9,-30.08)) ;
#114483 = CARTESIAN_POINT('',(0.600000000000001,-0.3,-30.08)) ;
#114484 = CARTESIAN_POINT('',(0.600000000000001,-2.39800009914441E-17,-30.08)) ;
#114485 = CARTESIAN_POINT('',(0.6,-0.4,-30.18)) ;
#114486 = CARTESIAN_POINT('Origin',(0.6,-0.3,-30.18)) ;
#114487 = CARTESIAN_POINT('',(0.6,-0.4,-30.78)) ;
#114488 = CARTESIAN_POINT('',(0.6,-0.4,-30.08)) ;
#114489 = CARTESIAN_POINT('Origin',(0.6,-0.3,-30.78)) ;
#114490 = CARTESIAN_POINT('',(0.600000000000001,-2.1,-31.08)) ;
#114491 = CARTESIAN_POINT('Origin',(0.600000000000001,-1.9,-31.08)) ;
#114492 = CARTESIAN_POINT('',(0.600000000000001,-2.1,-31.755)) ;
#114493 = CARTESIAN_POINT('',(0.600000000000001,-2.1,-30.48)) ;
#114494 = CARTESIAN_POINT('',(0.600000000000001,-2.9,-31.755)) ;
#114495 = CARTESIAN_POINT('',(0.600000000000001,-3.69904270612699E-17,-31.755)) ;
#114496 = CARTESIAN_POINT('',(0.600000000000001,-2.9,-29.205)) ;
#114497 = CARTESIAN_POINT('',(0.600000000000001,-2.9,-30.48)) ;
#114498 = CARTESIAN_POINT('',(0.600000000000001,-2.1,-29.205)) ;
#114499 = CARTESIAN_POINT('',(0.600000000000001,1.58165963986121E-16,-29.205)) ;
#114500 = CARTESIAN_POINT('',(0.600000000000001,-2.1,-29.88)) ;
#114501 = CARTESIAN_POINT('',(0.600000000000001,-2.1,-30.48)) ;
#114502 = CARTESIAN_POINT('Origin',(0.600000000000001,-1.9,-29.88)) ;
#114503 = CARTESIAN_POINT('Origin',(0.600000000000001,2.80617032878603E-17,
-26.67)) ;
#114504 = CARTESIAN_POINT('',(0.600000000000001,-1.9,-26.27)) ;
#114505 = CARTESIAN_POINT('',(0.600000000000001,-0.3,-26.27)) ;
#114506 = CARTESIAN_POINT('',(0.600000000000001,-2.39800009914441E-17,-26.27)) ;
#114507 = CARTESIAN_POINT('',(0.6,-0.4,-26.37)) ;
#114508 = CARTESIAN_POINT('Origin',(0.6,-0.3,-26.37)) ;
#114509 = CARTESIAN_POINT('',(0.6,-0.4,-26.97)) ;
#114510 = CARTESIAN_POINT('',(0.6,-0.4,-26.27)) ;
#114511 = CARTESIAN_POINT('Origin',(0.6,-0.3,-26.97)) ;
#114512 = CARTESIAN_POINT('',(0.600000000000001,-2.1,-27.27)) ;
#114513 = CARTESIAN_POINT('Origin',(0.600000000000001,-1.9,-27.27)) ;
#114514 = CARTESIAN_POINT('',(0.600000000000001,-2.1,-27.945)) ;
#114515 = CARTESIAN_POINT('',(0.600000000000001,-2.1,-26.67)) ;
#114516 = CARTESIAN_POINT('',(0.600000000000001,-2.9,-27.945)) ;
#114517 = CARTESIAN_POINT('',(0.600000000000001,-3.69904270612701E-17,-27.945)) ;
#114518 = CARTESIAN_POINT('',(0.600000000000001,-2.9,-25.395)) ;
#114519 = CARTESIAN_POINT('',(0.600000000000001,-2.9,-26.67)) ;
#114520 = CARTESIAN_POINT('',(0.600000000000001,-2.1,-25.395)) ;
#114521 = CARTESIAN_POINT('',(0.600000000000001,1.58165963986121E-16,-25.395)) ;
#114522 = CARTESIAN_POINT('',(0.600000000000001,-2.1,-26.07)) ;
#114523 = CARTESIAN_POINT('',(0.600000000000001,-2.1,-26.67)) ;
#114524 = CARTESIAN_POINT('Origin',(0.600000000000001,-1.9,-26.07)) ;
#114525 = CARTESIAN_POINT('Origin',(0.600000000000001,2.80617032878603E-17,
-22.86)) ;
#114526 = CARTESIAN_POINT('',(0.600000000000001,-1.9,-22.46)) ;
#114527 = CARTESIAN_POINT('',(0.600000000000001,-0.3,-22.46)) ;
#114528 = CARTESIAN_POINT('',(0.600000000000001,-2.39800009914441E-17,-22.46)) ;
#114529 = CARTESIAN_POINT('',(0.6,-0.4,-22.56)) ;
#114530 = CARTESIAN_POINT('Origin',(0.6,-0.3,-22.56)) ;
#114531 = CARTESIAN_POINT('',(0.6,-0.4,-23.16)) ;
#114532 = CARTESIAN_POINT('',(0.6,-0.4,-22.46)) ;
#114533 = CARTESIAN_POINT('Origin',(0.6,-0.3,-23.16)) ;
#114534 = CARTESIAN_POINT('',(0.600000000000001,-2.1,-23.46)) ;
#114535 = CARTESIAN_POINT('Origin',(0.600000000000001,-1.9,-23.46)) ;
#114536 = CARTESIAN_POINT('',(0.600000000000001,-2.1,-24.135)) ;
#114537 = CARTESIAN_POINT('',(0.600000000000001,-2.1,-22.86)) ;
#114538 = CARTESIAN_POINT('',(0.600000000000001,-2.9,-24.135)) ;
#114539 = CARTESIAN_POINT('',(0.600000000000001,-3.69904270612701E-17,-24.135)) ;
#114540 = CARTESIAN_POINT('',(0.600000000000001,-2.9,-21.585)) ;
#114541 = CARTESIAN_POINT('',(0.600000000000001,-2.9,-22.86)) ;
#114542 = CARTESIAN_POINT('',(0.600000000000001,-2.1,-21.585)) ;
#114543 = CARTESIAN_POINT('',(0.600000000000001,1.58165963986121E-16,-21.585)) ;
#114544 = CARTESIAN_POINT('',(0.600000000000001,-2.1,-22.26)) ;
#114545 = CARTESIAN_POINT('',(0.600000000000001,-2.1,-22.86)) ;
#114546 = CARTESIAN_POINT('Origin',(0.600000000000001,-1.9,-22.26)) ;
#114547 = CARTESIAN_POINT('Origin',(0.600000000000001,2.80617032878603E-17,
-19.05)) ;
#114548 = CARTESIAN_POINT('',(0.600000000000001,-1.9,-18.65)) ;
#114549 = CARTESIAN_POINT('',(0.600000000000001,-0.3,-18.65)) ;
#114550 = CARTESIAN_POINT('',(0.600000000000001,-2.39800009914441E-17,-18.65)) ;
#114551 = CARTESIAN_POINT('',(0.6,-0.4,-18.75)) ;
#114552 = CARTESIAN_POINT('Origin',(0.6,-0.3,-18.75)) ;
#114553 = CARTESIAN_POINT('',(0.6,-0.4,-19.35)) ;
#114554 = CARTESIAN_POINT('',(0.6,-0.4,-18.65)) ;
#114555 = CARTESIAN_POINT('Origin',(0.6,-0.3,-19.35)) ;
#114556 = CARTESIAN_POINT('',(0.600000000000001,-2.1,-19.65)) ;
#114557 = CARTESIAN_POINT('Origin',(0.600000000000001,-1.9,-19.65)) ;
#114558 = CARTESIAN_POINT('',(0.600000000000001,-2.1,-20.325)) ;
#114559 = CARTESIAN_POINT('',(0.600000000000001,-2.1,-19.05)) ;
#114560 = CARTESIAN_POINT('',(0.600000000000001,-2.9,-20.325)) ;
#114561 = CARTESIAN_POINT('',(0.600000000000001,-3.69904270612701E-17,-20.325)) ;
#114562 = CARTESIAN_POINT('',(0.600000000000001,-2.9,-17.775)) ;
#114563 = CARTESIAN_POINT('',(0.600000000000001,-2.9,-19.05)) ;
#114564 = CARTESIAN_POINT('',(0.600000000000001,-2.1,-17.775)) ;
#114565 = CARTESIAN_POINT('',(0.600000000000001,1.58165963986121E-16,-17.775)) ;
#114566 = CARTESIAN_POINT('',(0.600000000000001,-2.1,-18.45)) ;
#114567 = CARTESIAN_POINT('',(0.600000000000001,-2.1,-19.05)) ;
#114568 = CARTESIAN_POINT('Origin',(0.600000000000001,-1.9,-18.45)) ;
#114569 = CARTESIAN_POINT('Origin',(0.600000000000001,2.80617032878603E-17,
-15.24)) ;
#114570 = CARTESIAN_POINT('',(0.600000000000001,-1.9,-14.84)) ;
#114571 = CARTESIAN_POINT('',(0.600000000000001,-0.3,-14.84)) ;
#114572 = CARTESIAN_POINT('',(0.600000000000001,-2.39800009914441E-17,-14.84)) ;
#114573 = CARTESIAN_POINT('',(0.6,-0.4,-14.94)) ;
#114574 = CARTESIAN_POINT('Origin',(0.6,-0.3,-14.94)) ;
#114575 = CARTESIAN_POINT('',(0.6,-0.4,-15.54)) ;
#114576 = CARTESIAN_POINT('',(0.6,-0.4,-14.84)) ;
#114577 = CARTESIAN_POINT('Origin',(0.6,-0.3,-15.54)) ;
#114578 = CARTESIAN_POINT('',(0.600000000000001,-2.1,-15.84)) ;
#114579 = CARTESIAN_POINT('Origin',(0.600000000000001,-1.9,-15.84)) ;
#114580 = CARTESIAN_POINT('',(0.600000000000001,-2.1,-16.515)) ;
#114581 = CARTESIAN_POINT('',(0.600000000000001,-2.1,-15.24)) ;
#114582 = CARTESIAN_POINT('',(0.600000000000001,-2.9,-16.515)) ;
#114583 = CARTESIAN_POINT('',(0.600000000000001,-3.69904270612701E-17,-16.515)) ;
#114584 = CARTESIAN_POINT('',(0.600000000000001,-2.9,-13.965)) ;
#114585 = CARTESIAN_POINT('',(0.600000000000001,-2.9,-15.24)) ;
#114586 = CARTESIAN_POINT('',(0.600000000000001,-2.1,-13.965)) ;
#114587 = CARTESIAN_POINT('',(0.600000000000001,1.58165963986121E-16,-13.965)) ;
#114588 = CARTESIAN_POINT('',(0.600000000000001,-2.1,-14.64)) ;
#114589 = CARTESIAN_POINT('',(0.600000000000001,-2.1,-15.24)) ;
#114590 = CARTESIAN_POINT('Origin',(0.600000000000001,-1.9,-14.64)) ;
#114591 = CARTESIAN_POINT('Origin',(0.600000000000001,2.80617032878603E-17,
-11.43)) ;
#114592 = CARTESIAN_POINT('',(0.600000000000001,-1.9,-11.03)) ;
#114593 = CARTESIAN_POINT('',(0.600000000000001,-0.3,-11.03)) ;
#114594 = CARTESIAN_POINT('',(0.600000000000001,-2.39800009914441E-17,-11.03)) ;
#114595 = CARTESIAN_POINT('',(0.6,-0.4,-11.13)) ;
#114596 = CARTESIAN_POINT('Origin',(0.6,-0.3,-11.13)) ;
#114597 = CARTESIAN_POINT('',(0.6,-0.4,-11.73)) ;
#114598 = CARTESIAN_POINT('',(0.6,-0.4,-11.03)) ;
#114599 = CARTESIAN_POINT('Origin',(0.6,-0.3,-11.73)) ;
#114600 = CARTESIAN_POINT('',(0.600000000000001,-2.1,-12.03)) ;
#114601 = CARTESIAN_POINT('Origin',(0.600000000000001,-1.9,-12.03)) ;
#114602 = CARTESIAN_POINT('',(0.600000000000001,-2.1,-12.705)) ;
#114603 = CARTESIAN_POINT('',(0.600000000000001,-2.1,-11.43)) ;
#114604 = CARTESIAN_POINT('',(0.600000000000001,-2.9,-12.705)) ;
#114605 = CARTESIAN_POINT('',(0.600000000000001,-3.69904270612701E-17,-12.705)) ;
#114606 = CARTESIAN_POINT('',(0.600000000000001,-2.9,-10.155)) ;
#114607 = CARTESIAN_POINT('',(0.600000000000001,-2.9,-11.43)) ;
#114608 = CARTESIAN_POINT('',(0.600000000000001,-2.1,-10.155)) ;
#114609 = CARTESIAN_POINT('',(0.600000000000001,1.58165963986121E-16,-10.155)) ;
#114610 = CARTESIAN_POINT('',(0.600000000000001,-2.1,-10.83)) ;
#114611 = CARTESIAN_POINT('',(0.600000000000001,-2.1,-11.43)) ;
#114612 = CARTESIAN_POINT('Origin',(0.600000000000001,-1.9,-10.83)) ;
#114613 = CARTESIAN_POINT('Origin',(0.600000000000001,2.80617032878603E-17,
-7.62)) ;
#114614 = CARTESIAN_POINT('',(0.600000000000001,-1.9,-7.22)) ;
#114615 = CARTESIAN_POINT('',(0.600000000000001,-0.3,-7.22)) ;
#114616 = CARTESIAN_POINT('',(0.600000000000001,-2.39800009914439E-17,-7.22)) ;
#114617 = CARTESIAN_POINT('',(0.6,-0.4,-7.32)) ;
#114618 = CARTESIAN_POINT('Origin',(0.6,-0.3,-7.32)) ;
#114619 = CARTESIAN_POINT('',(0.6,-0.4,-7.92)) ;
#114620 = CARTESIAN_POINT('',(0.6,-0.4,-7.22)) ;
#114621 = CARTESIAN_POINT('Origin',(0.6,-0.3,-7.92)) ;
#114622 = CARTESIAN_POINT('',(0.600000000000001,-2.1,-8.22)) ;
#114623 = CARTESIAN_POINT('Origin',(0.600000000000001,-1.9,-8.22)) ;
#114624 = CARTESIAN_POINT('',(0.600000000000001,-2.1,-8.895)) ;
#114625 = CARTESIAN_POINT('',(0.600000000000001,-2.1,-7.62)) ;
#114626 = CARTESIAN_POINT('',(0.600000000000001,-2.9,-8.895)) ;
#114627 = CARTESIAN_POINT('',(0.600000000000001,-3.69904270612701E-17,-8.895)) ;
#114628 = CARTESIAN_POINT('',(0.600000000000001,-2.9,-6.345)) ;
#114629 = CARTESIAN_POINT('',(0.600000000000001,-2.9,-7.62)) ;
#114630 = CARTESIAN_POINT('',(0.600000000000001,-2.1,-6.345)) ;
#114631 = CARTESIAN_POINT('',(0.600000000000001,1.58165963986121E-16,-6.345)) ;
#114632 = CARTESIAN_POINT('',(0.600000000000001,-2.1,-7.02)) ;
#114633 = CARTESIAN_POINT('',(0.600000000000001,-2.1,-7.62)) ;
#114634 = CARTESIAN_POINT('Origin',(0.600000000000001,-1.9,-7.02)) ;
#114635 = CARTESIAN_POINT('Origin',(0.600000000000001,2.80617032878603E-17,
-3.81)) ;
#114636 = CARTESIAN_POINT('',(0.600000000000001,-1.9,-3.41)) ;
#114637 = CARTESIAN_POINT('',(0.600000000000001,-0.3,-3.41)) ;
#114638 = CARTESIAN_POINT('',(0.600000000000001,-2.3980000991444E-17,-3.41)) ;
#114639 = CARTESIAN_POINT('',(0.6,-0.4,-3.51)) ;
#114640 = CARTESIAN_POINT('Origin',(0.6,-0.3,-3.51)) ;
#114641 = CARTESIAN_POINT('',(0.6,-0.4,-4.11)) ;
#114642 = CARTESIAN_POINT('',(0.6,-0.4,-3.41)) ;
#114643 = CARTESIAN_POINT('Origin',(0.6,-0.3,-4.11)) ;
#114644 = CARTESIAN_POINT('',(0.600000000000001,-2.1,-4.41)) ;
#114645 = CARTESIAN_POINT('Origin',(0.600000000000001,-1.9,-4.41)) ;
#114646 = CARTESIAN_POINT('',(0.600000000000001,-2.1,-5.085)) ;
#114647 = CARTESIAN_POINT('',(0.600000000000001,-2.1,-3.81)) ;
#114648 = CARTESIAN_POINT('',(0.600000000000001,-2.9,-5.085)) ;
#114649 = CARTESIAN_POINT('',(0.600000000000001,-3.699042706127E-17,-5.085)) ;
#114650 = CARTESIAN_POINT('',(0.600000000000001,-2.9,-2.535)) ;
#114651 = CARTESIAN_POINT('',(0.600000000000001,-2.9,-3.81)) ;
#114652 = CARTESIAN_POINT('',(0.600000000000001,-2.1,-2.535)) ;
#114653 = CARTESIAN_POINT('',(0.600000000000001,1.58165963986121E-16,-2.535)) ;
#114654 = CARTESIAN_POINT('',(0.600000000000001,-2.1,-3.21)) ;
#114655 = CARTESIAN_POINT('',(0.600000000000001,-2.1,-3.81)) ;
#114656 = CARTESIAN_POINT('Origin',(0.600000000000001,-1.9,-3.21)) ;
#114657 = CARTESIAN_POINT('Origin',(-0.999999999999999,1.25,-35.665)) ;
#114658 = CARTESIAN_POINT('',(-1.1,-1.9,-35.665)) ;
#114659 = CARTESIAN_POINT('',(-0.899999999999999,-2.1,-35.665)) ;
#114660 = CARTESIAN_POINT('Origin',(-0.899999999999999,-1.9,-35.665)) ;
#114661 = CARTESIAN_POINT('',(-1.1,-2.9,-35.665)) ;
#114662 = CARTESIAN_POINT('',(-1.1,-2.9,-35.665)) ;
#114663 = CARTESIAN_POINT('',(0.500000000000001,-2.9,-35.665)) ;
#114664 = CARTESIAN_POINT('',(0.600000000000001,-2.9,-35.665)) ;
#114665 = CARTESIAN_POINT('',(0.500000000000001,-2.1,-35.665)) ;
#114666 = CARTESIAN_POINT('',(0.5,1.25,-35.665)) ;
#114667 = CARTESIAN_POINT('',(-0.999999999999999,-2.1,-35.665)) ;
#114668 = CARTESIAN_POINT('Origin',(-0.999999999999999,1.25,-32.915)) ;
#114669 = CARTESIAN_POINT('',(-0.899999999999999,-2.1,-32.915)) ;
#114670 = CARTESIAN_POINT('',(-1.1,-1.9,-32.915)) ;
#114671 = CARTESIAN_POINT('Origin',(-0.899999999999999,-1.9,-32.915)) ;
#114672 = CARTESIAN_POINT('',(0.500000000000001,-2.1,-32.915)) ;
#114673 = CARTESIAN_POINT('',(0.600000000000001,-2.1,-32.915)) ;
#114674 = CARTESIAN_POINT('',(0.500000000000001,-2.9,-32.915)) ;
#114675 = CARTESIAN_POINT('',(0.5,1.25,-32.915)) ;
#114676 = CARTESIAN_POINT('',(-1.1,-2.9,-32.915)) ;
#114677 = CARTESIAN_POINT('',(-1.1,-2.9,-32.915)) ;
#114678 = CARTESIAN_POINT('',(-1.1,1.25,-32.915)) ;
#114679 = CARTESIAN_POINT('Origin',(-0.999999999999999,1.25,-31.855)) ;
#114680 = CARTESIAN_POINT('',(-1.1,-1.9,-31.855)) ;
#114681 = CARTESIAN_POINT('',(-0.899999999999999,-2.1,-31.855)) ;
#114682 = CARTESIAN_POINT('Origin',(-0.899999999999999,-1.9,-31.855)) ;
#114683 = CARTESIAN_POINT('',(-1.1,-2.9,-31.855)) ;
#114684 = CARTESIAN_POINT('',(-1.1,-2.9,-31.855)) ;
#114685 = CARTESIAN_POINT('',(0.500000000000001,-2.9,-31.855)) ;
#114686 = CARTESIAN_POINT('',(0.600000000000001,-2.9,-31.855)) ;
#114687 = CARTESIAN_POINT('',(0.500000000000001,-2.1,-31.855)) ;
#114688 = CARTESIAN_POINT('',(0.5,1.25,-31.855)) ;
#114689 = CARTESIAN_POINT('',(-0.999999999999999,-2.1,-31.855)) ;
#114690 = CARTESIAN_POINT('Origin',(-0.999999999999999,1.25,-29.105)) ;
#114691 = CARTESIAN_POINT('',(-0.899999999999999,-2.1,-29.105)) ;
#114692 = CARTESIAN_POINT('',(-1.1,-1.9,-29.105)) ;
#114693 = CARTESIAN_POINT('Origin',(-0.899999999999999,-1.9,-29.105)) ;
#114694 = CARTESIAN_POINT('',(0.500000000000001,-2.1,-29.105)) ;
#114695 = CARTESIAN_POINT('',(0.600000000000001,-2.1,-29.105)) ;
#114696 = CARTESIAN_POINT('',(0.500000000000001,-2.9,-29.105)) ;
#114697 = CARTESIAN_POINT('',(0.5,1.25,-29.105)) ;
#114698 = CARTESIAN_POINT('',(-1.1,-2.9,-29.105)) ;
#114699 = CARTESIAN_POINT('',(-1.1,-2.9,-29.105)) ;
#114700 = CARTESIAN_POINT('',(-1.1,1.25,-29.105)) ;
#114701 = CARTESIAN_POINT('Origin',(-0.999999999999999,1.25,-28.045)) ;
#114702 = CARTESIAN_POINT('',(-1.1,-1.9,-28.045)) ;
#114703 = CARTESIAN_POINT('',(-0.899999999999999,-2.1,-28.045)) ;
#114704 = CARTESIAN_POINT('Origin',(-0.899999999999999,-1.9,-28.045)) ;
#114705 = CARTESIAN_POINT('',(-1.1,-2.9,-28.045)) ;
#114706 = CARTESIAN_POINT('',(-1.1,-2.9,-28.045)) ;
#114707 = CARTESIAN_POINT('',(0.500000000000001,-2.9,-28.045)) ;
#114708 = CARTESIAN_POINT('',(0.600000000000001,-2.9,-28.045)) ;
#114709 = CARTESIAN_POINT('',(0.500000000000001,-2.1,-28.045)) ;
#114710 = CARTESIAN_POINT('',(0.5,1.25,-28.045)) ;
#114711 = CARTESIAN_POINT('',(-0.999999999999999,-2.1,-28.045)) ;
#114712 = CARTESIAN_POINT('Origin',(-0.999999999999999,1.25,-25.295)) ;
#114713 = CARTESIAN_POINT('',(-0.899999999999999,-2.1,-25.295)) ;
#114714 = CARTESIAN_POINT('',(-1.1,-1.9,-25.295)) ;
#114715 = CARTESIAN_POINT('Origin',(-0.899999999999999,-1.9,-25.295)) ;
#114716 = CARTESIAN_POINT('',(0.500000000000001,-2.1,-25.295)) ;
#114717 = CARTESIAN_POINT('',(0.600000000000001,-2.1,-25.295)) ;
#114718 = CARTESIAN_POINT('',(0.500000000000001,-2.9,-25.295)) ;
#114719 = CARTESIAN_POINT('',(0.5,1.25,-25.295)) ;
#114720 = CARTESIAN_POINT('',(-1.1,-2.9,-25.295)) ;
#114721 = CARTESIAN_POINT('',(-1.1,-2.9,-25.295)) ;
#114722 = CARTESIAN_POINT('',(-1.1,1.25,-25.295)) ;
#114723 = CARTESIAN_POINT('Origin',(-0.999999999999999,1.25,-24.235)) ;
#114724 = CARTESIAN_POINT('',(-1.1,-1.9,-24.235)) ;
#114725 = CARTESIAN_POINT('',(-0.899999999999999,-2.1,-24.235)) ;
#114726 = CARTESIAN_POINT('Origin',(-0.899999999999999,-1.9,-24.235)) ;
#114727 = CARTESIAN_POINT('',(-1.1,-2.9,-24.235)) ;
#114728 = CARTESIAN_POINT('',(-1.1,-2.9,-24.235)) ;
#114729 = CARTESIAN_POINT('',(0.500000000000001,-2.9,-24.235)) ;
#114730 = CARTESIAN_POINT('',(0.600000000000001,-2.9,-24.235)) ;
#114731 = CARTESIAN_POINT('',(0.500000000000001,-2.1,-24.235)) ;
#114732 = CARTESIAN_POINT('',(0.5,1.25,-24.235)) ;
#114733 = CARTESIAN_POINT('',(-0.999999999999999,-2.1,-24.235)) ;
#114734 = CARTESIAN_POINT('Origin',(-0.999999999999999,1.25,-21.485)) ;
#114735 = CARTESIAN_POINT('',(-0.899999999999999,-2.1,-21.485)) ;
#114736 = CARTESIAN_POINT('',(-1.1,-1.9,-21.485)) ;
#114737 = CARTESIAN_POINT('Origin',(-0.899999999999999,-1.9,-21.485)) ;
#114738 = CARTESIAN_POINT('',(0.500000000000001,-2.1,-21.485)) ;
#114739 = CARTESIAN_POINT('',(0.600000000000001,-2.1,-21.485)) ;
#114740 = CARTESIAN_POINT('',(0.500000000000001,-2.9,-21.485)) ;
#114741 = CARTESIAN_POINT('',(0.5,1.25,-21.485)) ;
#114742 = CARTESIAN_POINT('',(-1.1,-2.9,-21.485)) ;
#114743 = CARTESIAN_POINT('',(-1.1,-2.9,-21.485)) ;
#114744 = CARTESIAN_POINT('',(-1.1,1.25,-21.485)) ;
#114745 = CARTESIAN_POINT('Origin',(-0.999999999999999,1.25,-20.425)) ;
#114746 = CARTESIAN_POINT('',(-1.1,-1.9,-20.425)) ;
#114747 = CARTESIAN_POINT('',(-0.899999999999999,-2.1,-20.425)) ;
#114748 = CARTESIAN_POINT('Origin',(-0.899999999999999,-1.9,-20.425)) ;
#114749 = CARTESIAN_POINT('',(-1.1,-2.9,-20.425)) ;
#114750 = CARTESIAN_POINT('',(-1.1,-2.9,-20.425)) ;
#114751 = CARTESIAN_POINT('',(0.500000000000001,-2.9,-20.425)) ;
#114752 = CARTESIAN_POINT('',(0.600000000000001,-2.9,-20.425)) ;
#114753 = CARTESIAN_POINT('',(0.500000000000001,-2.1,-20.425)) ;
#114754 = CARTESIAN_POINT('',(0.5,1.25,-20.425)) ;
#114755 = CARTESIAN_POINT('',(-0.999999999999999,-2.1,-20.425)) ;
#114756 = CARTESIAN_POINT('Origin',(-0.999999999999999,1.25,-17.675)) ;
#114757 = CARTESIAN_POINT('',(-0.899999999999999,-2.1,-17.675)) ;
#114758 = CARTESIAN_POINT('',(-1.1,-1.9,-17.675)) ;
#114759 = CARTESIAN_POINT('Origin',(-0.899999999999999,-1.9,-17.675)) ;
#114760 = CARTESIAN_POINT('',(0.500000000000001,-2.1,-17.675)) ;
#114761 = CARTESIAN_POINT('',(0.600000000000001,-2.1,-17.675)) ;
#114762 = CARTESIAN_POINT('',(0.500000000000001,-2.9,-17.675)) ;
#114763 = CARTESIAN_POINT('',(0.5,1.25,-17.675)) ;
#114764 = CARTESIAN_POINT('',(-1.1,-2.9,-17.675)) ;
#114765 = CARTESIAN_POINT('',(-1.1,-2.9,-17.675)) ;
#114766 = CARTESIAN_POINT('',(-1.1,1.25,-17.675)) ;
#114767 = CARTESIAN_POINT('Origin',(-0.999999999999999,1.25,-16.615)) ;
#114768 = CARTESIAN_POINT('',(-1.1,-1.9,-16.615)) ;
#114769 = CARTESIAN_POINT('',(-0.899999999999999,-2.1,-16.615)) ;
#114770 = CARTESIAN_POINT('Origin',(-0.899999999999999,-1.9,-16.615)) ;
#114771 = CARTESIAN_POINT('',(-1.1,-2.9,-16.615)) ;
#114772 = CARTESIAN_POINT('',(-1.1,-2.9,-16.615)) ;
#114773 = CARTESIAN_POINT('',(0.500000000000001,-2.9,-16.615)) ;
#114774 = CARTESIAN_POINT('',(0.600000000000001,-2.9,-16.615)) ;
#114775 = CARTESIAN_POINT('',(0.500000000000001,-2.1,-16.615)) ;
#114776 = CARTESIAN_POINT('',(0.5,1.25,-16.615)) ;
#114777 = CARTESIAN_POINT('',(-0.999999999999999,-2.1,-16.615)) ;
#114778 = CARTESIAN_POINT('Origin',(-0.999999999999999,1.25,-13.865)) ;
#114779 = CARTESIAN_POINT('',(-0.899999999999999,-2.1,-13.865)) ;
#114780 = CARTESIAN_POINT('',(-1.1,-1.9,-13.865)) ;
#114781 = CARTESIAN_POINT('Origin',(-0.899999999999999,-1.9,-13.865)) ;
#114782 = CARTESIAN_POINT('',(0.500000000000001,-2.1,-13.865)) ;
#114783 = CARTESIAN_POINT('',(0.600000000000001,-2.1,-13.865)) ;
#114784 = CARTESIAN_POINT('',(0.500000000000001,-2.9,-13.865)) ;
#114785 = CARTESIAN_POINT('',(0.5,1.25,-13.865)) ;
#114786 = CARTESIAN_POINT('',(-1.1,-2.9,-13.865)) ;
#114787 = CARTESIAN_POINT('',(-1.1,-2.9,-13.865)) ;
#114788 = CARTESIAN_POINT('',(-1.1,1.25,-13.865)) ;
#114789 = CARTESIAN_POINT('Origin',(-0.999999999999999,1.25,-12.805)) ;
#114790 = CARTESIAN_POINT('',(-1.1,-1.9,-12.805)) ;
#114791 = CARTESIAN_POINT('',(-0.899999999999999,-2.1,-12.805)) ;
#114792 = CARTESIAN_POINT('Origin',(-0.899999999999999,-1.9,-12.805)) ;
#114793 = CARTESIAN_POINT('',(-1.1,-2.9,-12.805)) ;
#114794 = CARTESIAN_POINT('',(-1.1,-2.9,-12.805)) ;
#114795 = CARTESIAN_POINT('',(0.500000000000001,-2.9,-12.805)) ;
#114796 = CARTESIAN_POINT('',(0.600000000000001,-2.9,-12.805)) ;
#114797 = CARTESIAN_POINT('',(0.500000000000001,-2.1,-12.805)) ;
#114798 = CARTESIAN_POINT('',(0.5,1.25,-12.805)) ;
#114799 = CARTESIAN_POINT('',(-0.999999999999999,-2.1,-12.805)) ;
#114800 = CARTESIAN_POINT('Origin',(-0.999999999999999,1.25,-10.055)) ;
#114801 = CARTESIAN_POINT('',(-0.899999999999999,-2.1,-10.055)) ;
#114802 = CARTESIAN_POINT('',(-1.1,-1.9,-10.055)) ;
#114803 = CARTESIAN_POINT('Origin',(-0.899999999999999,-1.9,-10.055)) ;
#114804 = CARTESIAN_POINT('',(0.500000000000001,-2.1,-10.055)) ;
#114805 = CARTESIAN_POINT('',(0.600000000000001,-2.1,-10.055)) ;
#114806 = CARTESIAN_POINT('',(0.500000000000001,-2.9,-10.055)) ;
#114807 = CARTESIAN_POINT('',(0.5,1.25,-10.055)) ;
#114808 = CARTESIAN_POINT('',(-1.1,-2.9,-10.055)) ;
#114809 = CARTESIAN_POINT('',(-1.1,-2.9,-10.055)) ;
#114810 = CARTESIAN_POINT('',(-1.1,1.25,-10.055)) ;
#114811 = CARTESIAN_POINT('Origin',(-0.999999999999999,1.25,-8.995)) ;
#114812 = CARTESIAN_POINT('',(-1.1,-1.9,-8.995)) ;
#114813 = CARTESIAN_POINT('',(-0.899999999999999,-2.1,-8.995)) ;
#114814 = CARTESIAN_POINT('Origin',(-0.899999999999999,-1.9,-8.995)) ;
#114815 = CARTESIAN_POINT('',(-1.1,-2.9,-8.995)) ;
#114816 = CARTESIAN_POINT('',(-1.1,-2.9,-8.995)) ;
#114817 = CARTESIAN_POINT('',(0.500000000000001,-2.9,-8.995)) ;
#114818 = CARTESIAN_POINT('',(0.600000000000001,-2.9,-8.995)) ;
#114819 = CARTESIAN_POINT('',(0.500000000000001,-2.1,-8.995)) ;
#114820 = CARTESIAN_POINT('',(0.5,1.25,-8.995)) ;
#114821 = CARTESIAN_POINT('',(-0.999999999999999,-2.1,-8.995)) ;
#114822 = CARTESIAN_POINT('Origin',(-0.999999999999999,1.25,-6.245)) ;
#114823 = CARTESIAN_POINT('',(-0.899999999999999,-2.1,-6.245)) ;
#114824 = CARTESIAN_POINT('',(-1.1,-1.9,-6.245)) ;
#114825 = CARTESIAN_POINT('Origin',(-0.899999999999999,-1.9,-6.245)) ;
#114826 = CARTESIAN_POINT('',(0.500000000000001,-2.1,-6.245)) ;
#114827 = CARTESIAN_POINT('',(0.600000000000001,-2.1,-6.245)) ;
#114828 = CARTESIAN_POINT('',(0.500000000000001,-2.9,-6.245)) ;
#114829 = CARTESIAN_POINT('',(0.5,1.25,-6.245)) ;
#114830 = CARTESIAN_POINT('',(-1.1,-2.9,-6.245)) ;
#114831 = CARTESIAN_POINT('',(-1.1,-2.9,-6.245)) ;
#114832 = CARTESIAN_POINT('',(-1.1,1.25,-6.245)) ;
#114833 = CARTESIAN_POINT('Origin',(-0.999999999999999,1.25,-5.185)) ;
#114834 = CARTESIAN_POINT('',(-1.1,-1.9,-5.185)) ;
#114835 = CARTESIAN_POINT('',(-0.899999999999999,-2.1,-5.185)) ;
#114836 = CARTESIAN_POINT('Origin',(-0.899999999999999,-1.9,-5.185)) ;
#114837 = CARTESIAN_POINT('',(-1.1,-2.9,-5.185)) ;
#114838 = CARTESIAN_POINT('',(-1.1,-2.9,-5.185)) ;
#114839 = CARTESIAN_POINT('',(0.500000000000001,-2.9,-5.185)) ;
#114840 = CARTESIAN_POINT('',(0.600000000000001,-2.9,-5.185)) ;
#114841 = CARTESIAN_POINT('',(0.500000000000001,-2.1,-5.185)) ;
#114842 = CARTESIAN_POINT('',(0.5,1.25,-5.185)) ;
#114843 = CARTESIAN_POINT('',(-0.999999999999999,-2.1,-5.185)) ;
#114844 = CARTESIAN_POINT('Origin',(-0.999999999999999,1.25,-2.435)) ;
#114845 = CARTESIAN_POINT('',(-0.899999999999999,-2.1,-2.435)) ;
#114846 = CARTESIAN_POINT('',(-1.1,-1.9,-2.435)) ;
#114847 = CARTESIAN_POINT('Origin',(-0.899999999999999,-1.9,-2.435)) ;
#114848 = CARTESIAN_POINT('',(0.500000000000001,-2.1,-2.435)) ;
#114849 = CARTESIAN_POINT('',(0.600000000000001,-2.1,-2.435)) ;
#114850 = CARTESIAN_POINT('',(0.500000000000001,-2.9,-2.435)) ;
#114851 = CARTESIAN_POINT('',(0.5,1.25,-2.435)) ;
#114852 = CARTESIAN_POINT('',(-1.1,-2.9,-2.435)) ;
#114853 = CARTESIAN_POINT('',(-1.1,-2.9,-2.435)) ;
#114854 = CARTESIAN_POINT('',(-1.1,1.25,-2.435)) ;
#114855 = CARTESIAN_POINT('Origin',(-1.1,-2.9,-36.89)) ;
#114856 = CARTESIAN_POINT('',(-1.2,-2.9,-2.335)) ;
#114857 = CARTESIAN_POINT('',(-1.2,-2.9,-1.475)) ;
#114858 = CARTESIAN_POINT('',(-1.2,-2.9,-36.89)) ;
#114859 = CARTESIAN_POINT('',(-1.1,-3.,-2.335)) ;
#114860 = CARTESIAN_POINT('Origin',(-1.1,-2.9,-2.335)) ;
#114861 = CARTESIAN_POINT('',(-1.1,-3.,-1.475)) ;
#114862 = CARTESIAN_POINT('',(-1.1,-3.,-36.89)) ;
#114863 = CARTESIAN_POINT('Origin',(-1.1,-2.9,-1.475)) ;
#114864 = CARTESIAN_POINT('Origin',(-1.1,-2.9,-36.89)) ;
#114865 = CARTESIAN_POINT('',(-1.2,-2.9,-6.145)) ;
#114866 = CARTESIAN_POINT('',(-1.2,-2.9,-5.285)) ;
#114867 = CARTESIAN_POINT('',(-1.2,-2.9,-36.89)) ;
#114868 = CARTESIAN_POINT('',(-1.1,-3.,-6.145)) ;
#114869 = CARTESIAN_POINT('Origin',(-1.1,-2.9,-6.145)) ;
#114870 = CARTESIAN_POINT('',(-1.1,-3.,-5.285)) ;
#114871 = CARTESIAN_POINT('',(-1.1,-3.,-36.89)) ;
#114872 = CARTESIAN_POINT('Origin',(-1.1,-2.9,-5.285)) ;
#114873 = CARTESIAN_POINT('Origin',(-1.1,-2.9,-36.89)) ;
#114874 = CARTESIAN_POINT('',(-1.2,-2.9,-9.955)) ;
#114875 = CARTESIAN_POINT('',(-1.2,-2.9,-9.095)) ;
#114876 = CARTESIAN_POINT('',(-1.2,-2.9,-36.89)) ;
#114877 = CARTESIAN_POINT('',(-1.1,-3.,-9.955)) ;
#114878 = CARTESIAN_POINT('Origin',(-1.1,-2.9,-9.955)) ;
#114879 = CARTESIAN_POINT('',(-1.1,-3.,-9.095)) ;
#114880 = CARTESIAN_POINT('',(-1.1,-3.,-36.89)) ;
#114881 = CARTESIAN_POINT('Origin',(-1.1,-2.9,-9.095)) ;
#114882 = CARTESIAN_POINT('Origin',(-1.1,-2.9,-36.89)) ;
#114883 = CARTESIAN_POINT('',(-1.2,-2.9,-13.765)) ;
#114884 = CARTESIAN_POINT('',(-1.2,-2.9,-12.905)) ;
#114885 = CARTESIAN_POINT('',(-1.2,-2.9,-36.89)) ;
#114886 = CARTESIAN_POINT('',(-1.1,-3.,-13.765)) ;
#114887 = CARTESIAN_POINT('Origin',(-1.1,-2.9,-13.765)) ;
#114888 = CARTESIAN_POINT('',(-1.1,-3.,-12.905)) ;
#114889 = CARTESIAN_POINT('',(-1.1,-3.,-36.89)) ;
#114890 = CARTESIAN_POINT('Origin',(-1.1,-2.9,-12.905)) ;
#114891 = CARTESIAN_POINT('Origin',(-1.1,-2.9,-36.89)) ;
#114892 = CARTESIAN_POINT('',(-1.2,-2.9,-17.575)) ;
#114893 = CARTESIAN_POINT('',(-1.2,-2.9,-16.715)) ;
#114894 = CARTESIAN_POINT('',(-1.2,-2.9,-36.89)) ;
#114895 = CARTESIAN_POINT('',(-1.1,-3.,-17.575)) ;
#114896 = CARTESIAN_POINT('Origin',(-1.1,-2.9,-17.575)) ;
#114897 = CARTESIAN_POINT('',(-1.1,-3.,-16.715)) ;
#114898 = CARTESIAN_POINT('',(-1.1,-3.,-36.89)) ;
#114899 = CARTESIAN_POINT('Origin',(-1.1,-2.9,-16.715)) ;
#114900 = CARTESIAN_POINT('Origin',(-1.1,-2.9,-36.89)) ;
#114901 = CARTESIAN_POINT('',(-1.2,-2.9,-21.385)) ;
#114902 = CARTESIAN_POINT('',(-1.2,-2.9,-20.525)) ;
#114903 = CARTESIAN_POINT('',(-1.2,-2.9,-36.89)) ;
#114904 = CARTESIAN_POINT('',(-1.1,-3.,-21.385)) ;
#114905 = CARTESIAN_POINT('Origin',(-1.1,-2.9,-21.385)) ;
#114906 = CARTESIAN_POINT('',(-1.1,-3.,-20.525)) ;
#114907 = CARTESIAN_POINT('',(-1.1,-3.,-36.89)) ;
#114908 = CARTESIAN_POINT('Origin',(-1.1,-2.9,-20.525)) ;
#114909 = CARTESIAN_POINT('Origin',(-1.1,-2.9,-36.89)) ;
#114910 = CARTESIAN_POINT('',(-1.2,-2.9,-25.195)) ;
#114911 = CARTESIAN_POINT('',(-1.2,-2.9,-24.335)) ;
#114912 = CARTESIAN_POINT('',(-1.2,-2.9,-36.89)) ;
#114913 = CARTESIAN_POINT('',(-1.1,-3.,-25.195)) ;
#114914 = CARTESIAN_POINT('Origin',(-1.1,-2.9,-25.195)) ;
#114915 = CARTESIAN_POINT('',(-1.1,-3.,-24.335)) ;
#114916 = CARTESIAN_POINT('',(-1.1,-3.,-36.89)) ;
#114917 = CARTESIAN_POINT('Origin',(-1.1,-2.9,-24.335)) ;
#114918 = CARTESIAN_POINT('Origin',(-1.1,-2.9,-36.89)) ;
#114919 = CARTESIAN_POINT('',(-1.2,-2.9,-29.005)) ;
#114920 = CARTESIAN_POINT('',(-1.2,-2.9,-28.145)) ;
#114921 = CARTESIAN_POINT('',(-1.2,-2.9,-36.89)) ;
#114922 = CARTESIAN_POINT('',(-1.1,-3.,-29.005)) ;
#114923 = CARTESIAN_POINT('Origin',(-1.1,-2.9,-29.005)) ;
#114924 = CARTESIAN_POINT('',(-1.1,-3.,-28.145)) ;
#114925 = CARTESIAN_POINT('',(-1.1,-3.,-36.89)) ;
#114926 = CARTESIAN_POINT('Origin',(-1.1,-2.9,-28.145)) ;
#114927 = CARTESIAN_POINT('Origin',(-1.1,-2.9,-36.89)) ;
#114928 = CARTESIAN_POINT('',(-1.2,-2.9,-32.815)) ;
#114929 = CARTESIAN_POINT('',(-1.2,-2.9,-31.955)) ;
#114930 = CARTESIAN_POINT('',(-1.2,-2.9,-36.89)) ;
#114931 = CARTESIAN_POINT('',(-1.1,-3.,-32.815)) ;
#114932 = CARTESIAN_POINT('Origin',(-1.1,-2.9,-32.815)) ;
#114933 = CARTESIAN_POINT('',(-1.1,-3.,-31.955)) ;
#114934 = CARTESIAN_POINT('',(-1.1,-3.,-36.89)) ;
#114935 = CARTESIAN_POINT('Origin',(-1.1,-2.9,-31.955)) ;
#114936 = CARTESIAN_POINT('Origin',(0.600000000000001,2.80617032878603E-17,
0.)) ;
#114937 = CARTESIAN_POINT('',(0.600000000000001,-1.9,0.4)) ;
#114938 = CARTESIAN_POINT('',(0.600000000000001,-0.3,0.4)) ;
#114939 = CARTESIAN_POINT('',(0.600000000000001,-2.3980000991444E-17,0.4)) ;
#114940 = CARTESIAN_POINT('',(0.6,-0.4,0.3)) ;
#114941 = CARTESIAN_POINT('Origin',(0.6,-0.3,0.3)) ;
#114942 = CARTESIAN_POINT('',(0.6,-0.4,-0.3)) ;
#114943 = CARTESIAN_POINT('',(0.6,-0.4,0.4)) ;
#114944 = CARTESIAN_POINT('Origin',(0.6,-0.3,-0.3)) ;
#114945 = CARTESIAN_POINT('',(0.600000000000001,-2.1,-0.6)) ;
#114946 = CARTESIAN_POINT('Origin',(0.600000000000001,-1.9,-0.6)) ;
#114947 = CARTESIAN_POINT('',(0.600000000000001,-2.1,-1.275)) ;
#114948 = CARTESIAN_POINT('',(0.600000000000001,-2.1,0.)) ;
#114949 = CARTESIAN_POINT('',(0.600000000000001,-2.9,-1.275)) ;
#114950 = CARTESIAN_POINT('',(0.600000000000001,-3.699042706127E-17,-1.275)) ;
#114951 = CARTESIAN_POINT('',(0.600000000000001,-2.9,1.275)) ;
#114952 = CARTESIAN_POINT('',(0.600000000000001,-2.9,0.)) ;
#114953 = CARTESIAN_POINT('',(0.600000000000001,-2.1,1.275)) ;
#114954 = CARTESIAN_POINT('',(0.600000000000001,1.58165963986121E-16,1.275)) ;
#114955 = CARTESIAN_POINT('',(0.600000000000001,-2.1,0.6)) ;
#114956 = CARTESIAN_POINT('',(0.600000000000001,-2.1,0.)) ;
#114957 = CARTESIAN_POINT('Origin',(0.600000000000001,-1.9,0.6)) ;
#114958 = CARTESIAN_POINT('Origin',(-0.999999999999999,1.25,-1.375)) ;
#114959 = CARTESIAN_POINT('',(-1.1,-1.9,-1.375)) ;
#114960 = CARTESIAN_POINT('',(-0.899999999999999,-2.1,-1.375)) ;
#114961 = CARTESIAN_POINT('Origin',(-0.899999999999999,-1.9,-1.375)) ;
#114962 = CARTESIAN_POINT('',(-1.1,-2.9,-1.375)) ;
#114963 = CARTESIAN_POINT('',(-1.1,-2.9,-1.375)) ;
#114964 = CARTESIAN_POINT('',(0.500000000000001,-2.9,-1.375)) ;
#114965 = CARTESIAN_POINT('',(0.600000000000001,-2.9,-1.375)) ;
#114966 = CARTESIAN_POINT('',(0.500000000000001,-2.1,-1.375)) ;
#114967 = CARTESIAN_POINT('',(0.5,1.25,-1.375)) ;
#114968 = CARTESIAN_POINT('',(-0.999999999999999,-2.1,-1.375)) ;
#114969 = CARTESIAN_POINT('Origin',(-0.999999999999999,1.25,1.375)) ;
#114970 = CARTESIAN_POINT('',(-0.899999999999999,-2.1,1.375)) ;
#114971 = CARTESIAN_POINT('',(-1.1,-1.9,1.375)) ;
#114972 = CARTESIAN_POINT('Origin',(-0.899999999999999,-1.9,1.375)) ;
#114973 = CARTESIAN_POINT('',(0.500000000000001,-2.1,1.375)) ;
#114974 = CARTESIAN_POINT('',(0.600000000000001,-2.1,1.375)) ;
#114975 = CARTESIAN_POINT('',(0.500000000000001,-2.9,1.375)) ;
#114976 = CARTESIAN_POINT('',(0.5,1.25,1.375)) ;
#114977 = CARTESIAN_POINT('',(-1.1,-2.9,1.375)) ;
#114978 = CARTESIAN_POINT('',(-1.1,-2.9,1.375)) ;
#114979 = CARTESIAN_POINT('',(-1.1,1.25,1.375)) ;
#114980 = CARTESIAN_POINT('Origin',(-1.1,-2.9,-36.89)) ;
#114981 = CARTESIAN_POINT('',(-1.2,-2.9,1.475)) ;
#114982 = CARTESIAN_POINT('',(-1.2,-2.9,2.5)) ;
#114983 = CARTESIAN_POINT('',(-1.2,-2.9,-36.89)) ;
#114984 = CARTESIAN_POINT('',(-1.1,-3.,1.475)) ;
#114985 = CARTESIAN_POINT('Origin',(-1.1,-2.9,1.475)) ;
#114986 = CARTESIAN_POINT('',(-1.1,-3.,2.5)) ;
#114987 = CARTESIAN_POINT('',(-1.1,-3.,-36.89)) ;
#114988 = CARTESIAN_POINT('Origin',(-1.1,-2.9,2.5)) ;
#114989 = CARTESIAN_POINT('Origin',(7.9,-2.9,-36.89)) ;
#114990 = CARTESIAN_POINT('',(7.9,-3.,-36.79)) ;
#114991 = CARTESIAN_POINT('',(7.9,-3.,2.5)) ;
#114992 = CARTESIAN_POINT('',(7.9,-3.,-36.89)) ;
#114993 = CARTESIAN_POINT('',(8.,-2.9,-36.79)) ;
#114994 = CARTESIAN_POINT('Origin',(7.9,-2.9,-36.79)) ;
#114995 = CARTESIAN_POINT('',(8.,-2.9,2.5)) ;
#114996 = CARTESIAN_POINT('',(8.,-2.9,-36.89)) ;
#114997 = CARTESIAN_POINT('Origin',(7.9,-2.9,2.5)) ;
#114998 = CARTESIAN_POINT('Origin',(-1.1,-3.,-36.89)) ;
#114999 = CARTESIAN_POINT('',(0.500000000000001,-3.,-35.765)) ;
#115000 = CARTESIAN_POINT('',(0.700000000000002,-3.,-35.565)) ;
#115001 = CARTESIAN_POINT('Origin',(0.500000000000001,-3.,-35.565)) ;
#115002 = CARTESIAN_POINT('',(-1.1,-3.,-35.765)) ;
#115003 = CARTESIAN_POINT('',(-1.1,-3.,-35.765)) ;
#115004 = CARTESIAN_POINT('',(-1.1,-3.,-36.79)) ;
#115005 = CARTESIAN_POINT('',(-1.1,-3.,-36.89)) ;
#115006 = CARTESIAN_POINT('',(7.9,-3.,-36.79)) ;
#115007 = CARTESIAN_POINT('',(-1.1,-3.,2.5)) ;
#115008 = CARTESIAN_POINT('',(0.500000000000001,-3.,1.475)) ;
#115009 = CARTESIAN_POINT('',(0.600000000000001,-3.,1.475)) ;
#115010 = CARTESIAN_POINT('',(0.700000000000002,-3.,1.275)) ;
#115011 = CARTESIAN_POINT('Origin',(0.500000000000001,-3.,1.275)) ;
#115012 = CARTESIAN_POINT('',(0.700000000000002,-3.,-1.275)) ;
#115013 = CARTESIAN_POINT('',(0.700000000000002,-3.,-36.89)) ;
#115014 = CARTESIAN_POINT('',(0.500000000000001,-3.,-1.475)) ;
#115015 = CARTESIAN_POINT('Origin',(0.500000000000001,-3.,-1.275)) ;
#115016 = CARTESIAN_POINT('',(-1.1,-3.,-1.475)) ;
#115017 = CARTESIAN_POINT('',(0.500000000000001,-3.,-2.335)) ;
#115018 = CARTESIAN_POINT('',(0.600000000000001,-3.,-2.335)) ;
#115019 = CARTESIAN_POINT('',(0.700000000000002,-3.,-2.535)) ;
#115020 = CARTESIAN_POINT('Origin',(0.500000000000001,-3.,-2.535)) ;
#115021 = CARTESIAN_POINT('',(0.700000000000002,-3.,-5.085)) ;
#115022 = CARTESIAN_POINT('',(0.700000000000002,-3.,-36.89)) ;
#115023 = CARTESIAN_POINT('',(0.500000000000001,-3.,-5.285)) ;
#115024 = CARTESIAN_POINT('Origin',(0.500000000000001,-3.,-5.085)) ;
#115025 = CARTESIAN_POINT('',(-1.1,-3.,-5.285)) ;
#115026 = CARTESIAN_POINT('',(0.500000000000001,-3.,-6.145)) ;
#115027 = CARTESIAN_POINT('',(0.600000000000001,-3.,-6.145)) ;
#115028 = CARTESIAN_POINT('',(0.700000000000002,-3.,-6.345)) ;
#115029 = CARTESIAN_POINT('Origin',(0.500000000000001,-3.,-6.345)) ;
#115030 = CARTESIAN_POINT('',(0.700000000000002,-3.,-8.895)) ;
#115031 = CARTESIAN_POINT('',(0.700000000000002,-3.,-36.89)) ;
#115032 = CARTESIAN_POINT('',(0.500000000000001,-3.,-9.095)) ;
#115033 = CARTESIAN_POINT('Origin',(0.500000000000001,-3.,-8.895)) ;
#115034 = CARTESIAN_POINT('',(-1.1,-3.,-9.095)) ;
#115035 = CARTESIAN_POINT('',(0.500000000000001,-3.,-9.955)) ;
#115036 = CARTESIAN_POINT('',(0.600000000000001,-3.,-9.955)) ;
#115037 = CARTESIAN_POINT('',(0.700000000000002,-3.,-10.155)) ;
#115038 = CARTESIAN_POINT('Origin',(0.500000000000001,-3.,-10.155)) ;
#115039 = CARTESIAN_POINT('',(0.700000000000002,-3.,-12.705)) ;
#115040 = CARTESIAN_POINT('',(0.700000000000002,-3.,-36.89)) ;
#115041 = CARTESIAN_POINT('',(0.500000000000001,-3.,-12.905)) ;
#115042 = CARTESIAN_POINT('Origin',(0.500000000000001,-3.,-12.705)) ;
#115043 = CARTESIAN_POINT('',(-1.1,-3.,-12.905)) ;
#115044 = CARTESIAN_POINT('',(0.500000000000001,-3.,-13.765)) ;
#115045 = CARTESIAN_POINT('',(0.600000000000001,-3.,-13.765)) ;
#115046 = CARTESIAN_POINT('',(0.700000000000002,-3.,-13.965)) ;
#115047 = CARTESIAN_POINT('Origin',(0.500000000000001,-3.,-13.965)) ;
#115048 = CARTESIAN_POINT('',(0.700000000000002,-3.,-16.515)) ;
#115049 = CARTESIAN_POINT('',(0.700000000000002,-3.,-36.89)) ;
#115050 = CARTESIAN_POINT('',(0.500000000000001,-3.,-16.715)) ;
#115051 = CARTESIAN_POINT('Origin',(0.500000000000001,-3.,-16.515)) ;
#115052 = CARTESIAN_POINT('',(-1.1,-3.,-16.715)) ;
#115053 = CARTESIAN_POINT('',(0.500000000000001,-3.,-17.575)) ;
#115054 = CARTESIAN_POINT('',(0.600000000000001,-3.,-17.575)) ;
#115055 = CARTESIAN_POINT('',(0.700000000000002,-3.,-17.775)) ;
#115056 = CARTESIAN_POINT('Origin',(0.500000000000001,-3.,-17.775)) ;
#115057 = CARTESIAN_POINT('',(0.700000000000002,-3.,-20.325)) ;
#115058 = CARTESIAN_POINT('',(0.700000000000002,-3.,-36.89)) ;
#115059 = CARTESIAN_POINT('',(0.500000000000001,-3.,-20.525)) ;
#115060 = CARTESIAN_POINT('Origin',(0.500000000000001,-3.,-20.325)) ;
#115061 = CARTESIAN_POINT('',(-1.1,-3.,-20.525)) ;
#115062 = CARTESIAN_POINT('',(0.500000000000001,-3.,-21.385)) ;
#115063 = CARTESIAN_POINT('',(0.600000000000001,-3.,-21.385)) ;
#115064 = CARTESIAN_POINT('',(0.700000000000002,-3.,-21.585)) ;
#115065 = CARTESIAN_POINT('Origin',(0.500000000000001,-3.,-21.585)) ;
#115066 = CARTESIAN_POINT('',(0.700000000000002,-3.,-24.135)) ;
#115067 = CARTESIAN_POINT('',(0.700000000000002,-3.,-36.89)) ;
#115068 = CARTESIAN_POINT('',(0.500000000000001,-3.,-24.335)) ;
#115069 = CARTESIAN_POINT('Origin',(0.500000000000001,-3.,-24.135)) ;
#115070 = CARTESIAN_POINT('',(-1.1,-3.,-24.335)) ;
#115071 = CARTESIAN_POINT('',(0.500000000000001,-3.,-25.195)) ;
#115072 = CARTESIAN_POINT('',(0.600000000000001,-3.,-25.195)) ;
#115073 = CARTESIAN_POINT('',(0.700000000000002,-3.,-25.395)) ;
#115074 = CARTESIAN_POINT('Origin',(0.500000000000001,-3.,-25.395)) ;
#115075 = CARTESIAN_POINT('',(0.700000000000002,-3.,-27.945)) ;
#115076 = CARTESIAN_POINT('',(0.700000000000002,-3.,-36.89)) ;
#115077 = CARTESIAN_POINT('',(0.500000000000001,-3.,-28.145)) ;
#115078 = CARTESIAN_POINT('Origin',(0.500000000000001,-3.,-27.945)) ;
#115079 = CARTESIAN_POINT('',(-1.1,-3.,-28.145)) ;
#115080 = CARTESIAN_POINT('',(0.500000000000001,-3.,-29.005)) ;
#115081 = CARTESIAN_POINT('',(0.600000000000001,-3.,-29.005)) ;
#115082 = CARTESIAN_POINT('',(0.700000000000002,-3.,-29.205)) ;
#115083 = CARTESIAN_POINT('Origin',(0.500000000000001,-3.,-29.205)) ;
#115084 = CARTESIAN_POINT('',(0.700000000000002,-3.,-31.755)) ;
#115085 = CARTESIAN_POINT('',(0.700000000000002,-3.,-36.89)) ;
#115086 = CARTESIAN_POINT('',(0.500000000000001,-3.,-31.955)) ;
#115087 = CARTESIAN_POINT('Origin',(0.500000000000001,-3.,-31.755)) ;
#115088 = CARTESIAN_POINT('',(-1.1,-3.,-31.955)) ;
#115089 = CARTESIAN_POINT('',(0.500000000000001,-3.,-32.815)) ;
#115090 = CARTESIAN_POINT('',(0.600000000000001,-3.,-32.815)) ;
#115091 = CARTESIAN_POINT('',(0.700000000000002,-3.,-33.015)) ;
#115092 = CARTESIAN_POINT('Origin',(0.500000000000001,-3.,-33.015)) ;
#115093 = CARTESIAN_POINT('',(0.700000000000002,-3.,-36.89)) ;
#115094 = CARTESIAN_POINT('Origin',(-1.1,-2.9,-36.89)) ;
#115095 = CARTESIAN_POINT('',(-1.2,-2.9,-35.765)) ;
#115096 = CARTESIAN_POINT('Origin',(-1.1,-2.9,-35.765)) ;
#115097 = CARTESIAN_POINT('',(-1.2,-2.9,-36.79)) ;
#115098 = CARTESIAN_POINT('',(-1.2,-2.9,-36.89)) ;
#115099 = CARTESIAN_POINT('Origin',(-1.1,-2.9,-36.79)) ;
#115100 = CARTESIAN_POINT('Origin',(-1.2,4.15,-36.89)) ;
#115101 = CARTESIAN_POINT('',(-1.2,1.15,-32.815)) ;
#115102 = CARTESIAN_POINT('',(-1.2,1.35,-33.015)) ;
#115103 = CARTESIAN_POINT('Origin',(-1.2,1.15,-33.015)) ;
#115104 = CARTESIAN_POINT('',(-1.2,-2.9,-32.815)) ;
#115105 = CARTESIAN_POINT('',(-1.2,1.15,-31.955)) ;
#115106 = CARTESIAN_POINT('',(-1.2,1.25,-31.955)) ;
#115107 = CARTESIAN_POINT('',(-1.2,1.35,-31.755)) ;
#115108 = CARTESIAN_POINT('Origin',(-1.2,1.15,-31.755)) ;
#115109 = CARTESIAN_POINT('',(-1.2,1.35,-29.205)) ;
#115110 = CARTESIAN_POINT('',(-1.2,1.35,-29.105)) ;
#115111 = CARTESIAN_POINT('',(-1.2,1.15,-29.005)) ;
#115112 = CARTESIAN_POINT('Origin',(-1.2,1.15,-29.205)) ;
#115113 = CARTESIAN_POINT('',(-1.2,-2.9,-29.005)) ;
#115114 = CARTESIAN_POINT('',(-1.2,1.15,-28.145)) ;
#115115 = CARTESIAN_POINT('',(-1.2,1.25,-28.145)) ;
#115116 = CARTESIAN_POINT('',(-1.2,1.35,-27.945)) ;
#115117 = CARTESIAN_POINT('Origin',(-1.2,1.15,-27.945)) ;
#115118 = CARTESIAN_POINT('',(-1.2,1.35,-25.395)) ;
#115119 = CARTESIAN_POINT('',(-1.2,1.35,-25.295)) ;
#115120 = CARTESIAN_POINT('',(-1.2,1.15,-25.195)) ;
#115121 = CARTESIAN_POINT('Origin',(-1.2,1.15,-25.395)) ;
#115122 = CARTESIAN_POINT('',(-1.2,-2.9,-25.195)) ;
#115123 = CARTESIAN_POINT('',(-1.2,1.15,-24.335)) ;
#115124 = CARTESIAN_POINT('',(-1.2,1.25,-24.335)) ;
#115125 = CARTESIAN_POINT('',(-1.2,1.35,-24.135)) ;
#115126 = CARTESIAN_POINT('Origin',(-1.2,1.15,-24.135)) ;
#115127 = CARTESIAN_POINT('',(-1.2,1.35,-21.585)) ;
#115128 = CARTESIAN_POINT('',(-1.2,1.35,-21.485)) ;
#115129 = CARTESIAN_POINT('',(-1.2,1.15,-21.385)) ;
#115130 = CARTESIAN_POINT('Origin',(-1.2,1.15,-21.585)) ;
#115131 = CARTESIAN_POINT('',(-1.2,-2.9,-21.385)) ;
#115132 = CARTESIAN_POINT('',(-1.2,1.15,-20.525)) ;
#115133 = CARTESIAN_POINT('',(-1.2,1.25,-20.525)) ;
#115134 = CARTESIAN_POINT('',(-1.2,1.35,-20.325)) ;
#115135 = CARTESIAN_POINT('Origin',(-1.2,1.15,-20.325)) ;
#115136 = CARTESIAN_POINT('',(-1.2,1.35,-17.775)) ;
#115137 = CARTESIAN_POINT('',(-1.2,1.35,-17.675)) ;
#115138 = CARTESIAN_POINT('',(-1.2,1.15,-17.575)) ;
#115139 = CARTESIAN_POINT('Origin',(-1.2,1.15,-17.775)) ;
#115140 = CARTESIAN_POINT('',(-1.2,-2.9,-17.575)) ;
#115141 = CARTESIAN_POINT('',(-1.2,1.15,-16.715)) ;
#115142 = CARTESIAN_POINT('',(-1.2,1.25,-16.715)) ;
#115143 = CARTESIAN_POINT('',(-1.2,1.35,-16.515)) ;
#115144 = CARTESIAN_POINT('Origin',(-1.2,1.15,-16.515)) ;
#115145 = CARTESIAN_POINT('',(-1.2,1.35,-13.965)) ;
#115146 = CARTESIAN_POINT('',(-1.2,1.35,-13.865)) ;
#115147 = CARTESIAN_POINT('',(-1.2,1.15,-13.765)) ;
#115148 = CARTESIAN_POINT('Origin',(-1.2,1.15,-13.965)) ;
#115149 = CARTESIAN_POINT('',(-1.2,-2.9,-13.765)) ;
#115150 = CARTESIAN_POINT('',(-1.2,1.15,-12.905)) ;
#115151 = CARTESIAN_POINT('',(-1.2,1.25,-12.905)) ;
#115152 = CARTESIAN_POINT('',(-1.2,1.35,-12.705)) ;
#115153 = CARTESIAN_POINT('Origin',(-1.2,1.15,-12.705)) ;
#115154 = CARTESIAN_POINT('',(-1.2,1.35,-10.155)) ;
#115155 = CARTESIAN_POINT('',(-1.2,1.35,-10.055)) ;
#115156 = CARTESIAN_POINT('',(-1.2,1.15,-9.955)) ;
#115157 = CARTESIAN_POINT('Origin',(-1.2,1.15,-10.155)) ;
#115158 = CARTESIAN_POINT('',(-1.2,-2.9,-9.955)) ;
#115159 = CARTESIAN_POINT('',(-1.2,1.15,-9.095)) ;
#115160 = CARTESIAN_POINT('',(-1.2,1.25,-9.095)) ;
#115161 = CARTESIAN_POINT('',(-1.2,1.35,-8.895)) ;
#115162 = CARTESIAN_POINT('Origin',(-1.2,1.15,-8.895)) ;
#115163 = CARTESIAN_POINT('',(-1.2,1.35,-6.345)) ;
#115164 = CARTESIAN_POINT('',(-1.2,1.35,-6.245)) ;
#115165 = CARTESIAN_POINT('',(-1.2,1.15,-6.145)) ;
#115166 = CARTESIAN_POINT('Origin',(-1.2,1.15,-6.345)) ;
#115167 = CARTESIAN_POINT('',(-1.2,-2.9,-6.145)) ;
#115168 = CARTESIAN_POINT('',(-1.2,1.15,-5.285)) ;
#115169 = CARTESIAN_POINT('',(-1.2,1.25,-5.285)) ;
#115170 = CARTESIAN_POINT('',(-1.2,1.35,-5.085)) ;
#115171 = CARTESIAN_POINT('Origin',(-1.2,1.15,-5.085)) ;
#115172 = CARTESIAN_POINT('',(-1.2,1.35,-2.535)) ;
#115173 = CARTESIAN_POINT('',(-1.2,1.35,-2.435)) ;
#115174 = CARTESIAN_POINT('',(-1.2,1.15,-2.335)) ;
#115175 = CARTESIAN_POINT('Origin',(-1.2,1.15,-2.535)) ;
#115176 = CARTESIAN_POINT('',(-1.2,-2.9,-2.335)) ;
#115177 = CARTESIAN_POINT('',(-1.2,1.15,-1.475)) ;
#115178 = CARTESIAN_POINT('',(-1.2,1.25,-1.475)) ;
#115179 = CARTESIAN_POINT('',(-1.2,1.35,-1.275)) ;
#115180 = CARTESIAN_POINT('Origin',(-1.2,1.15,-1.275)) ;
#115181 = CARTESIAN_POINT('',(-1.2,1.35,1.275)) ;
#115182 = CARTESIAN_POINT('',(-1.2,1.35,1.37499999999999)) ;
#115183 = CARTESIAN_POINT('',(-1.2,1.15,1.475)) ;
#115184 = CARTESIAN_POINT('Origin',(-1.2,1.15,1.275)) ;
#115185 = CARTESIAN_POINT('',(-1.2,-2.9,1.475)) ;
#115186 = CARTESIAN_POINT('',(-1.2,4.15,2.5)) ;
#115187 = CARTESIAN_POINT('',(-1.2,4.15,2.5)) ;
#115188 = CARTESIAN_POINT('',(-1.2,4.15,-36.79)) ;
#115189 = CARTESIAN_POINT('',(-1.2,4.15,-36.89)) ;
#115190 = CARTESIAN_POINT('',(-1.2,-2.9,-36.79)) ;
#115191 = CARTESIAN_POINT('',(-1.2,1.15,-35.765)) ;
#115192 = CARTESIAN_POINT('',(-1.2,1.25,-35.765)) ;
#115193 = CARTESIAN_POINT('',(-1.2,1.35,-35.565)) ;
#115194 = CARTESIAN_POINT('Origin',(-1.2,1.15,-35.565)) ;
#115195 = CARTESIAN_POINT('',(-1.2,1.35,-32.915)) ;
#115196 = CARTESIAN_POINT('Origin',(-1.1,4.15,-36.89)) ;
#115197 = CARTESIAN_POINT('',(-1.1,4.25,-36.79)) ;
#115198 = CARTESIAN_POINT('',(-1.1,4.25,2.5)) ;
#115199 = CARTESIAN_POINT('',(-1.1,4.25,-36.89)) ;
#115200 = CARTESIAN_POINT('Origin',(-1.1,4.15,-36.79)) ;
#115201 = CARTESIAN_POINT('Origin',(-1.1,4.15,2.5)) ;
#115202 = CARTESIAN_POINT('Origin',(-1.1,4.25,-36.89)) ;
#115203 = CARTESIAN_POINT('',(4.35,4.25,-36.79)) ;
#115204 = CARTESIAN_POINT('',(4.35,4.25,2.5)) ;
#115205 = CARTESIAN_POINT('',(4.35,4.25,-36.89)) ;
#115206 = CARTESIAN_POINT('',(-1.1,4.25,-36.79)) ;
#115207 = CARTESIAN_POINT('',(-1.1,4.25,2.5)) ;
#115208 = CARTESIAN_POINT('Origin',(4.35,4.35,-36.89)) ;
#115209 = CARTESIAN_POINT('',(4.45,4.35,-36.79)) ;
#115210 = CARTESIAN_POINT('',(4.45,4.35,2.5)) ;
#115211 = CARTESIAN_POINT('',(4.45,4.35,-36.89)) ;
#115212 = CARTESIAN_POINT('Origin',(4.35,4.35,-36.79)) ;
#115213 = CARTESIAN_POINT('Origin',(4.35,4.35,2.5)) ;
#115214 = CARTESIAN_POINT('Origin',(4.45,4.55,-36.89)) ;
#115215 = CARTESIAN_POINT('',(4.45,4.55,-36.79)) ;
#115216 = CARTESIAN_POINT('',(4.45,4.55,2.5)) ;
#115217 = CARTESIAN_POINT('',(4.45,4.55,-36.89)) ;
#115218 = CARTESIAN_POINT('',(4.45,4.35,-36.79)) ;
#115219 = CARTESIAN_POINT('',(4.45,4.55,2.5)) ;
#115220 = CARTESIAN_POINT('Origin',(4.55,4.55,-36.89)) ;
#115221 = CARTESIAN_POINT('',(4.55,4.65,-36.79)) ;
#115222 = CARTESIAN_POINT('',(4.55,4.65,2.5)) ;
#115223 = CARTESIAN_POINT('',(4.55,4.65,-36.89)) ;
#115224 = CARTESIAN_POINT('Origin',(4.55,4.55,-36.79)) ;
#115225 = CARTESIAN_POINT('Origin',(4.55,4.55,2.5)) ;
#115226 = CARTESIAN_POINT('Origin',(4.75,4.65,-36.89)) ;
#115227 = CARTESIAN_POINT('',(4.75,4.65,-36.79)) ;
#115228 = CARTESIAN_POINT('',(4.75,4.65,2.5)) ;
#115229 = CARTESIAN_POINT('',(4.75,4.65,-36.89)) ;
#115230 = CARTESIAN_POINT('',(4.55,4.65,-36.79)) ;
#115231 = CARTESIAN_POINT('',(4.75,4.65,2.5)) ;
#115232 = CARTESIAN_POINT('Origin',(4.75,4.55,-36.89)) ;
#115233 = CARTESIAN_POINT('',(4.85,4.55,-36.79)) ;
#115234 = CARTESIAN_POINT('',(4.85,4.55,2.5)) ;
#115235 = CARTESIAN_POINT('',(4.85,4.55,-36.89)) ;
#115236 = CARTESIAN_POINT('Origin',(4.75,4.55,-36.79)) ;
#115237 = CARTESIAN_POINT('Origin',(4.75,4.55,2.5)) ;
#115238 = CARTESIAN_POINT('Origin',(4.85,4.35,-36.89)) ;
#115239 = CARTESIAN_POINT('',(4.85,4.35,-36.79)) ;
#115240 = CARTESIAN_POINT('',(4.85,4.35,2.5)) ;
#115241 = CARTESIAN_POINT('',(4.85,4.35,-36.89)) ;
#115242 = CARTESIAN_POINT('',(4.85,4.55,-36.79)) ;
#115243 = CARTESIAN_POINT('',(4.85,4.35,2.5)) ;
#115244 = CARTESIAN_POINT('Origin',(4.95,4.35,-36.89)) ;
#115245 = CARTESIAN_POINT('',(4.95,4.25,-36.79)) ;
#115246 = CARTESIAN_POINT('',(4.95,4.25,2.5)) ;
#115247 = CARTESIAN_POINT('',(4.95,4.25,-36.89)) ;
#115248 = CARTESIAN_POINT('Origin',(4.95,4.35,-36.79)) ;
#115249 = CARTESIAN_POINT('Origin',(4.95,4.35,2.5)) ;
#115250 = CARTESIAN_POINT('Origin',(4.95,4.25,-36.89)) ;
#115251 = CARTESIAN_POINT('',(7.9,4.25,-36.79)) ;
#115252 = CARTESIAN_POINT('',(7.9,4.25,2.5)) ;
#115253 = CARTESIAN_POINT('',(7.9,4.25,-36.89)) ;
#115254 = CARTESIAN_POINT('',(4.95,4.25,-36.79)) ;
#115255 = CARTESIAN_POINT('',(4.95,4.25,2.5)) ;
#115256 = CARTESIAN_POINT('Origin',(7.9,4.15,-36.89)) ;
#115257 = CARTESIAN_POINT('',(8.,4.15,-36.79)) ;
#115258 = CARTESIAN_POINT('',(8.,4.15,2.5)) ;
#115259 = CARTESIAN_POINT('',(8.,4.15,-36.89)) ;
#115260 = CARTESIAN_POINT('Origin',(7.9,4.15,-36.79)) ;
#115261 = CARTESIAN_POINT('Origin',(7.9,4.15,2.5)) ;
#115262 = CARTESIAN_POINT('Origin',(8.,4.15,-36.89)) ;
#115263 = CARTESIAN_POINT('',(8.,4.15,-36.79)) ;
#115264 = CARTESIAN_POINT('',(8.,4.15,2.5)) ;
#115265 = CARTESIAN_POINT('',(8.,1.9,-32.54)) ;
#115266 = CARTESIAN_POINT('',(8.,2.1,-32.74)) ;
#115267 = CARTESIAN_POINT('Origin',(8.,1.9,-32.74)) ;
#115268 = CARTESIAN_POINT('',(8.,2.1,-33.69)) ;
#115269 = CARTESIAN_POINT('',(8.,2.1,-33.69)) ;
#115270 = CARTESIAN_POINT('',(8.,2.4,-33.69)) ;
#115271 = CARTESIAN_POINT('',(8.,2.4,-33.69)) ;
#115272 = CARTESIAN_POINT('',(8.,2.4,-33.5814213562373)) ;
#115273 = CARTESIAN_POINT('',(8.,2.4,-33.5814213562373)) ;
#115274 = CARTESIAN_POINT('',(8.,2.45857864376269,-33.44)) ;
#115275 = CARTESIAN_POINT('Origin',(8.,2.6,-33.5814213562373)) ;
#115276 = CARTESIAN_POINT('',(8.,3.00857864376269,-32.89)) ;
#115277 = CARTESIAN_POINT('',(8.,3.00857864376269,-32.89)) ;
#115278 = CARTESIAN_POINT('',(8.,3.35,-33.0314213562373)) ;
#115279 = CARTESIAN_POINT('Origin',(8.,3.15,-33.0314213562373)) ;
#115280 = CARTESIAN_POINT('',(8.,3.35,-35.5485786437627)) ;
#115281 = CARTESIAN_POINT('',(8.,2.45857864376269,-35.14)) ;
#115282 = CARTESIAN_POINT('',(8.,2.45857864376269,-35.14)) ;
#115283 = CARTESIAN_POINT('',(8.,2.4,-34.9985786437627)) ;
#115284 = CARTESIAN_POINT('Origin',(8.,2.6,-34.9985786437627)) ;
#115285 = CARTESIAN_POINT('',(8.,2.4,-34.89)) ;
#115286 = CARTESIAN_POINT('',(8.,2.4,-34.89)) ;
#115287 = CARTESIAN_POINT('',(8.,2.1,-34.89)) ;
#115288 = CARTESIAN_POINT('',(8.,2.1,-34.89)) ;
#115289 = CARTESIAN_POINT('',(8.,2.1,-35.84)) ;
#115290 = CARTESIAN_POINT('',(8.,2.1,-35.84)) ;
#115291 = CARTESIAN_POINT('',(8.,1.9,-36.04)) ;
#115292 = CARTESIAN_POINT('Origin',(8.,1.9,-35.84)) ;
#115293 = CARTESIAN_POINT('',(8.,-2.15,-36.04)) ;
#115294 = CARTESIAN_POINT('',(8.,-2.15,-36.04)) ;
#115295 = CARTESIAN_POINT('',(8.,-2.35,-35.84)) ;
#115296 = CARTESIAN_POINT('Origin',(8.,-2.15,-35.84)) ;
#115297 = CARTESIAN_POINT('',(8.,-2.35,-35.1931195934094)) ;
#115298 = CARTESIAN_POINT('',(8.,-2.35,-35.1931195934094)) ;
#115299 = CARTESIAN_POINT('',(8.,-2.32153024911032,-35.0902732340176)) ;
#115300 = CARTESIAN_POINT('Origin',(8.,-2.15,-35.1931195934094)) ;
#115301 = CARTESIAN_POINT('',(8.,-2.32153024911033,-33.4897267659824)) ;
#115302 = CARTESIAN_POINT('Origin',(8.,-3.65625,-34.29)) ;
#115303 = CARTESIAN_POINT('',(8.,-2.35,-33.3868804065906)) ;
#115304 = CARTESIAN_POINT('Origin',(8.,-2.15,-33.3868804065906)) ;
#115305 = CARTESIAN_POINT('',(8.,-2.35,-32.74)) ;
#115306 = CARTESIAN_POINT('',(8.,-2.35,-32.74)) ;
#115307 = CARTESIAN_POINT('',(8.,-2.15,-32.54)) ;
#115308 = CARTESIAN_POINT('Origin',(8.,-2.15,-32.74)) ;
#115309 = CARTESIAN_POINT('',(8.,1.9,-32.54)) ;
#115310 = CARTESIAN_POINT('',(8.,1.9,-28.73)) ;
#115311 = CARTESIAN_POINT('',(8.,2.1,-28.93)) ;
#115312 = CARTESIAN_POINT('Origin',(8.,1.9,-28.93)) ;
#115313 = CARTESIAN_POINT('',(8.,2.1,-29.88)) ;
#115314 = CARTESIAN_POINT('',(8.,2.1,-29.88)) ;
#115315 = CARTESIAN_POINT('',(8.,2.4,-29.88)) ;
#115316 = CARTESIAN_POINT('',(8.,2.4,-29.88)) ;
#115317 = CARTESIAN_POINT('',(8.,2.4,-29.7714213562373)) ;
#115318 = CARTESIAN_POINT('',(8.,2.4,-29.7714213562373)) ;
#115319 = CARTESIAN_POINT('',(8.,2.45857864376269,-29.63)) ;
#115320 = CARTESIAN_POINT('Origin',(8.,2.6,-29.7714213562373)) ;
#115321 = CARTESIAN_POINT('',(8.,3.00857864376269,-29.08)) ;
#115322 = CARTESIAN_POINT('',(8.,3.00857864376269,-29.08)) ;
#115323 = CARTESIAN_POINT('',(8.,3.35,-29.2214213562373)) ;
#115324 = CARTESIAN_POINT('Origin',(8.,3.15,-29.2214213562373)) ;
#115325 = CARTESIAN_POINT('',(8.,3.35,-31.7385786437627)) ;
#115326 = CARTESIAN_POINT('',(8.,2.45857864376269,-31.33)) ;
#115327 = CARTESIAN_POINT('',(8.,2.45857864376269,-31.33)) ;
#115328 = CARTESIAN_POINT('',(8.,2.4,-31.1885786437627)) ;
#115329 = CARTESIAN_POINT('Origin',(8.,2.6,-31.1885786437627)) ;
#115330 = CARTESIAN_POINT('',(8.,2.4,-31.08)) ;
#115331 = CARTESIAN_POINT('',(8.,2.4,-31.08)) ;
#115332 = CARTESIAN_POINT('',(8.,2.1,-31.08)) ;
#115333 = CARTESIAN_POINT('',(8.,2.1,-31.08)) ;
#115334 = CARTESIAN_POINT('',(8.,2.1,-32.03)) ;
#115335 = CARTESIAN_POINT('',(8.,2.1,-32.03)) ;
#115336 = CARTESIAN_POINT('',(8.,1.9,-32.23)) ;
#115337 = CARTESIAN_POINT('Origin',(8.,1.9,-32.03)) ;
#115338 = CARTESIAN_POINT('',(8.,-2.15,-32.23)) ;
#115339 = CARTESIAN_POINT('',(8.,-2.15,-32.23)) ;
#115340 = CARTESIAN_POINT('',(8.,-2.35,-32.03)) ;
#115341 = CARTESIAN_POINT('Origin',(8.,-2.15,-32.03)) ;
#115342 = CARTESIAN_POINT('',(8.,-2.35,-31.3831195934094)) ;
#115343 = CARTESIAN_POINT('',(8.,-2.35,-31.3831195934094)) ;
#115344 = CARTESIAN_POINT('',(8.,-2.32153024911032,-31.2802732340176)) ;
#115345 = CARTESIAN_POINT('Origin',(8.,-2.15,-31.3831195934094)) ;
#115346 = CARTESIAN_POINT('',(8.,-2.32153024911032,-29.6797267659824)) ;
#115347 = CARTESIAN_POINT('Origin',(8.,-3.65625,-30.48)) ;
#115348 = CARTESIAN_POINT('',(8.,-2.35,-29.5768804065906)) ;
#115349 = CARTESIAN_POINT('Origin',(8.,-2.15,-29.5768804065906)) ;
#115350 = CARTESIAN_POINT('',(8.,-2.35,-28.93)) ;
#115351 = CARTESIAN_POINT('',(8.,-2.35,-28.93)) ;
#115352 = CARTESIAN_POINT('',(8.,-2.15,-28.73)) ;
#115353 = CARTESIAN_POINT('Origin',(8.,-2.15,-28.93)) ;
#115354 = CARTESIAN_POINT('',(8.,1.9,-28.73)) ;
#115355 = CARTESIAN_POINT('',(8.,1.9,-24.92)) ;
#115356 = CARTESIAN_POINT('',(8.,2.1,-25.12)) ;
#115357 = CARTESIAN_POINT('Origin',(8.,1.9,-25.12)) ;
#115358 = CARTESIAN_POINT('',(8.,2.1,-26.07)) ;
#115359 = CARTESIAN_POINT('',(8.,2.1,-26.07)) ;
#115360 = CARTESIAN_POINT('',(8.,2.4,-26.07)) ;
#115361 = CARTESIAN_POINT('',(8.,2.4,-26.07)) ;
#115362 = CARTESIAN_POINT('',(8.,2.4,-25.9614213562373)) ;
#115363 = CARTESIAN_POINT('',(8.,2.4,-25.9614213562373)) ;
#115364 = CARTESIAN_POINT('',(8.,2.45857864376269,-25.82)) ;
#115365 = CARTESIAN_POINT('Origin',(8.,2.6,-25.9614213562373)) ;
#115366 = CARTESIAN_POINT('',(8.,3.00857864376269,-25.27)) ;
#115367 = CARTESIAN_POINT('',(8.,3.00857864376269,-25.27)) ;
#115368 = CARTESIAN_POINT('',(8.,3.35,-25.4114213562373)) ;
#115369 = CARTESIAN_POINT('Origin',(8.,3.15,-25.4114213562373)) ;
#115370 = CARTESIAN_POINT('',(8.,3.35,-27.9285786437627)) ;
#115371 = CARTESIAN_POINT('',(8.,2.45857864376269,-27.52)) ;
#115372 = CARTESIAN_POINT('',(8.,2.45857864376269,-27.52)) ;
#115373 = CARTESIAN_POINT('',(8.,2.4,-27.3785786437627)) ;
#115374 = CARTESIAN_POINT('Origin',(8.,2.6,-27.3785786437627)) ;
#115375 = CARTESIAN_POINT('',(8.,2.4,-27.27)) ;
#115376 = CARTESIAN_POINT('',(8.,2.4,-27.27)) ;
#115377 = CARTESIAN_POINT('',(8.,2.1,-27.27)) ;
#115378 = CARTESIAN_POINT('',(8.,2.1,-27.27)) ;
#115379 = CARTESIAN_POINT('',(8.,2.1,-28.22)) ;
#115380 = CARTESIAN_POINT('',(8.,2.1,-28.22)) ;
#115381 = CARTESIAN_POINT('',(8.,1.9,-28.42)) ;
#115382 = CARTESIAN_POINT('Origin',(8.,1.9,-28.22)) ;
#115383 = CARTESIAN_POINT('',(8.,-2.15,-28.42)) ;
#115384 = CARTESIAN_POINT('',(8.,-2.15,-28.42)) ;
#115385 = CARTESIAN_POINT('',(8.,-2.35,-28.22)) ;
#115386 = CARTESIAN_POINT('Origin',(8.,-2.15,-28.22)) ;
#115387 = CARTESIAN_POINT('',(8.,-2.35,-27.5731195934094)) ;
#115388 = CARTESIAN_POINT('',(8.,-2.35,-27.5731195934094)) ;
#115389 = CARTESIAN_POINT('',(8.,-2.32153024911032,-27.4702732340176)) ;
#115390 = CARTESIAN_POINT('Origin',(8.,-2.15,-27.5731195934094)) ;
#115391 = CARTESIAN_POINT('',(8.,-2.32153024911032,-25.8697267659824)) ;
#115392 = CARTESIAN_POINT('Origin',(8.,-3.65625,-26.67)) ;
#115393 = CARTESIAN_POINT('',(8.,-2.35,-25.7668804065906)) ;
#115394 = CARTESIAN_POINT('Origin',(8.,-2.15,-25.7668804065906)) ;
#115395 = CARTESIAN_POINT('',(8.,-2.35,-25.12)) ;
#115396 = CARTESIAN_POINT('',(8.,-2.35,-25.12)) ;
#115397 = CARTESIAN_POINT('',(8.,-2.15,-24.92)) ;
#115398 = CARTESIAN_POINT('Origin',(8.,-2.15,-25.12)) ;
#115399 = CARTESIAN_POINT('',(8.,1.9,-24.92)) ;
#115400 = CARTESIAN_POINT('',(8.,1.9,-21.11)) ;
#115401 = CARTESIAN_POINT('',(8.,2.1,-21.31)) ;
#115402 = CARTESIAN_POINT('Origin',(8.,1.9,-21.31)) ;
#115403 = CARTESIAN_POINT('',(8.,2.1,-22.26)) ;
#115404 = CARTESIAN_POINT('',(8.,2.1,-22.26)) ;
#115405 = CARTESIAN_POINT('',(8.,2.4,-22.26)) ;
#115406 = CARTESIAN_POINT('',(8.,2.4,-22.26)) ;
#115407 = CARTESIAN_POINT('',(8.,2.4,-22.1514213562373)) ;
#115408 = CARTESIAN_POINT('',(8.,2.4,-22.1514213562373)) ;
#115409 = CARTESIAN_POINT('',(8.,2.45857864376269,-22.01)) ;
#115410 = CARTESIAN_POINT('Origin',(8.,2.6,-22.1514213562373)) ;
#115411 = CARTESIAN_POINT('',(8.,3.00857864376269,-21.46)) ;
#115412 = CARTESIAN_POINT('',(8.,3.00857864376269,-21.46)) ;
#115413 = CARTESIAN_POINT('',(8.,3.35,-21.6014213562373)) ;
#115414 = CARTESIAN_POINT('Origin',(8.,3.15,-21.6014213562373)) ;
#115415 = CARTESIAN_POINT('',(8.,3.35,-24.1185786437627)) ;
#115416 = CARTESIAN_POINT('',(8.,2.45857864376269,-23.71)) ;
#115417 = CARTESIAN_POINT('',(8.,2.45857864376269,-23.71)) ;
#115418 = CARTESIAN_POINT('',(8.,2.4,-23.5685786437627)) ;
#115419 = CARTESIAN_POINT('Origin',(8.,2.6,-23.5685786437627)) ;
#115420 = CARTESIAN_POINT('',(8.,2.4,-23.46)) ;
#115421 = CARTESIAN_POINT('',(8.,2.4,-23.46)) ;
#115422 = CARTESIAN_POINT('',(8.,2.1,-23.46)) ;
#115423 = CARTESIAN_POINT('',(8.,2.1,-23.46)) ;
#115424 = CARTESIAN_POINT('',(8.,2.1,-24.41)) ;
#115425 = CARTESIAN_POINT('',(8.,2.1,-24.41)) ;
#115426 = CARTESIAN_POINT('',(8.,1.9,-24.61)) ;
#115427 = CARTESIAN_POINT('Origin',(8.,1.9,-24.41)) ;
#115428 = CARTESIAN_POINT('',(8.,-2.15,-24.61)) ;
#115429 = CARTESIAN_POINT('',(8.,-2.15,-24.61)) ;
#115430 = CARTESIAN_POINT('',(8.,-2.35,-24.41)) ;
#115431 = CARTESIAN_POINT('Origin',(8.,-2.15,-24.41)) ;
#115432 = CARTESIAN_POINT('',(8.,-2.35,-23.7631195934094)) ;
#115433 = CARTESIAN_POINT('',(8.,-2.35,-23.7631195934094)) ;
#115434 = CARTESIAN_POINT('',(8.,-2.32153024911032,-23.6602732340176)) ;
#115435 = CARTESIAN_POINT('Origin',(8.,-2.15,-23.7631195934094)) ;
#115436 = CARTESIAN_POINT('',(8.,-2.32153024911032,-22.0597267659824)) ;
#115437 = CARTESIAN_POINT('Origin',(8.,-3.65625,-22.86)) ;
#115438 = CARTESIAN_POINT('',(8.,-2.35,-21.9568804065906)) ;
#115439 = CARTESIAN_POINT('Origin',(8.,-2.15,-21.9568804065906)) ;
#115440 = CARTESIAN_POINT('',(8.,-2.35,-21.31)) ;
#115441 = CARTESIAN_POINT('',(8.,-2.35,-21.31)) ;
#115442 = CARTESIAN_POINT('',(8.,-2.15,-21.11)) ;
#115443 = CARTESIAN_POINT('Origin',(8.,-2.15,-21.31)) ;
#115444 = CARTESIAN_POINT('',(8.,1.9,-21.11)) ;
#115445 = CARTESIAN_POINT('',(8.,1.9,-17.3)) ;
#115446 = CARTESIAN_POINT('',(8.,2.1,-17.5)) ;
#115447 = CARTESIAN_POINT('Origin',(8.,1.9,-17.5)) ;
#115448 = CARTESIAN_POINT('',(8.,2.1,-18.45)) ;
#115449 = CARTESIAN_POINT('',(8.,2.1,-18.45)) ;
#115450 = CARTESIAN_POINT('',(8.,2.4,-18.45)) ;
#115451 = CARTESIAN_POINT('',(8.,2.4,-18.45)) ;
#115452 = CARTESIAN_POINT('',(8.,2.4,-18.3414213562373)) ;
#115453 = CARTESIAN_POINT('',(8.,2.4,-18.3414213562373)) ;
#115454 = CARTESIAN_POINT('',(8.,2.45857864376269,-18.2)) ;
#115455 = CARTESIAN_POINT('Origin',(8.,2.6,-18.3414213562373)) ;
#115456 = CARTESIAN_POINT('',(8.,3.00857864376269,-17.65)) ;
#115457 = CARTESIAN_POINT('',(8.,3.00857864376269,-17.65)) ;
#115458 = CARTESIAN_POINT('',(8.,3.35,-17.7914213562373)) ;
#115459 = CARTESIAN_POINT('Origin',(8.,3.15,-17.7914213562373)) ;
#115460 = CARTESIAN_POINT('',(8.,3.35,-20.3085786437627)) ;
#115461 = CARTESIAN_POINT('',(8.,2.45857864376269,-19.9)) ;
#115462 = CARTESIAN_POINT('',(8.,2.45857864376269,-19.9)) ;
#115463 = CARTESIAN_POINT('',(8.,2.4,-19.7585786437627)) ;
#115464 = CARTESIAN_POINT('Origin',(8.,2.6,-19.7585786437627)) ;
#115465 = CARTESIAN_POINT('',(8.,2.4,-19.65)) ;
#115466 = CARTESIAN_POINT('',(8.,2.4,-19.65)) ;
#115467 = CARTESIAN_POINT('',(8.,2.1,-19.65)) ;
#115468 = CARTESIAN_POINT('',(8.,2.1,-19.65)) ;
#115469 = CARTESIAN_POINT('',(8.,2.1,-20.6)) ;
#115470 = CARTESIAN_POINT('',(8.,2.1,-20.6)) ;
#115471 = CARTESIAN_POINT('',(8.,1.9,-20.8)) ;
#115472 = CARTESIAN_POINT('Origin',(8.,1.9,-20.6)) ;
#115473 = CARTESIAN_POINT('',(8.,-2.15,-20.8)) ;
#115474 = CARTESIAN_POINT('',(8.,-2.15,-20.8)) ;
#115475 = CARTESIAN_POINT('',(8.,-2.35,-20.6)) ;
#115476 = CARTESIAN_POINT('Origin',(8.,-2.15,-20.6)) ;
#115477 = CARTESIAN_POINT('',(8.,-2.35,-19.9531195934094)) ;
#115478 = CARTESIAN_POINT('',(8.,-2.35,-19.9531195934094)) ;
#115479 = CARTESIAN_POINT('',(8.,-2.32153024911032,-19.8502732340176)) ;
#115480 = CARTESIAN_POINT('Origin',(8.,-2.15,-19.9531195934094)) ;
#115481 = CARTESIAN_POINT('',(8.,-2.32153024911032,-18.2497267659824)) ;
#115482 = CARTESIAN_POINT('Origin',(8.,-3.65625,-19.05)) ;
#115483 = CARTESIAN_POINT('',(8.,-2.35,-18.1468804065906)) ;
#115484 = CARTESIAN_POINT('Origin',(8.,-2.15,-18.1468804065906)) ;
#115485 = CARTESIAN_POINT('',(8.,-2.35,-17.5)) ;
#115486 = CARTESIAN_POINT('',(8.,-2.35,-17.5)) ;
#115487 = CARTESIAN_POINT('',(8.,-2.15,-17.3)) ;
#115488 = CARTESIAN_POINT('Origin',(8.,-2.15,-17.5)) ;
#115489 = CARTESIAN_POINT('',(8.,1.9,-17.3)) ;
#115490 = CARTESIAN_POINT('',(8.,1.9,-13.49)) ;
#115491 = CARTESIAN_POINT('',(8.,2.1,-13.69)) ;
#115492 = CARTESIAN_POINT('Origin',(8.,1.9,-13.69)) ;
#115493 = CARTESIAN_POINT('',(8.,2.1,-14.64)) ;
#115494 = CARTESIAN_POINT('',(8.,2.1,-14.64)) ;
#115495 = CARTESIAN_POINT('',(8.,2.4,-14.64)) ;
#115496 = CARTESIAN_POINT('',(8.,2.4,-14.64)) ;
#115497 = CARTESIAN_POINT('',(8.,2.4,-14.5314213562373)) ;
#115498 = CARTESIAN_POINT('',(8.,2.4,-14.5314213562373)) ;
#115499 = CARTESIAN_POINT('',(8.,2.45857864376269,-14.39)) ;
#115500 = CARTESIAN_POINT('Origin',(8.,2.6,-14.5314213562373)) ;
#115501 = CARTESIAN_POINT('',(8.,3.00857864376269,-13.84)) ;
#115502 = CARTESIAN_POINT('',(8.,3.00857864376269,-13.84)) ;
#115503 = CARTESIAN_POINT('',(8.,3.35,-13.9814213562373)) ;
#115504 = CARTESIAN_POINT('Origin',(8.,3.15,-13.9814213562373)) ;
#115505 = CARTESIAN_POINT('',(8.,3.35,-16.4985786437627)) ;
#115506 = CARTESIAN_POINT('',(8.,2.45857864376269,-16.09)) ;
#115507 = CARTESIAN_POINT('',(8.,2.45857864376269,-16.09)) ;
#115508 = CARTESIAN_POINT('',(8.,2.4,-15.9485786437627)) ;
#115509 = CARTESIAN_POINT('Origin',(8.,2.6,-15.9485786437627)) ;
#115510 = CARTESIAN_POINT('',(8.,2.4,-15.84)) ;
#115511 = CARTESIAN_POINT('',(8.,2.4,-15.84)) ;
#115512 = CARTESIAN_POINT('',(8.,2.1,-15.84)) ;
#115513 = CARTESIAN_POINT('',(8.,2.1,-15.84)) ;
#115514 = CARTESIAN_POINT('',(8.,2.1,-16.79)) ;
#115515 = CARTESIAN_POINT('',(8.,2.1,-16.79)) ;
#115516 = CARTESIAN_POINT('',(8.,1.9,-16.99)) ;
#115517 = CARTESIAN_POINT('Origin',(8.,1.9,-16.79)) ;
#115518 = CARTESIAN_POINT('',(8.,-2.15,-16.99)) ;
#115519 = CARTESIAN_POINT('',(8.,-2.15,-16.99)) ;
#115520 = CARTESIAN_POINT('',(8.,-2.35,-16.79)) ;
#115521 = CARTESIAN_POINT('Origin',(8.,-2.15,-16.79)) ;
#115522 = CARTESIAN_POINT('',(8.,-2.35,-16.1431195934094)) ;
#115523 = CARTESIAN_POINT('',(8.,-2.35,-16.1431195934094)) ;
#115524 = CARTESIAN_POINT('',(8.,-2.32153024911032,-16.0402732340176)) ;
#115525 = CARTESIAN_POINT('Origin',(8.,-2.15,-16.1431195934094)) ;
#115526 = CARTESIAN_POINT('',(8.,-2.32153024911032,-14.4397267659824)) ;
#115527 = CARTESIAN_POINT('Origin',(8.,-3.65625,-15.24)) ;
#115528 = CARTESIAN_POINT('',(8.,-2.35,-14.3368804065906)) ;
#115529 = CARTESIAN_POINT('Origin',(8.,-2.15,-14.3368804065906)) ;
#115530 = CARTESIAN_POINT('',(8.,-2.35,-13.69)) ;
#115531 = CARTESIAN_POINT('',(8.,-2.35,-13.69)) ;
#115532 = CARTESIAN_POINT('',(8.,-2.15,-13.49)) ;
#115533 = CARTESIAN_POINT('Origin',(8.,-2.15,-13.69)) ;
#115534 = CARTESIAN_POINT('',(8.,1.9,-13.49)) ;
#115535 = CARTESIAN_POINT('',(8.,1.9,-9.68)) ;
#115536 = CARTESIAN_POINT('',(8.,2.1,-9.88)) ;
#115537 = CARTESIAN_POINT('Origin',(8.,1.9,-9.88)) ;
#115538 = CARTESIAN_POINT('',(8.,2.1,-10.83)) ;
#115539 = CARTESIAN_POINT('',(8.,2.1,-10.83)) ;
#115540 = CARTESIAN_POINT('',(8.,2.4,-10.83)) ;
#115541 = CARTESIAN_POINT('',(8.,2.4,-10.83)) ;
#115542 = CARTESIAN_POINT('',(8.,2.4,-10.7214213562373)) ;
#115543 = CARTESIAN_POINT('',(8.,2.4,-10.7214213562373)) ;
#115544 = CARTESIAN_POINT('',(8.,2.45857864376269,-10.58)) ;
#115545 = CARTESIAN_POINT('Origin',(8.,2.6,-10.7214213562373)) ;
#115546 = CARTESIAN_POINT('',(8.,3.00857864376269,-10.03)) ;
#115547 = CARTESIAN_POINT('',(8.,3.00857864376269,-10.03)) ;
#115548 = CARTESIAN_POINT('',(8.,3.35,-10.1714213562373)) ;
#115549 = CARTESIAN_POINT('Origin',(8.,3.15,-10.1714213562373)) ;
#115550 = CARTESIAN_POINT('',(8.,3.35,-12.6885786437627)) ;
#115551 = CARTESIAN_POINT('',(8.,2.45857864376269,-12.28)) ;
#115552 = CARTESIAN_POINT('',(8.,2.45857864376269,-12.28)) ;
#115553 = CARTESIAN_POINT('',(8.,2.4,-12.1385786437627)) ;
#115554 = CARTESIAN_POINT('Origin',(8.,2.6,-12.1385786437627)) ;
#115555 = CARTESIAN_POINT('',(8.,2.4,-12.03)) ;
#115556 = CARTESIAN_POINT('',(8.,2.4,-12.03)) ;
#115557 = CARTESIAN_POINT('',(8.,2.1,-12.03)) ;
#115558 = CARTESIAN_POINT('',(8.,2.1,-12.03)) ;
#115559 = CARTESIAN_POINT('',(8.,2.1,-12.98)) ;
#115560 = CARTESIAN_POINT('',(8.,2.1,-12.98)) ;
#115561 = CARTESIAN_POINT('',(8.,1.9,-13.18)) ;
#115562 = CARTESIAN_POINT('Origin',(8.,1.9,-12.98)) ;
#115563 = CARTESIAN_POINT('',(8.,-2.15,-13.18)) ;
#115564 = CARTESIAN_POINT('',(8.,-2.15,-13.18)) ;
#115565 = CARTESIAN_POINT('',(8.,-2.35,-12.98)) ;
#115566 = CARTESIAN_POINT('Origin',(8.,-2.15,-12.98)) ;
#115567 = CARTESIAN_POINT('',(8.,-2.35,-12.3331195934094)) ;
#115568 = CARTESIAN_POINT('',(8.,-2.35,-12.3331195934094)) ;
#115569 = CARTESIAN_POINT('',(8.,-2.32153024911032,-12.2302732340176)) ;
#115570 = CARTESIAN_POINT('Origin',(8.,-2.15,-12.3331195934094)) ;
#115571 = CARTESIAN_POINT('',(8.,-2.32153024911032,-10.6297267659824)) ;
#115572 = CARTESIAN_POINT('Origin',(8.,-3.65625,-11.43)) ;
#115573 = CARTESIAN_POINT('',(8.,-2.35,-10.5268804065906)) ;
#115574 = CARTESIAN_POINT('Origin',(8.,-2.15,-10.5268804065906)) ;
#115575 = CARTESIAN_POINT('',(8.,-2.35,-9.88)) ;
#115576 = CARTESIAN_POINT('',(8.,-2.35,-9.88)) ;
#115577 = CARTESIAN_POINT('',(8.,-2.15,-9.68)) ;
#115578 = CARTESIAN_POINT('Origin',(8.,-2.15,-9.88)) ;
#115579 = CARTESIAN_POINT('',(8.,1.9,-9.68)) ;
#115580 = CARTESIAN_POINT('',(8.,1.9,-5.87)) ;
#115581 = CARTESIAN_POINT('',(8.,2.1,-6.07)) ;
#115582 = CARTESIAN_POINT('Origin',(8.,1.9,-6.07)) ;
#115583 = CARTESIAN_POINT('',(8.,2.1,-7.02)) ;
#115584 = CARTESIAN_POINT('',(8.,2.1,-7.02)) ;
#115585 = CARTESIAN_POINT('',(8.,2.4,-7.02)) ;
#115586 = CARTESIAN_POINT('',(8.,2.4,-7.02)) ;
#115587 = CARTESIAN_POINT('',(8.,2.4,-6.91142135623731)) ;
#115588 = CARTESIAN_POINT('',(8.,2.4,-6.91142135623731)) ;
#115589 = CARTESIAN_POINT('',(8.,2.45857864376269,-6.77)) ;
#115590 = CARTESIAN_POINT('Origin',(8.,2.6,-6.91142135623731)) ;
#115591 = CARTESIAN_POINT('',(8.,3.00857864376269,-6.22)) ;
#115592 = CARTESIAN_POINT('',(8.,3.00857864376269,-6.22)) ;
#115593 = CARTESIAN_POINT('',(8.,3.35,-6.36142135623731)) ;
#115594 = CARTESIAN_POINT('Origin',(8.,3.15,-6.36142135623731)) ;
#115595 = CARTESIAN_POINT('',(8.,3.35,-8.87857864376269)) ;
#115596 = CARTESIAN_POINT('',(8.,2.45857864376269,-8.47)) ;
#115597 = CARTESIAN_POINT('',(8.,2.45857864376269,-8.47)) ;
#115598 = CARTESIAN_POINT('',(8.,2.4,-8.32857864376269)) ;
#115599 = CARTESIAN_POINT('Origin',(8.,2.6,-8.32857864376269)) ;
#115600 = CARTESIAN_POINT('',(8.,2.4,-8.22)) ;
#115601 = CARTESIAN_POINT('',(8.,2.4,-8.22)) ;
#115602 = CARTESIAN_POINT('',(8.,2.1,-8.22)) ;
#115603 = CARTESIAN_POINT('',(8.,2.1,-8.22)) ;
#115604 = CARTESIAN_POINT('',(8.,2.1,-9.17)) ;
#115605 = CARTESIAN_POINT('',(8.,2.1,-9.17)) ;
#115606 = CARTESIAN_POINT('',(8.,1.9,-9.37)) ;
#115607 = CARTESIAN_POINT('Origin',(8.,1.9,-9.17)) ;
#115608 = CARTESIAN_POINT('',(8.,-2.15,-9.37)) ;
#115609 = CARTESIAN_POINT('',(8.,-2.15,-9.37)) ;
#115610 = CARTESIAN_POINT('',(8.,-2.35,-9.17)) ;
#115611 = CARTESIAN_POINT('Origin',(8.,-2.15,-9.17)) ;
#115612 = CARTESIAN_POINT('',(8.,-2.35,-8.52311959340942)) ;
#115613 = CARTESIAN_POINT('',(8.,-2.35,-8.52311959340942)) ;
#115614 = CARTESIAN_POINT('',(8.,-2.32153024911032,-8.4202732340176)) ;
#115615 = CARTESIAN_POINT('Origin',(8.,-2.15,-8.52311959340942)) ;
#115616 = CARTESIAN_POINT('',(8.,-2.32153024911032,-6.8197267659824)) ;
#115617 = CARTESIAN_POINT('Origin',(8.,-3.65625,-7.62)) ;
#115618 = CARTESIAN_POINT('',(8.,-2.35,-6.71688040659058)) ;
#115619 = CARTESIAN_POINT('Origin',(8.,-2.15,-6.71688040659058)) ;
#115620 = CARTESIAN_POINT('',(8.,-2.35,-6.07)) ;
#115621 = CARTESIAN_POINT('',(8.,-2.35,-6.07)) ;
#115622 = CARTESIAN_POINT('',(8.,-2.15,-5.87)) ;
#115623 = CARTESIAN_POINT('Origin',(8.,-2.15,-6.07)) ;
#115624 = CARTESIAN_POINT('',(8.,1.9,-5.87)) ;
#115625 = CARTESIAN_POINT('',(8.,1.9,-2.06)) ;
#115626 = CARTESIAN_POINT('',(8.,2.1,-2.26)) ;
#115627 = CARTESIAN_POINT('Origin',(8.,1.9,-2.26)) ;
#115628 = CARTESIAN_POINT('',(8.,2.1,-3.21)) ;
#115629 = CARTESIAN_POINT('',(8.,2.1,-3.21)) ;
#115630 = CARTESIAN_POINT('',(8.,2.4,-3.21)) ;
#115631 = CARTESIAN_POINT('',(8.,2.4,-3.21)) ;
#115632 = CARTESIAN_POINT('',(8.,2.4,-3.10142135623731)) ;
#115633 = CARTESIAN_POINT('',(8.,2.4,-3.10142135623731)) ;
#115634 = CARTESIAN_POINT('',(8.,2.45857864376269,-2.96)) ;
#115635 = CARTESIAN_POINT('Origin',(8.,2.6,-3.10142135623731)) ;
#115636 = CARTESIAN_POINT('',(8.,3.00857864376269,-2.41)) ;
#115637 = CARTESIAN_POINT('',(8.,3.00857864376269,-2.41)) ;
#115638 = CARTESIAN_POINT('',(8.,3.35,-2.55142135623731)) ;
#115639 = CARTESIAN_POINT('Origin',(8.,3.15,-2.55142135623731)) ;
#115640 = CARTESIAN_POINT('',(8.,3.35,-5.06857864376269)) ;
#115641 = CARTESIAN_POINT('',(8.,2.45857864376269,-4.66)) ;
#115642 = CARTESIAN_POINT('',(8.,2.45857864376269,-4.66)) ;
#115643 = CARTESIAN_POINT('',(8.,2.4,-4.51857864376269)) ;
#115644 = CARTESIAN_POINT('Origin',(8.,2.6,-4.51857864376269)) ;
#115645 = CARTESIAN_POINT('',(8.,2.4,-4.41)) ;
#115646 = CARTESIAN_POINT('',(8.,2.4,-4.41)) ;
#115647 = CARTESIAN_POINT('',(8.,2.1,-4.41)) ;
#115648 = CARTESIAN_POINT('',(8.,2.1,-4.41)) ;
#115649 = CARTESIAN_POINT('',(8.,2.1,-5.36)) ;
#115650 = CARTESIAN_POINT('',(8.,2.1,-5.36)) ;
#115651 = CARTESIAN_POINT('',(8.,1.9,-5.56)) ;
#115652 = CARTESIAN_POINT('Origin',(8.,1.9,-5.36)) ;
#115653 = CARTESIAN_POINT('',(8.,-2.15,-5.56)) ;
#115654 = CARTESIAN_POINT('',(8.,-2.15,-5.56)) ;
#115655 = CARTESIAN_POINT('',(8.,-2.35,-5.36)) ;
#115656 = CARTESIAN_POINT('Origin',(8.,-2.15,-5.36)) ;
#115657 = CARTESIAN_POINT('',(8.,-2.35,-4.71311959340942)) ;
#115658 = CARTESIAN_POINT('',(8.,-2.35,-4.71311959340942)) ;
#115659 = CARTESIAN_POINT('',(8.,-2.32153024911032,-4.6102732340176)) ;
#115660 = CARTESIAN_POINT('Origin',(8.,-2.15,-4.71311959340942)) ;
#115661 = CARTESIAN_POINT('',(8.,-2.32153024911032,-3.0097267659824)) ;
#115662 = CARTESIAN_POINT('Origin',(8.,-3.65625,-3.81)) ;
#115663 = CARTESIAN_POINT('',(8.,-2.35,-2.90688040659058)) ;
#115664 = CARTESIAN_POINT('Origin',(8.,-2.15,-2.90688040659058)) ;
#115665 = CARTESIAN_POINT('',(8.,-2.35,-2.26)) ;
#115666 = CARTESIAN_POINT('',(8.,-2.35,-2.26)) ;
#115667 = CARTESIAN_POINT('',(8.,-2.15,-2.06)) ;
#115668 = CARTESIAN_POINT('Origin',(8.,-2.15,-2.26)) ;
#115669 = CARTESIAN_POINT('',(8.,1.9,-2.06)) ;
#115670 = CARTESIAN_POINT('',(8.,1.9,1.75)) ;
#115671 = CARTESIAN_POINT('',(8.,2.1,1.55)) ;
#115672 = CARTESIAN_POINT('Origin',(8.,1.9,1.55)) ;
#115673 = CARTESIAN_POINT('',(8.,2.1,0.6)) ;
#115674 = CARTESIAN_POINT('',(8.,2.1,0.600000000000003)) ;
#115675 = CARTESIAN_POINT('',(8.,2.4,0.6)) ;
#115676 = CARTESIAN_POINT('',(8.,2.4,0.6)) ;
#115677 = CARTESIAN_POINT('',(8.,2.4,0.70857864376269)) ;
#115678 = CARTESIAN_POINT('',(8.,2.4,0.70857864376269)) ;
#115679 = CARTESIAN_POINT('',(8.,2.45857864376269,0.849999999999999)) ;
#115680 = CARTESIAN_POINT('Origin',(8.,2.6,0.70857864376269)) ;
#115681 = CARTESIAN_POINT('',(8.,3.00857864376269,1.4)) ;
#115682 = CARTESIAN_POINT('',(8.,3.00857864376269,1.4)) ;
#115683 = CARTESIAN_POINT('',(8.,3.35,1.25857864376269)) ;
#115684 = CARTESIAN_POINT('Origin',(8.,3.15,1.25857864376269)) ;
#115685 = CARTESIAN_POINT('',(8.,3.35,-1.25857864376269)) ;
#115686 = CARTESIAN_POINT('',(8.,2.45857864376269,-0.850000000000001)) ;
#115687 = CARTESIAN_POINT('',(8.,2.45857864376269,-0.85)) ;
#115688 = CARTESIAN_POINT('',(8.,2.4,-0.70857864376269)) ;
#115689 = CARTESIAN_POINT('Origin',(8.,2.6,-0.70857864376269)) ;
#115690 = CARTESIAN_POINT('',(8.,2.4,-0.6)) ;
#115691 = CARTESIAN_POINT('',(8.,2.4,-0.6)) ;
#115692 = CARTESIAN_POINT('',(8.,2.1,-0.6)) ;
#115693 = CARTESIAN_POINT('',(8.,2.1,-0.6)) ;
#115694 = CARTESIAN_POINT('',(8.,2.1,-1.55)) ;
#115695 = CARTESIAN_POINT('',(8.,2.1,-1.55)) ;
#115696 = CARTESIAN_POINT('',(8.,1.9,-1.75)) ;
#115697 = CARTESIAN_POINT('Origin',(8.,1.9,-1.55)) ;
#115698 = CARTESIAN_POINT('',(8.,-2.15,-1.75)) ;
#115699 = CARTESIAN_POINT('',(8.,-2.15,-1.75)) ;
#115700 = CARTESIAN_POINT('',(8.,-2.35,-1.55)) ;
#115701 = CARTESIAN_POINT('Origin',(8.,-2.15,-1.55)) ;
#115702 = CARTESIAN_POINT('',(8.,-2.35,-0.903119593409422)) ;
#115703 = CARTESIAN_POINT('',(8.,-2.35,-0.903119593409422)) ;
#115704 = CARTESIAN_POINT('',(8.,-2.32153024911032,-0.800273234017602)) ;
#115705 = CARTESIAN_POINT('Origin',(8.,-2.15,-0.903119593409422)) ;
#115706 = CARTESIAN_POINT('',(8.,-2.32153024911032,0.800273234017602)) ;
#115707 = CARTESIAN_POINT('Origin',(8.,-3.65625,0.)) ;
#115708 = CARTESIAN_POINT('',(8.,-2.35,0.903119593409422)) ;
#115709 = CARTESIAN_POINT('Origin',(8.,-2.15,0.903119593409422)) ;
#115710 = CARTESIAN_POINT('',(8.,-2.35,1.55)) ;
#115711 = CARTESIAN_POINT('',(8.,-2.35,1.55)) ;
#115712 = CARTESIAN_POINT('',(8.,-2.15,1.75)) ;
#115713 = CARTESIAN_POINT('Origin',(8.,-2.15,1.55)) ;
#115714 = CARTESIAN_POINT('',(8.,1.9,1.75)) ;
#115715 = CARTESIAN_POINT('Origin',(7.9,-2.9,-36.89)) ;
#115716 = CARTESIAN_POINT('',(7.9,4.15,-36.89)) ;
#115717 = CARTESIAN_POINT('',(7.9,-2.9,-36.89)) ;
#115718 = CARTESIAN_POINT('',(7.9,-2.9,-36.89)) ;
#115719 = CARTESIAN_POINT('',(-1.1,-2.9,-36.89)) ;
#115720 = CARTESIAN_POINT('',(-1.1,-2.9,-36.89)) ;
#115721 = CARTESIAN_POINT('',(-1.1,4.15,-36.89)) ;
#115722 = CARTESIAN_POINT('',(-1.1,4.15,-36.89)) ;
#115723 = CARTESIAN_POINT('',(4.35,4.15,-36.89)) ;
#115724 = CARTESIAN_POINT('',(4.35,4.15,-36.89)) ;
#115725 = CARTESIAN_POINT('',(4.55,4.35,-36.89)) ;
#115726 = CARTESIAN_POINT('Origin',(4.35,4.35,-36.89)) ;
#115727 = CARTESIAN_POINT('',(4.55,4.55,-36.89)) ;
#115728 = CARTESIAN_POINT('',(4.55,4.55,-36.89)) ;
#115729 = CARTESIAN_POINT('',(4.75,4.55,-36.89)) ;
#115730 = CARTESIAN_POINT('',(4.75,4.55,-36.89)) ;
#115731 = CARTESIAN_POINT('',(4.75,4.35,-36.89)) ;
#115732 = CARTESIAN_POINT('',(4.75,4.35,-36.89)) ;
#115733 = CARTESIAN_POINT('',(4.95,4.15,-36.89)) ;
#115734 = CARTESIAN_POINT('Origin',(4.95,4.35,-36.89)) ;
#115735 = CARTESIAN_POINT('',(7.9,4.15,-36.89)) ;
#115736 = CARTESIAN_POINT('Origin',(7.9,-2.9,2.6)) ;
#115737 = CARTESIAN_POINT('',(-1.1,4.15,2.6)) ;
#115738 = CARTESIAN_POINT('',(-1.1,-2.9,2.6)) ;
#115739 = CARTESIAN_POINT('',(-1.1,-2.9,2.6)) ;
#115740 = CARTESIAN_POINT('',(7.9,-2.9,2.6)) ;
#115741 = CARTESIAN_POINT('',(7.9,-2.9,2.6)) ;
#115742 = CARTESIAN_POINT('',(7.9,4.15,2.6)) ;
#115743 = CARTESIAN_POINT('',(7.9,-2.9,2.6)) ;
#115744 = CARTESIAN_POINT('',(4.95,4.15,2.6)) ;
#115745 = CARTESIAN_POINT('',(7.9,4.15,2.6)) ;
#115746 = CARTESIAN_POINT('',(4.75,4.35,2.6)) ;
#115747 = CARTESIAN_POINT('Origin',(4.95,4.35,2.6)) ;
#115748 = CARTESIAN_POINT('',(4.75,4.55,2.6)) ;
#115749 = CARTESIAN_POINT('',(4.74999999999997,-2.89999999999999,2.6)) ;
#115750 = CARTESIAN_POINT('',(4.55,4.55,2.6)) ;
#115751 = CARTESIAN_POINT('',(7.9,4.55,2.6)) ;
#115752 = CARTESIAN_POINT('',(4.55,4.35,2.6)) ;
#115753 = CARTESIAN_POINT('',(4.55,-2.9,2.6)) ;
#115754 = CARTESIAN_POINT('',(4.35,4.15,2.6)) ;
#115755 = CARTESIAN_POINT('Origin',(4.35,4.35,2.6)) ;
#115756 = CARTESIAN_POINT('',(7.9,4.15,2.6)) ;
#115757 = CARTESIAN_POINT('Origin',(-0.999999999999999,-1.59070596587277E-16,
0.)) ;
#115758 = CARTESIAN_POINT('',(-0.999999999999999,-1.9,0.6)) ;
#115759 = CARTESIAN_POINT('',(-0.999999999999999,-1.9,1.275)) ;
#115760 = CARTESIAN_POINT('',(-0.999999999999999,-1.9,1.375)) ;
#115761 = CARTESIAN_POINT('',(-0.999999999999999,1.15,1.275)) ;
#115762 = CARTESIAN_POINT('',(-0.999999999999999,-2.89663358890161E-17,1.275)) ;
#115763 = CARTESIAN_POINT('',(-0.999999999999999,1.15,-1.275)) ;
#115764 = CARTESIAN_POINT('',(-0.999999999999999,1.15,0.)) ;
#115765 = CARTESIAN_POINT('',(-0.999999999999999,-1.9,-1.275)) ;
#115766 = CARTESIAN_POINT('',(-0.999999999999999,-2.24122726936407E-16,-1.275)) ;
#115767 = CARTESIAN_POINT('',(-0.999999999999999,-1.9,-0.6)) ;
#115768 = CARTESIAN_POINT('',(-0.999999999999999,-1.9,-0.5)) ;
#115769 = CARTESIAN_POINT('',(-0.999999999999999,0.4,-0.6)) ;
#115770 = CARTESIAN_POINT('',(-0.999999999999999,0.5,-0.6)) ;
#115771 = CARTESIAN_POINT('',(-0.999999999999999,0.6,-0.4)) ;
#115772 = CARTESIAN_POINT('Origin',(-0.999999999999999,0.4,-0.4)) ;
#115773 = CARTESIAN_POINT('',(-0.999999999999999,0.6,0.4)) ;
#115774 = CARTESIAN_POINT('',(-0.999999999999999,0.6,0.5)) ;
#115775 = CARTESIAN_POINT('',(-0.999999999999999,0.4,0.6)) ;
#115776 = CARTESIAN_POINT('Origin',(-0.999999999999999,0.4,0.4)) ;
#115777 = CARTESIAN_POINT('',(-0.999999999999999,-2.,0.6)) ;
#115778 = CARTESIAN_POINT('Origin',(0.600000000000001,-2.,-0.5)) ;
#115779 = CARTESIAN_POINT('',(0.500000000000001,-2.,-0.6)) ;
#115780 = CARTESIAN_POINT('',(-0.899999999999999,-2.,-0.6)) ;
#115781 = CARTESIAN_POINT('',(0.600000000000001,-2.,-0.6)) ;
#115782 = CARTESIAN_POINT('',(-0.899999999999999,-2.,-1.275)) ;
#115783 = CARTESIAN_POINT('',(-0.899999999999999,-2.,-1.375)) ;
#115784 = CARTESIAN_POINT('',(0.500000000000001,-2.,-1.275)) ;
#115785 = CARTESIAN_POINT('',(0.600000000000001,-2.,-1.275)) ;
#115786 = CARTESIAN_POINT('',(0.500000000000001,-2.,-0.5)) ;
#115787 = CARTESIAN_POINT('Origin',(0.600000000000001,0.5,-0.5)) ;
#115788 = CARTESIAN_POINT('',(-0.899999999999999,0.4,-0.5)) ;
#115789 = CARTESIAN_POINT('',(-0.999999999999999,0.4,-0.5)) ;
#115790 = CARTESIAN_POINT('',(-0.899999999999999,-1.9,-0.5)) ;
#115791 = CARTESIAN_POINT('',(-0.899999999999999,-2.,-0.5)) ;
#115792 = CARTESIAN_POINT('',(0.600000000000001,-1.9,-0.5)) ;
#115793 = CARTESIAN_POINT('Origin',(0.600000000000001,0.5,0.5)) ;
#115794 = CARTESIAN_POINT('',(0.500000000000001,0.5,0.4)) ;
#115795 = CARTESIAN_POINT('',(-0.899999999999999,0.5,0.4)) ;
#115796 = CARTESIAN_POINT('',(-0.999999999999999,0.5,0.4)) ;
#115797 = CARTESIAN_POINT('',(-0.899999999999999,0.5,-0.4)) ;
#115798 = CARTESIAN_POINT('',(-0.899999999999999,0.5,-0.5)) ;
#115799 = CARTESIAN_POINT('',(0.500000000000001,0.5,-0.4)) ;
#115800 = CARTESIAN_POINT('',(0.600000000000001,0.5,-0.4)) ;
#115801 = CARTESIAN_POINT('',(0.500000000000001,0.5,0.5)) ;
#115802 = CARTESIAN_POINT('Origin',(0.600000000000001,-2.,0.5)) ;
#115803 = CARTESIAN_POINT('',(0.500000000000001,-1.9,0.5)) ;
#115804 = CARTESIAN_POINT('',(-0.899999999999999,-1.9,0.5)) ;
#115805 = CARTESIAN_POINT('',(0.600000000000001,-1.9,0.5)) ;
#115806 = CARTESIAN_POINT('',(-0.899999999999999,0.4,0.5)) ;
#115807 = CARTESIAN_POINT('',(-0.899999999999999,0.5,0.5)) ;
#115808 = CARTESIAN_POINT('',(0.500000000000001,0.4,0.5)) ;
#115809 = CARTESIAN_POINT('',(0.600000000000001,0.4,0.5)) ;
#115810 = CARTESIAN_POINT('',(0.500000000000001,-2.,0.5)) ;
#115811 = CARTESIAN_POINT('Origin',(0.600000000000001,-2.,1.375)) ;
#115812 = CARTESIAN_POINT('',(0.500000000000001,-2.,1.275)) ;
#115813 = CARTESIAN_POINT('',(-0.899999999999999,-2.,1.275)) ;
#115814 = CARTESIAN_POINT('',(-0.999999999999999,-2.,1.275)) ;
#115815 = CARTESIAN_POINT('',(-0.899999999999999,-2.,0.6)) ;
#115816 = CARTESIAN_POINT('',(-0.899999999999999,-2.,0.5)) ;
#115817 = CARTESIAN_POINT('',(0.500000000000001,-2.,0.6)) ;
#115818 = CARTESIAN_POINT('',(0.600000000000001,-2.,0.6)) ;
#115819 = CARTESIAN_POINT('',(0.500000000000001,-2.,1.375)) ;
#115820 = CARTESIAN_POINT('Origin',(1.4,2.1,0.6)) ;
#115821 = CARTESIAN_POINT('',(1.5,2.,0.6)) ;
#115822 = CARTESIAN_POINT('',(7.9,2.,0.6)) ;
#115823 = CARTESIAN_POINT('',(1.4,2.,0.6)) ;
#115824 = CARTESIAN_POINT('',(1.5,2.1,0.5)) ;
#115825 = CARTESIAN_POINT('Origin',(1.5,2.1,0.6)) ;
#115826 = CARTESIAN_POINT('',(7.9,2.1,0.5)) ;
#115827 = CARTESIAN_POINT('',(1.4,2.1,0.5)) ;
#115828 = CARTESIAN_POINT('Origin',(7.9,2.1,0.6)) ;
#115829 = CARTESIAN_POINT('Origin',(1.4,2.4,0.5)) ;
#115830 = CARTESIAN_POINT('',(1.5,2.4,0.5)) ;
#115831 = CARTESIAN_POINT('',(1.5,2.4,0.5)) ;
#115832 = CARTESIAN_POINT('',(7.9,2.4,0.5)) ;
#115833 = CARTESIAN_POINT('',(1.4,2.4,0.5)) ;
#115834 = CARTESIAN_POINT('',(7.9,2.1,0.5)) ;
#115835 = CARTESIAN_POINT('Origin',(1.4,2.4,0.6)) ;
#115836 = CARTESIAN_POINT('',(1.5,2.5,0.6)) ;
#115837 = CARTESIAN_POINT('Origin',(1.5,2.4,0.6)) ;
#115838 = CARTESIAN_POINT('',(7.9,2.5,0.6)) ;
#115839 = CARTESIAN_POINT('',(1.4,2.5,0.6)) ;
#115840 = CARTESIAN_POINT('Origin',(7.9,2.4,0.6)) ;
#115841 = CARTESIAN_POINT('Origin',(1.4,2.5,0.70857864376269)) ;
#115842 = CARTESIAN_POINT('',(1.5,2.5,0.70857864376269)) ;
#115843 = CARTESIAN_POINT('',(1.5,2.5,0.70857864376269)) ;
#115844 = CARTESIAN_POINT('',(7.9,2.5,0.70857864376269)) ;
#115845 = CARTESIAN_POINT('',(1.4,2.5,0.70857864376269)) ;
#115846 = CARTESIAN_POINT('',(7.9,2.5,0.6)) ;
#115847 = CARTESIAN_POINT('Origin',(1.4,2.6,0.70857864376269)) ;
#115848 = CARTESIAN_POINT('',(1.5,2.52928932188135,0.779289321881344)) ;
#115849 = CARTESIAN_POINT('Origin',(1.5,2.6,0.70857864376269)) ;
#115850 = CARTESIAN_POINT('',(7.9,2.52928932188135,0.779289321881344)) ;
#115851 = CARTESIAN_POINT('',(1.4,2.52928932188135,0.779289321881344)) ;
#115852 = CARTESIAN_POINT('Origin',(7.9,2.6,0.70857864376269)) ;
#115853 = CARTESIAN_POINT('Origin',(1.4,3.07928932188135,1.32928932188135)) ;
#115854 = CARTESIAN_POINT('',(1.5,3.07928932188135,1.32928932188134)) ;
#115855 = CARTESIAN_POINT('',(7.9,3.07928932188135,1.32928932188135)) ;
#115856 = CARTESIAN_POINT('',(1.4,3.07928932188135,1.32928932188135)) ;
#115857 = CARTESIAN_POINT('',(7.9,2.52928932188135,0.779289321881344)) ;
#115858 = CARTESIAN_POINT('Origin',(1.4,3.15,1.25857864376269)) ;
#115859 = CARTESIAN_POINT('',(7.9,3.25,1.25857864376269)) ;
#115860 = CARTESIAN_POINT('',(1.4,3.25,1.25857864376269)) ;
#115861 = CARTESIAN_POINT('Origin',(7.9,3.15,1.25857864376269)) ;
#115862 = CARTESIAN_POINT('Origin',(1.4,3.25,-1.25857864376269)) ;
#115863 = CARTESIAN_POINT('',(1.5,3.25,-1.25857864376269)) ;
#115864 = CARTESIAN_POINT('',(7.9,3.25,1.25857864376269)) ;
#115865 = CARTESIAN_POINT('Origin',(1.4,2.52928932188134,-0.779289321881346)) ;
#115866 = CARTESIAN_POINT('',(1.5,2.52928932188134,-0.779289321881346)) ;
#115867 = CARTESIAN_POINT('',(1.5,2.52928932188134,-0.779289321881346)) ;
#115868 = CARTESIAN_POINT('',(7.9,2.52928932188134,-0.779289321881346)) ;
#115869 = CARTESIAN_POINT('',(1.4,2.52928932188134,-0.779289321881346)) ;
#115870 = CARTESIAN_POINT('',(7.9,3.07928932188135,-1.32928932188135)) ;
#115871 = CARTESIAN_POINT('Origin',(1.4,2.6,-0.70857864376269)) ;
#115872 = CARTESIAN_POINT('',(1.5,2.5,-0.70857864376269)) ;
#115873 = CARTESIAN_POINT('Origin',(1.5,2.6,-0.70857864376269)) ;
#115874 = CARTESIAN_POINT('',(7.9,2.5,-0.70857864376269)) ;
#115875 = CARTESIAN_POINT('',(1.4,2.5,-0.70857864376269)) ;
#115876 = CARTESIAN_POINT('Origin',(7.9,2.6,-0.70857864376269)) ;
#115877 = CARTESIAN_POINT('Origin',(1.4,2.5,-0.6)) ;
#115878 = CARTESIAN_POINT('',(1.5,2.5,-0.6)) ;
#115879 = CARTESIAN_POINT('',(1.5,2.5,-0.6)) ;
#115880 = CARTESIAN_POINT('',(7.9,2.5,-0.6)) ;
#115881 = CARTESIAN_POINT('',(1.4,2.5,-0.6)) ;
#115882 = CARTESIAN_POINT('',(7.9,2.5,-0.70857864376269)) ;
#115883 = CARTESIAN_POINT('Origin',(1.4,2.4,-0.6)) ;
#115884 = CARTESIAN_POINT('',(1.5,2.4,-0.5)) ;
#115885 = CARTESIAN_POINT('Origin',(1.5,2.4,-0.6)) ;
#115886 = CARTESIAN_POINT('',(7.9,2.4,-0.5)) ;
#115887 = CARTESIAN_POINT('',(1.4,2.4,-0.5)) ;
#115888 = CARTESIAN_POINT('Origin',(7.9,2.4,-0.6)) ;
#115889 = CARTESIAN_POINT('Origin',(1.4,2.1,-0.5)) ;
#115890 = CARTESIAN_POINT('',(1.5,2.1,-0.5)) ;
#115891 = CARTESIAN_POINT('',(1.5,2.1,-0.5)) ;
#115892 = CARTESIAN_POINT('',(7.9,2.1,-0.5)) ;
#115893 = CARTESIAN_POINT('',(1.4,2.1,-0.5)) ;
#115894 = CARTESIAN_POINT('',(7.9,2.4,-0.5)) ;
#115895 = CARTESIAN_POINT('Origin',(1.4,2.1,-0.6)) ;
#115896 = CARTESIAN_POINT('',(1.5,2.,-0.6)) ;
#115897 = CARTESIAN_POINT('Origin',(1.5,2.1,-0.6)) ;
#115898 = CARTESIAN_POINT('',(7.9,2.,-0.6)) ;
#115899 = CARTESIAN_POINT('',(1.4,2.,-0.6)) ;
#115900 = CARTESIAN_POINT('Origin',(7.9,2.1,-0.6)) ;
#115901 = CARTESIAN_POINT('Origin',(1.4,2.,-0.6)) ;
#115902 = CARTESIAN_POINT('',(1.5,2.,-1.55)) ;
#115903 = CARTESIAN_POINT('',(1.5,2.,-1.55)) ;
#115904 = CARTESIAN_POINT('',(7.9,2.,-1.55)) ;
#115905 = CARTESIAN_POINT('',(1.4,2.,-1.55)) ;
#115906 = CARTESIAN_POINT('',(7.9,2.,-0.6)) ;
#115907 = CARTESIAN_POINT('Origin',(1.4,1.9,-1.55)) ;
#115908 = CARTESIAN_POINT('',(1.5,1.9,-1.65)) ;
#115909 = CARTESIAN_POINT('Origin',(1.5,1.9,-1.55)) ;
#115910 = CARTESIAN_POINT('',(7.9,1.9,-1.65)) ;
#115911 = CARTESIAN_POINT('',(1.4,1.9,-1.65)) ;
#115912 = CARTESIAN_POINT('Origin',(7.9,1.9,-1.55)) ;
#115913 = CARTESIAN_POINT('Origin',(1.4,1.9,-1.65)) ;
#115914 = CARTESIAN_POINT('',(1.5,-2.15,-1.65)) ;
#115915 = CARTESIAN_POINT('',(1.5,-2.15,-1.65)) ;
#115916 = CARTESIAN_POINT('',(7.9,-2.15,-1.65)) ;
#115917 = CARTESIAN_POINT('',(1.4,-2.15,-1.65)) ;
#115918 = CARTESIAN_POINT('',(7.9,1.9,-1.65)) ;
#115919 = CARTESIAN_POINT('Origin',(1.4,-2.15,-1.55)) ;
#115920 = CARTESIAN_POINT('',(1.5,-2.25,-1.55)) ;
#115921 = CARTESIAN_POINT('Origin',(1.5,-2.15,-1.55)) ;
#115922 = CARTESIAN_POINT('',(7.9,-2.25,-1.55)) ;
#115923 = CARTESIAN_POINT('',(1.4,-2.25,-1.55)) ;
#115924 = CARTESIAN_POINT('Origin',(7.9,-2.15,-1.55)) ;
#115925 = CARTESIAN_POINT('Origin',(1.4,-2.25,-0.903119593409422)) ;
#115926 = CARTESIAN_POINT('',(1.5,-2.25,-0.903119593409422)) ;
#115927 = CARTESIAN_POINT('',(1.5,-2.25,-0.903119593409423)) ;
#115928 = CARTESIAN_POINT('',(7.9,-2.25,-0.903119593409422)) ;
#115929 = CARTESIAN_POINT('',(1.4,-2.25,-0.903119593409422)) ;
#115930 = CARTESIAN_POINT('',(7.9,-2.25,-1.55)) ;
#115931 = CARTESIAN_POINT('Origin',(1.4,-2.15,-0.903119593409422)) ;
#115932 = CARTESIAN_POINT('',(1.5,-2.23576512455516,-0.851696413713512)) ;
#115933 = CARTESIAN_POINT('Origin',(1.5,-2.15,-0.903119593409422)) ;
#115934 = CARTESIAN_POINT('',(7.9,-2.23576512455516,-0.851696413713512)) ;
#115935 = CARTESIAN_POINT('',(1.4,-2.23576512455516,-0.851696413713512)) ;
#115936 = CARTESIAN_POINT('Origin',(7.9,-2.15,-0.903119593409422)) ;
#115937 = CARTESIAN_POINT('Origin',(1.4,-3.65625,0.)) ;
#115938 = CARTESIAN_POINT('',(1.5,-2.23576512455516,0.851696413713512)) ;
#115939 = CARTESIAN_POINT('Origin',(1.5,-3.65625,0.)) ;
#115940 = CARTESIAN_POINT('',(7.9,-2.23576512455516,0.851696413713512)) ;
#115941 = CARTESIAN_POINT('',(1.4,-2.23576512455516,0.851696413713512)) ;
#115942 = CARTESIAN_POINT('Origin',(7.9,-3.65625,0.)) ;
#115943 = CARTESIAN_POINT('Origin',(1.4,-2.15,0.903119593409422)) ;
#115944 = CARTESIAN_POINT('',(1.5,-2.25,0.903119593409422)) ;
#115945 = CARTESIAN_POINT('Origin',(1.5,-2.15,0.903119593409422)) ;
#115946 = CARTESIAN_POINT('',(7.9,-2.25,0.903119593409422)) ;
#115947 = CARTESIAN_POINT('',(1.4,-2.25,0.903119593409422)) ;
#115948 = CARTESIAN_POINT('Origin',(7.9,-2.15,0.903119593409422)) ;
#115949 = CARTESIAN_POINT('Origin',(1.4,-2.25,1.55)) ;
#115950 = CARTESIAN_POINT('',(1.5,-2.25,1.55)) ;
#115951 = CARTESIAN_POINT('',(1.5,-2.25,1.55)) ;
#115952 = CARTESIAN_POINT('',(7.9,-2.25,1.55)) ;
#115953 = CARTESIAN_POINT('',(1.4,-2.25,1.55)) ;
#115954 = CARTESIAN_POINT('',(7.9,-2.25,0.903119593409422)) ;
#115955 = CARTESIAN_POINT('Origin',(1.4,-2.15,1.55)) ;
#115956 = CARTESIAN_POINT('',(1.5,-2.15,1.65)) ;
#115957 = CARTESIAN_POINT('Origin',(1.5,-2.15,1.55)) ;
#115958 = CARTESIAN_POINT('',(7.9,-2.15,1.65)) ;
#115959 = CARTESIAN_POINT('',(1.4,-2.15,1.65)) ;
#115960 = CARTESIAN_POINT('Origin',(7.9,-2.15,1.55)) ;
#115961 = CARTESIAN_POINT('Origin',(1.4,1.9,1.65)) ;
#115962 = CARTESIAN_POINT('',(1.5,1.9,1.65)) ;
#115963 = CARTESIAN_POINT('',(1.5,1.9,1.65)) ;
#115964 = CARTESIAN_POINT('',(7.9,1.9,1.65)) ;
#115965 = CARTESIAN_POINT('',(1.4,1.9,1.65)) ;
#115966 = CARTESIAN_POINT('',(7.9,-2.15,1.65)) ;
#115967 = CARTESIAN_POINT('Origin',(1.4,1.9,1.55)) ;
#115968 = CARTESIAN_POINT('',(1.5,2.,1.55)) ;
#115969 = CARTESIAN_POINT('Origin',(1.5,1.9,1.55)) ;
#115970 = CARTESIAN_POINT('',(7.9,2.,1.55)) ;
#115971 = CARTESIAN_POINT('',(1.4,2.,1.55)) ;
#115972 = CARTESIAN_POINT('Origin',(7.9,1.9,1.55)) ;
#115973 = CARTESIAN_POINT('Origin',(1.4,2.,1.55)) ;
#115974 = CARTESIAN_POINT('',(1.5,2.,0.6)) ;
#115975 = CARTESIAN_POINT('',(7.9,2.,1.55)) ;
#115976 = CARTESIAN_POINT('Origin',(1.4,2.1,0.6)) ;
#115977 = CARTESIAN_POINT('',(1.4,2.6,0.6)) ;
#115978 = CARTESIAN_POINT('',(1.4,2.4,0.4)) ;
#115979 = CARTESIAN_POINT('Origin',(1.4,2.4,0.6)) ;
#115980 = CARTESIAN_POINT('',(1.4,2.1,0.4)) ;
#115981 = CARTESIAN_POINT('',(1.4,2.1,0.4)) ;
#115982 = CARTESIAN_POINT('',(1.4,1.9,0.6)) ;
#115983 = CARTESIAN_POINT('Origin',(1.4,2.1,0.6)) ;
#115984 = CARTESIAN_POINT('',(1.4,1.9,1.55)) ;
#115985 = CARTESIAN_POINT('',(1.4,1.9,1.55)) ;
#115986 = CARTESIAN_POINT('',(1.4,-2.15,1.55)) ;
#115987 = CARTESIAN_POINT('',(1.4,-2.15,1.55)) ;
#115988 = CARTESIAN_POINT('',(1.4,-2.15,0.903119593409422)) ;
#115989 = CARTESIAN_POINT('',(1.4,-2.15,0.903119593409422)) ;
#115990 = CARTESIAN_POINT('',(1.4,-2.15,-0.903119593409422)) ;
#115991 = CARTESIAN_POINT('Origin',(1.4,-3.65625,0.)) ;
#115992 = CARTESIAN_POINT('',(1.4,-2.15,-1.55)) ;
#115993 = CARTESIAN_POINT('',(1.4,-2.15,-1.55)) ;
#115994 = CARTESIAN_POINT('',(1.4,1.9,-1.55)) ;
#115995 = CARTESIAN_POINT('',(1.4,1.9,-1.55)) ;
#115996 = CARTESIAN_POINT('',(1.4,1.9,-0.6)) ;
#115997 = CARTESIAN_POINT('',(1.4,1.9,-0.6)) ;
#115998 = CARTESIAN_POINT('',(1.4,2.1,-0.4)) ;
#115999 = CARTESIAN_POINT('Origin',(1.4,2.1,-0.6)) ;
#116000 = CARTESIAN_POINT('',(1.4,2.4,-0.4)) ;
#116001 = CARTESIAN_POINT('',(1.4,2.4,-0.4)) ;
#116002 = CARTESIAN_POINT('',(1.4,2.6,-0.6)) ;
#116003 = CARTESIAN_POINT('Origin',(1.4,2.4,-0.6)) ;
#116004 = CARTESIAN_POINT('',(1.4,2.6,-0.70857864376269)) ;
#116005 = CARTESIAN_POINT('',(1.4,2.6,-0.70857864376269)) ;
#116006 = CARTESIAN_POINT('',(1.4,3.15,-1.25857864376269)) ;
#116007 = CARTESIAN_POINT('',(1.4,3.15,-1.25857864376269)) ;
#116008 = CARTESIAN_POINT('',(1.4,3.15,1.25857864376269)) ;
#116009 = CARTESIAN_POINT('',(1.4,2.6,0.708578643762689)) ;
#116010 = CARTESIAN_POINT('',(1.4,2.6,0.708578643762689)) ;
#116011 = CARTESIAN_POINT('',(1.4,2.6,0.6)) ;
#116012 = CARTESIAN_POINT('Origin',(2.4,0.,0.)) ;
#116013 = CARTESIAN_POINT('',(2.4,0.3,0.4)) ;
#116014 = CARTESIAN_POINT('',(2.4,-0.3,0.4)) ;
#116015 = CARTESIAN_POINT('',(2.4,0.,0.4)) ;
#116016 = CARTESIAN_POINT('',(2.4,0.4,0.3)) ;
#116017 = CARTESIAN_POINT('Origin',(2.4,0.3,0.3)) ;
#116018 = CARTESIAN_POINT('',(2.4,0.4,-0.3)) ;
#116019 = CARTESIAN_POINT('',(2.4,0.4,0.)) ;
#116020 = CARTESIAN_POINT('',(2.4,0.3,-0.4)) ;
#116021 = CARTESIAN_POINT('Origin',(2.4,0.3,-0.3)) ;
#116022 = CARTESIAN_POINT('',(2.4,-0.3,-0.4)) ;
#116023 = CARTESIAN_POINT('',(2.4,0.,-0.4)) ;
#116024 = CARTESIAN_POINT('',(2.4,-0.4,-0.3)) ;
#116025 = CARTESIAN_POINT('Origin',(2.4,-0.3,-0.3)) ;
#116026 = CARTESIAN_POINT('',(2.4,-0.4,0.3)) ;
#116027 = CARTESIAN_POINT('',(2.4,-0.4,0.)) ;
#116028 = CARTESIAN_POINT('Origin',(2.4,-0.3,0.3)) ;
#116029 = CARTESIAN_POINT('Origin',(-0.899999999999999,-2.,0.6)) ;
#116030 = CARTESIAN_POINT('Origin',(-0.899999999999999,0.4,0.6)) ;
#116031 = CARTESIAN_POINT('Origin',(-0.899999999999999,-1.9,0.6)) ;
#116032 = CARTESIAN_POINT('Origin',(0.600000000000001,0.4,0.4)) ;
#116033 = CARTESIAN_POINT('Origin',(0.500000000000001,0.4,0.4)) ;
#116034 = CARTESIAN_POINT('Origin',(-0.899999999999999,0.4,0.4)) ;
#116035 = CARTESIAN_POINT('Origin',(0.500000000000001,0.4,0.4)) ;
#116036 = CARTESIAN_POINT('',(0.600000000000001,0.4,0.4)) ;
#116037 = CARTESIAN_POINT('Origin',(0.500000000000001,0.4,0.4)) ;
#116038 = CARTESIAN_POINT('Origin',(0.500000000000001,0.4,0.4)) ;
#116039 = CARTESIAN_POINT('Origin',(-0.899999999999999,-1.9,0.6)) ;
#116040 = CARTESIAN_POINT('Origin',(-0.899999999999999,-1.9,0.6)) ;
#116041 = CARTESIAN_POINT('Origin',(-0.899999999999999,-1.9,0.6)) ;
#116042 = CARTESIAN_POINT('Origin',(-0.899999999999999,0.4,0.4)) ;
#116043 = CARTESIAN_POINT('Origin',(-0.899999999999999,0.6,0.4)) ;
#116044 = CARTESIAN_POINT('Origin',(0.500000000000001,0.4,0.)) ;
#116045 = CARTESIAN_POINT('Origin',(0.500000000000001,0.4,-0.4)) ;
#116046 = CARTESIAN_POINT('',(0.600000000000001,0.4,-0.3)) ;
#116047 = CARTESIAN_POINT('Ctrl Pts',(0.595612997216081,0.370705721320403,
-0.370705721320403)) ;
#116048 = CARTESIAN_POINT('Ctrl Pts',(0.596180587760892,0.372558268494357,
-0.368855498832167)) ;
#116049 = CARTESIAN_POINT('Ctrl Pts',(0.596672461925686,0.374355839771985,
-0.36691417986631)) ;
#116050 = CARTESIAN_POINT('Ctrl Pts',(0.599015141889212,0.383869350930065,
-0.355764993656267)) ;
#116051 = CARTESIAN_POINT('Ctrl Pts',(0.599609996542525,0.390224332900451,
-0.34497260265412)) ;
#116052 = CARTESIAN_POINT('Ctrl Pts',(0.600050586298726,0.398117439141561,
-0.32233105320467)) ;
#116053 = CARTESIAN_POINT('Ctrl Pts',(0.600000000000001,0.399999999999999,
-0.311201250633524)) ;
#116054 = CARTESIAN_POINT('Ctrl Pts',(0.600000000000001,0.399999999999999,
-0.3)) ;
#116055 = CARTESIAN_POINT('',(0.600000000000001,0.4,0.)) ;
#116056 = CARTESIAN_POINT('Origin',(0.500000000000001,-4.5664044441154E-17,
0.4)) ;
#116057 = CARTESIAN_POINT('',(0.500000000000001,0.394987437106619,0.3)) ;
#116058 = CARTESIAN_POINT('Ctrl Pts',(0.500000000000001,0.394987437106619,
0.3)) ;
#116059 = CARTESIAN_POINT('Ctrl Pts',(0.505940567948951,0.3955844866499,0.3)) ;
#116060 = CARTESIAN_POINT('Ctrl Pts',(0.511931971019139,0.396132036079018,
0.300533699672039)) ;
#116061 = CARTESIAN_POINT('Ctrl Pts',(0.517829015308548,0.396618246075354,
0.301602204226276)) ;
#116062 = CARTESIAN_POINT('Ctrl Pts',(0.522982218721202,0.397043126556053,
0.30253592984289)) ;
#116063 = CARTESIAN_POINT('Ctrl Pts',(0.528062648970231,0.397421319341388,
0.303877173202936)) ;
#116064 = CARTESIAN_POINT('Ctrl Pts',(0.532978106724001,0.397751505046071,
0.305594256123367)) ;
#116065 = CARTESIAN_POINT('Ctrl Pts',(0.538583536338965,0.398128038182999,
0.307552362150451)) ;
#116066 = CARTESIAN_POINT('Ctrl Pts',(0.544059405914892,0.398447721828296,
0.310029991688954)) ;
#116067 = CARTESIAN_POINT('Ctrl Pts',(0.549268572255782,0.398712331108984,
0.312979268057107)) ;
#116068 = CARTESIAN_POINT('Ctrl Pts',(0.553856850427146,0.398945401221756,
0.315577015853159)) ;
#116069 = CARTESIAN_POINT('Ctrl Pts',(0.558237825069326,0.399135987683843,
0.318539615020013)) ;
#116070 = CARTESIAN_POINT('Ctrl Pts',(0.562333836086213,0.399290378266507,
0.32180477713583)) ;
#116071 = CARTESIAN_POINT('Ctrl Pts',(0.566990328957893,0.399465895042381,
0.325516731047696)) ;
#116072 = CARTESIAN_POINT('Ctrl Pts',(0.571349096493423,0.399597278936107,
0.329677193515201)) ;
#116073 = CARTESIAN_POINT('Ctrl Pts',(0.575296920056712,0.399694832180837,
0.334194424020656)) ;
#116074 = CARTESIAN_POINT('Ctrl Pts',(0.578744263667908,0.399780018245913,
0.338138988784921)) ;
#116075 = CARTESIAN_POINT('Ctrl Pts',(0.58187831456043,0.399839626289636,
0.342354478157894)) ;
#116076 = CARTESIAN_POINT('Ctrl Pts',(0.584648147334856,0.399882153365958,
0.346758182292707)) ;
#116077 = CARTESIAN_POINT('Ctrl Pts',(0.587839270208173,0.399931148788079,
0.351831687495501)) ;
#116078 = CARTESIAN_POINT('Ctrl Pts',(0.590595054415093,0.399958289583404,
0.357233363755549)) ;
#116079 = CARTESIAN_POINT('Ctrl Pts',(0.592838618943104,0.399974357003159,
0.362838314990607)) ;
#116080 = CARTESIAN_POINT('Ctrl Pts',(0.594777336851655,0.399988241245861,
0.367681687757603)) ;
#116081 = CARTESIAN_POINT('Ctrl Pts',(0.596334051506189,0.399993946552814,
0.372675833772872)) ;
#116082 = CARTESIAN_POINT('Ctrl Pts',(0.597488309822308,0.39999684570125,
0.377728281431604)) ;
#116083 = CARTESIAN_POINT('Ctrl Pts',(0.598804024094401,0.400000150378306,
0.383487458039442)) ;
#116084 = CARTESIAN_POINT('Ctrl Pts',(0.599612685195431,0.399999963509465,
0.389397156109403)) ;
#116085 = CARTESIAN_POINT('Ctrl Pts',(0.599890230999721,0.399999993975383,
0.395315797738928)) ;
#116086 = CARTESIAN_POINT('Ctrl Pts',(0.5999634645494,0.400000002014155,0.396877497210183)) ;
#116087 = CARTESIAN_POINT('Ctrl Pts',(0.600000000000001,0.399999999999999,
0.398439778490821)) ;
#116088 = CARTESIAN_POINT('Ctrl Pts',(0.600000000000001,0.399999999999999,
0.4)) ;
#116089 = CARTESIAN_POINT('',(0.600000000000001,0.299999999999999,0.4)) ;
#116090 = CARTESIAN_POINT('Ctrl Pts',(0.500000000000001,0.394987437106619,
0.3)) ;
#116091 = CARTESIAN_POINT('Ctrl Pts',(0.500454935589698,0.395033159853734,
0.3)) ;
#116092 = CARTESIAN_POINT('Ctrl Pts',(0.500909898680399,0.395078570329052,
0.300003104508874)) ;
#116093 = CARTESIAN_POINT('Ctrl Pts',(0.502892456245148,0.395275075889088,
0.300030166058056)) ;
#116094 = CARTESIAN_POINT('Ctrl Pts',(0.504418747482362,0.395422812032197,
0.300086014579005)) ;
#116095 = CARTESIAN_POINT('Ctrl Pts',(0.508462199543372,0.395804395682036,
0.300326718943359)) ;
#116096 = CARTESIAN_POINT('Ctrl Pts',(0.510974953343318,0.396031485023319,
0.300572060854946)) ;
#116097 = CARTESIAN_POINT('Ctrl Pts',(0.521160739721334,0.396903453186241,
0.301957205508451)) ;
#116098 = CARTESIAN_POINT('Ctrl Pts',(0.528708678528457,0.397444933153163,
0.303895782295333)) ;
#116099 = CARTESIAN_POINT('Ctrl Pts',(0.54594320635814,0.398105551684111,
0.310535360548881)) ;
#116100 = CARTESIAN_POINT('Ctrl Pts',(0.555229535466871,0.397987646678423,
0.315964641164077)) ;
#116101 = CARTESIAN_POINT('Ctrl Pts',(0.571394604995807,0.395490482808029,
0.329224486636193)) ;
#116102 = CARTESIAN_POINT('Ctrl Pts',(0.578055313702881,0.393198948698321,
0.336759254368297)) ;
#116103 = CARTESIAN_POINT('Ctrl Pts',(0.58855913220255,0.385442756729278,
0.352607766016028)) ;
#116104 = CARTESIAN_POINT('Ctrl Pts',(0.592167355639995,0.380240075126846,
0.360451734393248)) ;
#116105 = CARTESIAN_POINT('Ctrl Pts',(0.597496615531129,0.365892753466911,
0.376074478204782)) ;
#116106 = CARTESIAN_POINT('Ctrl Pts',(0.598734255154207,0.356660564300593,
0.38322725827313)) ;
#116107 = CARTESIAN_POINT('Ctrl Pts',(0.600012754681692,0.335223914398488,
0.394417694134416)) ;
#116108 = CARTESIAN_POINT('Ctrl Pts',(0.59999390055981,0.32265503709182,0.398338480634425)) ;
#116109 = CARTESIAN_POINT('Ctrl Pts',(0.600000296204999,0.306106913582345,
0.399860373652956)) ;
#116110 = CARTESIAN_POINT('Ctrl Pts',(0.600000000000001,0.303050992413431,
0.4)) ;
#116111 = CARTESIAN_POINT('Ctrl Pts',(0.600000000000001,0.299999999999999,
0.4)) ;
#116112 = CARTESIAN_POINT('',(0.600000000000001,-2.3980000991444E-17,0.4)) ;
#116113 = CARTESIAN_POINT('Origin',(0.500000000000001,-1.9,0.4)) ;
#116114 = CARTESIAN_POINT('Origin',(0.600000000000001,-1.9,0.6)) ;
#116115 = CARTESIAN_POINT('Origin',(0.500000000000001,-1.9,0.6)) ;
#116116 = CARTESIAN_POINT('Origin',(-0.899999999999999,-1.9,1.375)) ;
#116117 = CARTESIAN_POINT('Origin',(-0.899999999999999,-1.9,1.275)) ;
#116118 = CARTESIAN_POINT('Origin',(-0.899999999999999,0.6,0.5)) ;
#116119 = CARTESIAN_POINT('Origin',(-0.899999999999999,0.6,-0.4)) ;
#116120 = CARTESIAN_POINT('Origin',(0.600000000000001,0.4,-0.4)) ;
#116121 = CARTESIAN_POINT('Origin',(0.500000000000001,0.4,-0.4)) ;
#116122 = CARTESIAN_POINT('Origin',(-0.899999999999999,0.4,-0.4)) ;
#116123 = CARTESIAN_POINT('Origin',(0.500000000000001,0.4,-0.4)) ;
#116124 = CARTESIAN_POINT('Origin',(0.500000000000001,-1.9,0.6)) ;
#116125 = CARTESIAN_POINT('Origin',(0.500000000000001,-2.1,0.6)) ;
#116126 = CARTESIAN_POINT('Origin',(-0.899999999999999,-1.9,1.275)) ;
#116127 = CARTESIAN_POINT('Origin',(-1.1,-1.9,1.275)) ;
#116128 = CARTESIAN_POINT('Origin',(-0.899999999999999,-2.1,1.275)) ;
#116129 = CARTESIAN_POINT('Origin',(-0.899999999999999,0.4,-0.4)) ;
#116130 = CARTESIAN_POINT('Origin',(-0.899999999999999,0.4,-0.6)) ;
#116131 = CARTESIAN_POINT('Origin',(0.500000000000001,-2.1,0.)) ;
#116132 = CARTESIAN_POINT('Origin',(0.500000000000001,-2.1,1.275)) ;
#116133 = CARTESIAN_POINT('Origin',(0.600000000000001,-2.1,1.275)) ;
#116134 = CARTESIAN_POINT('Origin',(0.500000000000001,-2.1,1.275)) ;
#116135 = CARTESIAN_POINT('Origin',(-1.1,-4.42727195005762E-17,1.275)) ;
#116136 = CARTESIAN_POINT('',(-1.1,1.15,1.375)) ;
#116137 = CARTESIAN_POINT('',(-1.1,1.25,1.375)) ;
#116138 = CARTESIAN_POINT('Origin',(-1.1,1.15,1.275)) ;
#116139 = CARTESIAN_POINT('Origin',(-0.899999999999999,0.5,-0.6)) ;
#116140 = CARTESIAN_POINT('Origin',(-0.899999999999999,-1.9,-0.6)) ;
#116141 = CARTESIAN_POINT('Origin',(0.600000000000001,-1.9,-0.6)) ;
#116142 = CARTESIAN_POINT('Origin',(0.500000000000001,-1.9,-0.6)) ;
#116143 = CARTESIAN_POINT('Origin',(-0.899999999999999,-1.9,-0.6)) ;
#116144 = CARTESIAN_POINT('Origin',(0.500000000000001,-1.9,-0.6)) ;
#116145 = CARTESIAN_POINT('Origin',(0.500000000000001,-2.1,-0.6)) ;
#116146 = CARTESIAN_POINT('Origin',(0.500000000000001,-2.1,1.275)) ;
#116147 = CARTESIAN_POINT('Origin',(0.500000000000001,-2.1,1.275)) ;
#116148 = CARTESIAN_POINT('Origin',(-1.1,-2.9,1.475)) ;
#116149 = CARTESIAN_POINT('Origin',(-1.1,-2.9,1.475)) ;
#116150 = CARTESIAN_POINT('Origin',(-1.1,-2.9,1.475)) ;
#116151 = CARTESIAN_POINT('Origin',(-1.1,1.25,1.475)) ;
#116152 = CARTESIAN_POINT('Origin',(-1.1,1.15,1.475)) ;
#116153 = CARTESIAN_POINT('Origin',(-1.1,1.15,1.275)) ;
#116154 = CARTESIAN_POINT('',(-1.1,1.25,1.275)) ;
#116155 = CARTESIAN_POINT('Origin',(-1.1,1.15,1.275)) ;
#116156 = CARTESIAN_POINT('Origin',(-1.1,1.15,1.275)) ;
#116157 = CARTESIAN_POINT('Origin',(-0.899999999999999,-1.9,-0.6)) ;
#116158 = CARTESIAN_POINT('Origin',(-0.899999999999999,-1.9,-0.6)) ;
#116159 = CARTESIAN_POINT('Origin',(0.500000000000001,-2.1,0.)) ;
#116160 = CARTESIAN_POINT('Origin',(0.500000000000001,-2.1,-1.275)) ;
#116161 = CARTESIAN_POINT('Origin',(0.500000000000001,1.36481920536411E-16,
1.275)) ;
#116162 = CARTESIAN_POINT('Origin',(0.500000000000001,-2.9,1.275)) ;
#116163 = CARTESIAN_POINT('Origin',(-0.999999999999999,-2.9,1.475)) ;
#116164 = CARTESIAN_POINT('Origin',(0.500000000000001,-2.9,1.475)) ;
#116165 = CARTESIAN_POINT('Origin',(-1.1,1.15,1.275)) ;
#116166 = CARTESIAN_POINT('Origin',(-1.1,1.35,1.275)) ;
#116167 = CARTESIAN_POINT('Origin',(-1.1,1.15,0.)) ;
#116168 = CARTESIAN_POINT('',(-1.1,1.25,-1.275)) ;
#116169 = CARTESIAN_POINT('',(-1.1,1.25,-1.375)) ;
#116170 = CARTESIAN_POINT('Origin',(-1.1,1.15,-1.275)) ;
#116171 = CARTESIAN_POINT('Origin',(-0.899999999999999,-1.9,-0.5)) ;
#116172 = CARTESIAN_POINT('Origin',(-0.899999999999999,-1.9,-1.275)) ;
#116173 = CARTESIAN_POINT('Origin',(-0.999999999999999,-2.1,-1.275)) ;
#116174 = CARTESIAN_POINT('Origin',(0.500000000000001,-2.1,-1.275)) ;
#116175 = CARTESIAN_POINT('Origin',(-0.899999999999999,-2.1,-1.275)) ;
#116176 = CARTESIAN_POINT('Origin',(0.500000000000001,-2.1,-1.275)) ;
#116177 = CARTESIAN_POINT('Origin',(0.500000000000001,-2.1,-1.275)) ;
#116178 = CARTESIAN_POINT('Origin',(0.500000000000001,-2.9,1.275)) ;
#116179 = CARTESIAN_POINT('Origin',(0.700000000000002,-2.9,1.275)) ;
#116180 = CARTESIAN_POINT('Origin',(-1.1,1.35,-1.375)) ;
#116181 = CARTESIAN_POINT('Origin',(-1.1,1.35,-1.275)) ;
#116182 = CARTESIAN_POINT('Origin',(-1.1,1.15,-1.275)) ;
#116183 = CARTESIAN_POINT('',(-1.1,1.15,-1.375)) ;
#116184 = CARTESIAN_POINT('Origin',(-1.1,1.15,-1.275)) ;
#116185 = CARTESIAN_POINT('Origin',(-1.1,1.15,-1.275)) ;
#116186 = CARTESIAN_POINT('Origin',(-0.899999999999999,-1.9,-1.275)) ;
#116187 = CARTESIAN_POINT('Origin',(-1.1,-1.9,-1.275)) ;
#116188 = CARTESIAN_POINT('Origin',(0.500000000000001,-5.86744705109801E-17,
-1.275)) ;
#116189 = CARTESIAN_POINT('Origin',(0.500000000000001,-2.9,-1.275)) ;
#116190 = CARTESIAN_POINT('Origin',(0.700000000000002,-2.9,0.)) ;
#116191 = CARTESIAN_POINT('Origin',(0.700000000000002,-2.9,-1.275)) ;
#116192 = CARTESIAN_POINT('Origin',(-1.1,1.15,-1.275)) ;
#116193 = CARTESIAN_POINT('Origin',(-1.1,1.15,-1.475)) ;
#116194 = CARTESIAN_POINT('Origin',(-1.1,-2.39429110547967E-16,-1.275)) ;
#116195 = CARTESIAN_POINT('',(-1.1,1.25,-1.375)) ;
#116196 = CARTESIAN_POINT('Origin',(0.500000000000001,-2.9,-1.275)) ;
#116197 = CARTESIAN_POINT('Origin',(0.500000000000001,-2.9,-1.475)) ;
#116198 = CARTESIAN_POINT('Origin',(-1.1,1.25,-1.475)) ;
#116199 = CARTESIAN_POINT('Origin',(-1.1,-2.9,-1.475)) ;
#116200 = CARTESIAN_POINT('Origin',(-1.1,-2.9,-1.475)) ;
#116201 = CARTESIAN_POINT('Origin',(-1.1,-2.9,-1.475)) ;
#116202 = CARTESIAN_POINT('Origin',(-1.1,-2.9,-1.475)) ;
#116203 = CARTESIAN_POINT('Origin',(4.55,4.55,-36.79)) ;
#116204 = CARTESIAN_POINT('Origin',(4.55,4.55,-36.79)) ;
#116205 = CARTESIAN_POINT('Origin',(4.55,4.55,-36.79)) ;
#116206 = CARTESIAN_POINT('Origin',(4.55,4.55,-36.79)) ;
#116207 = CARTESIAN_POINT('Origin',(4.55,4.35,-36.79)) ;
#116208 = CARTESIAN_POINT('Origin',(4.75,4.55,-36.79)) ;
#116209 = CARTESIAN_POINT('Origin',(4.75,4.55,-36.79)) ;
#116210 = CARTESIAN_POINT('Origin',(4.35,4.35,-36.79)) ;
#116211 = CARTESIAN_POINT('Origin',(4.35,4.15,-36.79)) ;
#116212 = CARTESIAN_POINT('Origin',(4.75,4.55,-36.79)) ;
#116213 = CARTESIAN_POINT('Origin',(4.75,4.55,-36.79)) ;
#116214 = CARTESIAN_POINT('Origin',(-1.1,4.15,-36.79)) ;
#116215 = CARTESIAN_POINT('Origin',(-1.1,4.15,-36.79)) ;
#116216 = CARTESIAN_POINT('Origin',(4.75,4.35,-36.79)) ;
#116217 = CARTESIAN_POINT('Origin',(4.75,4.35,-36.79)) ;
#116218 = CARTESIAN_POINT('Origin',(-1.1,4.15,-36.79)) ;
#116219 = CARTESIAN_POINT('Origin',(-1.1,4.15,-36.79)) ;
#116220 = CARTESIAN_POINT('Origin',(4.95,4.35,-36.79)) ;
#116221 = CARTESIAN_POINT('Origin',(4.95,4.15,-36.79)) ;
#116222 = CARTESIAN_POINT('Origin',(-1.1,4.15,-36.79)) ;
#116223 = CARTESIAN_POINT('Origin',(-1.1,-2.9,-36.79)) ;
#116224 = CARTESIAN_POINT('Origin',(4.95,4.15,-36.79)) ;
#116225 = CARTESIAN_POINT('Origin',(7.9,4.15,-36.79)) ;
#116226 = CARTESIAN_POINT('Origin',(-1.1,-2.9,-36.79)) ;
#116227 = CARTESIAN_POINT('Origin',(-1.1,-2.9,-36.79)) ;
#116228 = CARTESIAN_POINT('Origin',(7.9,4.15,-36.79)) ;
#116229 = CARTESIAN_POINT('Origin',(7.9,4.15,-36.79)) ;
#116230 = CARTESIAN_POINT('Origin',(-1.1,-2.9,-36.79)) ;
#116231 = CARTESIAN_POINT('Origin',(7.9,-2.9,-36.79)) ;
#116232 = CARTESIAN_POINT('Origin',(7.9,4.15,-36.79)) ;
#116233 = CARTESIAN_POINT('Origin',(7.9,-2.9,-36.79)) ;
#116234 = CARTESIAN_POINT('Origin',(7.9,-2.9,-36.79)) ;
#116235 = CARTESIAN_POINT('Origin',(4.55,4.55,2.5)) ;
#116236 = CARTESIAN_POINT('Origin',(4.55,4.55,2.5)) ;
#116237 = CARTESIAN_POINT('Origin',(4.55,4.55,2.5)) ;
#116238 = CARTESIAN_POINT('Origin',(4.55,-2.9,2.5)) ;
#116239 = CARTESIAN_POINT('Origin',(4.55,4.35,2.5)) ;
#116240 = CARTESIAN_POINT('Origin',(7.9,4.55,2.5)) ;
#116241 = CARTESIAN_POINT('Origin',(4.75,4.55,2.5)) ;
#116242 = CARTESIAN_POINT('Origin',(4.35,4.35,2.5)) ;
#116243 = CARTESIAN_POINT('Origin',(4.35,4.15,2.5)) ;
#116244 = CARTESIAN_POINT('Origin',(4.75,4.55,2.5)) ;
#116245 = CARTESIAN_POINT('Origin',(4.75,4.55,2.5)) ;
#116246 = CARTESIAN_POINT('Origin',(7.9,4.15,2.5)) ;
#116247 = CARTESIAN_POINT('Origin',(-1.1,4.15,2.5)) ;
#116248 = CARTESIAN_POINT('Origin',(4.74999999999997,-2.89999999999999,2.5)) ;
#116249 = CARTESIAN_POINT('Origin',(4.75,4.35,2.5)) ;
#116250 = CARTESIAN_POINT('Origin',(-1.1,4.15,2.5)) ;
#116251 = CARTESIAN_POINT('Origin',(-1.1,4.15,2.5)) ;
#116252 = CARTESIAN_POINT('Origin',(4.95,4.35,2.5)) ;
#116253 = CARTESIAN_POINT('Origin',(4.95,4.15,2.5)) ;
#116254 = CARTESIAN_POINT('Origin',(-1.1,-2.9,2.5)) ;
#116255 = CARTESIAN_POINT('Origin',(-1.1,-2.9,2.5)) ;
#116256 = CARTESIAN_POINT('Origin',(7.9,4.15,2.5)) ;
#116257 = CARTESIAN_POINT('Origin',(7.9,4.15,2.5)) ;
#116258 = CARTESIAN_POINT('Origin',(-1.1,-2.9,2.5)) ;
#116259 = CARTESIAN_POINT('Origin',(-1.1,-2.9,2.5)) ;
#116260 = CARTESIAN_POINT('Origin',(7.9,4.15,2.5)) ;
#116261 = CARTESIAN_POINT('Origin',(7.9,4.15,2.5)) ;
#116262 = CARTESIAN_POINT('Origin',(7.9,-2.9,2.5)) ;
#116263 = CARTESIAN_POINT('Origin',(7.9,-2.9,2.5)) ;
#116264 = CARTESIAN_POINT('Origin',(7.9,-2.9,2.5)) ;
#116265 = CARTESIAN_POINT('Origin',(7.9,-2.9,2.5)) ;
#116266 = CARTESIAN_POINT('Origin',(7.9,-2.9,2.5)) ;
#116267 = CARTESIAN_POINT('Origin',(1.5,1.9,0.6)) ;
#116268 = CARTESIAN_POINT('Origin',(1.5,1.9,-1.55)) ;
#116269 = CARTESIAN_POINT('Origin',(1.5,1.9,-0.6)) ;
#116270 = CARTESIAN_POINT('Origin',(1.5,2.1,-0.6)) ;
#116271 = CARTESIAN_POINT('Origin',(1.5,2.1,-0.4)) ;
#116272 = CARTESIAN_POINT('Origin',(1.5,1.9,-1.55)) ;
#116273 = CARTESIAN_POINT('Origin',(1.5,1.9,-1.55)) ;
#116274 = CARTESIAN_POINT('Origin',(1.5,2.1,-0.4)) ;
#116275 = CARTESIAN_POINT('Origin',(1.5,2.4,-0.4)) ;
#116276 = CARTESIAN_POINT('Origin',(1.5,2.1,-1.55)) ;
#116277 = CARTESIAN_POINT('Origin',(1.5,-2.15,-1.55)) ;
#116278 = CARTESIAN_POINT('Origin',(1.5,2.4,-0.6)) ;
#116279 = CARTESIAN_POINT('Origin',(1.5,2.6,-0.6)) ;
#116280 = CARTESIAN_POINT('Origin',(1.5,-2.15,-1.55)) ;
#116281 = CARTESIAN_POINT('Origin',(1.5,-2.15,-1.55)) ;
#116282 = CARTESIAN_POINT('Origin',(1.5,2.6,0.6)) ;
#116283 = CARTESIAN_POINT('Origin',(1.5,2.6,-0.70857864376269)) ;
#116284 = CARTESIAN_POINT('Origin',(1.5,-2.15,0.6)) ;
#116285 = CARTESIAN_POINT('Origin',(1.5,-2.15,-0.903119593409422)) ;
#116286 = CARTESIAN_POINT('Origin',(1.5,2.6,-0.70857864376269)) ;
#116287 = CARTESIAN_POINT('Origin',(1.5,2.6,-0.70857864376269)) ;
#116288 = CARTESIAN_POINT('Origin',(1.5,-2.15,-0.903119593409422)) ;
#116289 = CARTESIAN_POINT('Origin',(1.5,-2.15,-0.903119593409422)) ;
#116290 = CARTESIAN_POINT('Origin',(1.5,1.69571067811865,0.195710678118654)) ;
#116291 = CARTESIAN_POINT('Origin',(1.5,3.15,-1.25857864376269)) ;
#116292 = CARTESIAN_POINT('Origin',(1.5,-3.65625,0.)) ;
#116293 = CARTESIAN_POINT('Origin',(1.5,-2.15,0.903119593409423)) ;
#116294 = CARTESIAN_POINT('Origin',(1.5,3.15,-1.25857864376269)) ;
#116295 = CARTESIAN_POINT('Origin',(1.5,3.15,-1.25857864376269)) ;
#116296 = CARTESIAN_POINT('Origin',(1.5,-2.15,0.903119593409422)) ;
#116297 = CARTESIAN_POINT('Origin',(1.5,-2.15,0.903119593409422)) ;
#116298 = CARTESIAN_POINT('Origin',(1.5,3.15,0.6)) ;
#116299 = CARTESIAN_POINT('Origin',(1.5,-2.15,0.6)) ;
#116300 = CARTESIAN_POINT('Origin',(1.5,-2.15,1.55)) ;
#116301 = CARTESIAN_POINT('Origin',(1.5,-2.15,1.55)) ;
#116302 = CARTESIAN_POINT('Origin',(1.5,-2.15,1.55)) ;
#116303 = CARTESIAN_POINT('Origin',(1.5,2.29571067811866,0.404289321881344)) ;
#116304 = CARTESIAN_POINT('Origin',(1.5,2.6,0.708578643762689)) ;
#116305 = CARTESIAN_POINT('Origin',(1.5,2.1,1.55)) ;
#116306 = CARTESIAN_POINT('Origin',(1.5,1.9,1.55)) ;
#116307 = CARTESIAN_POINT('Origin',(1.5,2.6,0.70857864376269)) ;
#116308 = CARTESIAN_POINT('Origin',(1.5,2.6,0.70857864376269)) ;
#116309 = CARTESIAN_POINT('Origin',(1.5,1.9,1.55)) ;
#116310 = CARTESIAN_POINT('Origin',(1.5,1.9,1.55)) ;
#116311 = CARTESIAN_POINT('Origin',(1.5,2.6,0.599999999999998)) ;
#116312 = CARTESIAN_POINT('Origin',(1.5,2.6,0.6)) ;
#116313 = CARTESIAN_POINT('Origin',(1.5,1.9,0.6)) ;
#116314 = CARTESIAN_POINT('Origin',(1.5,1.9,0.6)) ;
#116315 = CARTESIAN_POINT('Origin',(1.5,2.4,0.6)) ;
#116316 = CARTESIAN_POINT('Origin',(1.5,2.4,0.4)) ;
#116317 = CARTESIAN_POINT('Origin',(1.5,2.1,0.6)) ;
#116318 = CARTESIAN_POINT('Origin',(1.5,2.1,0.4)) ;
#116319 = CARTESIAN_POINT('Origin',(1.5,2.1,0.4)) ;
#116320 = CARTESIAN_POINT('Origin',(7.9,2.1,-0.6)) ;
#116321 = CARTESIAN_POINT('Origin',(7.9,2.4,-0.6)) ;
#116322 = CARTESIAN_POINT('Origin',(7.9,2.1,-0.6)) ;
#116323 = CARTESIAN_POINT('Origin',(7.9,2.4,-0.6)) ;
#116324 = CARTESIAN_POINT('Origin',(7.9,2.4,-0.6)) ;
#116325 = CARTESIAN_POINT('Origin',(7.9,2.1,-0.6)) ;
#116326 = CARTESIAN_POINT('Origin',(7.9,2.1,-0.6)) ;
#116327 = CARTESIAN_POINT('Origin',(7.9,2.4,-0.6)) ;
#116328 = CARTESIAN_POINT('Origin',(7.9,2.4,-0.70857864376269)) ;
#116329 = CARTESIAN_POINT('Origin',(7.9,2.1,-0.6)) ;
#116330 = CARTESIAN_POINT('Origin',(7.9,2.1,-1.55)) ;
#116331 = CARTESIAN_POINT('Origin',(7.9,2.6,-0.70857864376269)) ;
#116332 = CARTESIAN_POINT('Origin',(7.9,2.45857864376269,-0.85)) ;
#116333 = CARTESIAN_POINT('Origin',(7.9,1.9,-1.55)) ;
#116334 = CARTESIAN_POINT('Origin',(7.9,1.9,-1.75)) ;
#116335 = CARTESIAN_POINT('Origin',(7.9,2.45857864376269,-0.85)) ;
#116336 = CARTESIAN_POINT('Origin',(7.9,1.9,-1.75)) ;
#116337 = CARTESIAN_POINT('Origin',(7.9,-2.15,-1.75)) ;
#116338 = CARTESIAN_POINT('Origin',(7.9,-2.15,-1.55)) ;
#116339 = CARTESIAN_POINT('Origin',(7.9,-2.35,-1.55)) ;
#116340 = CARTESIAN_POINT('Origin',(7.9,3.35,-1.25857864376269)) ;
#116341 = CARTESIAN_POINT('Origin',(7.9,3.35,1.25857864376269)) ;
#116342 = CARTESIAN_POINT('Origin',(7.9,-2.35,-0.903119593409422)) ;
#116343 = CARTESIAN_POINT('Origin',(7.9,-2.35,-0.903119593409422)) ;
#116344 = CARTESIAN_POINT('Origin',(7.9,3.15,1.25857864376269)) ;
#116345 = CARTESIAN_POINT('Origin',(7.9,3.00857864376269,1.4)) ;
#116346 = CARTESIAN_POINT('Origin',(7.9,-2.15,-0.903119593409422)) ;
#116347 = CARTESIAN_POINT('Origin',(7.9,-2.32153024911032,-0.800273234017602)) ;
#116348 = CARTESIAN_POINT('Origin',(7.9,3.00857864376269,1.4)) ;
#116349 = CARTESIAN_POINT('Origin',(7.9,2.45857864376269,0.849999999999999)) ;
#116350 = CARTESIAN_POINT('Origin',(7.9,-3.65625,0.)) ;
#116351 = CARTESIAN_POINT('Origin',(7.9,-2.32153024911032,0.800273234017602)) ;
#116352 = CARTESIAN_POINT('Origin',(7.9,2.6,0.70857864376269)) ;
#116353 = CARTESIAN_POINT('Origin',(7.9,2.4,0.70857864376269)) ;
#116354 = CARTESIAN_POINT('Origin',(7.9,-2.15,0.903119593409422)) ;
#116355 = CARTESIAN_POINT('Origin',(7.9,-2.35,0.903119593409422)) ;
#116356 = CARTESIAN_POINT('Origin',(7.9,2.4,0.70857864376269)) ;
#116357 = CARTESIAN_POINT('Origin',(7.9,2.4,0.600000000000001)) ;
#116358 = CARTESIAN_POINT('Origin',(7.9,-2.35,1.55)) ;
#116359 = CARTESIAN_POINT('Origin',(7.9,-2.35,1.55)) ;
#116360 = CARTESIAN_POINT('Origin',(7.9,2.4,0.6)) ;
#116361 = CARTESIAN_POINT('Origin',(7.9,2.4,0.6)) ;
#116362 = CARTESIAN_POINT('Origin',(7.9,-2.15,1.55)) ;
#116363 = CARTESIAN_POINT('Origin',(7.9,-2.15,1.75)) ;
#116364 = CARTESIAN_POINT('Origin',(7.9,2.4,0.6)) ;
#116365 = CARTESIAN_POINT('Origin',(7.9,2.1,0.6)) ;
#116366 = CARTESIAN_POINT('Origin',(7.9,1.9,1.75)) ;
#116367 = CARTESIAN_POINT('Origin',(7.9,1.9,1.75)) ;
#116368 = CARTESIAN_POINT('Origin',(7.9,2.1,0.6)) ;
#116369 = CARTESIAN_POINT('Origin',(7.9,2.1,0.6)) ;
#116370 = CARTESIAN_POINT('Origin',(7.9,1.9,1.55)) ;
#116371 = CARTESIAN_POINT('Origin',(7.9,2.1,1.55)) ;
#116372 = CARTESIAN_POINT('Origin',(7.9,2.1,1.55)) ;
#116373 = CARTESIAN_POINT('Origin',(-0.4,-0.600000000000001,0.4)) ;
#116374 = CARTESIAN_POINT('',(-0.4,-0.600000000000001,0.3)) ;
#116375 = CARTESIAN_POINT('',(-0.4,-0.600000000000001,-0.3)) ;
#116376 = CARTESIAN_POINT('',(-0.4,-0.600000000000001,0.4)) ;
#116377 = CARTESIAN_POINT('',(-0.4,-6.05857864376269,-0.3)) ;
#116378 = CARTESIAN_POINT('',(-0.4,-0.600000000000001,-0.3)) ;
#116379 = CARTESIAN_POINT('',(-0.4,-6.05857864376269,0.3)) ;
#116380 = CARTESIAN_POINT('',(-0.4,-6.05857864376269,0.4)) ;
#116381 = CARTESIAN_POINT('',(-0.4,-0.600000000000001,0.3)) ;
#116382 = CARTESIAN_POINT('Origin',(-0.4,-6.1,0.4)) ;
#116383 = CARTESIAN_POINT('',(-0.129289321881346,-6.37071067811866,-0.0585786437626899)) ;
#116384 = CARTESIAN_POINT('',(-0.129289321881346,-6.37071067811866,0.0585786437626899)) ;
#116385 = CARTESIAN_POINT('',(-0.129289321881346,-6.37071067811866,0.4)) ;
#116386 = CARTESIAN_POINT('',(-0.370710678118655,-6.12928932188134,0.3)) ;
#116387 = CARTESIAN_POINT('',(-0.423570226039552,-6.07642977396045,0.352859547920897)) ;
#116388 = CARTESIAN_POINT('',(-0.370710678118655,-6.12928932188134,-0.3)) ;
#116389 = CARTESIAN_POINT('',(-0.370710678118655,-6.12928932188134,0.4)) ;
#116390 = CARTESIAN_POINT('',(-0.156903559372884,-6.34309644062712,-0.0861928812542289)) ;
#116391 = CARTESIAN_POINT('Origin',(-0.1,-6.4,0.4)) ;
#116392 = CARTESIAN_POINT('',(0.0585786437626908,-6.4,-0.0585786437626897)) ;
#116393 = CARTESIAN_POINT('',(0.0585786437626908,-6.4,0.0585786437626898)) ;
#116394 = CARTESIAN_POINT('',(0.0585786437626908,-6.4,0.4)) ;
#116395 = CARTESIAN_POINT('',(-0.0585786437626908,-6.4,0.0585786437626898)) ;
#116396 = CARTESIAN_POINT('',(-0.1,-6.4,0.0585786437626898)) ;
#116397 = CARTESIAN_POINT('',(-0.0585786437626908,-6.4,-0.0585786437626897)) ;
#116398 = CARTESIAN_POINT('',(-0.0585786437626908,-6.4,0.4)) ;
#116399 = CARTESIAN_POINT('',(-0.1,-6.4,-0.0585786437626898)) ;
#116400 = CARTESIAN_POINT('Origin',(0.1,-6.4,0.4)) ;
#116401 = CARTESIAN_POINT('',(0.370710678118655,-6.12928932188134,-0.3)) ;
#116402 = CARTESIAN_POINT('',(0.370710678118655,-6.12928932188134,0.299999999999999)) ;
#116403 = CARTESIAN_POINT('',(0.370710678118655,-6.12928932188134,0.4)) ;
#116404 = CARTESIAN_POINT('',(0.129289321881346,-6.37071067811866,0.0585786437626892)) ;
#116405 = CARTESIAN_POINT('',(0.223570226039552,-6.27642977396045,0.152859547920897)) ;
#116406 = CARTESIAN_POINT('',(0.129289321881346,-6.37071067811866,-0.05857864376269)) ;
#116407 = CARTESIAN_POINT('',(0.129289321881346,-6.37071067811866,0.4)) ;
#116408 = CARTESIAN_POINT('',(-0.0430964406271149,-6.54309644062712,0.113807118745771)) ;
#116409 = CARTESIAN_POINT('Origin',(0.4,-6.1,0.4)) ;
#116410 = CARTESIAN_POINT('',(0.4,-6.05857864376269,0.3)) ;
#116411 = CARTESIAN_POINT('',(0.4,-6.05857864376269,-0.3)) ;
#116412 = CARTESIAN_POINT('',(0.4,-6.05857864376269,0.4)) ;
#116413 = CARTESIAN_POINT('',(0.4,-0.6,-0.3)) ;
#116414 = CARTESIAN_POINT('',(0.4,-6.1,-0.3)) ;
#116415 = CARTESIAN_POINT('',(0.4,-0.6,0.3)) ;
#116416 = CARTESIAN_POINT('',(0.4,-0.6,0.4)) ;
#116417 = CARTESIAN_POINT('',(0.4,-6.05857864376269,0.3)) ;
#116418 = CARTESIAN_POINT('Origin',(0.6,-0.600000000000001,0.4)) ;
#116419 = CARTESIAN_POINT('',(0.3,-6.05857864376269,0.4)) ;
#116420 = CARTESIAN_POINT('',(0.3,-0.6,0.4)) ;
#116421 = CARTESIAN_POINT('',(0.3,-0.6,0.4)) ;
#116422 = CARTESIAN_POINT('Origin',(0.6,-0.6,0.4)) ;
#116423 = CARTESIAN_POINT('',(-0.3,-0.600000000000001,0.4)) ;
#116424 = CARTESIAN_POINT('Origin',(0.6,-0.600000000000001,0.4)) ;
#116425 = CARTESIAN_POINT('',(-0.3,-6.05857864376269,0.4)) ;
#116426 = CARTESIAN_POINT('',(-0.3,-0.600000000000001,0.4)) ;
#116427 = CARTESIAN_POINT('',(0.4,-6.05857864376269,0.4)) ;
#116428 = CARTESIAN_POINT('Origin',(0.6,-0.600000000000001,-0.4)) ;
#116429 = CARTESIAN_POINT('',(-0.3,-6.05857864376269,-0.4)) ;
#116430 = CARTESIAN_POINT('',(-0.3,-0.600000000000001,-0.4)) ;
#116431 = CARTESIAN_POINT('',(-0.3,-0.600000000000001,-0.4)) ;
#116432 = CARTESIAN_POINT('Origin',(0.6,-0.600000000000001,-0.4)) ;
#116433 = CARTESIAN_POINT('',(0.3,-0.6,-0.4)) ;
#116434 = CARTESIAN_POINT('Origin',(0.6,-0.6,-0.4)) ;
#116435 = CARTESIAN_POINT('',(0.3,-6.05857864376269,-0.4)) ;
#116436 = CARTESIAN_POINT('',(0.3,-0.600000000000001,-0.4)) ;
#116437 = CARTESIAN_POINT('',(0.6,-6.05857864376269,-0.4)) ;
#116438 = CARTESIAN_POINT('Origin',(0.6,-0.600000000000001,0.4)) ;
#116439 = CARTESIAN_POINT('Origin',(0.6,-0.600000000000001,-0.3)) ;
#116440 = CARTESIAN_POINT('Origin',(0.6,-0.600000000000001,0.3)) ;
#116441 = CARTESIAN_POINT('Origin',(0.6,-0.6,0.4)) ;
#116442 = CARTESIAN_POINT('Origin',(0.6,-0.6,-0.3)) ;
#116443 = CARTESIAN_POINT('Origin',(0.6,-0.6,0.3)) ;
#116444 = CARTESIAN_POINT('Origin',(7.,0.1,0.4)) ;
#116445 = CARTESIAN_POINT('',(6.72928932188135,0.370710678118655,-0.3)) ;
#116446 = CARTESIAN_POINT('',(6.72928932188135,0.370710678118655,0.3)) ;
#116447 = CARTESIAN_POINT('',(6.72928932188135,0.370710678118655,0.4)) ;
#116448 = CARTESIAN_POINT('',(6.97071067811866,0.129289321881346,0.0585786437626902)) ;
#116449 = CARTESIAN_POINT('',(6.87642977396045,0.223570226039552,0.152859547920897)) ;
#116450 = CARTESIAN_POINT('',(6.97071067811866,0.129289321881346,-0.0585786437626903)) ;
#116451 = CARTESIAN_POINT('',(6.97071067811866,0.129289321881346,0.4)) ;
#116452 = CARTESIAN_POINT('',(7.14309644062712,-0.043096440627115,0.11380711874577)) ;
#116453 = CARTESIAN_POINT('Origin',(6.7,0.400000000000001,0.4)) ;
#116454 = CARTESIAN_POINT('',(6.65857864376269,0.400000000000001,0.3)) ;
#116455 = CARTESIAN_POINT('',(6.65857864376269,0.400000000000001,-0.3)) ;
#116456 = CARTESIAN_POINT('',(6.65857864376269,0.400000000000001,0.4)) ;
#116457 = CARTESIAN_POINT('',(6.7,0.400000000000001,-0.3)) ;
#116458 = CARTESIAN_POINT('',(6.65857864376269,0.400000000000001,0.3)) ;
#116459 = CARTESIAN_POINT('Origin',(0.6,-0.4,0.4)) ;
#116460 = CARTESIAN_POINT('',(6.65857864376269,-0.400000000000001,-0.3)) ;
#116461 = CARTESIAN_POINT('',(0.6,-0.4,-0.3)) ;
#116462 = CARTESIAN_POINT('',(6.65857864376269,-0.400000000000001,0.3)) ;
#116463 = CARTESIAN_POINT('',(6.65857864376269,-0.400000000000001,0.4)) ;
#116464 = CARTESIAN_POINT('',(2.4,-0.4,0.3)) ;
#116465 = CARTESIAN_POINT('Origin',(6.7,-0.400000000000001,0.4)) ;
#116466 = CARTESIAN_POINT('',(6.97071067811866,-0.129289321881346,-0.0585786437626903)) ;
#116467 = CARTESIAN_POINT('',(6.97071067811866,-0.129289321881346,0.0585786437626901)) ;
#116468 = CARTESIAN_POINT('',(6.97071067811866,-0.129289321881346,0.4)) ;
#116469 = CARTESIAN_POINT('',(6.72928932188135,-0.370710678118655,0.3)) ;
#116470 = CARTESIAN_POINT('',(6.67642977396045,-0.423570226039552,0.352859547920897)) ;
#116471 = CARTESIAN_POINT('',(6.72928932188135,-0.370710678118655,-0.3)) ;
#116472 = CARTESIAN_POINT('',(6.72928932188135,-0.370710678118655,0.4)) ;
#116473 = CARTESIAN_POINT('',(6.94309644062712,-0.156903559372885,-0.0861928812542298)) ;
#116474 = CARTESIAN_POINT('Origin',(7.,-0.1,0.4)) ;
#116475 = CARTESIAN_POINT('',(7.,-0.0585786437626909,0.0585786437626901)) ;
#116476 = CARTESIAN_POINT('',(7.,-0.0585786437626909,-0.05857864376269)) ;
#116477 = CARTESIAN_POINT('',(7.,-0.0585786437626909,0.4)) ;
#116478 = CARTESIAN_POINT('',(7.,0.0585786437626909,-0.05857864376269)) ;
#116479 = CARTESIAN_POINT('',(7.,-0.1,-0.05857864376269)) ;
#116480 = CARTESIAN_POINT('',(7.,0.0585786437626909,0.05857864376269)) ;
#116481 = CARTESIAN_POINT('',(7.,0.0585786437626909,0.4)) ;
#116482 = CARTESIAN_POINT('',(7.,-0.1,0.0585786437626901)) ;
#116483 = CARTESIAN_POINT('Origin',(0.6,-0.600000000000001,0.4)) ;
#116484 = CARTESIAN_POINT('',(6.65857864376269,-0.300000000000001,0.4)) ;
#116485 = CARTESIAN_POINT('',(6.65857864376269,0.300000000000001,0.4)) ;
#116486 = CARTESIAN_POINT('',(6.65857864376269,-0.399999999999999,0.4)) ;
#116487 = CARTESIAN_POINT('',(2.4,0.3,0.4)) ;
#116488 = CARTESIAN_POINT('',(6.65857864376269,-0.300000000000001,0.4)) ;
#116489 = CARTESIAN_POINT('Origin',(0.6,-0.600000000000001,-0.4)) ;
#116490 = CARTESIAN_POINT('',(6.65857864376269,0.300000000000001,-0.4)) ;
#116491 = CARTESIAN_POINT('',(0.6,0.299999999999999,-0.4)) ;
#116492 = CARTESIAN_POINT('',(6.65857864376269,-0.300000000000001,-0.4)) ;
#116493 = CARTESIAN_POINT('',(6.65857864376269,-0.6,-0.4)) ;
#116494 = CARTESIAN_POINT('',(0.6,-0.3,-0.4)) ;
#116495 = CARTESIAN_POINT('Origin',(0.4,-6.4,-0.0999999999999988)) ;
#116496 = CARTESIAN_POINT('',(-0.0585786437626909,-6.37071067811866,-0.129289321881344)) ;
#116497 = CARTESIAN_POINT('',(-0.3,-6.12928932188134,-0.370710678118655)) ;
#116498 = CARTESIAN_POINT('',(0.113807118745769,-6.54309644062712,0.0430964406271166)) ;
#116499 = CARTESIAN_POINT('',(0.3,-6.12928932188134,-0.370710678118655)) ;
#116500 = CARTESIAN_POINT('',(0.4,-6.12928932188134,-0.370710678118654)) ;
#116501 = CARTESIAN_POINT('',(0.058578643762691,-6.37071067811866,-0.129289321881344)) ;
#116502 = CARTESIAN_POINT('',(0.152859547920897,-6.27642977396045,-0.22357022603955)) ;
#116503 = CARTESIAN_POINT('',(0.4,-6.37071067811866,-0.129289321881344)) ;
#116504 = CARTESIAN_POINT('Origin',(0.4,-6.1,0.4)) ;
#116505 = CARTESIAN_POINT('',(0.0585786437626902,-6.37071067811866,0.129289321881344)) ;
#116506 = CARTESIAN_POINT('',(0.299999999999999,-6.12928932188134,0.370710678118655)) ;
#116507 = CARTESIAN_POINT('',(0.352859547920896,-6.07642977396045,0.423570226039552)) ;
#116508 = CARTESIAN_POINT('',(-0.3,-6.12928932188134,0.370710678118655)) ;
#116509 = CARTESIAN_POINT('',(0.4,-6.12928932188134,0.370710678118654)) ;
#116510 = CARTESIAN_POINT('',(-0.058578643762691,-6.37071067811866,0.129289321881344)) ;
#116511 = CARTESIAN_POINT('',(-0.086192881254231,-6.34309644062712,0.156903559372885)) ;
#116512 = CARTESIAN_POINT('',(0.4,-6.37071067811866,0.129289321881344)) ;
#116513 = CARTESIAN_POINT('Origin',(6.7,-0.399999999999999,-0.4)) ;
#116514 = CARTESIAN_POINT('',(6.97071067811866,-0.0585786437626912,-0.129289321881345)) ;
#116515 = CARTESIAN_POINT('',(6.72928932188135,-0.300000000000001,-0.370710678118655)) ;
#116516 = CARTESIAN_POINT('',(6.67642977396045,-0.352859547920897,-0.423570226039551)) ;
#116517 = CARTESIAN_POINT('',(6.72928932188135,0.300000000000001,-0.370710678118655)) ;
#116518 = CARTESIAN_POINT('',(6.72928932188135,-0.399999999999999,-0.370710678118655)) ;
#116519 = CARTESIAN_POINT('',(6.97071067811866,0.0585786437626912,-0.129289321881345)) ;
#116520 = CARTESIAN_POINT('',(6.94309644062712,0.0861928812542309,-0.156903559372884)) ;
#116521 = CARTESIAN_POINT('',(6.97071067811866,-0.4,-0.129289321881345)) ;
#116522 = CARTESIAN_POINT('Origin',(7.,-0.399999999999999,0.0999999999999993)) ;
#116523 = CARTESIAN_POINT('',(6.97071067811866,0.0585786437626911,0.129289321881345)) ;
#116524 = CARTESIAN_POINT('',(6.72928932188135,0.300000000000001,0.370710678118655)) ;
#116525 = CARTESIAN_POINT('',(7.14309644062712,-0.113807118745769,-0.043096440627116)) ;
#116526 = CARTESIAN_POINT('',(6.72928932188135,-0.300000000000001,0.370710678118655)) ;
#116527 = CARTESIAN_POINT('',(6.72928932188135,-0.399999999999999,0.370710678118655)) ;
#116528 = CARTESIAN_POINT('',(6.97071067811866,-0.0585786437626911,0.129289321881345)) ;
#116529 = CARTESIAN_POINT('',(6.87642977396045,-0.152859547920897,0.223570226039551)) ;
#116530 = CARTESIAN_POINT('',(6.97071067811866,-0.399999999999999,0.129289321881345)) ;
#116531 = CARTESIAN_POINT('Origin',(-0.11380711874577,-6.47238576250846,0.113807118745771)) ;
#116532 = CARTESIAN_POINT('Origin',(0.3,-6.05857864376269,-0.3)) ;
#116533 = CARTESIAN_POINT('Origin',(0.058578643762691,-6.3,-0.0585786437626897)) ;
#116534 = CARTESIAN_POINT('Origin',(0.3,-6.05857864376269,0.4)) ;
#116535 = CARTESIAN_POINT('Origin',(0.3,-6.05857864376269,-0.3)) ;
#116536 = CARTESIAN_POINT('Origin',(0.3,-6.05857864376269,0.3)) ;
#116537 = CARTESIAN_POINT('Origin',(0.0585786437626908,-6.3,-0.0585786437626897)) ;
#116538 = CARTESIAN_POINT('Origin',(0.0585786437626908,-6.3,-0.0585786437626897)) ;
#116539 = CARTESIAN_POINT('Origin',(0.0585786437626908,-6.3,-0.05857864376269)) ;
#116540 = CARTESIAN_POINT('Origin',(0.152859547920897,-6.20571909584179,0.152859547920897)) ;
#116541 = CARTESIAN_POINT('Origin',(0.3,-6.05857864376269,0.3)) ;
#116542 = CARTESIAN_POINT('Origin',(0.0585786437626908,-6.3,0.0585786437626892)) ;
#116543 = CARTESIAN_POINT('Origin',(0.0585786437626908,-6.3,0.4)) ;
#116544 = CARTESIAN_POINT('Origin',(0.0585786437626908,-6.3,0.0585786437626898)) ;
#116545 = CARTESIAN_POINT('Origin',(0.4,-6.3,-0.0585786437626897)) ;
#116546 = CARTESIAN_POINT('Origin',(-0.0585786437626909,-6.3,-0.0585786437626897)) ;
#116547 = CARTESIAN_POINT('Origin',(0.0585786437626908,-6.3,0.0585786437626898)) ;
#116548 = CARTESIAN_POINT('Origin',(0.0585786437626902,-6.3,0.0585786437626897)) ;
#116549 = CARTESIAN_POINT('Origin',(-0.0585786437626908,-6.3,-0.0585786437626897)) ;
#116550 = CARTESIAN_POINT('Origin',(-0.0585786437626908,-6.3,-0.0585786437626899)) ;
#116551 = CARTESIAN_POINT('Origin',(-0.0585786437626908,-6.3,-0.0585786437626897)) ;
#116552 = CARTESIAN_POINT('Origin',(-0.1,-6.3,0.0585786437626898)) ;
#116553 = CARTESIAN_POINT('Origin',(-0.0585786437626908,-6.3,0.0585786437626898)) ;
#116554 = CARTESIAN_POINT('Origin',(-0.0585786437626908,-6.3,0.4)) ;
#116555 = CARTESIAN_POINT('Origin',(-0.0585786437626908,-6.3,0.0585786437626899)) ;
#116556 = CARTESIAN_POINT('Origin',(-0.0861928812542298,-6.27238576250846,
-0.0861928812542288)) ;
#116557 = CARTESIAN_POINT('Origin',(-0.3,-6.05857864376269,-0.3)) ;
#116558 = CARTESIAN_POINT('Origin',(-0.0585786437626909,-6.3,0.0585786437626898)) ;
#116559 = CARTESIAN_POINT('Origin',(-0.058578643762691,-6.3,0.0585786437626897)) ;
#116560 = CARTESIAN_POINT('Origin',(-0.3,-6.05857864376269,0.4)) ;
#116561 = CARTESIAN_POINT('Origin',(-0.3,-6.05857864376269,-0.3)) ;
#116562 = CARTESIAN_POINT('Origin',(-0.3,-6.05857864376269,0.3)) ;
#116563 = CARTESIAN_POINT('Origin',(-0.352859547920897,-6.00571909584179,
0.352859547920897)) ;
#116564 = CARTESIAN_POINT('Origin',(-0.3,-6.05857864376269,0.3)) ;
#116565 = CARTESIAN_POINT('Origin',(7.07238576250846,-0.11380711874577,0.113807118745771)) ;
#116566 = CARTESIAN_POINT('Origin',(6.65857864376269,0.300000000000001,-0.3)) ;
#116567 = CARTESIAN_POINT('Origin',(6.9,0.0585786437626912,-0.05857864376269)) ;
#116568 = CARTESIAN_POINT('Origin',(6.65857864376269,0.300000000000001,0.4)) ;
#116569 = CARTESIAN_POINT('Origin',(6.65857864376269,0.300000000000001,-0.3)) ;
#116570 = CARTESIAN_POINT('Origin',(6.65857864376269,0.300000000000001,0.3)) ;
#116571 = CARTESIAN_POINT('Origin',(6.9,0.0585786437626909,-0.05857864376269)) ;
#116572 = CARTESIAN_POINT('Origin',(6.9,0.0585786437626909,-0.05857864376269)) ;
#116573 = CARTESIAN_POINT('Origin',(6.9,0.0585786437626909,-0.0585786437626903)) ;
#116574 = CARTESIAN_POINT('Origin',(6.80571909584179,0.152859547920897,0.152859547920897)) ;
#116575 = CARTESIAN_POINT('Origin',(6.65857864376269,0.300000000000001,0.3)) ;
#116576 = CARTESIAN_POINT('Origin',(6.9,0.0585786437626909,0.0585786437626902)) ;
#116577 = CARTESIAN_POINT('Origin',(6.9,0.0585786437626909,0.4)) ;
#116578 = CARTESIAN_POINT('Origin',(6.9,0.0585786437626909,0.05857864376269)) ;
#116579 = CARTESIAN_POINT('Origin',(6.9,-0.1,-0.05857864376269)) ;
#116580 = CARTESIAN_POINT('Origin',(6.9,-0.0585786437626912,-0.05857864376269)) ;
#116581 = CARTESIAN_POINT('Origin',(6.9,0.0585786437626909,0.05857864376269)) ;
#116582 = CARTESIAN_POINT('Origin',(6.9,0.0585786437626911,0.05857864376269)) ;
#116583 = CARTESIAN_POINT('Origin',(6.9,-0.058578643762691,-0.0585786437626901)) ;
#116584 = CARTESIAN_POINT('Origin',(6.9,-0.0585786437626909,-0.0585786437626903)) ;
#116585 = CARTESIAN_POINT('Origin',(6.9,-0.0585786437626909,-0.05857864376269)) ;
#116586 = CARTESIAN_POINT('Origin',(6.9,-0.399999999999999,0.0585786437626901)) ;
#116587 = CARTESIAN_POINT('Origin',(6.9,-0.0585786437626909,0.0585786437626901)) ;
#116588 = CARTESIAN_POINT('Origin',(6.9,-0.0585786437626909,0.4)) ;
#116589 = CARTESIAN_POINT('Origin',(6.9,-0.0585786437626909,0.0585786437626901)) ;
#116590 = CARTESIAN_POINT('Origin',(6.87238576250846,-0.0861928812542305,
-0.0861928812542296)) ;
#116591 = CARTESIAN_POINT('Origin',(6.65857864376269,-0.300000000000001,-0.3)) ;
#116592 = CARTESIAN_POINT('Origin',(6.9,-0.058578643762691,0.0585786437626901)) ;
#116593 = CARTESIAN_POINT('Origin',(6.9,-0.0585786437626911,0.05857864376269)) ;
#116594 = CARTESIAN_POINT('Origin',(6.65857864376269,-0.300000000000001,0.4)) ;
#116595 = CARTESIAN_POINT('Origin',(6.65857864376269,-0.300000000000001,-0.3)) ;
#116596 = CARTESIAN_POINT('Origin',(6.65857864376269,-0.300000000000001,0.3)) ;
#116597 = CARTESIAN_POINT('Origin',(6.60571909584179,-0.352859547920898,0.352859547920897)) ;
#116598 = CARTESIAN_POINT('Origin',(6.65857864376269,-0.300000000000001,0.3)) ;
#116599 = CARTESIAN_POINT('Origin',(0.6,-0.6,-0.3)) ;
#116600 = CARTESIAN_POINT('Origin',(0.3,-0.6,-0.3)) ;
#116601 = CARTESIAN_POINT('Origin',(0.3,-6.1,-0.3)) ;
#116602 = CARTESIAN_POINT('Origin',(0.3,-6.05857864376269,-0.3)) ;
#116603 = CARTESIAN_POINT('Origin',(0.3,-6.05857864376269,-0.3)) ;
#116604 = CARTESIAN_POINT('Origin',(0.3,-6.05857864376269,-0.3)) ;
#116605 = CARTESIAN_POINT('Origin',(0.4,-6.05857864376269,-0.3)) ;
#116606 = CARTESIAN_POINT('Origin',(-0.3,-6.05857864376269,-0.3)) ;
#116607 = CARTESIAN_POINT('Origin',(-0.3,-6.05857864376269,-0.3)) ;
#116608 = CARTESIAN_POINT('Origin',(-0.3,-6.05857864376269,-0.3)) ;
#116609 = CARTESIAN_POINT('Origin',(-0.3,-0.600000000000001,-0.3)) ;
#116610 = CARTESIAN_POINT('Origin',(-0.3,-0.600000000000001,-0.3)) ;
#116611 = CARTESIAN_POINT('Origin',(0.6,-0.600000000000001,-0.3)) ;
#116612 = CARTESIAN_POINT('Origin',(0.6,-0.600000000000001,0.3)) ;
#116613 = CARTESIAN_POINT('Origin',(-0.3,-0.600000000000001,0.3)) ;
#116614 = CARTESIAN_POINT('Origin',(-0.3,-0.600000000000001,0.3)) ;
#116615 = CARTESIAN_POINT('Origin',(-0.3,-6.05857864376269,0.3)) ;
#116616 = CARTESIAN_POINT('Origin',(-0.3,-6.05857864376269,0.3)) ;
#116617 = CARTESIAN_POINT('Origin',(-0.3,-6.05857864376269,0.3)) ;
#116618 = CARTESIAN_POINT('Origin',(0.4,-6.05857864376269,0.3)) ;
#116619 = CARTESIAN_POINT('Origin',(0.299999999999999,-6.05857864376269,0.3)) ;
#116620 = CARTESIAN_POINT('Origin',(0.3,-6.05857864376269,0.3)) ;
#116621 = CARTESIAN_POINT('Origin',(0.3,-6.05857864376269,0.3)) ;
#116622 = CARTESIAN_POINT('Origin',(0.3,-0.600000000000001,0.3)) ;
#116623 = CARTESIAN_POINT('Origin',(0.3,-0.6,0.3)) ;
#116624 = CARTESIAN_POINT('Origin',(0.6,-0.6,0.3)) ;
#116625 = CARTESIAN_POINT('Origin',(6.7,0.300000000000001,-0.3)) ;
#116626 = CARTESIAN_POINT('Origin',(6.65857864376269,0.300000000000001,-0.3)) ;
#116627 = CARTESIAN_POINT('Origin',(6.65857864376269,0.300000000000001,-0.3)) ;
#116628 = CARTESIAN_POINT('Origin',(6.65857864376269,0.300000000000001,-0.3)) ;
#116629 = CARTESIAN_POINT('Origin',(6.65857864376269,-0.399999999999999,-0.3)) ;
#116630 = CARTESIAN_POINT('Origin',(6.65857864376269,-0.300000000000001,-0.3)) ;
#116631 = CARTESIAN_POINT('Origin',(6.65857864376269,-0.300000000000001,-0.3)) ;
#116632 = CARTESIAN_POINT('Origin',(6.65857864376269,-0.300000000000001,-0.3)) ;
#116633 = CARTESIAN_POINT('Origin',(0.6,-0.3,-0.3)) ;
#116634 = CARTESIAN_POINT('Origin',(0.6,0.299999999999999,0.3)) ;
#116635 = CARTESIAN_POINT('Origin',(6.65857864376269,0.300000000000001,0.3)) ;
#116636 = CARTESIAN_POINT('Origin',(6.65857864376269,0.300000000000001,0.3)) ;
#116637 = CARTESIAN_POINT('Origin',(6.65857864376269,0.300000000000001,0.3)) ;
#116638 = CARTESIAN_POINT('Origin',(6.65857864376269,-0.399999999999999,0.3)) ;
#116639 = CARTESIAN_POINT('Origin',(6.65857864376269,-0.300000000000001,0.3)) ;
#116640 = CARTESIAN_POINT('Origin',(0.6,-0.3,0.3)) ;
#116641 = CARTESIAN_POINT('Origin',(6.65857864376269,-0.300000000000001,0.3)) ;
#116642 = CARTESIAN_POINT('Origin',(6.65857864376269,-0.300000000000001,0.3)) ;
#116643 = CARTESIAN_POINT('Origin',(-0.999999999999999,-1.59070596587277E-16,
-34.29)) ;
#116644 = CARTESIAN_POINT('',(-0.999999999999999,-1.9,-33.69)) ;
#116645 = CARTESIAN_POINT('',(-0.999999999999999,-1.9,-33.015)) ;
#116646 = CARTESIAN_POINT('',(-0.999999999999999,-1.9,-32.915)) ;
#116647 = CARTESIAN_POINT('',(-0.999999999999999,1.15,-33.015)) ;
#116648 = CARTESIAN_POINT('',(-0.999999999999999,-2.89663358890162E-17,-33.015)) ;
#116649 = CARTESIAN_POINT('',(-0.999999999999999,1.15,-35.565)) ;
#116650 = CARTESIAN_POINT('',(-0.999999999999999,1.15,-34.29)) ;
#116651 = CARTESIAN_POINT('',(-0.999999999999999,-1.9,-35.565)) ;
#116652 = CARTESIAN_POINT('',(-0.999999999999999,-2.24122726936407E-16,-35.565)) ;
#116653 = CARTESIAN_POINT('',(-0.999999999999999,-1.9,-34.89)) ;
#116654 = CARTESIAN_POINT('',(-0.999999999999999,-1.9,-34.79)) ;
#116655 = CARTESIAN_POINT('',(-0.999999999999999,0.4,-34.89)) ;
#116656 = CARTESIAN_POINT('',(-0.999999999999999,0.5,-34.89)) ;
#116657 = CARTESIAN_POINT('',(-0.999999999999999,0.6,-34.69)) ;
#116658 = CARTESIAN_POINT('Origin',(-0.999999999999999,0.4,-34.69)) ;
#116659 = CARTESIAN_POINT('',(-0.999999999999999,0.6,-33.89)) ;
#116660 = CARTESIAN_POINT('',(-0.999999999999999,0.6,-33.79)) ;
#116661 = CARTESIAN_POINT('',(-0.999999999999999,0.4,-33.69)) ;
#116662 = CARTESIAN_POINT('Origin',(-0.999999999999999,0.4,-33.89)) ;
#116663 = CARTESIAN_POINT('',(-0.999999999999999,-2.,-33.69)) ;
#116664 = CARTESIAN_POINT('Origin',(-0.999999999999999,-1.59070596587277E-16,
-30.48)) ;
#116665 = CARTESIAN_POINT('',(-0.999999999999999,-1.9,-29.88)) ;
#116666 = CARTESIAN_POINT('',(-0.999999999999999,-1.9,-29.205)) ;
#116667 = CARTESIAN_POINT('',(-0.999999999999999,-1.9,-29.105)) ;
#116668 = CARTESIAN_POINT('',(-0.999999999999999,1.15,-29.205)) ;
#116669 = CARTESIAN_POINT('',(-0.999999999999999,-2.89663358890162E-17,-29.205)) ;
#116670 = CARTESIAN_POINT('',(-0.999999999999999,1.15,-31.755)) ;
#116671 = CARTESIAN_POINT('',(-0.999999999999999,1.15,-30.48)) ;
#116672 = CARTESIAN_POINT('',(-0.999999999999999,-1.9,-31.755)) ;
#116673 = CARTESIAN_POINT('',(-0.999999999999999,-2.24122726936407E-16,-31.755)) ;
#116674 = CARTESIAN_POINT('',(-0.999999999999999,-1.9,-31.08)) ;
#116675 = CARTESIAN_POINT('',(-0.999999999999999,-1.9,-30.98)) ;
#116676 = CARTESIAN_POINT('',(-0.999999999999999,0.4,-31.08)) ;
#116677 = CARTESIAN_POINT('',(-0.999999999999999,0.5,-31.08)) ;
#116678 = CARTESIAN_POINT('',(-0.999999999999999,0.6,-30.88)) ;
#116679 = CARTESIAN_POINT('Origin',(-0.999999999999999,0.4,-30.88)) ;
#116680 = CARTESIAN_POINT('',(-0.999999999999999,0.6,-30.08)) ;
#116681 = CARTESIAN_POINT('',(-0.999999999999999,0.6,-29.98)) ;
#116682 = CARTESIAN_POINT('',(-0.999999999999999,0.4,-29.88)) ;
#116683 = CARTESIAN_POINT('Origin',(-0.999999999999999,0.4,-30.08)) ;
#116684 = CARTESIAN_POINT('',(-0.999999999999999,-2.,-29.88)) ;
#116685 = CARTESIAN_POINT('Origin',(-0.999999999999999,-1.59070596587277E-16,
-26.67)) ;
#116686 = CARTESIAN_POINT('',(-0.999999999999999,-1.9,-26.07)) ;
#116687 = CARTESIAN_POINT('',(-0.999999999999999,-1.9,-25.395)) ;
#116688 = CARTESIAN_POINT('',(-0.999999999999999,-1.9,-25.295)) ;
#116689 = CARTESIAN_POINT('',(-0.999999999999999,1.15,-25.395)) ;
#116690 = CARTESIAN_POINT('',(-0.999999999999999,-2.89663358890162E-17,-25.395)) ;
#116691 = CARTESIAN_POINT('',(-0.999999999999999,1.15,-27.945)) ;
#116692 = CARTESIAN_POINT('',(-0.999999999999999,1.15,-26.67)) ;
#116693 = CARTESIAN_POINT('',(-0.999999999999999,-1.9,-27.945)) ;
#116694 = CARTESIAN_POINT('',(-0.999999999999999,-2.24122726936407E-16,-27.945)) ;
#116695 = CARTESIAN_POINT('',(-0.999999999999999,-1.9,-27.27)) ;
#116696 = CARTESIAN_POINT('',(-0.999999999999999,-1.9,-27.17)) ;
#116697 = CARTESIAN_POINT('',(-0.999999999999999,0.4,-27.27)) ;
#116698 = CARTESIAN_POINT('',(-0.999999999999999,0.5,-27.27)) ;
#116699 = CARTESIAN_POINT('',(-0.999999999999999,0.6,-27.07)) ;
#116700 = CARTESIAN_POINT('Origin',(-0.999999999999999,0.4,-27.07)) ;
#116701 = CARTESIAN_POINT('',(-0.999999999999999,0.6,-26.27)) ;
#116702 = CARTESIAN_POINT('',(-0.999999999999999,0.6,-26.17)) ;
#116703 = CARTESIAN_POINT('',(-0.999999999999999,0.4,-26.07)) ;
#116704 = CARTESIAN_POINT('Origin',(-0.999999999999999,0.4,-26.27)) ;
#116705 = CARTESIAN_POINT('',(-0.999999999999999,-2.,-26.07)) ;
#116706 = CARTESIAN_POINT('Origin',(-0.999999999999999,-1.59070596587277E-16,
-22.86)) ;
#116707 = CARTESIAN_POINT('',(-0.999999999999999,-1.9,-22.26)) ;
#116708 = CARTESIAN_POINT('',(-0.999999999999999,-1.9,-21.585)) ;
#116709 = CARTESIAN_POINT('',(-0.999999999999999,-1.9,-21.485)) ;
#116710 = CARTESIAN_POINT('',(-0.999999999999999,1.15,-21.585)) ;
#116711 = CARTESIAN_POINT('',(-0.999999999999999,-2.89663358890162E-17,-21.585)) ;
#116712 = CARTESIAN_POINT('',(-0.999999999999999,1.15,-24.135)) ;
#116713 = CARTESIAN_POINT('',(-0.999999999999999,1.15,-22.86)) ;
#116714 = CARTESIAN_POINT('',(-0.999999999999999,-1.9,-24.135)) ;
#116715 = CARTESIAN_POINT('',(-0.999999999999999,-2.24122726936407E-16,-24.135)) ;
#116716 = CARTESIAN_POINT('',(-0.999999999999999,-1.9,-23.46)) ;
#116717 = CARTESIAN_POINT('',(-0.999999999999999,-1.9,-23.36)) ;
#116718 = CARTESIAN_POINT('',(-0.999999999999999,0.4,-23.46)) ;
#116719 = CARTESIAN_POINT('',(-0.999999999999999,0.5,-23.46)) ;
#116720 = CARTESIAN_POINT('',(-0.999999999999999,0.6,-23.26)) ;
#116721 = CARTESIAN_POINT('Origin',(-0.999999999999999,0.4,-23.26)) ;
#116722 = CARTESIAN_POINT('',(-0.999999999999999,0.6,-22.46)) ;
#116723 = CARTESIAN_POINT('',(-0.999999999999999,0.6,-22.36)) ;
#116724 = CARTESIAN_POINT('',(-0.999999999999999,0.4,-22.26)) ;
#116725 = CARTESIAN_POINT('Origin',(-0.999999999999999,0.4,-22.46)) ;
#116726 = CARTESIAN_POINT('',(-0.999999999999999,-2.,-22.26)) ;
#116727 = CARTESIAN_POINT('Origin',(-0.999999999999999,-1.59070596587277E-16,
-19.05)) ;
#116728 = CARTESIAN_POINT('',(-0.999999999999999,-1.9,-18.45)) ;
#116729 = CARTESIAN_POINT('',(-0.999999999999999,-1.9,-17.775)) ;
#116730 = CARTESIAN_POINT('',(-0.999999999999999,-1.9,-17.675)) ;
#116731 = CARTESIAN_POINT('',(-0.999999999999999,1.15,-17.775)) ;
#116732 = CARTESIAN_POINT('',(-0.999999999999999,-2.89663358890162E-17,-17.775)) ;
#116733 = CARTESIAN_POINT('',(-0.999999999999999,1.15,-20.325)) ;
#116734 = CARTESIAN_POINT('',(-0.999999999999999,1.15,-19.05)) ;
#116735 = CARTESIAN_POINT('',(-0.999999999999999,-1.9,-20.325)) ;
#116736 = CARTESIAN_POINT('',(-0.999999999999999,-2.24122726936407E-16,-20.325)) ;
#116737 = CARTESIAN_POINT('',(-0.999999999999999,-1.9,-19.65)) ;
#116738 = CARTESIAN_POINT('',(-0.999999999999999,-1.9,-19.55)) ;
#116739 = CARTESIAN_POINT('',(-0.999999999999999,0.4,-19.65)) ;
#116740 = CARTESIAN_POINT('',(-0.999999999999999,0.5,-19.65)) ;
#116741 = CARTESIAN_POINT('',(-0.999999999999999,0.6,-19.45)) ;
#116742 = CARTESIAN_POINT('Origin',(-0.999999999999999,0.4,-19.45)) ;
#116743 = CARTESIAN_POINT('',(-0.999999999999999,0.6,-18.65)) ;
#116744 = CARTESIAN_POINT('',(-0.999999999999999,0.6,-18.55)) ;
#116745 = CARTESIAN_POINT('',(-0.999999999999999,0.4,-18.45)) ;
#116746 = CARTESIAN_POINT('Origin',(-0.999999999999999,0.4,-18.65)) ;
#116747 = CARTESIAN_POINT('',(-0.999999999999999,-2.,-18.45)) ;
#116748 = CARTESIAN_POINT('Origin',(-0.999999999999999,-1.59070596587277E-16,
-15.24)) ;
#116749 = CARTESIAN_POINT('',(-0.999999999999999,-1.9,-14.64)) ;
#116750 = CARTESIAN_POINT('',(-0.999999999999999,-1.9,-13.965)) ;
#116751 = CARTESIAN_POINT('',(-0.999999999999999,-1.9,-13.865)) ;
#116752 = CARTESIAN_POINT('',(-0.999999999999999,1.15,-13.965)) ;
#116753 = CARTESIAN_POINT('',(-0.999999999999999,-2.8966335889016E-17,-13.965)) ;
#116754 = CARTESIAN_POINT('',(-0.999999999999999,1.15,-16.515)) ;
#116755 = CARTESIAN_POINT('',(-0.999999999999999,1.15,-15.24)) ;
#116756 = CARTESIAN_POINT('',(-0.999999999999999,-1.9,-16.515)) ;
#116757 = CARTESIAN_POINT('',(-0.999999999999999,-2.24122726936407E-16,-16.515)) ;
#116758 = CARTESIAN_POINT('',(-0.999999999999999,-1.9,-15.84)) ;
#116759 = CARTESIAN_POINT('',(-0.999999999999999,-1.9,-15.74)) ;
#116760 = CARTESIAN_POINT('',(-0.999999999999999,0.4,-15.84)) ;
#116761 = CARTESIAN_POINT('',(-0.999999999999999,0.5,-15.84)) ;
#116762 = CARTESIAN_POINT('',(-0.999999999999999,0.6,-15.64)) ;
#116763 = CARTESIAN_POINT('Origin',(-0.999999999999999,0.4,-15.64)) ;
#116764 = CARTESIAN_POINT('',(-0.999999999999999,0.6,-14.84)) ;
#116765 = CARTESIAN_POINT('',(-0.999999999999999,0.6,-14.74)) ;
#116766 = CARTESIAN_POINT('',(-0.999999999999999,0.4,-14.64)) ;
#116767 = CARTESIAN_POINT('Origin',(-0.999999999999999,0.4,-14.84)) ;
#116768 = CARTESIAN_POINT('',(-0.999999999999999,-2.,-14.64)) ;
#116769 = CARTESIAN_POINT('Origin',(-0.999999999999999,-1.59070596587277E-16,
-11.43)) ;
#116770 = CARTESIAN_POINT('',(-0.999999999999999,-1.9,-10.83)) ;
#116771 = CARTESIAN_POINT('',(-0.999999999999999,-1.9,-10.155)) ;
#116772 = CARTESIAN_POINT('',(-0.999999999999999,-1.9,-10.055)) ;
#116773 = CARTESIAN_POINT('',(-0.999999999999999,1.15,-10.155)) ;
#116774 = CARTESIAN_POINT('',(-0.999999999999999,-2.8966335889016E-17,-10.155)) ;
#116775 = CARTESIAN_POINT('',(-0.999999999999999,1.15,-12.705)) ;
#116776 = CARTESIAN_POINT('',(-0.999999999999999,1.15,-11.43)) ;
#116777 = CARTESIAN_POINT('',(-0.999999999999999,-1.9,-12.705)) ;
#116778 = CARTESIAN_POINT('',(-0.999999999999999,-2.24122726936407E-16,-12.705)) ;
#116779 = CARTESIAN_POINT('',(-0.999999999999999,-1.9,-12.03)) ;
#116780 = CARTESIAN_POINT('',(-0.999999999999999,-1.9,-11.93)) ;
#116781 = CARTESIAN_POINT('',(-0.999999999999999,0.4,-12.03)) ;
#116782 = CARTESIAN_POINT('',(-0.999999999999999,0.5,-12.03)) ;
#116783 = CARTESIAN_POINT('',(-0.999999999999999,0.6,-11.83)) ;
#116784 = CARTESIAN_POINT('Origin',(-0.999999999999999,0.4,-11.83)) ;
#116785 = CARTESIAN_POINT('',(-0.999999999999999,0.6,-11.03)) ;
#116786 = CARTESIAN_POINT('',(-0.999999999999999,0.6,-10.93)) ;
#116787 = CARTESIAN_POINT('',(-0.999999999999999,0.4,-10.83)) ;
#116788 = CARTESIAN_POINT('Origin',(-0.999999999999999,0.4,-11.03)) ;
#116789 = CARTESIAN_POINT('',(-0.999999999999999,-2.,-10.83)) ;
#116790 = CARTESIAN_POINT('Origin',(-0.999999999999999,-1.59070596587277E-16,
-7.62)) ;
#116791 = CARTESIAN_POINT('',(-0.999999999999999,-1.9,-7.02)) ;
#116792 = CARTESIAN_POINT('',(-0.999999999999999,-1.9,-6.345)) ;
#116793 = CARTESIAN_POINT('',(-0.999999999999999,-1.9,-6.245)) ;
#116794 = CARTESIAN_POINT('',(-0.999999999999999,1.15,-6.345)) ;
#116795 = CARTESIAN_POINT('',(-0.999999999999999,-2.89663358890161E-17,-6.345)) ;
#116796 = CARTESIAN_POINT('',(-0.999999999999999,1.15,-8.895)) ;
#116797 = CARTESIAN_POINT('',(-0.999999999999999,1.15,-7.62)) ;
#116798 = CARTESIAN_POINT('',(-0.999999999999999,-1.9,-8.895)) ;
#116799 = CARTESIAN_POINT('',(-0.999999999999999,-2.24122726936407E-16,-8.895)) ;
#116800 = CARTESIAN_POINT('',(-0.999999999999999,-1.9,-8.22)) ;
#116801 = CARTESIAN_POINT('',(-0.999999999999999,-1.9,-8.12)) ;
#116802 = CARTESIAN_POINT('',(-0.999999999999999,0.4,-8.22)) ;
#116803 = CARTESIAN_POINT('',(-0.999999999999999,0.5,-8.22)) ;
#116804 = CARTESIAN_POINT('',(-0.999999999999999,0.6,-8.02)) ;
#116805 = CARTESIAN_POINT('Origin',(-0.999999999999999,0.4,-8.02)) ;
#116806 = CARTESIAN_POINT('',(-0.999999999999999,0.6,-7.22)) ;
#116807 = CARTESIAN_POINT('',(-0.999999999999999,0.6,-7.12)) ;
#116808 = CARTESIAN_POINT('',(-0.999999999999999,0.4,-7.02)) ;
#116809 = CARTESIAN_POINT('Origin',(-0.999999999999999,0.4,-7.22)) ;
#116810 = CARTESIAN_POINT('',(-0.999999999999999,-2.,-7.02)) ;
#116811 = CARTESIAN_POINT('Origin',(-0.999999999999999,-1.59070596587277E-16,
-3.81)) ;
#116812 = CARTESIAN_POINT('',(-0.999999999999999,-1.9,-3.21)) ;
#116813 = CARTESIAN_POINT('',(-0.999999999999999,-1.9,-2.535)) ;
#116814 = CARTESIAN_POINT('',(-0.999999999999999,-1.9,-2.435)) ;
#116815 = CARTESIAN_POINT('',(-0.999999999999999,1.15,-2.535)) ;
#116816 = CARTESIAN_POINT('',(-0.999999999999999,-2.89663358890161E-17,-2.535)) ;
#116817 = CARTESIAN_POINT('',(-0.999999999999999,1.15,-5.085)) ;
#116818 = CARTESIAN_POINT('',(-0.999999999999999,1.15,-3.81)) ;
#116819 = CARTESIAN_POINT('',(-0.999999999999999,-1.9,-5.085)) ;
#116820 = CARTESIAN_POINT('',(-0.999999999999999,-2.24122726936407E-16,-5.085)) ;
#116821 = CARTESIAN_POINT('',(-0.999999999999999,-1.9,-4.41)) ;
#116822 = CARTESIAN_POINT('',(-0.999999999999999,-1.9,-4.31)) ;
#116823 = CARTESIAN_POINT('',(-0.999999999999999,0.4,-4.41)) ;
#116824 = CARTESIAN_POINT('',(-0.999999999999999,0.5,-4.41)) ;
#116825 = CARTESIAN_POINT('',(-0.999999999999999,0.6,-4.21)) ;
#116826 = CARTESIAN_POINT('Origin',(-0.999999999999999,0.4,-4.21)) ;
#116827 = CARTESIAN_POINT('',(-0.999999999999999,0.6,-3.41)) ;
#116828 = CARTESIAN_POINT('',(-0.999999999999999,0.6,-3.31)) ;
#116829 = CARTESIAN_POINT('',(-0.999999999999999,0.4,-3.21)) ;
#116830 = CARTESIAN_POINT('Origin',(-0.999999999999999,0.4,-3.41)) ;
#116831 = CARTESIAN_POINT('',(-0.999999999999999,-2.,-3.21)) ;
#116832 = CARTESIAN_POINT('Origin',(0.600000000000001,-2.,-4.31)) ;
#116833 = CARTESIAN_POINT('',(0.500000000000001,-2.,-4.41)) ;
#116834 = CARTESIAN_POINT('',(-0.899999999999999,-2.,-4.41)) ;
#116835 = CARTESIAN_POINT('',(0.600000000000001,-2.,-4.41)) ;
#116836 = CARTESIAN_POINT('',(-0.899999999999999,-2.,-5.085)) ;
#116837 = CARTESIAN_POINT('',(-0.899999999999999,-2.,-5.185)) ;
#116838 = CARTESIAN_POINT('',(0.500000000000001,-2.,-5.085)) ;
#116839 = CARTESIAN_POINT('',(0.600000000000001,-2.,-5.085)) ;
#116840 = CARTESIAN_POINT('',(0.500000000000001,-2.,-4.31)) ;
#116841 = CARTESIAN_POINT('Origin',(0.600000000000001,0.5,-4.31)) ;
#116842 = CARTESIAN_POINT('',(-0.899999999999999,0.4,-4.31)) ;
#116843 = CARTESIAN_POINT('',(-0.999999999999999,0.4,-4.31)) ;
#116844 = CARTESIAN_POINT('',(-0.899999999999999,-1.9,-4.31)) ;
#116845 = CARTESIAN_POINT('',(-0.899999999999999,-2.,-4.31)) ;
#116846 = CARTESIAN_POINT('',(0.600000000000001,-1.9,-4.31)) ;
#116847 = CARTESIAN_POINT('Origin',(0.600000000000001,0.5,-3.31)) ;
#116848 = CARTESIAN_POINT('',(0.500000000000001,0.5,-3.41)) ;
#116849 = CARTESIAN_POINT('',(-0.899999999999999,0.5,-3.41)) ;
#116850 = CARTESIAN_POINT('',(-0.999999999999999,0.5,-3.41)) ;
#116851 = CARTESIAN_POINT('',(-0.899999999999999,0.5,-4.21)) ;
#116852 = CARTESIAN_POINT('',(-0.899999999999999,0.5,-4.31)) ;
#116853 = CARTESIAN_POINT('',(0.500000000000001,0.5,-4.21)) ;
#116854 = CARTESIAN_POINT('',(0.600000000000001,0.5,-4.21)) ;
#116855 = CARTESIAN_POINT('',(0.500000000000001,0.5,-3.31)) ;
#116856 = CARTESIAN_POINT('Origin',(0.600000000000001,-2.,-3.31)) ;
#116857 = CARTESIAN_POINT('',(0.500000000000001,-1.9,-3.31)) ;
#116858 = CARTESIAN_POINT('',(-0.899999999999999,-1.9,-3.31)) ;
#116859 = CARTESIAN_POINT('',(0.600000000000001,-1.9,-3.31)) ;
#116860 = CARTESIAN_POINT('',(-0.899999999999999,0.4,-3.31)) ;
#116861 = CARTESIAN_POINT('',(-0.899999999999999,0.5,-3.31)) ;
#116862 = CARTESIAN_POINT('',(0.500000000000001,0.4,-3.31)) ;
#116863 = CARTESIAN_POINT('',(0.600000000000001,0.4,-3.31)) ;
#116864 = CARTESIAN_POINT('',(0.500000000000001,-2.,-3.31)) ;
#116865 = CARTESIAN_POINT('Origin',(0.600000000000001,-2.,-2.435)) ;
#116866 = CARTESIAN_POINT('',(0.500000000000001,-2.,-2.535)) ;
#116867 = CARTESIAN_POINT('',(-0.899999999999999,-2.,-2.535)) ;
#116868 = CARTESIAN_POINT('',(-0.999999999999999,-2.,-2.535)) ;
#116869 = CARTESIAN_POINT('',(-0.899999999999999,-2.,-3.21)) ;
#116870 = CARTESIAN_POINT('',(-0.899999999999999,-2.,-3.31)) ;
#116871 = CARTESIAN_POINT('',(0.500000000000001,-2.,-3.21)) ;
#116872 = CARTESIAN_POINT('',(0.600000000000001,-2.,-3.21)) ;
#116873 = CARTESIAN_POINT('',(0.500000000000001,-2.,-2.435)) ;
#116874 = CARTESIAN_POINT('Origin',(0.600000000000001,-2.,-8.12)) ;
#116875 = CARTESIAN_POINT('',(0.500000000000001,-2.,-8.22)) ;
#116876 = CARTESIAN_POINT('',(-0.899999999999999,-2.,-8.22)) ;
#116877 = CARTESIAN_POINT('',(0.600000000000001,-2.,-8.22)) ;
#116878 = CARTESIAN_POINT('',(-0.899999999999999,-2.,-8.895)) ;
#116879 = CARTESIAN_POINT('',(-0.899999999999999,-2.,-8.995)) ;
#116880 = CARTESIAN_POINT('',(0.500000000000001,-2.,-8.895)) ;
#116881 = CARTESIAN_POINT('',(0.600000000000001,-2.,-8.895)) ;
#116882 = CARTESIAN_POINT('',(0.500000000000001,-2.,-8.12)) ;
#116883 = CARTESIAN_POINT('Origin',(0.600000000000001,0.5,-8.12)) ;
#116884 = CARTESIAN_POINT('',(-0.899999999999999,0.4,-8.12)) ;
#116885 = CARTESIAN_POINT('',(-0.999999999999999,0.4,-8.12)) ;
#116886 = CARTESIAN_POINT('',(-0.899999999999999,-1.9,-8.12)) ;
#116887 = CARTESIAN_POINT('',(-0.899999999999999,-2.,-8.12)) ;
#116888 = CARTESIAN_POINT('',(0.600000000000001,-1.9,-8.12)) ;
#116889 = CARTESIAN_POINT('Origin',(0.600000000000001,0.5,-7.12)) ;
#116890 = CARTESIAN_POINT('',(0.500000000000001,0.5,-7.22)) ;
#116891 = CARTESIAN_POINT('',(-0.899999999999999,0.5,-7.22)) ;
#116892 = CARTESIAN_POINT('',(-0.999999999999999,0.5,-7.22)) ;
#116893 = CARTESIAN_POINT('',(-0.899999999999999,0.5,-8.02)) ;
#116894 = CARTESIAN_POINT('',(-0.899999999999999,0.5,-8.12)) ;
#116895 = CARTESIAN_POINT('',(0.500000000000001,0.5,-8.02)) ;
#116896 = CARTESIAN_POINT('',(0.600000000000001,0.5,-8.02)) ;
#116897 = CARTESIAN_POINT('',(0.500000000000001,0.5,-7.12)) ;
#116898 = CARTESIAN_POINT('Origin',(0.600000000000001,-2.,-7.12)) ;
#116899 = CARTESIAN_POINT('',(0.500000000000001,-1.9,-7.12)) ;
#116900 = CARTESIAN_POINT('',(-0.899999999999999,-1.9,-7.12)) ;
#116901 = CARTESIAN_POINT('',(0.600000000000001,-1.9,-7.12)) ;
#116902 = CARTESIAN_POINT('',(-0.899999999999999,0.4,-7.12)) ;
#116903 = CARTESIAN_POINT('',(-0.899999999999999,0.5,-7.12)) ;
#116904 = CARTESIAN_POINT('',(0.500000000000001,0.4,-7.12)) ;
#116905 = CARTESIAN_POINT('',(0.600000000000001,0.4,-7.12)) ;
#116906 = CARTESIAN_POINT('',(0.500000000000001,-2.,-7.12)) ;
#116907 = CARTESIAN_POINT('Origin',(0.600000000000001,-2.,-6.245)) ;
#116908 = CARTESIAN_POINT('',(0.500000000000001,-2.,-6.345)) ;
#116909 = CARTESIAN_POINT('',(-0.899999999999999,-2.,-6.345)) ;
#116910 = CARTESIAN_POINT('',(-0.999999999999999,-2.,-6.345)) ;
#116911 = CARTESIAN_POINT('',(-0.899999999999999,-2.,-7.02)) ;
#116912 = CARTESIAN_POINT('',(-0.899999999999999,-2.,-7.12)) ;
#116913 = CARTESIAN_POINT('',(0.500000000000001,-2.,-7.02)) ;
#116914 = CARTESIAN_POINT('',(0.600000000000001,-2.,-7.02)) ;
#116915 = CARTESIAN_POINT('',(0.500000000000001,-2.,-6.245)) ;
#116916 = CARTESIAN_POINT('Origin',(0.600000000000001,-2.,-11.93)) ;
#116917 = CARTESIAN_POINT('',(0.500000000000001,-2.,-12.03)) ;
#116918 = CARTESIAN_POINT('',(-0.899999999999999,-2.,-12.03)) ;
#116919 = CARTESIAN_POINT('',(0.600000000000001,-2.,-12.03)) ;
#116920 = CARTESIAN_POINT('',(-0.899999999999999,-2.,-12.705)) ;
#116921 = CARTESIAN_POINT('',(-0.899999999999999,-2.,-12.805)) ;
#116922 = CARTESIAN_POINT('',(0.500000000000001,-2.,-12.705)) ;
#116923 = CARTESIAN_POINT('',(0.600000000000001,-2.,-12.705)) ;
#116924 = CARTESIAN_POINT('',(0.500000000000001,-2.,-11.93)) ;
#116925 = CARTESIAN_POINT('Origin',(0.600000000000001,0.5,-11.93)) ;
#116926 = CARTESIAN_POINT('',(-0.899999999999999,0.4,-11.93)) ;
#116927 = CARTESIAN_POINT('',(-0.999999999999999,0.4,-11.93)) ;
#116928 = CARTESIAN_POINT('',(-0.899999999999999,-1.9,-11.93)) ;
#116929 = CARTESIAN_POINT('',(-0.899999999999999,-2.,-11.93)) ;
#116930 = CARTESIAN_POINT('',(0.600000000000001,-1.9,-11.93)) ;
#116931 = CARTESIAN_POINT('Origin',(0.600000000000001,0.5,-10.93)) ;
#116932 = CARTESIAN_POINT('',(0.500000000000001,0.5,-11.03)) ;
#116933 = CARTESIAN_POINT('',(-0.899999999999999,0.5,-11.03)) ;
#116934 = CARTESIAN_POINT('',(-0.999999999999999,0.5,-11.03)) ;
#116935 = CARTESIAN_POINT('',(-0.899999999999999,0.5,-11.83)) ;
#116936 = CARTESIAN_POINT('',(-0.899999999999999,0.5,-11.93)) ;
#116937 = CARTESIAN_POINT('',(0.500000000000001,0.5,-11.83)) ;
#116938 = CARTESIAN_POINT('',(0.600000000000001,0.5,-11.83)) ;
#116939 = CARTESIAN_POINT('',(0.500000000000001,0.5,-10.93)) ;
#116940 = CARTESIAN_POINT('Origin',(0.600000000000001,-2.,-10.93)) ;
#116941 = CARTESIAN_POINT('',(0.500000000000001,-1.9,-10.93)) ;
#116942 = CARTESIAN_POINT('',(-0.899999999999999,-1.9,-10.93)) ;
#116943 = CARTESIAN_POINT('',(0.600000000000001,-1.9,-10.93)) ;
#116944 = CARTESIAN_POINT('',(-0.899999999999999,0.4,-10.93)) ;
#116945 = CARTESIAN_POINT('',(-0.899999999999999,0.5,-10.93)) ;
#116946 = CARTESIAN_POINT('',(0.500000000000001,0.4,-10.93)) ;
#116947 = CARTESIAN_POINT('',(0.600000000000001,0.4,-10.93)) ;
#116948 = CARTESIAN_POINT('',(0.500000000000001,-2.,-10.93)) ;
#116949 = CARTESIAN_POINT('Origin',(0.600000000000001,-2.,-10.055)) ;
#116950 = CARTESIAN_POINT('',(0.500000000000001,-2.,-10.155)) ;
#116951 = CARTESIAN_POINT('',(-0.899999999999999,-2.,-10.155)) ;
#116952 = CARTESIAN_POINT('',(-0.999999999999999,-2.,-10.155)) ;
#116953 = CARTESIAN_POINT('',(-0.899999999999999,-2.,-10.83)) ;
#116954 = CARTESIAN_POINT('',(-0.899999999999999,-2.,-10.93)) ;
#116955 = CARTESIAN_POINT('',(0.500000000000001,-2.,-10.83)) ;
#116956 = CARTESIAN_POINT('',(0.600000000000001,-2.,-10.83)) ;
#116957 = CARTESIAN_POINT('',(0.500000000000001,-2.,-10.055)) ;
#116958 = CARTESIAN_POINT('Origin',(0.600000000000001,-2.,-15.74)) ;
#116959 = CARTESIAN_POINT('',(0.500000000000001,-2.,-15.84)) ;
#116960 = CARTESIAN_POINT('',(-0.899999999999999,-2.,-15.84)) ;
#116961 = CARTESIAN_POINT('',(0.600000000000001,-2.,-15.84)) ;
#116962 = CARTESIAN_POINT('',(-0.899999999999999,-2.,-16.515)) ;
#116963 = CARTESIAN_POINT('',(-0.899999999999999,-2.,-16.615)) ;
#116964 = CARTESIAN_POINT('',(0.500000000000001,-2.,-16.515)) ;
#116965 = CARTESIAN_POINT('',(0.600000000000001,-2.,-16.515)) ;
#116966 = CARTESIAN_POINT('',(0.500000000000001,-2.,-15.74)) ;
#116967 = CARTESIAN_POINT('Origin',(0.600000000000001,0.5,-15.74)) ;
#116968 = CARTESIAN_POINT('',(-0.899999999999999,0.4,-15.74)) ;
#116969 = CARTESIAN_POINT('',(-0.999999999999999,0.4,-15.74)) ;
#116970 = CARTESIAN_POINT('',(-0.899999999999999,-1.9,-15.74)) ;
#116971 = CARTESIAN_POINT('',(-0.899999999999999,-2.,-15.74)) ;
#116972 = CARTESIAN_POINT('',(0.600000000000001,-1.9,-15.74)) ;
#116973 = CARTESIAN_POINT('Origin',(0.600000000000001,0.5,-14.74)) ;
#116974 = CARTESIAN_POINT('',(0.500000000000001,0.5,-14.84)) ;
#116975 = CARTESIAN_POINT('',(-0.899999999999999,0.5,-14.84)) ;
#116976 = CARTESIAN_POINT('',(-0.999999999999999,0.5,-14.84)) ;
#116977 = CARTESIAN_POINT('',(-0.899999999999999,0.5,-15.64)) ;
#116978 = CARTESIAN_POINT('',(-0.899999999999999,0.5,-15.74)) ;
#116979 = CARTESIAN_POINT('',(0.500000000000001,0.5,-15.64)) ;
#116980 = CARTESIAN_POINT('',(0.600000000000001,0.5,-15.64)) ;
#116981 = CARTESIAN_POINT('',(0.500000000000001,0.5,-14.74)) ;
#116982 = CARTESIAN_POINT('Origin',(0.600000000000001,-2.,-14.74)) ;
#116983 = CARTESIAN_POINT('',(0.500000000000001,-1.9,-14.74)) ;
#116984 = CARTESIAN_POINT('',(-0.899999999999999,-1.9,-14.74)) ;
#116985 = CARTESIAN_POINT('',(0.600000000000001,-1.9,-14.74)) ;
#116986 = CARTESIAN_POINT('',(-0.899999999999999,0.4,-14.74)) ;
#116987 = CARTESIAN_POINT('',(-0.899999999999999,0.5,-14.74)) ;
#116988 = CARTESIAN_POINT('',(0.500000000000001,0.4,-14.74)) ;
#116989 = CARTESIAN_POINT('',(0.600000000000001,0.4,-14.74)) ;
#116990 = CARTESIAN_POINT('',(0.500000000000001,-2.,-14.74)) ;
#116991 = CARTESIAN_POINT('Origin',(0.600000000000001,-2.,-13.865)) ;
#116992 = CARTESIAN_POINT('',(0.500000000000001,-2.,-13.965)) ;
#116993 = CARTESIAN_POINT('',(-0.899999999999999,-2.,-13.965)) ;
#116994 = CARTESIAN_POINT('',(-0.999999999999999,-2.,-13.965)) ;
#116995 = CARTESIAN_POINT('',(-0.899999999999999,-2.,-14.64)) ;
#116996 = CARTESIAN_POINT('',(-0.899999999999999,-2.,-14.74)) ;
#116997 = CARTESIAN_POINT('',(0.500000000000001,-2.,-14.64)) ;
#116998 = CARTESIAN_POINT('',(0.600000000000001,-2.,-14.64)) ;
#116999 = CARTESIAN_POINT('',(0.500000000000001,-2.,-13.865)) ;
#117000 = CARTESIAN_POINT('Origin',(0.600000000000001,-2.,-19.55)) ;
#117001 = CARTESIAN_POINT('',(0.500000000000001,-2.,-19.65)) ;
#117002 = CARTESIAN_POINT('',(-0.899999999999999,-2.,-19.65)) ;
#117003 = CARTESIAN_POINT('',(0.600000000000001,-2.,-19.65)) ;
#117004 = CARTESIAN_POINT('',(-0.899999999999999,-2.,-20.325)) ;
#117005 = CARTESIAN_POINT('',(-0.899999999999999,-2.,-20.425)) ;
#117006 = CARTESIAN_POINT('',(0.500000000000001,-2.,-20.325)) ;
#117007 = CARTESIAN_POINT('',(0.600000000000001,-2.,-20.325)) ;
#117008 = CARTESIAN_POINT('',(0.500000000000001,-2.,-19.55)) ;
#117009 = CARTESIAN_POINT('Origin',(0.600000000000001,0.5,-19.55)) ;
#117010 = CARTESIAN_POINT('',(-0.899999999999999,0.4,-19.55)) ;
#117011 = CARTESIAN_POINT('',(-0.999999999999999,0.4,-19.55)) ;
#117012 = CARTESIAN_POINT('',(-0.899999999999999,-1.9,-19.55)) ;
#117013 = CARTESIAN_POINT('',(-0.899999999999999,-2.,-19.55)) ;
#117014 = CARTESIAN_POINT('',(0.600000000000001,-1.9,-19.55)) ;
#117015 = CARTESIAN_POINT('Origin',(0.600000000000001,0.5,-18.55)) ;
#117016 = CARTESIAN_POINT('',(0.500000000000001,0.5,-18.65)) ;
#117017 = CARTESIAN_POINT('',(-0.899999999999999,0.5,-18.65)) ;
#117018 = CARTESIAN_POINT('',(-0.999999999999999,0.5,-18.65)) ;
#117019 = CARTESIAN_POINT('',(-0.899999999999999,0.5,-19.45)) ;
#117020 = CARTESIAN_POINT('',(-0.899999999999999,0.5,-19.55)) ;
#117021 = CARTESIAN_POINT('',(0.500000000000001,0.5,-19.45)) ;
#117022 = CARTESIAN_POINT('',(0.600000000000001,0.5,-19.45)) ;
#117023 = CARTESIAN_POINT('',(0.500000000000001,0.5,-18.55)) ;
#117024 = CARTESIAN_POINT('Origin',(0.600000000000001,-2.,-18.55)) ;
#117025 = CARTESIAN_POINT('',(0.500000000000001,-1.9,-18.55)) ;
#117026 = CARTESIAN_POINT('',(-0.899999999999999,-1.9,-18.55)) ;
#117027 = CARTESIAN_POINT('',(0.600000000000001,-1.9,-18.55)) ;
#117028 = CARTESIAN_POINT('',(-0.899999999999999,0.4,-18.55)) ;
#117029 = CARTESIAN_POINT('',(-0.899999999999999,0.5,-18.55)) ;
#117030 = CARTESIAN_POINT('',(0.500000000000001,0.4,-18.55)) ;
#117031 = CARTESIAN_POINT('',(0.600000000000001,0.4,-18.55)) ;
#117032 = CARTESIAN_POINT('',(0.500000000000001,-2.,-18.55)) ;
#117033 = CARTESIAN_POINT('Origin',(0.600000000000001,-2.,-17.675)) ;
#117034 = CARTESIAN_POINT('',(0.500000000000001,-2.,-17.775)) ;
#117035 = CARTESIAN_POINT('',(-0.899999999999999,-2.,-17.775)) ;
#117036 = CARTESIAN_POINT('',(-0.999999999999999,-2.,-17.775)) ;
#117037 = CARTESIAN_POINT('',(-0.899999999999999,-2.,-18.45)) ;
#117038 = CARTESIAN_POINT('',(-0.899999999999999,-2.,-18.55)) ;
#117039 = CARTESIAN_POINT('',(0.500000000000001,-2.,-18.45)) ;
#117040 = CARTESIAN_POINT('',(0.600000000000001,-2.,-18.45)) ;
#117041 = CARTESIAN_POINT('',(0.500000000000001,-2.,-17.675)) ;
#117042 = CARTESIAN_POINT('Origin',(0.600000000000001,-2.,-23.36)) ;
#117043 = CARTESIAN_POINT('',(0.500000000000001,-2.,-23.46)) ;
#117044 = CARTESIAN_POINT('',(-0.899999999999999,-2.,-23.46)) ;
#117045 = CARTESIAN_POINT('',(0.600000000000001,-2.,-23.46)) ;
#117046 = CARTESIAN_POINT('',(-0.899999999999999,-2.,-24.135)) ;
#117047 = CARTESIAN_POINT('',(-0.899999999999999,-2.,-24.235)) ;
#117048 = CARTESIAN_POINT('',(0.500000000000001,-2.,-24.135)) ;
#117049 = CARTESIAN_POINT('',(0.600000000000001,-2.,-24.135)) ;
#117050 = CARTESIAN_POINT('',(0.500000000000001,-2.,-23.36)) ;
#117051 = CARTESIAN_POINT('Origin',(0.600000000000001,0.5,-23.36)) ;
#117052 = CARTESIAN_POINT('',(-0.899999999999999,0.4,-23.36)) ;
#117053 = CARTESIAN_POINT('',(-0.999999999999999,0.4,-23.36)) ;
#117054 = CARTESIAN_POINT('',(-0.899999999999999,-1.9,-23.36)) ;
#117055 = CARTESIAN_POINT('',(-0.899999999999999,-2.,-23.36)) ;
#117056 = CARTESIAN_POINT('',(0.600000000000001,-1.9,-23.36)) ;
#117057 = CARTESIAN_POINT('Origin',(0.600000000000001,0.5,-22.36)) ;
#117058 = CARTESIAN_POINT('',(0.500000000000001,0.5,-22.46)) ;
#117059 = CARTESIAN_POINT('',(-0.899999999999999,0.5,-22.46)) ;
#117060 = CARTESIAN_POINT('',(-0.999999999999999,0.5,-22.46)) ;
#117061 = CARTESIAN_POINT('',(-0.899999999999999,0.5,-23.26)) ;
#117062 = CARTESIAN_POINT('',(-0.899999999999999,0.5,-23.36)) ;
#117063 = CARTESIAN_POINT('',(0.500000000000001,0.5,-23.26)) ;
#117064 = CARTESIAN_POINT('',(0.600000000000001,0.5,-23.26)) ;
#117065 = CARTESIAN_POINT('',(0.500000000000001,0.5,-22.36)) ;
#117066 = CARTESIAN_POINT('Origin',(0.600000000000001,-2.,-22.36)) ;
#117067 = CARTESIAN_POINT('',(0.500000000000001,-1.9,-22.36)) ;
#117068 = CARTESIAN_POINT('',(-0.899999999999999,-1.9,-22.36)) ;
#117069 = CARTESIAN_POINT('',(0.600000000000001,-1.9,-22.36)) ;
#117070 = CARTESIAN_POINT('',(-0.899999999999999,0.4,-22.36)) ;
#117071 = CARTESIAN_POINT('',(-0.899999999999999,0.5,-22.36)) ;
#117072 = CARTESIAN_POINT('',(0.500000000000001,0.4,-22.36)) ;
#117073 = CARTESIAN_POINT('',(0.600000000000001,0.4,-22.36)) ;
#117074 = CARTESIAN_POINT('',(0.500000000000001,-2.,-22.36)) ;
#117075 = CARTESIAN_POINT('Origin',(0.600000000000001,-2.,-21.485)) ;
#117076 = CARTESIAN_POINT('',(0.500000000000001,-2.,-21.585)) ;
#117077 = CARTESIAN_POINT('',(-0.899999999999999,-2.,-21.585)) ;
#117078 = CARTESIAN_POINT('',(-0.999999999999999,-2.,-21.585)) ;
#117079 = CARTESIAN_POINT('',(-0.899999999999999,-2.,-22.26)) ;
#117080 = CARTESIAN_POINT('',(-0.899999999999999,-2.,-22.36)) ;
#117081 = CARTESIAN_POINT('',(0.500000000000001,-2.,-22.26)) ;
#117082 = CARTESIAN_POINT('',(0.600000000000001,-2.,-22.26)) ;
#117083 = CARTESIAN_POINT('',(0.500000000000001,-2.,-21.485)) ;
#117084 = CARTESIAN_POINT('Origin',(0.600000000000001,-2.,-27.17)) ;
#117085 = CARTESIAN_POINT('',(0.500000000000001,-2.,-27.27)) ;
#117086 = CARTESIAN_POINT('',(-0.899999999999999,-2.,-27.27)) ;
#117087 = CARTESIAN_POINT('',(0.600000000000001,-2.,-27.27)) ;
#117088 = CARTESIAN_POINT('',(-0.899999999999999,-2.,-27.945)) ;
#117089 = CARTESIAN_POINT('',(-0.899999999999999,-2.,-28.045)) ;
#117090 = CARTESIAN_POINT('',(0.500000000000001,-2.,-27.945)) ;
#117091 = CARTESIAN_POINT('',(0.600000000000001,-2.,-27.945)) ;
#117092 = CARTESIAN_POINT('',(0.500000000000001,-2.,-27.17)) ;
#117093 = CARTESIAN_POINT('Origin',(0.600000000000001,0.5,-27.17)) ;
#117094 = CARTESIAN_POINT('',(-0.899999999999999,0.4,-27.17)) ;
#117095 = CARTESIAN_POINT('',(-0.999999999999999,0.4,-27.17)) ;
#117096 = CARTESIAN_POINT('',(-0.899999999999999,-1.9,-27.17)) ;
#117097 = CARTESIAN_POINT('',(-0.899999999999999,-2.,-27.17)) ;
#117098 = CARTESIAN_POINT('',(0.600000000000001,-1.9,-27.17)) ;
#117099 = CARTESIAN_POINT('Origin',(0.600000000000001,0.5,-26.17)) ;
#117100 = CARTESIAN_POINT('',(0.500000000000001,0.5,-26.27)) ;
#117101 = CARTESIAN_POINT('',(-0.899999999999999,0.5,-26.27)) ;
#117102 = CARTESIAN_POINT('',(-0.999999999999999,0.5,-26.27)) ;
#117103 = CARTESIAN_POINT('',(-0.899999999999999,0.5,-27.07)) ;
#117104 = CARTESIAN_POINT('',(-0.899999999999999,0.5,-27.17)) ;
#117105 = CARTESIAN_POINT('',(0.500000000000001,0.5,-27.07)) ;
#117106 = CARTESIAN_POINT('',(0.600000000000001,0.5,-27.07)) ;
#117107 = CARTESIAN_POINT('',(0.500000000000001,0.5,-26.17)) ;
#117108 = CARTESIAN_POINT('Origin',(0.600000000000001,-2.,-26.17)) ;
#117109 = CARTESIAN_POINT('',(0.500000000000001,-1.9,-26.17)) ;
#117110 = CARTESIAN_POINT('',(-0.899999999999999,-1.9,-26.17)) ;
#117111 = CARTESIAN_POINT('',(0.600000000000001,-1.9,-26.17)) ;
#117112 = CARTESIAN_POINT('',(-0.899999999999999,0.4,-26.17)) ;
#117113 = CARTESIAN_POINT('',(-0.899999999999999,0.5,-26.17)) ;
#117114 = CARTESIAN_POINT('',(0.500000000000001,0.4,-26.17)) ;
#117115 = CARTESIAN_POINT('',(0.600000000000001,0.4,-26.17)) ;
#117116 = CARTESIAN_POINT('',(0.500000000000001,-2.,-26.17)) ;
#117117 = CARTESIAN_POINT('Origin',(0.600000000000001,-2.,-25.295)) ;
#117118 = CARTESIAN_POINT('',(0.500000000000001,-2.,-25.395)) ;
#117119 = CARTESIAN_POINT('',(-0.899999999999999,-2.,-25.395)) ;
#117120 = CARTESIAN_POINT('',(-0.999999999999999,-2.,-25.395)) ;
#117121 = CARTESIAN_POINT('',(-0.899999999999999,-2.,-26.07)) ;
#117122 = CARTESIAN_POINT('',(-0.899999999999999,-2.,-26.17)) ;
#117123 = CARTESIAN_POINT('',(0.500000000000001,-2.,-26.07)) ;
#117124 = CARTESIAN_POINT('',(0.600000000000001,-2.,-26.07)) ;
#117125 = CARTESIAN_POINT('',(0.500000000000001,-2.,-25.295)) ;
#117126 = CARTESIAN_POINT('Origin',(0.600000000000001,-2.,-30.98)) ;
#117127 = CARTESIAN_POINT('',(0.500000000000001,-2.,-31.08)) ;
#117128 = CARTESIAN_POINT('',(-0.899999999999999,-2.,-31.08)) ;
#117129 = CARTESIAN_POINT('',(0.600000000000001,-2.,-31.08)) ;
#117130 = CARTESIAN_POINT('',(-0.899999999999999,-2.,-31.755)) ;
#117131 = CARTESIAN_POINT('',(-0.899999999999999,-2.,-31.855)) ;
#117132 = CARTESIAN_POINT('',(0.500000000000001,-2.,-31.755)) ;
#117133 = CARTESIAN_POINT('',(0.600000000000001,-2.,-31.755)) ;
#117134 = CARTESIAN_POINT('',(0.500000000000001,-2.,-30.98)) ;
#117135 = CARTESIAN_POINT('Origin',(0.600000000000001,0.5,-30.98)) ;
#117136 = CARTESIAN_POINT('',(-0.899999999999999,0.4,-30.98)) ;
#117137 = CARTESIAN_POINT('',(-0.999999999999999,0.4,-30.98)) ;
#117138 = CARTESIAN_POINT('',(-0.899999999999999,-1.9,-30.98)) ;
#117139 = CARTESIAN_POINT('',(-0.899999999999999,-2.,-30.98)) ;
#117140 = CARTESIAN_POINT('',(0.600000000000001,-1.9,-30.98)) ;
#117141 = CARTESIAN_POINT('Origin',(0.600000000000001,0.5,-29.98)) ;
#117142 = CARTESIAN_POINT('',(0.500000000000001,0.5,-30.08)) ;
#117143 = CARTESIAN_POINT('',(-0.899999999999999,0.5,-30.08)) ;
#117144 = CARTESIAN_POINT('',(-0.999999999999999,0.5,-30.08)) ;
#117145 = CARTESIAN_POINT('',(-0.899999999999999,0.5,-30.88)) ;
#117146 = CARTESIAN_POINT('',(-0.899999999999999,0.5,-30.98)) ;
#117147 = CARTESIAN_POINT('',(0.500000000000001,0.5,-30.88)) ;
#117148 = CARTESIAN_POINT('',(0.600000000000001,0.5,-30.88)) ;
#117149 = CARTESIAN_POINT('',(0.500000000000001,0.5,-29.98)) ;
#117150 = CARTESIAN_POINT('Origin',(0.600000000000001,-2.,-29.98)) ;
#117151 = CARTESIAN_POINT('',(0.500000000000001,-1.9,-29.98)) ;
#117152 = CARTESIAN_POINT('',(-0.899999999999999,-1.9,-29.98)) ;
#117153 = CARTESIAN_POINT('',(0.600000000000001,-1.9,-29.98)) ;
#117154 = CARTESIAN_POINT('',(-0.899999999999999,0.4,-29.98)) ;
#117155 = CARTESIAN_POINT('',(-0.899999999999999,0.5,-29.98)) ;
#117156 = CARTESIAN_POINT('',(0.500000000000001,0.4,-29.98)) ;
#117157 = CARTESIAN_POINT('',(0.600000000000001,0.4,-29.98)) ;
#117158 = CARTESIAN_POINT('',(0.500000000000001,-2.,-29.98)) ;
#117159 = CARTESIAN_POINT('Origin',(0.600000000000001,-2.,-29.105)) ;
#117160 = CARTESIAN_POINT('',(0.500000000000001,-2.,-29.205)) ;
#117161 = CARTESIAN_POINT('',(-0.899999999999999,-2.,-29.205)) ;
#117162 = CARTESIAN_POINT('',(-0.999999999999999,-2.,-29.205)) ;
#117163 = CARTESIAN_POINT('',(-0.899999999999999,-2.,-29.88)) ;
#117164 = CARTESIAN_POINT('',(-0.899999999999999,-2.,-29.98)) ;
#117165 = CARTESIAN_POINT('',(0.500000000000001,-2.,-29.88)) ;
#117166 = CARTESIAN_POINT('',(0.600000000000001,-2.,-29.88)) ;
#117167 = CARTESIAN_POINT('',(0.500000000000001,-2.,-29.105)) ;
#117168 = CARTESIAN_POINT('Origin',(0.600000000000001,-2.,-34.79)) ;
#117169 = CARTESIAN_POINT('',(0.500000000000001,-2.,-34.89)) ;
#117170 = CARTESIAN_POINT('',(-0.899999999999999,-2.,-34.89)) ;
#117171 = CARTESIAN_POINT('',(0.600000000000001,-2.,-34.89)) ;
#117172 = CARTESIAN_POINT('',(-0.899999999999999,-2.,-35.565)) ;
#117173 = CARTESIAN_POINT('',(-0.899999999999999,-2.,-35.665)) ;
#117174 = CARTESIAN_POINT('',(0.500000000000001,-2.,-35.565)) ;
#117175 = CARTESIAN_POINT('',(0.600000000000001,-2.,-35.565)) ;
#117176 = CARTESIAN_POINT('',(0.500000000000001,-2.,-34.79)) ;
#117177 = CARTESIAN_POINT('Origin',(0.600000000000001,0.5,-34.79)) ;
#117178 = CARTESIAN_POINT('',(-0.899999999999999,0.4,-34.79)) ;
#117179 = CARTESIAN_POINT('',(-0.999999999999999,0.4,-34.79)) ;
#117180 = CARTESIAN_POINT('',(-0.899999999999999,-1.9,-34.79)) ;
#117181 = CARTESIAN_POINT('',(-0.899999999999999,-2.,-34.79)) ;
#117182 = CARTESIAN_POINT('',(0.600000000000001,-1.9,-34.79)) ;
#117183 = CARTESIAN_POINT('Origin',(0.600000000000001,0.5,-33.79)) ;
#117184 = CARTESIAN_POINT('',(0.500000000000001,0.5,-33.89)) ;
#117185 = CARTESIAN_POINT('',(-0.899999999999999,0.5,-33.89)) ;
#117186 = CARTESIAN_POINT('',(-0.999999999999999,0.5,-33.89)) ;
#117187 = CARTESIAN_POINT('',(-0.899999999999999,0.5,-34.69)) ;
#117188 = CARTESIAN_POINT('',(-0.899999999999999,0.5,-34.79)) ;
#117189 = CARTESIAN_POINT('',(0.500000000000001,0.5,-34.69)) ;
#117190 = CARTESIAN_POINT('',(0.600000000000001,0.5,-34.69)) ;
#117191 = CARTESIAN_POINT('',(0.500000000000001,0.5,-33.79)) ;
#117192 = CARTESIAN_POINT('Origin',(0.600000000000001,-2.,-33.79)) ;
#117193 = CARTESIAN_POINT('',(0.500000000000001,-1.9,-33.79)) ;
#117194 = CARTESIAN_POINT('',(-0.899999999999999,-1.9,-33.79)) ;
#117195 = CARTESIAN_POINT('',(0.600000000000001,-1.9,-33.79)) ;
#117196 = CARTESIAN_POINT('',(-0.899999999999999,0.4,-33.79)) ;
#117197 = CARTESIAN_POINT('',(-0.899999999999999,0.5,-33.79)) ;
#117198 = CARTESIAN_POINT('',(0.500000000000001,0.4,-33.79)) ;
#117199 = CARTESIAN_POINT('',(0.600000000000001,0.4,-33.79)) ;
#117200 = CARTESIAN_POINT('',(0.500000000000001,-2.,-33.79)) ;
#117201 = CARTESIAN_POINT('Origin',(0.600000000000001,-2.,-32.915)) ;
#117202 = CARTESIAN_POINT('',(0.500000000000001,-2.,-33.015)) ;
#117203 = CARTESIAN_POINT('',(-0.899999999999999,-2.,-33.015)) ;
#117204 = CARTESIAN_POINT('',(-0.999999999999999,-2.,-33.015)) ;
#117205 = CARTESIAN_POINT('',(-0.899999999999999,-2.,-33.69)) ;
#117206 = CARTESIAN_POINT('',(-0.899999999999999,-2.,-33.79)) ;
#117207 = CARTESIAN_POINT('',(0.500000000000001,-2.,-33.69)) ;
#117208 = CARTESIAN_POINT('',(0.600000000000001,-2.,-33.69)) ;
#117209 = CARTESIAN_POINT('',(0.500000000000001,-2.,-32.915)) ;
#117210 = CARTESIAN_POINT('Origin',(1.4,2.1,-33.69)) ;
#117211 = CARTESIAN_POINT('',(1.5,2.,-33.69)) ;
#117212 = CARTESIAN_POINT('',(7.9,2.,-33.69)) ;
#117213 = CARTESIAN_POINT('',(1.4,2.,-33.69)) ;
#117214 = CARTESIAN_POINT('',(1.5,2.1,-33.79)) ;
#117215 = CARTESIAN_POINT('Origin',(1.5,2.1,-33.69)) ;
#117216 = CARTESIAN_POINT('',(7.9,2.1,-33.79)) ;
#117217 = CARTESIAN_POINT('',(1.4,2.1,-33.79)) ;
#117218 = CARTESIAN_POINT('Origin',(7.9,2.1,-33.69)) ;
#117219 = CARTESIAN_POINT('Origin',(1.4,2.4,-33.79)) ;
#117220 = CARTESIAN_POINT('',(1.5,2.4,-33.79)) ;
#117221 = CARTESIAN_POINT('',(1.5,2.4,-33.79)) ;
#117222 = CARTESIAN_POINT('',(7.9,2.4,-33.79)) ;
#117223 = CARTESIAN_POINT('',(1.4,2.4,-33.79)) ;
#117224 = CARTESIAN_POINT('',(7.9,2.1,-33.79)) ;
#117225 = CARTESIAN_POINT('Origin',(1.4,2.4,-33.69)) ;
#117226 = CARTESIAN_POINT('',(1.5,2.5,-33.69)) ;
#117227 = CARTESIAN_POINT('Origin',(1.5,2.4,-33.69)) ;
#117228 = CARTESIAN_POINT('',(7.9,2.5,-33.69)) ;
#117229 = CARTESIAN_POINT('',(1.4,2.5,-33.69)) ;
#117230 = CARTESIAN_POINT('Origin',(7.9,2.4,-33.69)) ;
#117231 = CARTESIAN_POINT('Origin',(1.4,2.5,-33.5814213562373)) ;
#117232 = CARTESIAN_POINT('',(1.5,2.5,-33.5814213562373)) ;
#117233 = CARTESIAN_POINT('',(1.5,2.5,-33.5814213562373)) ;
#117234 = CARTESIAN_POINT('',(7.9,2.5,-33.5814213562373)) ;
#117235 = CARTESIAN_POINT('',(1.4,2.5,-33.5814213562373)) ;
#117236 = CARTESIAN_POINT('',(7.9,2.5,-33.69)) ;
#117237 = CARTESIAN_POINT('Origin',(1.4,2.6,-33.5814213562373)) ;
#117238 = CARTESIAN_POINT('',(1.5,2.52928932188135,-33.5107106781187)) ;
#117239 = CARTESIAN_POINT('Origin',(1.5,2.6,-33.5814213562373)) ;
#117240 = CARTESIAN_POINT('',(7.9,2.52928932188135,-33.5107106781187)) ;
#117241 = CARTESIAN_POINT('',(1.4,2.52928932188135,-33.5107106781187)) ;
#117242 = CARTESIAN_POINT('Origin',(7.9,2.6,-33.5814213562373)) ;
#117243 = CARTESIAN_POINT('Origin',(1.4,3.07928932188135,-32.9607106781187)) ;
#117244 = CARTESIAN_POINT('',(1.5,3.07928932188135,-32.9607106781187)) ;
#117245 = CARTESIAN_POINT('',(7.9,3.07928932188135,-32.9607106781187)) ;
#117246 = CARTESIAN_POINT('',(1.4,3.07928932188135,-32.9607106781187)) ;
#117247 = CARTESIAN_POINT('',(7.9,2.52928932188135,-33.5107106781187)) ;
#117248 = CARTESIAN_POINT('Origin',(1.4,3.15,-33.0314213562373)) ;
#117249 = CARTESIAN_POINT('',(7.9,3.25,-33.0314213562373)) ;
#117250 = CARTESIAN_POINT('',(1.4,3.25,-33.0314213562373)) ;
#117251 = CARTESIAN_POINT('Origin',(7.9,3.15,-33.0314213562373)) ;
#117252 = CARTESIAN_POINT('Origin',(1.4,3.25,-35.5485786437627)) ;
#117253 = CARTESIAN_POINT('',(1.5,3.25,-35.5485786437627)) ;
#117254 = CARTESIAN_POINT('',(7.9,3.25,-33.0314213562373)) ;
#117255 = CARTESIAN_POINT('Origin',(1.4,2.52928932188134,-35.0692893218813)) ;
#117256 = CARTESIAN_POINT('',(1.5,2.52928932188134,-35.0692893218813)) ;
#117257 = CARTESIAN_POINT('',(1.5,2.52928932188134,-35.0692893218813)) ;
#117258 = CARTESIAN_POINT('',(7.9,2.52928932188134,-35.0692893218813)) ;
#117259 = CARTESIAN_POINT('',(1.4,2.52928932188134,-35.0692893218813)) ;
#117260 = CARTESIAN_POINT('',(7.9,3.07928932188135,-35.6192893218813)) ;
#117261 = CARTESIAN_POINT('Origin',(1.4,2.6,-34.9985786437627)) ;
#117262 = CARTESIAN_POINT('',(1.5,2.5,-34.9985786437627)) ;
#117263 = CARTESIAN_POINT('Origin',(1.5,2.6,-34.9985786437627)) ;
#117264 = CARTESIAN_POINT('',(7.9,2.5,-34.9985786437627)) ;
#117265 = CARTESIAN_POINT('',(1.4,2.5,-34.9985786437627)) ;
#117266 = CARTESIAN_POINT('Origin',(7.9,2.6,-34.9985786437627)) ;
#117267 = CARTESIAN_POINT('Origin',(1.4,2.5,-34.89)) ;
#117268 = CARTESIAN_POINT('',(1.5,2.5,-34.89)) ;
#117269 = CARTESIAN_POINT('',(1.5,2.5,-34.89)) ;
#117270 = CARTESIAN_POINT('',(7.9,2.5,-34.89)) ;
#117271 = CARTESIAN_POINT('',(1.4,2.5,-34.89)) ;
#117272 = CARTESIAN_POINT('',(7.9,2.5,-34.9985786437627)) ;
#117273 = CARTESIAN_POINT('Origin',(1.4,2.4,-34.89)) ;
#117274 = CARTESIAN_POINT('',(1.5,2.4,-34.79)) ;
#117275 = CARTESIAN_POINT('Origin',(1.5,2.4,-34.89)) ;
#117276 = CARTESIAN_POINT('',(7.9,2.4,-34.79)) ;
#117277 = CARTESIAN_POINT('',(1.4,2.4,-34.79)) ;
#117278 = CARTESIAN_POINT('Origin',(7.9,2.4,-34.89)) ;
#117279 = CARTESIAN_POINT('Origin',(1.4,2.1,-34.79)) ;
#117280 = CARTESIAN_POINT('',(1.5,2.1,-34.79)) ;
#117281 = CARTESIAN_POINT('',(1.5,2.1,-34.79)) ;
#117282 = CARTESIAN_POINT('',(7.9,2.1,-34.79)) ;
#117283 = CARTESIAN_POINT('',(1.4,2.1,-34.79)) ;
#117284 = CARTESIAN_POINT('',(7.9,2.4,-34.79)) ;
#117285 = CARTESIAN_POINT('Origin',(1.4,2.1,-34.89)) ;
#117286 = CARTESIAN_POINT('',(1.5,2.,-34.89)) ;
#117287 = CARTESIAN_POINT('Origin',(1.5,2.1,-34.89)) ;
#117288 = CARTESIAN_POINT('',(7.9,2.,-34.89)) ;
#117289 = CARTESIAN_POINT('',(1.4,2.,-34.89)) ;
#117290 = CARTESIAN_POINT('Origin',(7.9,2.1,-34.89)) ;
#117291 = CARTESIAN_POINT('Origin',(1.4,2.,-34.89)) ;
#117292 = CARTESIAN_POINT('',(1.5,2.,-35.84)) ;
#117293 = CARTESIAN_POINT('',(1.5,2.,-35.84)) ;
#117294 = CARTESIAN_POINT('',(7.9,2.,-35.84)) ;
#117295 = CARTESIAN_POINT('',(1.4,2.,-35.84)) ;
#117296 = CARTESIAN_POINT('',(7.9,2.,-34.89)) ;
#117297 = CARTESIAN_POINT('Origin',(1.4,1.9,-35.84)) ;
#117298 = CARTESIAN_POINT('',(1.5,1.9,-35.94)) ;
#117299 = CARTESIAN_POINT('Origin',(1.5,1.9,-35.84)) ;
#117300 = CARTESIAN_POINT('',(7.9,1.9,-35.94)) ;
#117301 = CARTESIAN_POINT('',(1.4,1.9,-35.94)) ;
#117302 = CARTESIAN_POINT('Origin',(7.9,1.9,-35.84)) ;
#117303 = CARTESIAN_POINT('Origin',(1.4,1.9,-35.94)) ;
#117304 = CARTESIAN_POINT('',(1.5,-2.15,-35.94)) ;
#117305 = CARTESIAN_POINT('',(1.5,-2.15,-35.94)) ;
#117306 = CARTESIAN_POINT('',(7.9,-2.15,-35.94)) ;
#117307 = CARTESIAN_POINT('',(1.4,-2.15,-35.94)) ;
#117308 = CARTESIAN_POINT('',(7.9,1.9,-35.94)) ;
#117309 = CARTESIAN_POINT('Origin',(1.4,-2.15,-35.84)) ;
#117310 = CARTESIAN_POINT('',(1.5,-2.25,-35.84)) ;
#117311 = CARTESIAN_POINT('Origin',(1.5,-2.15,-35.84)) ;
#117312 = CARTESIAN_POINT('',(7.9,-2.25,-35.84)) ;
#117313 = CARTESIAN_POINT('',(1.4,-2.25,-35.84)) ;
#117314 = CARTESIAN_POINT('Origin',(7.9,-2.15,-35.84)) ;
#117315 = CARTESIAN_POINT('Origin',(1.4,-2.25,-35.1931195934094)) ;
#117316 = CARTESIAN_POINT('',(1.5,-2.25,-35.1931195934094)) ;
#117317 = CARTESIAN_POINT('',(1.5,-2.25,-35.1931195934094)) ;
#117318 = CARTESIAN_POINT('',(7.9,-2.25,-35.1931195934094)) ;
#117319 = CARTESIAN_POINT('',(1.4,-2.25,-35.1931195934094)) ;
#117320 = CARTESIAN_POINT('',(7.9,-2.25,-35.84)) ;
#117321 = CARTESIAN_POINT('Origin',(1.4,-2.15,-35.1931195934094)) ;
#117322 = CARTESIAN_POINT('',(1.5,-2.23576512455516,-35.1416964137135)) ;
#117323 = CARTESIAN_POINT('Origin',(1.5,-2.15,-35.1931195934094)) ;
#117324 = CARTESIAN_POINT('',(7.9,-2.23576512455516,-35.1416964137135)) ;
#117325 = CARTESIAN_POINT('',(1.4,-2.23576512455516,-35.1416964137135)) ;
#117326 = CARTESIAN_POINT('Origin',(7.9,-2.15,-35.1931195934094)) ;
#117327 = CARTESIAN_POINT('Origin',(1.4,-3.65625,-34.29)) ;
#117328 = CARTESIAN_POINT('',(1.5,-2.23576512455516,-33.4383035862865)) ;
#117329 = CARTESIAN_POINT('Origin',(1.5,-3.65625,-34.29)) ;
#117330 = CARTESIAN_POINT('',(7.9,-2.23576512455516,-33.4383035862865)) ;
#117331 = CARTESIAN_POINT('',(1.4,-2.23576512455516,-33.4383035862865)) ;
#117332 = CARTESIAN_POINT('Origin',(7.9,-3.65625,-34.29)) ;
#117333 = CARTESIAN_POINT('Origin',(1.4,-2.15,-33.3868804065906)) ;
#117334 = CARTESIAN_POINT('',(1.5,-2.25,-33.3868804065906)) ;
#117335 = CARTESIAN_POINT('Origin',(1.5,-2.15,-33.3868804065906)) ;
#117336 = CARTESIAN_POINT('',(7.9,-2.25,-33.3868804065906)) ;
#117337 = CARTESIAN_POINT('',(1.4,-2.25,-33.3868804065906)) ;
#117338 = CARTESIAN_POINT('Origin',(7.9,-2.15,-33.3868804065906)) ;
#117339 = CARTESIAN_POINT('Origin',(1.4,-2.25,-32.74)) ;
#117340 = CARTESIAN_POINT('',(1.5,-2.25,-32.74)) ;
#117341 = CARTESIAN_POINT('',(1.5,-2.25,-32.74)) ;
#117342 = CARTESIAN_POINT('',(7.9,-2.25,-32.74)) ;
#117343 = CARTESIAN_POINT('',(1.4,-2.25,-32.74)) ;
#117344 = CARTESIAN_POINT('',(7.9,-2.25,-33.3868804065906)) ;
#117345 = CARTESIAN_POINT('Origin',(1.4,-2.15,-32.74)) ;
#117346 = CARTESIAN_POINT('',(1.5,-2.15,-32.64)) ;
#117347 = CARTESIAN_POINT('Origin',(1.5,-2.15,-32.74)) ;
#117348 = CARTESIAN_POINT('',(7.9,-2.15,-32.64)) ;
#117349 = CARTESIAN_POINT('',(1.4,-2.15,-32.64)) ;
#117350 = CARTESIAN_POINT('Origin',(7.9,-2.15,-32.74)) ;
#117351 = CARTESIAN_POINT('Origin',(1.4,1.9,-32.64)) ;
#117352 = CARTESIAN_POINT('',(1.5,1.9,-32.64)) ;
#117353 = CARTESIAN_POINT('',(1.5,1.9,-32.64)) ;
#117354 = CARTESIAN_POINT('',(7.9,1.9,-32.64)) ;
#117355 = CARTESIAN_POINT('',(1.4,1.9,-32.64)) ;
#117356 = CARTESIAN_POINT('',(7.9,-2.15,-32.64)) ;
#117357 = CARTESIAN_POINT('Origin',(1.4,1.9,-32.74)) ;
#117358 = CARTESIAN_POINT('',(1.5,2.,-32.74)) ;
#117359 = CARTESIAN_POINT('Origin',(1.5,1.9,-32.74)) ;
#117360 = CARTESIAN_POINT('',(7.9,2.,-32.74)) ;
#117361 = CARTESIAN_POINT('',(1.4,2.,-32.74)) ;
#117362 = CARTESIAN_POINT('Origin',(7.9,1.9,-32.74)) ;
#117363 = CARTESIAN_POINT('Origin',(1.4,2.,-32.74)) ;
#117364 = CARTESIAN_POINT('',(1.5,2.,-33.69)) ;
#117365 = CARTESIAN_POINT('',(7.9,2.,-32.74)) ;
#117366 = CARTESIAN_POINT('Origin',(1.4,2.1,-33.69)) ;
#117367 = CARTESIAN_POINT('',(1.4,2.6,-33.69)) ;
#117368 = CARTESIAN_POINT('',(1.4,2.4,-33.89)) ;
#117369 = CARTESIAN_POINT('Origin',(1.4,2.4,-33.69)) ;
#117370 = CARTESIAN_POINT('',(1.4,2.1,-33.89)) ;
#117371 = CARTESIAN_POINT('',(1.4,2.1,-33.89)) ;
#117372 = CARTESIAN_POINT('',(1.4,1.9,-33.69)) ;
#117373 = CARTESIAN_POINT('Origin',(1.4,2.1,-33.69)) ;
#117374 = CARTESIAN_POINT('',(1.4,1.9,-32.74)) ;
#117375 = CARTESIAN_POINT('',(1.4,1.9,-32.74)) ;
#117376 = CARTESIAN_POINT('',(1.4,-2.15,-32.74)) ;
#117377 = CARTESIAN_POINT('',(1.4,-2.15,-32.74)) ;
#117378 = CARTESIAN_POINT('',(1.4,-2.15,-33.3868804065906)) ;
#117379 = CARTESIAN_POINT('',(1.4,-2.15,-33.3868804065906)) ;
#117380 = CARTESIAN_POINT('',(1.4,-2.15,-35.1931195934094)) ;
#117381 = CARTESIAN_POINT('Origin',(1.4,-3.65625,-34.29)) ;
#117382 = CARTESIAN_POINT('',(1.4,-2.15,-35.84)) ;
#117383 = CARTESIAN_POINT('',(1.4,-2.15,-35.84)) ;
#117384 = CARTESIAN_POINT('',(1.4,1.9,-35.84)) ;
#117385 = CARTESIAN_POINT('',(1.4,1.9,-35.84)) ;
#117386 = CARTESIAN_POINT('',(1.4,1.9,-34.89)) ;
#117387 = CARTESIAN_POINT('',(1.4,1.9,-34.89)) ;
#117388 = CARTESIAN_POINT('',(1.4,2.1,-34.69)) ;
#117389 = CARTESIAN_POINT('Origin',(1.4,2.1,-34.89)) ;
#117390 = CARTESIAN_POINT('',(1.4,2.4,-34.69)) ;
#117391 = CARTESIAN_POINT('',(1.4,2.4,-34.69)) ;
#117392 = CARTESIAN_POINT('',(1.4,2.6,-34.89)) ;
#117393 = CARTESIAN_POINT('Origin',(1.4,2.4,-34.89)) ;
#117394 = CARTESIAN_POINT('',(1.4,2.6,-34.9985786437627)) ;
#117395 = CARTESIAN_POINT('',(1.4,2.6,-34.9985786437627)) ;
#117396 = CARTESIAN_POINT('',(1.4,3.15,-35.5485786437627)) ;
#117397 = CARTESIAN_POINT('',(1.4,3.15,-35.5485786437627)) ;
#117398 = CARTESIAN_POINT('',(1.4,3.15,-33.0314213562373)) ;
#117399 = CARTESIAN_POINT('',(1.4,2.6,-33.5814213562373)) ;
#117400 = CARTESIAN_POINT('',(1.4,2.6,-33.5814213562373)) ;
#117401 = CARTESIAN_POINT('',(1.4,2.6,-33.69)) ;
#117402 = CARTESIAN_POINT('Origin',(1.4,2.1,-29.88)) ;
#117403 = CARTESIAN_POINT('',(1.5,2.,-29.88)) ;
#117404 = CARTESIAN_POINT('',(7.9,2.,-29.88)) ;
#117405 = CARTESIAN_POINT('',(1.4,2.,-29.88)) ;
#117406 = CARTESIAN_POINT('',(1.5,2.1,-29.98)) ;
#117407 = CARTESIAN_POINT('Origin',(1.5,2.1,-29.88)) ;
#117408 = CARTESIAN_POINT('',(7.9,2.1,-29.98)) ;
#117409 = CARTESIAN_POINT('',(1.4,2.1,-29.98)) ;
#117410 = CARTESIAN_POINT('Origin',(7.9,2.1,-29.88)) ;
#117411 = CARTESIAN_POINT('Origin',(1.4,2.4,-29.98)) ;
#117412 = CARTESIAN_POINT('',(1.5,2.4,-29.98)) ;
#117413 = CARTESIAN_POINT('',(1.5,2.4,-29.98)) ;
#117414 = CARTESIAN_POINT('',(7.9,2.4,-29.98)) ;
#117415 = CARTESIAN_POINT('',(1.4,2.4,-29.98)) ;
#117416 = CARTESIAN_POINT('',(7.9,2.1,-29.98)) ;
#117417 = CARTESIAN_POINT('Origin',(1.4,2.4,-29.88)) ;
#117418 = CARTESIAN_POINT('',(1.5,2.5,-29.88)) ;
#117419 = CARTESIAN_POINT('Origin',(1.5,2.4,-29.88)) ;
#117420 = CARTESIAN_POINT('',(7.9,2.5,-29.88)) ;
#117421 = CARTESIAN_POINT('',(1.4,2.5,-29.88)) ;
#117422 = CARTESIAN_POINT('Origin',(7.9,2.4,-29.88)) ;
#117423 = CARTESIAN_POINT('Origin',(1.4,2.5,-29.7714213562373)) ;
#117424 = CARTESIAN_POINT('',(1.5,2.5,-29.7714213562373)) ;
#117425 = CARTESIAN_POINT('',(1.5,2.5,-29.7714213562373)) ;
#117426 = CARTESIAN_POINT('',(7.9,2.5,-29.7714213562373)) ;
#117427 = CARTESIAN_POINT('',(1.4,2.5,-29.7714213562373)) ;
#117428 = CARTESIAN_POINT('',(7.9,2.5,-29.88)) ;
#117429 = CARTESIAN_POINT('Origin',(1.4,2.6,-29.7714213562373)) ;
#117430 = CARTESIAN_POINT('',(1.5,2.52928932188135,-29.7007106781187)) ;
#117431 = CARTESIAN_POINT('Origin',(1.5,2.6,-29.7714213562373)) ;
#117432 = CARTESIAN_POINT('',(7.9,2.52928932188135,-29.7007106781187)) ;
#117433 = CARTESIAN_POINT('',(1.4,2.52928932188135,-29.7007106781187)) ;
#117434 = CARTESIAN_POINT('Origin',(7.9,2.6,-29.7714213562373)) ;
#117435 = CARTESIAN_POINT('Origin',(1.4,3.07928932188135,-29.1507106781187)) ;
#117436 = CARTESIAN_POINT('',(1.5,3.07928932188135,-29.1507106781187)) ;
#117437 = CARTESIAN_POINT('',(7.9,3.07928932188135,-29.1507106781187)) ;
#117438 = CARTESIAN_POINT('',(1.4,3.07928932188135,-29.1507106781187)) ;
#117439 = CARTESIAN_POINT('',(7.9,2.52928932188135,-29.7007106781187)) ;
#117440 = CARTESIAN_POINT('Origin',(1.4,3.15,-29.2214213562373)) ;
#117441 = CARTESIAN_POINT('',(7.9,3.25,-29.2214213562373)) ;
#117442 = CARTESIAN_POINT('',(1.4,3.25,-29.2214213562373)) ;
#117443 = CARTESIAN_POINT('Origin',(7.9,3.15,-29.2214213562373)) ;
#117444 = CARTESIAN_POINT('Origin',(1.4,3.25,-31.7385786437627)) ;
#117445 = CARTESIAN_POINT('',(1.5,3.25,-31.7385786437627)) ;
#117446 = CARTESIAN_POINT('',(7.9,3.25,-29.2214213562373)) ;
#117447 = CARTESIAN_POINT('Origin',(1.4,2.52928932188134,-31.2592893218813)) ;
#117448 = CARTESIAN_POINT('',(1.5,2.52928932188134,-31.2592893218813)) ;
#117449 = CARTESIAN_POINT('',(1.5,2.52928932188135,-31.2592893218813)) ;
#117450 = CARTESIAN_POINT('',(7.9,2.52928932188134,-31.2592893218813)) ;
#117451 = CARTESIAN_POINT('',(1.4,2.52928932188134,-31.2592893218813)) ;
#117452 = CARTESIAN_POINT('',(7.9,3.07928932188135,-31.8092893218813)) ;
#117453 = CARTESIAN_POINT('Origin',(1.4,2.6,-31.1885786437627)) ;
#117454 = CARTESIAN_POINT('',(1.5,2.5,-31.1885786437627)) ;
#117455 = CARTESIAN_POINT('Origin',(1.5,2.6,-31.1885786437627)) ;
#117456 = CARTESIAN_POINT('',(7.9,2.5,-31.1885786437627)) ;
#117457 = CARTESIAN_POINT('',(1.4,2.5,-31.1885786437627)) ;
#117458 = CARTESIAN_POINT('Origin',(7.9,2.6,-31.1885786437627)) ;
#117459 = CARTESIAN_POINT('Origin',(1.4,2.5,-31.08)) ;
#117460 = CARTESIAN_POINT('',(1.5,2.5,-31.08)) ;
#117461 = CARTESIAN_POINT('',(1.5,2.5,-31.08)) ;
#117462 = CARTESIAN_POINT('',(7.9,2.5,-31.08)) ;
#117463 = CARTESIAN_POINT('',(1.4,2.5,-31.08)) ;
#117464 = CARTESIAN_POINT('',(7.9,2.5,-31.1885786437627)) ;
#117465 = CARTESIAN_POINT('Origin',(1.4,2.4,-31.08)) ;
#117466 = CARTESIAN_POINT('',(1.5,2.4,-30.98)) ;
#117467 = CARTESIAN_POINT('Origin',(1.5,2.4,-31.08)) ;
#117468 = CARTESIAN_POINT('',(7.9,2.4,-30.98)) ;
#117469 = CARTESIAN_POINT('',(1.4,2.4,-30.98)) ;
#117470 = CARTESIAN_POINT('Origin',(7.9,2.4,-31.08)) ;
#117471 = CARTESIAN_POINT('Origin',(1.4,2.1,-30.98)) ;
#117472 = CARTESIAN_POINT('',(1.5,2.1,-30.98)) ;
#117473 = CARTESIAN_POINT('',(1.5,2.1,-30.98)) ;
#117474 = CARTESIAN_POINT('',(7.9,2.1,-30.98)) ;
#117475 = CARTESIAN_POINT('',(1.4,2.1,-30.98)) ;
#117476 = CARTESIAN_POINT('',(7.9,2.4,-30.98)) ;
#117477 = CARTESIAN_POINT('Origin',(1.4,2.1,-31.08)) ;
#117478 = CARTESIAN_POINT('',(1.5,2.,-31.08)) ;
#117479 = CARTESIAN_POINT('Origin',(1.5,2.1,-31.08)) ;
#117480 = CARTESIAN_POINT('',(7.9,2.,-31.08)) ;
#117481 = CARTESIAN_POINT('',(1.4,2.,-31.08)) ;
#117482 = CARTESIAN_POINT('Origin',(7.9,2.1,-31.08)) ;
#117483 = CARTESIAN_POINT('Origin',(1.4,2.,-31.08)) ;
#117484 = CARTESIAN_POINT('',(1.5,2.,-32.03)) ;
#117485 = CARTESIAN_POINT('',(1.5,2.,-32.03)) ;
#117486 = CARTESIAN_POINT('',(7.9,2.,-32.03)) ;
#117487 = CARTESIAN_POINT('',(1.4,2.,-32.03)) ;
#117488 = CARTESIAN_POINT('',(7.9,2.,-31.08)) ;
#117489 = CARTESIAN_POINT('Origin',(1.4,1.9,-32.03)) ;
#117490 = CARTESIAN_POINT('',(1.5,1.9,-32.13)) ;
#117491 = CARTESIAN_POINT('Origin',(1.5,1.9,-32.03)) ;
#117492 = CARTESIAN_POINT('',(7.9,1.9,-32.13)) ;
#117493 = CARTESIAN_POINT('',(1.4,1.9,-32.13)) ;
#117494 = CARTESIAN_POINT('Origin',(7.9,1.9,-32.03)) ;
#117495 = CARTESIAN_POINT('Origin',(1.4,1.9,-32.13)) ;
#117496 = CARTESIAN_POINT('',(1.5,-2.15,-32.13)) ;
#117497 = CARTESIAN_POINT('',(1.5,-2.15,-32.13)) ;
#117498 = CARTESIAN_POINT('',(7.9,-2.15,-32.13)) ;
#117499 = CARTESIAN_POINT('',(1.4,-2.15,-32.13)) ;
#117500 = CARTESIAN_POINT('',(7.9,1.9,-32.13)) ;
#117501 = CARTESIAN_POINT('Origin',(1.4,-2.15,-32.03)) ;
#117502 = CARTESIAN_POINT('',(1.5,-2.25,-32.03)) ;
#117503 = CARTESIAN_POINT('Origin',(1.5,-2.15,-32.03)) ;
#117504 = CARTESIAN_POINT('',(7.9,-2.25,-32.03)) ;
#117505 = CARTESIAN_POINT('',(1.4,-2.25,-32.03)) ;
#117506 = CARTESIAN_POINT('Origin',(7.9,-2.15,-32.03)) ;
#117507 = CARTESIAN_POINT('Origin',(1.4,-2.25,-31.3831195934094)) ;
#117508 = CARTESIAN_POINT('',(1.5,-2.25,-31.3831195934094)) ;
#117509 = CARTESIAN_POINT('',(1.5,-2.25,-31.3831195934094)) ;
#117510 = CARTESIAN_POINT('',(7.9,-2.25,-31.3831195934094)) ;
#117511 = CARTESIAN_POINT('',(1.4,-2.25,-31.3831195934094)) ;
#117512 = CARTESIAN_POINT('',(7.9,-2.25,-32.03)) ;
#117513 = CARTESIAN_POINT('Origin',(1.4,-2.15,-31.3831195934094)) ;
#117514 = CARTESIAN_POINT('',(1.5,-2.23576512455516,-31.3316964137135)) ;
#117515 = CARTESIAN_POINT('Origin',(1.5,-2.15,-31.3831195934094)) ;
#117516 = CARTESIAN_POINT('',(7.9,-2.23576512455516,-31.3316964137135)) ;
#117517 = CARTESIAN_POINT('',(1.4,-2.23576512455516,-31.3316964137135)) ;
#117518 = CARTESIAN_POINT('Origin',(7.9,-2.15,-31.3831195934094)) ;
#117519 = CARTESIAN_POINT('Origin',(1.4,-3.65625,-30.48)) ;
#117520 = CARTESIAN_POINT('',(1.5,-2.23576512455516,-29.6283035862865)) ;
#117521 = CARTESIAN_POINT('Origin',(1.5,-3.65625,-30.48)) ;
#117522 = CARTESIAN_POINT('',(7.9,-2.23576512455516,-29.6283035862865)) ;
#117523 = CARTESIAN_POINT('',(1.4,-2.23576512455516,-29.6283035862865)) ;
#117524 = CARTESIAN_POINT('Origin',(7.9,-3.65625,-30.48)) ;
#117525 = CARTESIAN_POINT('Origin',(1.4,-2.15,-29.5768804065906)) ;
#117526 = CARTESIAN_POINT('',(1.5,-2.25,-29.5768804065906)) ;
#117527 = CARTESIAN_POINT('Origin',(1.5,-2.15,-29.5768804065906)) ;
#117528 = CARTESIAN_POINT('',(7.9,-2.25,-29.5768804065906)) ;
#117529 = CARTESIAN_POINT('',(1.4,-2.25,-29.5768804065906)) ;
#117530 = CARTESIAN_POINT('Origin',(7.9,-2.15,-29.5768804065906)) ;
#117531 = CARTESIAN_POINT('Origin',(1.4,-2.25,-28.93)) ;
#117532 = CARTESIAN_POINT('',(1.5,-2.25,-28.93)) ;
#117533 = CARTESIAN_POINT('',(1.5,-2.25,-28.93)) ;
#117534 = CARTESIAN_POINT('',(7.9,-2.25,-28.93)) ;
#117535 = CARTESIAN_POINT('',(1.4,-2.25,-28.93)) ;
#117536 = CARTESIAN_POINT('',(7.9,-2.25,-29.5768804065906)) ;
#117537 = CARTESIAN_POINT('Origin',(1.4,-2.15,-28.93)) ;
#117538 = CARTESIAN_POINT('',(1.5,-2.15,-28.83)) ;
#117539 = CARTESIAN_POINT('Origin',(1.5,-2.15,-28.93)) ;
#117540 = CARTESIAN_POINT('',(7.9,-2.15,-28.83)) ;
#117541 = CARTESIAN_POINT('',(1.4,-2.15,-28.83)) ;
#117542 = CARTESIAN_POINT('Origin',(7.9,-2.15,-28.93)) ;
#117543 = CARTESIAN_POINT('Origin',(1.4,1.9,-28.83)) ;
#117544 = CARTESIAN_POINT('',(1.5,1.9,-28.83)) ;
#117545 = CARTESIAN_POINT('',(1.5,1.9,-28.83)) ;
#117546 = CARTESIAN_POINT('',(7.9,1.9,-28.83)) ;
#117547 = CARTESIAN_POINT('',(1.4,1.9,-28.83)) ;
#117548 = CARTESIAN_POINT('',(7.9,-2.15,-28.83)) ;
#117549 = CARTESIAN_POINT('Origin',(1.4,1.9,-28.93)) ;
#117550 = CARTESIAN_POINT('',(1.5,2.,-28.93)) ;
#117551 = CARTESIAN_POINT('Origin',(1.5,1.9,-28.93)) ;
#117552 = CARTESIAN_POINT('',(7.9,2.,-28.93)) ;
#117553 = CARTESIAN_POINT('',(1.4,2.,-28.93)) ;
#117554 = CARTESIAN_POINT('Origin',(7.9,1.9,-28.93)) ;
#117555 = CARTESIAN_POINT('Origin',(1.4,2.,-28.93)) ;
#117556 = CARTESIAN_POINT('',(1.5,2.,-29.88)) ;
#117557 = CARTESIAN_POINT('',(7.9,2.,-28.93)) ;
#117558 = CARTESIAN_POINT('Origin',(1.4,2.1,-29.88)) ;
#117559 = CARTESIAN_POINT('',(1.4,2.6,-29.88)) ;
#117560 = CARTESIAN_POINT('',(1.4,2.4,-30.08)) ;
#117561 = CARTESIAN_POINT('Origin',(1.4,2.4,-29.88)) ;
#117562 = CARTESIAN_POINT('',(1.4,2.1,-30.08)) ;
#117563 = CARTESIAN_POINT('',(1.4,2.1,-30.08)) ;
#117564 = CARTESIAN_POINT('',(1.4,1.9,-29.88)) ;
#117565 = CARTESIAN_POINT('Origin',(1.4,2.1,-29.88)) ;
#117566 = CARTESIAN_POINT('',(1.4,1.9,-28.93)) ;
#117567 = CARTESIAN_POINT('',(1.4,1.9,-28.93)) ;
#117568 = CARTESIAN_POINT('',(1.4,-2.15,-28.93)) ;
#117569 = CARTESIAN_POINT('',(1.4,-2.15,-28.93)) ;
#117570 = CARTESIAN_POINT('',(1.4,-2.15,-29.5768804065906)) ;
#117571 = CARTESIAN_POINT('',(1.4,-2.15,-29.5768804065906)) ;
#117572 = CARTESIAN_POINT('',(1.4,-2.15,-31.3831195934094)) ;
#117573 = CARTESIAN_POINT('Origin',(1.4,-3.65625,-30.48)) ;
#117574 = CARTESIAN_POINT('',(1.4,-2.15,-32.03)) ;
#117575 = CARTESIAN_POINT('',(1.4,-2.15,-32.03)) ;
#117576 = CARTESIAN_POINT('',(1.4,1.9,-32.03)) ;
#117577 = CARTESIAN_POINT('',(1.4,1.9,-32.03)) ;
#117578 = CARTESIAN_POINT('',(1.4,1.9,-31.08)) ;
#117579 = CARTESIAN_POINT('',(1.4,1.9,-31.08)) ;
#117580 = CARTESIAN_POINT('',(1.4,2.1,-30.88)) ;
#117581 = CARTESIAN_POINT('Origin',(1.4,2.1,-31.08)) ;
#117582 = CARTESIAN_POINT('',(1.4,2.4,-30.88)) ;
#117583 = CARTESIAN_POINT('',(1.4,2.4,-30.88)) ;
#117584 = CARTESIAN_POINT('',(1.4,2.6,-31.08)) ;
#117585 = CARTESIAN_POINT('Origin',(1.4,2.4,-31.08)) ;
#117586 = CARTESIAN_POINT('',(1.4,2.6,-31.1885786437627)) ;
#117587 = CARTESIAN_POINT('',(1.4,2.6,-31.1885786437627)) ;
#117588 = CARTESIAN_POINT('',(1.4,3.15,-31.7385786437627)) ;
#117589 = CARTESIAN_POINT('',(1.4,3.15,-31.7385786437627)) ;
#117590 = CARTESIAN_POINT('',(1.4,3.15,-29.2214213562373)) ;
#117591 = CARTESIAN_POINT('',(1.4,2.6,-29.7714213562373)) ;
#117592 = CARTESIAN_POINT('',(1.4,2.6,-29.7714213562373)) ;
#117593 = CARTESIAN_POINT('',(1.4,2.6,-29.88)) ;
#117594 = CARTESIAN_POINT('Origin',(1.4,2.1,-26.07)) ;
#117595 = CARTESIAN_POINT('',(1.5,2.,-26.07)) ;
#117596 = CARTESIAN_POINT('',(7.9,2.,-26.07)) ;
#117597 = CARTESIAN_POINT('',(1.4,2.,-26.07)) ;
#117598 = CARTESIAN_POINT('',(1.5,2.1,-26.17)) ;
#117599 = CARTESIAN_POINT('Origin',(1.5,2.1,-26.07)) ;
#117600 = CARTESIAN_POINT('',(7.9,2.1,-26.17)) ;
#117601 = CARTESIAN_POINT('',(1.4,2.1,-26.17)) ;
#117602 = CARTESIAN_POINT('Origin',(7.9,2.1,-26.07)) ;
#117603 = CARTESIAN_POINT('Origin',(1.4,2.4,-26.17)) ;
#117604 = CARTESIAN_POINT('',(1.5,2.4,-26.17)) ;
#117605 = CARTESIAN_POINT('',(1.5,2.4,-26.17)) ;
#117606 = CARTESIAN_POINT('',(7.9,2.4,-26.17)) ;
#117607 = CARTESIAN_POINT('',(1.4,2.4,-26.17)) ;
#117608 = CARTESIAN_POINT('',(7.9,2.1,-26.17)) ;
#117609 = CARTESIAN_POINT('Origin',(1.4,2.4,-26.07)) ;
#117610 = CARTESIAN_POINT('',(1.5,2.5,-26.07)) ;
#117611 = CARTESIAN_POINT('Origin',(1.5,2.4,-26.07)) ;
#117612 = CARTESIAN_POINT('',(7.9,2.5,-26.07)) ;
#117613 = CARTESIAN_POINT('',(1.4,2.5,-26.07)) ;
#117614 = CARTESIAN_POINT('Origin',(7.9,2.4,-26.07)) ;
#117615 = CARTESIAN_POINT('Origin',(1.4,2.5,-25.9614213562373)) ;
#117616 = CARTESIAN_POINT('',(1.5,2.5,-25.9614213562373)) ;
#117617 = CARTESIAN_POINT('',(1.5,2.5,-25.9614213562373)) ;
#117618 = CARTESIAN_POINT('',(7.9,2.5,-25.9614213562373)) ;
#117619 = CARTESIAN_POINT('',(1.4,2.5,-25.9614213562373)) ;
#117620 = CARTESIAN_POINT('',(7.9,2.5,-26.07)) ;
#117621 = CARTESIAN_POINT('Origin',(1.4,2.6,-25.9614213562373)) ;
#117622 = CARTESIAN_POINT('',(1.5,2.52928932188135,-25.8907106781187)) ;
#117623 = CARTESIAN_POINT('Origin',(1.5,2.6,-25.9614213562373)) ;
#117624 = CARTESIAN_POINT('',(7.9,2.52928932188135,-25.8907106781187)) ;
#117625 = CARTESIAN_POINT('',(1.4,2.52928932188135,-25.8907106781187)) ;
#117626 = CARTESIAN_POINT('Origin',(7.9,2.6,-25.9614213562373)) ;
#117627 = CARTESIAN_POINT('Origin',(1.4,3.07928932188135,-25.3407106781187)) ;
#117628 = CARTESIAN_POINT('',(1.5,3.07928932188135,-25.3407106781187)) ;
#117629 = CARTESIAN_POINT('',(7.9,3.07928932188135,-25.3407106781187)) ;
#117630 = CARTESIAN_POINT('',(1.4,3.07928932188135,-25.3407106781187)) ;
#117631 = CARTESIAN_POINT('',(7.9,2.52928932188135,-25.8907106781187)) ;
#117632 = CARTESIAN_POINT('Origin',(1.4,3.15,-25.4114213562373)) ;
#117633 = CARTESIAN_POINT('',(7.9,3.25,-25.4114213562373)) ;
#117634 = CARTESIAN_POINT('',(1.4,3.25,-25.4114213562373)) ;
#117635 = CARTESIAN_POINT('Origin',(7.9,3.15,-25.4114213562373)) ;
#117636 = CARTESIAN_POINT('Origin',(1.4,3.25,-27.9285786437627)) ;
#117637 = CARTESIAN_POINT('',(1.5,3.25,-27.9285786437627)) ;
#117638 = CARTESIAN_POINT('',(7.9,3.25,-25.4114213562373)) ;
#117639 = CARTESIAN_POINT('Origin',(1.4,2.52928932188134,-27.4492893218813)) ;
#117640 = CARTESIAN_POINT('',(1.5,2.52928932188134,-27.4492893218813)) ;
#117641 = CARTESIAN_POINT('',(1.5,2.52928932188135,-27.4492893218813)) ;
#117642 = CARTESIAN_POINT('',(7.9,2.52928932188134,-27.4492893218813)) ;
#117643 = CARTESIAN_POINT('',(1.4,2.52928932188134,-27.4492893218813)) ;
#117644 = CARTESIAN_POINT('',(7.9,3.07928932188134,-27.9992893218813)) ;
#117645 = CARTESIAN_POINT('Origin',(1.4,2.6,-27.3785786437627)) ;
#117646 = CARTESIAN_POINT('',(1.5,2.5,-27.3785786437627)) ;
#117647 = CARTESIAN_POINT('Origin',(1.5,2.6,-27.3785786437627)) ;
#117648 = CARTESIAN_POINT('',(7.9,2.5,-27.3785786437627)) ;
#117649 = CARTESIAN_POINT('',(1.4,2.5,-27.3785786437627)) ;
#117650 = CARTESIAN_POINT('Origin',(7.9,2.6,-27.3785786437627)) ;
#117651 = CARTESIAN_POINT('Origin',(1.4,2.5,-27.27)) ;
#117652 = CARTESIAN_POINT('',(1.5,2.5,-27.27)) ;
#117653 = CARTESIAN_POINT('',(1.5,2.5,-27.27)) ;
#117654 = CARTESIAN_POINT('',(7.9,2.5,-27.27)) ;
#117655 = CARTESIAN_POINT('',(1.4,2.5,-27.27)) ;
#117656 = CARTESIAN_POINT('',(7.9,2.5,-27.3785786437627)) ;
#117657 = CARTESIAN_POINT('Origin',(1.4,2.4,-27.27)) ;
#117658 = CARTESIAN_POINT('',(1.5,2.4,-27.17)) ;
#117659 = CARTESIAN_POINT('Origin',(1.5,2.4,-27.27)) ;
#117660 = CARTESIAN_POINT('',(7.9,2.4,-27.17)) ;
#117661 = CARTESIAN_POINT('',(1.4,2.4,-27.17)) ;
#117662 = CARTESIAN_POINT('Origin',(7.9,2.4,-27.27)) ;
#117663 = CARTESIAN_POINT('Origin',(1.4,2.1,-27.17)) ;
#117664 = CARTESIAN_POINT('',(1.5,2.1,-27.17)) ;
#117665 = CARTESIAN_POINT('',(1.5,2.1,-27.17)) ;
#117666 = CARTESIAN_POINT('',(7.9,2.1,-27.17)) ;
#117667 = CARTESIAN_POINT('',(1.4,2.1,-27.17)) ;
#117668 = CARTESIAN_POINT('',(7.9,2.4,-27.17)) ;
#117669 = CARTESIAN_POINT('Origin',(1.4,2.1,-27.27)) ;
#117670 = CARTESIAN_POINT('',(1.5,2.,-27.27)) ;
#117671 = CARTESIAN_POINT('Origin',(1.5,2.1,-27.27)) ;
#117672 = CARTESIAN_POINT('',(7.9,2.,-27.27)) ;
#117673 = CARTESIAN_POINT('',(1.4,2.,-27.27)) ;
#117674 = CARTESIAN_POINT('Origin',(7.9,2.1,-27.27)) ;
#117675 = CARTESIAN_POINT('Origin',(1.4,2.,-27.27)) ;
#117676 = CARTESIAN_POINT('',(1.5,2.,-28.22)) ;
#117677 = CARTESIAN_POINT('',(1.5,2.,-28.22)) ;
#117678 = CARTESIAN_POINT('',(7.9,2.,-28.22)) ;
#117679 = CARTESIAN_POINT('',(1.4,2.,-28.22)) ;
#117680 = CARTESIAN_POINT('',(7.9,2.,-27.27)) ;
#117681 = CARTESIAN_POINT('Origin',(1.4,1.9,-28.22)) ;
#117682 = CARTESIAN_POINT('',(1.5,1.9,-28.32)) ;
#117683 = CARTESIAN_POINT('Origin',(1.5,1.9,-28.22)) ;
#117684 = CARTESIAN_POINT('',(7.9,1.9,-28.32)) ;
#117685 = CARTESIAN_POINT('',(1.4,1.9,-28.32)) ;
#117686 = CARTESIAN_POINT('Origin',(7.9,1.9,-28.22)) ;
#117687 = CARTESIAN_POINT('Origin',(1.4,1.9,-28.32)) ;
#117688 = CARTESIAN_POINT('',(1.5,-2.15,-28.32)) ;
#117689 = CARTESIAN_POINT('',(1.5,-2.15,-28.32)) ;
#117690 = CARTESIAN_POINT('',(7.9,-2.15,-28.32)) ;
#117691 = CARTESIAN_POINT('',(1.4,-2.15,-28.32)) ;
#117692 = CARTESIAN_POINT('',(7.9,1.9,-28.32)) ;
#117693 = CARTESIAN_POINT('Origin',(1.4,-2.15,-28.22)) ;
#117694 = CARTESIAN_POINT('',(1.5,-2.25,-28.22)) ;
#117695 = CARTESIAN_POINT('Origin',(1.5,-2.15,-28.22)) ;
#117696 = CARTESIAN_POINT('',(7.9,-2.25,-28.22)) ;
#117697 = CARTESIAN_POINT('',(1.4,-2.25,-28.22)) ;
#117698 = CARTESIAN_POINT('Origin',(7.9,-2.15,-28.22)) ;
#117699 = CARTESIAN_POINT('Origin',(1.4,-2.25,-27.5731195934094)) ;
#117700 = CARTESIAN_POINT('',(1.5,-2.25,-27.5731195934094)) ;
#117701 = CARTESIAN_POINT('',(1.5,-2.25,-27.5731195934094)) ;
#117702 = CARTESIAN_POINT('',(7.9,-2.25,-27.5731195934094)) ;
#117703 = CARTESIAN_POINT('',(1.4,-2.25,-27.5731195934094)) ;
#117704 = CARTESIAN_POINT('',(7.9,-2.25,-28.22)) ;
#117705 = CARTESIAN_POINT('Origin',(1.4,-2.15,-27.5731195934094)) ;
#117706 = CARTESIAN_POINT('',(1.5,-2.23576512455516,-27.5216964137135)) ;
#117707 = CARTESIAN_POINT('Origin',(1.5,-2.15,-27.5731195934094)) ;
#117708 = CARTESIAN_POINT('',(7.9,-2.23576512455516,-27.5216964137135)) ;
#117709 = CARTESIAN_POINT('',(1.4,-2.23576512455516,-27.5216964137135)) ;
#117710 = CARTESIAN_POINT('Origin',(7.9,-2.15,-27.5731195934094)) ;
#117711 = CARTESIAN_POINT('Origin',(1.4,-3.65625,-26.67)) ;
#117712 = CARTESIAN_POINT('',(1.5,-2.23576512455516,-25.8183035862865)) ;
#117713 = CARTESIAN_POINT('Origin',(1.5,-3.65625,-26.67)) ;
#117714 = CARTESIAN_POINT('',(7.9,-2.23576512455516,-25.8183035862865)) ;
#117715 = CARTESIAN_POINT('',(1.4,-2.23576512455516,-25.8183035862865)) ;
#117716 = CARTESIAN_POINT('Origin',(7.9,-3.65625,-26.67)) ;
#117717 = CARTESIAN_POINT('Origin',(1.4,-2.15,-25.7668804065906)) ;
#117718 = CARTESIAN_POINT('',(1.5,-2.25,-25.7668804065906)) ;
#117719 = CARTESIAN_POINT('Origin',(1.5,-2.15,-25.7668804065906)) ;
#117720 = CARTESIAN_POINT('',(7.9,-2.25,-25.7668804065906)) ;
#117721 = CARTESIAN_POINT('',(1.4,-2.25,-25.7668804065906)) ;
#117722 = CARTESIAN_POINT('Origin',(7.9,-2.15,-25.7668804065906)) ;
#117723 = CARTESIAN_POINT('Origin',(1.4,-2.25,-25.12)) ;
#117724 = CARTESIAN_POINT('',(1.5,-2.25,-25.12)) ;
#117725 = CARTESIAN_POINT('',(1.5,-2.25,-25.12)) ;
#117726 = CARTESIAN_POINT('',(7.9,-2.25,-25.12)) ;
#117727 = CARTESIAN_POINT('',(1.4,-2.25,-25.12)) ;
#117728 = CARTESIAN_POINT('',(7.9,-2.25,-25.7668804065906)) ;
#117729 = CARTESIAN_POINT('Origin',(1.4,-2.15,-25.12)) ;
#117730 = CARTESIAN_POINT('',(1.5,-2.15,-25.02)) ;
#117731 = CARTESIAN_POINT('Origin',(1.5,-2.15,-25.12)) ;
#117732 = CARTESIAN_POINT('',(7.9,-2.15,-25.02)) ;
#117733 = CARTESIAN_POINT('',(1.4,-2.15,-25.02)) ;
#117734 = CARTESIAN_POINT('Origin',(7.9,-2.15,-25.12)) ;
#117735 = CARTESIAN_POINT('Origin',(1.4,1.9,-25.02)) ;
#117736 = CARTESIAN_POINT('',(1.5,1.9,-25.02)) ;
#117737 = CARTESIAN_POINT('',(1.5,1.9,-25.02)) ;
#117738 = CARTESIAN_POINT('',(7.9,1.9,-25.02)) ;
#117739 = CARTESIAN_POINT('',(1.4,1.9,-25.02)) ;
#117740 = CARTESIAN_POINT('',(7.9,-2.15,-25.02)) ;
#117741 = CARTESIAN_POINT('Origin',(1.4,1.9,-25.12)) ;
#117742 = CARTESIAN_POINT('',(1.5,2.,-25.12)) ;
#117743 = CARTESIAN_POINT('Origin',(1.5,1.9,-25.12)) ;
#117744 = CARTESIAN_POINT('',(7.9,2.,-25.12)) ;
#117745 = CARTESIAN_POINT('',(1.4,2.,-25.12)) ;
#117746 = CARTESIAN_POINT('Origin',(7.9,1.9,-25.12)) ;
#117747 = CARTESIAN_POINT('Origin',(1.4,2.,-25.12)) ;
#117748 = CARTESIAN_POINT('',(1.5,2.,-26.07)) ;
#117749 = CARTESIAN_POINT('',(7.9,2.,-25.12)) ;
#117750 = CARTESIAN_POINT('Origin',(1.4,2.1,-26.07)) ;
#117751 = CARTESIAN_POINT('',(1.4,2.6,-26.07)) ;
#117752 = CARTESIAN_POINT('',(1.4,2.4,-26.27)) ;
#117753 = CARTESIAN_POINT('Origin',(1.4,2.4,-26.07)) ;
#117754 = CARTESIAN_POINT('',(1.4,2.1,-26.27)) ;
#117755 = CARTESIAN_POINT('',(1.4,2.1,-26.27)) ;
#117756 = CARTESIAN_POINT('',(1.4,1.9,-26.07)) ;
#117757 = CARTESIAN_POINT('Origin',(1.4,2.1,-26.07)) ;
#117758 = CARTESIAN_POINT('',(1.4,1.9,-25.12)) ;
#117759 = CARTESIAN_POINT('',(1.4,1.9,-25.12)) ;
#117760 = CARTESIAN_POINT('',(1.4,-2.15,-25.12)) ;
#117761 = CARTESIAN_POINT('',(1.4,-2.15,-25.12)) ;
#117762 = CARTESIAN_POINT('',(1.4,-2.15,-25.7668804065906)) ;
#117763 = CARTESIAN_POINT('',(1.4,-2.15,-25.7668804065906)) ;
#117764 = CARTESIAN_POINT('',(1.4,-2.15,-27.5731195934094)) ;
#117765 = CARTESIAN_POINT('Origin',(1.4,-3.65625,-26.67)) ;
#117766 = CARTESIAN_POINT('',(1.4,-2.15,-28.22)) ;
#117767 = CARTESIAN_POINT('',(1.4,-2.15,-28.22)) ;
#117768 = CARTESIAN_POINT('',(1.4,1.9,-28.22)) ;
#117769 = CARTESIAN_POINT('',(1.4,1.9,-28.22)) ;
#117770 = CARTESIAN_POINT('',(1.4,1.9,-27.27)) ;
#117771 = CARTESIAN_POINT('',(1.4,1.9,-27.27)) ;
#117772 = CARTESIAN_POINT('',(1.4,2.1,-27.07)) ;
#117773 = CARTESIAN_POINT('Origin',(1.4,2.1,-27.27)) ;
#117774 = CARTESIAN_POINT('',(1.4,2.4,-27.07)) ;
#117775 = CARTESIAN_POINT('',(1.4,2.4,-27.07)) ;
#117776 = CARTESIAN_POINT('',(1.4,2.6,-27.27)) ;
#117777 = CARTESIAN_POINT('Origin',(1.4,2.4,-27.27)) ;
#117778 = CARTESIAN_POINT('',(1.4,2.6,-27.3785786437627)) ;
#117779 = CARTESIAN_POINT('',(1.4,2.6,-27.3785786437627)) ;
#117780 = CARTESIAN_POINT('',(1.4,3.15,-27.9285786437627)) ;
#117781 = CARTESIAN_POINT('',(1.4,3.15,-27.9285786437627)) ;
#117782 = CARTESIAN_POINT('',(1.4,3.15,-25.4114213562373)) ;
#117783 = CARTESIAN_POINT('',(1.4,2.6,-25.9614213562373)) ;
#117784 = CARTESIAN_POINT('',(1.4,2.6,-25.9614213562373)) ;
#117785 = CARTESIAN_POINT('',(1.4,2.6,-26.07)) ;
#117786 = CARTESIAN_POINT('Origin',(1.4,2.1,-22.26)) ;
#117787 = CARTESIAN_POINT('',(1.5,2.,-22.26)) ;
#117788 = CARTESIAN_POINT('',(7.9,2.,-22.26)) ;
#117789 = CARTESIAN_POINT('',(1.4,2.,-22.26)) ;
#117790 = CARTESIAN_POINT('',(1.5,2.1,-22.36)) ;
#117791 = CARTESIAN_POINT('Origin',(1.5,2.1,-22.26)) ;
#117792 = CARTESIAN_POINT('',(7.9,2.1,-22.36)) ;
#117793 = CARTESIAN_POINT('',(1.4,2.1,-22.36)) ;
#117794 = CARTESIAN_POINT('Origin',(7.9,2.1,-22.26)) ;
#117795 = CARTESIAN_POINT('Origin',(1.4,2.4,-22.36)) ;
#117796 = CARTESIAN_POINT('',(1.5,2.4,-22.36)) ;
#117797 = CARTESIAN_POINT('',(1.5,2.4,-22.36)) ;
#117798 = CARTESIAN_POINT('',(7.9,2.4,-22.36)) ;
#117799 = CARTESIAN_POINT('',(1.4,2.4,-22.36)) ;
#117800 = CARTESIAN_POINT('',(7.9,2.1,-22.36)) ;
#117801 = CARTESIAN_POINT('Origin',(1.4,2.4,-22.26)) ;
#117802 = CARTESIAN_POINT('',(1.5,2.5,-22.26)) ;
#117803 = CARTESIAN_POINT('Origin',(1.5,2.4,-22.26)) ;
#117804 = CARTESIAN_POINT('',(7.9,2.5,-22.26)) ;
#117805 = CARTESIAN_POINT('',(1.4,2.5,-22.26)) ;
#117806 = CARTESIAN_POINT('Origin',(7.9,2.4,-22.26)) ;
#117807 = CARTESIAN_POINT('Origin',(1.4,2.5,-22.1514213562373)) ;
#117808 = CARTESIAN_POINT('',(1.5,2.5,-22.1514213562373)) ;
#117809 = CARTESIAN_POINT('',(1.5,2.5,-22.1514213562373)) ;
#117810 = CARTESIAN_POINT('',(7.9,2.5,-22.1514213562373)) ;
#117811 = CARTESIAN_POINT('',(1.4,2.5,-22.1514213562373)) ;
#117812 = CARTESIAN_POINT('',(7.9,2.5,-22.26)) ;
#117813 = CARTESIAN_POINT('Origin',(1.4,2.6,-22.1514213562373)) ;
#117814 = CARTESIAN_POINT('',(1.5,2.52928932188135,-22.0807106781187)) ;
#117815 = CARTESIAN_POINT('Origin',(1.5,2.6,-22.1514213562373)) ;
#117816 = CARTESIAN_POINT('',(7.9,2.52928932188135,-22.0807106781187)) ;
#117817 = CARTESIAN_POINT('',(1.4,2.52928932188135,-22.0807106781187)) ;
#117818 = CARTESIAN_POINT('Origin',(7.9,2.6,-22.1514213562373)) ;
#117819 = CARTESIAN_POINT('Origin',(1.4,3.07928932188135,-21.5307106781187)) ;
#117820 = CARTESIAN_POINT('',(1.5,3.07928932188135,-21.5307106781187)) ;
#117821 = CARTESIAN_POINT('',(7.9,3.07928932188135,-21.5307106781187)) ;
#117822 = CARTESIAN_POINT('',(1.4,3.07928932188135,-21.5307106781187)) ;
#117823 = CARTESIAN_POINT('',(7.9,2.52928932188135,-22.0807106781187)) ;
#117824 = CARTESIAN_POINT('Origin',(1.4,3.15,-21.6014213562373)) ;
#117825 = CARTESIAN_POINT('',(7.9,3.25,-21.6014213562373)) ;
#117826 = CARTESIAN_POINT('',(1.4,3.25,-21.6014213562373)) ;
#117827 = CARTESIAN_POINT('Origin',(7.9,3.15,-21.6014213562373)) ;
#117828 = CARTESIAN_POINT('Origin',(1.4,3.25,-24.1185786437627)) ;
#117829 = CARTESIAN_POINT('',(1.5,3.25,-24.1185786437627)) ;
#117830 = CARTESIAN_POINT('',(7.9,3.25,-21.6014213562373)) ;
#117831 = CARTESIAN_POINT('Origin',(1.4,2.52928932188134,-23.6392893218813)) ;
#117832 = CARTESIAN_POINT('',(1.5,2.52928932188134,-23.6392893218813)) ;
#117833 = CARTESIAN_POINT('',(1.5,2.52928932188135,-23.6392893218813)) ;
#117834 = CARTESIAN_POINT('',(7.9,2.52928932188134,-23.6392893218813)) ;
#117835 = CARTESIAN_POINT('',(1.4,2.52928932188134,-23.6392893218813)) ;
#117836 = CARTESIAN_POINT('',(7.9,3.07928932188134,-24.1892893218813)) ;
#117837 = CARTESIAN_POINT('Origin',(1.4,2.6,-23.5685786437627)) ;
#117838 = CARTESIAN_POINT('',(1.5,2.5,-23.5685786437627)) ;
#117839 = CARTESIAN_POINT('Origin',(1.5,2.6,-23.5685786437627)) ;
#117840 = CARTESIAN_POINT('',(7.9,2.5,-23.5685786437627)) ;
#117841 = CARTESIAN_POINT('',(1.4,2.5,-23.5685786437627)) ;
#117842 = CARTESIAN_POINT('Origin',(7.9,2.6,-23.5685786437627)) ;
#117843 = CARTESIAN_POINT('Origin',(1.4,2.5,-23.46)) ;
#117844 = CARTESIAN_POINT('',(1.5,2.5,-23.46)) ;
#117845 = CARTESIAN_POINT('',(1.5,2.5,-23.46)) ;
#117846 = CARTESIAN_POINT('',(7.9,2.5,-23.46)) ;
#117847 = CARTESIAN_POINT('',(1.4,2.5,-23.46)) ;
#117848 = CARTESIAN_POINT('',(7.9,2.5,-23.5685786437627)) ;
#117849 = CARTESIAN_POINT('Origin',(1.4,2.4,-23.46)) ;
#117850 = CARTESIAN_POINT('',(1.5,2.4,-23.36)) ;
#117851 = CARTESIAN_POINT('Origin',(1.5,2.4,-23.46)) ;
#117852 = CARTESIAN_POINT('',(7.9,2.4,-23.36)) ;
#117853 = CARTESIAN_POINT('',(1.4,2.4,-23.36)) ;
#117854 = CARTESIAN_POINT('Origin',(7.9,2.4,-23.46)) ;
#117855 = CARTESIAN_POINT('Origin',(1.4,2.1,-23.36)) ;
#117856 = CARTESIAN_POINT('',(1.5,2.1,-23.36)) ;
#117857 = CARTESIAN_POINT('',(1.5,2.1,-23.36)) ;
#117858 = CARTESIAN_POINT('',(7.9,2.1,-23.36)) ;
#117859 = CARTESIAN_POINT('',(1.4,2.1,-23.36)) ;
#117860 = CARTESIAN_POINT('',(7.9,2.4,-23.36)) ;
#117861 = CARTESIAN_POINT('Origin',(1.4,2.1,-23.46)) ;
#117862 = CARTESIAN_POINT('',(1.5,2.,-23.46)) ;
#117863 = CARTESIAN_POINT('Origin',(1.5,2.1,-23.46)) ;
#117864 = CARTESIAN_POINT('',(7.9,2.,-23.46)) ;
#117865 = CARTESIAN_POINT('',(1.4,2.,-23.46)) ;
#117866 = CARTESIAN_POINT('Origin',(7.9,2.1,-23.46)) ;
#117867 = CARTESIAN_POINT('Origin',(1.4,2.,-23.46)) ;
#117868 = CARTESIAN_POINT('',(1.5,2.,-24.41)) ;
#117869 = CARTESIAN_POINT('',(1.5,2.,-24.41)) ;
#117870 = CARTESIAN_POINT('',(7.9,2.,-24.41)) ;
#117871 = CARTESIAN_POINT('',(1.4,2.,-24.41)) ;
#117872 = CARTESIAN_POINT('',(7.9,2.,-23.46)) ;
#117873 = CARTESIAN_POINT('Origin',(1.4,1.9,-24.41)) ;
#117874 = CARTESIAN_POINT('',(1.5,1.9,-24.51)) ;
#117875 = CARTESIAN_POINT('Origin',(1.5,1.9,-24.41)) ;
#117876 = CARTESIAN_POINT('',(7.9,1.9,-24.51)) ;
#117877 = CARTESIAN_POINT('',(1.4,1.9,-24.51)) ;
#117878 = CARTESIAN_POINT('Origin',(7.9,1.9,-24.41)) ;
#117879 = CARTESIAN_POINT('Origin',(1.4,1.9,-24.51)) ;
#117880 = CARTESIAN_POINT('',(1.5,-2.15,-24.51)) ;
#117881 = CARTESIAN_POINT('',(1.5,-2.15,-24.51)) ;
#117882 = CARTESIAN_POINT('',(7.9,-2.15,-24.51)) ;
#117883 = CARTESIAN_POINT('',(1.4,-2.15,-24.51)) ;
#117884 = CARTESIAN_POINT('',(7.9,1.9,-24.51)) ;
#117885 = CARTESIAN_POINT('Origin',(1.4,-2.15,-24.41)) ;
#117886 = CARTESIAN_POINT('',(1.5,-2.25,-24.41)) ;
#117887 = CARTESIAN_POINT('Origin',(1.5,-2.15,-24.41)) ;
#117888 = CARTESIAN_POINT('',(7.9,-2.25,-24.41)) ;
#117889 = CARTESIAN_POINT('',(1.4,-2.25,-24.41)) ;
#117890 = CARTESIAN_POINT('Origin',(7.9,-2.15,-24.41)) ;
#117891 = CARTESIAN_POINT('Origin',(1.4,-2.25,-23.7631195934094)) ;
#117892 = CARTESIAN_POINT('',(1.5,-2.25,-23.7631195934094)) ;
#117893 = CARTESIAN_POINT('',(1.5,-2.25,-23.7631195934094)) ;
#117894 = CARTESIAN_POINT('',(7.9,-2.25,-23.7631195934094)) ;
#117895 = CARTESIAN_POINT('',(1.4,-2.25,-23.7631195934094)) ;
#117896 = CARTESIAN_POINT('',(7.9,-2.25,-24.41)) ;
#117897 = CARTESIAN_POINT('Origin',(1.4,-2.15,-23.7631195934094)) ;
#117898 = CARTESIAN_POINT('',(1.5,-2.23576512455516,-23.7116964137135)) ;
#117899 = CARTESIAN_POINT('Origin',(1.5,-2.15,-23.7631195934094)) ;
#117900 = CARTESIAN_POINT('',(7.9,-2.23576512455516,-23.7116964137135)) ;
#117901 = CARTESIAN_POINT('',(1.4,-2.23576512455516,-23.7116964137135)) ;
#117902 = CARTESIAN_POINT('Origin',(7.9,-2.15,-23.7631195934094)) ;
#117903 = CARTESIAN_POINT('Origin',(1.4,-3.65625,-22.86)) ;
#117904 = CARTESIAN_POINT('',(1.5,-2.23576512455516,-22.0083035862865)) ;
#117905 = CARTESIAN_POINT('Origin',(1.5,-3.65625,-22.86)) ;
#117906 = CARTESIAN_POINT('',(7.9,-2.23576512455516,-22.0083035862865)) ;
#117907 = CARTESIAN_POINT('',(1.4,-2.23576512455516,-22.0083035862865)) ;
#117908 = CARTESIAN_POINT('Origin',(7.9,-3.65625,-22.86)) ;
#117909 = CARTESIAN_POINT('Origin',(1.4,-2.15,-21.9568804065906)) ;
#117910 = CARTESIAN_POINT('',(1.5,-2.25,-21.9568804065906)) ;
#117911 = CARTESIAN_POINT('Origin',(1.5,-2.15,-21.9568804065906)) ;
#117912 = CARTESIAN_POINT('',(7.9,-2.25,-21.9568804065906)) ;
#117913 = CARTESIAN_POINT('',(1.4,-2.25,-21.9568804065906)) ;
#117914 = CARTESIAN_POINT('Origin',(7.9,-2.15,-21.9568804065906)) ;
#117915 = CARTESIAN_POINT('Origin',(1.4,-2.25,-21.31)) ;
#117916 = CARTESIAN_POINT('',(1.5,-2.25,-21.31)) ;
#117917 = CARTESIAN_POINT('',(1.5,-2.25,-21.31)) ;
#117918 = CARTESIAN_POINT('',(7.9,-2.25,-21.31)) ;
#117919 = CARTESIAN_POINT('',(1.4,-2.25,-21.31)) ;
#117920 = CARTESIAN_POINT('',(7.9,-2.25,-21.9568804065906)) ;
#117921 = CARTESIAN_POINT('Origin',(1.4,-2.15,-21.31)) ;
#117922 = CARTESIAN_POINT('',(1.5,-2.15,-21.21)) ;
#117923 = CARTESIAN_POINT('Origin',(1.5,-2.15,-21.31)) ;
#117924 = CARTESIAN_POINT('',(7.9,-2.15,-21.21)) ;
#117925 = CARTESIAN_POINT('',(1.4,-2.15,-21.21)) ;
#117926 = CARTESIAN_POINT('Origin',(7.9,-2.15,-21.31)) ;
#117927 = CARTESIAN_POINT('Origin',(1.4,1.9,-21.21)) ;
#117928 = CARTESIAN_POINT('',(1.5,1.9,-21.21)) ;
#117929 = CARTESIAN_POINT('',(1.5,1.9,-21.21)) ;
#117930 = CARTESIAN_POINT('',(7.9,1.9,-21.21)) ;
#117931 = CARTESIAN_POINT('',(1.4,1.9,-21.21)) ;
#117932 = CARTESIAN_POINT('',(7.9,-2.15,-21.21)) ;
#117933 = CARTESIAN_POINT('Origin',(1.4,1.9,-21.31)) ;
#117934 = CARTESIAN_POINT('',(1.5,2.,-21.31)) ;
#117935 = CARTESIAN_POINT('Origin',(1.5,1.9,-21.31)) ;
#117936 = CARTESIAN_POINT('',(7.9,2.,-21.31)) ;
#117937 = CARTESIAN_POINT('',(1.4,2.,-21.31)) ;
#117938 = CARTESIAN_POINT('Origin',(7.9,1.9,-21.31)) ;
#117939 = CARTESIAN_POINT('Origin',(1.4,2.,-21.31)) ;
#117940 = CARTESIAN_POINT('',(1.5,2.,-22.26)) ;
#117941 = CARTESIAN_POINT('',(7.9,2.,-21.31)) ;
#117942 = CARTESIAN_POINT('Origin',(1.4,2.1,-22.26)) ;
#117943 = CARTESIAN_POINT('',(1.4,2.6,-22.26)) ;
#117944 = CARTESIAN_POINT('',(1.4,2.4,-22.46)) ;
#117945 = CARTESIAN_POINT('Origin',(1.4,2.4,-22.26)) ;
#117946 = CARTESIAN_POINT('',(1.4,2.1,-22.46)) ;
#117947 = CARTESIAN_POINT('',(1.4,2.1,-22.46)) ;
#117948 = CARTESIAN_POINT('',(1.4,1.9,-22.26)) ;
#117949 = CARTESIAN_POINT('Origin',(1.4,2.1,-22.26)) ;
#117950 = CARTESIAN_POINT('',(1.4,1.9,-21.31)) ;
#117951 = CARTESIAN_POINT('',(1.4,1.9,-21.31)) ;
#117952 = CARTESIAN_POINT('',(1.4,-2.15,-21.31)) ;
#117953 = CARTESIAN_POINT('',(1.4,-2.15,-21.31)) ;
#117954 = CARTESIAN_POINT('',(1.4,-2.15,-21.9568804065906)) ;
#117955 = CARTESIAN_POINT('',(1.4,-2.15,-21.9568804065906)) ;
#117956 = CARTESIAN_POINT('',(1.4,-2.15,-23.7631195934094)) ;
#117957 = CARTESIAN_POINT('Origin',(1.4,-3.65625,-22.86)) ;
#117958 = CARTESIAN_POINT('',(1.4,-2.15,-24.41)) ;
#117959 = CARTESIAN_POINT('',(1.4,-2.15,-24.41)) ;
#117960 = CARTESIAN_POINT('',(1.4,1.9,-24.41)) ;
#117961 = CARTESIAN_POINT('',(1.4,1.9,-24.41)) ;
#117962 = CARTESIAN_POINT('',(1.4,1.9,-23.46)) ;
#117963 = CARTESIAN_POINT('',(1.4,1.9,-23.46)) ;
#117964 = CARTESIAN_POINT('',(1.4,2.1,-23.26)) ;
#117965 = CARTESIAN_POINT('Origin',(1.4,2.1,-23.46)) ;
#117966 = CARTESIAN_POINT('',(1.4,2.4,-23.26)) ;
#117967 = CARTESIAN_POINT('',(1.4,2.4,-23.26)) ;
#117968 = CARTESIAN_POINT('',(1.4,2.6,-23.46)) ;
#117969 = CARTESIAN_POINT('Origin',(1.4,2.4,-23.46)) ;
#117970 = CARTESIAN_POINT('',(1.4,2.6,-23.5685786437627)) ;
#117971 = CARTESIAN_POINT('',(1.4,2.6,-23.5685786437627)) ;
#117972 = CARTESIAN_POINT('',(1.4,3.15,-24.1185786437627)) ;
#117973 = CARTESIAN_POINT('',(1.4,3.15,-24.1185786437627)) ;
#117974 = CARTESIAN_POINT('',(1.4,3.15,-21.6014213562373)) ;
#117975 = CARTESIAN_POINT('',(1.4,2.6,-22.1514213562373)) ;
#117976 = CARTESIAN_POINT('',(1.4,2.6,-22.1514213562373)) ;
#117977 = CARTESIAN_POINT('',(1.4,2.6,-22.26)) ;
#117978 = CARTESIAN_POINT('Origin',(1.4,2.1,-18.45)) ;
#117979 = CARTESIAN_POINT('',(1.5,2.,-18.45)) ;
#117980 = CARTESIAN_POINT('',(7.9,2.,-18.45)) ;
#117981 = CARTESIAN_POINT('',(1.4,2.,-18.45)) ;
#117982 = CARTESIAN_POINT('',(1.5,2.1,-18.55)) ;
#117983 = CARTESIAN_POINT('Origin',(1.5,2.1,-18.45)) ;
#117984 = CARTESIAN_POINT('',(7.9,2.1,-18.55)) ;
#117985 = CARTESIAN_POINT('',(1.4,2.1,-18.55)) ;
#117986 = CARTESIAN_POINT('Origin',(7.9,2.1,-18.45)) ;
#117987 = CARTESIAN_POINT('Origin',(1.4,2.4,-18.55)) ;
#117988 = CARTESIAN_POINT('',(1.5,2.4,-18.55)) ;
#117989 = CARTESIAN_POINT('',(1.5,2.4,-18.55)) ;
#117990 = CARTESIAN_POINT('',(7.9,2.4,-18.55)) ;
#117991 = CARTESIAN_POINT('',(1.4,2.4,-18.55)) ;
#117992 = CARTESIAN_POINT('',(7.9,2.1,-18.55)) ;
#117993 = CARTESIAN_POINT('Origin',(1.4,2.4,-18.45)) ;
#117994 = CARTESIAN_POINT('',(1.5,2.5,-18.45)) ;
#117995 = CARTESIAN_POINT('Origin',(1.5,2.4,-18.45)) ;
#117996 = CARTESIAN_POINT('',(7.9,2.5,-18.45)) ;
#117997 = CARTESIAN_POINT('',(1.4,2.5,-18.45)) ;
#117998 = CARTESIAN_POINT('Origin',(7.9,2.4,-18.45)) ;
#117999 = CARTESIAN_POINT('Origin',(1.4,2.5,-18.3414213562373)) ;
#118000 = CARTESIAN_POINT('',(1.5,2.5,-18.3414213562373)) ;
#118001 = CARTESIAN_POINT('',(1.5,2.5,-18.3414213562373)) ;
#118002 = CARTESIAN_POINT('',(7.9,2.5,-18.3414213562373)) ;
#118003 = CARTESIAN_POINT('',(1.4,2.5,-18.3414213562373)) ;
#118004 = CARTESIAN_POINT('',(7.9,2.5,-18.45)) ;
#118005 = CARTESIAN_POINT('Origin',(1.4,2.6,-18.3414213562373)) ;
#118006 = CARTESIAN_POINT('',(1.5,2.52928932188135,-18.2707106781187)) ;
#118007 = CARTESIAN_POINT('Origin',(1.5,2.6,-18.3414213562373)) ;
#118008 = CARTESIAN_POINT('',(7.9,2.52928932188135,-18.2707106781187)) ;
#118009 = CARTESIAN_POINT('',(1.4,2.52928932188135,-18.2707106781187)) ;
#118010 = CARTESIAN_POINT('Origin',(7.9,2.6,-18.3414213562373)) ;
#118011 = CARTESIAN_POINT('Origin',(1.4,3.07928932188135,-17.7207106781187)) ;
#118012 = CARTESIAN_POINT('',(1.5,3.07928932188135,-17.7207106781187)) ;
#118013 = CARTESIAN_POINT('',(7.9,3.07928932188135,-17.7207106781187)) ;
#118014 = CARTESIAN_POINT('',(1.4,3.07928932188135,-17.7207106781187)) ;
#118015 = CARTESIAN_POINT('',(7.9,2.52928932188135,-18.2707106781187)) ;
#118016 = CARTESIAN_POINT('Origin',(1.4,3.15,-17.7914213562373)) ;
#118017 = CARTESIAN_POINT('',(7.9,3.25,-17.7914213562373)) ;
#118018 = CARTESIAN_POINT('',(1.4,3.25,-17.7914213562373)) ;
#118019 = CARTESIAN_POINT('Origin',(7.9,3.15,-17.7914213562373)) ;
#118020 = CARTESIAN_POINT('Origin',(1.4,3.25,-20.3085786437627)) ;
#118021 = CARTESIAN_POINT('',(1.5,3.25,-20.3085786437627)) ;
#118022 = CARTESIAN_POINT('',(7.9,3.25,-17.7914213562373)) ;
#118023 = CARTESIAN_POINT('Origin',(1.4,2.52928932188134,-19.8292893218813)) ;
#118024 = CARTESIAN_POINT('',(1.5,2.52928932188134,-19.8292893218813)) ;
#118025 = CARTESIAN_POINT('',(1.5,2.52928932188135,-19.8292893218813)) ;
#118026 = CARTESIAN_POINT('',(7.9,2.52928932188134,-19.8292893218813)) ;
#118027 = CARTESIAN_POINT('',(1.4,2.52928932188134,-19.8292893218813)) ;
#118028 = CARTESIAN_POINT('',(7.9,3.07928932188134,-20.3792893218813)) ;
#118029 = CARTESIAN_POINT('Origin',(1.4,2.6,-19.7585786437627)) ;
#118030 = CARTESIAN_POINT('',(1.5,2.5,-19.7585786437627)) ;
#118031 = CARTESIAN_POINT('Origin',(1.5,2.6,-19.7585786437627)) ;
#118032 = CARTESIAN_POINT('',(7.9,2.5,-19.7585786437627)) ;
#118033 = CARTESIAN_POINT('',(1.4,2.5,-19.7585786437627)) ;
#118034 = CARTESIAN_POINT('Origin',(7.9,2.6,-19.7585786437627)) ;
#118035 = CARTESIAN_POINT('Origin',(1.4,2.5,-19.65)) ;
#118036 = CARTESIAN_POINT('',(1.5,2.5,-19.65)) ;
#118037 = CARTESIAN_POINT('',(1.5,2.5,-19.65)) ;
#118038 = CARTESIAN_POINT('',(7.9,2.5,-19.65)) ;
#118039 = CARTESIAN_POINT('',(1.4,2.5,-19.65)) ;
#118040 = CARTESIAN_POINT('',(7.9,2.5,-19.7585786437627)) ;
#118041 = CARTESIAN_POINT('Origin',(1.4,2.4,-19.65)) ;
#118042 = CARTESIAN_POINT('',(1.5,2.4,-19.55)) ;
#118043 = CARTESIAN_POINT('Origin',(1.5,2.4,-19.65)) ;
#118044 = CARTESIAN_POINT('',(7.9,2.4,-19.55)) ;
#118045 = CARTESIAN_POINT('',(1.4,2.4,-19.55)) ;
#118046 = CARTESIAN_POINT('Origin',(7.9,2.4,-19.65)) ;
#118047 = CARTESIAN_POINT('Origin',(1.4,2.1,-19.55)) ;
#118048 = CARTESIAN_POINT('',(1.5,2.1,-19.55)) ;
#118049 = CARTESIAN_POINT('',(1.5,2.1,-19.55)) ;
#118050 = CARTESIAN_POINT('',(7.9,2.1,-19.55)) ;
#118051 = CARTESIAN_POINT('',(1.4,2.1,-19.55)) ;
#118052 = CARTESIAN_POINT('',(7.9,2.4,-19.55)) ;
#118053 = CARTESIAN_POINT('Origin',(1.4,2.1,-19.65)) ;
#118054 = CARTESIAN_POINT('',(1.5,2.,-19.65)) ;
#118055 = CARTESIAN_POINT('Origin',(1.5,2.1,-19.65)) ;
#118056 = CARTESIAN_POINT('',(7.9,2.,-19.65)) ;
#118057 = CARTESIAN_POINT('',(1.4,2.,-19.65)) ;
#118058 = CARTESIAN_POINT('Origin',(7.9,2.1,-19.65)) ;
#118059 = CARTESIAN_POINT('Origin',(1.4,2.,-19.65)) ;
#118060 = CARTESIAN_POINT('',(1.5,2.,-20.6)) ;
#118061 = CARTESIAN_POINT('',(1.5,2.,-20.6)) ;
#118062 = CARTESIAN_POINT('',(7.9,2.,-20.6)) ;
#118063 = CARTESIAN_POINT('',(1.4,2.,-20.6)) ;
#118064 = CARTESIAN_POINT('',(7.9,2.,-19.65)) ;
#118065 = CARTESIAN_POINT('Origin',(1.4,1.9,-20.6)) ;
#118066 = CARTESIAN_POINT('',(1.5,1.9,-20.7)) ;
#118067 = CARTESIAN_POINT('Origin',(1.5,1.9,-20.6)) ;
#118068 = CARTESIAN_POINT('',(7.9,1.9,-20.7)) ;
#118069 = CARTESIAN_POINT('',(1.4,1.9,-20.7)) ;
#118070 = CARTESIAN_POINT('Origin',(7.9,1.9,-20.6)) ;
#118071 = CARTESIAN_POINT('Origin',(1.4,1.9,-20.7)) ;
#118072 = CARTESIAN_POINT('',(1.5,-2.15,-20.7)) ;
#118073 = CARTESIAN_POINT('',(1.5,-2.15,-20.7)) ;
#118074 = CARTESIAN_POINT('',(7.9,-2.15,-20.7)) ;
#118075 = CARTESIAN_POINT('',(1.4,-2.15,-20.7)) ;
#118076 = CARTESIAN_POINT('',(7.9,1.9,-20.7)) ;
#118077 = CARTESIAN_POINT('Origin',(1.4,-2.15,-20.6)) ;
#118078 = CARTESIAN_POINT('',(1.5,-2.25,-20.6)) ;
#118079 = CARTESIAN_POINT('Origin',(1.5,-2.15,-20.6)) ;
#118080 = CARTESIAN_POINT('',(7.9,-2.25,-20.6)) ;
#118081 = CARTESIAN_POINT('',(1.4,-2.25,-20.6)) ;
#118082 = CARTESIAN_POINT('Origin',(7.9,-2.15,-20.6)) ;
#118083 = CARTESIAN_POINT('Origin',(1.4,-2.25,-19.9531195934094)) ;
#118084 = CARTESIAN_POINT('',(1.5,-2.25,-19.9531195934094)) ;
#118085 = CARTESIAN_POINT('',(1.5,-2.25,-19.9531195934094)) ;
#118086 = CARTESIAN_POINT('',(7.9,-2.25,-19.9531195934094)) ;
#118087 = CARTESIAN_POINT('',(1.4,-2.25,-19.9531195934094)) ;
#118088 = CARTESIAN_POINT('',(7.9,-2.25,-20.6)) ;
#118089 = CARTESIAN_POINT('Origin',(1.4,-2.15,-19.9531195934094)) ;
#118090 = CARTESIAN_POINT('',(1.5,-2.23576512455516,-19.9016964137135)) ;
#118091 = CARTESIAN_POINT('Origin',(1.5,-2.15,-19.9531195934094)) ;
#118092 = CARTESIAN_POINT('',(7.9,-2.23576512455516,-19.9016964137135)) ;
#118093 = CARTESIAN_POINT('',(1.4,-2.23576512455516,-19.9016964137135)) ;
#118094 = CARTESIAN_POINT('Origin',(7.9,-2.15,-19.9531195934094)) ;
#118095 = CARTESIAN_POINT('Origin',(1.4,-3.65625,-19.05)) ;
#118096 = CARTESIAN_POINT('',(1.5,-2.23576512455516,-18.1983035862865)) ;
#118097 = CARTESIAN_POINT('Origin',(1.5,-3.65625,-19.05)) ;
#118098 = CARTESIAN_POINT('',(7.9,-2.23576512455516,-18.1983035862865)) ;
#118099 = CARTESIAN_POINT('',(1.4,-2.23576512455516,-18.1983035862865)) ;
#118100 = CARTESIAN_POINT('Origin',(7.9,-3.65625,-19.05)) ;
#118101 = CARTESIAN_POINT('Origin',(1.4,-2.15,-18.1468804065906)) ;
#118102 = CARTESIAN_POINT('',(1.5,-2.25,-18.1468804065906)) ;
#118103 = CARTESIAN_POINT('Origin',(1.5,-2.15,-18.1468804065906)) ;
#118104 = CARTESIAN_POINT('',(7.9,-2.25,-18.1468804065906)) ;
#118105 = CARTESIAN_POINT('',(1.4,-2.25,-18.1468804065906)) ;
#118106 = CARTESIAN_POINT('Origin',(7.9,-2.15,-18.1468804065906)) ;
#118107 = CARTESIAN_POINT('Origin',(1.4,-2.25,-17.5)) ;
#118108 = CARTESIAN_POINT('',(1.5,-2.25,-17.5)) ;
#118109 = CARTESIAN_POINT('',(1.5,-2.25,-17.5)) ;
#118110 = CARTESIAN_POINT('',(7.9,-2.25,-17.5)) ;
#118111 = CARTESIAN_POINT('',(1.4,-2.25,-17.5)) ;
#118112 = CARTESIAN_POINT('',(7.9,-2.25,-18.1468804065906)) ;
#118113 = CARTESIAN_POINT('Origin',(1.4,-2.15,-17.5)) ;
#118114 = CARTESIAN_POINT('',(1.5,-2.15,-17.4)) ;
#118115 = CARTESIAN_POINT('Origin',(1.5,-2.15,-17.5)) ;
#118116 = CARTESIAN_POINT('',(7.9,-2.15,-17.4)) ;
#118117 = CARTESIAN_POINT('',(1.4,-2.15,-17.4)) ;
#118118 = CARTESIAN_POINT('Origin',(7.9,-2.15,-17.5)) ;
#118119 = CARTESIAN_POINT('Origin',(1.4,1.9,-17.4)) ;
#118120 = CARTESIAN_POINT('',(1.5,1.9,-17.4)) ;
#118121 = CARTESIAN_POINT('',(1.5,1.9,-17.4)) ;
#118122 = CARTESIAN_POINT('',(7.9,1.9,-17.4)) ;
#118123 = CARTESIAN_POINT('',(1.4,1.9,-17.4)) ;
#118124 = CARTESIAN_POINT('',(7.9,-2.15,-17.4)) ;
#118125 = CARTESIAN_POINT('Origin',(1.4,1.9,-17.5)) ;
#118126 = CARTESIAN_POINT('',(1.5,2.,-17.5)) ;
#118127 = CARTESIAN_POINT('Origin',(1.5,1.9,-17.5)) ;
#118128 = CARTESIAN_POINT('',(7.9,2.,-17.5)) ;
#118129 = CARTESIAN_POINT('',(1.4,2.,-17.5)) ;
#118130 = CARTESIAN_POINT('Origin',(7.9,1.9,-17.5)) ;
#118131 = CARTESIAN_POINT('Origin',(1.4,2.,-17.5)) ;
#118132 = CARTESIAN_POINT('',(1.5,2.,-18.45)) ;
#118133 = CARTESIAN_POINT('',(7.9,2.,-17.5)) ;
#118134 = CARTESIAN_POINT('Origin',(1.4,2.1,-18.45)) ;
#118135 = CARTESIAN_POINT('',(1.4,2.6,-18.45)) ;
#118136 = CARTESIAN_POINT('',(1.4,2.4,-18.65)) ;
#118137 = CARTESIAN_POINT('Origin',(1.4,2.4,-18.45)) ;
#118138 = CARTESIAN_POINT('',(1.4,2.1,-18.65)) ;
#118139 = CARTESIAN_POINT('',(1.4,2.1,-18.65)) ;
#118140 = CARTESIAN_POINT('',(1.4,1.9,-18.45)) ;
#118141 = CARTESIAN_POINT('Origin',(1.4,2.1,-18.45)) ;
#118142 = CARTESIAN_POINT('',(1.4,1.9,-17.5)) ;
#118143 = CARTESIAN_POINT('',(1.4,1.9,-17.5)) ;
#118144 = CARTESIAN_POINT('',(1.4,-2.15,-17.5)) ;
#118145 = CARTESIAN_POINT('',(1.4,-2.15,-17.5)) ;
#118146 = CARTESIAN_POINT('',(1.4,-2.15,-18.1468804065906)) ;
#118147 = CARTESIAN_POINT('',(1.4,-2.15,-18.1468804065906)) ;
#118148 = CARTESIAN_POINT('',(1.4,-2.15,-19.9531195934094)) ;
#118149 = CARTESIAN_POINT('Origin',(1.4,-3.65625,-19.05)) ;
#118150 = CARTESIAN_POINT('',(1.4,-2.15,-20.6)) ;
#118151 = CARTESIAN_POINT('',(1.4,-2.15,-20.6)) ;
#118152 = CARTESIAN_POINT('',(1.4,1.9,-20.6)) ;
#118153 = CARTESIAN_POINT('',(1.4,1.9,-20.6)) ;
#118154 = CARTESIAN_POINT('',(1.4,1.9,-19.65)) ;
#118155 = CARTESIAN_POINT('',(1.4,1.9,-19.65)) ;
#118156 = CARTESIAN_POINT('',(1.4,2.1,-19.45)) ;
#118157 = CARTESIAN_POINT('Origin',(1.4,2.1,-19.65)) ;
#118158 = CARTESIAN_POINT('',(1.4,2.4,-19.45)) ;
#118159 = CARTESIAN_POINT('',(1.4,2.4,-19.45)) ;
#118160 = CARTESIAN_POINT('',(1.4,2.6,-19.65)) ;
#118161 = CARTESIAN_POINT('Origin',(1.4,2.4,-19.65)) ;
#118162 = CARTESIAN_POINT('',(1.4,2.6,-19.7585786437627)) ;
#118163 = CARTESIAN_POINT('',(1.4,2.6,-19.7585786437627)) ;
#118164 = CARTESIAN_POINT('',(1.4,3.15,-20.3085786437627)) ;
#118165 = CARTESIAN_POINT('',(1.4,3.15,-20.3085786437627)) ;
#118166 = CARTESIAN_POINT('',(1.4,3.15,-17.7914213562373)) ;
#118167 = CARTESIAN_POINT('',(1.4,2.6,-18.3414213562373)) ;
#118168 = CARTESIAN_POINT('',(1.4,2.6,-18.3414213562373)) ;
#118169 = CARTESIAN_POINT('',(1.4,2.6,-18.45)) ;
#118170 = CARTESIAN_POINT('Origin',(1.4,2.1,-14.64)) ;
#118171 = CARTESIAN_POINT('',(1.5,2.,-14.64)) ;
#118172 = CARTESIAN_POINT('',(7.9,2.,-14.64)) ;
#118173 = CARTESIAN_POINT('',(1.4,2.,-14.64)) ;
#118174 = CARTESIAN_POINT('',(1.5,2.1,-14.74)) ;
#118175 = CARTESIAN_POINT('Origin',(1.5,2.1,-14.64)) ;
#118176 = CARTESIAN_POINT('',(7.9,2.1,-14.74)) ;
#118177 = CARTESIAN_POINT('',(1.4,2.1,-14.74)) ;
#118178 = CARTESIAN_POINT('Origin',(7.9,2.1,-14.64)) ;
#118179 = CARTESIAN_POINT('Origin',(1.4,2.4,-14.74)) ;
#118180 = CARTESIAN_POINT('',(1.5,2.4,-14.74)) ;
#118181 = CARTESIAN_POINT('',(1.5,2.4,-14.74)) ;
#118182 = CARTESIAN_POINT('',(7.9,2.4,-14.74)) ;
#118183 = CARTESIAN_POINT('',(1.4,2.4,-14.74)) ;
#118184 = CARTESIAN_POINT('',(7.9,2.1,-14.74)) ;
#118185 = CARTESIAN_POINT('Origin',(1.4,2.4,-14.64)) ;
#118186 = CARTESIAN_POINT('',(1.5,2.5,-14.64)) ;
#118187 = CARTESIAN_POINT('Origin',(1.5,2.4,-14.64)) ;
#118188 = CARTESIAN_POINT('',(7.9,2.5,-14.64)) ;
#118189 = CARTESIAN_POINT('',(1.4,2.5,-14.64)) ;
#118190 = CARTESIAN_POINT('Origin',(7.9,2.4,-14.64)) ;
#118191 = CARTESIAN_POINT('Origin',(1.4,2.5,-14.5314213562373)) ;
#118192 = CARTESIAN_POINT('',(1.5,2.5,-14.5314213562373)) ;
#118193 = CARTESIAN_POINT('',(1.5,2.5,-14.5314213562373)) ;
#118194 = CARTESIAN_POINT('',(7.9,2.5,-14.5314213562373)) ;
#118195 = CARTESIAN_POINT('',(1.4,2.5,-14.5314213562373)) ;
#118196 = CARTESIAN_POINT('',(7.9,2.5,-14.64)) ;
#118197 = CARTESIAN_POINT('Origin',(1.4,2.6,-14.5314213562373)) ;
#118198 = CARTESIAN_POINT('',(1.5,2.52928932188135,-14.4607106781187)) ;
#118199 = CARTESIAN_POINT('Origin',(1.5,2.6,-14.5314213562373)) ;
#118200 = CARTESIAN_POINT('',(7.9,2.52928932188135,-14.4607106781187)) ;
#118201 = CARTESIAN_POINT('',(1.4,2.52928932188135,-14.4607106781187)) ;
#118202 = CARTESIAN_POINT('Origin',(7.9,2.6,-14.5314213562373)) ;
#118203 = CARTESIAN_POINT('Origin',(1.4,3.07928932188135,-13.9107106781187)) ;
#118204 = CARTESIAN_POINT('',(1.5,3.07928932188135,-13.9107106781187)) ;
#118205 = CARTESIAN_POINT('',(7.9,3.07928932188135,-13.9107106781187)) ;
#118206 = CARTESIAN_POINT('',(1.4,3.07928932188135,-13.9107106781187)) ;
#118207 = CARTESIAN_POINT('',(7.9,2.52928932188135,-14.4607106781187)) ;
#118208 = CARTESIAN_POINT('Origin',(1.4,3.15,-13.9814213562373)) ;
#118209 = CARTESIAN_POINT('',(7.9,3.25,-13.9814213562373)) ;
#118210 = CARTESIAN_POINT('',(1.4,3.25,-13.9814213562373)) ;
#118211 = CARTESIAN_POINT('Origin',(7.9,3.15,-13.9814213562373)) ;
#118212 = CARTESIAN_POINT('Origin',(1.4,3.25,-16.4985786437627)) ;
#118213 = CARTESIAN_POINT('',(1.5,3.25,-16.4985786437627)) ;
#118214 = CARTESIAN_POINT('',(7.9,3.25,-13.9814213562373)) ;
#118215 = CARTESIAN_POINT('Origin',(1.4,2.52928932188134,-16.0192893218813)) ;
#118216 = CARTESIAN_POINT('',(1.5,2.52928932188134,-16.0192893218813)) ;
#118217 = CARTESIAN_POINT('',(1.5,2.52928932188135,-16.0192893218813)) ;
#118218 = CARTESIAN_POINT('',(7.9,2.52928932188134,-16.0192893218813)) ;
#118219 = CARTESIAN_POINT('',(1.4,2.52928932188134,-16.0192893218813)) ;
#118220 = CARTESIAN_POINT('',(7.9,3.07928932188134,-16.5692893218813)) ;
#118221 = CARTESIAN_POINT('Origin',(1.4,2.6,-15.9485786437627)) ;
#118222 = CARTESIAN_POINT('',(1.5,2.5,-15.9485786437627)) ;
#118223 = CARTESIAN_POINT('Origin',(1.5,2.6,-15.9485786437627)) ;
#118224 = CARTESIAN_POINT('',(7.9,2.5,-15.9485786437627)) ;
#118225 = CARTESIAN_POINT('',(1.4,2.5,-15.9485786437627)) ;
#118226 = CARTESIAN_POINT('Origin',(7.9,2.6,-15.9485786437627)) ;
#118227 = CARTESIAN_POINT('Origin',(1.4,2.5,-15.84)) ;
#118228 = CARTESIAN_POINT('',(1.5,2.5,-15.84)) ;
#118229 = CARTESIAN_POINT('',(1.5,2.5,-15.84)) ;
#118230 = CARTESIAN_POINT('',(7.9,2.5,-15.84)) ;
#118231 = CARTESIAN_POINT('',(1.4,2.5,-15.84)) ;
#118232 = CARTESIAN_POINT('',(7.9,2.5,-15.9485786437627)) ;
#118233 = CARTESIAN_POINT('Origin',(1.4,2.4,-15.84)) ;
#118234 = CARTESIAN_POINT('',(1.5,2.4,-15.74)) ;
#118235 = CARTESIAN_POINT('Origin',(1.5,2.4,-15.84)) ;
#118236 = CARTESIAN_POINT('',(7.9,2.4,-15.74)) ;
#118237 = CARTESIAN_POINT('',(1.4,2.4,-15.74)) ;
#118238 = CARTESIAN_POINT('Origin',(7.9,2.4,-15.84)) ;
#118239 = CARTESIAN_POINT('Origin',(1.4,2.1,-15.74)) ;
#118240 = CARTESIAN_POINT('',(1.5,2.1,-15.74)) ;
#118241 = CARTESIAN_POINT('',(1.5,2.1,-15.74)) ;
#118242 = CARTESIAN_POINT('',(7.9,2.1,-15.74)) ;
#118243 = CARTESIAN_POINT('',(1.4,2.1,-15.74)) ;
#118244 = CARTESIAN_POINT('',(7.9,2.4,-15.74)) ;
#118245 = CARTESIAN_POINT('Origin',(1.4,2.1,-15.84)) ;
#118246 = CARTESIAN_POINT('',(1.5,2.,-15.84)) ;
#118247 = CARTESIAN_POINT('Origin',(1.5,2.1,-15.84)) ;
#118248 = CARTESIAN_POINT('',(7.9,2.,-15.84)) ;
#118249 = CARTESIAN_POINT('',(1.4,2.,-15.84)) ;
#118250 = CARTESIAN_POINT('Origin',(7.9,2.1,-15.84)) ;
#118251 = CARTESIAN_POINT('Origin',(1.4,2.,-15.84)) ;
#118252 = CARTESIAN_POINT('',(1.5,2.,-16.79)) ;
#118253 = CARTESIAN_POINT('',(1.5,2.,-16.79)) ;
#118254 = CARTESIAN_POINT('',(7.9,2.,-16.79)) ;
#118255 = CARTESIAN_POINT('',(1.4,2.,-16.79)) ;
#118256 = CARTESIAN_POINT('',(7.9,2.,-15.84)) ;
#118257 = CARTESIAN_POINT('Origin',(1.4,1.9,-16.79)) ;
#118258 = CARTESIAN_POINT('',(1.5,1.9,-16.89)) ;
#118259 = CARTESIAN_POINT('Origin',(1.5,1.9,-16.79)) ;
#118260 = CARTESIAN_POINT('',(7.9,1.9,-16.89)) ;
#118261 = CARTESIAN_POINT('',(1.4,1.9,-16.89)) ;
#118262 = CARTESIAN_POINT('Origin',(7.9,1.9,-16.79)) ;
#118263 = CARTESIAN_POINT('Origin',(1.4,1.9,-16.89)) ;
#118264 = CARTESIAN_POINT('',(1.5,-2.15,-16.89)) ;
#118265 = CARTESIAN_POINT('',(1.5,-2.15,-16.89)) ;
#118266 = CARTESIAN_POINT('',(7.9,-2.15,-16.89)) ;
#118267 = CARTESIAN_POINT('',(1.4,-2.15,-16.89)) ;
#118268 = CARTESIAN_POINT('',(7.9,1.9,-16.89)) ;
#118269 = CARTESIAN_POINT('Origin',(1.4,-2.15,-16.79)) ;
#118270 = CARTESIAN_POINT('',(1.5,-2.25,-16.79)) ;
#118271 = CARTESIAN_POINT('Origin',(1.5,-2.15,-16.79)) ;
#118272 = CARTESIAN_POINT('',(7.9,-2.25,-16.79)) ;
#118273 = CARTESIAN_POINT('',(1.4,-2.25,-16.79)) ;
#118274 = CARTESIAN_POINT('Origin',(7.9,-2.15,-16.79)) ;
#118275 = CARTESIAN_POINT('Origin',(1.4,-2.25,-16.1431195934094)) ;
#118276 = CARTESIAN_POINT('',(1.5,-2.25,-16.1431195934094)) ;
#118277 = CARTESIAN_POINT('',(1.5,-2.25,-16.1431195934094)) ;
#118278 = CARTESIAN_POINT('',(7.9,-2.25,-16.1431195934094)) ;
#118279 = CARTESIAN_POINT('',(1.4,-2.25,-16.1431195934094)) ;
#118280 = CARTESIAN_POINT('',(7.9,-2.25,-16.79)) ;
#118281 = CARTESIAN_POINT('Origin',(1.4,-2.15,-16.1431195934094)) ;
#118282 = CARTESIAN_POINT('',(1.5,-2.23576512455516,-16.0916964137135)) ;
#118283 = CARTESIAN_POINT('Origin',(1.5,-2.15,-16.1431195934094)) ;
#118284 = CARTESIAN_POINT('',(7.9,-2.23576512455516,-16.0916964137135)) ;
#118285 = CARTESIAN_POINT('',(1.4,-2.23576512455516,-16.0916964137135)) ;
#118286 = CARTESIAN_POINT('Origin',(7.9,-2.15,-16.1431195934094)) ;
#118287 = CARTESIAN_POINT('Origin',(1.4,-3.65625,-15.24)) ;
#118288 = CARTESIAN_POINT('',(1.5,-2.23576512455516,-14.3883035862865)) ;
#118289 = CARTESIAN_POINT('Origin',(1.5,-3.65625,-15.24)) ;
#118290 = CARTESIAN_POINT('',(7.9,-2.23576512455516,-14.3883035862865)) ;
#118291 = CARTESIAN_POINT('',(1.4,-2.23576512455516,-14.3883035862865)) ;
#118292 = CARTESIAN_POINT('Origin',(7.9,-3.65625,-15.24)) ;
#118293 = CARTESIAN_POINT('Origin',(1.4,-2.15,-14.3368804065906)) ;
#118294 = CARTESIAN_POINT('',(1.5,-2.25,-14.3368804065906)) ;
#118295 = CARTESIAN_POINT('Origin',(1.5,-2.15,-14.3368804065906)) ;
#118296 = CARTESIAN_POINT('',(7.9,-2.25,-14.3368804065906)) ;
#118297 = CARTESIAN_POINT('',(1.4,-2.25,-14.3368804065906)) ;
#118298 = CARTESIAN_POINT('Origin',(7.9,-2.15,-14.3368804065906)) ;
#118299 = CARTESIAN_POINT('Origin',(1.4,-2.25,-13.69)) ;
#118300 = CARTESIAN_POINT('',(1.5,-2.25,-13.69)) ;
#118301 = CARTESIAN_POINT('',(1.5,-2.25,-13.69)) ;
#118302 = CARTESIAN_POINT('',(7.9,-2.25,-13.69)) ;
#118303 = CARTESIAN_POINT('',(1.4,-2.25,-13.69)) ;
#118304 = CARTESIAN_POINT('',(7.9,-2.25,-14.3368804065906)) ;
#118305 = CARTESIAN_POINT('Origin',(1.4,-2.15,-13.69)) ;
#118306 = CARTESIAN_POINT('',(1.5,-2.15,-13.59)) ;
#118307 = CARTESIAN_POINT('Origin',(1.5,-2.15,-13.69)) ;
#118308 = CARTESIAN_POINT('',(7.9,-2.15,-13.59)) ;
#118309 = CARTESIAN_POINT('',(1.4,-2.15,-13.59)) ;
#118310 = CARTESIAN_POINT('Origin',(7.9,-2.15,-13.69)) ;
#118311 = CARTESIAN_POINT('Origin',(1.4,1.9,-13.59)) ;
#118312 = CARTESIAN_POINT('',(1.5,1.9,-13.59)) ;
#118313 = CARTESIAN_POINT('',(1.5,1.9,-13.59)) ;
#118314 = CARTESIAN_POINT('',(7.9,1.9,-13.59)) ;
#118315 = CARTESIAN_POINT('',(1.4,1.9,-13.59)) ;
#118316 = CARTESIAN_POINT('',(7.9,-2.15,-13.59)) ;
#118317 = CARTESIAN_POINT('Origin',(1.4,1.9,-13.69)) ;
#118318 = CARTESIAN_POINT('',(1.5,2.,-13.69)) ;
#118319 = CARTESIAN_POINT('Origin',(1.5,1.9,-13.69)) ;
#118320 = CARTESIAN_POINT('',(7.9,2.,-13.69)) ;
#118321 = CARTESIAN_POINT('',(1.4,2.,-13.69)) ;
#118322 = CARTESIAN_POINT('Origin',(7.9,1.9,-13.69)) ;
#118323 = CARTESIAN_POINT('Origin',(1.4,2.,-13.69)) ;
#118324 = CARTESIAN_POINT('',(1.5,2.,-14.64)) ;
#118325 = CARTESIAN_POINT('',(7.9,2.,-13.69)) ;
#118326 = CARTESIAN_POINT('Origin',(1.4,2.1,-14.64)) ;
#118327 = CARTESIAN_POINT('',(1.4,2.6,-14.64)) ;
#118328 = CARTESIAN_POINT('',(1.4,2.4,-14.84)) ;
#118329 = CARTESIAN_POINT('Origin',(1.4,2.4,-14.64)) ;
#118330 = CARTESIAN_POINT('',(1.4,2.1,-14.84)) ;
#118331 = CARTESIAN_POINT('',(1.4,2.1,-14.84)) ;
#118332 = CARTESIAN_POINT('',(1.4,1.9,-14.64)) ;
#118333 = CARTESIAN_POINT('Origin',(1.4,2.1,-14.64)) ;
#118334 = CARTESIAN_POINT('',(1.4,1.9,-13.69)) ;
#118335 = CARTESIAN_POINT('',(1.4,1.9,-13.69)) ;
#118336 = CARTESIAN_POINT('',(1.4,-2.15,-13.69)) ;
#118337 = CARTESIAN_POINT('',(1.4,-2.15,-13.69)) ;
#118338 = CARTESIAN_POINT('',(1.4,-2.15,-14.3368804065906)) ;
#118339 = CARTESIAN_POINT('',(1.4,-2.15,-14.3368804065906)) ;
#118340 = CARTESIAN_POINT('',(1.4,-2.15,-16.1431195934094)) ;
#118341 = CARTESIAN_POINT('Origin',(1.4,-3.65625,-15.24)) ;
#118342 = CARTESIAN_POINT('',(1.4,-2.15,-16.79)) ;
#118343 = CARTESIAN_POINT('',(1.4,-2.15,-16.79)) ;
#118344 = CARTESIAN_POINT('',(1.4,1.9,-16.79)) ;
#118345 = CARTESIAN_POINT('',(1.4,1.9,-16.79)) ;
#118346 = CARTESIAN_POINT('',(1.4,1.9,-15.84)) ;
#118347 = CARTESIAN_POINT('',(1.4,1.9,-15.84)) ;
#118348 = CARTESIAN_POINT('',(1.4,2.1,-15.64)) ;
#118349 = CARTESIAN_POINT('Origin',(1.4,2.1,-15.84)) ;
#118350 = CARTESIAN_POINT('',(1.4,2.4,-15.64)) ;
#118351 = CARTESIAN_POINT('',(1.4,2.4,-15.64)) ;
#118352 = CARTESIAN_POINT('',(1.4,2.6,-15.84)) ;
#118353 = CARTESIAN_POINT('Origin',(1.4,2.4,-15.84)) ;
#118354 = CARTESIAN_POINT('',(1.4,2.6,-15.9485786437627)) ;
#118355 = CARTESIAN_POINT('',(1.4,2.6,-15.9485786437627)) ;
#118356 = CARTESIAN_POINT('',(1.4,3.15,-16.4985786437627)) ;
#118357 = CARTESIAN_POINT('',(1.4,3.15,-16.4985786437627)) ;
#118358 = CARTESIAN_POINT('',(1.4,3.15,-13.9814213562373)) ;
#118359 = CARTESIAN_POINT('',(1.4,2.6,-14.5314213562373)) ;
#118360 = CARTESIAN_POINT('',(1.4,2.6,-14.5314213562373)) ;
#118361 = CARTESIAN_POINT('',(1.4,2.6,-14.64)) ;
#118362 = CARTESIAN_POINT('Origin',(1.4,2.1,-10.83)) ;
#118363 = CARTESIAN_POINT('',(1.5,2.,-10.83)) ;
#118364 = CARTESIAN_POINT('',(7.9,2.,-10.83)) ;
#118365 = CARTESIAN_POINT('',(1.4,2.,-10.83)) ;
#118366 = CARTESIAN_POINT('',(1.5,2.1,-10.93)) ;
#118367 = CARTESIAN_POINT('Origin',(1.5,2.1,-10.83)) ;
#118368 = CARTESIAN_POINT('',(7.9,2.1,-10.93)) ;
#118369 = CARTESIAN_POINT('',(1.4,2.1,-10.93)) ;
#118370 = CARTESIAN_POINT('Origin',(7.9,2.1,-10.83)) ;
#118371 = CARTESIAN_POINT('Origin',(1.4,2.4,-10.93)) ;
#118372 = CARTESIAN_POINT('',(1.5,2.4,-10.93)) ;
#118373 = CARTESIAN_POINT('',(1.5,2.4,-10.93)) ;
#118374 = CARTESIAN_POINT('',(7.9,2.4,-10.93)) ;
#118375 = CARTESIAN_POINT('',(1.4,2.4,-10.93)) ;
#118376 = CARTESIAN_POINT('',(7.9,2.1,-10.93)) ;
#118377 = CARTESIAN_POINT('Origin',(1.4,2.4,-10.83)) ;
#118378 = CARTESIAN_POINT('',(1.5,2.5,-10.83)) ;
#118379 = CARTESIAN_POINT('Origin',(1.5,2.4,-10.83)) ;
#118380 = CARTESIAN_POINT('',(7.9,2.5,-10.83)) ;
#118381 = CARTESIAN_POINT('',(1.4,2.5,-10.83)) ;
#118382 = CARTESIAN_POINT('Origin',(7.9,2.4,-10.83)) ;
#118383 = CARTESIAN_POINT('Origin',(1.4,2.5,-10.7214213562373)) ;
#118384 = CARTESIAN_POINT('',(1.5,2.5,-10.7214213562373)) ;
#118385 = CARTESIAN_POINT('',(1.5,2.5,-10.7214213562373)) ;
#118386 = CARTESIAN_POINT('',(7.9,2.5,-10.7214213562373)) ;
#118387 = CARTESIAN_POINT('',(1.4,2.5,-10.7214213562373)) ;
#118388 = CARTESIAN_POINT('',(7.9,2.5,-10.83)) ;
#118389 = CARTESIAN_POINT('Origin',(1.4,2.6,-10.7214213562373)) ;
#118390 = CARTESIAN_POINT('',(1.5,2.52928932188135,-10.6507106781187)) ;
#118391 = CARTESIAN_POINT('Origin',(1.5,2.6,-10.7214213562373)) ;
#118392 = CARTESIAN_POINT('',(7.9,2.52928932188135,-10.6507106781187)) ;
#118393 = CARTESIAN_POINT('',(1.4,2.52928932188135,-10.6507106781187)) ;
#118394 = CARTESIAN_POINT('Origin',(7.9,2.6,-10.7214213562373)) ;
#118395 = CARTESIAN_POINT('Origin',(1.4,3.07928932188135,-10.1007106781187)) ;
#118396 = CARTESIAN_POINT('',(1.5,3.07928932188135,-10.1007106781187)) ;
#118397 = CARTESIAN_POINT('',(7.9,3.07928932188135,-10.1007106781187)) ;
#118398 = CARTESIAN_POINT('',(1.4,3.07928932188135,-10.1007106781187)) ;
#118399 = CARTESIAN_POINT('',(7.9,2.52928932188135,-10.6507106781187)) ;
#118400 = CARTESIAN_POINT('Origin',(1.4,3.15,-10.1714213562373)) ;
#118401 = CARTESIAN_POINT('',(7.9,3.25,-10.1714213562373)) ;
#118402 = CARTESIAN_POINT('',(1.4,3.25,-10.1714213562373)) ;
#118403 = CARTESIAN_POINT('Origin',(7.9,3.15,-10.1714213562373)) ;
#118404 = CARTESIAN_POINT('Origin',(1.4,3.25,-12.6885786437627)) ;
#118405 = CARTESIAN_POINT('',(1.5,3.25,-12.6885786437627)) ;
#118406 = CARTESIAN_POINT('',(7.9,3.25,-10.1714213562373)) ;
#118407 = CARTESIAN_POINT('Origin',(1.4,2.52928932188134,-12.2092893218813)) ;
#118408 = CARTESIAN_POINT('',(1.5,2.52928932188134,-12.2092893218813)) ;
#118409 = CARTESIAN_POINT('',(1.5,2.52928932188134,-12.2092893218813)) ;
#118410 = CARTESIAN_POINT('',(7.9,2.52928932188134,-12.2092893218813)) ;
#118411 = CARTESIAN_POINT('',(1.4,2.52928932188134,-12.2092893218813)) ;
#118412 = CARTESIAN_POINT('',(7.9,3.07928932188135,-12.7592893218813)) ;
#118413 = CARTESIAN_POINT('Origin',(1.4,2.6,-12.1385786437627)) ;
#118414 = CARTESIAN_POINT('',(1.5,2.5,-12.1385786437627)) ;
#118415 = CARTESIAN_POINT('Origin',(1.5,2.6,-12.1385786437627)) ;
#118416 = CARTESIAN_POINT('',(7.9,2.5,-12.1385786437627)) ;
#118417 = CARTESIAN_POINT('',(1.4,2.5,-12.1385786437627)) ;
#118418 = CARTESIAN_POINT('Origin',(7.9,2.6,-12.1385786437627)) ;
#118419 = CARTESIAN_POINT('Origin',(1.4,2.5,-12.03)) ;
#118420 = CARTESIAN_POINT('',(1.5,2.5,-12.03)) ;
#118421 = CARTESIAN_POINT('',(1.5,2.5,-12.03)) ;
#118422 = CARTESIAN_POINT('',(7.9,2.5,-12.03)) ;
#118423 = CARTESIAN_POINT('',(1.4,2.5,-12.03)) ;
#118424 = CARTESIAN_POINT('',(7.9,2.5,-12.1385786437627)) ;
#118425 = CARTESIAN_POINT('Origin',(1.4,2.4,-12.03)) ;
#118426 = CARTESIAN_POINT('',(1.5,2.4,-11.93)) ;
#118427 = CARTESIAN_POINT('Origin',(1.5,2.4,-12.03)) ;
#118428 = CARTESIAN_POINT('',(7.9,2.4,-11.93)) ;
#118429 = CARTESIAN_POINT('',(1.4,2.4,-11.93)) ;
#118430 = CARTESIAN_POINT('Origin',(7.9,2.4,-12.03)) ;
#118431 = CARTESIAN_POINT('Origin',(1.4,2.1,-11.93)) ;
#118432 = CARTESIAN_POINT('',(1.5,2.1,-11.93)) ;
#118433 = CARTESIAN_POINT('',(1.5,2.1,-11.93)) ;
#118434 = CARTESIAN_POINT('',(7.9,2.1,-11.93)) ;
#118435 = CARTESIAN_POINT('',(1.4,2.1,-11.93)) ;
#118436 = CARTESIAN_POINT('',(7.9,2.4,-11.93)) ;
#118437 = CARTESIAN_POINT('Origin',(1.4,2.1,-12.03)) ;
#118438 = CARTESIAN_POINT('',(1.5,2.,-12.03)) ;
#118439 = CARTESIAN_POINT('Origin',(1.5,2.1,-12.03)) ;
#118440 = CARTESIAN_POINT('',(7.9,2.,-12.03)) ;
#118441 = CARTESIAN_POINT('',(1.4,2.,-12.03)) ;
#118442 = CARTESIAN_POINT('Origin',(7.9,2.1,-12.03)) ;
#118443 = CARTESIAN_POINT('Origin',(1.4,2.,-12.03)) ;
#118444 = CARTESIAN_POINT('',(1.5,2.,-12.98)) ;
#118445 = CARTESIAN_POINT('',(1.5,2.,-12.98)) ;
#118446 = CARTESIAN_POINT('',(7.9,2.,-12.98)) ;
#118447 = CARTESIAN_POINT('',(1.4,2.,-12.98)) ;
#118448 = CARTESIAN_POINT('',(7.9,2.,-12.03)) ;
#118449 = CARTESIAN_POINT('Origin',(1.4,1.9,-12.98)) ;
#118450 = CARTESIAN_POINT('',(1.5,1.9,-13.08)) ;
#118451 = CARTESIAN_POINT('Origin',(1.5,1.9,-12.98)) ;
#118452 = CARTESIAN_POINT('',(7.9,1.9,-13.08)) ;
#118453 = CARTESIAN_POINT('',(1.4,1.9,-13.08)) ;
#118454 = CARTESIAN_POINT('Origin',(7.9,1.9,-12.98)) ;
#118455 = CARTESIAN_POINT('Origin',(1.4,1.9,-13.08)) ;
#118456 = CARTESIAN_POINT('',(1.5,-2.15,-13.08)) ;
#118457 = CARTESIAN_POINT('',(1.5,-2.15,-13.08)) ;
#118458 = CARTESIAN_POINT('',(7.9,-2.15,-13.08)) ;
#118459 = CARTESIAN_POINT('',(1.4,-2.15,-13.08)) ;
#118460 = CARTESIAN_POINT('',(7.9,1.9,-13.08)) ;
#118461 = CARTESIAN_POINT('Origin',(1.4,-2.15,-12.98)) ;
#118462 = CARTESIAN_POINT('',(1.5,-2.25,-12.98)) ;
#118463 = CARTESIAN_POINT('Origin',(1.5,-2.15,-12.98)) ;
#118464 = CARTESIAN_POINT('',(7.9,-2.25,-12.98)) ;
#118465 = CARTESIAN_POINT('',(1.4,-2.25,-12.98)) ;
#118466 = CARTESIAN_POINT('Origin',(7.9,-2.15,-12.98)) ;
#118467 = CARTESIAN_POINT('Origin',(1.4,-2.25,-12.3331195934094)) ;
#118468 = CARTESIAN_POINT('',(1.5,-2.25,-12.3331195934094)) ;
#118469 = CARTESIAN_POINT('',(1.5,-2.25,-12.3331195934094)) ;
#118470 = CARTESIAN_POINT('',(7.9,-2.25,-12.3331195934094)) ;
#118471 = CARTESIAN_POINT('',(1.4,-2.25,-12.3331195934094)) ;
#118472 = CARTESIAN_POINT('',(7.9,-2.25,-12.98)) ;
#118473 = CARTESIAN_POINT('Origin',(1.4,-2.15,-12.3331195934094)) ;
#118474 = CARTESIAN_POINT('',(1.5,-2.23576512455516,-12.2816964137135)) ;
#118475 = CARTESIAN_POINT('Origin',(1.5,-2.15,-12.3331195934094)) ;
#118476 = CARTESIAN_POINT('',(7.9,-2.23576512455516,-12.2816964137135)) ;
#118477 = CARTESIAN_POINT('',(1.4,-2.23576512455516,-12.2816964137135)) ;
#118478 = CARTESIAN_POINT('Origin',(7.9,-2.15,-12.3331195934094)) ;
#118479 = CARTESIAN_POINT('Origin',(1.4,-3.65625,-11.43)) ;
#118480 = CARTESIAN_POINT('',(1.5,-2.23576512455516,-10.5783035862865)) ;
#118481 = CARTESIAN_POINT('Origin',(1.5,-3.65625,-11.43)) ;
#118482 = CARTESIAN_POINT('',(7.9,-2.23576512455516,-10.5783035862865)) ;
#118483 = CARTESIAN_POINT('',(1.4,-2.23576512455516,-10.5783035862865)) ;
#118484 = CARTESIAN_POINT('Origin',(7.9,-3.65625,-11.43)) ;
#118485 = CARTESIAN_POINT('Origin',(1.4,-2.15,-10.5268804065906)) ;
#118486 = CARTESIAN_POINT('',(1.5,-2.25,-10.5268804065906)) ;
#118487 = CARTESIAN_POINT('Origin',(1.5,-2.15,-10.5268804065906)) ;
#118488 = CARTESIAN_POINT('',(7.9,-2.25,-10.5268804065906)) ;
#118489 = CARTESIAN_POINT('',(1.4,-2.25,-10.5268804065906)) ;
#118490 = CARTESIAN_POINT('Origin',(7.9,-2.15,-10.5268804065906)) ;
#118491 = CARTESIAN_POINT('Origin',(1.4,-2.25,-9.88)) ;
#118492 = CARTESIAN_POINT('',(1.5,-2.25,-9.88)) ;
#118493 = CARTESIAN_POINT('',(1.5,-2.25,-9.88)) ;
#118494 = CARTESIAN_POINT('',(7.9,-2.25,-9.88)) ;
#118495 = CARTESIAN_POINT('',(1.4,-2.25,-9.88)) ;
#118496 = CARTESIAN_POINT('',(7.9,-2.25,-10.5268804065906)) ;
#118497 = CARTESIAN_POINT('Origin',(1.4,-2.15,-9.88)) ;
#118498 = CARTESIAN_POINT('',(1.5,-2.15,-9.78)) ;
#118499 = CARTESIAN_POINT('Origin',(1.5,-2.15,-9.88)) ;
#118500 = CARTESIAN_POINT('',(7.9,-2.15,-9.78)) ;
#118501 = CARTESIAN_POINT('',(1.4,-2.15,-9.78)) ;
#118502 = CARTESIAN_POINT('Origin',(7.9,-2.15,-9.88)) ;
#118503 = CARTESIAN_POINT('Origin',(1.4,1.9,-9.78)) ;
#118504 = CARTESIAN_POINT('',(1.5,1.9,-9.78)) ;
#118505 = CARTESIAN_POINT('',(1.5,1.9,-9.78)) ;
#118506 = CARTESIAN_POINT('',(7.9,1.9,-9.78)) ;
#118507 = CARTESIAN_POINT('',(1.4,1.9,-9.78)) ;
#118508 = CARTESIAN_POINT('',(7.9,-2.15,-9.78)) ;
#118509 = CARTESIAN_POINT('Origin',(1.4,1.9,-9.88)) ;
#118510 = CARTESIAN_POINT('',(1.5,2.,-9.88)) ;
#118511 = CARTESIAN_POINT('Origin',(1.5,1.9,-9.88)) ;
#118512 = CARTESIAN_POINT('',(7.9,2.,-9.88)) ;
#118513 = CARTESIAN_POINT('',(1.4,2.,-9.88)) ;
#118514 = CARTESIAN_POINT('Origin',(7.9,1.9,-9.88)) ;
#118515 = CARTESIAN_POINT('Origin',(1.4,2.,-9.88)) ;
#118516 = CARTESIAN_POINT('',(1.5,2.,-10.83)) ;
#118517 = CARTESIAN_POINT('',(7.9,2.,-9.88)) ;
#118518 = CARTESIAN_POINT('Origin',(1.4,2.1,-10.83)) ;
#118519 = CARTESIAN_POINT('',(1.4,2.6,-10.83)) ;
#118520 = CARTESIAN_POINT('',(1.4,2.4,-11.03)) ;
#118521 = CARTESIAN_POINT('Origin',(1.4,2.4,-10.83)) ;
#118522 = CARTESIAN_POINT('',(1.4,2.1,-11.03)) ;
#118523 = CARTESIAN_POINT('',(1.4,2.1,-11.03)) ;
#118524 = CARTESIAN_POINT('',(1.4,1.9,-10.83)) ;
#118525 = CARTESIAN_POINT('Origin',(1.4,2.1,-10.83)) ;
#118526 = CARTESIAN_POINT('',(1.4,1.9,-9.88)) ;
#118527 = CARTESIAN_POINT('',(1.4,1.9,-9.88)) ;
#118528 = CARTESIAN_POINT('',(1.4,-2.15,-9.88)) ;
#118529 = CARTESIAN_POINT('',(1.4,-2.15,-9.88)) ;
#118530 = CARTESIAN_POINT('',(1.4,-2.15,-10.5268804065906)) ;
#118531 = CARTESIAN_POINT('',(1.4,-2.15,-10.5268804065906)) ;
#118532 = CARTESIAN_POINT('',(1.4,-2.15,-12.3331195934094)) ;
#118533 = CARTESIAN_POINT('Origin',(1.4,-3.65625,-11.43)) ;
#118534 = CARTESIAN_POINT('',(1.4,-2.15,-12.98)) ;
#118535 = CARTESIAN_POINT('',(1.4,-2.15,-12.98)) ;
#118536 = CARTESIAN_POINT('',(1.4,1.9,-12.98)) ;
#118537 = CARTESIAN_POINT('',(1.4,1.9,-12.98)) ;
#118538 = CARTESIAN_POINT('',(1.4,1.9,-12.03)) ;
#118539 = CARTESIAN_POINT('',(1.4,1.9,-12.03)) ;
#118540 = CARTESIAN_POINT('',(1.4,2.1,-11.83)) ;
#118541 = CARTESIAN_POINT('Origin',(1.4,2.1,-12.03)) ;
#118542 = CARTESIAN_POINT('',(1.4,2.4,-11.83)) ;
#118543 = CARTESIAN_POINT('',(1.4,2.4,-11.83)) ;
#118544 = CARTESIAN_POINT('',(1.4,2.6,-12.03)) ;
#118545 = CARTESIAN_POINT('Origin',(1.4,2.4,-12.03)) ;
#118546 = CARTESIAN_POINT('',(1.4,2.6,-12.1385786437627)) ;
#118547 = CARTESIAN_POINT('',(1.4,2.6,-12.1385786437627)) ;
#118548 = CARTESIAN_POINT('',(1.4,3.15,-12.6885786437627)) ;
#118549 = CARTESIAN_POINT('',(1.4,3.15,-12.6885786437627)) ;
#118550 = CARTESIAN_POINT('',(1.4,3.15,-10.1714213562373)) ;
#118551 = CARTESIAN_POINT('',(1.4,2.6,-10.7214213562373)) ;
#118552 = CARTESIAN_POINT('',(1.4,2.6,-10.7214213562373)) ;
#118553 = CARTESIAN_POINT('',(1.4,2.6,-10.83)) ;
#118554 = CARTESIAN_POINT('Origin',(1.4,2.1,-7.02)) ;
#118555 = CARTESIAN_POINT('',(1.5,2.,-7.02)) ;
#118556 = CARTESIAN_POINT('',(7.9,2.,-7.02)) ;
#118557 = CARTESIAN_POINT('',(1.4,2.,-7.02)) ;
#118558 = CARTESIAN_POINT('',(1.5,2.1,-7.12)) ;
#118559 = CARTESIAN_POINT('Origin',(1.5,2.1,-7.02)) ;
#118560 = CARTESIAN_POINT('',(7.9,2.1,-7.12)) ;
#118561 = CARTESIAN_POINT('',(1.4,2.1,-7.12)) ;
#118562 = CARTESIAN_POINT('Origin',(7.9,2.1,-7.02)) ;
#118563 = CARTESIAN_POINT('Origin',(1.4,2.4,-7.12)) ;
#118564 = CARTESIAN_POINT('',(1.5,2.4,-7.12)) ;
#118565 = CARTESIAN_POINT('',(1.5,2.4,-7.12)) ;
#118566 = CARTESIAN_POINT('',(7.9,2.4,-7.12)) ;
#118567 = CARTESIAN_POINT('',(1.4,2.4,-7.12)) ;
#118568 = CARTESIAN_POINT('',(7.9,2.1,-7.12)) ;
#118569 = CARTESIAN_POINT('Origin',(1.4,2.4,-7.02)) ;
#118570 = CARTESIAN_POINT('',(1.5,2.5,-7.02)) ;
#118571 = CARTESIAN_POINT('Origin',(1.5,2.4,-7.02)) ;
#118572 = CARTESIAN_POINT('',(7.9,2.5,-7.02)) ;
#118573 = CARTESIAN_POINT('',(1.4,2.5,-7.02)) ;
#118574 = CARTESIAN_POINT('Origin',(7.9,2.4,-7.02)) ;
#118575 = CARTESIAN_POINT('Origin',(1.4,2.5,-6.91142135623731)) ;
#118576 = CARTESIAN_POINT('',(1.5,2.5,-6.91142135623731)) ;
#118577 = CARTESIAN_POINT('',(1.5,2.5,-6.91142135623731)) ;
#118578 = CARTESIAN_POINT('',(7.9,2.5,-6.91142135623731)) ;
#118579 = CARTESIAN_POINT('',(1.4,2.5,-6.91142135623731)) ;
#118580 = CARTESIAN_POINT('',(7.9,2.5,-7.02)) ;
#118581 = CARTESIAN_POINT('Origin',(1.4,2.6,-6.91142135623731)) ;
#118582 = CARTESIAN_POINT('',(1.5,2.52928932188135,-6.84071067811866)) ;
#118583 = CARTESIAN_POINT('Origin',(1.5,2.6,-6.91142135623731)) ;
#118584 = CARTESIAN_POINT('',(7.9,2.52928932188135,-6.84071067811866)) ;
#118585 = CARTESIAN_POINT('',(1.4,2.52928932188135,-6.84071067811866)) ;
#118586 = CARTESIAN_POINT('Origin',(7.9,2.6,-6.91142135623731)) ;
#118587 = CARTESIAN_POINT('Origin',(1.4,3.07928932188135,-6.29071067811866)) ;
#118588 = CARTESIAN_POINT('',(1.5,3.07928932188135,-6.29071067811866)) ;
#118589 = CARTESIAN_POINT('',(7.9,3.07928932188135,-6.29071067811866)) ;
#118590 = CARTESIAN_POINT('',(1.4,3.07928932188135,-6.29071067811866)) ;
#118591 = CARTESIAN_POINT('',(7.9,2.52928932188135,-6.84071067811866)) ;
#118592 = CARTESIAN_POINT('Origin',(1.4,3.15,-6.36142135623731)) ;
#118593 = CARTESIAN_POINT('',(7.9,3.25,-6.36142135623731)) ;
#118594 = CARTESIAN_POINT('',(1.4,3.25,-6.36142135623731)) ;
#118595 = CARTESIAN_POINT('Origin',(7.9,3.15,-6.36142135623731)) ;
#118596 = CARTESIAN_POINT('Origin',(1.4,3.25,-8.87857864376269)) ;
#118597 = CARTESIAN_POINT('',(1.5,3.25,-8.87857864376269)) ;
#118598 = CARTESIAN_POINT('',(7.9,3.25,-6.36142135623731)) ;
#118599 = CARTESIAN_POINT('Origin',(1.4,2.52928932188134,-8.39928932188135)) ;
#118600 = CARTESIAN_POINT('',(1.5,2.52928932188134,-8.39928932188135)) ;
#118601 = CARTESIAN_POINT('',(1.5,2.52928932188134,-8.39928932188135)) ;
#118602 = CARTESIAN_POINT('',(7.9,2.52928932188134,-8.39928932188135)) ;
#118603 = CARTESIAN_POINT('',(1.4,2.52928932188134,-8.39928932188135)) ;
#118604 = CARTESIAN_POINT('',(7.9,3.07928932188135,-8.94928932188134)) ;
#118605 = CARTESIAN_POINT('Origin',(1.4,2.6,-8.32857864376269)) ;
#118606 = CARTESIAN_POINT('',(1.5,2.5,-8.32857864376269)) ;
#118607 = CARTESIAN_POINT('Origin',(1.5,2.6,-8.32857864376269)) ;
#118608 = CARTESIAN_POINT('',(7.9,2.5,-8.32857864376269)) ;
#118609 = CARTESIAN_POINT('',(1.4,2.5,-8.32857864376269)) ;
#118610 = CARTESIAN_POINT('Origin',(7.9,2.6,-8.32857864376269)) ;
#118611 = CARTESIAN_POINT('Origin',(1.4,2.5,-8.22)) ;
#118612 = CARTESIAN_POINT('',(1.5,2.5,-8.22)) ;
#118613 = CARTESIAN_POINT('',(1.5,2.5,-8.22)) ;
#118614 = CARTESIAN_POINT('',(7.9,2.5,-8.22)) ;
#118615 = CARTESIAN_POINT('',(1.4,2.5,-8.22)) ;
#118616 = CARTESIAN_POINT('',(7.9,2.5,-8.32857864376269)) ;
#118617 = CARTESIAN_POINT('Origin',(1.4,2.4,-8.22)) ;
#118618 = CARTESIAN_POINT('',(1.5,2.4,-8.12)) ;
#118619 = CARTESIAN_POINT('Origin',(1.5,2.4,-8.22)) ;
#118620 = CARTESIAN_POINT('',(7.9,2.4,-8.12)) ;
#118621 = CARTESIAN_POINT('',(1.4,2.4,-8.12)) ;
#118622 = CARTESIAN_POINT('Origin',(7.9,2.4,-8.22)) ;
#118623 = CARTESIAN_POINT('Origin',(1.4,2.1,-8.12)) ;
#118624 = CARTESIAN_POINT('',(1.5,2.1,-8.12)) ;
#118625 = CARTESIAN_POINT('',(1.5,2.1,-8.12)) ;
#118626 = CARTESIAN_POINT('',(7.9,2.1,-8.12)) ;
#118627 = CARTESIAN_POINT('',(1.4,2.1,-8.12)) ;
#118628 = CARTESIAN_POINT('',(7.9,2.4,-8.12)) ;
#118629 = CARTESIAN_POINT('Origin',(1.4,2.1,-8.22)) ;
#118630 = CARTESIAN_POINT('',(1.5,2.,-8.22)) ;
#118631 = CARTESIAN_POINT('Origin',(1.5,2.1,-8.22)) ;
#118632 = CARTESIAN_POINT('',(7.9,2.,-8.22)) ;
#118633 = CARTESIAN_POINT('',(1.4,2.,-8.22)) ;
#118634 = CARTESIAN_POINT('Origin',(7.9,2.1,-8.22)) ;
#118635 = CARTESIAN_POINT('Origin',(1.4,2.,-8.22)) ;
#118636 = CARTESIAN_POINT('',(1.5,2.,-9.17)) ;
#118637 = CARTESIAN_POINT('',(1.5,2.,-9.17)) ;
#118638 = CARTESIAN_POINT('',(7.9,2.,-9.17)) ;
#118639 = CARTESIAN_POINT('',(1.4,2.,-9.17)) ;
#118640 = CARTESIAN_POINT('',(7.9,2.,-8.22)) ;
#118641 = CARTESIAN_POINT('Origin',(1.4,1.9,-9.17)) ;
#118642 = CARTESIAN_POINT('',(1.5,1.9,-9.27)) ;
#118643 = CARTESIAN_POINT('Origin',(1.5,1.9,-9.17)) ;
#118644 = CARTESIAN_POINT('',(7.9,1.9,-9.27)) ;
#118645 = CARTESIAN_POINT('',(1.4,1.9,-9.27)) ;
#118646 = CARTESIAN_POINT('Origin',(7.9,1.9,-9.17)) ;
#118647 = CARTESIAN_POINT('Origin',(1.4,1.9,-9.27)) ;
#118648 = CARTESIAN_POINT('',(1.5,-2.15,-9.27)) ;
#118649 = CARTESIAN_POINT('',(1.5,-2.15,-9.27)) ;
#118650 = CARTESIAN_POINT('',(7.9,-2.15,-9.27)) ;
#118651 = CARTESIAN_POINT('',(1.4,-2.15,-9.27)) ;
#118652 = CARTESIAN_POINT('',(7.9,1.9,-9.27)) ;
#118653 = CARTESIAN_POINT('Origin',(1.4,-2.15,-9.17)) ;
#118654 = CARTESIAN_POINT('',(1.5,-2.25,-9.17)) ;
#118655 = CARTESIAN_POINT('Origin',(1.5,-2.15,-9.17)) ;
#118656 = CARTESIAN_POINT('',(7.9,-2.25,-9.17)) ;
#118657 = CARTESIAN_POINT('',(1.4,-2.25,-9.17)) ;
#118658 = CARTESIAN_POINT('Origin',(7.9,-2.15,-9.17)) ;
#118659 = CARTESIAN_POINT('Origin',(1.4,-2.25,-8.52311959340942)) ;
#118660 = CARTESIAN_POINT('',(1.5,-2.25,-8.52311959340942)) ;
#118661 = CARTESIAN_POINT('',(1.5,-2.25,-8.52311959340942)) ;
#118662 = CARTESIAN_POINT('',(7.9,-2.25,-8.52311959340942)) ;
#118663 = CARTESIAN_POINT('',(1.4,-2.25,-8.52311959340942)) ;
#118664 = CARTESIAN_POINT('',(7.9,-2.25,-9.17)) ;
#118665 = CARTESIAN_POINT('Origin',(1.4,-2.15,-8.52311959340942)) ;
#118666 = CARTESIAN_POINT('',(1.5,-2.23576512455516,-8.47169641371351)) ;
#118667 = CARTESIAN_POINT('Origin',(1.5,-2.15,-8.52311959340942)) ;
#118668 = CARTESIAN_POINT('',(7.9,-2.23576512455516,-8.47169641371351)) ;
#118669 = CARTESIAN_POINT('',(1.4,-2.23576512455516,-8.47169641371351)) ;
#118670 = CARTESIAN_POINT('Origin',(7.9,-2.15,-8.52311959340942)) ;
#118671 = CARTESIAN_POINT('Origin',(1.4,-3.65625,-7.62)) ;
#118672 = CARTESIAN_POINT('',(1.5,-2.23576512455516,-6.76830358628649)) ;
#118673 = CARTESIAN_POINT('Origin',(1.5,-3.65625,-7.62)) ;
#118674 = CARTESIAN_POINT('',(7.9,-2.23576512455516,-6.76830358628649)) ;
#118675 = CARTESIAN_POINT('',(1.4,-2.23576512455516,-6.76830358628649)) ;
#118676 = CARTESIAN_POINT('Origin',(7.9,-3.65625,-7.62)) ;
#118677 = CARTESIAN_POINT('Origin',(1.4,-2.15,-6.71688040659058)) ;
#118678 = CARTESIAN_POINT('',(1.5,-2.25,-6.71688040659058)) ;
#118679 = CARTESIAN_POINT('Origin',(1.5,-2.15,-6.71688040659058)) ;
#118680 = CARTESIAN_POINT('',(7.9,-2.25,-6.71688040659058)) ;
#118681 = CARTESIAN_POINT('',(1.4,-2.25,-6.71688040659058)) ;
#118682 = CARTESIAN_POINT('Origin',(7.9,-2.15,-6.71688040659058)) ;
#118683 = CARTESIAN_POINT('Origin',(1.4,-2.25,-6.07)) ;
#118684 = CARTESIAN_POINT('',(1.5,-2.25,-6.07)) ;
#118685 = CARTESIAN_POINT('',(1.5,-2.25,-6.07)) ;
#118686 = CARTESIAN_POINT('',(7.9,-2.25,-6.07)) ;
#118687 = CARTESIAN_POINT('',(1.4,-2.25,-6.07)) ;
#118688 = CARTESIAN_POINT('',(7.9,-2.25,-6.71688040659058)) ;
#118689 = CARTESIAN_POINT('Origin',(1.4,-2.15,-6.07)) ;
#118690 = CARTESIAN_POINT('',(1.5,-2.15,-5.97)) ;
#118691 = CARTESIAN_POINT('Origin',(1.5,-2.15,-6.07)) ;
#118692 = CARTESIAN_POINT('',(7.9,-2.15,-5.97)) ;
#118693 = CARTESIAN_POINT('',(1.4,-2.15,-5.97)) ;
#118694 = CARTESIAN_POINT('Origin',(7.9,-2.15,-6.07)) ;
#118695 = CARTESIAN_POINT('Origin',(1.4,1.9,-5.97)) ;
#118696 = CARTESIAN_POINT('',(1.5,1.9,-5.97)) ;
#118697 = CARTESIAN_POINT('',(1.5,1.9,-5.97)) ;
#118698 = CARTESIAN_POINT('',(7.9,1.9,-5.97)) ;
#118699 = CARTESIAN_POINT('',(1.4,1.9,-5.97)) ;
#118700 = CARTESIAN_POINT('',(7.9,-2.15,-5.97)) ;
#118701 = CARTESIAN_POINT('Origin',(1.4,1.9,-6.07)) ;
#118702 = CARTESIAN_POINT('',(1.5,2.,-6.07)) ;
#118703 = CARTESIAN_POINT('Origin',(1.5,1.9,-6.07)) ;
#118704 = CARTESIAN_POINT('',(7.9,2.,-6.07)) ;
#118705 = CARTESIAN_POINT('',(1.4,2.,-6.07)) ;
#118706 = CARTESIAN_POINT('Origin',(7.9,1.9,-6.07)) ;
#118707 = CARTESIAN_POINT('Origin',(1.4,2.,-6.07)) ;
#118708 = CARTESIAN_POINT('',(1.5,2.,-7.02)) ;
#118709 = CARTESIAN_POINT('',(7.9,2.,-6.07)) ;
#118710 = CARTESIAN_POINT('Origin',(1.4,2.1,-7.02)) ;
#118711 = CARTESIAN_POINT('',(1.4,2.6,-7.02)) ;
#118712 = CARTESIAN_POINT('',(1.4,2.4,-7.22)) ;
#118713 = CARTESIAN_POINT('Origin',(1.4,2.4,-7.02)) ;
#118714 = CARTESIAN_POINT('',(1.4,2.1,-7.22)) ;
#118715 = CARTESIAN_POINT('',(1.4,2.1,-7.22)) ;
#118716 = CARTESIAN_POINT('',(1.4,1.9,-7.02)) ;
#118717 = CARTESIAN_POINT('Origin',(1.4,2.1,-7.02)) ;
#118718 = CARTESIAN_POINT('',(1.4,1.9,-6.07)) ;
#118719 = CARTESIAN_POINT('',(1.4,1.9,-6.07)) ;
#118720 = CARTESIAN_POINT('',(1.4,-2.15,-6.07)) ;
#118721 = CARTESIAN_POINT('',(1.4,-2.15,-6.07)) ;
#118722 = CARTESIAN_POINT('',(1.4,-2.15,-6.71688040659058)) ;
#118723 = CARTESIAN_POINT('',(1.4,-2.15,-6.71688040659058)) ;
#118724 = CARTESIAN_POINT('',(1.4,-2.15,-8.52311959340942)) ;
#118725 = CARTESIAN_POINT('Origin',(1.4,-3.65625,-7.62)) ;
#118726 = CARTESIAN_POINT('',(1.4,-2.15,-9.17)) ;
#118727 = CARTESIAN_POINT('',(1.4,-2.15,-9.17)) ;
#118728 = CARTESIAN_POINT('',(1.4,1.9,-9.17)) ;
#118729 = CARTESIAN_POINT('',(1.4,1.9,-9.17)) ;
#118730 = CARTESIAN_POINT('',(1.4,1.9,-8.22)) ;
#118731 = CARTESIAN_POINT('',(1.4,1.9,-8.22)) ;
#118732 = CARTESIAN_POINT('',(1.4,2.1,-8.02)) ;
#118733 = CARTESIAN_POINT('Origin',(1.4,2.1,-8.22)) ;
#118734 = CARTESIAN_POINT('',(1.4,2.4,-8.02)) ;
#118735 = CARTESIAN_POINT('',(1.4,2.4,-8.02)) ;
#118736 = CARTESIAN_POINT('',(1.4,2.6,-8.22)) ;
#118737 = CARTESIAN_POINT('Origin',(1.4,2.4,-8.22)) ;
#118738 = CARTESIAN_POINT('',(1.4,2.6,-8.32857864376269)) ;
#118739 = CARTESIAN_POINT('',(1.4,2.6,-8.32857864376269)) ;
#118740 = CARTESIAN_POINT('',(1.4,3.15,-8.87857864376269)) ;
#118741 = CARTESIAN_POINT('',(1.4,3.15,-8.87857864376269)) ;
#118742 = CARTESIAN_POINT('',(1.4,3.15,-6.36142135623731)) ;
#118743 = CARTESIAN_POINT('',(1.4,2.6,-6.91142135623731)) ;
#118744 = CARTESIAN_POINT('',(1.4,2.6,-6.91142135623731)) ;
#118745 = CARTESIAN_POINT('',(1.4,2.6,-7.02)) ;
#118746 = CARTESIAN_POINT('Origin',(1.4,2.1,-3.21)) ;
#118747 = CARTESIAN_POINT('',(1.5,2.,-3.21)) ;
#118748 = CARTESIAN_POINT('',(7.9,2.,-3.21)) ;
#118749 = CARTESIAN_POINT('',(1.4,2.,-3.21)) ;
#118750 = CARTESIAN_POINT('',(1.5,2.1,-3.31)) ;
#118751 = CARTESIAN_POINT('Origin',(1.5,2.1,-3.21)) ;
#118752 = CARTESIAN_POINT('',(7.9,2.1,-3.31)) ;
#118753 = CARTESIAN_POINT('',(1.4,2.1,-3.31)) ;
#118754 = CARTESIAN_POINT('Origin',(7.9,2.1,-3.21)) ;
#118755 = CARTESIAN_POINT('Origin',(1.4,2.4,-3.31)) ;
#118756 = CARTESIAN_POINT('',(1.5,2.4,-3.31)) ;
#118757 = CARTESIAN_POINT('',(1.5,2.4,-3.31)) ;
#118758 = CARTESIAN_POINT('',(7.9,2.4,-3.31)) ;
#118759 = CARTESIAN_POINT('',(1.4,2.4,-3.31)) ;
#118760 = CARTESIAN_POINT('',(7.9,2.1,-3.31)) ;
#118761 = CARTESIAN_POINT('Origin',(1.4,2.4,-3.21)) ;
#118762 = CARTESIAN_POINT('',(1.5,2.5,-3.21)) ;
#118763 = CARTESIAN_POINT('Origin',(1.5,2.4,-3.21)) ;
#118764 = CARTESIAN_POINT('',(7.9,2.5,-3.21)) ;
#118765 = CARTESIAN_POINT('',(1.4,2.5,-3.21)) ;
#118766 = CARTESIAN_POINT('Origin',(7.9,2.4,-3.21)) ;
#118767 = CARTESIAN_POINT('Origin',(1.4,2.5,-3.10142135623731)) ;
#118768 = CARTESIAN_POINT('',(1.5,2.5,-3.10142135623731)) ;
#118769 = CARTESIAN_POINT('',(1.5,2.5,-3.10142135623731)) ;
#118770 = CARTESIAN_POINT('',(7.9,2.5,-3.10142135623731)) ;
#118771 = CARTESIAN_POINT('',(1.4,2.5,-3.10142135623731)) ;
#118772 = CARTESIAN_POINT('',(7.9,2.5,-3.21)) ;
#118773 = CARTESIAN_POINT('Origin',(1.4,2.6,-3.10142135623731)) ;
#118774 = CARTESIAN_POINT('',(1.5,2.52928932188135,-3.03071067811866)) ;
#118775 = CARTESIAN_POINT('Origin',(1.5,2.6,-3.10142135623731)) ;
#118776 = CARTESIAN_POINT('',(7.9,2.52928932188135,-3.03071067811866)) ;
#118777 = CARTESIAN_POINT('',(1.4,2.52928932188135,-3.03071067811866)) ;
#118778 = CARTESIAN_POINT('Origin',(7.9,2.6,-3.10142135623731)) ;
#118779 = CARTESIAN_POINT('Origin',(1.4,3.07928932188135,-2.48071067811865)) ;
#118780 = CARTESIAN_POINT('',(1.5,3.07928932188135,-2.48071067811865)) ;
#118781 = CARTESIAN_POINT('',(7.9,3.07928932188135,-2.48071067811865)) ;
#118782 = CARTESIAN_POINT('',(1.4,3.07928932188135,-2.48071067811865)) ;
#118783 = CARTESIAN_POINT('',(7.9,2.52928932188135,-3.03071067811866)) ;
#118784 = CARTESIAN_POINT('Origin',(1.4,3.15,-2.55142135623731)) ;
#118785 = CARTESIAN_POINT('',(7.9,3.25,-2.55142135623731)) ;
#118786 = CARTESIAN_POINT('',(1.4,3.25,-2.55142135623731)) ;
#118787 = CARTESIAN_POINT('Origin',(7.9,3.15,-2.55142135623731)) ;
#118788 = CARTESIAN_POINT('Origin',(1.4,3.25,-5.06857864376269)) ;
#118789 = CARTESIAN_POINT('',(1.5,3.25,-5.06857864376269)) ;
#118790 = CARTESIAN_POINT('',(7.9,3.25,-2.55142135623731)) ;
#118791 = CARTESIAN_POINT('Origin',(1.4,2.52928932188134,-4.58928932188135)) ;
#118792 = CARTESIAN_POINT('',(1.5,2.52928932188134,-4.58928932188135)) ;
#118793 = CARTESIAN_POINT('',(1.5,2.52928932188134,-4.58928932188135)) ;
#118794 = CARTESIAN_POINT('',(7.9,2.52928932188134,-4.58928932188135)) ;
#118795 = CARTESIAN_POINT('',(1.4,2.52928932188134,-4.58928932188135)) ;
#118796 = CARTESIAN_POINT('',(7.9,3.07928932188135,-5.13928932188135)) ;
#118797 = CARTESIAN_POINT('Origin',(1.4,2.6,-4.51857864376269)) ;
#118798 = CARTESIAN_POINT('',(1.5,2.5,-4.51857864376269)) ;
#118799 = CARTESIAN_POINT('Origin',(1.5,2.6,-4.51857864376269)) ;
#118800 = CARTESIAN_POINT('',(7.9,2.5,-4.51857864376269)) ;
#118801 = CARTESIAN_POINT('',(1.4,2.5,-4.51857864376269)) ;
#118802 = CARTESIAN_POINT('Origin',(7.9,2.6,-4.51857864376269)) ;
#118803 = CARTESIAN_POINT('Origin',(1.4,2.5,-4.41)) ;
#118804 = CARTESIAN_POINT('',(1.5,2.5,-4.41)) ;
#118805 = CARTESIAN_POINT('',(1.5,2.5,-4.41)) ;
#118806 = CARTESIAN_POINT('',(7.9,2.5,-4.41)) ;
#118807 = CARTESIAN_POINT('',(1.4,2.5,-4.41)) ;
#118808 = CARTESIAN_POINT('',(7.9,2.5,-4.51857864376269)) ;
#118809 = CARTESIAN_POINT('Origin',(1.4,2.4,-4.41)) ;
#118810 = CARTESIAN_POINT('',(1.5,2.4,-4.31)) ;
#118811 = CARTESIAN_POINT('Origin',(1.5,2.4,-4.41)) ;
#118812 = CARTESIAN_POINT('',(7.9,2.4,-4.31)) ;
#118813 = CARTESIAN_POINT('',(1.4,2.4,-4.31)) ;
#118814 = CARTESIAN_POINT('Origin',(7.9,2.4,-4.41)) ;
#118815 = CARTESIAN_POINT('Origin',(1.4,2.1,-4.31)) ;
#118816 = CARTESIAN_POINT('',(1.5,2.1,-4.31)) ;
#118817 = CARTESIAN_POINT('',(1.5,2.1,-4.31)) ;
#118818 = CARTESIAN_POINT('',(7.9,2.1,-4.31)) ;
#118819 = CARTESIAN_POINT('',(1.4,2.1,-4.31)) ;
#118820 = CARTESIAN_POINT('',(7.9,2.4,-4.31)) ;
#118821 = CARTESIAN_POINT('Origin',(1.4,2.1,-4.41)) ;
#118822 = CARTESIAN_POINT('',(1.5,2.,-4.41)) ;
#118823 = CARTESIAN_POINT('Origin',(1.5,2.1,-4.41)) ;
#118824 = CARTESIAN_POINT('',(7.9,2.,-4.41)) ;
#118825 = CARTESIAN_POINT('',(1.4,2.,-4.41)) ;
#118826 = CARTESIAN_POINT('Origin',(7.9,2.1,-4.41)) ;
#118827 = CARTESIAN_POINT('Origin',(1.4,2.,-4.41)) ;
#118828 = CARTESIAN_POINT('',(1.5,2.,-5.36)) ;
#118829 = CARTESIAN_POINT('',(1.5,2.,-5.36)) ;
#118830 = CARTESIAN_POINT('',(7.9,2.,-5.36)) ;
#118831 = CARTESIAN_POINT('',(1.4,2.,-5.36)) ;
#118832 = CARTESIAN_POINT('',(7.9,2.,-4.41)) ;
#118833 = CARTESIAN_POINT('Origin',(1.4,1.9,-5.36)) ;
#118834 = CARTESIAN_POINT('',(1.5,1.9,-5.46)) ;
#118835 = CARTESIAN_POINT('Origin',(1.5,1.9,-5.36)) ;
#118836 = CARTESIAN_POINT('',(7.9,1.9,-5.46)) ;
#118837 = CARTESIAN_POINT('',(1.4,1.9,-5.46)) ;
#118838 = CARTESIAN_POINT('Origin',(7.9,1.9,-5.36)) ;
#118839 = CARTESIAN_POINT('Origin',(1.4,1.9,-5.46)) ;
#118840 = CARTESIAN_POINT('',(1.5,-2.15,-5.46)) ;
#118841 = CARTESIAN_POINT('',(1.5,-2.15,-5.46)) ;
#118842 = CARTESIAN_POINT('',(7.9,-2.15,-5.46)) ;
#118843 = CARTESIAN_POINT('',(1.4,-2.15,-5.46)) ;
#118844 = CARTESIAN_POINT('',(7.9,1.9,-5.46)) ;
#118845 = CARTESIAN_POINT('Origin',(1.4,-2.15,-5.36)) ;
#118846 = CARTESIAN_POINT('',(1.5,-2.25,-5.36)) ;
#118847 = CARTESIAN_POINT('Origin',(1.5,-2.15,-5.36)) ;
#118848 = CARTESIAN_POINT('',(7.9,-2.25,-5.36)) ;
#118849 = CARTESIAN_POINT('',(1.4,-2.25,-5.36)) ;
#118850 = CARTESIAN_POINT('Origin',(7.9,-2.15,-5.36)) ;
#118851 = CARTESIAN_POINT('Origin',(1.4,-2.25,-4.71311959340942)) ;
#118852 = CARTESIAN_POINT('',(1.5,-2.25,-4.71311959340942)) ;
#118853 = CARTESIAN_POINT('',(1.5,-2.25,-4.71311959340942)) ;
#118854 = CARTESIAN_POINT('',(7.9,-2.25,-4.71311959340942)) ;
#118855 = CARTESIAN_POINT('',(1.4,-2.25,-4.71311959340942)) ;
#118856 = CARTESIAN_POINT('',(7.9,-2.25,-5.36)) ;
#118857 = CARTESIAN_POINT('Origin',(1.4,-2.15,-4.71311959340942)) ;
#118858 = CARTESIAN_POINT('',(1.5,-2.23576512455516,-4.66169641371351)) ;
#118859 = CARTESIAN_POINT('Origin',(1.5,-2.15,-4.71311959340942)) ;
#118860 = CARTESIAN_POINT('',(7.9,-2.23576512455516,-4.66169641371351)) ;
#118861 = CARTESIAN_POINT('',(1.4,-2.23576512455516,-4.66169641371351)) ;
#118862 = CARTESIAN_POINT('Origin',(7.9,-2.15,-4.71311959340942)) ;
#118863 = CARTESIAN_POINT('Origin',(1.4,-3.65625,-3.81)) ;
#118864 = CARTESIAN_POINT('',(1.5,-2.23576512455516,-2.95830358628649)) ;
#118865 = CARTESIAN_POINT('Origin',(1.5,-3.65625,-3.81)) ;
#118866 = CARTESIAN_POINT('',(7.9,-2.23576512455516,-2.95830358628649)) ;
#118867 = CARTESIAN_POINT('',(1.4,-2.23576512455516,-2.95830358628649)) ;
#118868 = CARTESIAN_POINT('Origin',(7.9,-3.65625,-3.81)) ;
#118869 = CARTESIAN_POINT('Origin',(1.4,-2.15,-2.90688040659058)) ;
#118870 = CARTESIAN_POINT('',(1.5,-2.25,-2.90688040659058)) ;
#118871 = CARTESIAN_POINT('Origin',(1.5,-2.15,-2.90688040659058)) ;
#118872 = CARTESIAN_POINT('',(7.9,-2.25,-2.90688040659058)) ;
#118873 = CARTESIAN_POINT('',(1.4,-2.25,-2.90688040659058)) ;
#118874 = CARTESIAN_POINT('Origin',(7.9,-2.15,-2.90688040659058)) ;
#118875 = CARTESIAN_POINT('Origin',(1.4,-2.25,-2.26)) ;
#118876 = CARTESIAN_POINT('',(1.5,-2.25,-2.26)) ;
#118877 = CARTESIAN_POINT('',(1.5,-2.25,-2.26)) ;
#118878 = CARTESIAN_POINT('',(7.9,-2.25,-2.26)) ;
#118879 = CARTESIAN_POINT('',(1.4,-2.25,-2.26)) ;
#118880 = CARTESIAN_POINT('',(7.9,-2.25,-2.90688040659058)) ;
#118881 = CARTESIAN_POINT('Origin',(1.4,-2.15,-2.26)) ;
#118882 = CARTESIAN_POINT('',(1.5,-2.15,-2.16)) ;
#118883 = CARTESIAN_POINT('Origin',(1.5,-2.15,-2.26)) ;
#118884 = CARTESIAN_POINT('',(7.9,-2.15,-2.16)) ;
#118885 = CARTESIAN_POINT('',(1.4,-2.15,-2.16)) ;
#118886 = CARTESIAN_POINT('Origin',(7.9,-2.15,-2.26)) ;
#118887 = CARTESIAN_POINT('Origin',(1.4,1.9,-2.16)) ;
#118888 = CARTESIAN_POINT('',(1.5,1.9,-2.16)) ;
#118889 = CARTESIAN_POINT('',(1.5,1.9,-2.16)) ;
#118890 = CARTESIAN_POINT('',(7.9,1.9,-2.16)) ;
#118891 = CARTESIAN_POINT('',(1.4,1.9,-2.16)) ;
#118892 = CARTESIAN_POINT('',(7.9,-2.15,-2.16)) ;
#118893 = CARTESIAN_POINT('Origin',(1.4,1.9,-2.26)) ;
#118894 = CARTESIAN_POINT('',(1.5,2.,-2.26)) ;
#118895 = CARTESIAN_POINT('Origin',(1.5,1.9,-2.26)) ;
#118896 = CARTESIAN_POINT('',(7.9,2.,-2.26)) ;
#118897 = CARTESIAN_POINT('',(1.4,2.,-2.26)) ;
#118898 = CARTESIAN_POINT('Origin',(7.9,1.9,-2.26)) ;
#118899 = CARTESIAN_POINT('Origin',(1.4,2.,-2.26)) ;
#118900 = CARTESIAN_POINT('',(1.5,2.,-3.21)) ;
#118901 = CARTESIAN_POINT('',(7.9,2.,-2.26)) ;
#118902 = CARTESIAN_POINT('Origin',(1.4,2.1,-3.21)) ;
#118903 = CARTESIAN_POINT('',(1.4,2.6,-3.21)) ;
#118904 = CARTESIAN_POINT('',(1.4,2.4,-3.41)) ;
#118905 = CARTESIAN_POINT('Origin',(1.4,2.4,-3.21)) ;
#118906 = CARTESIAN_POINT('',(1.4,2.1,-3.41)) ;
#118907 = CARTESIAN_POINT('',(1.4,2.1,-3.41)) ;
#118908 = CARTESIAN_POINT('',(1.4,1.9,-3.21)) ;
#118909 = CARTESIAN_POINT('Origin',(1.4,2.1,-3.21)) ;
#118910 = CARTESIAN_POINT('',(1.4,1.9,-2.26)) ;
#118911 = CARTESIAN_POINT('',(1.4,1.9,-2.26)) ;
#118912 = CARTESIAN_POINT('',(1.4,-2.15,-2.26)) ;
#118913 = CARTESIAN_POINT('',(1.4,-2.15,-2.26)) ;
#118914 = CARTESIAN_POINT('',(1.4,-2.15,-2.90688040659058)) ;
#118915 = CARTESIAN_POINT('',(1.4,-2.15,-2.90688040659058)) ;
#118916 = CARTESIAN_POINT('',(1.4,-2.15,-4.71311959340942)) ;
#118917 = CARTESIAN_POINT('Origin',(1.4,-3.65625,-3.81)) ;
#118918 = CARTESIAN_POINT('',(1.4,-2.15,-5.36)) ;
#118919 = CARTESIAN_POINT('',(1.4,-2.15,-5.36)) ;
#118920 = CARTESIAN_POINT('',(1.4,1.9,-5.36)) ;
#118921 = CARTESIAN_POINT('',(1.4,1.9,-5.36)) ;
#118922 = CARTESIAN_POINT('',(1.4,1.9,-4.41)) ;
#118923 = CARTESIAN_POINT('',(1.4,1.9,-4.41)) ;
#118924 = CARTESIAN_POINT('',(1.4,2.1,-4.21)) ;
#118925 = CARTESIAN_POINT('Origin',(1.4,2.1,-4.41)) ;
#118926 = CARTESIAN_POINT('',(1.4,2.4,-4.21)) ;
#118927 = CARTESIAN_POINT('',(1.4,2.4,-4.21)) ;
#118928 = CARTESIAN_POINT('',(1.4,2.6,-4.41)) ;
#118929 = CARTESIAN_POINT('Origin',(1.4,2.4,-4.41)) ;
#118930 = CARTESIAN_POINT('',(1.4,2.6,-4.51857864376269)) ;
#118931 = CARTESIAN_POINT('',(1.4,2.6,-4.51857864376269)) ;
#118932 = CARTESIAN_POINT('',(1.4,3.15,-5.06857864376269)) ;
#118933 = CARTESIAN_POINT('',(1.4,3.15,-5.06857864376269)) ;
#118934 = CARTESIAN_POINT('',(1.4,3.15,-2.55142135623731)) ;
#118935 = CARTESIAN_POINT('',(1.4,2.6,-3.10142135623731)) ;
#118936 = CARTESIAN_POINT('',(1.4,2.6,-3.10142135623731)) ;
#118937 = CARTESIAN_POINT('',(1.4,2.6,-3.21)) ;
#118938 = CARTESIAN_POINT('Origin',(2.4,0.,-3.81)) ;
#118939 = CARTESIAN_POINT('',(2.4,0.3,-3.41)) ;
#118940 = CARTESIAN_POINT('',(2.4,-0.3,-3.41)) ;
#118941 = CARTESIAN_POINT('',(2.4,0.,-3.41)) ;
#118942 = CARTESIAN_POINT('',(2.4,0.4,-3.51)) ;
#118943 = CARTESIAN_POINT('Origin',(2.4,0.3,-3.51)) ;
#118944 = CARTESIAN_POINT('',(2.4,0.4,-4.11)) ;
#118945 = CARTESIAN_POINT('',(2.4,0.4,-3.81)) ;
#118946 = CARTESIAN_POINT('',(2.4,0.3,-4.21)) ;
#118947 = CARTESIAN_POINT('Origin',(2.4,0.3,-4.11)) ;
#118948 = CARTESIAN_POINT('',(2.4,-0.3,-4.21)) ;
#118949 = CARTESIAN_POINT('',(2.4,0.,-4.21)) ;
#118950 = CARTESIAN_POINT('',(2.4,-0.4,-4.11)) ;
#118951 = CARTESIAN_POINT('Origin',(2.4,-0.3,-4.11)) ;
#118952 = CARTESIAN_POINT('',(2.4,-0.4,-3.51)) ;
#118953 = CARTESIAN_POINT('',(2.4,-0.4,-3.81)) ;
#118954 = CARTESIAN_POINT('Origin',(2.4,-0.3,-3.51)) ;
#118955 = CARTESIAN_POINT('Origin',(2.4,0.,-7.62)) ;
#118956 = CARTESIAN_POINT('',(2.4,0.3,-7.22)) ;
#118957 = CARTESIAN_POINT('',(2.4,-0.3,-7.22)) ;
#118958 = CARTESIAN_POINT('',(2.4,0.,-7.22)) ;
#118959 = CARTESIAN_POINT('',(2.4,0.4,-7.32)) ;
#118960 = CARTESIAN_POINT('Origin',(2.4,0.3,-7.32)) ;
#118961 = CARTESIAN_POINT('',(2.4,0.4,-7.92)) ;
#118962 = CARTESIAN_POINT('',(2.4,0.4,-7.62)) ;
#118963 = CARTESIAN_POINT('',(2.4,0.3,-8.02)) ;
#118964 = CARTESIAN_POINT('Origin',(2.4,0.3,-7.92)) ;
#118965 = CARTESIAN_POINT('',(2.4,-0.3,-8.02)) ;
#118966 = CARTESIAN_POINT('',(2.4,0.,-8.02)) ;
#118967 = CARTESIAN_POINT('',(2.4,-0.4,-7.92)) ;
#118968 = CARTESIAN_POINT('Origin',(2.4,-0.3,-7.92)) ;
#118969 = CARTESIAN_POINT('',(2.4,-0.4,-7.32)) ;
#118970 = CARTESIAN_POINT('',(2.4,-0.4,-7.62)) ;
#118971 = CARTESIAN_POINT('Origin',(2.4,-0.3,-7.32)) ;
#118972 = CARTESIAN_POINT('Origin',(2.4,0.,-11.43)) ;
#118973 = CARTESIAN_POINT('',(2.4,0.3,-11.03)) ;
#118974 = CARTESIAN_POINT('',(2.4,-0.3,-11.03)) ;
#118975 = CARTESIAN_POINT('',(2.4,0.,-11.03)) ;
#118976 = CARTESIAN_POINT('',(2.4,0.4,-11.13)) ;
#118977 = CARTESIAN_POINT('Origin',(2.4,0.3,-11.13)) ;
#118978 = CARTESIAN_POINT('',(2.4,0.4,-11.73)) ;
#118979 = CARTESIAN_POINT('',(2.4,0.4,-11.43)) ;
#118980 = CARTESIAN_POINT('',(2.4,0.3,-11.83)) ;
#118981 = CARTESIAN_POINT('Origin',(2.4,0.3,-11.73)) ;
#118982 = CARTESIAN_POINT('',(2.4,-0.3,-11.83)) ;
#118983 = CARTESIAN_POINT('',(2.4,0.,-11.83)) ;
#118984 = CARTESIAN_POINT('',(2.4,-0.4,-11.73)) ;
#118985 = CARTESIAN_POINT('Origin',(2.4,-0.3,-11.73)) ;
#118986 = CARTESIAN_POINT('',(2.4,-0.4,-11.13)) ;
#118987 = CARTESIAN_POINT('',(2.4,-0.4,-11.43)) ;
#118988 = CARTESIAN_POINT('Origin',(2.4,-0.3,-11.13)) ;
#118989 = CARTESIAN_POINT('Origin',(2.4,0.,-15.24)) ;
#118990 = CARTESIAN_POINT('',(2.4,0.3,-14.84)) ;
#118991 = CARTESIAN_POINT('',(2.4,-0.3,-14.84)) ;
#118992 = CARTESIAN_POINT('',(2.4,0.,-14.84)) ;
#118993 = CARTESIAN_POINT('',(2.4,0.4,-14.94)) ;
#118994 = CARTESIAN_POINT('Origin',(2.4,0.3,-14.94)) ;
#118995 = CARTESIAN_POINT('',(2.4,0.4,-15.54)) ;
#118996 = CARTESIAN_POINT('',(2.4,0.4,-15.24)) ;
#118997 = CARTESIAN_POINT('',(2.4,0.3,-15.64)) ;
#118998 = CARTESIAN_POINT('Origin',(2.4,0.3,-15.54)) ;
#118999 = CARTESIAN_POINT('',(2.4,-0.3,-15.64)) ;
#119000 = CARTESIAN_POINT('',(2.4,0.,-15.64)) ;
#119001 = CARTESIAN_POINT('',(2.4,-0.4,-15.54)) ;
#119002 = CARTESIAN_POINT('Origin',(2.4,-0.3,-15.54)) ;
#119003 = CARTESIAN_POINT('',(2.4,-0.4,-14.94)) ;
#119004 = CARTESIAN_POINT('',(2.4,-0.4,-15.24)) ;
#119005 = CARTESIAN_POINT('Origin',(2.4,-0.3,-14.94)) ;
#119006 = CARTESIAN_POINT('Origin',(2.4,0.,-19.05)) ;
#119007 = CARTESIAN_POINT('',(2.4,0.3,-18.65)) ;
#119008 = CARTESIAN_POINT('',(2.4,-0.3,-18.65)) ;
#119009 = CARTESIAN_POINT('',(2.4,0.,-18.65)) ;
#119010 = CARTESIAN_POINT('',(2.4,0.4,-18.75)) ;
#119011 = CARTESIAN_POINT('Origin',(2.4,0.3,-18.75)) ;
#119012 = CARTESIAN_POINT('',(2.4,0.4,-19.35)) ;
#119013 = CARTESIAN_POINT('',(2.4,0.4,-19.05)) ;
#119014 = CARTESIAN_POINT('',(2.4,0.3,-19.45)) ;
#119015 = CARTESIAN_POINT('Origin',(2.4,0.3,-19.35)) ;
#119016 = CARTESIAN_POINT('',(2.4,-0.3,-19.45)) ;
#119017 = CARTESIAN_POINT('',(2.4,0.,-19.45)) ;
#119018 = CARTESIAN_POINT('',(2.4,-0.4,-19.35)) ;
#119019 = CARTESIAN_POINT('Origin',(2.4,-0.3,-19.35)) ;
#119020 = CARTESIAN_POINT('',(2.4,-0.4,-18.75)) ;
#119021 = CARTESIAN_POINT('',(2.4,-0.4,-19.05)) ;
#119022 = CARTESIAN_POINT('Origin',(2.4,-0.3,-18.75)) ;
#119023 = CARTESIAN_POINT('Origin',(2.4,0.,-22.86)) ;
#119024 = CARTESIAN_POINT('',(2.4,0.3,-22.46)) ;
#119025 = CARTESIAN_POINT('',(2.4,-0.3,-22.46)) ;
#119026 = CARTESIAN_POINT('',(2.4,0.,-22.46)) ;
#119027 = CARTESIAN_POINT('',(2.4,0.4,-22.56)) ;
#119028 = CARTESIAN_POINT('Origin',(2.4,0.3,-22.56)) ;
#119029 = CARTESIAN_POINT('',(2.4,0.4,-23.16)) ;
#119030 = CARTESIAN_POINT('',(2.4,0.4,-22.86)) ;
#119031 = CARTESIAN_POINT('',(2.4,0.3,-23.26)) ;
#119032 = CARTESIAN_POINT('Origin',(2.4,0.3,-23.16)) ;
#119033 = CARTESIAN_POINT('',(2.4,-0.3,-23.26)) ;
#119034 = CARTESIAN_POINT('',(2.4,0.,-23.26)) ;
#119035 = CARTESIAN_POINT('',(2.4,-0.4,-23.16)) ;
#119036 = CARTESIAN_POINT('Origin',(2.4,-0.3,-23.16)) ;
#119037 = CARTESIAN_POINT('',(2.4,-0.4,-22.56)) ;
#119038 = CARTESIAN_POINT('',(2.4,-0.4,-22.86)) ;
#119039 = CARTESIAN_POINT('Origin',(2.4,-0.3,-22.56)) ;
#119040 = CARTESIAN_POINT('Origin',(2.4,0.,-26.67)) ;
#119041 = CARTESIAN_POINT('',(2.4,0.3,-26.27)) ;
#119042 = CARTESIAN_POINT('',(2.4,-0.3,-26.27)) ;
#119043 = CARTESIAN_POINT('',(2.4,0.,-26.27)) ;
#119044 = CARTESIAN_POINT('',(2.4,0.4,-26.37)) ;
#119045 = CARTESIAN_POINT('Origin',(2.4,0.3,-26.37)) ;
#119046 = CARTESIAN_POINT('',(2.4,0.4,-26.97)) ;
#119047 = CARTESIAN_POINT('',(2.4,0.4,-26.67)) ;
#119048 = CARTESIAN_POINT('',(2.4,0.3,-27.07)) ;
#119049 = CARTESIAN_POINT('Origin',(2.4,0.3,-26.97)) ;
#119050 = CARTESIAN_POINT('',(2.4,-0.3,-27.07)) ;
#119051 = CARTESIAN_POINT('',(2.4,0.,-27.07)) ;
#119052 = CARTESIAN_POINT('',(2.4,-0.4,-26.97)) ;
#119053 = CARTESIAN_POINT('Origin',(2.4,-0.3,-26.97)) ;
#119054 = CARTESIAN_POINT('',(2.4,-0.4,-26.37)) ;
#119055 = CARTESIAN_POINT('',(2.4,-0.4,-26.67)) ;
#119056 = CARTESIAN_POINT('Origin',(2.4,-0.3,-26.37)) ;
#119057 = CARTESIAN_POINT('Origin',(2.4,0.,-30.48)) ;
#119058 = CARTESIAN_POINT('',(2.4,0.3,-30.08)) ;
#119059 = CARTESIAN_POINT('',(2.4,-0.3,-30.08)) ;
#119060 = CARTESIAN_POINT('',(2.4,0.,-30.08)) ;
#119061 = CARTESIAN_POINT('',(2.4,0.4,-30.18)) ;
#119062 = CARTESIAN_POINT('Origin',(2.4,0.3,-30.18)) ;
#119063 = CARTESIAN_POINT('',(2.4,0.4,-30.78)) ;
#119064 = CARTESIAN_POINT('',(2.4,0.4,-30.48)) ;
#119065 = CARTESIAN_POINT('',(2.4,0.3,-30.88)) ;
#119066 = CARTESIAN_POINT('Origin',(2.4,0.3,-30.78)) ;
#119067 = CARTESIAN_POINT('',(2.4,-0.3,-30.88)) ;
#119068 = CARTESIAN_POINT('',(2.4,0.,-30.88)) ;
#119069 = CARTESIAN_POINT('',(2.4,-0.4,-30.78)) ;
#119070 = CARTESIAN_POINT('Origin',(2.4,-0.3,-30.78)) ;
#119071 = CARTESIAN_POINT('',(2.4,-0.4,-30.18)) ;
#119072 = CARTESIAN_POINT('',(2.4,-0.4,-30.48)) ;
#119073 = CARTESIAN_POINT('Origin',(2.4,-0.3,-30.18)) ;
#119074 = CARTESIAN_POINT('Origin',(2.4,0.,-34.29)) ;
#119075 = CARTESIAN_POINT('',(2.4,0.3,-33.89)) ;
#119076 = CARTESIAN_POINT('',(2.4,-0.3,-33.89)) ;
#119077 = CARTESIAN_POINT('',(2.4,0.,-33.89)) ;
#119078 = CARTESIAN_POINT('',(2.4,0.4,-33.99)) ;
#119079 = CARTESIAN_POINT('Origin',(2.4,0.3,-33.99)) ;
#119080 = CARTESIAN_POINT('',(2.4,0.4,-34.59)) ;
#119081 = CARTESIAN_POINT('',(2.4,0.4,-34.29)) ;
#119082 = CARTESIAN_POINT('',(2.4,0.3,-34.69)) ;
#119083 = CARTESIAN_POINT('Origin',(2.4,0.3,-34.59)) ;
#119084 = CARTESIAN_POINT('',(2.4,-0.3,-34.69)) ;
#119085 = CARTESIAN_POINT('',(2.4,0.,-34.69)) ;
#119086 = CARTESIAN_POINT('',(2.4,-0.4,-34.59)) ;
#119087 = CARTESIAN_POINT('Origin',(2.4,-0.3,-34.59)) ;
#119088 = CARTESIAN_POINT('',(2.4,-0.4,-33.99)) ;
#119089 = CARTESIAN_POINT('',(2.4,-0.4,-34.29)) ;
#119090 = CARTESIAN_POINT('Origin',(2.4,-0.3,-33.99)) ;
#119091 = CARTESIAN_POINT('Origin',(-0.899999999999999,-2.,-3.21)) ;
#119092 = CARTESIAN_POINT('Origin',(-0.899999999999999,0.4,-3.21)) ;
#119093 = CARTESIAN_POINT('Origin',(-0.899999999999999,-1.9,-3.21)) ;
#119094 = CARTESIAN_POINT('Origin',(0.600000000000001,0.4,-3.41)) ;
#119095 = CARTESIAN_POINT('Origin',(0.500000000000001,0.4,-3.41)) ;
#119096 = CARTESIAN_POINT('Origin',(-0.899999999999999,0.4,-3.41)) ;
#119097 = CARTESIAN_POINT('Origin',(0.500000000000001,0.4,-3.41)) ;
#119098 = CARTESIAN_POINT('',(0.600000000000001,0.4,-3.41)) ;
#119099 = CARTESIAN_POINT('Origin',(0.500000000000001,0.4,-3.41)) ;
#119100 = CARTESIAN_POINT('Origin',(0.500000000000001,0.4,-3.41)) ;
#119101 = CARTESIAN_POINT('Origin',(-0.899999999999999,-1.9,-3.21)) ;
#119102 = CARTESIAN_POINT('Origin',(-0.899999999999999,-1.9,-3.21)) ;
#119103 = CARTESIAN_POINT('Origin',(-0.899999999999999,-1.9,-3.21)) ;
#119104 = CARTESIAN_POINT('Origin',(-0.899999999999999,0.4,-3.41)) ;
#119105 = CARTESIAN_POINT('Origin',(-0.899999999999999,0.6,-3.41)) ;
#119106 = CARTESIAN_POINT('Origin',(0.500000000000001,0.4,-3.81)) ;
#119107 = CARTESIAN_POINT('Origin',(0.500000000000001,0.4,-4.21)) ;
#119108 = CARTESIAN_POINT('',(0.600000000000001,0.4,-4.11)) ;
#119109 = CARTESIAN_POINT('Ctrl Pts',(0.595612997216081,0.370705721320404,
-4.1807057213204)) ;
#119110 = CARTESIAN_POINT('Ctrl Pts',(0.596180587760892,0.372558268494358,
-4.17885549883217)) ;
#119111 = CARTESIAN_POINT('Ctrl Pts',(0.596672461925686,0.374355839771985,
-4.17691417986631)) ;
#119112 = CARTESIAN_POINT('Ctrl Pts',(0.599015141889212,0.383869350930066,
-4.16576499365627)) ;
#119113 = CARTESIAN_POINT('Ctrl Pts',(0.599609996542525,0.390224332900452,
-4.15497260265412)) ;
#119114 = CARTESIAN_POINT('Ctrl Pts',(0.600050586298726,0.398117439141561,
-4.13233105320467)) ;
#119115 = CARTESIAN_POINT('Ctrl Pts',(0.600000000000001,0.399999999999999,
-4.12120125063352)) ;
#119116 = CARTESIAN_POINT('Ctrl Pts',(0.600000000000001,0.399999999999999,
-4.11)) ;
#119117 = CARTESIAN_POINT('',(0.600000000000001,0.4,-3.81)) ;
#119118 = CARTESIAN_POINT('Origin',(0.500000000000001,-4.56640444411541E-17,
-3.41)) ;
#119119 = CARTESIAN_POINT('',(0.500000000000001,0.394987437106619,-3.51)) ;
#119120 = CARTESIAN_POINT('Ctrl Pts',(0.500000000000001,0.394987437106619,
-3.51)) ;
#119121 = CARTESIAN_POINT('Ctrl Pts',(0.505940567948953,0.3955844866499,-3.51)) ;
#119122 = CARTESIAN_POINT('Ctrl Pts',(0.511931971019142,0.396132036079018,
-3.50946630032796)) ;
#119123 = CARTESIAN_POINT('Ctrl Pts',(0.517829015308552,0.396618246075354,
-3.50839779577372)) ;
#119124 = CARTESIAN_POINT('Ctrl Pts',(0.522982218721203,0.397043126556053,
-3.50746407015711)) ;
#119125 = CARTESIAN_POINT('Ctrl Pts',(0.528062648970231,0.397421319341388,
-3.50612282679706)) ;
#119126 = CARTESIAN_POINT('Ctrl Pts',(0.532978106724,0.397751505046071,-3.50440574387663)) ;
#119127 = CARTESIAN_POINT('Ctrl Pts',(0.538583536338964,0.398128038182999,
-3.50244763784955)) ;
#119128 = CARTESIAN_POINT('Ctrl Pts',(0.544059405914891,0.398447721828295,
-3.49997000831105)) ;
#119129 = CARTESIAN_POINT('Ctrl Pts',(0.549268572255782,0.398712331108983,
-3.49702073194289)) ;
#119130 = CARTESIAN_POINT('Ctrl Pts',(0.553856850427147,0.398945401221756,
-3.49442298414684)) ;
#119131 = CARTESIAN_POINT('Ctrl Pts',(0.558237825069328,0.399135987683843,
-3.49146038497999)) ;
#119132 = CARTESIAN_POINT('Ctrl Pts',(0.562333836086213,0.399290378266507,
-3.48819522286417)) ;
#119133 = CARTESIAN_POINT('Ctrl Pts',(0.56699032895789,0.399465895042381,
-3.48448326895231)) ;
#119134 = CARTESIAN_POINT('Ctrl Pts',(0.571349096493424,0.399597278936107,
-3.4803228064848)) ;
#119135 = CARTESIAN_POINT('Ctrl Pts',(0.57529692005671,0.399694832180837,
-3.47580557597935)) ;
#119136 = CARTESIAN_POINT('Ctrl Pts',(0.578744263667905,0.399780018245913,
-3.47186101121508)) ;
#119137 = CARTESIAN_POINT('Ctrl Pts',(0.581878314560428,0.399839626289636,
-3.46764552184211)) ;
#119138 = CARTESIAN_POINT('Ctrl Pts',(0.584648147334855,0.399882153365958,
-3.4632418177073)) ;
#119139 = CARTESIAN_POINT('Ctrl Pts',(0.587839270208174,0.399931148788079,
-3.4581683125045)) ;
#119140 = CARTESIAN_POINT('Ctrl Pts',(0.590595054415095,0.399958289583404,
-3.45276663624445)) ;
#119141 = CARTESIAN_POINT('Ctrl Pts',(0.592838618943107,0.399974357003159,
-3.44716168500939)) ;
#119142 = CARTESIAN_POINT('Ctrl Pts',(0.594777336851657,0.399988241245861,
-3.44231831224239)) ;
#119143 = CARTESIAN_POINT('Ctrl Pts',(0.59633405150619,0.399993946552814,
-3.43732416622712)) ;
#119144 = CARTESIAN_POINT('Ctrl Pts',(0.597488309822309,0.39999684570125,
-3.43227171856839)) ;
#119145 = CARTESIAN_POINT('Ctrl Pts',(0.598804024094397,0.400000150378306,
-3.42651254196058)) ;
#119146 = CARTESIAN_POINT('Ctrl Pts',(0.599612685195426,0.399999963509465,
-3.42060284389063)) ;
#119147 = CARTESIAN_POINT('Ctrl Pts',(0.599890230999718,0.399999993975383,
-3.41468420226113)) ;
#119148 = CARTESIAN_POINT('Ctrl Pts',(0.599963464549399,0.400000002014155,
-3.41312250278986)) ;
#119149 = CARTESIAN_POINT('Ctrl Pts',(0.600000000000001,0.399999999999999,
-3.4115602215092)) ;
#119150 = CARTESIAN_POINT('Ctrl Pts',(0.600000000000001,0.399999999999999,
-3.41)) ;
#119151 = CARTESIAN_POINT('',(0.600000000000001,0.299999999999999,-3.41)) ;
#119152 = CARTESIAN_POINT('Ctrl Pts',(0.500000000000001,0.394987437106619,
-3.51)) ;
#119153 = CARTESIAN_POINT('Ctrl Pts',(0.500454935589683,0.395033159853733,
-3.51)) ;
#119154 = CARTESIAN_POINT('Ctrl Pts',(0.500909898680391,0.395078570329052,
-3.50999689549113)) ;
#119155 = CARTESIAN_POINT('Ctrl Pts',(0.502892456245154,0.395275075889088,
-3.50996983394194)) ;
#119156 = CARTESIAN_POINT('Ctrl Pts',(0.504418747482365,0.395422812032198,
-3.50991398542099)) ;
#119157 = CARTESIAN_POINT('Ctrl Pts',(0.508462199543374,0.395804395682036,
-3.50967328105664)) ;
#119158 = CARTESIAN_POINT('Ctrl Pts',(0.51097495334332,0.396031485023319,
-3.50942793914505)) ;
#119159 = CARTESIAN_POINT('Ctrl Pts',(0.521160739721337,0.396903453186241,
-3.50804279449155)) ;
#119160 = CARTESIAN_POINT('Ctrl Pts',(0.528708678528462,0.397444933153163,
-3.50610421770467)) ;
#119161 = CARTESIAN_POINT('Ctrl Pts',(0.545943206358151,0.398105551684111,
-3.49946463945111)) ;
#119162 = CARTESIAN_POINT('Ctrl Pts',(0.555229535466881,0.397987646678422,
-3.49403535883592)) ;
#119163 = CARTESIAN_POINT('Ctrl Pts',(0.571394604995817,0.395490482808027,
-3.4807755133638)) ;
#119164 = CARTESIAN_POINT('Ctrl Pts',(0.578055313702888,0.393198948698317,
-3.47324074563169)) ;
#119165 = CARTESIAN_POINT('Ctrl Pts',(0.588559132202554,0.385442756729274,
-3.45739223398396)) ;
#119166 = CARTESIAN_POINT('Ctrl Pts',(0.592167355639999,0.380240075126842,
-3.44954826560675)) ;
#119167 = CARTESIAN_POINT('Ctrl Pts',(0.597496615531132,0.365892753466902,
-3.43392552179521)) ;
#119168 = CARTESIAN_POINT('Ctrl Pts',(0.598734255154207,0.35666056430058,
-3.42677274172686)) ;
#119169 = CARTESIAN_POINT('Ctrl Pts',(0.600012754681691,0.335223914398476,
-3.41558230586558)) ;
#119170 = CARTESIAN_POINT('Ctrl Pts',(0.59999390055981,0.322655037091807,
-3.41166151936557)) ;
#119171 = CARTESIAN_POINT('Ctrl Pts',(0.600000296204999,0.306106913582338,
-3.41013962634704)) ;
#119172 = CARTESIAN_POINT('Ctrl Pts',(0.600000000000001,0.303050992413427,
-3.41)) ;
#119173 = CARTESIAN_POINT('Ctrl Pts',(0.600000000000001,0.299999999999999,
-3.41)) ;
#119174 = CARTESIAN_POINT('',(0.600000000000001,-2.3980000991444E-17,-3.41)) ;
#119175 = CARTESIAN_POINT('Origin',(0.500000000000001,-1.9,-3.41)) ;
#119176 = CARTESIAN_POINT('Origin',(0.600000000000001,-1.9,-3.21)) ;
#119177 = CARTESIAN_POINT('Origin',(0.500000000000001,-1.9,-3.21)) ;
#119178 = CARTESIAN_POINT('Origin',(-0.899999999999999,-1.9,-2.435)) ;
#119179 = CARTESIAN_POINT('Origin',(-0.899999999999999,-1.9,-2.535)) ;
#119180 = CARTESIAN_POINT('Origin',(-0.899999999999999,0.6,-3.31)) ;
#119181 = CARTESIAN_POINT('Origin',(-0.899999999999999,0.6,-4.21)) ;
#119182 = CARTESIAN_POINT('Origin',(0.600000000000001,0.4,-4.21)) ;
#119183 = CARTESIAN_POINT('Origin',(0.500000000000001,0.4,-4.21)) ;
#119184 = CARTESIAN_POINT('Origin',(-0.899999999999999,0.4,-4.21)) ;
#119185 = CARTESIAN_POINT('Origin',(0.500000000000001,0.4,-4.21)) ;
#119186 = CARTESIAN_POINT('Origin',(0.500000000000001,-1.9,-3.21)) ;
#119187 = CARTESIAN_POINT('Origin',(0.500000000000001,-2.1,-3.21)) ;
#119188 = CARTESIAN_POINT('Origin',(-0.899999999999999,-1.9,-2.535)) ;
#119189 = CARTESIAN_POINT('Origin',(-1.1,-1.9,-2.535)) ;
#119190 = CARTESIAN_POINT('Origin',(-0.899999999999999,-2.1,-2.535)) ;
#119191 = CARTESIAN_POINT('Origin',(-0.899999999999999,0.4,-4.21)) ;
#119192 = CARTESIAN_POINT('Origin',(-0.899999999999999,0.4,-4.41)) ;
#119193 = CARTESIAN_POINT('Origin',(0.500000000000001,-2.1,-3.81)) ;
#119194 = CARTESIAN_POINT('Origin',(0.500000000000001,-2.1,-2.535)) ;
#119195 = CARTESIAN_POINT('Origin',(0.600000000000001,-2.1,-2.535)) ;
#119196 = CARTESIAN_POINT('Origin',(0.500000000000001,-2.1,-2.535)) ;
#119197 = CARTESIAN_POINT('Origin',(-1.1,-4.42727195005761E-17,-2.535)) ;
#119198 = CARTESIAN_POINT('',(-1.1,1.15,-2.435)) ;
#119199 = CARTESIAN_POINT('',(-1.1,1.25,-2.435)) ;
#119200 = CARTESIAN_POINT('Origin',(-1.1,1.15,-2.535)) ;
#119201 = CARTESIAN_POINT('Origin',(-0.899999999999999,0.5,-4.41)) ;
#119202 = CARTESIAN_POINT('Origin',(-0.899999999999999,-1.9,-4.41)) ;
#119203 = CARTESIAN_POINT('Origin',(0.600000000000001,-1.9,-4.41)) ;
#119204 = CARTESIAN_POINT('Origin',(0.500000000000001,-1.9,-4.41)) ;
#119205 = CARTESIAN_POINT('Origin',(-0.899999999999999,-1.9,-4.41)) ;
#119206 = CARTESIAN_POINT('Origin',(0.500000000000001,-1.9,-4.41)) ;
#119207 = CARTESIAN_POINT('Origin',(0.500000000000001,-2.1,-4.41)) ;
#119208 = CARTESIAN_POINT('Origin',(0.500000000000001,-2.1,-2.535)) ;
#119209 = CARTESIAN_POINT('Origin',(0.500000000000001,-2.1,-2.535)) ;
#119210 = CARTESIAN_POINT('Origin',(-1.1,-2.9,-2.335)) ;
#119211 = CARTESIAN_POINT('Origin',(-1.1,-2.9,-2.335)) ;
#119212 = CARTESIAN_POINT('Origin',(-1.1,-2.9,-2.335)) ;
#119213 = CARTESIAN_POINT('Origin',(-1.1,1.25,-2.335)) ;
#119214 = CARTESIAN_POINT('Origin',(-1.1,1.15,-2.335)) ;
#119215 = CARTESIAN_POINT('Origin',(-1.1,1.15,-2.535)) ;
#119216 = CARTESIAN_POINT('',(-1.1,1.25,-2.535)) ;
#119217 = CARTESIAN_POINT('Origin',(-1.1,1.15,-2.535)) ;
#119218 = CARTESIAN_POINT('Origin',(-1.1,1.15,-2.535)) ;
#119219 = CARTESIAN_POINT('Origin',(-0.899999999999999,-1.9,-4.41)) ;
#119220 = CARTESIAN_POINT('Origin',(-0.899999999999999,-1.9,-4.41)) ;
#119221 = CARTESIAN_POINT('Origin',(0.500000000000001,-2.1,-3.81)) ;
#119222 = CARTESIAN_POINT('Origin',(0.500000000000001,-2.1,-5.085)) ;
#119223 = CARTESIAN_POINT('Origin',(0.500000000000001,1.36481920536411E-16,
-2.535)) ;
#119224 = CARTESIAN_POINT('Origin',(0.500000000000001,-2.9,-2.535)) ;
#119225 = CARTESIAN_POINT('Origin',(-0.999999999999999,-2.9,-2.335)) ;
#119226 = CARTESIAN_POINT('Origin',(0.500000000000001,-2.9,-2.335)) ;
#119227 = CARTESIAN_POINT('Origin',(-1.1,1.15,-2.535)) ;
#119228 = CARTESIAN_POINT('Origin',(-1.1,1.35,-2.535)) ;
#119229 = CARTESIAN_POINT('Origin',(-1.1,1.15,-3.81)) ;
#119230 = CARTESIAN_POINT('',(-1.1,1.25,-5.085)) ;
#119231 = CARTESIAN_POINT('',(-1.1,1.25,-5.185)) ;
#119232 = CARTESIAN_POINT('Origin',(-1.1,1.15,-5.085)) ;
#119233 = CARTESIAN_POINT('Origin',(-0.899999999999999,-1.9,-4.31)) ;
#119234 = CARTESIAN_POINT('Origin',(-0.899999999999999,-1.9,-5.085)) ;
#119235 = CARTESIAN_POINT('Origin',(-0.999999999999999,-2.1,-5.085)) ;
#119236 = CARTESIAN_POINT('Origin',(0.500000000000001,-2.1,-5.085)) ;
#119237 = CARTESIAN_POINT('Origin',(-0.899999999999999,-2.1,-5.085)) ;
#119238 = CARTESIAN_POINT('Origin',(0.500000000000001,-2.1,-5.085)) ;
#119239 = CARTESIAN_POINT('Origin',(0.500000000000001,-2.1,-5.085)) ;
#119240 = CARTESIAN_POINT('Origin',(0.500000000000001,-2.9,-2.535)) ;
#119241 = CARTESIAN_POINT('Origin',(0.700000000000002,-2.9,-2.535)) ;
#119242 = CARTESIAN_POINT('Origin',(-1.1,1.35,-5.185)) ;
#119243 = CARTESIAN_POINT('Origin',(-1.1,1.35,-5.085)) ;
#119244 = CARTESIAN_POINT('Origin',(-1.1,1.15,-5.085)) ;
#119245 = CARTESIAN_POINT('',(-1.1,1.15,-5.185)) ;
#119246 = CARTESIAN_POINT('Origin',(-1.1,1.15,-5.085)) ;
#119247 = CARTESIAN_POINT('Origin',(-1.1,1.15,-5.085)) ;
#119248 = CARTESIAN_POINT('Origin',(-0.899999999999999,-1.9,-5.085)) ;
#119249 = CARTESIAN_POINT('Origin',(-1.1,-1.9,-5.085)) ;
#119250 = CARTESIAN_POINT('Origin',(0.500000000000001,-5.86744705109801E-17,
-5.085)) ;
#119251 = CARTESIAN_POINT('Origin',(0.500000000000001,-2.9,-5.085)) ;
#119252 = CARTESIAN_POINT('Origin',(0.700000000000002,-2.9,-3.81)) ;
#119253 = CARTESIAN_POINT('Origin',(0.700000000000002,-2.9,-5.085)) ;
#119254 = CARTESIAN_POINT('Origin',(-1.1,1.15,-5.085)) ;
#119255 = CARTESIAN_POINT('Origin',(-1.1,1.15,-5.285)) ;
#119256 = CARTESIAN_POINT('Origin',(-1.1,-2.39429110547967E-16,-5.085)) ;
#119257 = CARTESIAN_POINT('',(-1.1,1.25,-5.185)) ;
#119258 = CARTESIAN_POINT('Origin',(0.500000000000001,-2.9,-5.085)) ;
#119259 = CARTESIAN_POINT('Origin',(0.500000000000001,-2.9,-5.285)) ;
#119260 = CARTESIAN_POINT('Origin',(-1.1,1.25,-5.285)) ;
#119261 = CARTESIAN_POINT('Origin',(-1.1,-2.9,-5.285)) ;
#119262 = CARTESIAN_POINT('Origin',(-1.1,-2.9,-5.285)) ;
#119263 = CARTESIAN_POINT('Origin',(-1.1,-2.9,-5.285)) ;
#119264 = CARTESIAN_POINT('Origin',(-1.1,-2.9,-5.285)) ;
#119265 = CARTESIAN_POINT('Origin',(1.5,1.9,-3.21)) ;
#119266 = CARTESIAN_POINT('Origin',(1.5,1.9,-5.36)) ;
#119267 = CARTESIAN_POINT('Origin',(1.5,1.9,-4.41)) ;
#119268 = CARTESIAN_POINT('Origin',(1.5,2.1,-4.41)) ;
#119269 = CARTESIAN_POINT('Origin',(1.5,2.1,-4.21)) ;
#119270 = CARTESIAN_POINT('Origin',(1.5,1.9,-5.36)) ;
#119271 = CARTESIAN_POINT('Origin',(1.5,1.9,-5.36)) ;
#119272 = CARTESIAN_POINT('Origin',(1.5,2.1,-4.21)) ;
#119273 = CARTESIAN_POINT('Origin',(1.5,2.4,-4.21)) ;
#119274 = CARTESIAN_POINT('Origin',(1.5,2.1,-5.36)) ;
#119275 = CARTESIAN_POINT('Origin',(1.5,-2.15,-5.36)) ;
#119276 = CARTESIAN_POINT('Origin',(1.5,2.4,-4.41)) ;
#119277 = CARTESIAN_POINT('Origin',(1.5,2.6,-4.41)) ;
#119278 = CARTESIAN_POINT('Origin',(1.5,-2.15,-5.36)) ;
#119279 = CARTESIAN_POINT('Origin',(1.5,-2.15,-5.36)) ;
#119280 = CARTESIAN_POINT('Origin',(1.5,2.6,-3.21)) ;
#119281 = CARTESIAN_POINT('Origin',(1.5,2.6,-4.51857864376269)) ;
#119282 = CARTESIAN_POINT('Origin',(1.5,-2.15,-3.21)) ;
#119283 = CARTESIAN_POINT('Origin',(1.5,-2.15,-4.71311959340942)) ;
#119284 = CARTESIAN_POINT('Origin',(1.5,2.6,-4.51857864376269)) ;
#119285 = CARTESIAN_POINT('Origin',(1.5,2.6,-4.51857864376269)) ;
#119286 = CARTESIAN_POINT('Origin',(1.5,-2.15,-4.71311959340942)) ;
#119287 = CARTESIAN_POINT('Origin',(1.5,-2.15,-4.71311959340942)) ;
#119288 = CARTESIAN_POINT('Origin',(1.5,1.69571067811865,-3.61428932188135)) ;
#119289 = CARTESIAN_POINT('Origin',(1.5,3.15,-5.06857864376269)) ;
#119290 = CARTESIAN_POINT('Origin',(1.5,-3.65625,-3.81)) ;
#119291 = CARTESIAN_POINT('Origin',(1.5,-2.15,-2.90688040659058)) ;
#119292 = CARTESIAN_POINT('Origin',(1.5,3.15,-5.06857864376269)) ;
#119293 = CARTESIAN_POINT('Origin',(1.5,3.15,-5.06857864376269)) ;
#119294 = CARTESIAN_POINT('Origin',(1.5,-2.15,-2.90688040659058)) ;
#119295 = CARTESIAN_POINT('Origin',(1.5,-2.15,-2.90688040659058)) ;
#119296 = CARTESIAN_POINT('Origin',(1.5,3.15,-3.21)) ;
#119297 = CARTESIAN_POINT('Origin',(1.5,-2.15,-3.21)) ;
#119298 = CARTESIAN_POINT('Origin',(1.5,-2.15,-2.26)) ;
#119299 = CARTESIAN_POINT('Origin',(1.5,-2.15,-2.26)) ;
#119300 = CARTESIAN_POINT('Origin',(1.5,-2.15,-2.26)) ;
#119301 = CARTESIAN_POINT('Origin',(1.5,2.29571067811866,-3.40571067811866)) ;
#119302 = CARTESIAN_POINT('Origin',(1.5,2.6,-3.10142135623731)) ;
#119303 = CARTESIAN_POINT('Origin',(1.5,2.1,-2.26)) ;
#119304 = CARTESIAN_POINT('Origin',(1.5,1.9,-2.26)) ;
#119305 = CARTESIAN_POINT('Origin',(1.5,2.6,-3.10142135623731)) ;
#119306 = CARTESIAN_POINT('Origin',(1.5,2.6,-3.10142135623731)) ;
#119307 = CARTESIAN_POINT('Origin',(1.5,1.9,-2.26)) ;
#119308 = CARTESIAN_POINT('Origin',(1.5,1.9,-2.26)) ;
#119309 = CARTESIAN_POINT('Origin',(1.5,2.6,-3.21)) ;
#119310 = CARTESIAN_POINT('Origin',(1.5,2.6,-3.21)) ;
#119311 = CARTESIAN_POINT('Origin',(1.5,1.9,-3.21)) ;
#119312 = CARTESIAN_POINT('Origin',(1.5,1.9,-3.21)) ;
#119313 = CARTESIAN_POINT('Origin',(1.5,2.4,-3.21)) ;
#119314 = CARTESIAN_POINT('Origin',(1.5,2.4,-3.41)) ;
#119315 = CARTESIAN_POINT('Origin',(1.5,2.1,-3.21)) ;
#119316 = CARTESIAN_POINT('Origin',(1.5,2.1,-3.41)) ;
#119317 = CARTESIAN_POINT('Origin',(1.5,2.1,-3.41)) ;
#119318 = CARTESIAN_POINT('Origin',(7.9,2.1,-34.89)) ;
#119319 = CARTESIAN_POINT('Origin',(7.9,2.4,-34.89)) ;
#119320 = CARTESIAN_POINT('Origin',(7.9,2.1,-34.89)) ;
#119321 = CARTESIAN_POINT('Origin',(7.9,2.4,-34.89)) ;
#119322 = CARTESIAN_POINT('Origin',(7.9,2.4,-34.89)) ;
#119323 = CARTESIAN_POINT('Origin',(7.9,2.1,-34.89)) ;
#119324 = CARTESIAN_POINT('Origin',(7.9,2.1,-34.89)) ;
#119325 = CARTESIAN_POINT('Origin',(7.9,2.4,-34.89)) ;
#119326 = CARTESIAN_POINT('Origin',(7.9,2.4,-34.9985786437627)) ;
#119327 = CARTESIAN_POINT('Origin',(7.9,2.1,-34.89)) ;
#119328 = CARTESIAN_POINT('Origin',(7.9,2.1,-35.84)) ;
#119329 = CARTESIAN_POINT('Origin',(7.9,2.6,-34.9985786437627)) ;
#119330 = CARTESIAN_POINT('Origin',(7.9,2.45857864376269,-35.14)) ;
#119331 = CARTESIAN_POINT('Origin',(7.9,1.9,-35.84)) ;
#119332 = CARTESIAN_POINT('Origin',(7.9,1.9,-36.04)) ;
#119333 = CARTESIAN_POINT('Origin',(7.9,2.45857864376269,-35.14)) ;
#119334 = CARTESIAN_POINT('Origin',(7.9,1.9,-36.04)) ;
#119335 = CARTESIAN_POINT('Origin',(7.9,-2.15,-36.04)) ;
#119336 = CARTESIAN_POINT('Origin',(7.9,-2.15,-35.84)) ;
#119337 = CARTESIAN_POINT('Origin',(7.9,-2.35,-35.84)) ;
#119338 = CARTESIAN_POINT('Origin',(7.9,3.35,-35.5485786437627)) ;
#119339 = CARTESIAN_POINT('Origin',(7.9,3.35,-33.0314213562373)) ;
#119340 = CARTESIAN_POINT('Origin',(7.9,-2.35,-35.1931195934094)) ;
#119341 = CARTESIAN_POINT('Origin',(7.9,-2.35,-35.1931195934094)) ;
#119342 = CARTESIAN_POINT('Origin',(7.9,3.15,-33.0314213562373)) ;
#119343 = CARTESIAN_POINT('Origin',(7.9,3.00857864376269,-32.89)) ;
#119344 = CARTESIAN_POINT('Origin',(7.9,-2.15,-35.1931195934094)) ;
#119345 = CARTESIAN_POINT('Origin',(7.9,-2.32153024911032,-35.0902732340176)) ;
#119346 = CARTESIAN_POINT('Origin',(7.9,3.00857864376269,-32.89)) ;
#119347 = CARTESIAN_POINT('Origin',(7.9,2.45857864376269,-33.44)) ;
#119348 = CARTESIAN_POINT('Origin',(7.9,-3.65625,-34.29)) ;
#119349 = CARTESIAN_POINT('Origin',(7.9,-2.32153024911033,-33.4897267659824)) ;
#119350 = CARTESIAN_POINT('Origin',(7.9,2.6,-33.5814213562373)) ;
#119351 = CARTESIAN_POINT('Origin',(7.9,2.4,-33.5814213562373)) ;
#119352 = CARTESIAN_POINT('Origin',(7.9,-2.15,-33.3868804065906)) ;
#119353 = CARTESIAN_POINT('Origin',(7.9,-2.35,-33.3868804065906)) ;
#119354 = CARTESIAN_POINT('Origin',(7.9,2.4,-33.5814213562373)) ;
#119355 = CARTESIAN_POINT('Origin',(7.9,2.4,-33.69)) ;
#119356 = CARTESIAN_POINT('Origin',(7.9,-2.35,-32.74)) ;
#119357 = CARTESIAN_POINT('Origin',(7.9,-2.35,-32.74)) ;
#119358 = CARTESIAN_POINT('Origin',(7.9,2.4,-33.69)) ;
#119359 = CARTESIAN_POINT('Origin',(7.9,2.4,-33.69)) ;
#119360 = CARTESIAN_POINT('Origin',(7.9,-2.15,-32.74)) ;
#119361 = CARTESIAN_POINT('Origin',(7.9,-2.15,-32.54)) ;
#119362 = CARTESIAN_POINT('Origin',(7.9,2.4,-33.69)) ;
#119363 = CARTESIAN_POINT('Origin',(7.9,2.1,-33.69)) ;
#119364 = CARTESIAN_POINT('Origin',(7.9,1.9,-32.54)) ;
#119365 = CARTESIAN_POINT('Origin',(7.9,1.9,-32.54)) ;
#119366 = CARTESIAN_POINT('Origin',(7.9,2.1,-33.69)) ;
#119367 = CARTESIAN_POINT('Origin',(7.9,2.1,-33.69)) ;
#119368 = CARTESIAN_POINT('Origin',(7.9,1.9,-32.74)) ;
#119369 = CARTESIAN_POINT('Origin',(7.9,2.1,-32.74)) ;
#119370 = CARTESIAN_POINT('Origin',(7.9,2.1,-32.74)) ;
#119371 = CARTESIAN_POINT('Origin',(7.9,2.1,-31.08)) ;
#119372 = CARTESIAN_POINT('Origin',(7.9,2.4,-31.08)) ;
#119373 = CARTESIAN_POINT('Origin',(7.9,2.1,-31.08)) ;
#119374 = CARTESIAN_POINT('Origin',(7.9,2.4,-31.08)) ;
#119375 = CARTESIAN_POINT('Origin',(7.9,2.4,-31.08)) ;
#119376 = CARTESIAN_POINT('Origin',(7.9,2.1,-31.08)) ;
#119377 = CARTESIAN_POINT('Origin',(7.9,2.1,-31.08)) ;
#119378 = CARTESIAN_POINT('Origin',(7.9,2.4,-31.08)) ;
#119379 = CARTESIAN_POINT('Origin',(7.9,2.4,-31.1885786437627)) ;
#119380 = CARTESIAN_POINT('Origin',(7.9,2.1,-31.08)) ;
#119381 = CARTESIAN_POINT('Origin',(7.9,2.1,-32.03)) ;
#119382 = CARTESIAN_POINT('Origin',(7.9,2.6,-31.1885786437627)) ;
#119383 = CARTESIAN_POINT('Origin',(7.9,2.45857864376269,-31.33)) ;
#119384 = CARTESIAN_POINT('Origin',(7.9,1.9,-32.03)) ;
#119385 = CARTESIAN_POINT('Origin',(7.9,1.9,-32.23)) ;
#119386 = CARTESIAN_POINT('Origin',(7.9,2.45857864376269,-31.33)) ;
#119387 = CARTESIAN_POINT('Origin',(7.9,1.9,-32.23)) ;
#119388 = CARTESIAN_POINT('Origin',(7.9,-2.15,-32.23)) ;
#119389 = CARTESIAN_POINT('Origin',(7.9,-2.15,-32.03)) ;
#119390 = CARTESIAN_POINT('Origin',(7.9,-2.35,-32.03)) ;
#119391 = CARTESIAN_POINT('Origin',(7.9,3.35,-31.7385786437627)) ;
#119392 = CARTESIAN_POINT('Origin',(7.9,3.35,-29.2214213562373)) ;
#119393 = CARTESIAN_POINT('Origin',(7.9,-2.35,-31.3831195934094)) ;
#119394 = CARTESIAN_POINT('Origin',(7.9,-2.35,-31.3831195934094)) ;
#119395 = CARTESIAN_POINT('Origin',(7.9,3.15,-29.2214213562373)) ;
#119396 = CARTESIAN_POINT('Origin',(7.9,3.00857864376269,-29.08)) ;
#119397 = CARTESIAN_POINT('Origin',(7.9,-2.15,-31.3831195934094)) ;
#119398 = CARTESIAN_POINT('Origin',(7.9,-2.32153024911032,-31.2802732340176)) ;
#119399 = CARTESIAN_POINT('Origin',(7.9,3.00857864376269,-29.08)) ;
#119400 = CARTESIAN_POINT('Origin',(7.9,2.45857864376269,-29.63)) ;
#119401 = CARTESIAN_POINT('Origin',(7.9,-3.65625,-30.48)) ;
#119402 = CARTESIAN_POINT('Origin',(7.9,-2.32153024911032,-29.6797267659824)) ;
#119403 = CARTESIAN_POINT('Origin',(7.9,2.6,-29.7714213562373)) ;
#119404 = CARTESIAN_POINT('Origin',(7.9,2.4,-29.7714213562373)) ;
#119405 = CARTESIAN_POINT('Origin',(7.9,-2.15,-29.5768804065906)) ;
#119406 = CARTESIAN_POINT('Origin',(7.9,-2.35,-29.5768804065906)) ;
#119407 = CARTESIAN_POINT('Origin',(7.9,2.4,-29.7714213562373)) ;
#119408 = CARTESIAN_POINT('Origin',(7.9,2.4,-29.88)) ;
#119409 = CARTESIAN_POINT('Origin',(7.9,-2.35,-28.93)) ;
#119410 = CARTESIAN_POINT('Origin',(7.9,-2.35,-28.93)) ;
#119411 = CARTESIAN_POINT('Origin',(7.9,2.4,-29.88)) ;
#119412 = CARTESIAN_POINT('Origin',(7.9,2.4,-29.88)) ;
#119413 = CARTESIAN_POINT('Origin',(7.9,-2.15,-28.93)) ;
#119414 = CARTESIAN_POINT('Origin',(7.9,-2.15,-28.73)) ;
#119415 = CARTESIAN_POINT('Origin',(7.9,2.4,-29.88)) ;
#119416 = CARTESIAN_POINT('Origin',(7.9,2.1,-29.88)) ;
#119417 = CARTESIAN_POINT('Origin',(7.9,1.9,-28.73)) ;
#119418 = CARTESIAN_POINT('Origin',(7.9,1.9,-28.73)) ;
#119419 = CARTESIAN_POINT('Origin',(7.9,2.1,-29.88)) ;
#119420 = CARTESIAN_POINT('Origin',(7.9,2.1,-29.88)) ;
#119421 = CARTESIAN_POINT('Origin',(7.9,1.9,-28.93)) ;
#119422 = CARTESIAN_POINT('Origin',(7.9,2.1,-28.93)) ;
#119423 = CARTESIAN_POINT('Origin',(7.9,2.1,-28.93)) ;
#119424 = CARTESIAN_POINT('Origin',(7.9,2.1,-27.27)) ;
#119425 = CARTESIAN_POINT('Origin',(7.9,2.4,-27.27)) ;
#119426 = CARTESIAN_POINT('Origin',(7.9,2.1,-27.27)) ;
#119427 = CARTESIAN_POINT('Origin',(7.9,2.4,-27.27)) ;
#119428 = CARTESIAN_POINT('Origin',(7.9,2.4,-27.27)) ;
#119429 = CARTESIAN_POINT('Origin',(7.9,2.1,-27.27)) ;
#119430 = CARTESIAN_POINT('Origin',(7.9,2.1,-27.27)) ;
#119431 = CARTESIAN_POINT('Origin',(7.9,2.4,-27.27)) ;
#119432 = CARTESIAN_POINT('Origin',(7.9,2.4,-27.3785786437627)) ;
#119433 = CARTESIAN_POINT('Origin',(7.9,2.1,-27.27)) ;
#119434 = CARTESIAN_POINT('Origin',(7.9,2.1,-28.22)) ;
#119435 = CARTESIAN_POINT('Origin',(7.9,2.6,-27.3785786437627)) ;
#119436 = CARTESIAN_POINT('Origin',(7.9,2.45857864376269,-27.52)) ;
#119437 = CARTESIAN_POINT('Origin',(7.9,1.9,-28.22)) ;
#119438 = CARTESIAN_POINT('Origin',(7.9,1.9,-28.42)) ;
#119439 = CARTESIAN_POINT('Origin',(7.9,2.45857864376269,-27.52)) ;
#119440 = CARTESIAN_POINT('Origin',(7.9,1.9,-28.42)) ;
#119441 = CARTESIAN_POINT('Origin',(7.9,-2.15,-28.42)) ;
#119442 = CARTESIAN_POINT('Origin',(7.9,-2.15,-28.22)) ;
#119443 = CARTESIAN_POINT('Origin',(7.9,-2.35,-28.22)) ;
#119444 = CARTESIAN_POINT('Origin',(7.9,3.35,-27.9285786437627)) ;
#119445 = CARTESIAN_POINT('Origin',(7.9,3.35,-25.4114213562373)) ;
#119446 = CARTESIAN_POINT('Origin',(7.9,-2.35,-27.5731195934094)) ;
#119447 = CARTESIAN_POINT('Origin',(7.9,-2.35,-27.5731195934094)) ;
#119448 = CARTESIAN_POINT('Origin',(7.9,3.15,-25.4114213562373)) ;
#119449 = CARTESIAN_POINT('Origin',(7.9,3.00857864376269,-25.27)) ;
#119450 = CARTESIAN_POINT('Origin',(7.9,-2.15,-27.5731195934094)) ;
#119451 = CARTESIAN_POINT('Origin',(7.9,-2.32153024911032,-27.4702732340176)) ;
#119452 = CARTESIAN_POINT('Origin',(7.9,3.00857864376269,-25.27)) ;
#119453 = CARTESIAN_POINT('Origin',(7.9,2.45857864376269,-25.82)) ;
#119454 = CARTESIAN_POINT('Origin',(7.9,-3.65625,-26.67)) ;
#119455 = CARTESIAN_POINT('Origin',(7.9,-2.32153024911032,-25.8697267659824)) ;
#119456 = CARTESIAN_POINT('Origin',(7.9,2.6,-25.9614213562373)) ;
#119457 = CARTESIAN_POINT('Origin',(7.9,2.4,-25.9614213562373)) ;
#119458 = CARTESIAN_POINT('Origin',(7.9,-2.15,-25.7668804065906)) ;
#119459 = CARTESIAN_POINT('Origin',(7.9,-2.35,-25.7668804065906)) ;
#119460 = CARTESIAN_POINT('Origin',(7.9,2.4,-25.9614213562373)) ;
#119461 = CARTESIAN_POINT('Origin',(7.9,2.4,-26.07)) ;
#119462 = CARTESIAN_POINT('Origin',(7.9,-2.35,-25.12)) ;
#119463 = CARTESIAN_POINT('Origin',(7.9,-2.35,-25.12)) ;
#119464 = CARTESIAN_POINT('Origin',(7.9,2.4,-26.07)) ;
#119465 = CARTESIAN_POINT('Origin',(7.9,2.4,-26.07)) ;
#119466 = CARTESIAN_POINT('Origin',(7.9,-2.15,-25.12)) ;
#119467 = CARTESIAN_POINT('Origin',(7.9,-2.15,-24.92)) ;
#119468 = CARTESIAN_POINT('Origin',(7.9,2.4,-26.07)) ;
#119469 = CARTESIAN_POINT('Origin',(7.9,2.1,-26.07)) ;
#119470 = CARTESIAN_POINT('Origin',(7.9,1.9,-24.92)) ;
#119471 = CARTESIAN_POINT('Origin',(7.9,1.9,-24.92)) ;
#119472 = CARTESIAN_POINT('Origin',(7.9,2.1,-26.07)) ;
#119473 = CARTESIAN_POINT('Origin',(7.9,2.1,-26.07)) ;
#119474 = CARTESIAN_POINT('Origin',(7.9,1.9,-25.12)) ;
#119475 = CARTESIAN_POINT('Origin',(7.9,2.1,-25.12)) ;
#119476 = CARTESIAN_POINT('Origin',(7.9,2.1,-25.12)) ;
#119477 = CARTESIAN_POINT('Origin',(7.9,2.1,-23.46)) ;
#119478 = CARTESIAN_POINT('Origin',(7.9,2.4,-23.46)) ;
#119479 = CARTESIAN_POINT('Origin',(7.9,2.1,-23.46)) ;
#119480 = CARTESIAN_POINT('Origin',(7.9,2.4,-23.46)) ;
#119481 = CARTESIAN_POINT('Origin',(7.9,2.4,-23.46)) ;
#119482 = CARTESIAN_POINT('Origin',(7.9,2.1,-23.46)) ;
#119483 = CARTESIAN_POINT('Origin',(7.9,2.1,-23.46)) ;
#119484 = CARTESIAN_POINT('Origin',(7.9,2.4,-23.46)) ;
#119485 = CARTESIAN_POINT('Origin',(7.9,2.4,-23.5685786437627)) ;
#119486 = CARTESIAN_POINT('Origin',(7.9,2.1,-23.46)) ;
#119487 = CARTESIAN_POINT('Origin',(7.9,2.1,-24.41)) ;
#119488 = CARTESIAN_POINT('Origin',(7.9,2.6,-23.5685786437627)) ;
#119489 = CARTESIAN_POINT('Origin',(7.9,2.45857864376269,-23.71)) ;
#119490 = CARTESIAN_POINT('Origin',(7.9,1.9,-24.41)) ;
#119491 = CARTESIAN_POINT('Origin',(7.9,1.9,-24.61)) ;
#119492 = CARTESIAN_POINT('Origin',(7.9,2.45857864376269,-23.71)) ;
#119493 = CARTESIAN_POINT('Origin',(7.9,1.9,-24.61)) ;
#119494 = CARTESIAN_POINT('Origin',(7.9,-2.15,-24.61)) ;
#119495 = CARTESIAN_POINT('Origin',(7.9,-2.15,-24.41)) ;
#119496 = CARTESIAN_POINT('Origin',(7.9,-2.35,-24.41)) ;
#119497 = CARTESIAN_POINT('Origin',(7.9,3.35,-24.1185786437627)) ;
#119498 = CARTESIAN_POINT('Origin',(7.9,3.35,-21.6014213562373)) ;
#119499 = CARTESIAN_POINT('Origin',(7.9,-2.35,-23.7631195934094)) ;
#119500 = CARTESIAN_POINT('Origin',(7.9,-2.35,-23.7631195934094)) ;
#119501 = CARTESIAN_POINT('Origin',(7.9,3.15,-21.6014213562373)) ;
#119502 = CARTESIAN_POINT('Origin',(7.9,3.00857864376269,-21.46)) ;
#119503 = CARTESIAN_POINT('Origin',(7.9,-2.15,-23.7631195934094)) ;
#119504 = CARTESIAN_POINT('Origin',(7.9,-2.32153024911032,-23.6602732340176)) ;
#119505 = CARTESIAN_POINT('Origin',(7.9,3.00857864376269,-21.46)) ;
#119506 = CARTESIAN_POINT('Origin',(7.9,2.45857864376269,-22.01)) ;
#119507 = CARTESIAN_POINT('Origin',(7.9,-3.65625,-22.86)) ;
#119508 = CARTESIAN_POINT('Origin',(7.9,-2.32153024911032,-22.0597267659824)) ;
#119509 = CARTESIAN_POINT('Origin',(7.9,2.6,-22.1514213562373)) ;
#119510 = CARTESIAN_POINT('Origin',(7.9,2.4,-22.1514213562373)) ;
#119511 = CARTESIAN_POINT('Origin',(7.9,-2.15,-21.9568804065906)) ;
#119512 = CARTESIAN_POINT('Origin',(7.9,-2.35,-21.9568804065906)) ;
#119513 = CARTESIAN_POINT('Origin',(7.9,2.4,-22.1514213562373)) ;
#119514 = CARTESIAN_POINT('Origin',(7.9,2.4,-22.26)) ;
#119515 = CARTESIAN_POINT('Origin',(7.9,-2.35,-21.31)) ;
#119516 = CARTESIAN_POINT('Origin',(7.9,-2.35,-21.31)) ;
#119517 = CARTESIAN_POINT('Origin',(7.9,2.4,-22.26)) ;
#119518 = CARTESIAN_POINT('Origin',(7.9,2.4,-22.26)) ;
#119519 = CARTESIAN_POINT('Origin',(7.9,-2.15,-21.31)) ;
#119520 = CARTESIAN_POINT('Origin',(7.9,-2.15,-21.11)) ;
#119521 = CARTESIAN_POINT('Origin',(7.9,2.4,-22.26)) ;
#119522 = CARTESIAN_POINT('Origin',(7.9,2.1,-22.26)) ;
#119523 = CARTESIAN_POINT('Origin',(7.9,1.9,-21.11)) ;
#119524 = CARTESIAN_POINT('Origin',(7.9,1.9,-21.11)) ;
#119525 = CARTESIAN_POINT('Origin',(7.9,2.1,-22.26)) ;
#119526 = CARTESIAN_POINT('Origin',(7.9,2.1,-22.26)) ;
#119527 = CARTESIAN_POINT('Origin',(7.9,1.9,-21.31)) ;
#119528 = CARTESIAN_POINT('Origin',(7.9,2.1,-21.31)) ;
#119529 = CARTESIAN_POINT('Origin',(7.9,2.1,-21.31)) ;
#119530 = CARTESIAN_POINT('Origin',(7.9,2.1,-19.65)) ;
#119531 = CARTESIAN_POINT('Origin',(7.9,2.4,-19.65)) ;
#119532 = CARTESIAN_POINT('Origin',(7.9,2.1,-19.65)) ;
#119533 = CARTESIAN_POINT('Origin',(7.9,2.4,-19.65)) ;
#119534 = CARTESIAN_POINT('Origin',(7.9,2.4,-19.65)) ;
#119535 = CARTESIAN_POINT('Origin',(7.9,2.1,-19.65)) ;
#119536 = CARTESIAN_POINT('Origin',(7.9,2.1,-19.65)) ;
#119537 = CARTESIAN_POINT('Origin',(7.9,2.4,-19.65)) ;
#119538 = CARTESIAN_POINT('Origin',(7.9,2.4,-19.7585786437627)) ;
#119539 = CARTESIAN_POINT('Origin',(7.9,2.1,-19.65)) ;
#119540 = CARTESIAN_POINT('Origin',(7.9,2.1,-20.6)) ;
#119541 = CARTESIAN_POINT('Origin',(7.9,2.6,-19.7585786437627)) ;
#119542 = CARTESIAN_POINT('Origin',(7.9,2.45857864376269,-19.9)) ;
#119543 = CARTESIAN_POINT('Origin',(7.9,1.9,-20.6)) ;
#119544 = CARTESIAN_POINT('Origin',(7.9,1.9,-20.8)) ;
#119545 = CARTESIAN_POINT('Origin',(7.9,2.45857864376269,-19.9)) ;
#119546 = CARTESIAN_POINT('Origin',(7.9,1.9,-20.8)) ;
#119547 = CARTESIAN_POINT('Origin',(7.9,-2.15,-20.8)) ;
#119548 = CARTESIAN_POINT('Origin',(7.9,-2.15,-20.6)) ;
#119549 = CARTESIAN_POINT('Origin',(7.9,-2.35,-20.6)) ;
#119550 = CARTESIAN_POINT('Origin',(7.9,3.35,-20.3085786437627)) ;
#119551 = CARTESIAN_POINT('Origin',(7.9,3.35,-17.7914213562373)) ;
#119552 = CARTESIAN_POINT('Origin',(7.9,-2.35,-19.9531195934094)) ;
#119553 = CARTESIAN_POINT('Origin',(7.9,-2.35,-19.9531195934094)) ;
#119554 = CARTESIAN_POINT('Origin',(7.9,3.15,-17.7914213562373)) ;
#119555 = CARTESIAN_POINT('Origin',(7.9,3.00857864376269,-17.65)) ;
#119556 = CARTESIAN_POINT('Origin',(7.9,-2.15,-19.9531195934094)) ;
#119557 = CARTESIAN_POINT('Origin',(7.9,-2.32153024911032,-19.8502732340176)) ;
#119558 = CARTESIAN_POINT('Origin',(7.9,3.00857864376269,-17.65)) ;
#119559 = CARTESIAN_POINT('Origin',(7.9,2.45857864376269,-18.2)) ;
#119560 = CARTESIAN_POINT('Origin',(7.9,-3.65625,-19.05)) ;
#119561 = CARTESIAN_POINT('Origin',(7.9,-2.32153024911032,-18.2497267659824)) ;
#119562 = CARTESIAN_POINT('Origin',(7.9,2.6,-18.3414213562373)) ;
#119563 = CARTESIAN_POINT('Origin',(7.9,2.4,-18.3414213562373)) ;
#119564 = CARTESIAN_POINT('Origin',(7.9,-2.15,-18.1468804065906)) ;
#119565 = CARTESIAN_POINT('Origin',(7.9,-2.35,-18.1468804065906)) ;
#119566 = CARTESIAN_POINT('Origin',(7.9,2.4,-18.3414213562373)) ;
#119567 = CARTESIAN_POINT('Origin',(7.9,2.4,-18.45)) ;
#119568 = CARTESIAN_POINT('Origin',(7.9,-2.35,-17.5)) ;
#119569 = CARTESIAN_POINT('Origin',(7.9,-2.35,-17.5)) ;
#119570 = CARTESIAN_POINT('Origin',(7.9,2.4,-18.45)) ;
#119571 = CARTESIAN_POINT('Origin',(7.9,2.4,-18.45)) ;
#119572 = CARTESIAN_POINT('Origin',(7.9,-2.15,-17.5)) ;
#119573 = CARTESIAN_POINT('Origin',(7.9,-2.15,-17.3)) ;
#119574 = CARTESIAN_POINT('Origin',(7.9,2.4,-18.45)) ;
#119575 = CARTESIAN_POINT('Origin',(7.9,2.1,-18.45)) ;
#119576 = CARTESIAN_POINT('Origin',(7.9,1.9,-17.3)) ;
#119577 = CARTESIAN_POINT('Origin',(7.9,1.9,-17.3)) ;
#119578 = CARTESIAN_POINT('Origin',(7.9,2.1,-18.45)) ;
#119579 = CARTESIAN_POINT('Origin',(7.9,2.1,-18.45)) ;
#119580 = CARTESIAN_POINT('Origin',(7.9,1.9,-17.5)) ;
#119581 = CARTESIAN_POINT('Origin',(7.9,2.1,-17.5)) ;
#119582 = CARTESIAN_POINT('Origin',(7.9,2.1,-17.5)) ;
#119583 = CARTESIAN_POINT('Origin',(7.9,2.1,-15.84)) ;
#119584 = CARTESIAN_POINT('Origin',(7.9,2.4,-15.84)) ;
#119585 = CARTESIAN_POINT('Origin',(7.9,2.1,-15.84)) ;
#119586 = CARTESIAN_POINT('Origin',(7.9,2.4,-15.84)) ;
#119587 = CARTESIAN_POINT('Origin',(7.9,2.4,-15.84)) ;
#119588 = CARTESIAN_POINT('Origin',(7.9,2.1,-15.84)) ;
#119589 = CARTESIAN_POINT('Origin',(7.9,2.1,-15.84)) ;
#119590 = CARTESIAN_POINT('Origin',(7.9,2.4,-15.84)) ;
#119591 = CARTESIAN_POINT('Origin',(7.9,2.4,-15.9485786437627)) ;
#119592 = CARTESIAN_POINT('Origin',(7.9,2.1,-15.84)) ;
#119593 = CARTESIAN_POINT('Origin',(7.9,2.1,-16.79)) ;
#119594 = CARTESIAN_POINT('Origin',(7.9,2.6,-15.9485786437627)) ;
#119595 = CARTESIAN_POINT('Origin',(7.9,2.45857864376269,-16.09)) ;
#119596 = CARTESIAN_POINT('Origin',(7.9,1.9,-16.79)) ;
#119597 = CARTESIAN_POINT('Origin',(7.9,1.9,-16.99)) ;
#119598 = CARTESIAN_POINT('Origin',(7.9,2.45857864376269,-16.09)) ;
#119599 = CARTESIAN_POINT('Origin',(7.9,1.9,-16.99)) ;
#119600 = CARTESIAN_POINT('Origin',(7.9,-2.15,-16.99)) ;
#119601 = CARTESIAN_POINT('Origin',(7.9,-2.15,-16.79)) ;
#119602 = CARTESIAN_POINT('Origin',(7.9,-2.35,-16.79)) ;
#119603 = CARTESIAN_POINT('Origin',(7.9,3.35,-16.4985786437627)) ;
#119604 = CARTESIAN_POINT('Origin',(7.9,3.35,-13.9814213562373)) ;
#119605 = CARTESIAN_POINT('Origin',(7.9,-2.35,-16.1431195934094)) ;
#119606 = CARTESIAN_POINT('Origin',(7.9,-2.35,-16.1431195934094)) ;
#119607 = CARTESIAN_POINT('Origin',(7.9,3.15,-13.9814213562373)) ;
#119608 = CARTESIAN_POINT('Origin',(7.9,3.00857864376269,-13.84)) ;
#119609 = CARTESIAN_POINT('Origin',(7.9,-2.15,-16.1431195934094)) ;
#119610 = CARTESIAN_POINT('Origin',(7.9,-2.32153024911032,-16.0402732340176)) ;
#119611 = CARTESIAN_POINT('Origin',(7.9,3.00857864376269,-13.84)) ;
#119612 = CARTESIAN_POINT('Origin',(7.9,2.45857864376269,-14.39)) ;
#119613 = CARTESIAN_POINT('Origin',(7.9,-3.65625,-15.24)) ;
#119614 = CARTESIAN_POINT('Origin',(7.9,-2.32153024911032,-14.4397267659824)) ;
#119615 = CARTESIAN_POINT('Origin',(7.9,2.6,-14.5314213562373)) ;
#119616 = CARTESIAN_POINT('Origin',(7.9,2.4,-14.5314213562373)) ;
#119617 = CARTESIAN_POINT('Origin',(7.9,-2.15,-14.3368804065906)) ;
#119618 = CARTESIAN_POINT('Origin',(7.9,-2.35,-14.3368804065906)) ;
#119619 = CARTESIAN_POINT('Origin',(7.9,2.4,-14.5314213562373)) ;
#119620 = CARTESIAN_POINT('Origin',(7.9,2.4,-14.64)) ;
#119621 = CARTESIAN_POINT('Origin',(7.9,-2.35,-13.69)) ;
#119622 = CARTESIAN_POINT('Origin',(7.9,-2.35,-13.69)) ;
#119623 = CARTESIAN_POINT('Origin',(7.9,2.4,-14.64)) ;
#119624 = CARTESIAN_POINT('Origin',(7.9,2.4,-14.64)) ;
#119625 = CARTESIAN_POINT('Origin',(7.9,-2.15,-13.69)) ;
#119626 = CARTESIAN_POINT('Origin',(7.9,-2.15,-13.49)) ;
#119627 = CARTESIAN_POINT('Origin',(7.9,2.4,-14.64)) ;
#119628 = CARTESIAN_POINT('Origin',(7.9,2.1,-14.64)) ;
#119629 = CARTESIAN_POINT('Origin',(7.9,1.9,-13.49)) ;
#119630 = CARTESIAN_POINT('Origin',(7.9,1.9,-13.49)) ;
#119631 = CARTESIAN_POINT('Origin',(7.9,2.1,-14.64)) ;
#119632 = CARTESIAN_POINT('Origin',(7.9,2.1,-14.64)) ;
#119633 = CARTESIAN_POINT('Origin',(7.9,1.9,-13.69)) ;
#119634 = CARTESIAN_POINT('Origin',(7.9,2.1,-13.69)) ;
#119635 = CARTESIAN_POINT('Origin',(7.9,2.1,-13.69)) ;
#119636 = CARTESIAN_POINT('Origin',(7.9,2.1,-12.03)) ;
#119637 = CARTESIAN_POINT('Origin',(7.9,2.4,-12.03)) ;
#119638 = CARTESIAN_POINT('Origin',(7.9,2.1,-12.03)) ;
#119639 = CARTESIAN_POINT('Origin',(7.9,2.4,-12.03)) ;
#119640 = CARTESIAN_POINT('Origin',(7.9,2.4,-12.03)) ;
#119641 = CARTESIAN_POINT('Origin',(7.9,2.1,-12.03)) ;
#119642 = CARTESIAN_POINT('Origin',(7.9,2.1,-12.03)) ;
#119643 = CARTESIAN_POINT('Origin',(7.9,2.4,-12.03)) ;
#119644 = CARTESIAN_POINT('Origin',(7.9,2.4,-12.1385786437627)) ;
#119645 = CARTESIAN_POINT('Origin',(7.9,2.1,-12.03)) ;
#119646 = CARTESIAN_POINT('Origin',(7.9,2.1,-12.98)) ;
#119647 = CARTESIAN_POINT('Origin',(7.9,2.6,-12.1385786437627)) ;
#119648 = CARTESIAN_POINT('Origin',(7.9,2.45857864376269,-12.28)) ;
#119649 = CARTESIAN_POINT('Origin',(7.9,1.9,-12.98)) ;
#119650 = CARTESIAN_POINT('Origin',(7.9,1.9,-13.18)) ;
#119651 = CARTESIAN_POINT('Origin',(7.9,2.45857864376269,-12.28)) ;
#119652 = CARTESIAN_POINT('Origin',(7.9,1.9,-13.18)) ;
#119653 = CARTESIAN_POINT('Origin',(7.9,-2.15,-13.18)) ;
#119654 = CARTESIAN_POINT('Origin',(7.9,-2.15,-12.98)) ;
#119655 = CARTESIAN_POINT('Origin',(7.9,-2.35,-12.98)) ;
#119656 = CARTESIAN_POINT('Origin',(7.9,3.35,-12.6885786437627)) ;
#119657 = CARTESIAN_POINT('Origin',(7.9,3.35,-10.1714213562373)) ;
#119658 = CARTESIAN_POINT('Origin',(7.9,-2.35,-12.3331195934094)) ;
#119659 = CARTESIAN_POINT('Origin',(7.9,-2.35,-12.3331195934094)) ;
#119660 = CARTESIAN_POINT('Origin',(7.9,3.15,-10.1714213562373)) ;
#119661 = CARTESIAN_POINT('Origin',(7.9,3.00857864376269,-10.03)) ;
#119662 = CARTESIAN_POINT('Origin',(7.9,-2.15,-12.3331195934094)) ;
#119663 = CARTESIAN_POINT('Origin',(7.9,-2.32153024911032,-12.2302732340176)) ;
#119664 = CARTESIAN_POINT('Origin',(7.9,3.00857864376269,-10.03)) ;
#119665 = CARTESIAN_POINT('Origin',(7.9,2.45857864376269,-10.58)) ;
#119666 = CARTESIAN_POINT('Origin',(7.9,-3.65625,-11.43)) ;
#119667 = CARTESIAN_POINT('Origin',(7.9,-2.32153024911032,-10.6297267659824)) ;
#119668 = CARTESIAN_POINT('Origin',(7.9,2.6,-10.7214213562373)) ;
#119669 = CARTESIAN_POINT('Origin',(7.9,2.4,-10.7214213562373)) ;
#119670 = CARTESIAN_POINT('Origin',(7.9,-2.15,-10.5268804065906)) ;
#119671 = CARTESIAN_POINT('Origin',(7.9,-2.35,-10.5268804065906)) ;
#119672 = CARTESIAN_POINT('Origin',(7.9,2.4,-10.7214213562373)) ;
#119673 = CARTESIAN_POINT('Origin',(7.9,2.4,-10.83)) ;
#119674 = CARTESIAN_POINT('Origin',(7.9,-2.35,-9.88)) ;
#119675 = CARTESIAN_POINT('Origin',(7.9,-2.35,-9.88)) ;
#119676 = CARTESIAN_POINT('Origin',(7.9,2.4,-10.83)) ;
#119677 = CARTESIAN_POINT('Origin',(7.9,2.4,-10.83)) ;
#119678 = CARTESIAN_POINT('Origin',(7.9,-2.15,-9.88)) ;
#119679 = CARTESIAN_POINT('Origin',(7.9,-2.15,-9.68)) ;
#119680 = CARTESIAN_POINT('Origin',(7.9,2.4,-10.83)) ;
#119681 = CARTESIAN_POINT('Origin',(7.9,2.1,-10.83)) ;
#119682 = CARTESIAN_POINT('Origin',(7.9,1.9,-9.68)) ;
#119683 = CARTESIAN_POINT('Origin',(7.9,1.9,-9.68)) ;
#119684 = CARTESIAN_POINT('Origin',(7.9,2.1,-10.83)) ;
#119685 = CARTESIAN_POINT('Origin',(7.9,2.1,-10.83)) ;
#119686 = CARTESIAN_POINT('Origin',(7.9,1.9,-9.88)) ;
#119687 = CARTESIAN_POINT('Origin',(7.9,2.1,-9.88)) ;
#119688 = CARTESIAN_POINT('Origin',(7.9,2.1,-9.88)) ;
#119689 = CARTESIAN_POINT('Origin',(7.9,2.1,-8.22)) ;
#119690 = CARTESIAN_POINT('Origin',(7.9,2.4,-8.22)) ;
#119691 = CARTESIAN_POINT('Origin',(7.9,2.1,-8.22)) ;
#119692 = CARTESIAN_POINT('Origin',(7.9,2.4,-8.22)) ;
#119693 = CARTESIAN_POINT('Origin',(7.9,2.4,-8.22)) ;
#119694 = CARTESIAN_POINT('Origin',(7.9,2.1,-8.22)) ;
#119695 = CARTESIAN_POINT('Origin',(7.9,2.1,-8.22)) ;
#119696 = CARTESIAN_POINT('Origin',(7.9,2.4,-8.22)) ;
#119697 = CARTESIAN_POINT('Origin',(7.9,2.4,-8.32857864376269)) ;
#119698 = CARTESIAN_POINT('Origin',(7.9,2.1,-8.22)) ;
#119699 = CARTESIAN_POINT('Origin',(7.9,2.1,-9.17)) ;
#119700 = CARTESIAN_POINT('Origin',(7.9,2.6,-8.32857864376269)) ;
#119701 = CARTESIAN_POINT('Origin',(7.9,2.45857864376269,-8.47)) ;
#119702 = CARTESIAN_POINT('Origin',(7.9,1.9,-9.17)) ;
#119703 = CARTESIAN_POINT('Origin',(7.9,1.9,-9.37)) ;
#119704 = CARTESIAN_POINT('Origin',(7.9,2.45857864376269,-8.47)) ;
#119705 = CARTESIAN_POINT('Origin',(7.9,1.9,-9.37)) ;
#119706 = CARTESIAN_POINT('Origin',(7.9,-2.15,-9.37)) ;
#119707 = CARTESIAN_POINT('Origin',(7.9,-2.15,-9.17)) ;
#119708 = CARTESIAN_POINT('Origin',(7.9,-2.35,-9.17)) ;
#119709 = CARTESIAN_POINT('Origin',(7.9,3.35,-8.87857864376269)) ;
#119710 = CARTESIAN_POINT('Origin',(7.9,3.35,-6.36142135623731)) ;
#119711 = CARTESIAN_POINT('Origin',(7.9,-2.35,-8.52311959340942)) ;
#119712 = CARTESIAN_POINT('Origin',(7.9,-2.35,-8.52311959340942)) ;
#119713 = CARTESIAN_POINT('Origin',(7.9,3.15,-6.36142135623731)) ;
#119714 = CARTESIAN_POINT('Origin',(7.9,3.00857864376269,-6.22)) ;
#119715 = CARTESIAN_POINT('Origin',(7.9,-2.15,-8.52311959340942)) ;
#119716 = CARTESIAN_POINT('Origin',(7.9,-2.32153024911032,-8.4202732340176)) ;
#119717 = CARTESIAN_POINT('Origin',(7.9,3.00857864376269,-6.22)) ;
#119718 = CARTESIAN_POINT('Origin',(7.9,2.45857864376269,-6.77)) ;
#119719 = CARTESIAN_POINT('Origin',(7.9,-3.65625,-7.62)) ;
#119720 = CARTESIAN_POINT('Origin',(7.9,-2.32153024911032,-6.8197267659824)) ;
#119721 = CARTESIAN_POINT('Origin',(7.9,2.6,-6.91142135623731)) ;
#119722 = CARTESIAN_POINT('Origin',(7.9,2.4,-6.91142135623731)) ;
#119723 = CARTESIAN_POINT('Origin',(7.9,-2.15,-6.71688040659058)) ;
#119724 = CARTESIAN_POINT('Origin',(7.9,-2.35,-6.71688040659058)) ;
#119725 = CARTESIAN_POINT('Origin',(7.9,2.4,-6.91142135623731)) ;
#119726 = CARTESIAN_POINT('Origin',(7.9,2.4,-7.02)) ;
#119727 = CARTESIAN_POINT('Origin',(7.9,-2.35,-6.07)) ;
#119728 = CARTESIAN_POINT('Origin',(7.9,-2.35,-6.07)) ;
#119729 = CARTESIAN_POINT('Origin',(7.9,2.4,-7.02)) ;
#119730 = CARTESIAN_POINT('Origin',(7.9,2.4,-7.02)) ;
#119731 = CARTESIAN_POINT('Origin',(7.9,-2.15,-6.07)) ;
#119732 = CARTESIAN_POINT('Origin',(7.9,-2.15,-5.87)) ;
#119733 = CARTESIAN_POINT('Origin',(7.9,2.4,-7.02)) ;
#119734 = CARTESIAN_POINT('Origin',(7.9,2.1,-7.02)) ;
#119735 = CARTESIAN_POINT('Origin',(7.9,1.9,-5.87)) ;
#119736 = CARTESIAN_POINT('Origin',(7.9,1.9,-5.87)) ;
#119737 = CARTESIAN_POINT('Origin',(7.9,2.1,-7.02)) ;
#119738 = CARTESIAN_POINT('Origin',(7.9,2.1,-7.02)) ;
#119739 = CARTESIAN_POINT('Origin',(7.9,1.9,-6.07)) ;
#119740 = CARTESIAN_POINT('Origin',(7.9,2.1,-6.07)) ;
#119741 = CARTESIAN_POINT('Origin',(7.9,2.1,-6.07)) ;
#119742 = CARTESIAN_POINT('Origin',(7.9,2.1,-4.41)) ;
#119743 = CARTESIAN_POINT('Origin',(7.9,2.4,-4.41)) ;
#119744 = CARTESIAN_POINT('Origin',(7.9,2.1,-4.41)) ;
#119745 = CARTESIAN_POINT('Origin',(7.9,2.4,-4.41)) ;
#119746 = CARTESIAN_POINT('Origin',(7.9,2.4,-4.41)) ;
#119747 = CARTESIAN_POINT('Origin',(7.9,2.1,-4.41)) ;
#119748 = CARTESIAN_POINT('Origin',(7.9,2.1,-4.41)) ;
#119749 = CARTESIAN_POINT('Origin',(7.9,2.4,-4.41)) ;
#119750 = CARTESIAN_POINT('Origin',(7.9,2.4,-4.51857864376269)) ;
#119751 = CARTESIAN_POINT('Origin',(7.9,2.1,-4.41)) ;
#119752 = CARTESIAN_POINT('Origin',(7.9,2.1,-5.36)) ;
#119753 = CARTESIAN_POINT('Origin',(7.9,2.6,-4.51857864376269)) ;
#119754 = CARTESIAN_POINT('Origin',(7.9,2.45857864376269,-4.66)) ;
#119755 = CARTESIAN_POINT('Origin',(7.9,1.9,-5.36)) ;
#119756 = CARTESIAN_POINT('Origin',(7.9,1.9,-5.56)) ;
#119757 = CARTESIAN_POINT('Origin',(7.9,2.45857864376269,-4.66)) ;
#119758 = CARTESIAN_POINT('Origin',(7.9,1.9,-5.56)) ;
#119759 = CARTESIAN_POINT('Origin',(7.9,-2.15,-5.56)) ;
#119760 = CARTESIAN_POINT('Origin',(7.9,-2.15,-5.36)) ;
#119761 = CARTESIAN_POINT('Origin',(7.9,-2.35,-5.36)) ;
#119762 = CARTESIAN_POINT('Origin',(7.9,3.35,-5.06857864376269)) ;
#119763 = CARTESIAN_POINT('Origin',(7.9,3.35,-2.55142135623731)) ;
#119764 = CARTESIAN_POINT('Origin',(7.9,-2.35,-4.71311959340942)) ;
#119765 = CARTESIAN_POINT('Origin',(7.9,-2.35,-4.71311959340942)) ;
#119766 = CARTESIAN_POINT('Origin',(7.9,3.15,-2.55142135623731)) ;
#119767 = CARTESIAN_POINT('Origin',(7.9,3.00857864376269,-2.41)) ;
#119768 = CARTESIAN_POINT('Origin',(7.9,-2.15,-4.71311959340942)) ;
#119769 = CARTESIAN_POINT('Origin',(7.9,-2.32153024911032,-4.6102732340176)) ;
#119770 = CARTESIAN_POINT('Origin',(7.9,3.00857864376269,-2.41)) ;
#119771 = CARTESIAN_POINT('Origin',(7.9,2.45857864376269,-2.96)) ;
#119772 = CARTESIAN_POINT('Origin',(7.9,-3.65625,-3.81)) ;
#119773 = CARTESIAN_POINT('Origin',(7.9,-2.32153024911032,-3.0097267659824)) ;
#119774 = CARTESIAN_POINT('Origin',(7.9,2.6,-3.10142135623731)) ;
#119775 = CARTESIAN_POINT('Origin',(7.9,2.4,-3.10142135623731)) ;
#119776 = CARTESIAN_POINT('Origin',(7.9,-2.15,-2.90688040659058)) ;
#119777 = CARTESIAN_POINT('Origin',(7.9,-2.35,-2.90688040659058)) ;
#119778 = CARTESIAN_POINT('Origin',(7.9,2.4,-3.10142135623731)) ;
#119779 = CARTESIAN_POINT('Origin',(7.9,2.4,-3.21)) ;
#119780 = CARTESIAN_POINT('Origin',(7.9,-2.35,-2.26)) ;
#119781 = CARTESIAN_POINT('Origin',(7.9,-2.35,-2.26)) ;
#119782 = CARTESIAN_POINT('Origin',(7.9,2.4,-3.21)) ;
#119783 = CARTESIAN_POINT('Origin',(7.9,2.4,-3.21)) ;
#119784 = CARTESIAN_POINT('Origin',(7.9,-2.15,-2.26)) ;
#119785 = CARTESIAN_POINT('Origin',(7.9,-2.15,-2.06)) ;
#119786 = CARTESIAN_POINT('Origin',(7.9,2.4,-3.21)) ;
#119787 = CARTESIAN_POINT('Origin',(7.9,2.1,-3.21)) ;
#119788 = CARTESIAN_POINT('Origin',(7.9,1.9,-2.06)) ;
#119789 = CARTESIAN_POINT('Origin',(7.9,1.9,-2.06)) ;
#119790 = CARTESIAN_POINT('Origin',(7.9,2.1,-3.21)) ;
#119791 = CARTESIAN_POINT('Origin',(7.9,2.1,-3.21)) ;
#119792 = CARTESIAN_POINT('Origin',(7.9,1.9,-2.26)) ;
#119793 = CARTESIAN_POINT('Origin',(7.9,2.1,-2.26)) ;
#119794 = CARTESIAN_POINT('Origin',(7.9,2.1,-2.26)) ;
#119795 = CARTESIAN_POINT('Origin',(-0.899999999999999,-2.,-7.02)) ;
#119796 = CARTESIAN_POINT('Origin',(-0.899999999999999,0.4,-7.02)) ;
#119797 = CARTESIAN_POINT('Origin',(-0.899999999999999,-1.9,-7.02)) ;
#119798 = CARTESIAN_POINT('Origin',(0.600000000000001,0.4,-7.22)) ;
#119799 = CARTESIAN_POINT('Origin',(0.500000000000001,0.4,-7.22)) ;
#119800 = CARTESIAN_POINT('Origin',(-0.899999999999999,0.4,-7.22)) ;
#119801 = CARTESIAN_POINT('Origin',(0.500000000000001,0.4,-7.22)) ;
#119802 = CARTESIAN_POINT('',(0.600000000000001,0.4,-7.22)) ;
#119803 = CARTESIAN_POINT('Origin',(0.500000000000001,0.4,-7.22)) ;
#119804 = CARTESIAN_POINT('Origin',(0.500000000000001,0.4,-7.22)) ;
#119805 = CARTESIAN_POINT('Origin',(-0.899999999999999,-1.9,-7.02)) ;
#119806 = CARTESIAN_POINT('Origin',(-0.899999999999999,-1.9,-7.02)) ;
#119807 = CARTESIAN_POINT('Origin',(-0.899999999999999,-1.9,-7.02)) ;
#119808 = CARTESIAN_POINT('Origin',(-0.899999999999999,0.4,-7.22)) ;
#119809 = CARTESIAN_POINT('Origin',(-0.899999999999999,0.6,-7.22)) ;
#119810 = CARTESIAN_POINT('Origin',(0.500000000000001,0.4,-7.62)) ;
#119811 = CARTESIAN_POINT('Origin',(0.500000000000001,0.4,-8.02)) ;
#119812 = CARTESIAN_POINT('',(0.600000000000001,0.4,-7.92)) ;
#119813 = CARTESIAN_POINT('Ctrl Pts',(0.595612997216081,0.370705721320404,
-7.9907057213204)) ;
#119814 = CARTESIAN_POINT('Ctrl Pts',(0.596180587760891,0.372558268494353,
-7.98885549883217)) ;
#119815 = CARTESIAN_POINT('Ctrl Pts',(0.596672461925684,0.374355839771976,
-7.98691417986632)) ;
#119816 = CARTESIAN_POINT('Ctrl Pts',(0.599015141889213,0.383869350930064,
-7.97576499365627)) ;
#119817 = CARTESIAN_POINT('Ctrl Pts',(0.599609996542524,0.390224332900447,
-7.96497260265412)) ;
#119818 = CARTESIAN_POINT('Ctrl Pts',(0.600050586298725,0.398117439141558,
-7.94233105320469)) ;
#119819 = CARTESIAN_POINT('Ctrl Pts',(0.600000000000001,0.399999999999999,
-7.93120125063353)) ;
#119820 = CARTESIAN_POINT('Ctrl Pts',(0.600000000000001,0.399999999999999,
-7.92)) ;
#119821 = CARTESIAN_POINT('',(0.600000000000001,0.4,-7.62)) ;
#119822 = CARTESIAN_POINT('Origin',(0.500000000000001,-4.5664044441154E-17,
-7.22)) ;
#119823 = CARTESIAN_POINT('',(0.500000000000001,0.394987437106619,-7.32)) ;
#119824 = CARTESIAN_POINT('Ctrl Pts',(0.500000000000001,0.394987437106619,
-7.32)) ;
#119825 = CARTESIAN_POINT('Ctrl Pts',(0.505940567948952,0.3955844866499,-7.32)) ;
#119826 = CARTESIAN_POINT('Ctrl Pts',(0.51193197101914,0.396132036079018,
-7.31946630032796)) ;
#119827 = CARTESIAN_POINT('Ctrl Pts',(0.517829015308548,0.396618246075354,
-7.31839779577372)) ;
#119828 = CARTESIAN_POINT('Ctrl Pts',(0.522982218721201,0.397043126556053,
-7.31746407015711)) ;
#119829 = CARTESIAN_POINT('Ctrl Pts',(0.52806264897023,0.397421319341388,
-7.31612282679706)) ;
#119830 = CARTESIAN_POINT('Ctrl Pts',(0.532978106724,0.397751505046071,-7.31440574387663)) ;
#119831 = CARTESIAN_POINT('Ctrl Pts',(0.538583536338966,0.398128038182999,
-7.31244763784955)) ;
#119832 = CARTESIAN_POINT('Ctrl Pts',(0.544059405914893,0.398447721828296,
-7.30997000831105)) ;
#119833 = CARTESIAN_POINT('Ctrl Pts',(0.549268572255785,0.398712331108984,
-7.30702073194289)) ;
#119834 = CARTESIAN_POINT('Ctrl Pts',(0.553856850427149,0.398945401221756,
-7.30442298414684)) ;
#119835 = CARTESIAN_POINT('Ctrl Pts',(0.558237825069329,0.399135987683843,
-7.30146038497999)) ;
#119836 = CARTESIAN_POINT('Ctrl Pts',(0.562333836086214,0.399290378266507,
-7.29819522286417)) ;
#119837 = CARTESIAN_POINT('Ctrl Pts',(0.566990328957901,0.399465895042381,
-7.2944832689523)) ;
#119838 = CARTESIAN_POINT('Ctrl Pts',(0.571349096493437,0.399597278936107,
-7.29032280648479)) ;
#119839 = CARTESIAN_POINT('Ctrl Pts',(0.57529692005673,0.399694832180838,
-7.28580557597932)) ;
#119840 = CARTESIAN_POINT('Ctrl Pts',(0.578744263667919,0.399780018245914,
-7.28186101121506)) ;
#119841 = CARTESIAN_POINT('Ctrl Pts',(0.581878314560434,0.399839626289636,
-7.2776455218421)) ;
#119842 = CARTESIAN_POINT('Ctrl Pts',(0.584648147334856,0.399882153365958,
-7.27324181770729)) ;
#119843 = CARTESIAN_POINT('Ctrl Pts',(0.587839270208173,0.399931148788079,
-7.2681683125045)) ;
#119844 = CARTESIAN_POINT('Ctrl Pts',(0.590595054415089,0.399958289583404,
-7.26276663624446)) ;
#119845 = CARTESIAN_POINT('Ctrl Pts',(0.5928386189431,0.399974357003159,-7.2571616850094)) ;
#119846 = CARTESIAN_POINT('Ctrl Pts',(0.594777336851653,0.399988241245861,
-7.2523183122424)) ;
#119847 = CARTESIAN_POINT('Ctrl Pts',(0.596334051506188,0.399993946552814,
-7.24732416622713)) ;
#119848 = CARTESIAN_POINT('Ctrl Pts',(0.597488309822308,0.39999684570125,
-7.24227171856839)) ;
#119849 = CARTESIAN_POINT('Ctrl Pts',(0.598804024094406,0.400000150378306,
-7.23651254196053)) ;
#119850 = CARTESIAN_POINT('Ctrl Pts',(0.599612685195437,0.399999963509465,
-7.23060284389055)) ;
#119851 = CARTESIAN_POINT('Ctrl Pts',(0.599890230999724,0.399999993975383,
-7.224684202261)) ;
#119852 = CARTESIAN_POINT('Ctrl Pts',(0.599963464549401,0.400000002014155,
-7.22312250278977)) ;
#119853 = CARTESIAN_POINT('Ctrl Pts',(0.600000000000001,0.399999999999999,
-7.22156022150916)) ;
#119854 = CARTESIAN_POINT('Ctrl Pts',(0.600000000000001,0.399999999999999,
-7.22)) ;
#119855 = CARTESIAN_POINT('',(0.600000000000001,0.299999999999999,-7.22)) ;
#119856 = CARTESIAN_POINT('Ctrl Pts',(0.500000000000001,0.394987437106619,
-7.32)) ;
#119857 = CARTESIAN_POINT('Ctrl Pts',(0.500454935589846,0.395033159853749,
-7.32)) ;
#119858 = CARTESIAN_POINT('Ctrl Pts',(0.500909898680472,0.39507857032906,
-7.31999689549112)) ;
#119859 = CARTESIAN_POINT('Ctrl Pts',(0.502892456245169,0.39527507588909,
-7.31996983394194)) ;
#119860 = CARTESIAN_POINT('Ctrl Pts',(0.504418747482366,0.395422812032198,
-7.31991398542099)) ;
#119861 = CARTESIAN_POINT('Ctrl Pts',(0.508462199543345,0.395804395682033,
-7.31967328105664)) ;
#119862 = CARTESIAN_POINT('Ctrl Pts',(0.510974953343295,0.396031485023317,
-7.31942793914506)) ;
#119863 = CARTESIAN_POINT('Ctrl Pts',(0.521160739721272,0.396903453186235,
-7.31804279449156)) ;
#119864 = CARTESIAN_POINT('Ctrl Pts',(0.528708678528402,0.397444933153161,
-7.31610421770469)) ;
#119865 = CARTESIAN_POINT('Ctrl Pts',(0.545943206358073,0.398105551684108,
-7.30946463945115)) ;
#119866 = CARTESIAN_POINT('Ctrl Pts',(0.555229535466813,0.397987646678431,
-7.30403535883597)) ;
#119867 = CARTESIAN_POINT('Ctrl Pts',(0.571394604995744,0.395490482808038,
-7.29077551336386)) ;
#119868 = CARTESIAN_POINT('Ctrl Pts',(0.578055313702842,0.39319894869835,
-7.28324074563176)) ;
#119869 = CARTESIAN_POINT('Ctrl Pts',(0.588559132202514,0.385442756729305,
-7.26739223398403)) ;
#119870 = CARTESIAN_POINT('Ctrl Pts',(0.592167355639978,0.380240075126892,
-7.2595482656068)) ;
#119871 = CARTESIAN_POINT('Ctrl Pts',(0.597496615531108,0.365892753466966,
-7.24392552179528)) ;
#119872 = CARTESIAN_POINT('Ctrl Pts',(0.598734255154202,0.356660564300668,
-7.23677274172691)) ;
#119873 = CARTESIAN_POINT('Ctrl Pts',(0.600012754681688,0.335223914398549,
-7.22558230586562)) ;
#119874 = CARTESIAN_POINT('Ctrl Pts',(0.59999390055981,0.322655037091896,
-7.22166151936558)) ;
#119875 = CARTESIAN_POINT('Ctrl Pts',(0.600000296204999,0.30610691358235,
-7.22013962634704)) ;
#119876 = CARTESIAN_POINT('Ctrl Pts',(0.600000000000001,0.303050992413436,
-7.22)) ;
#119877 = CARTESIAN_POINT('Ctrl Pts',(0.600000000000001,0.299999999999999,
-7.22)) ;
#119878 = CARTESIAN_POINT('',(0.600000000000001,-2.39800009914439E-17,-7.22)) ;
#119879 = CARTESIAN_POINT('Origin',(0.500000000000001,-1.9,-7.22)) ;
#119880 = CARTESIAN_POINT('Origin',(0.600000000000001,-1.9,-7.02)) ;
#119881 = CARTESIAN_POINT('Origin',(0.500000000000001,-1.9,-7.02)) ;
#119882 = CARTESIAN_POINT('Origin',(-0.899999999999999,-1.9,-6.245)) ;
#119883 = CARTESIAN_POINT('Origin',(-0.899999999999999,-1.9,-6.345)) ;
#119884 = CARTESIAN_POINT('Origin',(-0.899999999999999,0.6,-7.12)) ;
#119885 = CARTESIAN_POINT('Origin',(-0.899999999999999,0.6,-8.02)) ;
#119886 = CARTESIAN_POINT('Origin',(0.600000000000001,0.4,-8.02)) ;
#119887 = CARTESIAN_POINT('Origin',(0.500000000000001,0.4,-8.02)) ;
#119888 = CARTESIAN_POINT('Origin',(-0.899999999999999,0.4,-8.02)) ;
#119889 = CARTESIAN_POINT('Origin',(0.500000000000001,0.4,-8.02)) ;
#119890 = CARTESIAN_POINT('Origin',(0.500000000000001,-1.9,-7.02)) ;
#119891 = CARTESIAN_POINT('Origin',(0.500000000000001,-2.1,-7.02)) ;
#119892 = CARTESIAN_POINT('Origin',(-0.899999999999999,-1.9,-6.345)) ;
#119893 = CARTESIAN_POINT('Origin',(-1.1,-1.9,-6.345)) ;
#119894 = CARTESIAN_POINT('Origin',(-0.899999999999999,-2.1,-6.345)) ;
#119895 = CARTESIAN_POINT('Origin',(-0.899999999999999,0.4,-8.02)) ;
#119896 = CARTESIAN_POINT('Origin',(-0.899999999999999,0.4,-8.22)) ;
#119897 = CARTESIAN_POINT('Origin',(0.500000000000001,-2.1,-7.62)) ;
#119898 = CARTESIAN_POINT('Origin',(0.500000000000001,-2.1,-6.345)) ;
#119899 = CARTESIAN_POINT('Origin',(0.600000000000001,-2.1,-6.345)) ;
#119900 = CARTESIAN_POINT('Origin',(0.500000000000001,-2.1,-6.345)) ;
#119901 = CARTESIAN_POINT('Origin',(-1.1,-4.42727195005761E-17,-6.345)) ;
#119902 = CARTESIAN_POINT('',(-1.1,1.15,-6.245)) ;
#119903 = CARTESIAN_POINT('',(-1.1,1.25,-6.245)) ;
#119904 = CARTESIAN_POINT('Origin',(-1.1,1.15,-6.345)) ;
#119905 = CARTESIAN_POINT('Origin',(-0.899999999999999,0.5,-8.22)) ;
#119906 = CARTESIAN_POINT('Origin',(-0.899999999999999,-1.9,-8.22)) ;
#119907 = CARTESIAN_POINT('Origin',(0.600000000000001,-1.9,-8.22)) ;
#119908 = CARTESIAN_POINT('Origin',(0.500000000000001,-1.9,-8.22)) ;
#119909 = CARTESIAN_POINT('Origin',(-0.899999999999999,-1.9,-8.22)) ;
#119910 = CARTESIAN_POINT('Origin',(0.500000000000001,-1.9,-8.22)) ;
#119911 = CARTESIAN_POINT('Origin',(0.500000000000001,-2.1,-8.22)) ;
#119912 = CARTESIAN_POINT('Origin',(0.500000000000001,-2.1,-6.345)) ;
#119913 = CARTESIAN_POINT('Origin',(0.500000000000001,-2.1,-6.345)) ;
#119914 = CARTESIAN_POINT('Origin',(-1.1,-2.9,-6.145)) ;
#119915 = CARTESIAN_POINT('Origin',(-1.1,-2.9,-6.145)) ;
#119916 = CARTESIAN_POINT('Origin',(-1.1,-2.9,-6.145)) ;
#119917 = CARTESIAN_POINT('Origin',(-1.1,1.25,-6.145)) ;
#119918 = CARTESIAN_POINT('Origin',(-1.1,1.15,-6.145)) ;
#119919 = CARTESIAN_POINT('Origin',(-1.1,1.15,-6.345)) ;
#119920 = CARTESIAN_POINT('',(-1.1,1.25,-6.345)) ;
#119921 = CARTESIAN_POINT('Origin',(-1.1,1.15,-6.345)) ;
#119922 = CARTESIAN_POINT('Origin',(-1.1,1.15,-6.345)) ;
#119923 = CARTESIAN_POINT('Origin',(-0.899999999999999,-1.9,-8.22)) ;
#119924 = CARTESIAN_POINT('Origin',(-0.899999999999999,-1.9,-8.22)) ;
#119925 = CARTESIAN_POINT('Origin',(0.500000000000001,-2.1,-7.62)) ;
#119926 = CARTESIAN_POINT('Origin',(0.500000000000001,-2.1,-8.895)) ;
#119927 = CARTESIAN_POINT('Origin',(0.500000000000001,1.36481920536411E-16,
-6.345)) ;
#119928 = CARTESIAN_POINT('Origin',(0.500000000000001,-2.9,-6.345)) ;
#119929 = CARTESIAN_POINT('Origin',(-0.999999999999999,-2.9,-6.145)) ;
#119930 = CARTESIAN_POINT('Origin',(0.500000000000001,-2.9,-6.145)) ;
#119931 = CARTESIAN_POINT('Origin',(-1.1,1.15,-6.345)) ;
#119932 = CARTESIAN_POINT('Origin',(-1.1,1.35,-6.345)) ;
#119933 = CARTESIAN_POINT('Origin',(-1.1,1.15,-7.62)) ;
#119934 = CARTESIAN_POINT('',(-1.1,1.25,-8.895)) ;
#119935 = CARTESIAN_POINT('',(-1.1,1.25,-8.995)) ;
#119936 = CARTESIAN_POINT('Origin',(-1.1,1.15,-8.895)) ;
#119937 = CARTESIAN_POINT('Origin',(-0.899999999999999,-1.9,-8.12)) ;
#119938 = CARTESIAN_POINT('Origin',(-0.899999999999999,-1.9,-8.895)) ;
#119939 = CARTESIAN_POINT('Origin',(-0.999999999999999,-2.1,-8.895)) ;
#119940 = CARTESIAN_POINT('Origin',(0.500000000000001,-2.1,-8.895)) ;
#119941 = CARTESIAN_POINT('Origin',(-0.899999999999999,-2.1,-8.895)) ;
#119942 = CARTESIAN_POINT('Origin',(0.500000000000001,-2.1,-8.895)) ;
#119943 = CARTESIAN_POINT('Origin',(0.500000000000001,-2.1,-8.895)) ;
#119944 = CARTESIAN_POINT('Origin',(0.500000000000001,-2.9,-6.345)) ;
#119945 = CARTESIAN_POINT('Origin',(0.700000000000002,-2.9,-6.345)) ;
#119946 = CARTESIAN_POINT('Origin',(-1.1,1.35,-8.995)) ;
#119947 = CARTESIAN_POINT('Origin',(-1.1,1.35,-8.895)) ;
#119948 = CARTESIAN_POINT('Origin',(-1.1,1.15,-8.895)) ;
#119949 = CARTESIAN_POINT('',(-1.1,1.15,-8.995)) ;
#119950 = CARTESIAN_POINT('Origin',(-1.1,1.15,-8.895)) ;
#119951 = CARTESIAN_POINT('Origin',(-1.1,1.15,-8.895)) ;
#119952 = CARTESIAN_POINT('Origin',(-0.899999999999999,-1.9,-8.895)) ;
#119953 = CARTESIAN_POINT('Origin',(-1.1,-1.9,-8.895)) ;
#119954 = CARTESIAN_POINT('Origin',(0.500000000000001,-5.86744705109802E-17,
-8.895)) ;
#119955 = CARTESIAN_POINT('Origin',(0.500000000000001,-2.9,-8.895)) ;
#119956 = CARTESIAN_POINT('Origin',(0.700000000000002,-2.9,-7.62)) ;
#119957 = CARTESIAN_POINT('Origin',(0.700000000000002,-2.9,-8.895)) ;
#119958 = CARTESIAN_POINT('Origin',(-1.1,1.15,-8.895)) ;
#119959 = CARTESIAN_POINT('Origin',(-1.1,1.15,-9.095)) ;
#119960 = CARTESIAN_POINT('Origin',(-1.1,-2.39429110547967E-16,-8.895)) ;
#119961 = CARTESIAN_POINT('',(-1.1,1.25,-8.995)) ;
#119962 = CARTESIAN_POINT('Origin',(0.500000000000001,-2.9,-8.895)) ;
#119963 = CARTESIAN_POINT('Origin',(0.500000000000001,-2.9,-9.095)) ;
#119964 = CARTESIAN_POINT('Origin',(-1.1,1.25,-9.095)) ;
#119965 = CARTESIAN_POINT('Origin',(-1.1,-2.9,-9.095)) ;
#119966 = CARTESIAN_POINT('Origin',(-1.1,-2.9,-9.095)) ;
#119967 = CARTESIAN_POINT('Origin',(-1.1,-2.9,-9.095)) ;
#119968 = CARTESIAN_POINT('Origin',(-1.1,-2.9,-9.095)) ;
#119969 = CARTESIAN_POINT('Origin',(1.5,1.9,-7.02)) ;
#119970 = CARTESIAN_POINT('Origin',(1.5,1.9,-9.17)) ;
#119971 = CARTESIAN_POINT('Origin',(1.5,1.9,-8.22)) ;
#119972 = CARTESIAN_POINT('Origin',(1.5,2.1,-8.22)) ;
#119973 = CARTESIAN_POINT('Origin',(1.5,2.1,-8.02)) ;
#119974 = CARTESIAN_POINT('Origin',(1.5,1.9,-9.17)) ;
#119975 = CARTESIAN_POINT('Origin',(1.5,1.9,-9.17)) ;
#119976 = CARTESIAN_POINT('Origin',(1.5,2.1,-8.02)) ;
#119977 = CARTESIAN_POINT('Origin',(1.5,2.4,-8.02)) ;
#119978 = CARTESIAN_POINT('Origin',(1.5,2.1,-9.17)) ;
#119979 = CARTESIAN_POINT('Origin',(1.5,-2.15,-9.17)) ;
#119980 = CARTESIAN_POINT('Origin',(1.5,2.4,-8.22)) ;
#119981 = CARTESIAN_POINT('Origin',(1.5,2.6,-8.22)) ;
#119982 = CARTESIAN_POINT('Origin',(1.5,-2.15,-9.17)) ;
#119983 = CARTESIAN_POINT('Origin',(1.5,-2.15,-9.17)) ;
#119984 = CARTESIAN_POINT('Origin',(1.5,2.6,-7.02)) ;
#119985 = CARTESIAN_POINT('Origin',(1.5,2.6,-8.32857864376269)) ;
#119986 = CARTESIAN_POINT('Origin',(1.5,-2.15,-7.02)) ;
#119987 = CARTESIAN_POINT('Origin',(1.5,-2.15,-8.52311959340942)) ;
#119988 = CARTESIAN_POINT('Origin',(1.5,2.6,-8.32857864376269)) ;
#119989 = CARTESIAN_POINT('Origin',(1.5,2.6,-8.32857864376269)) ;
#119990 = CARTESIAN_POINT('Origin',(1.5,-2.15,-8.52311959340942)) ;
#119991 = CARTESIAN_POINT('Origin',(1.5,-2.15,-8.52311959340942)) ;
#119992 = CARTESIAN_POINT('Origin',(1.5,1.69571067811865,-7.42428932188135)) ;
#119993 = CARTESIAN_POINT('Origin',(1.5,3.15,-8.87857864376269)) ;
#119994 = CARTESIAN_POINT('Origin',(1.5,-3.65625,-7.62)) ;
#119995 = CARTESIAN_POINT('Origin',(1.5,-2.15,-6.71688040659058)) ;
#119996 = CARTESIAN_POINT('Origin',(1.5,3.15,-8.87857864376269)) ;
#119997 = CARTESIAN_POINT('Origin',(1.5,3.15,-8.87857864376269)) ;
#119998 = CARTESIAN_POINT('Origin',(1.5,-2.15,-6.71688040659058)) ;
#119999 = CARTESIAN_POINT('Origin',(1.5,-2.15,-6.71688040659058)) ;
#120000 = CARTESIAN_POINT('Origin',(1.5,3.15,-7.02)) ;
#120001 = CARTESIAN_POINT('Origin',(1.5,-2.15,-7.02)) ;
#120002 = CARTESIAN_POINT('Origin',(1.5,-2.15,-6.07)) ;
#120003 = CARTESIAN_POINT('Origin',(1.5,-2.15,-6.07)) ;
#120004 = CARTESIAN_POINT('Origin',(1.5,-2.15,-6.07)) ;
#120005 = CARTESIAN_POINT('Origin',(1.5,2.29571067811866,-7.21571067811866)) ;
#120006 = CARTESIAN_POINT('Origin',(1.5,2.6,-6.91142135623731)) ;
#120007 = CARTESIAN_POINT('Origin',(1.5,2.1,-6.07)) ;
#120008 = CARTESIAN_POINT('Origin',(1.5,1.9,-6.07)) ;
#120009 = CARTESIAN_POINT('Origin',(1.5,2.6,-6.91142135623731)) ;
#120010 = CARTESIAN_POINT('Origin',(1.5,2.6,-6.91142135623731)) ;
#120011 = CARTESIAN_POINT('Origin',(1.5,1.9,-6.07)) ;
#120012 = CARTESIAN_POINT('Origin',(1.5,1.9,-6.07)) ;
#120013 = CARTESIAN_POINT('Origin',(1.5,2.6,-7.02)) ;
#120014 = CARTESIAN_POINT('Origin',(1.5,2.6,-7.02)) ;
#120015 = CARTESIAN_POINT('Origin',(1.5,1.9,-7.02)) ;
#120016 = CARTESIAN_POINT('Origin',(1.5,1.9,-7.02)) ;
#120017 = CARTESIAN_POINT('Origin',(1.5,2.4,-7.02)) ;
#120018 = CARTESIAN_POINT('Origin',(1.5,2.4,-7.22)) ;
#120019 = CARTESIAN_POINT('Origin',(1.5,2.1,-7.02)) ;
#120020 = CARTESIAN_POINT('Origin',(1.5,2.1,-7.22)) ;
#120021 = CARTESIAN_POINT('Origin',(1.5,2.1,-7.22)) ;
#120022 = CARTESIAN_POINT('Origin',(-0.899999999999999,-2.,-10.83)) ;
#120023 = CARTESIAN_POINT('Origin',(-0.899999999999999,0.4,-10.83)) ;
#120024 = CARTESIAN_POINT('Origin',(-0.899999999999999,-1.9,-10.83)) ;
#120025 = CARTESIAN_POINT('Origin',(0.600000000000001,0.4,-11.03)) ;
#120026 = CARTESIAN_POINT('Origin',(0.500000000000001,0.4,-11.03)) ;
#120027 = CARTESIAN_POINT('Origin',(-0.899999999999999,0.4,-11.03)) ;
#120028 = CARTESIAN_POINT('Origin',(0.500000000000001,0.4,-11.03)) ;
#120029 = CARTESIAN_POINT('',(0.600000000000001,0.4,-11.03)) ;
#120030 = CARTESIAN_POINT('Origin',(0.500000000000001,0.4,-11.03)) ;
#120031 = CARTESIAN_POINT('Origin',(0.500000000000001,0.4,-11.03)) ;
#120032 = CARTESIAN_POINT('Origin',(-0.899999999999999,-1.9,-10.83)) ;
#120033 = CARTESIAN_POINT('Origin',(-0.899999999999999,-1.9,-10.83)) ;
#120034 = CARTESIAN_POINT('Origin',(-0.899999999999999,-1.9,-10.83)) ;
#120035 = CARTESIAN_POINT('Origin',(-0.899999999999999,0.4,-11.03)) ;
#120036 = CARTESIAN_POINT('Origin',(-0.899999999999999,0.6,-11.03)) ;
#120037 = CARTESIAN_POINT('Origin',(0.500000000000001,0.4,-11.43)) ;
#120038 = CARTESIAN_POINT('Origin',(0.500000000000001,0.4,-11.83)) ;
#120039 = CARTESIAN_POINT('',(0.600000000000001,0.4,-11.73)) ;
#120040 = CARTESIAN_POINT('Ctrl Pts',(0.595612997216082,0.370705721320405,
-11.8007057213204)) ;
#120041 = CARTESIAN_POINT('Ctrl Pts',(0.596180587760892,0.372558268494355,
-11.7988554988322)) ;
#120042 = CARTESIAN_POINT('Ctrl Pts',(0.596672461925685,0.374355839771978,
-11.7969141798663)) ;
#120043 = CARTESIAN_POINT('Ctrl Pts',(0.599015141889211,0.383869350930053,
-11.7857649936563)) ;
#120044 = CARTESIAN_POINT('Ctrl Pts',(0.599609996542523,0.390224332900442,
-11.7749726026541)) ;
#120045 = CARTESIAN_POINT('Ctrl Pts',(0.600050586298725,0.398117439141559,
-11.7523310532047)) ;
#120046 = CARTESIAN_POINT('Ctrl Pts',(0.600000000000001,0.399999999999999,
-11.7412012506335)) ;
#120047 = CARTESIAN_POINT('Ctrl Pts',(0.600000000000001,0.399999999999999,
-11.73)) ;
#120048 = CARTESIAN_POINT('',(0.600000000000001,0.4,-11.43)) ;
#120049 = CARTESIAN_POINT('Origin',(0.500000000000001,-4.56640444411542E-17,
-11.03)) ;
#120050 = CARTESIAN_POINT('',(0.500000000000001,0.394987437106619,-11.13)) ;
#120051 = CARTESIAN_POINT('Ctrl Pts',(0.500000000000001,0.394987437106619,
-11.13)) ;
#120052 = CARTESIAN_POINT('Ctrl Pts',(0.505940567948954,0.395584486649901,
-11.13)) ;
#120053 = CARTESIAN_POINT('Ctrl Pts',(0.511931971019137,0.396132036079018,
-11.129466300328)) ;
#120054 = CARTESIAN_POINT('Ctrl Pts',(0.51782901530855,0.396618246075355,
-11.1283977957737)) ;
#120055 = CARTESIAN_POINT('Ctrl Pts',(0.522982218721202,0.397043126556054,
-11.1274640701571)) ;
#120056 = CARTESIAN_POINT('Ctrl Pts',(0.528062648970239,0.397421319341388,
-11.1261228267971)) ;
#120057 = CARTESIAN_POINT('Ctrl Pts',(0.532978106724003,0.397751505046071,
-11.1244057438766)) ;
#120058 = CARTESIAN_POINT('Ctrl Pts',(0.538583536338951,0.398128038182998,
-11.1224476378496)) ;
#120059 = CARTESIAN_POINT('Ctrl Pts',(0.544059405914855,0.398447721828294,
-11.1199700083111)) ;
#120060 = CARTESIAN_POINT('Ctrl Pts',(0.549268572255748,0.398712331108982,
-11.1170207319429)) ;
#120061 = CARTESIAN_POINT('Ctrl Pts',(0.553856850427136,0.398945401221755,
-11.1144229841468)) ;
#120062 = CARTESIAN_POINT('Ctrl Pts',(0.558237825069313,0.399135987683842,
-11.11146038498)) ;
#120063 = CARTESIAN_POINT('Ctrl Pts',(0.562333836086205,0.399290378266507,
-11.1081952228642)) ;
#120064 = CARTESIAN_POINT('Ctrl Pts',(0.566990328957881,0.399465895042381,
-11.1044832689523)) ;
#120065 = CARTESIAN_POINT('Ctrl Pts',(0.571349096493411,0.399597278936107,
-11.1003228064848)) ;
#120066 = CARTESIAN_POINT('Ctrl Pts',(0.575296920056702,0.399694832180837,
-11.0958055759794)) ;
#120067 = CARTESIAN_POINT('Ctrl Pts',(0.578744263667896,0.399780018245913,
-11.0918610112151)) ;
#120068 = CARTESIAN_POINT('Ctrl Pts',(0.581878314560452,0.399839626289636,
-11.0876455218421)) ;
#120069 = CARTESIAN_POINT('Ctrl Pts',(0.584648147334861,0.399882153365958,
-11.0832418177073)) ;
#120070 = CARTESIAN_POINT('Ctrl Pts',(0.587839270208171,0.399931148788079,
-11.0781683125045)) ;
#120071 = CARTESIAN_POINT('Ctrl Pts',(0.590595054415094,0.399958289583404,
-11.0727666362445)) ;
#120072 = CARTESIAN_POINT('Ctrl Pts',(0.59283861894311,0.399974357003159,
-11.0671616850094)) ;
#120073 = CARTESIAN_POINT('Ctrl Pts',(0.594777336851653,0.399988241245861,
-11.0623183122424)) ;
#120074 = CARTESIAN_POINT('Ctrl Pts',(0.596334051506183,0.399993946552814,
-11.0573241662271)) ;
#120075 = CARTESIAN_POINT('Ctrl Pts',(0.597488309822303,0.39999684570125,
-11.0522717185684)) ;
#120076 = CARTESIAN_POINT('Ctrl Pts',(0.598804024094406,0.400000150378306,
-11.0465125419605)) ;
#120077 = CARTESIAN_POINT('Ctrl Pts',(0.599612685195435,0.399999963509465,
-11.0406028438906)) ;
#120078 = CARTESIAN_POINT('Ctrl Pts',(0.599890230999722,0.399999993975383,
-11.034684202261)) ;
#120079 = CARTESIAN_POINT('Ctrl Pts',(0.5999634645494,0.400000002014155,-11.0331225027898)) ;
#120080 = CARTESIAN_POINT('Ctrl Pts',(0.600000000000001,0.399999999999999,
-11.0315602215092)) ;
#120081 = CARTESIAN_POINT('Ctrl Pts',(0.600000000000001,0.399999999999999,
-11.03)) ;
#120082 = CARTESIAN_POINT('',(0.600000000000001,0.299999999999999,-11.03)) ;
#120083 = CARTESIAN_POINT('Ctrl Pts',(0.500000000000001,0.394987437106619,
-11.13)) ;
#120084 = CARTESIAN_POINT('Ctrl Pts',(0.50045493559049,0.395033159853814,
-11.13)) ;
#120085 = CARTESIAN_POINT('Ctrl Pts',(0.500909898680794,0.395078570329092,
-11.1299968954911)) ;
#120086 = CARTESIAN_POINT('Ctrl Pts',(0.502892456245032,0.395275075889076,
-11.1299698339419)) ;
#120087 = CARTESIAN_POINT('Ctrl Pts',(0.504418747482277,0.395422812032189,
-11.129913985421)) ;
#120088 = CARTESIAN_POINT('Ctrl Pts',(0.508462199543281,0.395804395682027,
-11.1296732810566)) ;
#120089 = CARTESIAN_POINT('Ctrl Pts',(0.510974953343229,0.396031485023311,
-11.1294279391451)) ;
#120090 = CARTESIAN_POINT('Ctrl Pts',(0.521160739721084,0.396903453186219,
-11.1280427944916)) ;
#120091 = CARTESIAN_POINT('Ctrl Pts',(0.528708678528227,0.397444933153154,
-11.1261042177048)) ;
#120092 = CARTESIAN_POINT('Ctrl Pts',(0.545943206357832,0.398105551684098,
-11.1194646394512)) ;
#120093 = CARTESIAN_POINT('Ctrl Pts',(0.555229535466621,0.397987646678464,
-11.1140353588361)) ;
#120094 = CARTESIAN_POINT('Ctrl Pts',(0.571394604995555,0.395490482808064,
-11.100775513364)) ;
#120095 = CARTESIAN_POINT('Ctrl Pts',(0.57805531370272,0.393198948698444,
-11.093240745632)) ;
#120096 = CARTESIAN_POINT('Ctrl Pts',(0.588559132202387,0.385442756729392,
-11.0773922339842)) ;
#120097 = CARTESIAN_POINT('Ctrl Pts',(0.592167355639922,0.380240075127053,
-11.069548265607)) ;
#120098 = CARTESIAN_POINT('Ctrl Pts',(0.597496615531038,0.36589275346714,
-11.0539255217955)) ;
#120099 = CARTESIAN_POINT('Ctrl Pts',(0.598734255154188,0.356660564300906,
-11.046772741727)) ;
#120100 = CARTESIAN_POINT('Ctrl Pts',(0.60001275468167,0.335223914398785,
-11.0355823058657)) ;
#120101 = CARTESIAN_POINT('Ctrl Pts',(0.59999390055981,0.322655037092193,
-11.0316615193656)) ;
#120102 = CARTESIAN_POINT('Ctrl Pts',(0.600000296204999,0.30610691358234,
-11.030139626347)) ;
#120103 = CARTESIAN_POINT('Ctrl Pts',(0.600000000000001,0.303050992413441,
-11.03)) ;
#120104 = CARTESIAN_POINT('Ctrl Pts',(0.600000000000001,0.299999999999999,
-11.03)) ;
#120105 = CARTESIAN_POINT('',(0.600000000000001,-2.39800009914441E-17,-11.03)) ;
#120106 = CARTESIAN_POINT('Origin',(0.500000000000001,-1.9,-11.03)) ;
#120107 = CARTESIAN_POINT('Origin',(0.600000000000001,-1.9,-10.83)) ;
#120108 = CARTESIAN_POINT('Origin',(0.500000000000001,-1.9,-10.83)) ;
#120109 = CARTESIAN_POINT('Origin',(-0.899999999999999,-1.9,-10.055)) ;
#120110 = CARTESIAN_POINT('Origin',(-0.899999999999999,-1.9,-10.155)) ;
#120111 = CARTESIAN_POINT('Origin',(-0.899999999999999,0.6,-10.93)) ;
#120112 = CARTESIAN_POINT('Origin',(-0.899999999999999,0.6,-11.83)) ;
#120113 = CARTESIAN_POINT('Origin',(0.600000000000001,0.4,-11.83)) ;
#120114 = CARTESIAN_POINT('Origin',(0.500000000000001,0.4,-11.83)) ;
#120115 = CARTESIAN_POINT('Origin',(-0.899999999999999,0.4,-11.83)) ;
#120116 = CARTESIAN_POINT('Origin',(0.500000000000001,0.4,-11.83)) ;
#120117 = CARTESIAN_POINT('Origin',(0.500000000000001,-1.9,-10.83)) ;
#120118 = CARTESIAN_POINT('Origin',(0.500000000000001,-2.1,-10.83)) ;
#120119 = CARTESIAN_POINT('Origin',(-0.899999999999999,-1.9,-10.155)) ;
#120120 = CARTESIAN_POINT('Origin',(-1.1,-1.9,-10.155)) ;
#120121 = CARTESIAN_POINT('Origin',(-0.899999999999999,-2.1,-10.155)) ;
#120122 = CARTESIAN_POINT('Origin',(-0.899999999999999,0.4,-11.83)) ;
#120123 = CARTESIAN_POINT('Origin',(-0.899999999999999,0.4,-12.03)) ;
#120124 = CARTESIAN_POINT('Origin',(0.500000000000001,-2.1,-11.43)) ;
#120125 = CARTESIAN_POINT('Origin',(0.500000000000001,-2.1,-10.155)) ;
#120126 = CARTESIAN_POINT('Origin',(0.600000000000001,-2.1,-10.155)) ;
#120127 = CARTESIAN_POINT('Origin',(0.500000000000001,-2.1,-10.155)) ;
#120128 = CARTESIAN_POINT('Origin',(-1.1,-4.4272719500576E-17,-10.155)) ;
#120129 = CARTESIAN_POINT('',(-1.1,1.15,-10.055)) ;
#120130 = CARTESIAN_POINT('',(-1.1,1.25,-10.055)) ;
#120131 = CARTESIAN_POINT('Origin',(-1.1,1.15,-10.155)) ;
#120132 = CARTESIAN_POINT('Origin',(-0.899999999999999,0.5,-12.03)) ;
#120133 = CARTESIAN_POINT('Origin',(-0.899999999999999,-1.9,-12.03)) ;
#120134 = CARTESIAN_POINT('Origin',(0.600000000000001,-1.9,-12.03)) ;
#120135 = CARTESIAN_POINT('Origin',(0.500000000000001,-1.9,-12.03)) ;
#120136 = CARTESIAN_POINT('Origin',(-0.899999999999999,-1.9,-12.03)) ;
#120137 = CARTESIAN_POINT('Origin',(0.500000000000001,-1.9,-12.03)) ;
#120138 = CARTESIAN_POINT('Origin',(0.500000000000001,-2.1,-12.03)) ;
#120139 = CARTESIAN_POINT('Origin',(0.500000000000001,-2.1,-10.155)) ;
#120140 = CARTESIAN_POINT('Origin',(0.500000000000001,-2.1,-10.155)) ;
#120141 = CARTESIAN_POINT('Origin',(-1.1,-2.9,-9.955)) ;
#120142 = CARTESIAN_POINT('Origin',(-1.1,-2.9,-9.955)) ;
#120143 = CARTESIAN_POINT('Origin',(-1.1,-2.9,-9.955)) ;
#120144 = CARTESIAN_POINT('Origin',(-1.1,1.25,-9.955)) ;
#120145 = CARTESIAN_POINT('Origin',(-1.1,1.15,-9.955)) ;
#120146 = CARTESIAN_POINT('Origin',(-1.1,1.15,-10.155)) ;
#120147 = CARTESIAN_POINT('',(-1.1,1.25,-10.155)) ;
#120148 = CARTESIAN_POINT('Origin',(-1.1,1.15,-10.155)) ;
#120149 = CARTESIAN_POINT('Origin',(-1.1,1.15,-10.155)) ;
#120150 = CARTESIAN_POINT('Origin',(-0.899999999999999,-1.9,-12.03)) ;
#120151 = CARTESIAN_POINT('Origin',(-0.899999999999999,-1.9,-12.03)) ;
#120152 = CARTESIAN_POINT('Origin',(0.500000000000001,-2.1,-11.43)) ;
#120153 = CARTESIAN_POINT('Origin',(0.500000000000001,-2.1,-12.705)) ;
#120154 = CARTESIAN_POINT('Origin',(0.500000000000001,1.36481920536411E-16,
-10.155)) ;
#120155 = CARTESIAN_POINT('Origin',(0.500000000000001,-2.9,-10.155)) ;
#120156 = CARTESIAN_POINT('Origin',(-0.999999999999999,-2.9,-9.955)) ;
#120157 = CARTESIAN_POINT('Origin',(0.500000000000001,-2.9,-9.955)) ;
#120158 = CARTESIAN_POINT('Origin',(-1.1,1.15,-10.155)) ;
#120159 = CARTESIAN_POINT('Origin',(-1.1,1.35,-10.155)) ;
#120160 = CARTESIAN_POINT('Origin',(-1.1,1.15,-11.43)) ;
#120161 = CARTESIAN_POINT('',(-1.1,1.25,-12.705)) ;
#120162 = CARTESIAN_POINT('',(-1.1,1.25,-12.805)) ;
#120163 = CARTESIAN_POINT('Origin',(-1.1,1.15,-12.705)) ;
#120164 = CARTESIAN_POINT('Origin',(-0.899999999999999,-1.9,-11.93)) ;
#120165 = CARTESIAN_POINT('Origin',(-0.899999999999999,-1.9,-12.705)) ;
#120166 = CARTESIAN_POINT('Origin',(-0.999999999999999,-2.1,-12.705)) ;
#120167 = CARTESIAN_POINT('Origin',(0.500000000000001,-2.1,-12.705)) ;
#120168 = CARTESIAN_POINT('Origin',(-0.899999999999999,-2.1,-12.705)) ;
#120169 = CARTESIAN_POINT('Origin',(0.500000000000001,-2.1,-12.705)) ;
#120170 = CARTESIAN_POINT('Origin',(0.500000000000001,-2.1,-12.705)) ;
#120171 = CARTESIAN_POINT('Origin',(0.500000000000001,-2.9,-10.155)) ;
#120172 = CARTESIAN_POINT('Origin',(0.700000000000002,-2.9,-10.155)) ;
#120173 = CARTESIAN_POINT('Origin',(-1.1,1.35,-12.805)) ;
#120174 = CARTESIAN_POINT('Origin',(-1.1,1.35,-12.705)) ;
#120175 = CARTESIAN_POINT('Origin',(-1.1,1.15,-12.705)) ;
#120176 = CARTESIAN_POINT('',(-1.1,1.15,-12.805)) ;
#120177 = CARTESIAN_POINT('Origin',(-1.1,1.15,-12.705)) ;
#120178 = CARTESIAN_POINT('Origin',(-1.1,1.15,-12.705)) ;
#120179 = CARTESIAN_POINT('Origin',(-0.899999999999999,-1.9,-12.705)) ;
#120180 = CARTESIAN_POINT('Origin',(-1.1,-1.9,-12.705)) ;
#120181 = CARTESIAN_POINT('Origin',(0.500000000000001,-5.86744705109802E-17,
-12.705)) ;
#120182 = CARTESIAN_POINT('Origin',(0.500000000000001,-2.9,-12.705)) ;
#120183 = CARTESIAN_POINT('Origin',(0.700000000000002,-2.9,-11.43)) ;
#120184 = CARTESIAN_POINT('Origin',(0.700000000000002,-2.9,-12.705)) ;
#120185 = CARTESIAN_POINT('Origin',(-1.1,1.15,-12.705)) ;
#120186 = CARTESIAN_POINT('Origin',(-1.1,1.15,-12.905)) ;
#120187 = CARTESIAN_POINT('Origin',(-1.1,-2.39429110547967E-16,-12.705)) ;
#120188 = CARTESIAN_POINT('',(-1.1,1.25,-12.805)) ;
#120189 = CARTESIAN_POINT('Origin',(0.500000000000001,-2.9,-12.705)) ;
#120190 = CARTESIAN_POINT('Origin',(0.500000000000001,-2.9,-12.905)) ;
#120191 = CARTESIAN_POINT('Origin',(-1.1,1.25,-12.905)) ;
#120192 = CARTESIAN_POINT('Origin',(-1.1,-2.9,-12.905)) ;
#120193 = CARTESIAN_POINT('Origin',(-1.1,-2.9,-12.905)) ;
#120194 = CARTESIAN_POINT('Origin',(-1.1,-2.9,-12.905)) ;
#120195 = CARTESIAN_POINT('Origin',(-1.1,-2.9,-12.905)) ;
#120196 = CARTESIAN_POINT('Origin',(1.5,1.9,-10.83)) ;
#120197 = CARTESIAN_POINT('Origin',(1.5,1.9,-12.98)) ;
#120198 = CARTESIAN_POINT('Origin',(1.5,1.9,-12.03)) ;
#120199 = CARTESIAN_POINT('Origin',(1.5,2.1,-12.03)) ;
#120200 = CARTESIAN_POINT('Origin',(1.5,2.1,-11.83)) ;
#120201 = CARTESIAN_POINT('Origin',(1.5,1.9,-12.98)) ;
#120202 = CARTESIAN_POINT('Origin',(1.5,1.9,-12.98)) ;
#120203 = CARTESIAN_POINT('Origin',(1.5,2.1,-11.83)) ;
#120204 = CARTESIAN_POINT('Origin',(1.5,2.4,-11.83)) ;
#120205 = CARTESIAN_POINT('Origin',(1.5,2.1,-12.98)) ;
#120206 = CARTESIAN_POINT('Origin',(1.5,-2.15,-12.98)) ;
#120207 = CARTESIAN_POINT('Origin',(1.5,2.4,-12.03)) ;
#120208 = CARTESIAN_POINT('Origin',(1.5,2.6,-12.03)) ;
#120209 = CARTESIAN_POINT('Origin',(1.5,-2.15,-12.98)) ;
#120210 = CARTESIAN_POINT('Origin',(1.5,-2.15,-12.98)) ;
#120211 = CARTESIAN_POINT('Origin',(1.5,2.6,-10.83)) ;
#120212 = CARTESIAN_POINT('Origin',(1.5,2.6,-12.1385786437627)) ;
#120213 = CARTESIAN_POINT('Origin',(1.5,-2.15,-10.83)) ;
#120214 = CARTESIAN_POINT('Origin',(1.5,-2.15,-12.3331195934094)) ;
#120215 = CARTESIAN_POINT('Origin',(1.5,2.6,-12.1385786437627)) ;
#120216 = CARTESIAN_POINT('Origin',(1.5,2.6,-12.1385786437627)) ;
#120217 = CARTESIAN_POINT('Origin',(1.5,-2.15,-12.3331195934094)) ;
#120218 = CARTESIAN_POINT('Origin',(1.5,-2.15,-12.3331195934094)) ;
#120219 = CARTESIAN_POINT('Origin',(1.5,1.69571067811865,-11.2342893218813)) ;
#120220 = CARTESIAN_POINT('Origin',(1.5,3.15,-12.6885786437627)) ;
#120221 = CARTESIAN_POINT('Origin',(1.5,-3.65625,-11.43)) ;
#120222 = CARTESIAN_POINT('Origin',(1.5,-2.15,-10.5268804065906)) ;
#120223 = CARTESIAN_POINT('Origin',(1.5,3.15,-12.6885786437627)) ;
#120224 = CARTESIAN_POINT('Origin',(1.5,3.15,-12.6885786437627)) ;
#120225 = CARTESIAN_POINT('Origin',(1.5,-2.15,-10.5268804065906)) ;
#120226 = CARTESIAN_POINT('Origin',(1.5,-2.15,-10.5268804065906)) ;
#120227 = CARTESIAN_POINT('Origin',(1.5,3.15,-10.83)) ;
#120228 = CARTESIAN_POINT('Origin',(1.5,-2.15,-10.83)) ;
#120229 = CARTESIAN_POINT('Origin',(1.5,-2.15,-9.88)) ;
#120230 = CARTESIAN_POINT('Origin',(1.5,-2.15,-9.88)) ;
#120231 = CARTESIAN_POINT('Origin',(1.5,-2.15,-9.88)) ;
#120232 = CARTESIAN_POINT('Origin',(1.5,2.29571067811866,-11.0257106781187)) ;
#120233 = CARTESIAN_POINT('Origin',(1.5,2.6,-10.7214213562373)) ;
#120234 = CARTESIAN_POINT('Origin',(1.5,2.1,-9.88)) ;
#120235 = CARTESIAN_POINT('Origin',(1.5,1.9,-9.88)) ;
#120236 = CARTESIAN_POINT('Origin',(1.5,2.6,-10.7214213562373)) ;
#120237 = CARTESIAN_POINT('Origin',(1.5,2.6,-10.7214213562373)) ;
#120238 = CARTESIAN_POINT('Origin',(1.5,1.9,-9.88)) ;
#120239 = CARTESIAN_POINT('Origin',(1.5,1.9,-9.88)) ;
#120240 = CARTESIAN_POINT('Origin',(1.5,2.6,-10.83)) ;
#120241 = CARTESIAN_POINT('Origin',(1.5,2.6,-10.83)) ;
#120242 = CARTESIAN_POINT('Origin',(1.5,1.9,-10.83)) ;
#120243 = CARTESIAN_POINT('Origin',(1.5,1.9,-10.83)) ;
#120244 = CARTESIAN_POINT('Origin',(1.5,2.4,-10.83)) ;
#120245 = CARTESIAN_POINT('Origin',(1.5,2.4,-11.03)) ;
#120246 = CARTESIAN_POINT('Origin',(1.5,2.1,-10.83)) ;
#120247 = CARTESIAN_POINT('Origin',(1.5,2.1,-11.03)) ;
#120248 = CARTESIAN_POINT('Origin',(1.5,2.1,-11.03)) ;
#120249 = CARTESIAN_POINT('Origin',(-0.899999999999999,-2.,-14.64)) ;
#120250 = CARTESIAN_POINT('Origin',(-0.899999999999999,0.4,-14.64)) ;
#120251 = CARTESIAN_POINT('Origin',(-0.899999999999999,-1.9,-14.64)) ;
#120252 = CARTESIAN_POINT('Origin',(0.600000000000001,0.4,-14.84)) ;
#120253 = CARTESIAN_POINT('Origin',(0.500000000000001,0.4,-14.84)) ;
#120254 = CARTESIAN_POINT('Origin',(-0.899999999999999,0.4,-14.84)) ;
#120255 = CARTESIAN_POINT('Origin',(0.500000000000001,0.4,-14.84)) ;
#120256 = CARTESIAN_POINT('',(0.600000000000001,0.4,-14.84)) ;
#120257 = CARTESIAN_POINT('Origin',(0.500000000000001,0.4,-14.84)) ;
#120258 = CARTESIAN_POINT('Origin',(0.500000000000001,0.4,-14.84)) ;
#120259 = CARTESIAN_POINT('Origin',(-0.899999999999999,-1.9,-14.64)) ;
#120260 = CARTESIAN_POINT('Origin',(-0.899999999999999,-1.9,-14.64)) ;
#120261 = CARTESIAN_POINT('Origin',(-0.899999999999999,-1.9,-14.64)) ;
#120262 = CARTESIAN_POINT('Origin',(-0.899999999999999,0.4,-14.84)) ;
#120263 = CARTESIAN_POINT('Origin',(-0.899999999999999,0.6,-14.84)) ;
#120264 = CARTESIAN_POINT('Origin',(0.500000000000001,0.4,-15.24)) ;
#120265 = CARTESIAN_POINT('Origin',(0.500000000000001,0.4,-15.64)) ;
#120266 = CARTESIAN_POINT('',(0.600000000000001,0.4,-15.54)) ;
#120267 = CARTESIAN_POINT('Ctrl Pts',(0.595612997216082,0.370705721320405,
-15.6107057213204)) ;
#120268 = CARTESIAN_POINT('Ctrl Pts',(0.596180587760893,0.372558268494361,
-15.6088554988322)) ;
#120269 = CARTESIAN_POINT('Ctrl Pts',(0.596672461925687,0.374355839771988,
-15.6069141798663)) ;
#120270 = CARTESIAN_POINT('Ctrl Pts',(0.599015141889213,0.383869350930072,
-15.5957649936563)) ;
#120271 = CARTESIAN_POINT('Ctrl Pts',(0.599609996542525,0.390224332900456,
-15.5849726026541)) ;
#120272 = CARTESIAN_POINT('Ctrl Pts',(0.600050586298725,0.398117439141561,
-15.5623310532047)) ;
#120273 = CARTESIAN_POINT('Ctrl Pts',(0.600000000000001,0.4,-15.5512012506335)) ;
#120274 = CARTESIAN_POINT('Ctrl Pts',(0.600000000000001,0.399999999999999,
-15.54)) ;
#120275 = CARTESIAN_POINT('',(0.600000000000001,0.4,-15.24)) ;
#120276 = CARTESIAN_POINT('Origin',(0.500000000000001,-4.56640444411542E-17,
-14.84)) ;
#120277 = CARTESIAN_POINT('',(0.500000000000001,0.394987437106619,-14.94)) ;
#120278 = CARTESIAN_POINT('Ctrl Pts',(0.500000000000001,0.394987437106619,
-14.94)) ;
#120279 = CARTESIAN_POINT('Ctrl Pts',(0.505940567948958,0.395584486649901,
-14.94)) ;
#120280 = CARTESIAN_POINT('Ctrl Pts',(0.511931971019147,0.396132036079019,
-14.939466300328)) ;
#120281 = CARTESIAN_POINT('Ctrl Pts',(0.517829015308562,0.396618246075356,
-14.9383977957737)) ;
#120282 = CARTESIAN_POINT('Ctrl Pts',(0.522982218721209,0.397043126556054,
-14.9374640701571)) ;
#120283 = CARTESIAN_POINT('Ctrl Pts',(0.528062648970245,0.397421319341388,
-14.9361228267971)) ;
#120284 = CARTESIAN_POINT('Ctrl Pts',(0.532978106724004,0.397751505046071,
-14.9344057438766)) ;
#120285 = CARTESIAN_POINT('Ctrl Pts',(0.538583536338963,0.398128038182999,
-14.9324476378495)) ;
#120286 = CARTESIAN_POINT('Ctrl Pts',(0.544059405914874,0.398447721828296,
-14.9299700083111)) ;
#120287 = CARTESIAN_POINT('Ctrl Pts',(0.549268572255776,0.398712331108984,
-14.9270207319429)) ;
#120288 = CARTESIAN_POINT('Ctrl Pts',(0.553856850427151,0.398945401221756,
-14.9244229841468)) ;
#120289 = CARTESIAN_POINT('Ctrl Pts',(0.558237825069319,0.399135987683843,
-14.92146038498)) ;
#120290 = CARTESIAN_POINT('Ctrl Pts',(0.562333836086205,0.399290378266507,
-14.9181952228642)) ;
#120291 = CARTESIAN_POINT('Ctrl Pts',(0.56699032895788,0.399465895042381,
-14.9144832689523)) ;
#120292 = CARTESIAN_POINT('Ctrl Pts',(0.571349096493406,0.399597278936107,
-14.9103228064848)) ;
#120293 = CARTESIAN_POINT('Ctrl Pts',(0.575296920056693,0.399694832180837,
-14.9058055759794)) ;
#120294 = CARTESIAN_POINT('Ctrl Pts',(0.578744263667893,0.399780018245913,
-14.9018610112151)) ;
#120295 = CARTESIAN_POINT('Ctrl Pts',(0.581878314560404,0.399839626289636,
-14.8976455218421)) ;
#120296 = CARTESIAN_POINT('Ctrl Pts',(0.584648147334845,0.399882153365958,
-14.8932418177073)) ;
#120297 = CARTESIAN_POINT('Ctrl Pts',(0.587839270208164,0.399931148788079,
-14.8881683125045)) ;
#120298 = CARTESIAN_POINT('Ctrl Pts',(0.590595054415084,0.399958289583404,
-14.8827666362445)) ;
#120299 = CARTESIAN_POINT('Ctrl Pts',(0.592838618943089,0.399974357003159,
-14.8771616850094)) ;
#120300 = CARTESIAN_POINT('Ctrl Pts',(0.594777336851653,0.399988241245861,
-14.8723183122424)) ;
#120301 = CARTESIAN_POINT('Ctrl Pts',(0.596334051506184,0.399993946552814,
-14.8673241662272)) ;
#120302 = CARTESIAN_POINT('Ctrl Pts',(0.597488309822312,0.39999684570125,
-14.8622717185684)) ;
#120303 = CARTESIAN_POINT('Ctrl Pts',(0.598804024094403,0.400000150378306,
-14.8565125419605)) ;
#120304 = CARTESIAN_POINT('Ctrl Pts',(0.599612685195422,0.399999963509465,
-14.8506028438907)) ;
#120305 = CARTESIAN_POINT('Ctrl Pts',(0.599890230999715,0.399999993975383,
-14.8446842022612)) ;
#120306 = CARTESIAN_POINT('Ctrl Pts',(0.599963464549397,0.400000002014155,
-14.8431225027899)) ;
#120307 = CARTESIAN_POINT('Ctrl Pts',(0.600000000000001,0.399999999999999,
-14.8415602215092)) ;
#120308 = CARTESIAN_POINT('Ctrl Pts',(0.600000000000001,0.399999999999999,
-14.84)) ;
#120309 = CARTESIAN_POINT('',(0.600000000000001,0.299999999999999,-14.84)) ;
#120310 = CARTESIAN_POINT('Ctrl Pts',(0.500000000000001,0.394987437106619,
-14.94)) ;
#120311 = CARTESIAN_POINT('Ctrl Pts',(0.500454935590171,0.395033159853782,
-14.94)) ;
#120312 = CARTESIAN_POINT('Ctrl Pts',(0.500909898680634,0.395078570329076,
-14.9399968954911)) ;
#120313 = CARTESIAN_POINT('Ctrl Pts',(0.502892456245054,0.395275075889078,
-14.9399698339419)) ;
#120314 = CARTESIAN_POINT('Ctrl Pts',(0.504418747482298,0.395422812032191,
-14.939913985421)) ;
#120315 = CARTESIAN_POINT('Ctrl Pts',(0.508462199543321,0.395804395682031,
-14.9396732810566)) ;
#120316 = CARTESIAN_POINT('Ctrl Pts',(0.510974953343265,0.396031485023314,
-14.9394279391451)) ;
#120317 = CARTESIAN_POINT('Ctrl Pts',(0.521160739721169,0.396903453186227,
-14.9380427944916)) ;
#120318 = CARTESIAN_POINT('Ctrl Pts',(0.528708678528302,0.397444933153157,
-14.9361042177047)) ;
#120319 = CARTESIAN_POINT('Ctrl Pts',(0.54594320635793,0.398105551684103,
-14.9294646394512)) ;
#120320 = CARTESIAN_POINT('Ctrl Pts',(0.555229535466698,0.397987646678449,
-14.9240353588361)) ;
#120321 = CARTESIAN_POINT('Ctrl Pts',(0.571394604995641,0.395490482808055,
-14.9107755133639)) ;
#120322 = CARTESIAN_POINT('Ctrl Pts',(0.578055313702769,0.393198948698403,
-14.9032407456319)) ;
#120323 = CARTESIAN_POINT('Ctrl Pts',(0.58855913220244,0.385442756729361,
-14.8873922339841)) ;
#120324 = CARTESIAN_POINT('Ctrl Pts',(0.592167355639942,0.380240075126989,
-14.8795482656069)) ;
#120325 = CARTESIAN_POINT('Ctrl Pts',(0.59749661553107,0.365892753467073,
-14.8639255217954)) ;
#120326 = CARTESIAN_POINT('Ctrl Pts',(0.598734255154193,0.356660564300806,
-14.856772741727)) ;
#120327 = CARTESIAN_POINT('Ctrl Pts',(0.600012754681677,0.335223914398739,
-14.8455823058657)) ;
#120328 = CARTESIAN_POINT('Ctrl Pts',(0.59999390055981,0.322655037092125,
-14.8416615193656)) ;
#120329 = CARTESIAN_POINT('Ctrl Pts',(0.600000296204999,0.306106913582367,
-14.840139626347)) ;
#120330 = CARTESIAN_POINT('Ctrl Pts',(0.600000000000001,0.303050992413449,
-14.84)) ;
#120331 = CARTESIAN_POINT('Ctrl Pts',(0.600000000000001,0.299999999999999,
-14.84)) ;
#120332 = CARTESIAN_POINT('',(0.600000000000001,-2.39800009914441E-17,-14.84)) ;
#120333 = CARTESIAN_POINT('Origin',(0.500000000000001,-1.9,-14.84)) ;
#120334 = CARTESIAN_POINT('Origin',(0.600000000000001,-1.9,-14.64)) ;
#120335 = CARTESIAN_POINT('Origin',(0.500000000000001,-1.9,-14.64)) ;
#120336 = CARTESIAN_POINT('Origin',(-0.899999999999999,-1.9,-13.865)) ;
#120337 = CARTESIAN_POINT('Origin',(-0.899999999999999,-1.9,-13.965)) ;
#120338 = CARTESIAN_POINT('Origin',(-0.899999999999999,0.6,-14.74)) ;
#120339 = CARTESIAN_POINT('Origin',(-0.899999999999999,0.6,-15.64)) ;
#120340 = CARTESIAN_POINT('Origin',(0.600000000000001,0.4,-15.64)) ;
#120341 = CARTESIAN_POINT('Origin',(0.500000000000001,0.4,-15.64)) ;
#120342 = CARTESIAN_POINT('Origin',(-0.899999999999999,0.4,-15.64)) ;
#120343 = CARTESIAN_POINT('Origin',(0.500000000000001,0.4,-15.64)) ;
#120344 = CARTESIAN_POINT('Origin',(0.500000000000001,-1.9,-14.64)) ;
#120345 = CARTESIAN_POINT('Origin',(0.500000000000001,-2.1,-14.64)) ;
#120346 = CARTESIAN_POINT('Origin',(-0.899999999999999,-1.9,-13.965)) ;
#120347 = CARTESIAN_POINT('Origin',(-1.1,-1.9,-13.965)) ;
#120348 = CARTESIAN_POINT('Origin',(-0.899999999999999,-2.1,-13.965)) ;
#120349 = CARTESIAN_POINT('Origin',(-0.899999999999999,0.4,-15.64)) ;
#120350 = CARTESIAN_POINT('Origin',(-0.899999999999999,0.4,-15.84)) ;
#120351 = CARTESIAN_POINT('Origin',(0.500000000000001,-2.1,-15.24)) ;
#120352 = CARTESIAN_POINT('Origin',(0.500000000000001,-2.1,-13.965)) ;
#120353 = CARTESIAN_POINT('Origin',(0.600000000000001,-2.1,-13.965)) ;
#120354 = CARTESIAN_POINT('Origin',(0.500000000000001,-2.1,-13.965)) ;
#120355 = CARTESIAN_POINT('Origin',(-1.1,-4.4272719500576E-17,-13.965)) ;
#120356 = CARTESIAN_POINT('',(-1.1,1.15,-13.865)) ;
#120357 = CARTESIAN_POINT('',(-1.1,1.25,-13.865)) ;
#120358 = CARTESIAN_POINT('Origin',(-1.1,1.15,-13.965)) ;
#120359 = CARTESIAN_POINT('Origin',(-0.899999999999999,0.5,-15.84)) ;
#120360 = CARTESIAN_POINT('Origin',(-0.899999999999999,-1.9,-15.84)) ;
#120361 = CARTESIAN_POINT('Origin',(0.600000000000001,-1.9,-15.84)) ;
#120362 = CARTESIAN_POINT('Origin',(0.500000000000001,-1.9,-15.84)) ;
#120363 = CARTESIAN_POINT('Origin',(-0.899999999999999,-1.9,-15.84)) ;
#120364 = CARTESIAN_POINT('Origin',(0.500000000000001,-1.9,-15.84)) ;
#120365 = CARTESIAN_POINT('Origin',(0.500000000000001,-2.1,-15.84)) ;
#120366 = CARTESIAN_POINT('Origin',(0.500000000000001,-2.1,-13.965)) ;
#120367 = CARTESIAN_POINT('Origin',(0.500000000000001,-2.1,-13.965)) ;
#120368 = CARTESIAN_POINT('Origin',(-1.1,-2.9,-13.765)) ;
#120369 = CARTESIAN_POINT('Origin',(-1.1,-2.9,-13.765)) ;
#120370 = CARTESIAN_POINT('Origin',(-1.1,-2.9,-13.765)) ;
#120371 = CARTESIAN_POINT('Origin',(-1.1,1.25,-13.765)) ;
#120372 = CARTESIAN_POINT('Origin',(-1.1,1.15,-13.765)) ;
#120373 = CARTESIAN_POINT('Origin',(-1.1,1.15,-13.965)) ;
#120374 = CARTESIAN_POINT('',(-1.1,1.25,-13.965)) ;
#120375 = CARTESIAN_POINT('Origin',(-1.1,1.15,-13.965)) ;
#120376 = CARTESIAN_POINT('Origin',(-1.1,1.15,-13.965)) ;
#120377 = CARTESIAN_POINT('Origin',(-0.899999999999999,-1.9,-15.84)) ;
#120378 = CARTESIAN_POINT('Origin',(-0.899999999999999,-1.9,-15.84)) ;
#120379 = CARTESIAN_POINT('Origin',(0.500000000000001,-2.1,-15.24)) ;
#120380 = CARTESIAN_POINT('Origin',(0.500000000000001,-2.1,-16.515)) ;
#120381 = CARTESIAN_POINT('Origin',(0.500000000000001,1.36481920536411E-16,
-13.965)) ;
#120382 = CARTESIAN_POINT('Origin',(0.500000000000001,-2.9,-13.965)) ;
#120383 = CARTESIAN_POINT('Origin',(-0.999999999999999,-2.9,-13.765)) ;
#120384 = CARTESIAN_POINT('Origin',(0.500000000000001,-2.9,-13.765)) ;
#120385 = CARTESIAN_POINT('Origin',(-1.1,1.15,-13.965)) ;
#120386 = CARTESIAN_POINT('Origin',(-1.1,1.35,-13.965)) ;
#120387 = CARTESIAN_POINT('Origin',(-1.1,1.15,-15.24)) ;
#120388 = CARTESIAN_POINT('',(-1.1,1.25,-16.515)) ;
#120389 = CARTESIAN_POINT('',(-1.1,1.25,-16.615)) ;
#120390 = CARTESIAN_POINT('Origin',(-1.1,1.15,-16.515)) ;
#120391 = CARTESIAN_POINT('Origin',(-0.899999999999999,-1.9,-15.74)) ;
#120392 = CARTESIAN_POINT('Origin',(-0.899999999999999,-1.9,-16.515)) ;
#120393 = CARTESIAN_POINT('Origin',(-0.999999999999999,-2.1,-16.515)) ;
#120394 = CARTESIAN_POINT('Origin',(0.500000000000001,-2.1,-16.515)) ;
#120395 = CARTESIAN_POINT('Origin',(-0.899999999999999,-2.1,-16.515)) ;
#120396 = CARTESIAN_POINT('Origin',(0.500000000000001,-2.1,-16.515)) ;
#120397 = CARTESIAN_POINT('Origin',(0.500000000000001,-2.1,-16.515)) ;
#120398 = CARTESIAN_POINT('Origin',(0.500000000000001,-2.9,-13.965)) ;
#120399 = CARTESIAN_POINT('Origin',(0.700000000000002,-2.9,-13.965)) ;
#120400 = CARTESIAN_POINT('Origin',(-1.1,1.35,-16.615)) ;
#120401 = CARTESIAN_POINT('Origin',(-1.1,1.35,-16.515)) ;
#120402 = CARTESIAN_POINT('Origin',(-1.1,1.15,-16.515)) ;
#120403 = CARTESIAN_POINT('',(-1.1,1.15,-16.615)) ;
#120404 = CARTESIAN_POINT('Origin',(-1.1,1.15,-16.515)) ;
#120405 = CARTESIAN_POINT('Origin',(-1.1,1.15,-16.515)) ;
#120406 = CARTESIAN_POINT('Origin',(-0.899999999999999,-1.9,-16.515)) ;
#120407 = CARTESIAN_POINT('Origin',(-1.1,-1.9,-16.515)) ;
#120408 = CARTESIAN_POINT('Origin',(0.500000000000001,-5.86744705109802E-17,
-16.515)) ;
#120409 = CARTESIAN_POINT('Origin',(0.500000000000001,-2.9,-16.515)) ;
#120410 = CARTESIAN_POINT('Origin',(0.700000000000002,-2.9,-15.24)) ;
#120411 = CARTESIAN_POINT('Origin',(0.700000000000002,-2.9,-16.515)) ;
#120412 = CARTESIAN_POINT('Origin',(-1.1,1.15,-16.515)) ;
#120413 = CARTESIAN_POINT('Origin',(-1.1,1.15,-16.715)) ;
#120414 = CARTESIAN_POINT('Origin',(-1.1,-2.39429110547967E-16,-16.515)) ;
#120415 = CARTESIAN_POINT('',(-1.1,1.25,-16.615)) ;
#120416 = CARTESIAN_POINT('Origin',(0.500000000000001,-2.9,-16.515)) ;
#120417 = CARTESIAN_POINT('Origin',(0.500000000000001,-2.9,-16.715)) ;
#120418 = CARTESIAN_POINT('Origin',(-1.1,1.25,-16.715)) ;
#120419 = CARTESIAN_POINT('Origin',(-1.1,-2.9,-16.715)) ;
#120420 = CARTESIAN_POINT('Origin',(-1.1,-2.9,-16.715)) ;
#120421 = CARTESIAN_POINT('Origin',(-1.1,-2.9,-16.715)) ;
#120422 = CARTESIAN_POINT('Origin',(-1.1,-2.9,-16.715)) ;
#120423 = CARTESIAN_POINT('Origin',(1.5,1.9,-14.64)) ;
#120424 = CARTESIAN_POINT('Origin',(1.5,1.9,-16.79)) ;
#120425 = CARTESIAN_POINT('Origin',(1.5,1.9,-15.84)) ;
#120426 = CARTESIAN_POINT('Origin',(1.5,2.1,-15.84)) ;
#120427 = CARTESIAN_POINT('Origin',(1.5,2.1,-15.64)) ;
#120428 = CARTESIAN_POINT('Origin',(1.5,1.9,-16.79)) ;
#120429 = CARTESIAN_POINT('Origin',(1.5,1.9,-16.79)) ;
#120430 = CARTESIAN_POINT('Origin',(1.5,2.1,-15.64)) ;
#120431 = CARTESIAN_POINT('Origin',(1.5,2.4,-15.64)) ;
#120432 = CARTESIAN_POINT('Origin',(1.5,2.1,-16.79)) ;
#120433 = CARTESIAN_POINT('Origin',(1.5,-2.15,-16.79)) ;
#120434 = CARTESIAN_POINT('Origin',(1.5,2.4,-15.84)) ;
#120435 = CARTESIAN_POINT('Origin',(1.5,2.6,-15.84)) ;
#120436 = CARTESIAN_POINT('Origin',(1.5,-2.15,-16.79)) ;
#120437 = CARTESIAN_POINT('Origin',(1.5,-2.15,-16.79)) ;
#120438 = CARTESIAN_POINT('Origin',(1.5,2.6,-14.64)) ;
#120439 = CARTESIAN_POINT('Origin',(1.5,2.6,-15.9485786437627)) ;
#120440 = CARTESIAN_POINT('Origin',(1.5,-2.15,-14.64)) ;
#120441 = CARTESIAN_POINT('Origin',(1.5,-2.15,-16.1431195934094)) ;
#120442 = CARTESIAN_POINT('Origin',(1.5,2.6,-15.9485786437627)) ;
#120443 = CARTESIAN_POINT('Origin',(1.5,2.6,-15.9485786437627)) ;
#120444 = CARTESIAN_POINT('Origin',(1.5,-2.15,-16.1431195934094)) ;
#120445 = CARTESIAN_POINT('Origin',(1.5,-2.15,-16.1431195934094)) ;
#120446 = CARTESIAN_POINT('Origin',(1.5,1.69571067811865,-15.0442893218814)) ;
#120447 = CARTESIAN_POINT('Origin',(1.5,3.15,-16.4985786437627)) ;
#120448 = CARTESIAN_POINT('Origin',(1.5,-3.65625,-15.24)) ;
#120449 = CARTESIAN_POINT('Origin',(1.5,-2.15,-14.3368804065906)) ;
#120450 = CARTESIAN_POINT('Origin',(1.5,3.15,-16.4985786437627)) ;
#120451 = CARTESIAN_POINT('Origin',(1.5,3.15,-16.4985786437627)) ;
#120452 = CARTESIAN_POINT('Origin',(1.5,-2.15,-14.3368804065906)) ;
#120453 = CARTESIAN_POINT('Origin',(1.5,-2.15,-14.3368804065906)) ;
#120454 = CARTESIAN_POINT('Origin',(1.5,3.15,-14.64)) ;
#120455 = CARTESIAN_POINT('Origin',(1.5,-2.15,-14.64)) ;
#120456 = CARTESIAN_POINT('Origin',(1.5,-2.15,-13.69)) ;
#120457 = CARTESIAN_POINT('Origin',(1.5,-2.15,-13.69)) ;
#120458 = CARTESIAN_POINT('Origin',(1.5,-2.15,-13.69)) ;
#120459 = CARTESIAN_POINT('Origin',(1.5,2.29571067811866,-14.8357106781187)) ;
#120460 = CARTESIAN_POINT('Origin',(1.5,2.6,-14.5314213562373)) ;
#120461 = CARTESIAN_POINT('Origin',(1.5,2.1,-13.69)) ;
#120462 = CARTESIAN_POINT('Origin',(1.5,1.9,-13.69)) ;
#120463 = CARTESIAN_POINT('Origin',(1.5,2.6,-14.5314213562373)) ;
#120464 = CARTESIAN_POINT('Origin',(1.5,2.6,-14.5314213562373)) ;
#120465 = CARTESIAN_POINT('Origin',(1.5,1.9,-13.69)) ;
#120466 = CARTESIAN_POINT('Origin',(1.5,1.9,-13.69)) ;
#120467 = CARTESIAN_POINT('Origin',(1.5,2.6,-14.64)) ;
#120468 = CARTESIAN_POINT('Origin',(1.5,2.6,-14.64)) ;
#120469 = CARTESIAN_POINT('Origin',(1.5,1.9,-14.64)) ;
#120470 = CARTESIAN_POINT('Origin',(1.5,1.9,-14.64)) ;
#120471 = CARTESIAN_POINT('Origin',(1.5,2.4,-14.64)) ;
#120472 = CARTESIAN_POINT('Origin',(1.5,2.4,-14.84)) ;
#120473 = CARTESIAN_POINT('Origin',(1.5,2.1,-14.64)) ;
#120474 = CARTESIAN_POINT('Origin',(1.5,2.1,-14.84)) ;
#120475 = CARTESIAN_POINT('Origin',(1.5,2.1,-14.84)) ;
#120476 = CARTESIAN_POINT('Origin',(-0.899999999999999,-2.,-18.45)) ;
#120477 = CARTESIAN_POINT('Origin',(-0.899999999999999,0.4,-18.45)) ;
#120478 = CARTESIAN_POINT('Origin',(-0.899999999999999,-1.9,-18.45)) ;
#120479 = CARTESIAN_POINT('Origin',(0.600000000000001,0.4,-18.65)) ;
#120480 = CARTESIAN_POINT('Origin',(0.500000000000001,0.4,-18.65)) ;
#120481 = CARTESIAN_POINT('Origin',(-0.899999999999999,0.4,-18.65)) ;
#120482 = CARTESIAN_POINT('Origin',(0.500000000000001,0.4,-18.65)) ;
#120483 = CARTESIAN_POINT('',(0.600000000000001,0.4,-18.65)) ;
#120484 = CARTESIAN_POINT('Origin',(0.500000000000001,0.4,-18.65)) ;
#120485 = CARTESIAN_POINT('Origin',(0.500000000000001,0.4,-18.65)) ;
#120486 = CARTESIAN_POINT('Origin',(-0.899999999999999,-1.9,-18.45)) ;
#120487 = CARTESIAN_POINT('Origin',(-0.899999999999999,-1.9,-18.45)) ;
#120488 = CARTESIAN_POINT('Origin',(-0.899999999999999,-1.9,-18.45)) ;
#120489 = CARTESIAN_POINT('Origin',(-0.899999999999999,0.4,-18.65)) ;
#120490 = CARTESIAN_POINT('Origin',(-0.899999999999999,0.6,-18.65)) ;
#120491 = CARTESIAN_POINT('Origin',(0.500000000000001,0.4,-19.05)) ;
#120492 = CARTESIAN_POINT('Origin',(0.500000000000001,0.4,-19.45)) ;
#120493 = CARTESIAN_POINT('',(0.600000000000001,0.4,-19.35)) ;
#120494 = CARTESIAN_POINT('Ctrl Pts',(0.595612997216082,0.370705721320406,
-19.4207057213204)) ;
#120495 = CARTESIAN_POINT('Ctrl Pts',(0.596180587760892,0.372558268494356,
-19.4188554988322)) ;
#120496 = CARTESIAN_POINT('Ctrl Pts',(0.596672461925685,0.374355839771979,
-19.4169141798663)) ;
#120497 = CARTESIAN_POINT('Ctrl Pts',(0.599015141889215,0.38386935093007,
-19.4057649936563)) ;
#120498 = CARTESIAN_POINT('Ctrl Pts',(0.599609996542524,0.390224332900451,
-19.3949726026541)) ;
#120499 = CARTESIAN_POINT('Ctrl Pts',(0.600050586298725,0.398117439141558,
-19.3723310532047)) ;
#120500 = CARTESIAN_POINT('Ctrl Pts',(0.600000000000001,0.399999999999999,
-19.3612012506335)) ;
#120501 = CARTESIAN_POINT('Ctrl Pts',(0.600000000000001,0.399999999999999,
-19.35)) ;
#120502 = CARTESIAN_POINT('',(0.600000000000001,0.4,-19.05)) ;
#120503 = CARTESIAN_POINT('Origin',(0.500000000000001,-4.56640444411542E-17,
-18.65)) ;
#120504 = CARTESIAN_POINT('',(0.500000000000001,0.394987437106619,-18.75)) ;
#120505 = CARTESIAN_POINT('Ctrl Pts',(0.500000000000001,0.394987437106619,
-18.75)) ;
#120506 = CARTESIAN_POINT('Ctrl Pts',(0.505940567948962,0.395584486649901,
-18.75)) ;
#120507 = CARTESIAN_POINT('Ctrl Pts',(0.511931971019156,0.39613203607902,
-18.749466300328)) ;
#120508 = CARTESIAN_POINT('Ctrl Pts',(0.517829015308575,0.396618246075357,
-18.7483977957737)) ;
#120509 = CARTESIAN_POINT('Ctrl Pts',(0.522982218721217,0.397043126556055,
-18.7474640701571)) ;
#120510 = CARTESIAN_POINT('Ctrl Pts',(0.528062648970247,0.397421319341388,
-18.7461228267971)) ;
#120511 = CARTESIAN_POINT('Ctrl Pts',(0.532978106724002,0.39775150504607,
-18.7444057438766)) ;
#120512 = CARTESIAN_POINT('Ctrl Pts',(0.538583536338963,0.398128038182999,
-18.7424476378495)) ;
#120513 = CARTESIAN_POINT('Ctrl Pts',(0.544059405914878,0.398447721828296,
-18.7399700083111)) ;
#120514 = CARTESIAN_POINT('Ctrl Pts',(0.549268572255783,0.398712331108984,
-18.7370207319429)) ;
#120515 = CARTESIAN_POINT('Ctrl Pts',(0.553856850427154,0.398945401221756,
-18.7344229841468)) ;
#120516 = CARTESIAN_POINT('Ctrl Pts',(0.558237825069319,0.399135987683843,
-18.73146038498)) ;
#120517 = CARTESIAN_POINT('Ctrl Pts',(0.5623338360862,0.399290378266507,-18.7281952228642)) ;
#120518 = CARTESIAN_POINT('Ctrl Pts',(0.566990328957884,0.399465895042381,
-18.7244832689523)) ;
#120519 = CARTESIAN_POINT('Ctrl Pts',(0.571349096493418,0.399597278936107,
-18.7203228064848)) ;
#120520 = CARTESIAN_POINT('Ctrl Pts',(0.575296920056713,0.399694832180838,
-18.7158055759793)) ;
#120521 = CARTESIAN_POINT('Ctrl Pts',(0.5787442636679,0.399780018245914,-18.7118610112151)) ;
#120522 = CARTESIAN_POINT('Ctrl Pts',(0.581878314560451,0.399839626289636,
-18.7076455218421)) ;
#120523 = CARTESIAN_POINT('Ctrl Pts',(0.584648147334859,0.399882153365958,
-18.7032418177073)) ;
#120524 = CARTESIAN_POINT('Ctrl Pts',(0.587839270208173,0.399931148788079,
-18.6981683125045)) ;
#120525 = CARTESIAN_POINT('Ctrl Pts',(0.590595054415093,0.399958289583404,
-18.6927666362444)) ;
#120526 = CARTESIAN_POINT('Ctrl Pts',(0.59283861894311,0.399974357003159,
-18.6871616850094)) ;
#120527 = CARTESIAN_POINT('Ctrl Pts',(0.594777336851653,0.399988241245861,
-18.6823183122424)) ;
#120528 = CARTESIAN_POINT('Ctrl Pts',(0.596334051506184,0.399993946552814,
-18.6773241662271)) ;
#120529 = CARTESIAN_POINT('Ctrl Pts',(0.597488309822305,0.39999684570125,
-18.6722717185684)) ;
#120530 = CARTESIAN_POINT('Ctrl Pts',(0.598804024094405,0.400000150378306,
-18.6665125419605)) ;
#120531 = CARTESIAN_POINT('Ctrl Pts',(0.599612685195428,0.399999963509465,
-18.6606028438907)) ;
#120532 = CARTESIAN_POINT('Ctrl Pts',(0.59989023099972,0.399999993975383,
-18.6546842022611)) ;
#120533 = CARTESIAN_POINT('Ctrl Pts',(0.5999634645494,0.400000002014155,-18.6531225027898)) ;
#120534 = CARTESIAN_POINT('Ctrl Pts',(0.600000000000001,0.399999999999999,
-18.6515602215092)) ;
#120535 = CARTESIAN_POINT('Ctrl Pts',(0.600000000000001,0.399999999999999,
-18.65)) ;
#120536 = CARTESIAN_POINT('',(0.600000000000001,0.299999999999999,-18.65)) ;
#120537 = CARTESIAN_POINT('Ctrl Pts',(0.500000000000001,0.394987437106619,
-18.75)) ;
#120538 = CARTESIAN_POINT('Ctrl Pts',(0.500454935590171,0.395033159853782,
-18.75)) ;
#120539 = CARTESIAN_POINT('Ctrl Pts',(0.500909898680634,0.395078570329076,
-18.7499968954911)) ;
#120540 = CARTESIAN_POINT('Ctrl Pts',(0.502892456245054,0.395275075889078,
-18.7499698339419)) ;
#120541 = CARTESIAN_POINT('Ctrl Pts',(0.504418747482298,0.395422812032191,
-18.749913985421)) ;
#120542 = CARTESIAN_POINT('Ctrl Pts',(0.508462199543321,0.395804395682031,
-18.7496732810566)) ;
#120543 = CARTESIAN_POINT('Ctrl Pts',(0.510974953343265,0.396031485023314,
-18.7494279391451)) ;
#120544 = CARTESIAN_POINT('Ctrl Pts',(0.521160739721169,0.396903453186227,
-18.7480427944916)) ;
#120545 = CARTESIAN_POINT('Ctrl Pts',(0.528708678528302,0.397444933153157,
-18.7461042177047)) ;
#120546 = CARTESIAN_POINT('Ctrl Pts',(0.54594320635793,0.398105551684103,
-18.7394646394512)) ;
#120547 = CARTESIAN_POINT('Ctrl Pts',(0.555229535466698,0.397987646678449,
-18.7340353588361)) ;
#120548 = CARTESIAN_POINT('Ctrl Pts',(0.571394604995641,0.395490482808055,
-18.7207755133639)) ;
#120549 = CARTESIAN_POINT('Ctrl Pts',(0.578055313702769,0.393198948698403,
-18.7132407456319)) ;
#120550 = CARTESIAN_POINT('Ctrl Pts',(0.58855913220244,0.385442756729361,
-18.6973922339841)) ;
#120551 = CARTESIAN_POINT('Ctrl Pts',(0.592167355639942,0.380240075126989,
-18.6895482656069)) ;
#120552 = CARTESIAN_POINT('Ctrl Pts',(0.59749661553107,0.365892753467073,
-18.6739255217954)) ;
#120553 = CARTESIAN_POINT('Ctrl Pts',(0.598734255154193,0.356660564300806,
-18.666772741727)) ;
#120554 = CARTESIAN_POINT('Ctrl Pts',(0.600012754681677,0.335223914398739,
-18.6555823058657)) ;
#120555 = CARTESIAN_POINT('Ctrl Pts',(0.59999390055981,0.322655037092125,
-18.6516615193656)) ;
#120556 = CARTESIAN_POINT('Ctrl Pts',(0.600000296204999,0.306106913582367,
-18.650139626347)) ;
#120557 = CARTESIAN_POINT('Ctrl Pts',(0.600000000000001,0.303050992413449,
-18.65)) ;
#120558 = CARTESIAN_POINT('Ctrl Pts',(0.600000000000001,0.299999999999999,
-18.65)) ;
#120559 = CARTESIAN_POINT('',(0.600000000000001,-2.39800009914441E-17,-18.65)) ;
#120560 = CARTESIAN_POINT('Origin',(0.500000000000001,-1.9,-18.65)) ;
#120561 = CARTESIAN_POINT('Origin',(0.600000000000001,-1.9,-18.45)) ;
#120562 = CARTESIAN_POINT('Origin',(0.500000000000001,-1.9,-18.45)) ;
#120563 = CARTESIAN_POINT('Origin',(-0.899999999999999,-1.9,-17.675)) ;
#120564 = CARTESIAN_POINT('Origin',(-0.899999999999999,-1.9,-17.775)) ;
#120565 = CARTESIAN_POINT('Origin',(-0.899999999999999,0.6,-18.55)) ;
#120566 = CARTESIAN_POINT('Origin',(-0.899999999999999,0.6,-19.45)) ;
#120567 = CARTESIAN_POINT('Origin',(0.600000000000001,0.4,-19.45)) ;
#120568 = CARTESIAN_POINT('Origin',(0.500000000000001,0.4,-19.45)) ;
#120569 = CARTESIAN_POINT('Origin',(-0.899999999999999,0.4,-19.45)) ;
#120570 = CARTESIAN_POINT('Origin',(0.500000000000001,0.4,-19.45)) ;
#120571 = CARTESIAN_POINT('Origin',(0.500000000000001,-1.9,-18.45)) ;
#120572 = CARTESIAN_POINT('Origin',(0.500000000000001,-2.1,-18.45)) ;
#120573 = CARTESIAN_POINT('Origin',(-0.899999999999999,-1.9,-17.775)) ;
#120574 = CARTESIAN_POINT('Origin',(-1.1,-1.9,-17.775)) ;
#120575 = CARTESIAN_POINT('Origin',(-0.899999999999999,-2.1,-17.775)) ;
#120576 = CARTESIAN_POINT('Origin',(-0.899999999999999,0.4,-19.45)) ;
#120577 = CARTESIAN_POINT('Origin',(-0.899999999999999,0.4,-19.65)) ;
#120578 = CARTESIAN_POINT('Origin',(0.500000000000001,-2.1,-19.05)) ;
#120579 = CARTESIAN_POINT('Origin',(0.500000000000001,-2.1,-17.775)) ;
#120580 = CARTESIAN_POINT('Origin',(0.600000000000001,-2.1,-17.775)) ;
#120581 = CARTESIAN_POINT('Origin',(0.500000000000001,-2.1,-17.775)) ;
#120582 = CARTESIAN_POINT('Origin',(-1.1,-4.42727195005762E-17,-17.775)) ;
#120583 = CARTESIAN_POINT('',(-1.1,1.15,-17.675)) ;
#120584 = CARTESIAN_POINT('',(-1.1,1.25,-17.675)) ;
#120585 = CARTESIAN_POINT('Origin',(-1.1,1.15,-17.775)) ;
#120586 = CARTESIAN_POINT('Origin',(-0.899999999999999,0.5,-19.65)) ;
#120587 = CARTESIAN_POINT('Origin',(-0.899999999999999,-1.9,-19.65)) ;
#120588 = CARTESIAN_POINT('Origin',(0.600000000000001,-1.9,-19.65)) ;
#120589 = CARTESIAN_POINT('Origin',(0.500000000000001,-1.9,-19.65)) ;
#120590 = CARTESIAN_POINT('Origin',(-0.899999999999999,-1.9,-19.65)) ;
#120591 = CARTESIAN_POINT('Origin',(0.500000000000001,-1.9,-19.65)) ;
#120592 = CARTESIAN_POINT('Origin',(0.500000000000001,-2.1,-19.65)) ;
#120593 = CARTESIAN_POINT('Origin',(0.500000000000001,-2.1,-17.775)) ;
#120594 = CARTESIAN_POINT('Origin',(0.500000000000001,-2.1,-17.775)) ;
#120595 = CARTESIAN_POINT('Origin',(-1.1,-2.9,-17.575)) ;
#120596 = CARTESIAN_POINT('Origin',(-1.1,-2.9,-17.575)) ;
#120597 = CARTESIAN_POINT('Origin',(-1.1,-2.9,-17.575)) ;
#120598 = CARTESIAN_POINT('Origin',(-1.1,1.25,-17.575)) ;
#120599 = CARTESIAN_POINT('Origin',(-1.1,1.15,-17.575)) ;
#120600 = CARTESIAN_POINT('Origin',(-1.1,1.15,-17.775)) ;
#120601 = CARTESIAN_POINT('',(-1.1,1.25,-17.775)) ;
#120602 = CARTESIAN_POINT('Origin',(-1.1,1.15,-17.775)) ;
#120603 = CARTESIAN_POINT('Origin',(-1.1,1.15,-17.775)) ;
#120604 = CARTESIAN_POINT('Origin',(-0.899999999999999,-1.9,-19.65)) ;
#120605 = CARTESIAN_POINT('Origin',(-0.899999999999999,-1.9,-19.65)) ;
#120606 = CARTESIAN_POINT('Origin',(0.500000000000001,-2.1,-19.05)) ;
#120607 = CARTESIAN_POINT('Origin',(0.500000000000001,-2.1,-20.325)) ;
#120608 = CARTESIAN_POINT('Origin',(0.500000000000001,1.36481920536411E-16,
-17.775)) ;
#120609 = CARTESIAN_POINT('Origin',(0.500000000000001,-2.9,-17.775)) ;
#120610 = CARTESIAN_POINT('Origin',(-0.999999999999999,-2.9,-17.575)) ;
#120611 = CARTESIAN_POINT('Origin',(0.500000000000001,-2.9,-17.575)) ;
#120612 = CARTESIAN_POINT('Origin',(-1.1,1.15,-17.775)) ;
#120613 = CARTESIAN_POINT('Origin',(-1.1,1.35,-17.775)) ;
#120614 = CARTESIAN_POINT('Origin',(-1.1,1.15,-19.05)) ;
#120615 = CARTESIAN_POINT('',(-1.1,1.25,-20.325)) ;
#120616 = CARTESIAN_POINT('',(-1.1,1.25,-20.425)) ;
#120617 = CARTESIAN_POINT('Origin',(-1.1,1.15,-20.325)) ;
#120618 = CARTESIAN_POINT('Origin',(-0.899999999999999,-1.9,-19.55)) ;
#120619 = CARTESIAN_POINT('Origin',(-0.899999999999999,-1.9,-20.325)) ;
#120620 = CARTESIAN_POINT('Origin',(-0.999999999999999,-2.1,-20.325)) ;
#120621 = CARTESIAN_POINT('Origin',(0.500000000000001,-2.1,-20.325)) ;
#120622 = CARTESIAN_POINT('Origin',(-0.899999999999999,-2.1,-20.325)) ;
#120623 = CARTESIAN_POINT('Origin',(0.500000000000001,-2.1,-20.325)) ;
#120624 = CARTESIAN_POINT('Origin',(0.500000000000001,-2.1,-20.325)) ;
#120625 = CARTESIAN_POINT('Origin',(0.500000000000001,-2.9,-17.775)) ;
#120626 = CARTESIAN_POINT('Origin',(0.700000000000002,-2.9,-17.775)) ;
#120627 = CARTESIAN_POINT('Origin',(-1.1,1.35,-20.425)) ;
#120628 = CARTESIAN_POINT('Origin',(-1.1,1.35,-20.325)) ;
#120629 = CARTESIAN_POINT('Origin',(-1.1,1.15,-20.325)) ;
#120630 = CARTESIAN_POINT('',(-1.1,1.15,-20.425)) ;
#120631 = CARTESIAN_POINT('Origin',(-1.1,1.15,-20.325)) ;
#120632 = CARTESIAN_POINT('Origin',(-1.1,1.15,-20.325)) ;
#120633 = CARTESIAN_POINT('Origin',(-0.899999999999999,-1.9,-20.325)) ;
#120634 = CARTESIAN_POINT('Origin',(-1.1,-1.9,-20.325)) ;
#120635 = CARTESIAN_POINT('Origin',(0.500000000000001,-5.86744705109802E-17,
-20.325)) ;
#120636 = CARTESIAN_POINT('Origin',(0.500000000000001,-2.9,-20.325)) ;
#120637 = CARTESIAN_POINT('Origin',(0.700000000000002,-2.9,-19.05)) ;
#120638 = CARTESIAN_POINT('Origin',(0.700000000000002,-2.9,-20.325)) ;
#120639 = CARTESIAN_POINT('Origin',(-1.1,1.15,-20.325)) ;
#120640 = CARTESIAN_POINT('Origin',(-1.1,1.15,-20.525)) ;
#120641 = CARTESIAN_POINT('Origin',(-1.1,-2.39429110547967E-16,-20.325)) ;
#120642 = CARTESIAN_POINT('',(-1.1,1.25,-20.425)) ;
#120643 = CARTESIAN_POINT('Origin',(0.500000000000001,-2.9,-20.325)) ;
#120644 = CARTESIAN_POINT('Origin',(0.500000000000001,-2.9,-20.525)) ;
#120645 = CARTESIAN_POINT('Origin',(-1.1,1.25,-20.525)) ;
#120646 = CARTESIAN_POINT('Origin',(-1.1,-2.9,-20.525)) ;
#120647 = CARTESIAN_POINT('Origin',(-1.1,-2.9,-20.525)) ;
#120648 = CARTESIAN_POINT('Origin',(-1.1,-2.9,-20.525)) ;
#120649 = CARTESIAN_POINT('Origin',(-1.1,-2.9,-20.525)) ;
#120650 = CARTESIAN_POINT('Origin',(1.5,1.9,-18.45)) ;
#120651 = CARTESIAN_POINT('Origin',(1.5,1.9,-20.6)) ;
#120652 = CARTESIAN_POINT('Origin',(1.5,1.9,-19.65)) ;
#120653 = CARTESIAN_POINT('Origin',(1.5,2.1,-19.65)) ;
#120654 = CARTESIAN_POINT('Origin',(1.5,2.1,-19.45)) ;
#120655 = CARTESIAN_POINT('Origin',(1.5,1.9,-20.6)) ;
#120656 = CARTESIAN_POINT('Origin',(1.5,1.9,-20.6)) ;
#120657 = CARTESIAN_POINT('Origin',(1.5,2.1,-19.45)) ;
#120658 = CARTESIAN_POINT('Origin',(1.5,2.4,-19.45)) ;
#120659 = CARTESIAN_POINT('Origin',(1.5,2.1,-20.6)) ;
#120660 = CARTESIAN_POINT('Origin',(1.5,-2.15,-20.6)) ;
#120661 = CARTESIAN_POINT('Origin',(1.5,2.4,-19.65)) ;
#120662 = CARTESIAN_POINT('Origin',(1.5,2.6,-19.65)) ;
#120663 = CARTESIAN_POINT('Origin',(1.5,-2.15,-20.6)) ;
#120664 = CARTESIAN_POINT('Origin',(1.5,-2.15,-20.6)) ;
#120665 = CARTESIAN_POINT('Origin',(1.5,2.6,-18.45)) ;
#120666 = CARTESIAN_POINT('Origin',(1.5,2.6,-19.7585786437627)) ;
#120667 = CARTESIAN_POINT('Origin',(1.5,-2.15,-18.45)) ;
#120668 = CARTESIAN_POINT('Origin',(1.5,-2.15,-19.9531195934094)) ;
#120669 = CARTESIAN_POINT('Origin',(1.5,2.6,-19.7585786437627)) ;
#120670 = CARTESIAN_POINT('Origin',(1.5,2.6,-19.7585786437627)) ;
#120671 = CARTESIAN_POINT('Origin',(1.5,-2.15,-19.9531195934094)) ;
#120672 = CARTESIAN_POINT('Origin',(1.5,-2.15,-19.9531195934094)) ;
#120673 = CARTESIAN_POINT('Origin',(1.5,1.69571067811865,-18.8542893218813)) ;
#120674 = CARTESIAN_POINT('Origin',(1.5,3.15,-20.3085786437627)) ;
#120675 = CARTESIAN_POINT('Origin',(1.5,-3.65625,-19.05)) ;
#120676 = CARTESIAN_POINT('Origin',(1.5,-2.15,-18.1468804065906)) ;
#120677 = CARTESIAN_POINT('Origin',(1.5,3.15,-20.3085786437627)) ;
#120678 = CARTESIAN_POINT('Origin',(1.5,3.15,-20.3085786437627)) ;
#120679 = CARTESIAN_POINT('Origin',(1.5,-2.15,-18.1468804065906)) ;
#120680 = CARTESIAN_POINT('Origin',(1.5,-2.15,-18.1468804065906)) ;
#120681 = CARTESIAN_POINT('Origin',(1.5,3.15,-18.45)) ;
#120682 = CARTESIAN_POINT('Origin',(1.5,-2.15,-18.45)) ;
#120683 = CARTESIAN_POINT('Origin',(1.5,-2.15,-17.5)) ;
#120684 = CARTESIAN_POINT('Origin',(1.5,-2.15,-17.5)) ;
#120685 = CARTESIAN_POINT('Origin',(1.5,-2.15,-17.5)) ;
#120686 = CARTESIAN_POINT('Origin',(1.5,2.29571067811866,-18.6457106781187)) ;
#120687 = CARTESIAN_POINT('Origin',(1.5,2.6,-18.3414213562373)) ;
#120688 = CARTESIAN_POINT('Origin',(1.5,2.1,-17.5)) ;
#120689 = CARTESIAN_POINT('Origin',(1.5,1.9,-17.5)) ;
#120690 = CARTESIAN_POINT('Origin',(1.5,2.6,-18.3414213562373)) ;
#120691 = CARTESIAN_POINT('Origin',(1.5,2.6,-18.3414213562373)) ;
#120692 = CARTESIAN_POINT('Origin',(1.5,1.9,-17.5)) ;
#120693 = CARTESIAN_POINT('Origin',(1.5,1.9,-17.5)) ;
#120694 = CARTESIAN_POINT('Origin',(1.5,2.6,-18.45)) ;
#120695 = CARTESIAN_POINT('Origin',(1.5,2.6,-18.45)) ;
#120696 = CARTESIAN_POINT('Origin',(1.5,1.9,-18.45)) ;
#120697 = CARTESIAN_POINT('Origin',(1.5,1.9,-18.45)) ;
#120698 = CARTESIAN_POINT('Origin',(1.5,2.4,-18.45)) ;
#120699 = CARTESIAN_POINT('Origin',(1.5,2.4,-18.65)) ;
#120700 = CARTESIAN_POINT('Origin',(1.5,2.1,-18.45)) ;
#120701 = CARTESIAN_POINT('Origin',(1.5,2.1,-18.65)) ;
#120702 = CARTESIAN_POINT('Origin',(1.5,2.1,-18.65)) ;
#120703 = CARTESIAN_POINT('Origin',(-0.899999999999999,-2.,-22.26)) ;
#120704 = CARTESIAN_POINT('Origin',(-0.899999999999999,0.4,-22.26)) ;
#120705 = CARTESIAN_POINT('Origin',(-0.899999999999999,-1.9,-22.26)) ;
#120706 = CARTESIAN_POINT('Origin',(0.600000000000001,0.4,-22.46)) ;
#120707 = CARTESIAN_POINT('Origin',(0.500000000000001,0.4,-22.46)) ;
#120708 = CARTESIAN_POINT('Origin',(-0.899999999999999,0.4,-22.46)) ;
#120709 = CARTESIAN_POINT('Origin',(0.500000000000001,0.4,-22.46)) ;
#120710 = CARTESIAN_POINT('',(0.600000000000001,0.4,-22.46)) ;
#120711 = CARTESIAN_POINT('Origin',(0.500000000000001,0.4,-22.46)) ;
#120712 = CARTESIAN_POINT('Origin',(0.500000000000001,0.4,-22.46)) ;
#120713 = CARTESIAN_POINT('Origin',(-0.899999999999999,-1.9,-22.26)) ;
#120714 = CARTESIAN_POINT('Origin',(-0.899999999999999,-1.9,-22.26)) ;
#120715 = CARTESIAN_POINT('Origin',(-0.899999999999999,-1.9,-22.26)) ;
#120716 = CARTESIAN_POINT('Origin',(-0.899999999999999,0.4,-22.46)) ;
#120717 = CARTESIAN_POINT('Origin',(-0.899999999999999,0.6,-22.46)) ;
#120718 = CARTESIAN_POINT('Origin',(0.500000000000001,0.4,-22.86)) ;
#120719 = CARTESIAN_POINT('Origin',(0.500000000000001,0.4,-23.26)) ;
#120720 = CARTESIAN_POINT('',(0.600000000000001,0.4,-23.16)) ;
#120721 = CARTESIAN_POINT('Ctrl Pts',(0.595612997216081,0.370705721320404,
-23.2307057213204)) ;
#120722 = CARTESIAN_POINT('Ctrl Pts',(0.596180587760893,0.372558268494359,
-23.2288554988322)) ;
#120723 = CARTESIAN_POINT('Ctrl Pts',(0.596672461925686,0.374355839771986,
-23.2269141798663)) ;
#120724 = CARTESIAN_POINT('Ctrl Pts',(0.599015141889206,0.38386935093004,
-23.2157649936563)) ;
#120725 = CARTESIAN_POINT('Ctrl Pts',(0.599609996542524,0.390224332900438,
-23.2049726026542)) ;
#120726 = CARTESIAN_POINT('Ctrl Pts',(0.600050586298726,0.398117439141562,
-23.1823310532047)) ;
#120727 = CARTESIAN_POINT('Ctrl Pts',(0.600000000000001,0.4,-23.1712012506335)) ;
#120728 = CARTESIAN_POINT('Ctrl Pts',(0.600000000000001,0.399999999999999,
-23.16)) ;
#120729 = CARTESIAN_POINT('',(0.600000000000001,0.4,-22.86)) ;
#120730 = CARTESIAN_POINT('Origin',(0.500000000000001,-4.56640444411542E-17,
-22.46)) ;
#120731 = CARTESIAN_POINT('',(0.500000000000001,0.394987437106619,-22.56)) ;
#120732 = CARTESIAN_POINT('Ctrl Pts',(0.500000000000001,0.394987437106619,
-22.56)) ;
#120733 = CARTESIAN_POINT('Ctrl Pts',(0.50594056794894,0.395584486649899,
-22.56)) ;
#120734 = CARTESIAN_POINT('Ctrl Pts',(0.511931971019111,0.396132036079016,
-22.559466300328)) ;
#120735 = CARTESIAN_POINT('Ctrl Pts',(0.517829015308511,0.396618246075352,
-22.5583977957737)) ;
#120736 = CARTESIAN_POINT('Ctrl Pts',(0.522982218721178,0.397043126556052,
-22.5574640701571)) ;
#120737 = CARTESIAN_POINT('Ctrl Pts',(0.528062648970232,0.397421319341387,
-22.5561228267971)) ;
#120738 = CARTESIAN_POINT('Ctrl Pts',(0.532978106724004,0.397751505046071,
-22.5544057438766)) ;
#120739 = CARTESIAN_POINT('Ctrl Pts',(0.538583536338997,0.398128038183002,
-22.5524476378495)) ;
#120740 = CARTESIAN_POINT('Ctrl Pts',(0.544059405914977,0.3984477218283,-22.549970008311)) ;
#120741 = CARTESIAN_POINT('Ctrl Pts',(0.549268572255885,0.398712331108989,
-22.5470207319428)) ;
#120742 = CARTESIAN_POINT('Ctrl Pts',(0.553856850427199,0.398945401221759,
-22.5444229841468)) ;
#120743 = CARTESIAN_POINT('Ctrl Pts',(0.558237825069336,0.399135987683844,
-22.54146038498)) ;
#120744 = CARTESIAN_POINT('Ctrl Pts',(0.562333836086193,0.399290378266507,
-22.5381952228642)) ;
#120745 = CARTESIAN_POINT('Ctrl Pts',(0.56699032895789,0.399465895042382,
-22.5344832689523)) ;
#120746 = CARTESIAN_POINT('Ctrl Pts',(0.571349096493477,0.399597278936108,
-22.5303228064847)) ;
#120747 = CARTESIAN_POINT('Ctrl Pts',(0.575296920056774,0.399694832180838,
-22.5258055759793)) ;
#120748 = CARTESIAN_POINT('Ctrl Pts',(0.578744263667953,0.399780018245914,
-22.521861011215)) ;
#120749 = CARTESIAN_POINT('Ctrl Pts',(0.581878314560456,0.399839626289636,
-22.5176455218421)) ;
#120750 = CARTESIAN_POINT('Ctrl Pts',(0.584648147334871,0.399882153365958,
-22.5132418177073)) ;
#120751 = CARTESIAN_POINT('Ctrl Pts',(0.587839270208222,0.39993114878808,
-22.5081683125044)) ;
#120752 = CARTESIAN_POINT('Ctrl Pts',(0.590595054415142,0.399958289583405,
-22.5027666362444)) ;
#120753 = CARTESIAN_POINT('Ctrl Pts',(0.592838618943166,0.39997435700316,
-22.4971616850092)) ;
#120754 = CARTESIAN_POINT('Ctrl Pts',(0.594777336851685,0.399988241245861,
-22.4923183122423)) ;
#120755 = CARTESIAN_POINT('Ctrl Pts',(0.596334051506206,0.399993946552814,
-22.4873241662271)) ;
#120756 = CARTESIAN_POINT('Ctrl Pts',(0.59748830982231,0.39999684570125,-22.4822717185684)) ;
#120757 = CARTESIAN_POINT('Ctrl Pts',(0.598804024094403,0.400000150378306,
-22.4765125419605)) ;
#120758 = CARTESIAN_POINT('Ctrl Pts',(0.599612685195435,0.399999963509465,
-22.4706028438905)) ;
#120759 = CARTESIAN_POINT('Ctrl Pts',(0.599890230999722,0.399999993975383,
-22.4646842022611)) ;
#120760 = CARTESIAN_POINT('Ctrl Pts',(0.5999634645494,0.400000002014155,-22.4631225027898)) ;
#120761 = CARTESIAN_POINT('Ctrl Pts',(0.600000000000001,0.399999999999999,
-22.4615602215092)) ;
#120762 = CARTESIAN_POINT('Ctrl Pts',(0.600000000000001,0.399999999999999,
-22.46)) ;
#120763 = CARTESIAN_POINT('',(0.600000000000001,0.299999999999999,-22.46)) ;
#120764 = CARTESIAN_POINT('Ctrl Pts',(0.500000000000001,0.394987437106619,
-22.56)) ;
#120765 = CARTESIAN_POINT('Ctrl Pts',(0.50045493558952,0.395033159853717,
-22.56)) ;
#120766 = CARTESIAN_POINT('Ctrl Pts',(0.50090989868031,0.395078570329044,
-22.5599968954911)) ;
#120767 = CARTESIAN_POINT('Ctrl Pts',(0.502892456245184,0.395275075889091,
-22.5599698339419)) ;
#120768 = CARTESIAN_POINT('Ctrl Pts',(0.504418747482384,0.395422812032199,
-22.559913985421)) ;
#120769 = CARTESIAN_POINT('Ctrl Pts',(0.508462199543371,0.395804395682036,
-22.5596732810566)) ;
#120770 = CARTESIAN_POINT('Ctrl Pts',(0.510974953343326,0.396031485023319,
-22.5594279391451)) ;
#120771 = CARTESIAN_POINT('Ctrl Pts',(0.521160739721382,0.396903453186245,
-22.5580427944915)) ;
#120772 = CARTESIAN_POINT('Ctrl Pts',(0.528708678528517,0.397444933153166,
-22.5561042177046)) ;
#120773 = CARTESIAN_POINT('Ctrl Pts',(0.545943206358243,0.398105551684114,
-22.5494646394511)) ;
#120774 = CARTESIAN_POINT('Ctrl Pts',(0.555229535466965,0.397987646678414,
-22.5440353588359)) ;
#120775 = CARTESIAN_POINT('Ctrl Pts',(0.57139460499589,0.395490482808011,
-22.5307755133637)) ;
#120776 = CARTESIAN_POINT('Ctrl Pts',(0.578055313702948,0.393198948698283,
-22.5232407456316)) ;
#120777 = CARTESIAN_POINT('Ctrl Pts',(0.588559132202604,0.385442756729229,
-22.5073922339839)) ;
#120778 = CARTESIAN_POINT('Ctrl Pts',(0.592167355640029,0.380240075126779,
-22.4995482656067)) ;
#120779 = CARTESIAN_POINT('Ctrl Pts',(0.597496615531157,0.365892753466814,
-22.4839255217951)) ;
#120780 = CARTESIAN_POINT('Ctrl Pts',(0.598734255154217,0.35666056430046,
-22.4767727417268)) ;
#120781 = CARTESIAN_POINT('Ctrl Pts',(0.600012754681695,0.335223914398355,
-22.4655823058655)) ;
#120782 = CARTESIAN_POINT('Ctrl Pts',(0.59999390055981,0.322655037091671,
-22.4616615193655)) ;
#120783 = CARTESIAN_POINT('Ctrl Pts',(0.600000296204999,0.306106913582289,
-22.460139626347)) ;
#120784 = CARTESIAN_POINT('Ctrl Pts',(0.600000000000001,0.303050992413402,
-22.46)) ;
#120785 = CARTESIAN_POINT('Ctrl Pts',(0.600000000000001,0.299999999999999,
-22.46)) ;
#120786 = CARTESIAN_POINT('',(0.600000000000001,-2.39800009914441E-17,-22.46)) ;
#120787 = CARTESIAN_POINT('Origin',(0.500000000000001,-1.9,-22.46)) ;
#120788 = CARTESIAN_POINT('Origin',(0.600000000000001,-1.9,-22.26)) ;
#120789 = CARTESIAN_POINT('Origin',(0.500000000000001,-1.9,-22.26)) ;
#120790 = CARTESIAN_POINT('Origin',(-0.899999999999999,-1.9,-21.485)) ;
#120791 = CARTESIAN_POINT('Origin',(-0.899999999999999,-1.9,-21.585)) ;
#120792 = CARTESIAN_POINT('Origin',(-0.899999999999999,0.6,-22.36)) ;
#120793 = CARTESIAN_POINT('Origin',(-0.899999999999999,0.6,-23.26)) ;
#120794 = CARTESIAN_POINT('Origin',(0.600000000000001,0.4,-23.26)) ;
#120795 = CARTESIAN_POINT('Origin',(0.500000000000001,0.4,-23.26)) ;
#120796 = CARTESIAN_POINT('Origin',(-0.899999999999999,0.4,-23.26)) ;
#120797 = CARTESIAN_POINT('Origin',(0.500000000000001,0.4,-23.26)) ;
#120798 = CARTESIAN_POINT('Origin',(0.500000000000001,-1.9,-22.26)) ;
#120799 = CARTESIAN_POINT('Origin',(0.500000000000001,-2.1,-22.26)) ;
#120800 = CARTESIAN_POINT('Origin',(-0.899999999999999,-1.9,-21.585)) ;
#120801 = CARTESIAN_POINT('Origin',(-1.1,-1.9,-21.585)) ;
#120802 = CARTESIAN_POINT('Origin',(-0.899999999999999,-2.1,-21.585)) ;
#120803 = CARTESIAN_POINT('Origin',(-0.899999999999999,0.4,-23.26)) ;
#120804 = CARTESIAN_POINT('Origin',(-0.899999999999999,0.4,-23.46)) ;
#120805 = CARTESIAN_POINT('Origin',(0.500000000000001,-2.1,-22.86)) ;
#120806 = CARTESIAN_POINT('Origin',(0.500000000000001,-2.1,-21.585)) ;
#120807 = CARTESIAN_POINT('Origin',(0.600000000000001,-2.1,-21.585)) ;
#120808 = CARTESIAN_POINT('Origin',(0.500000000000001,-2.1,-21.585)) ;
#120809 = CARTESIAN_POINT('Origin',(-1.1,-4.42727195005762E-17,-21.585)) ;
#120810 = CARTESIAN_POINT('',(-1.1,1.15,-21.485)) ;
#120811 = CARTESIAN_POINT('',(-1.1,1.25,-21.485)) ;
#120812 = CARTESIAN_POINT('Origin',(-1.1,1.15,-21.585)) ;
#120813 = CARTESIAN_POINT('Origin',(-0.899999999999999,0.5,-23.46)) ;
#120814 = CARTESIAN_POINT('Origin',(-0.899999999999999,-1.9,-23.46)) ;
#120815 = CARTESIAN_POINT('Origin',(0.600000000000001,-1.9,-23.46)) ;
#120816 = CARTESIAN_POINT('Origin',(0.500000000000001,-1.9,-23.46)) ;
#120817 = CARTESIAN_POINT('Origin',(-0.899999999999999,-1.9,-23.46)) ;
#120818 = CARTESIAN_POINT('Origin',(0.500000000000001,-1.9,-23.46)) ;
#120819 = CARTESIAN_POINT('Origin',(0.500000000000001,-2.1,-23.46)) ;
#120820 = CARTESIAN_POINT('Origin',(0.500000000000001,-2.1,-21.585)) ;
#120821 = CARTESIAN_POINT('Origin',(0.500000000000001,-2.1,-21.585)) ;
#120822 = CARTESIAN_POINT('Origin',(-1.1,-2.9,-21.385)) ;
#120823 = CARTESIAN_POINT('Origin',(-1.1,-2.9,-21.385)) ;
#120824 = CARTESIAN_POINT('Origin',(-1.1,-2.9,-21.385)) ;
#120825 = CARTESIAN_POINT('Origin',(-1.1,1.25,-21.385)) ;
#120826 = CARTESIAN_POINT('Origin',(-1.1,1.15,-21.385)) ;
#120827 = CARTESIAN_POINT('Origin',(-1.1,1.15,-21.585)) ;
#120828 = CARTESIAN_POINT('',(-1.1,1.25,-21.585)) ;
#120829 = CARTESIAN_POINT('Origin',(-1.1,1.15,-21.585)) ;
#120830 = CARTESIAN_POINT('Origin',(-1.1,1.15,-21.585)) ;
#120831 = CARTESIAN_POINT('Origin',(-0.899999999999999,-1.9,-23.46)) ;
#120832 = CARTESIAN_POINT('Origin',(-0.899999999999999,-1.9,-23.46)) ;
#120833 = CARTESIAN_POINT('Origin',(0.500000000000001,-2.1,-22.86)) ;
#120834 = CARTESIAN_POINT('Origin',(0.500000000000001,-2.1,-24.135)) ;
#120835 = CARTESIAN_POINT('Origin',(0.500000000000001,1.36481920536411E-16,
-21.585)) ;
#120836 = CARTESIAN_POINT('Origin',(0.500000000000001,-2.9,-21.585)) ;
#120837 = CARTESIAN_POINT('Origin',(-0.999999999999999,-2.9,-21.385)) ;
#120838 = CARTESIAN_POINT('Origin',(0.500000000000001,-2.9,-21.385)) ;
#120839 = CARTESIAN_POINT('Origin',(-1.1,1.15,-21.585)) ;
#120840 = CARTESIAN_POINT('Origin',(-1.1,1.35,-21.585)) ;
#120841 = CARTESIAN_POINT('Origin',(-1.1,1.15,-22.86)) ;
#120842 = CARTESIAN_POINT('',(-1.1,1.25,-24.135)) ;
#120843 = CARTESIAN_POINT('',(-1.1,1.25,-24.235)) ;
#120844 = CARTESIAN_POINT('Origin',(-1.1,1.15,-24.135)) ;
#120845 = CARTESIAN_POINT('Origin',(-0.899999999999999,-1.9,-23.36)) ;
#120846 = CARTESIAN_POINT('Origin',(-0.899999999999999,-1.9,-24.135)) ;
#120847 = CARTESIAN_POINT('Origin',(-0.999999999999999,-2.1,-24.135)) ;
#120848 = CARTESIAN_POINT('Origin',(0.500000000000001,-2.1,-24.135)) ;
#120849 = CARTESIAN_POINT('Origin',(-0.899999999999999,-2.1,-24.135)) ;
#120850 = CARTESIAN_POINT('Origin',(0.500000000000001,-2.1,-24.135)) ;
#120851 = CARTESIAN_POINT('Origin',(0.500000000000001,-2.1,-24.135)) ;
#120852 = CARTESIAN_POINT('Origin',(0.500000000000001,-2.9,-21.585)) ;
#120853 = CARTESIAN_POINT('Origin',(0.700000000000002,-2.9,-21.585)) ;
#120854 = CARTESIAN_POINT('Origin',(-1.1,1.35,-24.235)) ;
#120855 = CARTESIAN_POINT('Origin',(-1.1,1.35,-24.135)) ;
#120856 = CARTESIAN_POINT('Origin',(-1.1,1.15,-24.135)) ;
#120857 = CARTESIAN_POINT('',(-1.1,1.15,-24.235)) ;
#120858 = CARTESIAN_POINT('Origin',(-1.1,1.15,-24.135)) ;
#120859 = CARTESIAN_POINT('Origin',(-1.1,1.15,-24.135)) ;
#120860 = CARTESIAN_POINT('Origin',(-0.899999999999999,-1.9,-24.135)) ;
#120861 = CARTESIAN_POINT('Origin',(-1.1,-1.9,-24.135)) ;
#120862 = CARTESIAN_POINT('Origin',(0.500000000000001,-5.86744705109802E-17,
-24.135)) ;
#120863 = CARTESIAN_POINT('Origin',(0.500000000000001,-2.9,-24.135)) ;
#120864 = CARTESIAN_POINT('Origin',(0.700000000000002,-2.9,-22.86)) ;
#120865 = CARTESIAN_POINT('Origin',(0.700000000000002,-2.9,-24.135)) ;
#120866 = CARTESIAN_POINT('Origin',(-1.1,1.15,-24.135)) ;
#120867 = CARTESIAN_POINT('Origin',(-1.1,1.15,-24.335)) ;
#120868 = CARTESIAN_POINT('Origin',(-1.1,-2.39429110547967E-16,-24.135)) ;
#120869 = CARTESIAN_POINT('',(-1.1,1.25,-24.235)) ;
#120870 = CARTESIAN_POINT('Origin',(0.500000000000001,-2.9,-24.135)) ;
#120871 = CARTESIAN_POINT('Origin',(0.500000000000001,-2.9,-24.335)) ;
#120872 = CARTESIAN_POINT('Origin',(-1.1,1.25,-24.335)) ;
#120873 = CARTESIAN_POINT('Origin',(-1.1,-2.9,-24.335)) ;
#120874 = CARTESIAN_POINT('Origin',(-1.1,-2.9,-24.335)) ;
#120875 = CARTESIAN_POINT('Origin',(-1.1,-2.9,-24.335)) ;
#120876 = CARTESIAN_POINT('Origin',(-1.1,-2.9,-24.335)) ;
#120877 = CARTESIAN_POINT('Origin',(1.5,1.9,-22.26)) ;
#120878 = CARTESIAN_POINT('Origin',(1.5,1.9,-24.41)) ;
#120879 = CARTESIAN_POINT('Origin',(1.5,1.9,-23.46)) ;
#120880 = CARTESIAN_POINT('Origin',(1.5,2.1,-23.46)) ;
#120881 = CARTESIAN_POINT('Origin',(1.5,2.1,-23.26)) ;
#120882 = CARTESIAN_POINT('Origin',(1.5,1.9,-24.41)) ;
#120883 = CARTESIAN_POINT('Origin',(1.5,1.9,-24.41)) ;
#120884 = CARTESIAN_POINT('Origin',(1.5,2.1,-23.26)) ;
#120885 = CARTESIAN_POINT('Origin',(1.5,2.4,-23.26)) ;
#120886 = CARTESIAN_POINT('Origin',(1.5,2.1,-24.41)) ;
#120887 = CARTESIAN_POINT('Origin',(1.5,-2.15,-24.41)) ;
#120888 = CARTESIAN_POINT('Origin',(1.5,2.4,-23.46)) ;
#120889 = CARTESIAN_POINT('Origin',(1.5,2.6,-23.46)) ;
#120890 = CARTESIAN_POINT('Origin',(1.5,-2.15,-24.41)) ;
#120891 = CARTESIAN_POINT('Origin',(1.5,-2.15,-24.41)) ;
#120892 = CARTESIAN_POINT('Origin',(1.5,2.6,-22.26)) ;
#120893 = CARTESIAN_POINT('Origin',(1.5,2.6,-23.5685786437627)) ;
#120894 = CARTESIAN_POINT('Origin',(1.5,-2.15,-22.26)) ;
#120895 = CARTESIAN_POINT('Origin',(1.5,-2.15,-23.7631195934094)) ;
#120896 = CARTESIAN_POINT('Origin',(1.5,2.6,-23.5685786437627)) ;
#120897 = CARTESIAN_POINT('Origin',(1.5,2.6,-23.5685786437627)) ;
#120898 = CARTESIAN_POINT('Origin',(1.5,-2.15,-23.7631195934094)) ;
#120899 = CARTESIAN_POINT('Origin',(1.5,-2.15,-23.7631195934094)) ;
#120900 = CARTESIAN_POINT('Origin',(1.5,1.69571067811865,-22.6642893218813)) ;
#120901 = CARTESIAN_POINT('Origin',(1.5,3.15,-24.1185786437627)) ;
#120902 = CARTESIAN_POINT('Origin',(1.5,-3.65625,-22.86)) ;
#120903 = CARTESIAN_POINT('Origin',(1.5,-2.15,-21.9568804065906)) ;
#120904 = CARTESIAN_POINT('Origin',(1.5,3.15,-24.1185786437627)) ;
#120905 = CARTESIAN_POINT('Origin',(1.5,3.15,-24.1185786437627)) ;
#120906 = CARTESIAN_POINT('Origin',(1.5,-2.15,-21.9568804065906)) ;
#120907 = CARTESIAN_POINT('Origin',(1.5,-2.15,-21.9568804065906)) ;
#120908 = CARTESIAN_POINT('Origin',(1.5,3.15,-22.26)) ;
#120909 = CARTESIAN_POINT('Origin',(1.5,-2.15,-22.26)) ;
#120910 = CARTESIAN_POINT('Origin',(1.5,-2.15,-21.31)) ;
#120911 = CARTESIAN_POINT('Origin',(1.5,-2.15,-21.31)) ;
#120912 = CARTESIAN_POINT('Origin',(1.5,-2.15,-21.31)) ;
#120913 = CARTESIAN_POINT('Origin',(1.5,2.29571067811866,-22.4557106781187)) ;
#120914 = CARTESIAN_POINT('Origin',(1.5,2.6,-22.1514213562373)) ;
#120915 = CARTESIAN_POINT('Origin',(1.5,2.1,-21.31)) ;
#120916 = CARTESIAN_POINT('Origin',(1.5,1.9,-21.31)) ;
#120917 = CARTESIAN_POINT('Origin',(1.5,2.6,-22.1514213562373)) ;
#120918 = CARTESIAN_POINT('Origin',(1.5,2.6,-22.1514213562373)) ;
#120919 = CARTESIAN_POINT('Origin',(1.5,1.9,-21.31)) ;
#120920 = CARTESIAN_POINT('Origin',(1.5,1.9,-21.31)) ;
#120921 = CARTESIAN_POINT('Origin',(1.5,2.6,-22.26)) ;
#120922 = CARTESIAN_POINT('Origin',(1.5,2.6,-22.26)) ;
#120923 = CARTESIAN_POINT('Origin',(1.5,1.9,-22.26)) ;
#120924 = CARTESIAN_POINT('Origin',(1.5,1.9,-22.26)) ;
#120925 = CARTESIAN_POINT('Origin',(1.5,2.4,-22.26)) ;
#120926 = CARTESIAN_POINT('Origin',(1.5,2.4,-22.46)) ;
#120927 = CARTESIAN_POINT('Origin',(1.5,2.1,-22.26)) ;
#120928 = CARTESIAN_POINT('Origin',(1.5,2.1,-22.46)) ;
#120929 = CARTESIAN_POINT('Origin',(1.5,2.1,-22.46)) ;
#120930 = CARTESIAN_POINT('Origin',(-0.899999999999999,-2.,-26.07)) ;
#120931 = CARTESIAN_POINT('Origin',(-0.899999999999999,0.4,-26.07)) ;
#120932 = CARTESIAN_POINT('Origin',(-0.899999999999999,-1.9,-26.07)) ;
#120933 = CARTESIAN_POINT('Origin',(0.600000000000001,0.4,-26.27)) ;
#120934 = CARTESIAN_POINT('Origin',(0.500000000000001,0.4,-26.27)) ;
#120935 = CARTESIAN_POINT('Origin',(-0.899999999999999,0.4,-26.27)) ;
#120936 = CARTESIAN_POINT('Origin',(0.500000000000001,0.4,-26.27)) ;
#120937 = CARTESIAN_POINT('',(0.600000000000001,0.4,-26.27)) ;
#120938 = CARTESIAN_POINT('Origin',(0.500000000000001,0.4,-26.27)) ;
#120939 = CARTESIAN_POINT('Origin',(0.500000000000001,0.4,-26.27)) ;
#120940 = CARTESIAN_POINT('Origin',(-0.899999999999999,-1.9,-26.07)) ;
#120941 = CARTESIAN_POINT('Origin',(-0.899999999999999,-1.9,-26.07)) ;
#120942 = CARTESIAN_POINT('Origin',(-0.899999999999999,-1.9,-26.07)) ;
#120943 = CARTESIAN_POINT('Origin',(-0.899999999999999,0.4,-26.27)) ;
#120944 = CARTESIAN_POINT('Origin',(-0.899999999999999,0.6,-26.27)) ;
#120945 = CARTESIAN_POINT('Origin',(0.500000000000001,0.4,-26.67)) ;
#120946 = CARTESIAN_POINT('Origin',(0.500000000000001,0.4,-27.07)) ;
#120947 = CARTESIAN_POINT('',(0.600000000000001,0.4,-26.97)) ;
#120948 = CARTESIAN_POINT('Ctrl Pts',(0.595612997216081,0.370705721320404,
-27.0407057213204)) ;
#120949 = CARTESIAN_POINT('Ctrl Pts',(0.596180587760891,0.372558268494353,
-27.0388554988322)) ;
#120950 = CARTESIAN_POINT('Ctrl Pts',(0.596672461925684,0.374355839771976,
-27.0369141798663)) ;
#120951 = CARTESIAN_POINT('Ctrl Pts',(0.599015141889213,0.383869350930061,
-27.0257649936563)) ;
#120952 = CARTESIAN_POINT('Ctrl Pts',(0.599609996542524,0.390224332900445,
-27.0149726026541)) ;
#120953 = CARTESIAN_POINT('Ctrl Pts',(0.600050586298725,0.398117439141558,
-26.9923310532047)) ;
#120954 = CARTESIAN_POINT('Ctrl Pts',(0.600000000000001,0.4,-26.9812012506335)) ;
#120955 = CARTESIAN_POINT('Ctrl Pts',(0.600000000000001,0.399999999999999,
-26.97)) ;
#120956 = CARTESIAN_POINT('',(0.600000000000001,0.4,-26.67)) ;
#120957 = CARTESIAN_POINT('Origin',(0.500000000000001,-4.56640444411542E-17,
-26.27)) ;
#120958 = CARTESIAN_POINT('',(0.500000000000001,0.394987437106619,-26.37)) ;
#120959 = CARTESIAN_POINT('Ctrl Pts',(0.500000000000001,0.394987437106619,
-26.37)) ;
#120960 = CARTESIAN_POINT('Ctrl Pts',(0.505940567948943,0.395584486649899,
-26.37)) ;
#120961 = CARTESIAN_POINT('Ctrl Pts',(0.511931971019117,0.396132036079017,
-26.369466300328)) ;
#120962 = CARTESIAN_POINT('Ctrl Pts',(0.517829015308519,0.396618246075352,
-26.3683977957737)) ;
#120963 = CARTESIAN_POINT('Ctrl Pts',(0.522982218721183,0.397043126556052,
-26.3674640701571)) ;
#120964 = CARTESIAN_POINT('Ctrl Pts',(0.528062648970233,0.397421319341387,
-26.3661228267971)) ;
#120965 = CARTESIAN_POINT('Ctrl Pts',(0.532978106724005,0.397751505046071,
-26.3644057438766)) ;
#120966 = CARTESIAN_POINT('Ctrl Pts',(0.538583536338987,0.398128038183001,
-26.3624476378495)) ;
#120967 = CARTESIAN_POINT('Ctrl Pts',(0.544059405914956,0.398447721828298,
-26.359970008311)) ;
#120968 = CARTESIAN_POINT('Ctrl Pts',(0.549268572255855,0.398712331108987,
-26.3570207319429)) ;
#120969 = CARTESIAN_POINT('Ctrl Pts',(0.553856850427182,0.398945401221758,
-26.3544229841468)) ;
#120970 = CARTESIAN_POINT('Ctrl Pts',(0.558237825069334,0.399135987683844,
-26.35146038498)) ;
#120971 = CARTESIAN_POINT('Ctrl Pts',(0.562333836086203,0.399290378266507,
-26.3481952228642)) ;
#120972 = CARTESIAN_POINT('Ctrl Pts',(0.566990328957878,0.399465895042381,
-26.3444832689523)) ;
#120973 = CARTESIAN_POINT('Ctrl Pts',(0.571349096493401,0.399597278936106,
-26.3403228064848)) ;
#120974 = CARTESIAN_POINT('Ctrl Pts',(0.575296920056684,0.399694832180836,
-26.3358055759794)) ;
#120975 = CARTESIAN_POINT('Ctrl Pts',(0.57874426366789,0.399780018245913,
-26.3318610112151)) ;
#120976 = CARTESIAN_POINT('Ctrl Pts',(0.581878314560405,0.399839626289636,
-26.3276455218421)) ;
#120977 = CARTESIAN_POINT('Ctrl Pts',(0.584648147334854,0.399882153365959,
-26.3232418177073)) ;
#120978 = CARTESIAN_POINT('Ctrl Pts',(0.587839270208225,0.39993114878808,
-26.3181683125044)) ;
#120979 = CARTESIAN_POINT('Ctrl Pts',(0.590595054415145,0.399958289583405,
-26.3127666362444)) ;
#120980 = CARTESIAN_POINT('Ctrl Pts',(0.592838618943168,0.39997435700316,
-26.3071616850092)) ;
#120981 = CARTESIAN_POINT('Ctrl Pts',(0.594777336851685,0.399988241245861,
-26.3023183122423)) ;
#120982 = CARTESIAN_POINT('Ctrl Pts',(0.596334051506207,0.399993946552814,
-26.2973241662271)) ;
#120983 = CARTESIAN_POINT('Ctrl Pts',(0.597488309822313,0.39999684570125,
-26.2922717185684)) ;
#120984 = CARTESIAN_POINT('Ctrl Pts',(0.598804024094449,0.400000150378306,
-26.2865125419603)) ;
#120985 = CARTESIAN_POINT('Ctrl Pts',(0.599612685195482,0.399999963509465,
-26.2806028438903)) ;
#120986 = CARTESIAN_POINT('Ctrl Pts',(0.599890230999748,0.399999993975383,
-26.2746842022605)) ;
#120987 = CARTESIAN_POINT('Ctrl Pts',(0.59996346454941,0.400000002014155,
-26.2731225027894)) ;
#120988 = CARTESIAN_POINT('Ctrl Pts',(0.600000000000001,0.399999999999999,
-26.271560221509)) ;
#120989 = CARTESIAN_POINT('Ctrl Pts',(0.600000000000001,0.399999999999999,
-26.27)) ;
#120990 = CARTESIAN_POINT('',(0.600000000000001,0.299999999999999,-26.27)) ;
#120991 = CARTESIAN_POINT('Ctrl Pts',(0.500000000000001,0.394987437106619,
-26.37)) ;
#120992 = CARTESIAN_POINT('Ctrl Pts',(0.500454935590171,0.395033159853782,
-26.37)) ;
#120993 = CARTESIAN_POINT('Ctrl Pts',(0.500909898680634,0.395078570329076,
-26.3699968954911)) ;
#120994 = CARTESIAN_POINT('Ctrl Pts',(0.502892456244958,0.395275075889069,
-26.3699698339419)) ;
#120995 = CARTESIAN_POINT('Ctrl Pts',(0.50441874748225,0.395422812032187,
-26.369913985421)) ;
#120996 = CARTESIAN_POINT('Ctrl Pts',(0.508462199543321,0.395804395682031,
-26.3696732810567)) ;
#120997 = CARTESIAN_POINT('Ctrl Pts',(0.510974953343264,0.396031485023314,
-26.3694279391451)) ;
#120998 = CARTESIAN_POINT('Ctrl Pts',(0.521160739721166,0.396903453186226,
-26.3680427944916)) ;
#120999 = CARTESIAN_POINT('Ctrl Pts',(0.528708678528252,0.397444933153152,
-26.3661042177047)) ;
#121000 = CARTESIAN_POINT('Ctrl Pts',(0.545943206357825,0.398105551684101,
-26.3594646394513)) ;
#121001 = CARTESIAN_POINT('Ctrl Pts',(0.555229535466584,0.397987646678453,
-26.3540353588361)) ;
#121002 = CARTESIAN_POINT('Ctrl Pts',(0.571394604995541,0.395490482808082,
-26.3407755133641)) ;
#121003 = CARTESIAN_POINT('Ctrl Pts',(0.578055313702682,0.393198948698442,
-26.333240745632)) ;
#121004 = CARTESIAN_POINT('Ctrl Pts',(0.588559132202378,0.385442756729426,
-26.3173922339843)) ;
#121005 = CARTESIAN_POINT('Ctrl Pts',(0.592167355639896,0.380240075127069,
-26.309548265607)) ;
#121006 = CARTESIAN_POINT('Ctrl Pts',(0.597496615531045,0.365892753467188,
-26.2939255217955)) ;
#121007 = CARTESIAN_POINT('Ctrl Pts',(0.598734255154177,0.356660564300953,
-26.2867727417271)) ;
#121008 = CARTESIAN_POINT('Ctrl Pts',(0.60001275468168,0.335223914398804,
-26.2755823058657)) ;
#121009 = CARTESIAN_POINT('Ctrl Pts',(0.599993900559809,0.322655037092181,
-26.2716615193656)) ;
#121010 = CARTESIAN_POINT('Ctrl Pts',(0.600000296204999,0.30610691358248,
-26.2701396263471)) ;
#121011 = CARTESIAN_POINT('Ctrl Pts',(0.600000000000001,0.303050992413506,
-26.27)) ;
#121012 = CARTESIAN_POINT('Ctrl Pts',(0.600000000000001,0.299999999999999,
-26.27)) ;
#121013 = CARTESIAN_POINT('',(0.600000000000001,-2.39800009914441E-17,-26.27)) ;
#121014 = CARTESIAN_POINT('Origin',(0.500000000000001,-1.9,-26.27)) ;
#121015 = CARTESIAN_POINT('Origin',(0.600000000000001,-1.9,-26.07)) ;
#121016 = CARTESIAN_POINT('Origin',(0.500000000000001,-1.9,-26.07)) ;
#121017 = CARTESIAN_POINT('Origin',(-0.899999999999999,-1.9,-25.295)) ;
#121018 = CARTESIAN_POINT('Origin',(-0.899999999999999,-1.9,-25.395)) ;
#121019 = CARTESIAN_POINT('Origin',(-0.899999999999999,0.6,-26.17)) ;
#121020 = CARTESIAN_POINT('Origin',(-0.899999999999999,0.6,-27.07)) ;
#121021 = CARTESIAN_POINT('Origin',(0.600000000000001,0.4,-27.07)) ;
#121022 = CARTESIAN_POINT('Origin',(0.500000000000001,0.4,-27.07)) ;
#121023 = CARTESIAN_POINT('Origin',(-0.899999999999999,0.4,-27.07)) ;
#121024 = CARTESIAN_POINT('Origin',(0.500000000000001,0.4,-27.07)) ;
#121025 = CARTESIAN_POINT('Origin',(0.500000000000001,-1.9,-26.07)) ;
#121026 = CARTESIAN_POINT('Origin',(0.500000000000001,-2.1,-26.07)) ;
#121027 = CARTESIAN_POINT('Origin',(-0.899999999999999,-1.9,-25.395)) ;
#121028 = CARTESIAN_POINT('Origin',(-1.1,-1.9,-25.395)) ;
#121029 = CARTESIAN_POINT('Origin',(-0.899999999999999,-2.1,-25.395)) ;
#121030 = CARTESIAN_POINT('Origin',(-0.899999999999999,0.4,-27.07)) ;
#121031 = CARTESIAN_POINT('Origin',(-0.899999999999999,0.4,-27.27)) ;
#121032 = CARTESIAN_POINT('Origin',(0.500000000000001,-2.1,-26.67)) ;
#121033 = CARTESIAN_POINT('Origin',(0.500000000000001,-2.1,-25.395)) ;
#121034 = CARTESIAN_POINT('Origin',(0.600000000000001,-2.1,-25.395)) ;
#121035 = CARTESIAN_POINT('Origin',(0.500000000000001,-2.1,-25.395)) ;
#121036 = CARTESIAN_POINT('Origin',(-1.1,-4.42727195005762E-17,-25.395)) ;
#121037 = CARTESIAN_POINT('',(-1.1,1.15,-25.295)) ;
#121038 = CARTESIAN_POINT('',(-1.1,1.25,-25.295)) ;
#121039 = CARTESIAN_POINT('Origin',(-1.1,1.15,-25.395)) ;
#121040 = CARTESIAN_POINT('Origin',(-0.899999999999999,0.5,-27.27)) ;
#121041 = CARTESIAN_POINT('Origin',(-0.899999999999999,-1.9,-27.27)) ;
#121042 = CARTESIAN_POINT('Origin',(0.600000000000001,-1.9,-27.27)) ;
#121043 = CARTESIAN_POINT('Origin',(0.500000000000001,-1.9,-27.27)) ;
#121044 = CARTESIAN_POINT('Origin',(-0.899999999999999,-1.9,-27.27)) ;
#121045 = CARTESIAN_POINT('Origin',(0.500000000000001,-1.9,-27.27)) ;
#121046 = CARTESIAN_POINT('Origin',(0.500000000000001,-2.1,-27.27)) ;
#121047 = CARTESIAN_POINT('Origin',(0.500000000000001,-2.1,-25.395)) ;
#121048 = CARTESIAN_POINT('Origin',(0.500000000000001,-2.1,-25.395)) ;
#121049 = CARTESIAN_POINT('Origin',(-1.1,-2.9,-25.195)) ;
#121050 = CARTESIAN_POINT('Origin',(-1.1,-2.9,-25.195)) ;
#121051 = CARTESIAN_POINT('Origin',(-1.1,-2.9,-25.195)) ;
#121052 = CARTESIAN_POINT('Origin',(-1.1,1.25,-25.195)) ;
#121053 = CARTESIAN_POINT('Origin',(-1.1,1.15,-25.195)) ;
#121054 = CARTESIAN_POINT('Origin',(-1.1,1.15,-25.395)) ;
#121055 = CARTESIAN_POINT('',(-1.1,1.25,-25.395)) ;
#121056 = CARTESIAN_POINT('Origin',(-1.1,1.15,-25.395)) ;
#121057 = CARTESIAN_POINT('Origin',(-1.1,1.15,-25.395)) ;
#121058 = CARTESIAN_POINT('Origin',(-0.899999999999999,-1.9,-27.27)) ;
#121059 = CARTESIAN_POINT('Origin',(-0.899999999999999,-1.9,-27.27)) ;
#121060 = CARTESIAN_POINT('Origin',(0.500000000000001,-2.1,-26.67)) ;
#121061 = CARTESIAN_POINT('Origin',(0.500000000000001,-2.1,-27.945)) ;
#121062 = CARTESIAN_POINT('Origin',(0.500000000000001,1.36481920536411E-16,
-25.395)) ;
#121063 = CARTESIAN_POINT('Origin',(0.500000000000001,-2.9,-25.395)) ;
#121064 = CARTESIAN_POINT('Origin',(-0.999999999999999,-2.9,-25.195)) ;
#121065 = CARTESIAN_POINT('Origin',(0.500000000000001,-2.9,-25.195)) ;
#121066 = CARTESIAN_POINT('Origin',(-1.1,1.15,-25.395)) ;
#121067 = CARTESIAN_POINT('Origin',(-1.1,1.35,-25.395)) ;
#121068 = CARTESIAN_POINT('Origin',(-1.1,1.15,-26.67)) ;
#121069 = CARTESIAN_POINT('',(-1.1,1.25,-27.945)) ;
#121070 = CARTESIAN_POINT('',(-1.1,1.25,-28.045)) ;
#121071 = CARTESIAN_POINT('Origin',(-1.1,1.15,-27.945)) ;
#121072 = CARTESIAN_POINT('Origin',(-0.899999999999999,-1.9,-27.17)) ;
#121073 = CARTESIAN_POINT('Origin',(-0.899999999999999,-1.9,-27.945)) ;
#121074 = CARTESIAN_POINT('Origin',(-0.999999999999999,-2.1,-27.945)) ;
#121075 = CARTESIAN_POINT('Origin',(0.500000000000001,-2.1,-27.945)) ;
#121076 = CARTESIAN_POINT('Origin',(-0.899999999999999,-2.1,-27.945)) ;
#121077 = CARTESIAN_POINT('Origin',(0.500000000000001,-2.1,-27.945)) ;
#121078 = CARTESIAN_POINT('Origin',(0.500000000000001,-2.1,-27.945)) ;
#121079 = CARTESIAN_POINT('Origin',(0.500000000000001,-2.9,-25.395)) ;
#121080 = CARTESIAN_POINT('Origin',(0.700000000000002,-2.9,-25.395)) ;
#121081 = CARTESIAN_POINT('Origin',(-1.1,1.35,-28.045)) ;
#121082 = CARTESIAN_POINT('Origin',(-1.1,1.35,-27.945)) ;
#121083 = CARTESIAN_POINT('Origin',(-1.1,1.15,-27.945)) ;
#121084 = CARTESIAN_POINT('',(-1.1,1.15,-28.045)) ;
#121085 = CARTESIAN_POINT('Origin',(-1.1,1.15,-27.945)) ;
#121086 = CARTESIAN_POINT('Origin',(-1.1,1.15,-27.945)) ;
#121087 = CARTESIAN_POINT('Origin',(-0.899999999999999,-1.9,-27.945)) ;
#121088 = CARTESIAN_POINT('Origin',(-1.1,-1.9,-27.945)) ;
#121089 = CARTESIAN_POINT('Origin',(0.500000000000001,-5.86744705109802E-17,
-27.945)) ;
#121090 = CARTESIAN_POINT('Origin',(0.500000000000001,-2.9,-27.945)) ;
#121091 = CARTESIAN_POINT('Origin',(0.700000000000002,-2.9,-26.67)) ;
#121092 = CARTESIAN_POINT('Origin',(0.700000000000002,-2.9,-27.945)) ;
#121093 = CARTESIAN_POINT('Origin',(-1.1,1.15,-27.945)) ;
#121094 = CARTESIAN_POINT('Origin',(-1.1,1.15,-28.145)) ;
#121095 = CARTESIAN_POINT('Origin',(-1.1,-2.39429110547967E-16,-27.945)) ;
#121096 = CARTESIAN_POINT('',(-1.1,1.25,-28.045)) ;
#121097 = CARTESIAN_POINT('Origin',(0.500000000000001,-2.9,-27.945)) ;
#121098 = CARTESIAN_POINT('Origin',(0.500000000000001,-2.9,-28.145)) ;
#121099 = CARTESIAN_POINT('Origin',(-1.1,1.25,-28.145)) ;
#121100 = CARTESIAN_POINT('Origin',(-1.1,-2.9,-28.145)) ;
#121101 = CARTESIAN_POINT('Origin',(-1.1,-2.9,-28.145)) ;
#121102 = CARTESIAN_POINT('Origin',(-1.1,-2.9,-28.145)) ;
#121103 = CARTESIAN_POINT('Origin',(-1.1,-2.9,-28.145)) ;
#121104 = CARTESIAN_POINT('Origin',(1.5,1.9,-26.07)) ;
#121105 = CARTESIAN_POINT('Origin',(1.5,1.9,-28.22)) ;
#121106 = CARTESIAN_POINT('Origin',(1.5,1.9,-27.27)) ;
#121107 = CARTESIAN_POINT('Origin',(1.5,2.1,-27.27)) ;
#121108 = CARTESIAN_POINT('Origin',(1.5,2.1,-27.07)) ;
#121109 = CARTESIAN_POINT('Origin',(1.5,1.9,-28.22)) ;
#121110 = CARTESIAN_POINT('Origin',(1.5,1.9,-28.22)) ;
#121111 = CARTESIAN_POINT('Origin',(1.5,2.1,-27.07)) ;
#121112 = CARTESIAN_POINT('Origin',(1.5,2.4,-27.07)) ;
#121113 = CARTESIAN_POINT('Origin',(1.5,2.1,-28.22)) ;
#121114 = CARTESIAN_POINT('Origin',(1.5,-2.15,-28.22)) ;
#121115 = CARTESIAN_POINT('Origin',(1.5,2.4,-27.27)) ;
#121116 = CARTESIAN_POINT('Origin',(1.5,2.6,-27.27)) ;
#121117 = CARTESIAN_POINT('Origin',(1.5,-2.15,-28.22)) ;
#121118 = CARTESIAN_POINT('Origin',(1.5,-2.15,-28.22)) ;
#121119 = CARTESIAN_POINT('Origin',(1.5,2.6,-26.07)) ;
#121120 = CARTESIAN_POINT('Origin',(1.5,2.6,-27.3785786437627)) ;
#121121 = CARTESIAN_POINT('Origin',(1.5,-2.15,-26.07)) ;
#121122 = CARTESIAN_POINT('Origin',(1.5,-2.15,-27.5731195934094)) ;
#121123 = CARTESIAN_POINT('Origin',(1.5,2.6,-27.3785786437627)) ;
#121124 = CARTESIAN_POINT('Origin',(1.5,2.6,-27.3785786437627)) ;
#121125 = CARTESIAN_POINT('Origin',(1.5,-2.15,-27.5731195934094)) ;
#121126 = CARTESIAN_POINT('Origin',(1.5,-2.15,-27.5731195934094)) ;
#121127 = CARTESIAN_POINT('Origin',(1.5,1.69571067811865,-26.4742893218813)) ;
#121128 = CARTESIAN_POINT('Origin',(1.5,3.15,-27.9285786437627)) ;
#121129 = CARTESIAN_POINT('Origin',(1.5,-3.65625,-26.67)) ;
#121130 = CARTESIAN_POINT('Origin',(1.5,-2.15,-25.7668804065906)) ;
#121131 = CARTESIAN_POINT('Origin',(1.5,3.15,-27.9285786437627)) ;
#121132 = CARTESIAN_POINT('Origin',(1.5,3.15,-27.9285786437627)) ;
#121133 = CARTESIAN_POINT('Origin',(1.5,-2.15,-25.7668804065906)) ;
#121134 = CARTESIAN_POINT('Origin',(1.5,-2.15,-25.7668804065906)) ;
#121135 = CARTESIAN_POINT('Origin',(1.5,3.15,-26.07)) ;
#121136 = CARTESIAN_POINT('Origin',(1.5,-2.15,-26.07)) ;
#121137 = CARTESIAN_POINT('Origin',(1.5,-2.15,-25.12)) ;
#121138 = CARTESIAN_POINT('Origin',(1.5,-2.15,-25.12)) ;
#121139 = CARTESIAN_POINT('Origin',(1.5,-2.15,-25.12)) ;
#121140 = CARTESIAN_POINT('Origin',(1.5,2.29571067811866,-26.2657106781187)) ;
#121141 = CARTESIAN_POINT('Origin',(1.5,2.6,-25.9614213562373)) ;
#121142 = CARTESIAN_POINT('Origin',(1.5,2.1,-25.12)) ;
#121143 = CARTESIAN_POINT('Origin',(1.5,1.9,-25.12)) ;
#121144 = CARTESIAN_POINT('Origin',(1.5,2.6,-25.9614213562373)) ;
#121145 = CARTESIAN_POINT('Origin',(1.5,2.6,-25.9614213562373)) ;
#121146 = CARTESIAN_POINT('Origin',(1.5,1.9,-25.12)) ;
#121147 = CARTESIAN_POINT('Origin',(1.5,1.9,-25.12)) ;
#121148 = CARTESIAN_POINT('Origin',(1.5,2.6,-26.07)) ;
#121149 = CARTESIAN_POINT('Origin',(1.5,2.6,-26.07)) ;
#121150 = CARTESIAN_POINT('Origin',(1.5,1.9,-26.07)) ;
#121151 = CARTESIAN_POINT('Origin',(1.5,1.9,-26.07)) ;
#121152 = CARTESIAN_POINT('Origin',(1.5,2.4,-26.07)) ;
#121153 = CARTESIAN_POINT('Origin',(1.5,2.4,-26.27)) ;
#121154 = CARTESIAN_POINT('Origin',(1.5,2.1,-26.07)) ;
#121155 = CARTESIAN_POINT('Origin',(1.5,2.1,-26.27)) ;
#121156 = CARTESIAN_POINT('Origin',(1.5,2.1,-26.27)) ;
#121157 = CARTESIAN_POINT('Origin',(-0.899999999999999,-2.,-29.88)) ;
#121158 = CARTESIAN_POINT('Origin',(-0.899999999999999,0.4,-29.88)) ;
#121159 = CARTESIAN_POINT('Origin',(-0.899999999999999,-1.9,-29.88)) ;
#121160 = CARTESIAN_POINT('Origin',(0.600000000000001,0.4,-30.08)) ;
#121161 = CARTESIAN_POINT('Origin',(0.500000000000001,0.4,-30.08)) ;
#121162 = CARTESIAN_POINT('Origin',(-0.899999999999999,0.4,-30.08)) ;
#121163 = CARTESIAN_POINT('Origin',(0.500000000000001,0.4,-30.08)) ;
#121164 = CARTESIAN_POINT('',(0.600000000000001,0.4,-30.08)) ;
#121165 = CARTESIAN_POINT('Origin',(0.500000000000001,0.4,-30.08)) ;
#121166 = CARTESIAN_POINT('Origin',(0.500000000000001,0.4,-30.08)) ;
#121167 = CARTESIAN_POINT('Origin',(-0.899999999999999,-1.9,-29.88)) ;
#121168 = CARTESIAN_POINT('Origin',(-0.899999999999999,-1.9,-29.88)) ;
#121169 = CARTESIAN_POINT('Origin',(-0.899999999999999,-1.9,-29.88)) ;
#121170 = CARTESIAN_POINT('Origin',(-0.899999999999999,0.4,-30.08)) ;
#121171 = CARTESIAN_POINT('Origin',(-0.899999999999999,0.6,-30.08)) ;
#121172 = CARTESIAN_POINT('Origin',(0.500000000000001,0.4,-30.48)) ;
#121173 = CARTESIAN_POINT('Origin',(0.500000000000001,0.4,-30.88)) ;
#121174 = CARTESIAN_POINT('',(0.600000000000001,0.4,-30.78)) ;
#121175 = CARTESIAN_POINT('Ctrl Pts',(0.595612997216081,0.370705721320405,
-30.8507057213204)) ;
#121176 = CARTESIAN_POINT('Ctrl Pts',(0.596180587760891,0.372558268494354,
-30.8488554988322)) ;
#121177 = CARTESIAN_POINT('Ctrl Pts',(0.596672461925684,0.374355839771976,
-30.8469141798663)) ;
#121178 = CARTESIAN_POINT('Ctrl Pts',(0.599015141889203,0.383869350930023,
-30.8357649936563)) ;
#121179 = CARTESIAN_POINT('Ctrl Pts',(0.599609996542522,0.390224332900425,
-30.8249726026542)) ;
#121180 = CARTESIAN_POINT('Ctrl Pts',(0.600050586298725,0.398117439141557,
-30.8023310532047)) ;
#121181 = CARTESIAN_POINT('Ctrl Pts',(0.600000000000001,0.399999999999999,
-30.7912012506335)) ;
#121182 = CARTESIAN_POINT('Ctrl Pts',(0.600000000000001,0.399999999999999,
-30.78)) ;
#121183 = CARTESIAN_POINT('',(0.600000000000001,0.4,-30.48)) ;
#121184 = CARTESIAN_POINT('Origin',(0.500000000000001,-4.56640444411542E-17,
-30.08)) ;
#121185 = CARTESIAN_POINT('',(0.500000000000001,0.394987437106619,-30.18)) ;
#121186 = CARTESIAN_POINT('Ctrl Pts',(0.500000000000001,0.394987437106619,
-30.18)) ;
#121187 = CARTESIAN_POINT('Ctrl Pts',(0.505940567948935,0.395584486649899,
-30.18)) ;
#121188 = CARTESIAN_POINT('Ctrl Pts',(0.511931971019101,0.396132036079015,
-30.179466300328)) ;
#121189 = CARTESIAN_POINT('Ctrl Pts',(0.517829015308496,0.39661824607535,
-30.1783977957737)) ;
#121190 = CARTESIAN_POINT('Ctrl Pts',(0.522982218721168,0.397043126556051,
-30.1774640701571)) ;
#121191 = CARTESIAN_POINT('Ctrl Pts',(0.528062648970226,0.397421319341387,
-30.1761228267971)) ;
#121192 = CARTESIAN_POINT('Ctrl Pts',(0.532978106724004,0.397751505046071,
-30.1744057438766)) ;
#121193 = CARTESIAN_POINT('Ctrl Pts',(0.538583536338982,0.398128038183001,
-30.1724476378495)) ;
#121194 = CARTESIAN_POINT('Ctrl Pts',(0.544059405914951,0.398447721828298,
-30.169970008311)) ;
#121195 = CARTESIAN_POINT('Ctrl Pts',(0.549268572255847,0.398712331108986,
-30.1670207319429)) ;
#121196 = CARTESIAN_POINT('Ctrl Pts',(0.553856850427178,0.398945401221757,
-30.1644229841468)) ;
#121197 = CARTESIAN_POINT('Ctrl Pts',(0.558237825069329,0.399135987683843,
-30.16146038498)) ;
#121198 = CARTESIAN_POINT('Ctrl Pts',(0.562333836086197,0.399290378266506,
-30.1581952228642)) ;
#121199 = CARTESIAN_POINT('Ctrl Pts',(0.566990328957886,0.399465895042381,
-30.1544832689523)) ;
#121200 = CARTESIAN_POINT('Ctrl Pts',(0.57134909649342,0.399597278936108,
-30.1503228064848)) ;
#121201 = CARTESIAN_POINT('Ctrl Pts',(0.575296920056715,0.399694832180838,
-30.1458055759793)) ;
#121202 = CARTESIAN_POINT('Ctrl Pts',(0.5787442636679,0.399780018245914,-30.1418610112151)) ;
#121203 = CARTESIAN_POINT('Ctrl Pts',(0.581878314560451,0.399839626289636,
-30.1376455218421)) ;
#121204 = CARTESIAN_POINT('Ctrl Pts',(0.584648147334861,0.399882153365958,
-30.1332418177073)) ;
#121205 = CARTESIAN_POINT('Ctrl Pts',(0.587839270208171,0.399931148788079,
-30.1281683125045)) ;
#121206 = CARTESIAN_POINT('Ctrl Pts',(0.590595054415091,0.399958289583404,
-30.1227666362445)) ;
#121207 = CARTESIAN_POINT('Ctrl Pts',(0.592838618943106,0.399974357003159,
-30.1171616850094)) ;
#121208 = CARTESIAN_POINT('Ctrl Pts',(0.594777336851655,0.399988241245861,
-30.1123183122424)) ;
#121209 = CARTESIAN_POINT('Ctrl Pts',(0.596334051506183,0.399993946552814,
-30.1073241662271)) ;
#121210 = CARTESIAN_POINT('Ctrl Pts',(0.597488309822302,0.39999684570125,
-30.1022717185684)) ;
#121211 = CARTESIAN_POINT('Ctrl Pts',(0.598804024094428,0.400000150378306,
-30.0965125419604)) ;
#121212 = CARTESIAN_POINT('Ctrl Pts',(0.599612685195468,0.399999963509465,
-30.0906028438904)) ;
#121213 = CARTESIAN_POINT('Ctrl Pts',(0.599890230999741,0.399999993975383,
-30.0846842022606)) ;
#121214 = CARTESIAN_POINT('Ctrl Pts',(0.599963464549407,0.400000002014155,
-30.0831225027895)) ;
#121215 = CARTESIAN_POINT('Ctrl Pts',(0.600000000000001,0.399999999999999,
-30.081560221509)) ;
#121216 = CARTESIAN_POINT('Ctrl Pts',(0.600000000000001,0.399999999999999,
-30.08)) ;
#121217 = CARTESIAN_POINT('',(0.600000000000001,0.299999999999999,-30.08)) ;
#121218 = CARTESIAN_POINT('Ctrl Pts',(0.500000000000001,0.394987437106619,
-30.18)) ;
#121219 = CARTESIAN_POINT('Ctrl Pts',(0.500454935590171,0.395033159853782,
-30.18)) ;
#121220 = CARTESIAN_POINT('Ctrl Pts',(0.500909898680634,0.395078570329076,
-30.1799968954911)) ;
#121221 = CARTESIAN_POINT('Ctrl Pts',(0.502892456244958,0.395275075889069,
-30.1799698339419)) ;
#121222 = CARTESIAN_POINT('Ctrl Pts',(0.50441874748225,0.395422812032187,
-30.179913985421)) ;
#121223 = CARTESIAN_POINT('Ctrl Pts',(0.508462199543321,0.395804395682031,
-30.1796732810567)) ;
#121224 = CARTESIAN_POINT('Ctrl Pts',(0.510974953343264,0.396031485023314,
-30.1794279391451)) ;
#121225 = CARTESIAN_POINT('Ctrl Pts',(0.521160739721166,0.396903453186226,
-30.1780427944916)) ;
#121226 = CARTESIAN_POINT('Ctrl Pts',(0.528708678528252,0.397444933153152,
-30.1761042177047)) ;
#121227 = CARTESIAN_POINT('Ctrl Pts',(0.545943206357825,0.398105551684101,
-30.1694646394513)) ;
#121228 = CARTESIAN_POINT('Ctrl Pts',(0.555229535466584,0.397987646678453,
-30.1640353588361)) ;
#121229 = CARTESIAN_POINT('Ctrl Pts',(0.571394604995541,0.395490482808082,
-30.150775513364)) ;
#121230 = CARTESIAN_POINT('Ctrl Pts',(0.578055313702682,0.393198948698442,
-30.143240745632)) ;
#121231 = CARTESIAN_POINT('Ctrl Pts',(0.588559132202378,0.385442756729426,
-30.1273922339842)) ;
#121232 = CARTESIAN_POINT('Ctrl Pts',(0.592167355639896,0.380240075127069,
-30.119548265607)) ;
#121233 = CARTESIAN_POINT('Ctrl Pts',(0.597496615531045,0.365892753467188,
-30.1039255217955)) ;
#121234 = CARTESIAN_POINT('Ctrl Pts',(0.598734255154177,0.356660564300953,
-30.0967727417271)) ;
#121235 = CARTESIAN_POINT('Ctrl Pts',(0.60001275468168,0.335223914398804,
-30.0855823058657)) ;
#121236 = CARTESIAN_POINT('Ctrl Pts',(0.599993900559809,0.322655037092181,
-30.0816615193656)) ;
#121237 = CARTESIAN_POINT('Ctrl Pts',(0.600000296204999,0.30610691358248,
-30.0801396263471)) ;
#121238 = CARTESIAN_POINT('Ctrl Pts',(0.600000000000001,0.303050992413506,
-30.08)) ;
#121239 = CARTESIAN_POINT('Ctrl Pts',(0.600000000000001,0.299999999999999,
-30.08)) ;
#121240 = CARTESIAN_POINT('',(0.600000000000001,-2.39800009914441E-17,-30.08)) ;
#121241 = CARTESIAN_POINT('Origin',(0.500000000000001,-1.9,-30.08)) ;
#121242 = CARTESIAN_POINT('Origin',(0.600000000000001,-1.9,-29.88)) ;
#121243 = CARTESIAN_POINT('Origin',(0.500000000000001,-1.9,-29.88)) ;
#121244 = CARTESIAN_POINT('Origin',(-0.899999999999999,-1.9,-29.105)) ;
#121245 = CARTESIAN_POINT('Origin',(-0.899999999999999,-1.9,-29.205)) ;
#121246 = CARTESIAN_POINT('Origin',(-0.899999999999999,0.6,-29.98)) ;
#121247 = CARTESIAN_POINT('Origin',(-0.899999999999999,0.6,-30.88)) ;
#121248 = CARTESIAN_POINT('Origin',(0.600000000000001,0.4,-30.88)) ;
#121249 = CARTESIAN_POINT('Origin',(0.500000000000001,0.4,-30.88)) ;
#121250 = CARTESIAN_POINT('Origin',(-0.899999999999999,0.4,-30.88)) ;
#121251 = CARTESIAN_POINT('Origin',(0.500000000000001,0.4,-30.88)) ;
#121252 = CARTESIAN_POINT('Origin',(0.500000000000001,-1.9,-29.88)) ;
#121253 = CARTESIAN_POINT('Origin',(0.500000000000001,-2.1,-29.88)) ;
#121254 = CARTESIAN_POINT('Origin',(-0.899999999999999,-1.9,-29.205)) ;
#121255 = CARTESIAN_POINT('Origin',(-1.1,-1.9,-29.205)) ;
#121256 = CARTESIAN_POINT('Origin',(-0.899999999999999,-2.1,-29.205)) ;
#121257 = CARTESIAN_POINT('Origin',(-0.899999999999999,0.4,-30.88)) ;
#121258 = CARTESIAN_POINT('Origin',(-0.899999999999999,0.4,-31.08)) ;
#121259 = CARTESIAN_POINT('Origin',(0.500000000000001,-2.1,-30.48)) ;
#121260 = CARTESIAN_POINT('Origin',(0.500000000000001,-2.1,-29.205)) ;
#121261 = CARTESIAN_POINT('Origin',(0.600000000000001,-2.1,-29.205)) ;
#121262 = CARTESIAN_POINT('Origin',(0.500000000000001,-2.1,-29.205)) ;
#121263 = CARTESIAN_POINT('Origin',(-1.1,-4.42727195005762E-17,-29.205)) ;
#121264 = CARTESIAN_POINT('',(-1.1,1.15,-29.105)) ;
#121265 = CARTESIAN_POINT('',(-1.1,1.25,-29.105)) ;
#121266 = CARTESIAN_POINT('Origin',(-1.1,1.15,-29.205)) ;
#121267 = CARTESIAN_POINT('Origin',(-0.899999999999999,0.5,-31.08)) ;
#121268 = CARTESIAN_POINT('Origin',(-0.899999999999999,-1.9,-31.08)) ;
#121269 = CARTESIAN_POINT('Origin',(0.600000000000001,-1.9,-31.08)) ;
#121270 = CARTESIAN_POINT('Origin',(0.500000000000001,-1.9,-31.08)) ;
#121271 = CARTESIAN_POINT('Origin',(-0.899999999999999,-1.9,-31.08)) ;
#121272 = CARTESIAN_POINT('Origin',(0.500000000000001,-1.9,-31.08)) ;
#121273 = CARTESIAN_POINT('Origin',(0.500000000000001,-2.1,-31.08)) ;
#121274 = CARTESIAN_POINT('Origin',(0.500000000000001,-2.1,-29.205)) ;
#121275 = CARTESIAN_POINT('Origin',(0.500000000000001,-2.1,-29.205)) ;
#121276 = CARTESIAN_POINT('Origin',(-1.1,-2.9,-29.005)) ;
#121277 = CARTESIAN_POINT('Origin',(-1.1,-2.9,-29.005)) ;
#121278 = CARTESIAN_POINT('Origin',(-1.1,-2.9,-29.005)) ;
#121279 = CARTESIAN_POINT('Origin',(-1.1,1.25,-29.005)) ;
#121280 = CARTESIAN_POINT('Origin',(-1.1,1.15,-29.005)) ;
#121281 = CARTESIAN_POINT('Origin',(-1.1,1.15,-29.205)) ;
#121282 = CARTESIAN_POINT('',(-1.1,1.25,-29.205)) ;
#121283 = CARTESIAN_POINT('Origin',(-1.1,1.15,-29.205)) ;
#121284 = CARTESIAN_POINT('Origin',(-1.1,1.15,-29.205)) ;
#121285 = CARTESIAN_POINT('Origin',(-0.899999999999999,-1.9,-31.08)) ;
#121286 = CARTESIAN_POINT('Origin',(-0.899999999999999,-1.9,-31.08)) ;
#121287 = CARTESIAN_POINT('Origin',(0.500000000000001,-2.1,-30.48)) ;
#121288 = CARTESIAN_POINT('Origin',(0.500000000000001,-2.1,-31.755)) ;
#121289 = CARTESIAN_POINT('Origin',(0.500000000000001,1.36481920536411E-16,
-29.205)) ;
#121290 = CARTESIAN_POINT('Origin',(0.500000000000001,-2.9,-29.205)) ;
#121291 = CARTESIAN_POINT('Origin',(-0.999999999999999,-2.9,-29.005)) ;
#121292 = CARTESIAN_POINT('Origin',(0.500000000000001,-2.9,-29.005)) ;
#121293 = CARTESIAN_POINT('Origin',(-1.1,1.15,-29.205)) ;
#121294 = CARTESIAN_POINT('Origin',(-1.1,1.35,-29.205)) ;
#121295 = CARTESIAN_POINT('Origin',(-1.1,1.15,-30.48)) ;
#121296 = CARTESIAN_POINT('',(-1.1,1.25,-31.755)) ;
#121297 = CARTESIAN_POINT('',(-1.1,1.25,-31.855)) ;
#121298 = CARTESIAN_POINT('Origin',(-1.1,1.15,-31.755)) ;
#121299 = CARTESIAN_POINT('Origin',(-0.899999999999999,-1.9,-30.98)) ;
#121300 = CARTESIAN_POINT('Origin',(-0.899999999999999,-1.9,-31.755)) ;
#121301 = CARTESIAN_POINT('Origin',(-0.999999999999999,-2.1,-31.755)) ;
#121302 = CARTESIAN_POINT('Origin',(0.500000000000001,-2.1,-31.755)) ;
#121303 = CARTESIAN_POINT('Origin',(-0.899999999999999,-2.1,-31.755)) ;
#121304 = CARTESIAN_POINT('Origin',(0.500000000000001,-2.1,-31.755)) ;
#121305 = CARTESIAN_POINT('Origin',(0.500000000000001,-2.1,-31.755)) ;
#121306 = CARTESIAN_POINT('Origin',(0.500000000000001,-2.9,-29.205)) ;
#121307 = CARTESIAN_POINT('Origin',(0.700000000000002,-2.9,-29.205)) ;
#121308 = CARTESIAN_POINT('Origin',(-1.1,1.35,-31.855)) ;
#121309 = CARTESIAN_POINT('Origin',(-1.1,1.35,-31.755)) ;
#121310 = CARTESIAN_POINT('Origin',(-1.1,1.15,-31.755)) ;
#121311 = CARTESIAN_POINT('',(-1.1,1.15,-31.855)) ;
#121312 = CARTESIAN_POINT('Origin',(-1.1,1.15,-31.755)) ;
#121313 = CARTESIAN_POINT('Origin',(-1.1,1.15,-31.755)) ;
#121314 = CARTESIAN_POINT('Origin',(-0.899999999999999,-1.9,-31.755)) ;
#121315 = CARTESIAN_POINT('Origin',(-1.1,-1.9,-31.755)) ;
#121316 = CARTESIAN_POINT('Origin',(0.500000000000001,-5.867447051098E-17,
-31.755)) ;
#121317 = CARTESIAN_POINT('Origin',(0.500000000000001,-2.9,-31.755)) ;
#121318 = CARTESIAN_POINT('Origin',(0.700000000000002,-2.9,-30.48)) ;
#121319 = CARTESIAN_POINT('Origin',(0.700000000000002,-2.9,-31.755)) ;
#121320 = CARTESIAN_POINT('Origin',(-1.1,1.15,-31.755)) ;
#121321 = CARTESIAN_POINT('Origin',(-1.1,1.15,-31.955)) ;
#121322 = CARTESIAN_POINT('Origin',(-1.1,-2.39429110547967E-16,-31.755)) ;
#121323 = CARTESIAN_POINT('',(-1.1,1.25,-31.855)) ;
#121324 = CARTESIAN_POINT('Origin',(0.500000000000001,-2.9,-31.755)) ;
#121325 = CARTESIAN_POINT('Origin',(0.500000000000001,-2.9,-31.955)) ;
#121326 = CARTESIAN_POINT('Origin',(-1.1,1.25,-31.955)) ;
#121327 = CARTESIAN_POINT('Origin',(-1.1,-2.9,-31.955)) ;
#121328 = CARTESIAN_POINT('Origin',(-1.1,-2.9,-31.955)) ;
#121329 = CARTESIAN_POINT('Origin',(-1.1,-2.9,-31.955)) ;
#121330 = CARTESIAN_POINT('Origin',(-1.1,-2.9,-31.955)) ;
#121331 = CARTESIAN_POINT('Origin',(1.5,1.9,-29.88)) ;
#121332 = CARTESIAN_POINT('Origin',(1.5,1.9,-32.03)) ;
#121333 = CARTESIAN_POINT('Origin',(1.5,1.9,-31.08)) ;
#121334 = CARTESIAN_POINT('Origin',(1.5,2.1,-31.08)) ;
#121335 = CARTESIAN_POINT('Origin',(1.5,2.1,-30.88)) ;
#121336 = CARTESIAN_POINT('Origin',(1.5,1.9,-32.03)) ;
#121337 = CARTESIAN_POINT('Origin',(1.5,1.9,-32.03)) ;
#121338 = CARTESIAN_POINT('Origin',(1.5,2.1,-30.88)) ;
#121339 = CARTESIAN_POINT('Origin',(1.5,2.4,-30.88)) ;
#121340 = CARTESIAN_POINT('Origin',(1.5,2.1,-32.03)) ;
#121341 = CARTESIAN_POINT('Origin',(1.5,-2.15,-32.03)) ;
#121342 = CARTESIAN_POINT('Origin',(1.5,2.4,-31.08)) ;
#121343 = CARTESIAN_POINT('Origin',(1.5,2.6,-31.08)) ;
#121344 = CARTESIAN_POINT('Origin',(1.5,-2.15,-32.03)) ;
#121345 = CARTESIAN_POINT('Origin',(1.5,-2.15,-32.03)) ;
#121346 = CARTESIAN_POINT('Origin',(1.5,2.6,-29.88)) ;
#121347 = CARTESIAN_POINT('Origin',(1.5,2.6,-31.1885786437627)) ;
#121348 = CARTESIAN_POINT('Origin',(1.5,-2.15,-29.88)) ;
#121349 = CARTESIAN_POINT('Origin',(1.5,-2.15,-31.3831195934094)) ;
#121350 = CARTESIAN_POINT('Origin',(1.5,2.6,-31.1885786437627)) ;
#121351 = CARTESIAN_POINT('Origin',(1.5,2.6,-31.1885786437627)) ;
#121352 = CARTESIAN_POINT('Origin',(1.5,-2.15,-31.3831195934094)) ;
#121353 = CARTESIAN_POINT('Origin',(1.5,-2.15,-31.3831195934094)) ;
#121354 = CARTESIAN_POINT('Origin',(1.5,1.69571067811865,-30.2842893218813)) ;
#121355 = CARTESIAN_POINT('Origin',(1.5,3.15,-31.7385786437627)) ;
#121356 = CARTESIAN_POINT('Origin',(1.5,-3.65625,-30.48)) ;
#121357 = CARTESIAN_POINT('Origin',(1.5,-2.15,-29.5768804065906)) ;
#121358 = CARTESIAN_POINT('Origin',(1.5,3.15,-31.7385786437627)) ;
#121359 = CARTESIAN_POINT('Origin',(1.5,3.15,-31.7385786437627)) ;
#121360 = CARTESIAN_POINT('Origin',(1.5,-2.15,-29.5768804065906)) ;
#121361 = CARTESIAN_POINT('Origin',(1.5,-2.15,-29.5768804065906)) ;
#121362 = CARTESIAN_POINT('Origin',(1.5,3.15,-29.88)) ;
#121363 = CARTESIAN_POINT('Origin',(1.5,-2.15,-29.88)) ;
#121364 = CARTESIAN_POINT('Origin',(1.5,-2.15,-28.93)) ;
#121365 = CARTESIAN_POINT('Origin',(1.5,-2.15,-28.93)) ;
#121366 = CARTESIAN_POINT('Origin',(1.5,-2.15,-28.93)) ;
#121367 = CARTESIAN_POINT('Origin',(1.5,2.29571067811866,-30.0757106781187)) ;
#121368 = CARTESIAN_POINT('Origin',(1.5,2.6,-29.7714213562373)) ;
#121369 = CARTESIAN_POINT('Origin',(1.5,2.1,-28.93)) ;
#121370 = CARTESIAN_POINT('Origin',(1.5,1.9,-28.93)) ;
#121371 = CARTESIAN_POINT('Origin',(1.5,2.6,-29.7714213562373)) ;
#121372 = CARTESIAN_POINT('Origin',(1.5,2.6,-29.7714213562373)) ;
#121373 = CARTESIAN_POINT('Origin',(1.5,1.9,-28.93)) ;
#121374 = CARTESIAN_POINT('Origin',(1.5,1.9,-28.93)) ;
#121375 = CARTESIAN_POINT('Origin',(1.5,2.6,-29.88)) ;
#121376 = CARTESIAN_POINT('Origin',(1.5,2.6,-29.88)) ;
#121377 = CARTESIAN_POINT('Origin',(1.5,1.9,-29.88)) ;
#121378 = CARTESIAN_POINT('Origin',(1.5,1.9,-29.88)) ;
#121379 = CARTESIAN_POINT('Origin',(1.5,2.4,-29.88)) ;
#121380 = CARTESIAN_POINT('Origin',(1.5,2.4,-30.08)) ;
#121381 = CARTESIAN_POINT('Origin',(1.5,2.1,-29.88)) ;
#121382 = CARTESIAN_POINT('Origin',(1.5,2.1,-30.08)) ;
#121383 = CARTESIAN_POINT('Origin',(1.5,2.1,-30.08)) ;
#121384 = CARTESIAN_POINT('Origin',(-0.899999999999999,-2.,-33.69)) ;
#121385 = CARTESIAN_POINT('Origin',(-0.899999999999999,0.4,-33.69)) ;
#121386 = CARTESIAN_POINT('Origin',(-0.899999999999999,-1.9,-33.69)) ;
#121387 = CARTESIAN_POINT('Origin',(0.600000000000001,0.4,-33.89)) ;
#121388 = CARTESIAN_POINT('Origin',(0.500000000000001,0.4,-33.89)) ;
#121389 = CARTESIAN_POINT('Origin',(-0.899999999999999,0.4,-33.89)) ;
#121390 = CARTESIAN_POINT('Origin',(0.500000000000001,0.4,-33.89)) ;
#121391 = CARTESIAN_POINT('',(0.600000000000001,0.4,-33.89)) ;
#121392 = CARTESIAN_POINT('Origin',(0.500000000000001,0.4,-33.89)) ;
#121393 = CARTESIAN_POINT('Origin',(0.500000000000001,0.4,-33.89)) ;
#121394 = CARTESIAN_POINT('Origin',(-0.899999999999999,-1.9,-33.69)) ;
#121395 = CARTESIAN_POINT('Origin',(-0.899999999999999,-1.9,-33.69)) ;
#121396 = CARTESIAN_POINT('Origin',(-0.899999999999999,-1.9,-33.69)) ;
#121397 = CARTESIAN_POINT('Origin',(-0.899999999999999,0.4,-33.89)) ;
#121398 = CARTESIAN_POINT('Origin',(-0.899999999999999,0.6,-33.89)) ;
#121399 = CARTESIAN_POINT('Origin',(0.500000000000001,0.4,-34.29)) ;
#121400 = CARTESIAN_POINT('Origin',(0.500000000000001,0.4,-34.69)) ;
#121401 = CARTESIAN_POINT('',(0.600000000000001,0.4,-34.59)) ;
#121402 = CARTESIAN_POINT('Ctrl Pts',(0.595612997216083,0.370705721320409,
-34.6607057213204)) ;
#121403 = CARTESIAN_POINT('Ctrl Pts',(0.596180587760894,0.372558268494363,
-34.6588554988322)) ;
#121404 = CARTESIAN_POINT('Ctrl Pts',(0.596672461925687,0.374355839771987,
-34.6569141798663)) ;
#121405 = CARTESIAN_POINT('Ctrl Pts',(0.599015141889206,0.383869350930039,
-34.6457649936563)) ;
#121406 = CARTESIAN_POINT('Ctrl Pts',(0.599609996542524,0.390224332900438,
-34.6349726026542)) ;
#121407 = CARTESIAN_POINT('Ctrl Pts',(0.600050586298726,0.39811743914156,
-34.6123310532047)) ;
#121408 = CARTESIAN_POINT('Ctrl Pts',(0.600000000000001,0.4,-34.6012012506335)) ;
#121409 = CARTESIAN_POINT('Ctrl Pts',(0.600000000000001,0.399999999999999,
-34.59)) ;
#121410 = CARTESIAN_POINT('',(0.600000000000001,0.4,-34.29)) ;
#121411 = CARTESIAN_POINT('Origin',(0.500000000000001,-4.56640444411538E-17,
-33.89)) ;
#121412 = CARTESIAN_POINT('',(0.500000000000001,0.394987437106619,-33.99)) ;
#121413 = CARTESIAN_POINT('Ctrl Pts',(0.500000000000001,0.394987437106619,
-33.99)) ;
#121414 = CARTESIAN_POINT('Ctrl Pts',(0.505940567948938,0.395584486649899,
-33.99)) ;
#121415 = CARTESIAN_POINT('Ctrl Pts',(0.511931971019108,0.396132036079016,
-33.989466300328)) ;
#121416 = CARTESIAN_POINT('Ctrl Pts',(0.517829015308506,0.396618246075351,
-33.9883977957737)) ;
#121417 = CARTESIAN_POINT('Ctrl Pts',(0.522982218721175,0.397043126556051,
-33.9874640701571)) ;
#121418 = CARTESIAN_POINT('Ctrl Pts',(0.52806264897023,0.397421319341387,
-33.9861228267971)) ;
#121419 = CARTESIAN_POINT('Ctrl Pts',(0.532978106724009,0.397751505046071,
-33.9844057438766)) ;
#121420 = CARTESIAN_POINT('Ctrl Pts',(0.538583536338943,0.398128038182998,
-33.9824476378496)) ;
#121421 = CARTESIAN_POINT('Ctrl Pts',(0.544059405914837,0.398447721828293,
-33.9799700083111)) ;
#121422 = CARTESIAN_POINT('Ctrl Pts',(0.549268572255721,0.39871233110898,
-33.9770207319429)) ;
#121423 = CARTESIAN_POINT('Ctrl Pts',(0.553856850427124,0.398945401221754,
-33.9744229841469)) ;
#121424 = CARTESIAN_POINT('Ctrl Pts',(0.55823782506931,0.399135987683842,
-33.97146038498)) ;
#121425 = CARTESIAN_POINT('Ctrl Pts',(0.56233383608621,0.399290378266507,
-33.9681952228642)) ;
#121426 = CARTESIAN_POINT('Ctrl Pts',(0.566990328957886,0.399465895042381,
-33.9644832689523)) ;
#121427 = CARTESIAN_POINT('Ctrl Pts',(0.571349096493416,0.399597278936107,
-33.9603228064848)) ;
#121428 = CARTESIAN_POINT('Ctrl Pts',(0.575296920056707,0.399694832180838,
-33.9558055759793)) ;
#121429 = CARTESIAN_POINT('Ctrl Pts',(0.578744263667898,0.399780018245914,
-33.9518610112151)) ;
#121430 = CARTESIAN_POINT('Ctrl Pts',(0.581878314560451,0.399839626289636,
-33.9476455218421)) ;
#121431 = CARTESIAN_POINT('Ctrl Pts',(0.584648147334857,0.399882153365958,
-33.9432418177073)) ;
#121432 = CARTESIAN_POINT('Ctrl Pts',(0.587839270208177,0.399931148788079,
-33.9381683125045)) ;
#121433 = CARTESIAN_POINT('Ctrl Pts',(0.590595054415139,0.399958289583405,
-33.9327666362444)) ;
#121434 = CARTESIAN_POINT('Ctrl Pts',(0.592838618943155,0.39997435700316,
-33.9271616850093)) ;
#121435 = CARTESIAN_POINT('Ctrl Pts',(0.594777336851684,0.399988241245861,
-33.9223183122423)) ;
#121436 = CARTESIAN_POINT('Ctrl Pts',(0.596334051506209,0.399993946552814,
-33.917324166227)) ;
#121437 = CARTESIAN_POINT('Ctrl Pts',(0.597488309822315,0.39999684570125,
-33.9122717185684)) ;
#121438 = CARTESIAN_POINT('Ctrl Pts',(0.598804024094335,0.400000150378306,
-33.9065125419608)) ;
#121439 = CARTESIAN_POINT('Ctrl Pts',(0.599612685195353,0.399999963509465,
-33.9006028438911)) ;
#121440 = CARTESIAN_POINT('Ctrl Pts',(0.599890230999679,0.399999993975383,
-33.894684202262)) ;
#121441 = CARTESIAN_POINT('Ctrl Pts',(0.599963464549386,0.400000002014155,
-33.8931225027904)) ;
#121442 = CARTESIAN_POINT('Ctrl Pts',(0.600000000000001,0.399999999999999,
-33.8915602215095)) ;
#121443 = CARTESIAN_POINT('Ctrl Pts',(0.600000000000001,0.399999999999999,
-33.89)) ;
#121444 = CARTESIAN_POINT('',(0.600000000000001,0.299999999999999,-33.89)) ;
#121445 = CARTESIAN_POINT('Ctrl Pts',(0.500000000000001,0.394987437106619,
-33.99)) ;
#121446 = CARTESIAN_POINT('Ctrl Pts',(0.500454935590171,0.395033159853782,
-33.99)) ;
#121447 = CARTESIAN_POINT('Ctrl Pts',(0.500909898680634,0.395078570329076,
-33.9899968954911)) ;
#121448 = CARTESIAN_POINT('Ctrl Pts',(0.502892456244958,0.395275075889069,
-33.9899698339419)) ;
#121449 = CARTESIAN_POINT('Ctrl Pts',(0.50441874748225,0.395422812032187,
-33.989913985421)) ;
#121450 = CARTESIAN_POINT('Ctrl Pts',(0.508462199543321,0.395804395682031,
-33.9896732810567)) ;
#121451 = CARTESIAN_POINT('Ctrl Pts',(0.510974953343264,0.396031485023314,
-33.9894279391451)) ;
#121452 = CARTESIAN_POINT('Ctrl Pts',(0.521160739721166,0.396903453186226,
-33.9880427944916)) ;
#121453 = CARTESIAN_POINT('Ctrl Pts',(0.528708678528252,0.397444933153152,
-33.9861042177047)) ;
#121454 = CARTESIAN_POINT('Ctrl Pts',(0.545943206357825,0.398105551684101,
-33.9794646394513)) ;
#121455 = CARTESIAN_POINT('Ctrl Pts',(0.555229535466584,0.397987646678453,
-33.9740353588361)) ;
#121456 = CARTESIAN_POINT('Ctrl Pts',(0.571394604995541,0.395490482808082,
-33.960775513364)) ;
#121457 = CARTESIAN_POINT('Ctrl Pts',(0.578055313702682,0.393198948698442,
-33.953240745632)) ;
#121458 = CARTESIAN_POINT('Ctrl Pts',(0.588559132202378,0.385442756729426,
-33.9373922339843)) ;
#121459 = CARTESIAN_POINT('Ctrl Pts',(0.592167355639896,0.380240075127069,
-33.929548265607)) ;
#121460 = CARTESIAN_POINT('Ctrl Pts',(0.597496615531045,0.365892753467188,
-33.9139255217955)) ;
#121461 = CARTESIAN_POINT('Ctrl Pts',(0.598734255154177,0.356660564300953,
-33.9067727417271)) ;
#121462 = CARTESIAN_POINT('Ctrl Pts',(0.60001275468168,0.335223914398804,
-33.8955823058657)) ;
#121463 = CARTESIAN_POINT('Ctrl Pts',(0.599993900559809,0.322655037092181,
-33.8916615193656)) ;
#121464 = CARTESIAN_POINT('Ctrl Pts',(0.600000296204999,0.30610691358248,
-33.8901396263471)) ;
#121465 = CARTESIAN_POINT('Ctrl Pts',(0.600000000000001,0.303050992413506,
-33.89)) ;
#121466 = CARTESIAN_POINT('Ctrl Pts',(0.600000000000001,0.299999999999999,
-33.89)) ;
#121467 = CARTESIAN_POINT('',(0.600000000000001,-2.39800009914436E-17,-33.89)) ;
#121468 = CARTESIAN_POINT('Origin',(0.500000000000001,-1.9,-33.89)) ;
#121469 = CARTESIAN_POINT('Origin',(0.600000000000001,-1.9,-33.69)) ;
#121470 = CARTESIAN_POINT('Origin',(0.500000000000001,-1.9,-33.69)) ;
#121471 = CARTESIAN_POINT('Origin',(-0.899999999999999,-1.9,-32.915)) ;
#121472 = CARTESIAN_POINT('Origin',(-0.899999999999999,-1.9,-33.015)) ;
#121473 = CARTESIAN_POINT('Origin',(-0.899999999999999,0.6,-33.79)) ;
#121474 = CARTESIAN_POINT('Origin',(-0.899999999999999,0.6,-34.69)) ;
#121475 = CARTESIAN_POINT('Origin',(0.600000000000001,0.4,-34.69)) ;
#121476 = CARTESIAN_POINT('Origin',(0.500000000000001,0.4,-34.69)) ;
#121477 = CARTESIAN_POINT('Origin',(-0.899999999999999,0.4,-34.69)) ;
#121478 = CARTESIAN_POINT('Origin',(0.500000000000001,0.4,-34.69)) ;
#121479 = CARTESIAN_POINT('Origin',(0.500000000000001,-1.9,-33.69)) ;
#121480 = CARTESIAN_POINT('Origin',(0.500000000000001,-2.1,-33.69)) ;
#121481 = CARTESIAN_POINT('Origin',(-0.899999999999999,-1.9,-33.015)) ;
#121482 = CARTESIAN_POINT('Origin',(-1.1,-1.9,-33.015)) ;
#121483 = CARTESIAN_POINT('Origin',(-0.899999999999999,-2.1,-33.015)) ;
#121484 = CARTESIAN_POINT('Origin',(-0.899999999999999,0.4,-34.69)) ;
#121485 = CARTESIAN_POINT('Origin',(-0.899999999999999,0.4,-34.89)) ;
#121486 = CARTESIAN_POINT('Origin',(0.500000000000001,-2.1,-34.29)) ;
#121487 = CARTESIAN_POINT('Origin',(0.500000000000001,-2.1,-33.015)) ;
#121488 = CARTESIAN_POINT('Origin',(0.600000000000001,-2.1,-33.015)) ;
#121489 = CARTESIAN_POINT('Origin',(0.500000000000001,-2.1,-33.015)) ;
#121490 = CARTESIAN_POINT('Origin',(-1.1,-4.42727195005762E-17,-33.015)) ;
#121491 = CARTESIAN_POINT('',(-1.1,1.15,-32.915)) ;
#121492 = CARTESIAN_POINT('',(-1.1,1.25,-32.915)) ;
#121493 = CARTESIAN_POINT('Origin',(-1.1,1.15,-33.015)) ;
#121494 = CARTESIAN_POINT('Origin',(-0.899999999999999,0.5,-34.89)) ;
#121495 = CARTESIAN_POINT('Origin',(-0.899999999999999,-1.9,-34.89)) ;
#121496 = CARTESIAN_POINT('Origin',(0.600000000000001,-1.9,-34.89)) ;
#121497 = CARTESIAN_POINT('Origin',(0.500000000000001,-1.9,-34.89)) ;
#121498 = CARTESIAN_POINT('Origin',(-0.899999999999999,-1.9,-34.89)) ;
#121499 = CARTESIAN_POINT('Origin',(0.500000000000001,-1.9,-34.89)) ;
#121500 = CARTESIAN_POINT('Origin',(0.500000000000001,-2.1,-34.89)) ;
#121501 = CARTESIAN_POINT('Origin',(0.500000000000001,-2.1,-33.015)) ;
#121502 = CARTESIAN_POINT('Origin',(0.500000000000001,-2.1,-33.015)) ;
#121503 = CARTESIAN_POINT('Origin',(-1.1,-2.9,-32.815)) ;
#121504 = CARTESIAN_POINT('Origin',(-1.1,-2.9,-32.815)) ;
#121505 = CARTESIAN_POINT('Origin',(-1.1,-2.9,-32.815)) ;
#121506 = CARTESIAN_POINT('Origin',(-1.1,1.25,-32.815)) ;
#121507 = CARTESIAN_POINT('Origin',(-1.1,1.15,-32.815)) ;
#121508 = CARTESIAN_POINT('Origin',(-1.1,1.15,-33.015)) ;
#121509 = CARTESIAN_POINT('',(-1.1,1.25,-33.015)) ;
#121510 = CARTESIAN_POINT('Origin',(-1.1,1.15,-33.015)) ;
#121511 = CARTESIAN_POINT('Origin',(-1.1,1.15,-33.015)) ;
#121512 = CARTESIAN_POINT('Origin',(-0.899999999999999,-1.9,-34.89)) ;
#121513 = CARTESIAN_POINT('Origin',(-0.899999999999999,-1.9,-34.89)) ;
#121514 = CARTESIAN_POINT('Origin',(0.500000000000001,-2.1,-34.29)) ;
#121515 = CARTESIAN_POINT('Origin',(0.500000000000001,-2.1,-35.565)) ;
#121516 = CARTESIAN_POINT('Origin',(0.500000000000001,1.36481920536411E-16,
-33.015)) ;
#121517 = CARTESIAN_POINT('Origin',(0.500000000000001,-2.9,-33.015)) ;
#121518 = CARTESIAN_POINT('Origin',(-0.999999999999999,-2.9,-32.815)) ;
#121519 = CARTESIAN_POINT('Origin',(0.500000000000001,-2.9,-32.815)) ;
#121520 = CARTESIAN_POINT('Origin',(-1.1,1.15,-33.015)) ;
#121521 = CARTESIAN_POINT('Origin',(-1.1,1.35,-33.015)) ;
#121522 = CARTESIAN_POINT('Origin',(-1.1,1.15,-34.29)) ;
#121523 = CARTESIAN_POINT('',(-1.1,1.25,-35.565)) ;
#121524 = CARTESIAN_POINT('',(-1.1,1.25,-35.665)) ;
#121525 = CARTESIAN_POINT('Origin',(-1.1,1.15,-35.565)) ;
#121526 = CARTESIAN_POINT('Origin',(-0.899999999999999,-1.9,-34.79)) ;
#121527 = CARTESIAN_POINT('Origin',(-0.899999999999999,-1.9,-35.565)) ;
#121528 = CARTESIAN_POINT('Origin',(-0.999999999999999,-2.1,-35.565)) ;
#121529 = CARTESIAN_POINT('Origin',(0.500000000000001,-2.1,-35.565)) ;
#121530 = CARTESIAN_POINT('Origin',(-0.899999999999999,-2.1,-35.565)) ;
#121531 = CARTESIAN_POINT('Origin',(0.500000000000001,-2.1,-35.565)) ;
#121532 = CARTESIAN_POINT('Origin',(0.500000000000001,-2.1,-35.565)) ;
#121533 = CARTESIAN_POINT('Origin',(0.500000000000001,-2.9,-33.015)) ;
#121534 = CARTESIAN_POINT('Origin',(0.700000000000002,-2.9,-33.015)) ;
#121535 = CARTESIAN_POINT('Origin',(-1.1,1.35,-35.665)) ;
#121536 = CARTESIAN_POINT('Origin',(-1.1,1.35,-35.565)) ;
#121537 = CARTESIAN_POINT('Origin',(-1.1,1.15,-35.565)) ;
#121538 = CARTESIAN_POINT('',(-1.1,1.15,-35.665)) ;
#121539 = CARTESIAN_POINT('Origin',(-1.1,1.15,-35.565)) ;
#121540 = CARTESIAN_POINT('Origin',(-1.1,1.15,-35.565)) ;
#121541 = CARTESIAN_POINT('Origin',(-0.899999999999999,-1.9,-35.565)) ;
#121542 = CARTESIAN_POINT('Origin',(-1.1,-1.9,-35.565)) ;
#121543 = CARTESIAN_POINT('Origin',(0.500000000000001,-5.867447051098E-17,
-35.565)) ;
#121544 = CARTESIAN_POINT('Origin',(0.500000000000001,-2.9,-35.565)) ;
#121545 = CARTESIAN_POINT('Origin',(0.700000000000002,-2.9,-34.29)) ;
#121546 = CARTESIAN_POINT('Origin',(0.700000000000002,-2.9,-35.565)) ;
#121547 = CARTESIAN_POINT('Origin',(-1.1,1.15,-35.565)) ;
#121548 = CARTESIAN_POINT('Origin',(-1.1,1.15,-35.765)) ;
#121549 = CARTESIAN_POINT('Origin',(-1.1,-2.39429110547967E-16,-35.565)) ;
#121550 = CARTESIAN_POINT('',(-1.1,1.25,-35.665)) ;
#121551 = CARTESIAN_POINT('Origin',(0.500000000000001,-2.9,-35.565)) ;
#121552 = CARTESIAN_POINT('Origin',(0.500000000000001,-2.9,-35.765)) ;
#121553 = CARTESIAN_POINT('Origin',(-1.1,1.25,-35.765)) ;
#121554 = CARTESIAN_POINT('Origin',(-1.1,-2.9,-35.765)) ;
#121555 = CARTESIAN_POINT('Origin',(-1.1,-2.9,-35.765)) ;
#121556 = CARTESIAN_POINT('Origin',(-1.1,-2.9,-35.765)) ;
#121557 = CARTESIAN_POINT('Origin',(-1.1,-2.9,-35.765)) ;
#121558 = CARTESIAN_POINT('Origin',(1.5,1.9,-33.69)) ;
#121559 = CARTESIAN_POINT('Origin',(1.5,1.9,-35.84)) ;
#121560 = CARTESIAN_POINT('Origin',(1.5,1.9,-34.89)) ;
#121561 = CARTESIAN_POINT('Origin',(1.5,2.1,-34.89)) ;
#121562 = CARTESIAN_POINT('Origin',(1.5,2.1,-34.69)) ;
#121563 = CARTESIAN_POINT('Origin',(1.5,1.9,-35.84)) ;
#121564 = CARTESIAN_POINT('Origin',(1.5,1.9,-35.84)) ;
#121565 = CARTESIAN_POINT('Origin',(1.5,2.1,-34.69)) ;
#121566 = CARTESIAN_POINT('Origin',(1.5,2.4,-34.69)) ;
#121567 = CARTESIAN_POINT('Origin',(1.5,2.1,-35.84)) ;
#121568 = CARTESIAN_POINT('Origin',(1.5,-2.15,-35.84)) ;
#121569 = CARTESIAN_POINT('Origin',(1.5,2.4,-34.89)) ;
#121570 = CARTESIAN_POINT('Origin',(1.5,2.6,-34.89)) ;
#121571 = CARTESIAN_POINT('Origin',(1.5,-2.15,-35.84)) ;
#121572 = CARTESIAN_POINT('Origin',(1.5,-2.15,-35.84)) ;
#121573 = CARTESIAN_POINT('Origin',(1.5,2.6,-33.69)) ;
#121574 = CARTESIAN_POINT('Origin',(1.5,2.6,-34.9985786437627)) ;
#121575 = CARTESIAN_POINT('Origin',(1.5,-2.15,-33.69)) ;
#121576 = CARTESIAN_POINT('Origin',(1.5,-2.15,-35.1931195934094)) ;
#121577 = CARTESIAN_POINT('Origin',(1.5,2.6,-34.9985786437627)) ;
#121578 = CARTESIAN_POINT('Origin',(1.5,2.6,-34.9985786437627)) ;
#121579 = CARTESIAN_POINT('Origin',(1.5,-2.15,-35.1931195934094)) ;
#121580 = CARTESIAN_POINT('Origin',(1.5,-2.15,-35.1931195934094)) ;
#121581 = CARTESIAN_POINT('Origin',(1.5,1.69571067811865,-34.0942893218813)) ;
#121582 = CARTESIAN_POINT('Origin',(1.5,3.15,-35.5485786437627)) ;
#121583 = CARTESIAN_POINT('Origin',(1.5,-3.65625,-34.29)) ;
#121584 = CARTESIAN_POINT('Origin',(1.5,-2.15,-33.3868804065906)) ;
#121585 = CARTESIAN_POINT('Origin',(1.5,3.15,-35.5485786437627)) ;
#121586 = CARTESIAN_POINT('Origin',(1.5,3.15,-35.5485786437627)) ;
#121587 = CARTESIAN_POINT('Origin',(1.5,-2.15,-33.3868804065906)) ;
#121588 = CARTESIAN_POINT('Origin',(1.5,-2.15,-33.3868804065906)) ;
#121589 = CARTESIAN_POINT('Origin',(1.5,3.15,-33.69)) ;
#121590 = CARTESIAN_POINT('Origin',(1.5,-2.15,-33.69)) ;
#121591 = CARTESIAN_POINT('Origin',(1.5,-2.15,-32.74)) ;
#121592 = CARTESIAN_POINT('Origin',(1.5,-2.15,-32.74)) ;
#121593 = CARTESIAN_POINT('Origin',(1.5,-2.15,-32.74)) ;
#121594 = CARTESIAN_POINT('Origin',(1.5,2.29571067811866,-33.8857106781187)) ;
#121595 = CARTESIAN_POINT('Origin',(1.5,2.6,-33.5814213562373)) ;
#121596 = CARTESIAN_POINT('Origin',(1.5,2.1,-32.74)) ;
#121597 = CARTESIAN_POINT('Origin',(1.5,1.9,-32.74)) ;
#121598 = CARTESIAN_POINT('Origin',(1.5,2.6,-33.5814213562373)) ;
#121599 = CARTESIAN_POINT('Origin',(1.5,2.6,-33.5814213562373)) ;
#121600 = CARTESIAN_POINT('Origin',(1.5,1.9,-32.74)) ;
#121601 = CARTESIAN_POINT('Origin',(1.5,1.9,-32.74)) ;
#121602 = CARTESIAN_POINT('Origin',(1.5,2.6,-33.69)) ;
#121603 = CARTESIAN_POINT('Origin',(1.5,2.6,-33.69)) ;
#121604 = CARTESIAN_POINT('Origin',(1.5,1.9,-33.69)) ;
#121605 = CARTESIAN_POINT('Origin',(1.5,1.9,-33.69)) ;
#121606 = CARTESIAN_POINT('Origin',(1.5,2.4,-33.69)) ;
#121607 = CARTESIAN_POINT('Origin',(1.5,2.4,-33.89)) ;
#121608 = CARTESIAN_POINT('Origin',(1.5,2.1,-33.69)) ;
#121609 = CARTESIAN_POINT('Origin',(1.5,2.1,-33.89)) ;
#121610 = CARTESIAN_POINT('Origin',(1.5,2.1,-33.89)) ;
#121611 = CARTESIAN_POINT('Origin',(-0.4,-0.600000000000001,-3.41)) ;
#121612 = CARTESIAN_POINT('',(-0.4,-0.600000000000001,-3.51)) ;
#121613 = CARTESIAN_POINT('',(-0.4,-0.600000000000001,-4.11)) ;
#121614 = CARTESIAN_POINT('',(-0.4,-0.600000000000001,-3.41)) ;
#121615 = CARTESIAN_POINT('',(-0.4,-6.05857864376269,-4.11)) ;
#121616 = CARTESIAN_POINT('',(-0.4,-0.600000000000001,-4.11)) ;
#121617 = CARTESIAN_POINT('',(-0.4,-6.05857864376269,-3.51)) ;
#121618 = CARTESIAN_POINT('',(-0.4,-6.05857864376269,-3.41)) ;
#121619 = CARTESIAN_POINT('',(-0.4,-0.600000000000001,-3.51)) ;
#121620 = CARTESIAN_POINT('Origin',(-0.4,-6.1,-3.41)) ;
#121621 = CARTESIAN_POINT('',(-0.129289321881346,-6.37071067811866,-3.86857864376269)) ;
#121622 = CARTESIAN_POINT('',(-0.129289321881346,-6.37071067811866,-3.75142135623731)) ;
#121623 = CARTESIAN_POINT('',(-0.129289321881346,-6.37071067811866,-3.41)) ;
#121624 = CARTESIAN_POINT('',(-0.370710678118655,-6.12928932188134,-3.51)) ;
#121625 = CARTESIAN_POINT('',(-0.423570226039552,-6.07642977396045,-3.4571404520791)) ;
#121626 = CARTESIAN_POINT('',(-0.370710678118655,-6.12928932188134,-4.11)) ;
#121627 = CARTESIAN_POINT('',(-0.370710678118655,-6.12928932188134,-3.41)) ;
#121628 = CARTESIAN_POINT('',(-0.156903559372885,-6.34309644062712,-3.89619288125423)) ;
#121629 = CARTESIAN_POINT('Origin',(-0.1,-6.4,-3.41)) ;
#121630 = CARTESIAN_POINT('',(0.0585786437626908,-6.4,-3.86857864376269)) ;
#121631 = CARTESIAN_POINT('',(0.0585786437626908,-6.4,-3.75142135623731)) ;
#121632 = CARTESIAN_POINT('',(0.0585786437626908,-6.4,-3.41)) ;
#121633 = CARTESIAN_POINT('',(-0.0585786437626908,-6.4,-3.75142135623731)) ;
#121634 = CARTESIAN_POINT('',(-0.1,-6.4,-3.75142135623731)) ;
#121635 = CARTESIAN_POINT('',(-0.0585786437626908,-6.4,-3.86857864376269)) ;
#121636 = CARTESIAN_POINT('',(-0.0585786437626908,-6.4,-3.41)) ;
#121637 = CARTESIAN_POINT('',(-0.1,-6.4,-3.86857864376269)) ;
#121638 = CARTESIAN_POINT('Origin',(0.1,-6.4,-3.41)) ;
#121639 = CARTESIAN_POINT('',(0.370710678118655,-6.12928932188134,-4.11)) ;
#121640 = CARTESIAN_POINT('',(0.370710678118655,-6.12928932188134,-3.51)) ;
#121641 = CARTESIAN_POINT('',(0.370710678118655,-6.12928932188134,-3.41)) ;
#121642 = CARTESIAN_POINT('',(0.129289321881346,-6.37071067811866,-3.75142135623731)) ;
#121643 = CARTESIAN_POINT('',(0.223570226039552,-6.27642977396045,-3.6571404520791)) ;
#121644 = CARTESIAN_POINT('',(0.129289321881346,-6.37071067811866,-3.86857864376269)) ;
#121645 = CARTESIAN_POINT('',(0.129289321881346,-6.37071067811866,-3.41)) ;
#121646 = CARTESIAN_POINT('',(-0.0430964406271149,-6.54309644062712,-3.69619288125423)) ;
#121647 = CARTESIAN_POINT('Origin',(0.4,-6.1,-3.41)) ;
#121648 = CARTESIAN_POINT('',(0.4,-6.05857864376269,-3.51)) ;
#121649 = CARTESIAN_POINT('',(0.4,-6.05857864376269,-4.11)) ;
#121650 = CARTESIAN_POINT('',(0.4,-6.05857864376269,-3.41)) ;
#121651 = CARTESIAN_POINT('',(0.4,-0.6,-4.11)) ;
#121652 = CARTESIAN_POINT('',(0.4,-6.1,-4.11)) ;
#121653 = CARTESIAN_POINT('',(0.4,-0.6,-3.51)) ;
#121654 = CARTESIAN_POINT('',(0.4,-0.6,-3.41)) ;
#121655 = CARTESIAN_POINT('',(0.4,-6.05857864376269,-3.51)) ;
#121656 = CARTESIAN_POINT('Origin',(0.6,-0.600000000000001,-3.41)) ;
#121657 = CARTESIAN_POINT('',(0.3,-6.05857864376269,-3.41)) ;
#121658 = CARTESIAN_POINT('',(0.3,-0.6,-3.41)) ;
#121659 = CARTESIAN_POINT('',(0.3,-0.6,-3.41)) ;
#121660 = CARTESIAN_POINT('Origin',(0.6,-0.6,-3.41)) ;
#121661 = CARTESIAN_POINT('',(-0.3,-0.600000000000001,-3.41)) ;
#121662 = CARTESIAN_POINT('Origin',(0.6,-0.600000000000001,-3.41)) ;
#121663 = CARTESIAN_POINT('',(-0.299999999999999,-6.05857864376269,-3.41)) ;
#121664 = CARTESIAN_POINT('',(-0.3,-0.600000000000001,-3.41)) ;
#121665 = CARTESIAN_POINT('',(0.4,-6.05857864376269,-3.41)) ;
#121666 = CARTESIAN_POINT('Origin',(0.6,-0.600000000000001,-4.21)) ;
#121667 = CARTESIAN_POINT('',(-0.300000000000001,-6.05857864376269,-4.21)) ;
#121668 = CARTESIAN_POINT('',(-0.3,-0.600000000000001,-4.21)) ;
#121669 = CARTESIAN_POINT('',(-0.3,-0.600000000000001,-4.21)) ;
#121670 = CARTESIAN_POINT('Origin',(0.6,-0.600000000000001,-4.21)) ;
#121671 = CARTESIAN_POINT('',(0.3,-0.6,-4.21)) ;
#121672 = CARTESIAN_POINT('Origin',(0.6,-0.6,-4.21)) ;
#121673 = CARTESIAN_POINT('',(0.3,-6.05857864376269,-4.21)) ;
#121674 = CARTESIAN_POINT('',(0.3,-0.600000000000001,-4.21)) ;
#121675 = CARTESIAN_POINT('',(0.6,-6.05857864376269,-4.21)) ;
#121676 = CARTESIAN_POINT('Origin',(0.6,-0.600000000000001,-3.41)) ;
#121677 = CARTESIAN_POINT('Origin',(0.6,-0.600000000000001,-4.11)) ;
#121678 = CARTESIAN_POINT('Origin',(0.6,-0.600000000000001,-3.51)) ;
#121679 = CARTESIAN_POINT('Origin',(0.6,-0.6,-3.41)) ;
#121680 = CARTESIAN_POINT('Origin',(0.6,-0.6,-4.11)) ;
#121681 = CARTESIAN_POINT('Origin',(0.6,-0.6,-3.51)) ;
#121682 = CARTESIAN_POINT('Origin',(7.,0.1,-3.41)) ;
#121683 = CARTESIAN_POINT('',(6.72928932188135,0.370710678118655,-4.11)) ;
#121684 = CARTESIAN_POINT('',(6.72928932188135,0.370710678118655,-3.51)) ;
#121685 = CARTESIAN_POINT('',(6.72928932188135,0.370710678118655,-3.41)) ;
#121686 = CARTESIAN_POINT('',(6.97071067811866,0.129289321881346,-3.75142135623731)) ;
#121687 = CARTESIAN_POINT('',(6.87642977396045,0.223570226039552,-3.6571404520791)) ;
#121688 = CARTESIAN_POINT('',(6.97071067811866,0.129289321881346,-3.86857864376269)) ;
#121689 = CARTESIAN_POINT('',(6.97071067811866,0.129289321881346,-3.41)) ;
#121690 = CARTESIAN_POINT('',(7.14309644062712,-0.0430964406271146,-3.69619288125423)) ;
#121691 = CARTESIAN_POINT('Origin',(6.7,0.400000000000001,-3.41)) ;
#121692 = CARTESIAN_POINT('',(6.65857864376269,0.400000000000001,-3.51)) ;
#121693 = CARTESIAN_POINT('',(6.65857864376269,0.400000000000001,-4.11)) ;
#121694 = CARTESIAN_POINT('',(6.65857864376269,0.400000000000001,-3.41)) ;
#121695 = CARTESIAN_POINT('',(6.7,0.400000000000001,-4.11)) ;
#121696 = CARTESIAN_POINT('',(6.65857864376269,0.400000000000001,-3.51)) ;
#121697 = CARTESIAN_POINT('Origin',(0.6,-0.4,-3.41)) ;
#121698 = CARTESIAN_POINT('',(6.65857864376269,-0.400000000000001,-4.11)) ;
#121699 = CARTESIAN_POINT('',(0.6,-0.4,-4.11)) ;
#121700 = CARTESIAN_POINT('',(6.65857864376269,-0.400000000000001,-3.51)) ;
#121701 = CARTESIAN_POINT('',(6.65857864376269,-0.400000000000001,-3.41)) ;
#121702 = CARTESIAN_POINT('',(2.4,-0.4,-3.51)) ;
#121703 = CARTESIAN_POINT('Origin',(6.7,-0.400000000000001,-3.41)) ;
#121704 = CARTESIAN_POINT('',(6.97071067811866,-0.129289321881346,-3.86857864376269)) ;
#121705 = CARTESIAN_POINT('',(6.97071067811866,-0.129289321881346,-3.75142135623731)) ;
#121706 = CARTESIAN_POINT('',(6.97071067811866,-0.129289321881346,-3.41)) ;
#121707 = CARTESIAN_POINT('',(6.72928932188135,-0.370710678118655,-3.51)) ;
#121708 = CARTESIAN_POINT('',(6.67642977396045,-0.423570226039552,-3.4571404520791)) ;
#121709 = CARTESIAN_POINT('',(6.72928932188135,-0.370710678118655,-4.11)) ;
#121710 = CARTESIAN_POINT('',(6.72928932188135,-0.370710678118655,-3.41)) ;
#121711 = CARTESIAN_POINT('',(6.94309644062712,-0.156903559372885,-3.89619288125423)) ;
#121712 = CARTESIAN_POINT('Origin',(7.,-0.1,-3.41)) ;
#121713 = CARTESIAN_POINT('',(7.,-0.0585786437626909,-3.75142135623731)) ;
#121714 = CARTESIAN_POINT('',(7.,-0.0585786437626909,-3.86857864376269)) ;
#121715 = CARTESIAN_POINT('',(7.,-0.0585786437626909,-3.41)) ;
#121716 = CARTESIAN_POINT('',(7.,0.0585786437626909,-3.86857864376269)) ;
#121717 = CARTESIAN_POINT('',(7.,-0.1,-3.86857864376269)) ;
#121718 = CARTESIAN_POINT('',(7.,0.0585786437626909,-3.75142135623731)) ;
#121719 = CARTESIAN_POINT('',(7.,0.0585786437626909,-3.41)) ;
#121720 = CARTESIAN_POINT('',(7.,-0.1,-3.75142135623731)) ;
#121721 = CARTESIAN_POINT('Origin',(0.6,-0.600000000000001,-3.41)) ;
#121722 = CARTESIAN_POINT('',(6.65857864376269,-0.300000000000001,-3.41)) ;
#121723 = CARTESIAN_POINT('',(6.65857864376269,0.3,-3.41)) ;
#121724 = CARTESIAN_POINT('',(6.65857864376269,-0.399999999999999,-3.41)) ;
#121725 = CARTESIAN_POINT('',(2.4,0.3,-3.41)) ;
#121726 = CARTESIAN_POINT('',(6.65857864376269,-0.300000000000001,-3.41)) ;
#121727 = CARTESIAN_POINT('Origin',(0.6,-0.600000000000001,-4.21)) ;
#121728 = CARTESIAN_POINT('',(6.65857864376269,0.300000000000001,-4.21)) ;
#121729 = CARTESIAN_POINT('',(0.6,0.299999999999999,-4.21)) ;
#121730 = CARTESIAN_POINT('',(6.65857864376269,-0.300000000000001,-4.21)) ;
#121731 = CARTESIAN_POINT('',(6.65857864376269,-0.6,-4.21)) ;
#121732 = CARTESIAN_POINT('',(0.6,-0.3,-4.21)) ;
#121733 = CARTESIAN_POINT('Origin',(-0.4,-0.600000000000001,-7.22)) ;
#121734 = CARTESIAN_POINT('',(-0.4,-0.600000000000001,-7.32)) ;
#121735 = CARTESIAN_POINT('',(-0.4,-0.600000000000001,-7.92)) ;
#121736 = CARTESIAN_POINT('',(-0.4,-0.600000000000001,-7.22)) ;
#121737 = CARTESIAN_POINT('',(-0.4,-6.05857864376269,-7.92)) ;
#121738 = CARTESIAN_POINT('',(-0.4,-0.600000000000001,-7.92)) ;
#121739 = CARTESIAN_POINT('',(-0.4,-6.05857864376269,-7.32)) ;
#121740 = CARTESIAN_POINT('',(-0.4,-6.05857864376269,-7.22)) ;
#121741 = CARTESIAN_POINT('',(-0.4,-0.600000000000001,-7.32)) ;
#121742 = CARTESIAN_POINT('Origin',(-0.4,-6.1,-7.22)) ;
#121743 = CARTESIAN_POINT('',(-0.129289321881345,-6.37071067811866,-7.67857864376269)) ;
#121744 = CARTESIAN_POINT('',(-0.129289321881346,-6.37071067811866,-7.56142135623731)) ;
#121745 = CARTESIAN_POINT('',(-0.129289321881346,-6.37071067811866,-7.22)) ;
#121746 = CARTESIAN_POINT('',(-0.370710678118655,-6.12928932188134,-7.32)) ;
#121747 = CARTESIAN_POINT('',(-0.423570226039552,-6.07642977396045,-7.2671404520791)) ;
#121748 = CARTESIAN_POINT('',(-0.370710678118655,-6.12928932188134,-7.92)) ;
#121749 = CARTESIAN_POINT('',(-0.370710678118655,-6.12928932188134,-7.22)) ;
#121750 = CARTESIAN_POINT('',(-0.156903559372885,-6.34309644062712,-7.70619288125423)) ;
#121751 = CARTESIAN_POINT('Origin',(-0.1,-6.4,-7.22)) ;
#121752 = CARTESIAN_POINT('',(0.0585786437626908,-6.4,-7.67857864376269)) ;
#121753 = CARTESIAN_POINT('',(0.0585786437626908,-6.4,-7.56142135623731)) ;
#121754 = CARTESIAN_POINT('',(0.0585786437626908,-6.4,-7.22)) ;
#121755 = CARTESIAN_POINT('',(-0.0585786437626908,-6.4,-7.56142135623731)) ;
#121756 = CARTESIAN_POINT('',(-0.1,-6.4,-7.56142135623731)) ;
#121757 = CARTESIAN_POINT('',(-0.0585786437626908,-6.4,-7.67857864376269)) ;
#121758 = CARTESIAN_POINT('',(-0.0585786437626908,-6.4,-7.22)) ;
#121759 = CARTESIAN_POINT('',(-0.1,-6.4,-7.67857864376269)) ;
#121760 = CARTESIAN_POINT('Origin',(0.1,-6.4,-7.22)) ;
#121761 = CARTESIAN_POINT('',(0.370710678118655,-6.12928932188134,-7.92)) ;
#121762 = CARTESIAN_POINT('',(0.370710678118655,-6.12928932188134,-7.32)) ;
#121763 = CARTESIAN_POINT('',(0.370710678118655,-6.12928932188134,-7.22)) ;
#121764 = CARTESIAN_POINT('',(0.129289321881346,-6.37071067811866,-7.56142135623731)) ;
#121765 = CARTESIAN_POINT('',(0.223570226039553,-6.27642977396045,-7.4671404520791)) ;
#121766 = CARTESIAN_POINT('',(0.129289321881346,-6.37071067811866,-7.67857864376269)) ;
#121767 = CARTESIAN_POINT('',(0.129289321881346,-6.37071067811866,-7.22)) ;
#121768 = CARTESIAN_POINT('',(-0.0430964406271151,-6.54309644062712,-7.50619288125423)) ;
#121769 = CARTESIAN_POINT('Origin',(0.4,-6.1,-7.22)) ;
#121770 = CARTESIAN_POINT('',(0.4,-6.05857864376269,-7.32)) ;
#121771 = CARTESIAN_POINT('',(0.4,-6.05857864376269,-7.92)) ;
#121772 = CARTESIAN_POINT('',(0.4,-6.05857864376269,-7.22)) ;
#121773 = CARTESIAN_POINT('',(0.4,-0.6,-7.92)) ;
#121774 = CARTESIAN_POINT('',(0.4,-6.1,-7.92)) ;
#121775 = CARTESIAN_POINT('',(0.4,-0.6,-7.32)) ;
#121776 = CARTESIAN_POINT('',(0.4,-0.6,-7.22)) ;
#121777 = CARTESIAN_POINT('',(0.4,-6.05857864376269,-7.32)) ;
#121778 = CARTESIAN_POINT('Origin',(0.6,-0.600000000000001,-7.22)) ;
#121779 = CARTESIAN_POINT('',(0.3,-6.05857864376269,-7.22)) ;
#121780 = CARTESIAN_POINT('',(0.3,-0.6,-7.22)) ;
#121781 = CARTESIAN_POINT('',(0.3,-0.6,-7.22)) ;
#121782 = CARTESIAN_POINT('Origin',(0.6,-0.6,-7.22)) ;
#121783 = CARTESIAN_POINT('',(-0.3,-0.600000000000001,-7.22)) ;
#121784 = CARTESIAN_POINT('Origin',(0.6,-0.600000000000001,-7.22)) ;
#121785 = CARTESIAN_POINT('',(-0.300000000000001,-6.05857864376269,-7.22)) ;
#121786 = CARTESIAN_POINT('',(-0.3,-0.600000000000001,-7.22)) ;
#121787 = CARTESIAN_POINT('',(0.4,-6.05857864376269,-7.22)) ;
#121788 = CARTESIAN_POINT('Origin',(0.6,-0.600000000000001,-8.02)) ;
#121789 = CARTESIAN_POINT('',(-0.299999999999999,-6.05857864376269,-8.02)) ;
#121790 = CARTESIAN_POINT('',(-0.3,-0.600000000000001,-8.02)) ;
#121791 = CARTESIAN_POINT('',(-0.3,-0.600000000000001,-8.02)) ;
#121792 = CARTESIAN_POINT('Origin',(0.6,-0.600000000000001,-8.02)) ;
#121793 = CARTESIAN_POINT('',(0.3,-0.6,-8.02)) ;
#121794 = CARTESIAN_POINT('Origin',(0.6,-0.6,-8.02)) ;
#121795 = CARTESIAN_POINT('',(0.3,-6.05857864376269,-8.02)) ;
#121796 = CARTESIAN_POINT('',(0.3,-0.600000000000001,-8.02)) ;
#121797 = CARTESIAN_POINT('',(0.6,-6.05857864376269,-8.02)) ;
#121798 = CARTESIAN_POINT('Origin',(0.6,-0.600000000000001,-7.22)) ;
#121799 = CARTESIAN_POINT('Origin',(0.6,-0.600000000000001,-7.92)) ;
#121800 = CARTESIAN_POINT('Origin',(0.6,-0.600000000000001,-7.32)) ;
#121801 = CARTESIAN_POINT('Origin',(0.6,-0.6,-7.22)) ;
#121802 = CARTESIAN_POINT('Origin',(0.6,-0.6,-7.92)) ;
#121803 = CARTESIAN_POINT('Origin',(0.6,-0.6,-7.32)) ;
#121804 = CARTESIAN_POINT('Origin',(7.,0.1,-7.22)) ;
#121805 = CARTESIAN_POINT('',(6.72928932188135,0.370710678118655,-7.92)) ;
#121806 = CARTESIAN_POINT('',(6.72928932188135,0.370710678118655,-7.32)) ;
#121807 = CARTESIAN_POINT('',(6.72928932188135,0.370710678118655,-7.22)) ;
#121808 = CARTESIAN_POINT('',(6.97071067811866,0.129289321881346,-7.56142135623731)) ;
#121809 = CARTESIAN_POINT('',(6.87642977396045,0.223570226039553,-7.4671404520791)) ;
#121810 = CARTESIAN_POINT('',(6.97071067811866,0.129289321881346,-7.67857864376269)) ;
#121811 = CARTESIAN_POINT('',(6.97071067811866,0.129289321881346,-7.22)) ;
#121812 = CARTESIAN_POINT('',(7.14309644062712,-0.0430964406271152,-7.50619288125423)) ;
#121813 = CARTESIAN_POINT('Origin',(6.7,0.400000000000001,-7.22)) ;
#121814 = CARTESIAN_POINT('',(6.65857864376269,0.400000000000001,-7.32)) ;
#121815 = CARTESIAN_POINT('',(6.65857864376269,0.400000000000001,-7.92)) ;
#121816 = CARTESIAN_POINT('',(6.65857864376269,0.400000000000001,-7.22)) ;
#121817 = CARTESIAN_POINT('',(6.7,0.400000000000001,-7.92)) ;
#121818 = CARTESIAN_POINT('',(6.65857864376269,0.400000000000001,-7.32)) ;
#121819 = CARTESIAN_POINT('Origin',(0.6,-0.4,-7.22)) ;
#121820 = CARTESIAN_POINT('',(6.65857864376269,-0.400000000000001,-7.92)) ;
#121821 = CARTESIAN_POINT('',(0.6,-0.4,-7.92)) ;
#121822 = CARTESIAN_POINT('',(6.65857864376269,-0.400000000000001,-7.32)) ;
#121823 = CARTESIAN_POINT('',(6.65857864376269,-0.400000000000001,-7.22)) ;
#121824 = CARTESIAN_POINT('',(2.4,-0.4,-7.32)) ;
#121825 = CARTESIAN_POINT('Origin',(6.7,-0.400000000000001,-7.22)) ;
#121826 = CARTESIAN_POINT('',(6.97071067811866,-0.129289321881346,-7.67857864376269)) ;
#121827 = CARTESIAN_POINT('',(6.97071067811866,-0.129289321881346,-7.56142135623731)) ;
#121828 = CARTESIAN_POINT('',(6.97071067811866,-0.129289321881346,-7.22)) ;
#121829 = CARTESIAN_POINT('',(6.72928932188135,-0.370710678118655,-7.32)) ;
#121830 = CARTESIAN_POINT('',(6.67642977396045,-0.423570226039553,-7.2671404520791)) ;
#121831 = CARTESIAN_POINT('',(6.72928932188135,-0.370710678118655,-7.92)) ;
#121832 = CARTESIAN_POINT('',(6.72928932188135,-0.370710678118655,-7.22)) ;
#121833 = CARTESIAN_POINT('',(6.94309644062712,-0.156903559372885,-7.70619288125423)) ;
#121834 = CARTESIAN_POINT('Origin',(7.,-0.1,-7.22)) ;
#121835 = CARTESIAN_POINT('',(7.,-0.0585786437626909,-7.56142135623731)) ;
#121836 = CARTESIAN_POINT('',(7.,-0.0585786437626909,-7.67857864376269)) ;
#121837 = CARTESIAN_POINT('',(7.,-0.0585786437626909,-7.22)) ;
#121838 = CARTESIAN_POINT('',(7.,0.0585786437626909,-7.67857864376269)) ;
#121839 = CARTESIAN_POINT('',(7.,-0.1,-7.67857864376269)) ;
#121840 = CARTESIAN_POINT('',(7.,0.0585786437626909,-7.56142135623731)) ;
#121841 = CARTESIAN_POINT('',(7.,0.0585786437626909,-7.22)) ;
#121842 = CARTESIAN_POINT('',(7.,-0.1,-7.56142135623731)) ;
#121843 = CARTESIAN_POINT('Origin',(0.6,-0.600000000000001,-7.22)) ;
#121844 = CARTESIAN_POINT('',(6.65857864376269,-0.300000000000001,-7.22)) ;
#121845 = CARTESIAN_POINT('',(6.65857864376269,0.300000000000002,-7.22)) ;
#121846 = CARTESIAN_POINT('',(6.65857864376269,-0.399999999999999,-7.22)) ;
#121847 = CARTESIAN_POINT('',(2.4,0.3,-7.22)) ;
#121848 = CARTESIAN_POINT('',(6.65857864376269,-0.300000000000001,-7.22)) ;
#121849 = CARTESIAN_POINT('Origin',(0.6,-0.600000000000001,-8.02)) ;
#121850 = CARTESIAN_POINT('',(6.65857864376269,0.300000000000002,-8.02)) ;
#121851 = CARTESIAN_POINT('',(0.6,0.299999999999999,-8.02)) ;
#121852 = CARTESIAN_POINT('',(6.65857864376269,-0.300000000000001,-8.02)) ;
#121853 = CARTESIAN_POINT('',(6.65857864376269,-0.6,-8.02)) ;
#121854 = CARTESIAN_POINT('',(0.6,-0.3,-8.02)) ;
#121855 = CARTESIAN_POINT('Origin',(-0.4,-0.600000000000001,-11.03)) ;
#121856 = CARTESIAN_POINT('',(-0.4,-0.600000000000001,-11.13)) ;
#121857 = CARTESIAN_POINT('',(-0.4,-0.600000000000001,-11.73)) ;
#121858 = CARTESIAN_POINT('',(-0.4,-0.600000000000001,-11.03)) ;
#121859 = CARTESIAN_POINT('',(-0.4,-6.05857864376269,-11.73)) ;
#121860 = CARTESIAN_POINT('',(-0.4,-0.600000000000001,-11.73)) ;
#121861 = CARTESIAN_POINT('',(-0.4,-6.05857864376269,-11.13)) ;
#121862 = CARTESIAN_POINT('',(-0.4,-6.05857864376269,-11.03)) ;
#121863 = CARTESIAN_POINT('',(-0.4,-0.600000000000001,-11.13)) ;
#121864 = CARTESIAN_POINT('Origin',(-0.4,-6.1,-11.03)) ;
#121865 = CARTESIAN_POINT('',(-0.129289321881346,-6.37071067811866,-11.4885786437627)) ;
#121866 = CARTESIAN_POINT('',(-0.129289321881346,-6.37071067811866,-11.3714213562373)) ;
#121867 = CARTESIAN_POINT('',(-0.129289321881346,-6.37071067811866,-11.03)) ;
#121868 = CARTESIAN_POINT('',(-0.370710678118655,-6.12928932188134,-11.13)) ;
#121869 = CARTESIAN_POINT('',(-0.423570226039552,-6.07642977396045,-11.0771404520791)) ;
#121870 = CARTESIAN_POINT('',(-0.370710678118655,-6.12928932188134,-11.73)) ;
#121871 = CARTESIAN_POINT('',(-0.370710678118655,-6.12928932188134,-11.03)) ;
#121872 = CARTESIAN_POINT('',(-0.156903559372884,-6.34309644062712,-11.5161928812542)) ;
#121873 = CARTESIAN_POINT('Origin',(-0.1,-6.4,-11.03)) ;
#121874 = CARTESIAN_POINT('',(0.0585786437626908,-6.4,-11.4885786437627)) ;
#121875 = CARTESIAN_POINT('',(0.0585786437626908,-6.4,-11.3714213562373)) ;
#121876 = CARTESIAN_POINT('',(0.0585786437626908,-6.4,-11.03)) ;
#121877 = CARTESIAN_POINT('',(-0.0585786437626908,-6.4,-11.3714213562373)) ;
#121878 = CARTESIAN_POINT('',(-0.1,-6.4,-11.3714213562373)) ;
#121879 = CARTESIAN_POINT('',(-0.0585786437626908,-6.4,-11.4885786437627)) ;
#121880 = CARTESIAN_POINT('',(-0.0585786437626908,-6.4,-11.03)) ;
#121881 = CARTESIAN_POINT('',(-0.1,-6.4,-11.4885786437627)) ;
#121882 = CARTESIAN_POINT('Origin',(0.1,-6.4,-11.03)) ;
#121883 = CARTESIAN_POINT('',(0.370710678118655,-6.12928932188134,-11.73)) ;
#121884 = CARTESIAN_POINT('',(0.370710678118655,-6.12928932188134,-11.13)) ;
#121885 = CARTESIAN_POINT('',(0.370710678118655,-6.12928932188134,-11.03)) ;
#121886 = CARTESIAN_POINT('',(0.129289321881346,-6.37071067811866,-11.3714213562373)) ;
#121887 = CARTESIAN_POINT('',(0.223570226039553,-6.27642977396045,-11.2771404520791)) ;
#121888 = CARTESIAN_POINT('',(0.129289321881346,-6.37071067811866,-11.4885786437627)) ;
#121889 = CARTESIAN_POINT('',(0.129289321881346,-6.37071067811866,-11.03)) ;
#121890 = CARTESIAN_POINT('',(-0.0430964406271157,-6.54309644062712,-11.3161928812542)) ;
#121891 = CARTESIAN_POINT('Origin',(0.4,-6.1,-11.03)) ;
#121892 = CARTESIAN_POINT('',(0.4,-6.05857864376269,-11.13)) ;
#121893 = CARTESIAN_POINT('',(0.4,-6.05857864376269,-11.73)) ;
#121894 = CARTESIAN_POINT('',(0.4,-6.05857864376269,-11.03)) ;
#121895 = CARTESIAN_POINT('',(0.4,-0.6,-11.73)) ;
#121896 = CARTESIAN_POINT('',(0.4,-6.1,-11.73)) ;
#121897 = CARTESIAN_POINT('',(0.4,-0.6,-11.13)) ;
#121898 = CARTESIAN_POINT('',(0.4,-0.6,-11.03)) ;
#121899 = CARTESIAN_POINT('',(0.4,-6.05857864376269,-11.13)) ;
#121900 = CARTESIAN_POINT('Origin',(0.6,-0.600000000000001,-11.03)) ;
#121901 = CARTESIAN_POINT('',(0.3,-6.05857864376269,-11.03)) ;
#121902 = CARTESIAN_POINT('',(0.3,-0.6,-11.03)) ;
#121903 = CARTESIAN_POINT('',(0.3,-0.6,-11.03)) ;
#121904 = CARTESIAN_POINT('Origin',(0.6,-0.6,-11.03)) ;
#121905 = CARTESIAN_POINT('',(-0.3,-0.600000000000001,-11.03)) ;
#121906 = CARTESIAN_POINT('Origin',(0.6,-0.600000000000001,-11.03)) ;
#121907 = CARTESIAN_POINT('',(-0.300000000000003,-6.05857864376269,-11.03)) ;
#121908 = CARTESIAN_POINT('',(-0.3,-0.600000000000001,-11.03)) ;
#121909 = CARTESIAN_POINT('',(0.4,-6.05857864376269,-11.03)) ;
#121910 = CARTESIAN_POINT('Origin',(0.6,-0.600000000000001,-11.83)) ;
#121911 = CARTESIAN_POINT('',(-0.299999999999999,-6.05857864376269,-11.83)) ;
#121912 = CARTESIAN_POINT('',(-0.3,-0.600000000000001,-11.83)) ;
#121913 = CARTESIAN_POINT('',(-0.3,-0.600000000000001,-11.83)) ;
#121914 = CARTESIAN_POINT('Origin',(0.6,-0.600000000000001,-11.83)) ;
#121915 = CARTESIAN_POINT('',(0.3,-0.6,-11.83)) ;
#121916 = CARTESIAN_POINT('Origin',(0.6,-0.6,-11.83)) ;
#121917 = CARTESIAN_POINT('',(0.3,-6.05857864376269,-11.83)) ;
#121918 = CARTESIAN_POINT('',(0.3,-0.600000000000001,-11.83)) ;
#121919 = CARTESIAN_POINT('',(0.6,-6.05857864376269,-11.83)) ;
#121920 = CARTESIAN_POINT('Origin',(0.6,-0.600000000000001,-11.03)) ;
#121921 = CARTESIAN_POINT('Origin',(0.6,-0.600000000000001,-11.73)) ;
#121922 = CARTESIAN_POINT('Origin',(0.6,-0.600000000000001,-11.13)) ;
#121923 = CARTESIAN_POINT('Origin',(0.6,-0.6,-11.03)) ;
#121924 = CARTESIAN_POINT('Origin',(0.6,-0.6,-11.73)) ;
#121925 = CARTESIAN_POINT('Origin',(0.6,-0.6,-11.13)) ;
#121926 = CARTESIAN_POINT('Origin',(7.,0.1,-11.03)) ;
#121927 = CARTESIAN_POINT('',(6.72928932188135,0.370710678118655,-11.73)) ;
#121928 = CARTESIAN_POINT('',(6.72928932188135,0.370710678118655,-11.13)) ;
#121929 = CARTESIAN_POINT('',(6.72928932188135,0.370710678118655,-11.03)) ;
#121930 = CARTESIAN_POINT('',(6.97071067811866,0.129289321881346,-11.3714213562373)) ;
#121931 = CARTESIAN_POINT('',(6.87642977396045,0.223570226039553,-11.2771404520791)) ;
#121932 = CARTESIAN_POINT('',(6.97071067811866,0.129289321881346,-11.4885786437627)) ;
#121933 = CARTESIAN_POINT('',(6.97071067811866,0.129289321881346,-11.03)) ;
#121934 = CARTESIAN_POINT('',(7.14309644062712,-0.0430964406271147,-11.3161928812542)) ;
#121935 = CARTESIAN_POINT('Origin',(6.7,0.400000000000001,-11.03)) ;
#121936 = CARTESIAN_POINT('',(6.65857864376269,0.400000000000001,-11.13)) ;
#121937 = CARTESIAN_POINT('',(6.65857864376269,0.400000000000001,-11.73)) ;
#121938 = CARTESIAN_POINT('',(6.65857864376269,0.400000000000001,-11.03)) ;
#121939 = CARTESIAN_POINT('',(6.7,0.400000000000001,-11.73)) ;
#121940 = CARTESIAN_POINT('',(6.65857864376269,0.400000000000001,-11.13)) ;
#121941 = CARTESIAN_POINT('Origin',(0.6,-0.4,-11.03)) ;
#121942 = CARTESIAN_POINT('',(6.65857864376269,-0.400000000000001,-11.73)) ;
#121943 = CARTESIAN_POINT('',(0.6,-0.4,-11.73)) ;
#121944 = CARTESIAN_POINT('',(6.65857864376269,-0.400000000000001,-11.13)) ;
#121945 = CARTESIAN_POINT('',(6.65857864376269,-0.400000000000001,-11.03)) ;
#121946 = CARTESIAN_POINT('',(2.4,-0.4,-11.13)) ;
#121947 = CARTESIAN_POINT('Origin',(6.7,-0.400000000000001,-11.03)) ;
#121948 = CARTESIAN_POINT('',(6.97071067811866,-0.129289321881346,-11.4885786437627)) ;
#121949 = CARTESIAN_POINT('',(6.97071067811866,-0.129289321881346,-11.3714213562373)) ;
#121950 = CARTESIAN_POINT('',(6.97071067811866,-0.129289321881346,-11.03)) ;
#121951 = CARTESIAN_POINT('',(6.72928932188135,-0.370710678118655,-11.13)) ;
#121952 = CARTESIAN_POINT('',(6.67642977396045,-0.423570226039553,-11.0771404520791)) ;
#121953 = CARTESIAN_POINT('',(6.72928932188135,-0.370710678118655,-11.73)) ;
#121954 = CARTESIAN_POINT('',(6.72928932188135,-0.370710678118655,-11.03)) ;
#121955 = CARTESIAN_POINT('',(6.94309644062712,-0.156903559372885,-11.5161928812542)) ;
#121956 = CARTESIAN_POINT('Origin',(7.,-0.1,-11.03)) ;
#121957 = CARTESIAN_POINT('',(7.,-0.0585786437626909,-11.3714213562373)) ;
#121958 = CARTESIAN_POINT('',(7.,-0.0585786437626909,-11.4885786437627)) ;
#121959 = CARTESIAN_POINT('',(7.,-0.0585786437626909,-11.03)) ;
#121960 = CARTESIAN_POINT('',(7.,0.0585786437626909,-11.4885786437627)) ;
#121961 = CARTESIAN_POINT('',(7.,-0.1,-11.4885786437627)) ;
#121962 = CARTESIAN_POINT('',(7.,0.0585786437626909,-11.3714213562373)) ;
#121963 = CARTESIAN_POINT('',(7.,0.0585786437626909,-11.03)) ;
#121964 = CARTESIAN_POINT('',(7.,-0.1,-11.3714213562373)) ;
#121965 = CARTESIAN_POINT('Origin',(0.6,-0.600000000000001,-11.03)) ;
#121966 = CARTESIAN_POINT('',(6.65857864376269,-0.300000000000001,-11.03)) ;
#121967 = CARTESIAN_POINT('',(6.65857864376269,0.300000000000002,-11.03)) ;
#121968 = CARTESIAN_POINT('',(6.65857864376269,-0.399999999999999,-11.03)) ;
#121969 = CARTESIAN_POINT('',(2.4,0.3,-11.03)) ;
#121970 = CARTESIAN_POINT('',(6.65857864376269,-0.300000000000001,-11.03)) ;
#121971 = CARTESIAN_POINT('Origin',(0.6,-0.600000000000001,-11.83)) ;
#121972 = CARTESIAN_POINT('',(6.65857864376269,0.300000000000002,-11.83)) ;
#121973 = CARTESIAN_POINT('',(0.6,0.299999999999999,-11.83)) ;
#121974 = CARTESIAN_POINT('',(6.65857864376269,-0.300000000000001,-11.83)) ;
#121975 = CARTESIAN_POINT('',(6.65857864376269,-0.6,-11.83)) ;
#121976 = CARTESIAN_POINT('',(0.6,-0.3,-11.83)) ;
#121977 = CARTESIAN_POINT('Origin',(-0.4,-0.600000000000001,-14.84)) ;
#121978 = CARTESIAN_POINT('',(-0.4,-0.600000000000001,-14.94)) ;
#121979 = CARTESIAN_POINT('',(-0.4,-0.600000000000001,-15.54)) ;
#121980 = CARTESIAN_POINT('',(-0.4,-0.600000000000001,-14.84)) ;
#121981 = CARTESIAN_POINT('',(-0.4,-6.05857864376269,-15.54)) ;
#121982 = CARTESIAN_POINT('',(-0.4,-0.600000000000001,-15.54)) ;
#121983 = CARTESIAN_POINT('',(-0.4,-6.05857864376269,-14.94)) ;
#121984 = CARTESIAN_POINT('',(-0.4,-6.05857864376269,-14.84)) ;
#121985 = CARTESIAN_POINT('',(-0.4,-0.600000000000001,-14.94)) ;
#121986 = CARTESIAN_POINT('Origin',(-0.4,-6.1,-14.84)) ;
#121987 = CARTESIAN_POINT('',(-0.129289321881346,-6.37071067811866,-15.2985786437627)) ;
#121988 = CARTESIAN_POINT('',(-0.129289321881346,-6.37071067811866,-15.1814213562373)) ;
#121989 = CARTESIAN_POINT('',(-0.129289321881346,-6.37071067811866,-14.84)) ;
#121990 = CARTESIAN_POINT('',(-0.370710678118655,-6.12928932188134,-14.94)) ;
#121991 = CARTESIAN_POINT('',(-0.423570226039552,-6.07642977396045,-14.8871404520791)) ;
#121992 = CARTESIAN_POINT('',(-0.370710678118655,-6.12928932188134,-15.54)) ;
#121993 = CARTESIAN_POINT('',(-0.370710678118655,-6.12928932188134,-14.84)) ;
#121994 = CARTESIAN_POINT('',(-0.156903559372884,-6.34309644062712,-15.3261928812542)) ;
#121995 = CARTESIAN_POINT('Origin',(-0.1,-6.4,-14.84)) ;
#121996 = CARTESIAN_POINT('',(0.0585786437626908,-6.4,-15.2985786437627)) ;
#121997 = CARTESIAN_POINT('',(0.0585786437626908,-6.4,-15.1814213562373)) ;
#121998 = CARTESIAN_POINT('',(0.0585786437626908,-6.4,-14.84)) ;
#121999 = CARTESIAN_POINT('',(-0.0585786437626908,-6.4,-15.1814213562373)) ;
#122000 = CARTESIAN_POINT('',(-0.1,-6.4,-15.1814213562373)) ;
#122001 = CARTESIAN_POINT('',(-0.0585786437626908,-6.4,-15.2985786437627)) ;
#122002 = CARTESIAN_POINT('',(-0.0585786437626908,-6.4,-14.84)) ;
#122003 = CARTESIAN_POINT('',(-0.1,-6.4,-15.2985786437627)) ;
#122004 = CARTESIAN_POINT('Origin',(0.1,-6.4,-14.84)) ;
#122005 = CARTESIAN_POINT('',(0.370710678118655,-6.12928932188134,-15.54)) ;
#122006 = CARTESIAN_POINT('',(0.370710678118655,-6.12928932188134,-14.94)) ;
#122007 = CARTESIAN_POINT('',(0.370710678118655,-6.12928932188134,-14.84)) ;
#122008 = CARTESIAN_POINT('',(0.129289321881346,-6.37071067811866,-15.1814213562373)) ;
#122009 = CARTESIAN_POINT('',(0.223570226039553,-6.27642977396045,-15.0871404520791)) ;
#122010 = CARTESIAN_POINT('',(0.129289321881346,-6.37071067811866,-15.2985786437627)) ;
#122011 = CARTESIAN_POINT('',(0.129289321881346,-6.37071067811866,-14.84)) ;
#122012 = CARTESIAN_POINT('',(-0.0430964406271151,-6.54309644062712,-15.1261928812542)) ;
#122013 = CARTESIAN_POINT('Origin',(0.4,-6.1,-14.84)) ;
#122014 = CARTESIAN_POINT('',(0.4,-6.05857864376269,-14.94)) ;
#122015 = CARTESIAN_POINT('',(0.4,-6.05857864376269,-15.54)) ;
#122016 = CARTESIAN_POINT('',(0.4,-6.05857864376269,-14.84)) ;
#122017 = CARTESIAN_POINT('',(0.4,-0.6,-15.54)) ;
#122018 = CARTESIAN_POINT('',(0.4,-6.1,-15.54)) ;
#122019 = CARTESIAN_POINT('',(0.4,-0.6,-14.94)) ;
#122020 = CARTESIAN_POINT('',(0.4,-0.6,-14.84)) ;
#122021 = CARTESIAN_POINT('',(0.4,-6.05857864376269,-14.94)) ;
#122022 = CARTESIAN_POINT('Origin',(0.6,-0.600000000000001,-14.84)) ;
#122023 = CARTESIAN_POINT('',(0.3,-6.05857864376269,-14.84)) ;
#122024 = CARTESIAN_POINT('',(0.3,-0.6,-14.84)) ;
#122025 = CARTESIAN_POINT('',(0.3,-0.6,-14.84)) ;
#122026 = CARTESIAN_POINT('Origin',(0.6,-0.6,-14.84)) ;
#122027 = CARTESIAN_POINT('',(-0.3,-0.600000000000001,-14.84)) ;
#122028 = CARTESIAN_POINT('Origin',(0.6,-0.600000000000001,-14.84)) ;
#122029 = CARTESIAN_POINT('',(-0.300000000000001,-6.05857864376269,-14.84)) ;
#122030 = CARTESIAN_POINT('',(-0.3,-0.600000000000001,-14.84)) ;
#122031 = CARTESIAN_POINT('',(0.4,-6.05857864376269,-14.84)) ;
#122032 = CARTESIAN_POINT('Origin',(0.6,-0.600000000000001,-15.64)) ;
#122033 = CARTESIAN_POINT('',(-0.299999999999999,-6.05857864376269,-15.64)) ;
#122034 = CARTESIAN_POINT('',(-0.3,-0.600000000000001,-15.64)) ;
#122035 = CARTESIAN_POINT('',(-0.3,-0.600000000000001,-15.64)) ;
#122036 = CARTESIAN_POINT('Origin',(0.6,-0.600000000000001,-15.64)) ;
#122037 = CARTESIAN_POINT('',(0.3,-0.6,-15.64)) ;
#122038 = CARTESIAN_POINT('Origin',(0.6,-0.6,-15.64)) ;
#122039 = CARTESIAN_POINT('',(0.3,-6.05857864376269,-15.64)) ;
#122040 = CARTESIAN_POINT('',(0.3,-0.600000000000001,-15.64)) ;
#122041 = CARTESIAN_POINT('',(0.6,-6.05857864376269,-15.64)) ;
#122042 = CARTESIAN_POINT('Origin',(0.6,-0.600000000000001,-14.84)) ;
#122043 = CARTESIAN_POINT('Origin',(0.6,-0.600000000000001,-15.54)) ;
#122044 = CARTESIAN_POINT('Origin',(0.6,-0.600000000000001,-14.94)) ;
#122045 = CARTESIAN_POINT('Origin',(0.6,-0.6,-14.84)) ;
#122046 = CARTESIAN_POINT('Origin',(0.6,-0.6,-15.54)) ;
#122047 = CARTESIAN_POINT('Origin',(0.6,-0.6,-14.94)) ;
#122048 = CARTESIAN_POINT('Origin',(7.,0.1,-14.84)) ;
#122049 = CARTESIAN_POINT('',(6.72928932188135,0.370710678118655,-15.54)) ;
#122050 = CARTESIAN_POINT('',(6.72928932188135,0.370710678118655,-14.94)) ;
#122051 = CARTESIAN_POINT('',(6.72928932188135,0.370710678118655,-14.84)) ;
#122052 = CARTESIAN_POINT('',(6.97071067811866,0.129289321881346,-15.1814213562373)) ;
#122053 = CARTESIAN_POINT('',(6.87642977396045,0.223570226039552,-15.0871404520791)) ;
#122054 = CARTESIAN_POINT('',(6.97071067811866,0.129289321881346,-15.2985786437627)) ;
#122055 = CARTESIAN_POINT('',(6.97071067811866,0.129289321881346,-14.84)) ;
#122056 = CARTESIAN_POINT('',(7.14309644062712,-0.0430964406271147,-15.1261928812542)) ;
#122057 = CARTESIAN_POINT('Origin',(6.7,0.400000000000001,-14.84)) ;
#122058 = CARTESIAN_POINT('',(6.65857864376269,0.400000000000001,-14.94)) ;
#122059 = CARTESIAN_POINT('',(6.65857864376269,0.400000000000001,-15.54)) ;
#122060 = CARTESIAN_POINT('',(6.65857864376269,0.400000000000001,-14.84)) ;
#122061 = CARTESIAN_POINT('',(6.7,0.400000000000001,-15.54)) ;
#122062 = CARTESIAN_POINT('',(6.65857864376269,0.400000000000001,-14.94)) ;
#122063 = CARTESIAN_POINT('Origin',(0.6,-0.4,-14.84)) ;
#122064 = CARTESIAN_POINT('',(6.65857864376269,-0.400000000000001,-15.54)) ;
#122065 = CARTESIAN_POINT('',(0.6,-0.4,-15.54)) ;
#122066 = CARTESIAN_POINT('',(6.65857864376269,-0.400000000000001,-14.94)) ;
#122067 = CARTESIAN_POINT('',(6.65857864376269,-0.400000000000001,-14.84)) ;
#122068 = CARTESIAN_POINT('',(2.4,-0.4,-14.94)) ;
#122069 = CARTESIAN_POINT('Origin',(6.7,-0.400000000000001,-14.84)) ;
#122070 = CARTESIAN_POINT('',(6.97071067811866,-0.129289321881346,-15.2985786437627)) ;
#122071 = CARTESIAN_POINT('',(6.97071067811866,-0.129289321881346,-15.1814213562373)) ;
#122072 = CARTESIAN_POINT('',(6.97071067811866,-0.129289321881346,-14.84)) ;
#122073 = CARTESIAN_POINT('',(6.72928932188135,-0.370710678118655,-14.94)) ;
#122074 = CARTESIAN_POINT('',(6.67642977396045,-0.423570226039552,-14.8871404520791)) ;
#122075 = CARTESIAN_POINT('',(6.72928932188135,-0.370710678118655,-15.54)) ;
#122076 = CARTESIAN_POINT('',(6.72928932188135,-0.370710678118655,-14.84)) ;
#122077 = CARTESIAN_POINT('',(6.94309644062712,-0.156903559372885,-15.3261928812542)) ;
#122078 = CARTESIAN_POINT('Origin',(7.,-0.1,-14.84)) ;
#122079 = CARTESIAN_POINT('',(7.,-0.0585786437626909,-15.1814213562373)) ;
#122080 = CARTESIAN_POINT('',(7.,-0.0585786437626909,-15.2985786437627)) ;
#122081 = CARTESIAN_POINT('',(7.,-0.0585786437626909,-14.84)) ;
#122082 = CARTESIAN_POINT('',(7.,0.0585786437626909,-15.2985786437627)) ;
#122083 = CARTESIAN_POINT('',(7.,-0.1,-15.2985786437627)) ;
#122084 = CARTESIAN_POINT('',(7.,0.0585786437626909,-15.1814213562373)) ;
#122085 = CARTESIAN_POINT('',(7.,0.0585786437626909,-14.84)) ;
#122086 = CARTESIAN_POINT('',(7.,-0.1,-15.1814213562373)) ;
#122087 = CARTESIAN_POINT('Origin',(0.6,-0.600000000000001,-14.84)) ;
#122088 = CARTESIAN_POINT('',(6.65857864376269,-0.300000000000001,-14.84)) ;
#122089 = CARTESIAN_POINT('',(6.65857864376269,0.3,-14.84)) ;
#122090 = CARTESIAN_POINT('',(6.65857864376269,-0.399999999999999,-14.84)) ;
#122091 = CARTESIAN_POINT('',(2.4,0.3,-14.84)) ;
#122092 = CARTESIAN_POINT('',(6.65857864376269,-0.300000000000001,-14.84)) ;
#122093 = CARTESIAN_POINT('Origin',(0.6,-0.600000000000001,-15.64)) ;
#122094 = CARTESIAN_POINT('',(6.65857864376269,0.300000000000003,-15.64)) ;
#122095 = CARTESIAN_POINT('',(0.6,0.299999999999999,-15.64)) ;
#122096 = CARTESIAN_POINT('',(6.65857864376269,-0.300000000000001,-15.64)) ;
#122097 = CARTESIAN_POINT('',(6.65857864376269,-0.6,-15.64)) ;
#122098 = CARTESIAN_POINT('',(0.6,-0.3,-15.64)) ;
#122099 = CARTESIAN_POINT('Origin',(-0.4,-0.600000000000001,-18.65)) ;
#122100 = CARTESIAN_POINT('',(-0.4,-0.600000000000001,-18.75)) ;
#122101 = CARTESIAN_POINT('',(-0.4,-0.600000000000001,-19.35)) ;
#122102 = CARTESIAN_POINT('',(-0.4,-0.600000000000001,-18.65)) ;
#122103 = CARTESIAN_POINT('',(-0.4,-6.05857864376269,-19.35)) ;
#122104 = CARTESIAN_POINT('',(-0.4,-0.600000000000001,-19.35)) ;
#122105 = CARTESIAN_POINT('',(-0.4,-6.05857864376269,-18.75)) ;
#122106 = CARTESIAN_POINT('',(-0.4,-6.05857864376269,-18.65)) ;
#122107 = CARTESIAN_POINT('',(-0.4,-0.600000000000001,-18.75)) ;
#122108 = CARTESIAN_POINT('Origin',(-0.4,-6.1,-18.65)) ;
#122109 = CARTESIAN_POINT('',(-0.129289321881345,-6.37071067811866,-19.1085786437627)) ;
#122110 = CARTESIAN_POINT('',(-0.129289321881346,-6.37071067811866,-18.9914213562373)) ;
#122111 = CARTESIAN_POINT('',(-0.129289321881346,-6.37071067811866,-18.65)) ;
#122112 = CARTESIAN_POINT('',(-0.370710678118655,-6.12928932188134,-18.75)) ;
#122113 = CARTESIAN_POINT('',(-0.423570226039551,-6.07642977396045,-18.6971404520791)) ;
#122114 = CARTESIAN_POINT('',(-0.370710678118655,-6.12928932188134,-19.35)) ;
#122115 = CARTESIAN_POINT('',(-0.370710678118655,-6.12928932188134,-18.65)) ;
#122116 = CARTESIAN_POINT('',(-0.156903559372884,-6.34309644062712,-19.1361928812542)) ;
#122117 = CARTESIAN_POINT('Origin',(-0.1,-6.4,-18.65)) ;
#122118 = CARTESIAN_POINT('',(0.0585786437626908,-6.4,-19.1085786437627)) ;
#122119 = CARTESIAN_POINT('',(0.0585786437626908,-6.4,-18.9914213562373)) ;
#122120 = CARTESIAN_POINT('',(0.0585786437626908,-6.4,-18.65)) ;
#122121 = CARTESIAN_POINT('',(-0.0585786437626908,-6.4,-18.9914213562373)) ;
#122122 = CARTESIAN_POINT('',(-0.1,-6.4,-18.9914213562373)) ;
#122123 = CARTESIAN_POINT('',(-0.0585786437626908,-6.4,-19.1085786437627)) ;
#122124 = CARTESIAN_POINT('',(-0.0585786437626908,-6.4,-18.65)) ;
#122125 = CARTESIAN_POINT('',(-0.1,-6.4,-19.1085786437627)) ;
#122126 = CARTESIAN_POINT('Origin',(0.1,-6.4,-18.65)) ;
#122127 = CARTESIAN_POINT('',(0.370710678118654,-6.12928932188135,-19.35)) ;
#122128 = CARTESIAN_POINT('',(0.370710678118655,-6.12928932188134,-18.75)) ;
#122129 = CARTESIAN_POINT('',(0.370710678118655,-6.12928932188134,-18.65)) ;
#122130 = CARTESIAN_POINT('',(0.129289321881346,-6.37071067811866,-18.9914213562373)) ;
#122131 = CARTESIAN_POINT('',(0.223570226039551,-6.27642977396045,-18.8971404520791)) ;
#122132 = CARTESIAN_POINT('',(0.129289321881346,-6.37071067811866,-19.1085786437627)) ;
#122133 = CARTESIAN_POINT('',(0.129289321881346,-6.37071067811866,-18.65)) ;
#122134 = CARTESIAN_POINT('',(-0.0430964406271139,-6.54309644062711,-18.9361928812542)) ;
#122135 = CARTESIAN_POINT('Origin',(0.4,-6.1,-18.65)) ;
#122136 = CARTESIAN_POINT('',(0.4,-6.05857864376269,-18.75)) ;
#122137 = CARTESIAN_POINT('',(0.4,-6.05857864376269,-19.35)) ;
#122138 = CARTESIAN_POINT('',(0.4,-6.05857864376269,-18.65)) ;
#122139 = CARTESIAN_POINT('',(0.4,-0.6,-19.35)) ;
#122140 = CARTESIAN_POINT('',(0.4,-6.1,-19.35)) ;
#122141 = CARTESIAN_POINT('',(0.4,-0.6,-18.75)) ;
#122142 = CARTESIAN_POINT('',(0.4,-0.6,-18.65)) ;
#122143 = CARTESIAN_POINT('',(0.4,-6.05857864376269,-18.75)) ;
#122144 = CARTESIAN_POINT('Origin',(0.6,-0.600000000000001,-18.65)) ;
#122145 = CARTESIAN_POINT('',(0.3,-6.05857864376269,-18.65)) ;
#122146 = CARTESIAN_POINT('',(0.3,-0.6,-18.65)) ;
#122147 = CARTESIAN_POINT('',(0.3,-0.6,-18.65)) ;
#122148 = CARTESIAN_POINT('Origin',(0.6,-0.6,-18.65)) ;
#122149 = CARTESIAN_POINT('',(-0.3,-0.600000000000001,-18.65)) ;
#122150 = CARTESIAN_POINT('Origin',(0.6,-0.600000000000001,-18.65)) ;
#122151 = CARTESIAN_POINT('',(-0.299999999999994,-6.0585786437627,-18.65)) ;
#122152 = CARTESIAN_POINT('',(-0.3,-0.600000000000001,-18.65)) ;
#122153 = CARTESIAN_POINT('',(0.4,-6.0585786437627,-18.65)) ;
#122154 = CARTESIAN_POINT('Origin',(0.6,-0.600000000000001,-19.45)) ;
#122155 = CARTESIAN_POINT('',(-0.299999999999994,-6.0585786437627,-19.45)) ;
#122156 = CARTESIAN_POINT('',(-0.3,-0.600000000000001,-19.45)) ;
#122157 = CARTESIAN_POINT('',(-0.3,-0.600000000000001,-19.45)) ;
#122158 = CARTESIAN_POINT('Origin',(0.6,-0.600000000000001,-19.45)) ;
#122159 = CARTESIAN_POINT('',(0.3,-0.6,-19.45)) ;
#122160 = CARTESIAN_POINT('Origin',(0.6,-0.6,-19.45)) ;
#122161 = CARTESIAN_POINT('',(0.3,-6.05857864376269,-19.45)) ;
#122162 = CARTESIAN_POINT('',(0.3,-0.600000000000001,-19.45)) ;
#122163 = CARTESIAN_POINT('',(0.6,-6.05857864376269,-19.45)) ;
#122164 = CARTESIAN_POINT('Origin',(0.6,-0.600000000000001,-18.65)) ;
#122165 = CARTESIAN_POINT('Origin',(0.6,-0.600000000000001,-19.35)) ;
#122166 = CARTESIAN_POINT('Origin',(0.6,-0.600000000000001,-18.75)) ;
#122167 = CARTESIAN_POINT('Origin',(0.6,-0.6,-18.65)) ;
#122168 = CARTESIAN_POINT('Origin',(0.6,-0.6,-19.35)) ;
#122169 = CARTESIAN_POINT('Origin',(0.6,-0.6,-18.75)) ;
#122170 = CARTESIAN_POINT('Origin',(7.,0.1,-18.65)) ;
#122171 = CARTESIAN_POINT('',(6.72928932188135,0.370710678118656,-19.35)) ;
#122172 = CARTESIAN_POINT('',(6.72928932188135,0.370710678118655,-18.75)) ;
#122173 = CARTESIAN_POINT('',(6.72928932188135,0.370710678118655,-18.65)) ;
#122174 = CARTESIAN_POINT('',(6.97071067811866,0.129289321881346,-18.9914213562373)) ;
#122175 = CARTESIAN_POINT('',(6.87642977396045,0.22357022603955,-18.8971404520791)) ;
#122176 = CARTESIAN_POINT('',(6.97071067811866,0.129289321881346,-19.1085786437627)) ;
#122177 = CARTESIAN_POINT('',(6.97071067811866,0.129289321881346,-18.65)) ;
#122178 = CARTESIAN_POINT('',(7.14309644062712,-0.0430964406271155,-18.9361928812542)) ;
#122179 = CARTESIAN_POINT('Origin',(6.7,0.400000000000001,-18.65)) ;
#122180 = CARTESIAN_POINT('',(6.65857864376269,0.400000000000001,-18.75)) ;
#122181 = CARTESIAN_POINT('',(6.65857864376269,0.400000000000001,-19.35)) ;
#122182 = CARTESIAN_POINT('',(6.65857864376269,0.400000000000001,-18.65)) ;
#122183 = CARTESIAN_POINT('',(6.7,0.400000000000001,-19.35)) ;
#122184 = CARTESIAN_POINT('',(6.65857864376269,0.400000000000001,-18.75)) ;
#122185 = CARTESIAN_POINT('Origin',(0.6,-0.4,-18.65)) ;
#122186 = CARTESIAN_POINT('',(6.65857864376269,-0.400000000000001,-19.35)) ;
#122187 = CARTESIAN_POINT('',(0.6,-0.4,-19.35)) ;
#122188 = CARTESIAN_POINT('',(6.65857864376269,-0.400000000000001,-18.75)) ;
#122189 = CARTESIAN_POINT('',(6.65857864376269,-0.400000000000001,-18.65)) ;
#122190 = CARTESIAN_POINT('',(2.4,-0.4,-18.75)) ;
#122191 = CARTESIAN_POINT('Origin',(6.7,-0.400000000000001,-18.65)) ;
#122192 = CARTESIAN_POINT('',(6.97071067811866,-0.129289321881345,-19.1085786437627)) ;
#122193 = CARTESIAN_POINT('',(6.97071067811866,-0.129289321881346,-18.9914213562373)) ;
#122194 = CARTESIAN_POINT('',(6.97071067811866,-0.129289321881346,-18.65)) ;
#122195 = CARTESIAN_POINT('',(6.72928932188135,-0.370710678118655,-18.75)) ;
#122196 = CARTESIAN_POINT('',(6.67642977396045,-0.423570226039551,-18.6971404520791)) ;
#122197 = CARTESIAN_POINT('',(6.72928932188135,-0.370710678118655,-19.35)) ;
#122198 = CARTESIAN_POINT('',(6.72928932188135,-0.370710678118655,-18.65)) ;
#122199 = CARTESIAN_POINT('',(6.94309644062712,-0.156903559372885,-19.1361928812542)) ;
#122200 = CARTESIAN_POINT('Origin',(7.,-0.1,-18.65)) ;
#122201 = CARTESIAN_POINT('',(7.,-0.0585786437626909,-18.9914213562373)) ;
#122202 = CARTESIAN_POINT('',(7.,-0.0585786437626909,-19.1085786437627)) ;
#122203 = CARTESIAN_POINT('',(7.,-0.0585786437626909,-18.65)) ;
#122204 = CARTESIAN_POINT('',(7.,0.0585786437626909,-19.1085786437627)) ;
#122205 = CARTESIAN_POINT('',(7.,-0.1,-19.1085786437627)) ;
#122206 = CARTESIAN_POINT('',(7.,0.0585786437626909,-18.9914213562373)) ;
#122207 = CARTESIAN_POINT('',(7.,0.0585786437626909,-18.65)) ;
#122208 = CARTESIAN_POINT('',(7.,-0.1,-18.9914213562373)) ;
#122209 = CARTESIAN_POINT('Origin',(0.6,-0.600000000000001,-18.65)) ;
#122210 = CARTESIAN_POINT('',(6.65857864376269,-0.300000000000001,-18.65)) ;
#122211 = CARTESIAN_POINT('',(6.6585786437627,0.299999999999992,-18.65)) ;
#122212 = CARTESIAN_POINT('',(6.6585786437627,-0.399999999999999,-18.65)) ;
#122213 = CARTESIAN_POINT('',(2.4,0.3,-18.65)) ;
#122214 = CARTESIAN_POINT('',(6.65857864376269,-0.300000000000001,-18.65)) ;
#122215 = CARTESIAN_POINT('Origin',(0.6,-0.600000000000001,-19.45)) ;
#122216 = CARTESIAN_POINT('',(6.65857864376269,0.299999999999998,-19.45)) ;
#122217 = CARTESIAN_POINT('',(0.6,0.299999999999999,-19.45)) ;
#122218 = CARTESIAN_POINT('',(6.65857864376269,-0.300000000000001,-19.45)) ;
#122219 = CARTESIAN_POINT('',(6.65857864376269,-0.6,-19.45)) ;
#122220 = CARTESIAN_POINT('',(0.6,-0.3,-19.45)) ;
#122221 = CARTESIAN_POINT('Origin',(-0.4,-0.600000000000001,-22.46)) ;
#122222 = CARTESIAN_POINT('',(-0.4,-0.600000000000001,-22.56)) ;
#122223 = CARTESIAN_POINT('',(-0.4,-0.600000000000001,-23.16)) ;
#122224 = CARTESIAN_POINT('',(-0.4,-0.600000000000001,-22.46)) ;
#122225 = CARTESIAN_POINT('',(-0.4,-6.05857864376269,-23.16)) ;
#122226 = CARTESIAN_POINT('',(-0.4,-0.600000000000001,-23.16)) ;
#122227 = CARTESIAN_POINT('',(-0.4,-6.05857864376269,-22.56)) ;
#122228 = CARTESIAN_POINT('',(-0.4,-6.05857864376269,-22.46)) ;
#122229 = CARTESIAN_POINT('',(-0.4,-0.600000000000001,-22.56)) ;
#122230 = CARTESIAN_POINT('Origin',(-0.4,-6.1,-22.46)) ;
#122231 = CARTESIAN_POINT('',(-0.129289321881345,-6.37071067811866,-22.9185786437627)) ;
#122232 = CARTESIAN_POINT('',(-0.129289321881346,-6.37071067811866,-22.8014213562373)) ;
#122233 = CARTESIAN_POINT('',(-0.129289321881346,-6.37071067811866,-22.46)) ;
#122234 = CARTESIAN_POINT('',(-0.370710678118655,-6.12928932188134,-22.56)) ;
#122235 = CARTESIAN_POINT('',(-0.423570226039551,-6.07642977396045,-22.5071404520791)) ;
#122236 = CARTESIAN_POINT('',(-0.370710678118655,-6.12928932188134,-23.16)) ;
#122237 = CARTESIAN_POINT('',(-0.370710678118655,-6.12928932188134,-22.46)) ;
#122238 = CARTESIAN_POINT('',(-0.156903559372884,-6.34309644062712,-22.9461928812542)) ;
#122239 = CARTESIAN_POINT('Origin',(-0.1,-6.4,-22.46)) ;
#122240 = CARTESIAN_POINT('',(0.0585786437626908,-6.4,-22.9185786437627)) ;
#122241 = CARTESIAN_POINT('',(0.0585786437626908,-6.4,-22.8014213562373)) ;
#122242 = CARTESIAN_POINT('',(0.0585786437626908,-6.4,-22.46)) ;
#122243 = CARTESIAN_POINT('',(-0.0585786437626908,-6.4,-22.8014213562373)) ;
#122244 = CARTESIAN_POINT('',(-0.1,-6.4,-22.8014213562373)) ;
#122245 = CARTESIAN_POINT('',(-0.0585786437626908,-6.4,-22.9185786437627)) ;
#122246 = CARTESIAN_POINT('',(-0.0585786437626908,-6.4,-22.46)) ;
#122247 = CARTESIAN_POINT('',(-0.1,-6.4,-22.9185786437627)) ;
#122248 = CARTESIAN_POINT('Origin',(0.1,-6.4,-22.46)) ;
#122249 = CARTESIAN_POINT('',(0.370710678118654,-6.12928932188135,-23.16)) ;
#122250 = CARTESIAN_POINT('',(0.370710678118655,-6.12928932188134,-22.56)) ;
#122251 = CARTESIAN_POINT('',(0.370710678118655,-6.12928932188134,-22.46)) ;
#122252 = CARTESIAN_POINT('',(0.129289321881346,-6.37071067811866,-22.8014213562373)) ;
#122253 = CARTESIAN_POINT('',(0.223570226039551,-6.27642977396045,-22.7071404520791)) ;
#122254 = CARTESIAN_POINT('',(0.129289321881346,-6.37071067811866,-22.9185786437627)) ;
#122255 = CARTESIAN_POINT('',(0.129289321881346,-6.37071067811866,-22.46)) ;
#122256 = CARTESIAN_POINT('',(-0.0430964406271139,-6.54309644062711,-22.7461928812542)) ;
#122257 = CARTESIAN_POINT('Origin',(0.4,-6.1,-22.46)) ;
#122258 = CARTESIAN_POINT('',(0.4,-6.05857864376269,-22.56)) ;
#122259 = CARTESIAN_POINT('',(0.4,-6.05857864376269,-23.16)) ;
#122260 = CARTESIAN_POINT('',(0.4,-6.05857864376269,-22.46)) ;
#122261 = CARTESIAN_POINT('',(0.4,-0.6,-23.16)) ;
#122262 = CARTESIAN_POINT('',(0.4,-6.1,-23.16)) ;
#122263 = CARTESIAN_POINT('',(0.4,-0.6,-22.56)) ;
#122264 = CARTESIAN_POINT('',(0.4,-0.6,-22.46)) ;
#122265 = CARTESIAN_POINT('',(0.4,-6.05857864376269,-22.56)) ;
#122266 = CARTESIAN_POINT('Origin',(0.6,-0.600000000000001,-22.46)) ;
#122267 = CARTESIAN_POINT('',(0.3,-6.05857864376269,-22.46)) ;
#122268 = CARTESIAN_POINT('',(0.3,-0.6,-22.46)) ;
#122269 = CARTESIAN_POINT('',(0.3,-0.6,-22.46)) ;
#122270 = CARTESIAN_POINT('Origin',(0.6,-0.6,-22.46)) ;
#122271 = CARTESIAN_POINT('',(-0.3,-0.600000000000001,-22.46)) ;
#122272 = CARTESIAN_POINT('Origin',(0.6,-0.600000000000001,-22.46)) ;
#122273 = CARTESIAN_POINT('',(-0.299999999999994,-6.0585786437627,-22.46)) ;
#122274 = CARTESIAN_POINT('',(-0.3,-0.600000000000001,-22.46)) ;
#122275 = CARTESIAN_POINT('',(0.4,-6.0585786437627,-22.46)) ;
#122276 = CARTESIAN_POINT('Origin',(0.6,-0.600000000000001,-23.26)) ;
#122277 = CARTESIAN_POINT('',(-0.299999999999994,-6.0585786437627,-23.26)) ;
#122278 = CARTESIAN_POINT('',(-0.3,-0.600000000000001,-23.26)) ;
#122279 = CARTESIAN_POINT('',(-0.3,-0.600000000000001,-23.26)) ;
#122280 = CARTESIAN_POINT('Origin',(0.6,-0.600000000000001,-23.26)) ;
#122281 = CARTESIAN_POINT('',(0.3,-0.6,-23.26)) ;
#122282 = CARTESIAN_POINT('Origin',(0.6,-0.6,-23.26)) ;
#122283 = CARTESIAN_POINT('',(0.3,-6.05857864376269,-23.26)) ;
#122284 = CARTESIAN_POINT('',(0.3,-0.600000000000001,-23.26)) ;
#122285 = CARTESIAN_POINT('',(0.6,-6.05857864376269,-23.26)) ;
#122286 = CARTESIAN_POINT('Origin',(0.6,-0.600000000000001,-22.46)) ;
#122287 = CARTESIAN_POINT('Origin',(0.6,-0.600000000000001,-23.16)) ;
#122288 = CARTESIAN_POINT('Origin',(0.6,-0.600000000000001,-22.56)) ;
#122289 = CARTESIAN_POINT('Origin',(0.6,-0.6,-22.46)) ;
#122290 = CARTESIAN_POINT('Origin',(0.6,-0.6,-23.16)) ;
#122291 = CARTESIAN_POINT('Origin',(0.6,-0.6,-22.56)) ;
#122292 = CARTESIAN_POINT('Origin',(7.,0.1,-22.46)) ;
#122293 = CARTESIAN_POINT('',(6.72928932188135,0.370710678118656,-23.16)) ;
#122294 = CARTESIAN_POINT('',(6.72928932188135,0.370710678118655,-22.56)) ;
#122295 = CARTESIAN_POINT('',(6.72928932188135,0.370710678118655,-22.46)) ;
#122296 = CARTESIAN_POINT('',(6.97071067811866,0.129289321881346,-22.8014213562373)) ;
#122297 = CARTESIAN_POINT('',(6.87642977396045,0.22357022603955,-22.7071404520791)) ;
#122298 = CARTESIAN_POINT('',(6.97071067811866,0.129289321881346,-22.9185786437627)) ;
#122299 = CARTESIAN_POINT('',(6.97071067811866,0.129289321881346,-22.46)) ;
#122300 = CARTESIAN_POINT('',(7.14309644062712,-0.0430964406271155,-22.7461928812542)) ;
#122301 = CARTESIAN_POINT('Origin',(6.7,0.400000000000001,-22.46)) ;
#122302 = CARTESIAN_POINT('',(6.65857864376269,0.400000000000001,-22.56)) ;
#122303 = CARTESIAN_POINT('',(6.65857864376269,0.400000000000001,-23.16)) ;
#122304 = CARTESIAN_POINT('',(6.65857864376269,0.400000000000001,-22.46)) ;
#122305 = CARTESIAN_POINT('',(6.7,0.400000000000001,-23.16)) ;
#122306 = CARTESIAN_POINT('',(6.65857864376269,0.400000000000001,-22.56)) ;
#122307 = CARTESIAN_POINT('Origin',(0.6,-0.4,-22.46)) ;
#122308 = CARTESIAN_POINT('',(6.65857864376269,-0.400000000000001,-23.16)) ;
#122309 = CARTESIAN_POINT('',(0.6,-0.4,-23.16)) ;
#122310 = CARTESIAN_POINT('',(6.65857864376269,-0.400000000000001,-22.56)) ;
#122311 = CARTESIAN_POINT('',(6.65857864376269,-0.400000000000001,-22.46)) ;
#122312 = CARTESIAN_POINT('',(2.4,-0.4,-22.56)) ;
#122313 = CARTESIAN_POINT('Origin',(6.7,-0.400000000000001,-22.46)) ;
#122314 = CARTESIAN_POINT('',(6.97071067811866,-0.129289321881345,-22.9185786437627)) ;
#122315 = CARTESIAN_POINT('',(6.97071067811866,-0.129289321881346,-22.8014213562373)) ;
#122316 = CARTESIAN_POINT('',(6.97071067811866,-0.129289321881346,-22.46)) ;
#122317 = CARTESIAN_POINT('',(6.72928932188135,-0.370710678118655,-22.56)) ;
#122318 = CARTESIAN_POINT('',(6.67642977396045,-0.423570226039551,-22.5071404520791)) ;
#122319 = CARTESIAN_POINT('',(6.72928932188135,-0.370710678118655,-23.16)) ;
#122320 = CARTESIAN_POINT('',(6.72928932188135,-0.370710678118655,-22.46)) ;
#122321 = CARTESIAN_POINT('',(6.94309644062712,-0.156903559372885,-22.9461928812542)) ;
#122322 = CARTESIAN_POINT('Origin',(7.,-0.1,-22.46)) ;
#122323 = CARTESIAN_POINT('',(7.,-0.0585786437626909,-22.8014213562373)) ;
#122324 = CARTESIAN_POINT('',(7.,-0.0585786437626909,-22.9185786437627)) ;
#122325 = CARTESIAN_POINT('',(7.,-0.0585786437626909,-22.46)) ;
#122326 = CARTESIAN_POINT('',(7.,0.0585786437626909,-22.9185786437627)) ;
#122327 = CARTESIAN_POINT('',(7.,-0.1,-22.9185786437627)) ;
#122328 = CARTESIAN_POINT('',(7.,0.0585786437626909,-22.8014213562373)) ;
#122329 = CARTESIAN_POINT('',(7.,0.0585786437626909,-22.46)) ;
#122330 = CARTESIAN_POINT('',(7.,-0.1,-22.8014213562373)) ;
#122331 = CARTESIAN_POINT('Origin',(0.6,-0.600000000000001,-22.46)) ;
#122332 = CARTESIAN_POINT('',(6.65857864376269,-0.300000000000001,-22.46)) ;
#122333 = CARTESIAN_POINT('',(6.6585786437627,0.299999999999994,-22.46)) ;
#122334 = CARTESIAN_POINT('',(6.6585786437627,-0.399999999999999,-22.46)) ;
#122335 = CARTESIAN_POINT('',(2.4,0.3,-22.46)) ;
#122336 = CARTESIAN_POINT('',(6.65857864376269,-0.300000000000001,-22.46)) ;
#122337 = CARTESIAN_POINT('Origin',(0.6,-0.600000000000001,-23.26)) ;
#122338 = CARTESIAN_POINT('',(6.65857864376269,0.299999999999998,-23.26)) ;
#122339 = CARTESIAN_POINT('',(0.6,0.299999999999999,-23.26)) ;
#122340 = CARTESIAN_POINT('',(6.65857864376269,-0.300000000000001,-23.26)) ;
#122341 = CARTESIAN_POINT('',(6.65857864376269,-0.6,-23.26)) ;
#122342 = CARTESIAN_POINT('',(0.6,-0.3,-23.26)) ;
#122343 = CARTESIAN_POINT('Origin',(-0.4,-0.600000000000001,-26.27)) ;
#122344 = CARTESIAN_POINT('',(-0.4,-0.600000000000001,-26.37)) ;
#122345 = CARTESIAN_POINT('',(-0.4,-0.600000000000001,-26.97)) ;
#122346 = CARTESIAN_POINT('',(-0.4,-0.600000000000001,-26.27)) ;
#122347 = CARTESIAN_POINT('',(-0.4,-6.05857864376269,-26.97)) ;
#122348 = CARTESIAN_POINT('',(-0.4,-0.600000000000001,-26.97)) ;
#122349 = CARTESIAN_POINT('',(-0.4,-6.05857864376269,-26.37)) ;
#122350 = CARTESIAN_POINT('',(-0.4,-6.05857864376269,-26.27)) ;
#122351 = CARTESIAN_POINT('',(-0.4,-0.600000000000001,-26.37)) ;
#122352 = CARTESIAN_POINT('Origin',(-0.4,-6.1,-26.27)) ;
#122353 = CARTESIAN_POINT('',(-0.129289321881345,-6.37071067811866,-26.7285786437627)) ;
#122354 = CARTESIAN_POINT('',(-0.129289321881346,-6.37071067811866,-26.6114213562373)) ;
#122355 = CARTESIAN_POINT('',(-0.129289321881346,-6.37071067811866,-26.27)) ;
#122356 = CARTESIAN_POINT('',(-0.370710678118655,-6.12928932188134,-26.37)) ;
#122357 = CARTESIAN_POINT('',(-0.423570226039551,-6.07642977396045,-26.3171404520791)) ;
#122358 = CARTESIAN_POINT('',(-0.370710678118655,-6.12928932188134,-26.97)) ;
#122359 = CARTESIAN_POINT('',(-0.370710678118655,-6.12928932188134,-26.27)) ;
#122360 = CARTESIAN_POINT('',(-0.156903559372884,-6.34309644062712,-26.7561928812542)) ;
#122361 = CARTESIAN_POINT('Origin',(-0.1,-6.4,-26.27)) ;
#122362 = CARTESIAN_POINT('',(0.0585786437626908,-6.4,-26.7285786437627)) ;
#122363 = CARTESIAN_POINT('',(0.0585786437626908,-6.4,-26.6114213562373)) ;
#122364 = CARTESIAN_POINT('',(0.0585786437626908,-6.4,-26.27)) ;
#122365 = CARTESIAN_POINT('',(-0.0585786437626908,-6.4,-26.6114213562373)) ;
#122366 = CARTESIAN_POINT('',(-0.1,-6.4,-26.6114213562373)) ;
#122367 = CARTESIAN_POINT('',(-0.0585786437626908,-6.4,-26.7285786437627)) ;
#122368 = CARTESIAN_POINT('',(-0.0585786437626908,-6.4,-26.27)) ;
#122369 = CARTESIAN_POINT('',(-0.1,-6.4,-26.7285786437627)) ;
#122370 = CARTESIAN_POINT('Origin',(0.1,-6.4,-26.27)) ;
#122371 = CARTESIAN_POINT('',(0.370710678118654,-6.12928932188135,-26.97)) ;
#122372 = CARTESIAN_POINT('',(0.370710678118655,-6.12928932188134,-26.37)) ;
#122373 = CARTESIAN_POINT('',(0.370710678118655,-6.12928932188134,-26.27)) ;
#122374 = CARTESIAN_POINT('',(0.129289321881346,-6.37071067811866,-26.6114213562373)) ;
#122375 = CARTESIAN_POINT('',(0.223570226039551,-6.27642977396045,-26.5171404520791)) ;
#122376 = CARTESIAN_POINT('',(0.129289321881346,-6.37071067811866,-26.7285786437627)) ;
#122377 = CARTESIAN_POINT('',(0.129289321881346,-6.37071067811866,-26.27)) ;
#122378 = CARTESIAN_POINT('',(-0.0430964406271139,-6.54309644062711,-26.5561928812542)) ;
#122379 = CARTESIAN_POINT('Origin',(0.4,-6.1,-26.27)) ;
#122380 = CARTESIAN_POINT('',(0.4,-6.05857864376269,-26.37)) ;
#122381 = CARTESIAN_POINT('',(0.4,-6.05857864376269,-26.97)) ;
#122382 = CARTESIAN_POINT('',(0.4,-6.05857864376269,-26.27)) ;
#122383 = CARTESIAN_POINT('',(0.4,-0.6,-26.97)) ;
#122384 = CARTESIAN_POINT('',(0.4,-6.1,-26.97)) ;
#122385 = CARTESIAN_POINT('',(0.4,-0.6,-26.37)) ;
#122386 = CARTESIAN_POINT('',(0.4,-0.6,-26.27)) ;
#122387 = CARTESIAN_POINT('',(0.4,-6.05857864376269,-26.37)) ;
#122388 = CARTESIAN_POINT('Origin',(0.6,-0.600000000000001,-26.27)) ;
#122389 = CARTESIAN_POINT('',(0.3,-6.05857864376269,-26.27)) ;
#122390 = CARTESIAN_POINT('',(0.3,-0.6,-26.27)) ;
#122391 = CARTESIAN_POINT('',(0.3,-0.6,-26.27)) ;
#122392 = CARTESIAN_POINT('Origin',(0.6,-0.6,-26.27)) ;
#122393 = CARTESIAN_POINT('',(-0.3,-0.600000000000001,-26.27)) ;
#122394 = CARTESIAN_POINT('Origin',(0.6,-0.600000000000001,-26.27)) ;
#122395 = CARTESIAN_POINT('',(-0.299999999999994,-6.0585786437627,-26.27)) ;
#122396 = CARTESIAN_POINT('',(-0.3,-0.600000000000001,-26.27)) ;
#122397 = CARTESIAN_POINT('',(0.4,-6.0585786437627,-26.27)) ;
#122398 = CARTESIAN_POINT('Origin',(0.6,-0.600000000000001,-27.07)) ;
#122399 = CARTESIAN_POINT('',(-0.299999999999994,-6.0585786437627,-27.07)) ;
#122400 = CARTESIAN_POINT('',(-0.3,-0.600000000000001,-27.07)) ;
#122401 = CARTESIAN_POINT('',(-0.3,-0.600000000000001,-27.07)) ;
#122402 = CARTESIAN_POINT('Origin',(0.6,-0.600000000000001,-27.07)) ;
#122403 = CARTESIAN_POINT('',(0.3,-0.6,-27.07)) ;
#122404 = CARTESIAN_POINT('Origin',(0.6,-0.6,-27.07)) ;
#122405 = CARTESIAN_POINT('',(0.3,-6.05857864376269,-27.07)) ;
#122406 = CARTESIAN_POINT('',(0.3,-0.600000000000001,-27.07)) ;
#122407 = CARTESIAN_POINT('',(0.6,-6.05857864376269,-27.07)) ;
#122408 = CARTESIAN_POINT('Origin',(0.6,-0.600000000000001,-26.27)) ;
#122409 = CARTESIAN_POINT('Origin',(0.6,-0.600000000000001,-26.97)) ;
#122410 = CARTESIAN_POINT('Origin',(0.6,-0.600000000000001,-26.37)) ;
#122411 = CARTESIAN_POINT('Origin',(0.6,-0.6,-26.27)) ;
#122412 = CARTESIAN_POINT('Origin',(0.6,-0.6,-26.97)) ;
#122413 = CARTESIAN_POINT('Origin',(0.6,-0.6,-26.37)) ;
#122414 = CARTESIAN_POINT('Origin',(7.,0.1,-26.27)) ;
#122415 = CARTESIAN_POINT('',(6.72928932188135,0.370710678118656,-26.97)) ;
#122416 = CARTESIAN_POINT('',(6.72928932188135,0.370710678118655,-26.37)) ;
#122417 = CARTESIAN_POINT('',(6.72928932188135,0.370710678118655,-26.27)) ;
#122418 = CARTESIAN_POINT('',(6.97071067811866,0.129289321881346,-26.6114213562373)) ;
#122419 = CARTESIAN_POINT('',(6.87642977396045,0.22357022603955,-26.5171404520791)) ;
#122420 = CARTESIAN_POINT('',(6.97071067811866,0.129289321881346,-26.7285786437627)) ;
#122421 = CARTESIAN_POINT('',(6.97071067811866,0.129289321881346,-26.27)) ;
#122422 = CARTESIAN_POINT('',(7.14309644062712,-0.0430964406271155,-26.5561928812542)) ;
#122423 = CARTESIAN_POINT('Origin',(6.7,0.400000000000001,-26.27)) ;
#122424 = CARTESIAN_POINT('',(6.65857864376269,0.400000000000001,-26.37)) ;
#122425 = CARTESIAN_POINT('',(6.65857864376269,0.400000000000001,-26.97)) ;
#122426 = CARTESIAN_POINT('',(6.65857864376269,0.400000000000001,-26.27)) ;
#122427 = CARTESIAN_POINT('',(6.7,0.400000000000001,-26.97)) ;
#122428 = CARTESIAN_POINT('',(6.65857864376269,0.400000000000001,-26.37)) ;
#122429 = CARTESIAN_POINT('Origin',(0.6,-0.4,-26.27)) ;
#122430 = CARTESIAN_POINT('',(6.65857864376269,-0.400000000000001,-26.97)) ;
#122431 = CARTESIAN_POINT('',(0.6,-0.4,-26.97)) ;
#122432 = CARTESIAN_POINT('',(6.65857864376269,-0.400000000000001,-26.37)) ;
#122433 = CARTESIAN_POINT('',(6.65857864376269,-0.400000000000001,-26.27)) ;
#122434 = CARTESIAN_POINT('',(2.4,-0.4,-26.37)) ;
#122435 = CARTESIAN_POINT('Origin',(6.7,-0.400000000000001,-26.27)) ;
#122436 = CARTESIAN_POINT('',(6.97071067811866,-0.129289321881345,-26.7285786437627)) ;
#122437 = CARTESIAN_POINT('',(6.97071067811866,-0.129289321881346,-26.6114213562373)) ;
#122438 = CARTESIAN_POINT('',(6.97071067811866,-0.129289321881346,-26.27)) ;
#122439 = CARTESIAN_POINT('',(6.72928932188135,-0.370710678118655,-26.37)) ;
#122440 = CARTESIAN_POINT('',(6.67642977396045,-0.423570226039551,-26.3171404520791)) ;
#122441 = CARTESIAN_POINT('',(6.72928932188135,-0.370710678118655,-26.97)) ;
#122442 = CARTESIAN_POINT('',(6.72928932188135,-0.370710678118655,-26.27)) ;
#122443 = CARTESIAN_POINT('',(6.94309644062712,-0.156903559372885,-26.7561928812542)) ;
#122444 = CARTESIAN_POINT('Origin',(7.,-0.1,-26.27)) ;
#122445 = CARTESIAN_POINT('',(7.,-0.0585786437626909,-26.6114213562373)) ;
#122446 = CARTESIAN_POINT('',(7.,-0.0585786437626909,-26.7285786437627)) ;
#122447 = CARTESIAN_POINT('',(7.,-0.0585786437626909,-26.27)) ;
#122448 = CARTESIAN_POINT('',(7.,0.0585786437626909,-26.7285786437627)) ;
#122449 = CARTESIAN_POINT('',(7.,-0.1,-26.7285786437627)) ;
#122450 = CARTESIAN_POINT('',(7.,0.0585786437626909,-26.6114213562373)) ;
#122451 = CARTESIAN_POINT('',(7.,0.0585786437626909,-26.27)) ;
#122452 = CARTESIAN_POINT('',(7.,-0.1,-26.6114213562373)) ;
#122453 = CARTESIAN_POINT('Origin',(0.6,-0.600000000000001,-26.27)) ;
#122454 = CARTESIAN_POINT('',(6.65857864376269,-0.300000000000001,-26.27)) ;
#122455 = CARTESIAN_POINT('',(6.6585786437627,0.299999999999994,-26.27)) ;
#122456 = CARTESIAN_POINT('',(6.6585786437627,-0.399999999999999,-26.27)) ;
#122457 = CARTESIAN_POINT('',(2.4,0.3,-26.27)) ;
#122458 = CARTESIAN_POINT('',(6.65857864376269,-0.300000000000001,-26.27)) ;
#122459 = CARTESIAN_POINT('Origin',(0.6,-0.600000000000001,-27.07)) ;
#122460 = CARTESIAN_POINT('',(6.65857864376269,0.299999999999998,-27.07)) ;
#122461 = CARTESIAN_POINT('',(0.6,0.299999999999999,-27.07)) ;
#122462 = CARTESIAN_POINT('',(6.65857864376269,-0.300000000000001,-27.07)) ;
#122463 = CARTESIAN_POINT('',(6.65857864376269,-0.6,-27.07)) ;
#122464 = CARTESIAN_POINT('',(0.6,-0.3,-27.07)) ;
#122465 = CARTESIAN_POINT('Origin',(-0.4,-0.600000000000001,-30.08)) ;
#122466 = CARTESIAN_POINT('',(-0.4,-0.600000000000001,-30.18)) ;
#122467 = CARTESIAN_POINT('',(-0.4,-0.600000000000001,-30.78)) ;
#122468 = CARTESIAN_POINT('',(-0.4,-0.600000000000001,-30.08)) ;
#122469 = CARTESIAN_POINT('',(-0.4,-6.05857864376269,-30.78)) ;
#122470 = CARTESIAN_POINT('',(-0.4,-0.600000000000001,-30.78)) ;
#122471 = CARTESIAN_POINT('',(-0.4,-6.05857864376269,-30.18)) ;
#122472 = CARTESIAN_POINT('',(-0.4,-6.05857864376269,-30.08)) ;
#122473 = CARTESIAN_POINT('',(-0.4,-0.600000000000001,-30.18)) ;
#122474 = CARTESIAN_POINT('Origin',(-0.4,-6.1,-30.08)) ;
#122475 = CARTESIAN_POINT('',(-0.129289321881345,-6.37071067811866,-30.5385786437627)) ;
#122476 = CARTESIAN_POINT('',(-0.129289321881346,-6.37071067811866,-30.4214213562373)) ;
#122477 = CARTESIAN_POINT('',(-0.129289321881346,-6.37071067811866,-30.08)) ;
#122478 = CARTESIAN_POINT('',(-0.370710678118655,-6.12928932188134,-30.18)) ;
#122479 = CARTESIAN_POINT('',(-0.423570226039551,-6.07642977396045,-30.1271404520791)) ;
#122480 = CARTESIAN_POINT('',(-0.370710678118655,-6.12928932188134,-30.78)) ;
#122481 = CARTESIAN_POINT('',(-0.370710678118655,-6.12928932188134,-30.08)) ;
#122482 = CARTESIAN_POINT('',(-0.156903559372884,-6.34309644062712,-30.5661928812542)) ;
#122483 = CARTESIAN_POINT('Origin',(-0.1,-6.4,-30.08)) ;
#122484 = CARTESIAN_POINT('',(0.0585786437626908,-6.4,-30.5385786437627)) ;
#122485 = CARTESIAN_POINT('',(0.0585786437626908,-6.4,-30.4214213562373)) ;
#122486 = CARTESIAN_POINT('',(0.0585786437626908,-6.4,-30.08)) ;
#122487 = CARTESIAN_POINT('',(-0.0585786437626908,-6.4,-30.4214213562373)) ;
#122488 = CARTESIAN_POINT('',(-0.1,-6.4,-30.4214213562373)) ;
#122489 = CARTESIAN_POINT('',(-0.0585786437626908,-6.4,-30.5385786437627)) ;
#122490 = CARTESIAN_POINT('',(-0.0585786437626908,-6.4,-30.08)) ;
#122491 = CARTESIAN_POINT('',(-0.1,-6.4,-30.5385786437627)) ;
#122492 = CARTESIAN_POINT('Origin',(0.1,-6.4,-30.08)) ;
#122493 = CARTESIAN_POINT('',(0.370710678118654,-6.12928932188135,-30.78)) ;
#122494 = CARTESIAN_POINT('',(0.370710678118655,-6.12928932188134,-30.18)) ;
#122495 = CARTESIAN_POINT('',(0.370710678118655,-6.12928932188134,-30.08)) ;
#122496 = CARTESIAN_POINT('',(0.129289321881346,-6.37071067811866,-30.4214213562373)) ;
#122497 = CARTESIAN_POINT('',(0.223570226039551,-6.27642977396045,-30.3271404520791)) ;
#122498 = CARTESIAN_POINT('',(0.129289321881346,-6.37071067811866,-30.5385786437627)) ;
#122499 = CARTESIAN_POINT('',(0.129289321881346,-6.37071067811866,-30.08)) ;
#122500 = CARTESIAN_POINT('',(-0.0430964406271139,-6.54309644062711,-30.3661928812542)) ;
#122501 = CARTESIAN_POINT('Origin',(0.4,-6.1,-30.08)) ;
#122502 = CARTESIAN_POINT('',(0.4,-6.05857864376269,-30.18)) ;
#122503 = CARTESIAN_POINT('',(0.4,-6.05857864376269,-30.78)) ;
#122504 = CARTESIAN_POINT('',(0.4,-6.05857864376269,-30.08)) ;
#122505 = CARTESIAN_POINT('',(0.4,-0.6,-30.78)) ;
#122506 = CARTESIAN_POINT('',(0.4,-6.1,-30.78)) ;
#122507 = CARTESIAN_POINT('',(0.4,-0.6,-30.18)) ;
#122508 = CARTESIAN_POINT('',(0.4,-0.6,-30.08)) ;
#122509 = CARTESIAN_POINT('',(0.4,-6.05857864376269,-30.18)) ;
#122510 = CARTESIAN_POINT('Origin',(0.6,-0.600000000000001,-30.08)) ;
#122511 = CARTESIAN_POINT('',(0.3,-6.05857864376269,-30.08)) ;
#122512 = CARTESIAN_POINT('',(0.3,-0.6,-30.08)) ;
#122513 = CARTESIAN_POINT('',(0.3,-0.6,-30.08)) ;
#122514 = CARTESIAN_POINT('Origin',(0.6,-0.6,-30.08)) ;
#122515 = CARTESIAN_POINT('',(-0.3,-0.600000000000001,-30.08)) ;
#122516 = CARTESIAN_POINT('Origin',(0.6,-0.600000000000001,-30.08)) ;
#122517 = CARTESIAN_POINT('',(-0.299999999999994,-6.0585786437627,-30.08)) ;
#122518 = CARTESIAN_POINT('',(-0.3,-0.600000000000001,-30.08)) ;
#122519 = CARTESIAN_POINT('',(0.4,-6.0585786437627,-30.08)) ;
#122520 = CARTESIAN_POINT('Origin',(0.6,-0.600000000000001,-30.88)) ;
#122521 = CARTESIAN_POINT('',(-0.299999999999994,-6.0585786437627,-30.88)) ;
#122522 = CARTESIAN_POINT('',(-0.3,-0.600000000000001,-30.88)) ;
#122523 = CARTESIAN_POINT('',(-0.3,-0.600000000000001,-30.88)) ;
#122524 = CARTESIAN_POINT('Origin',(0.6,-0.600000000000001,-30.88)) ;
#122525 = CARTESIAN_POINT('',(0.3,-0.6,-30.88)) ;
#122526 = CARTESIAN_POINT('Origin',(0.6,-0.6,-30.88)) ;
#122527 = CARTESIAN_POINT('',(0.3,-6.05857864376269,-30.88)) ;
#122528 = CARTESIAN_POINT('',(0.3,-0.600000000000001,-30.88)) ;
#122529 = CARTESIAN_POINT('',(0.6,-6.05857864376269,-30.88)) ;
#122530 = CARTESIAN_POINT('Origin',(0.6,-0.600000000000001,-30.08)) ;
#122531 = CARTESIAN_POINT('Origin',(0.6,-0.600000000000001,-30.78)) ;
#122532 = CARTESIAN_POINT('Origin',(0.6,-0.600000000000001,-30.18)) ;
#122533 = CARTESIAN_POINT('Origin',(0.6,-0.6,-30.08)) ;
#122534 = CARTESIAN_POINT('Origin',(0.6,-0.6,-30.78)) ;
#122535 = CARTESIAN_POINT('Origin',(0.6,-0.6,-30.18)) ;
#122536 = CARTESIAN_POINT('Origin',(7.,0.1,-30.08)) ;
#122537 = CARTESIAN_POINT('',(6.72928932188135,0.370710678118656,-30.78)) ;
#122538 = CARTESIAN_POINT('',(6.72928932188135,0.370710678118655,-30.18)) ;
#122539 = CARTESIAN_POINT('',(6.72928932188135,0.370710678118655,-30.08)) ;
#122540 = CARTESIAN_POINT('',(6.97071067811866,0.129289321881346,-30.4214213562373)) ;
#122541 = CARTESIAN_POINT('',(6.87642977396045,0.22357022603955,-30.3271404520791)) ;
#122542 = CARTESIAN_POINT('',(6.97071067811866,0.129289321881346,-30.5385786437627)) ;
#122543 = CARTESIAN_POINT('',(6.97071067811866,0.129289321881346,-30.08)) ;
#122544 = CARTESIAN_POINT('',(7.14309644062712,-0.0430964406271155,-30.3661928812542)) ;
#122545 = CARTESIAN_POINT('Origin',(6.7,0.400000000000001,-30.08)) ;
#122546 = CARTESIAN_POINT('',(6.65857864376269,0.400000000000001,-30.18)) ;
#122547 = CARTESIAN_POINT('',(6.65857864376269,0.400000000000001,-30.78)) ;
#122548 = CARTESIAN_POINT('',(6.65857864376269,0.400000000000001,-30.08)) ;
#122549 = CARTESIAN_POINT('',(6.7,0.400000000000001,-30.78)) ;
#122550 = CARTESIAN_POINT('',(6.65857864376269,0.400000000000001,-30.18)) ;
#122551 = CARTESIAN_POINT('Origin',(0.6,-0.4,-30.08)) ;
#122552 = CARTESIAN_POINT('',(6.65857864376269,-0.400000000000001,-30.78)) ;
#122553 = CARTESIAN_POINT('',(0.6,-0.4,-30.78)) ;
#122554 = CARTESIAN_POINT('',(6.65857864376269,-0.400000000000001,-30.18)) ;
#122555 = CARTESIAN_POINT('',(6.65857864376269,-0.400000000000001,-30.08)) ;
#122556 = CARTESIAN_POINT('',(2.4,-0.4,-30.18)) ;
#122557 = CARTESIAN_POINT('Origin',(6.7,-0.400000000000001,-30.08)) ;
#122558 = CARTESIAN_POINT('',(6.97071067811866,-0.129289321881345,-30.5385786437627)) ;
#122559 = CARTESIAN_POINT('',(6.97071067811866,-0.129289321881346,-30.4214213562373)) ;
#122560 = CARTESIAN_POINT('',(6.97071067811866,-0.129289321881346,-30.08)) ;
#122561 = CARTESIAN_POINT('',(6.72928932188135,-0.370710678118655,-30.18)) ;
#122562 = CARTESIAN_POINT('',(6.67642977396045,-0.423570226039551,-30.1271404520791)) ;
#122563 = CARTESIAN_POINT('',(6.72928932188135,-0.370710678118655,-30.78)) ;
#122564 = CARTESIAN_POINT('',(6.72928932188135,-0.370710678118655,-30.08)) ;
#122565 = CARTESIAN_POINT('',(6.94309644062712,-0.156903559372885,-30.5661928812542)) ;
#122566 = CARTESIAN_POINT('Origin',(7.,-0.1,-30.08)) ;
#122567 = CARTESIAN_POINT('',(7.,-0.0585786437626909,-30.4214213562373)) ;
#122568 = CARTESIAN_POINT('',(7.,-0.0585786437626909,-30.5385786437627)) ;
#122569 = CARTESIAN_POINT('',(7.,-0.0585786437626909,-30.08)) ;
#122570 = CARTESIAN_POINT('',(7.,0.0585786437626909,-30.5385786437627)) ;
#122571 = CARTESIAN_POINT('',(7.,-0.1,-30.5385786437627)) ;
#122572 = CARTESIAN_POINT('',(7.,0.0585786437626909,-30.4214213562373)) ;
#122573 = CARTESIAN_POINT('',(7.,0.0585786437626909,-30.08)) ;
#122574 = CARTESIAN_POINT('',(7.,-0.1,-30.4214213562373)) ;
#122575 = CARTESIAN_POINT('Origin',(0.6,-0.600000000000001,-30.08)) ;
#122576 = CARTESIAN_POINT('',(6.65857864376269,-0.300000000000001,-30.08)) ;
#122577 = CARTESIAN_POINT('',(6.6585786437627,0.299999999999994,-30.08)) ;
#122578 = CARTESIAN_POINT('',(6.6585786437627,-0.399999999999999,-30.08)) ;
#122579 = CARTESIAN_POINT('',(2.4,0.3,-30.08)) ;
#122580 = CARTESIAN_POINT('',(6.65857864376269,-0.300000000000001,-30.08)) ;
#122581 = CARTESIAN_POINT('Origin',(0.6,-0.600000000000001,-30.88)) ;
#122582 = CARTESIAN_POINT('',(6.65857864376269,0.299999999999998,-30.88)) ;
#122583 = CARTESIAN_POINT('',(0.6,0.299999999999999,-30.88)) ;
#122584 = CARTESIAN_POINT('',(6.65857864376269,-0.300000000000001,-30.88)) ;
#122585 = CARTESIAN_POINT('',(6.65857864376269,-0.6,-30.88)) ;
#122586 = CARTESIAN_POINT('',(0.6,-0.3,-30.88)) ;
#122587 = CARTESIAN_POINT('Origin',(-0.4,-0.600000000000001,-33.89)) ;
#122588 = CARTESIAN_POINT('',(-0.4,-0.600000000000001,-33.99)) ;
#122589 = CARTESIAN_POINT('',(-0.4,-0.600000000000001,-34.59)) ;
#122590 = CARTESIAN_POINT('',(-0.4,-0.600000000000001,-33.89)) ;
#122591 = CARTESIAN_POINT('',(-0.4,-6.05857864376269,-34.59)) ;
#122592 = CARTESIAN_POINT('',(-0.4,-0.600000000000001,-34.59)) ;
#122593 = CARTESIAN_POINT('',(-0.4,-6.05857864376269,-33.99)) ;
#122594 = CARTESIAN_POINT('',(-0.4,-6.05857864376269,-33.89)) ;
#122595 = CARTESIAN_POINT('',(-0.4,-0.600000000000001,-33.99)) ;
#122596 = CARTESIAN_POINT('Origin',(-0.4,-6.1,-33.89)) ;
#122597 = CARTESIAN_POINT('',(-0.129289321881345,-6.37071067811866,-34.3485786437627)) ;
#122598 = CARTESIAN_POINT('',(-0.129289321881346,-6.37071067811866,-34.2314213562373)) ;
#122599 = CARTESIAN_POINT('',(-0.129289321881346,-6.37071067811866,-33.89)) ;
#122600 = CARTESIAN_POINT('',(-0.370710678118655,-6.12928932188134,-33.99)) ;
#122601 = CARTESIAN_POINT('',(-0.423570226039552,-6.07642977396045,-33.9371404520791)) ;
#122602 = CARTESIAN_POINT('',(-0.370710678118655,-6.12928932188134,-34.59)) ;
#122603 = CARTESIAN_POINT('',(-0.370710678118655,-6.12928932188134,-33.89)) ;
#122604 = CARTESIAN_POINT('',(-0.156903559372882,-6.34309644062712,-34.3761928812542)) ;
#122605 = CARTESIAN_POINT('Origin',(-0.1,-6.4,-33.89)) ;
#122606 = CARTESIAN_POINT('',(0.0585786437626908,-6.4,-34.3485786437627)) ;
#122607 = CARTESIAN_POINT('',(0.0585786437626908,-6.4,-34.2314213562373)) ;
#122608 = CARTESIAN_POINT('',(0.0585786437626908,-6.4,-33.89)) ;
#122609 = CARTESIAN_POINT('',(-0.0585786437626908,-6.4,-34.2314213562373)) ;
#122610 = CARTESIAN_POINT('',(-0.1,-6.4,-34.2314213562373)) ;
#122611 = CARTESIAN_POINT('',(-0.0585786437626908,-6.4,-34.3485786437627)) ;
#122612 = CARTESIAN_POINT('',(-0.0585786437626908,-6.4,-33.89)) ;
#122613 = CARTESIAN_POINT('',(-0.1,-6.4,-34.3485786437627)) ;
#122614 = CARTESIAN_POINT('Origin',(0.1,-6.4,-33.89)) ;
#122615 = CARTESIAN_POINT('',(0.370710678118654,-6.12928932188135,-34.59)) ;
#122616 = CARTESIAN_POINT('',(0.370710678118655,-6.12928932188134,-33.99)) ;
#122617 = CARTESIAN_POINT('',(0.370710678118655,-6.12928932188134,-33.89)) ;
#122618 = CARTESIAN_POINT('',(0.129289321881346,-6.37071067811866,-34.2314213562373)) ;
#122619 = CARTESIAN_POINT('',(0.223570226039555,-6.27642977396044,-34.1371404520791)) ;
#122620 = CARTESIAN_POINT('',(0.129289321881346,-6.37071067811866,-34.3485786437627)) ;
#122621 = CARTESIAN_POINT('',(0.129289321881346,-6.37071067811866,-33.89)) ;
#122622 = CARTESIAN_POINT('',(-0.0430964406271177,-6.54309644062712,-34.1761928812542)) ;
#122623 = CARTESIAN_POINT('Origin',(0.4,-6.1,-33.89)) ;
#122624 = CARTESIAN_POINT('',(0.4,-6.05857864376269,-33.99)) ;
#122625 = CARTESIAN_POINT('',(0.4,-6.05857864376269,-34.59)) ;
#122626 = CARTESIAN_POINT('',(0.4,-6.05857864376269,-33.89)) ;
#122627 = CARTESIAN_POINT('',(0.4,-0.6,-34.59)) ;
#122628 = CARTESIAN_POINT('',(0.4,-6.1,-34.59)) ;
#122629 = CARTESIAN_POINT('',(0.4,-0.6,-33.99)) ;
#122630 = CARTESIAN_POINT('',(0.4,-0.6,-33.89)) ;
#122631 = CARTESIAN_POINT('',(0.4,-6.05857864376269,-33.99)) ;
#122632 = CARTESIAN_POINT('Origin',(0.6,-0.600000000000001,-33.89)) ;
#122633 = CARTESIAN_POINT('',(0.3,-6.05857864376269,-33.89)) ;
#122634 = CARTESIAN_POINT('',(0.3,-0.6,-33.89)) ;
#122635 = CARTESIAN_POINT('',(0.3,-0.6,-33.89)) ;
#122636 = CARTESIAN_POINT('Origin',(0.6,-0.6,-33.89)) ;
#122637 = CARTESIAN_POINT('',(-0.3,-0.600000000000001,-33.89)) ;
#122638 = CARTESIAN_POINT('Origin',(0.6,-0.600000000000001,-33.89)) ;
#122639 = CARTESIAN_POINT('',(-0.300000000000006,-6.05857864376268,-33.89)) ;
#122640 = CARTESIAN_POINT('',(-0.3,-0.600000000000001,-33.89)) ;
#122641 = CARTESIAN_POINT('',(0.4,-6.05857864376269,-33.89)) ;
#122642 = CARTESIAN_POINT('Origin',(0.6,-0.600000000000001,-34.69)) ;
#122643 = CARTESIAN_POINT('',(-0.299999999999998,-6.05857864376269,-34.69)) ;
#122644 = CARTESIAN_POINT('',(-0.3,-0.600000000000001,-34.69)) ;
#122645 = CARTESIAN_POINT('',(-0.3,-0.600000000000001,-34.69)) ;
#122646 = CARTESIAN_POINT('Origin',(0.6,-0.600000000000001,-34.69)) ;
#122647 = CARTESIAN_POINT('',(0.3,-0.6,-34.69)) ;
#122648 = CARTESIAN_POINT('Origin',(0.6,-0.6,-34.69)) ;
#122649 = CARTESIAN_POINT('',(0.3,-6.05857864376269,-34.69)) ;
#122650 = CARTESIAN_POINT('',(0.3,-0.600000000000001,-34.69)) ;
#122651 = CARTESIAN_POINT('',(0.6,-6.05857864376269,-34.69)) ;
#122652 = CARTESIAN_POINT('Origin',(0.6,-0.600000000000001,-33.89)) ;
#122653 = CARTESIAN_POINT('Origin',(0.6,-0.600000000000001,-34.59)) ;
#122654 = CARTESIAN_POINT('Origin',(0.6,-0.600000000000001,-33.99)) ;
#122655 = CARTESIAN_POINT('Origin',(0.6,-0.6,-33.89)) ;
#122656 = CARTESIAN_POINT('Origin',(0.6,-0.6,-34.59)) ;
#122657 = CARTESIAN_POINT('Origin',(0.6,-0.6,-33.99)) ;
#122658 = CARTESIAN_POINT('Origin',(7.,0.1,-33.89)) ;
#122659 = CARTESIAN_POINT('',(6.72928932188135,0.370710678118655,-34.59)) ;
#122660 = CARTESIAN_POINT('',(6.72928932188135,0.370710678118655,-33.99)) ;
#122661 = CARTESIAN_POINT('',(6.72928932188135,0.370710678118655,-33.89)) ;
#122662 = CARTESIAN_POINT('',(6.97071067811866,0.129289321881346,-34.2314213562373)) ;
#122663 = CARTESIAN_POINT('',(6.87642977396044,0.223570226039555,-34.1371404520791)) ;
#122664 = CARTESIAN_POINT('',(6.97071067811866,0.129289321881346,-34.3485786437627)) ;
#122665 = CARTESIAN_POINT('',(6.97071067811866,0.129289321881346,-33.89)) ;
#122666 = CARTESIAN_POINT('',(7.14309644062712,-0.0430964406271179,-34.1761928812542)) ;
#122667 = CARTESIAN_POINT('Origin',(6.7,0.400000000000001,-33.89)) ;
#122668 = CARTESIAN_POINT('',(6.65857864376269,0.400000000000001,-33.99)) ;
#122669 = CARTESIAN_POINT('',(6.65857864376269,0.400000000000001,-34.59)) ;
#122670 = CARTESIAN_POINT('',(6.65857864376269,0.400000000000001,-33.89)) ;
#122671 = CARTESIAN_POINT('',(6.7,0.400000000000001,-34.59)) ;
#122672 = CARTESIAN_POINT('',(6.65857864376269,0.400000000000001,-33.99)) ;
#122673 = CARTESIAN_POINT('Origin',(0.6,-0.4,-33.89)) ;
#122674 = CARTESIAN_POINT('',(6.65857864376269,-0.400000000000001,-34.59)) ;
#122675 = CARTESIAN_POINT('',(0.6,-0.4,-34.59)) ;
#122676 = CARTESIAN_POINT('',(6.65857864376269,-0.400000000000001,-33.99)) ;
#122677 = CARTESIAN_POINT('',(6.65857864376269,-0.400000000000001,-33.89)) ;
#122678 = CARTESIAN_POINT('',(2.4,-0.4,-33.99)) ;
#122679 = CARTESIAN_POINT('Origin',(6.7,-0.400000000000001,-33.89)) ;
#122680 = CARTESIAN_POINT('',(6.97071067811866,-0.129289321881345,-34.3485786437627)) ;
#122681 = CARTESIAN_POINT('',(6.97071067811866,-0.129289321881346,-34.2314213562373)) ;
#122682 = CARTESIAN_POINT('',(6.97071067811866,-0.129289321881346,-33.89)) ;
#122683 = CARTESIAN_POINT('',(6.72928932188135,-0.370710678118655,-33.99)) ;
#122684 = CARTESIAN_POINT('',(6.67642977396045,-0.423570226039555,-33.9371404520791)) ;
#122685 = CARTESIAN_POINT('',(6.72928932188135,-0.370710678118655,-34.59)) ;
#122686 = CARTESIAN_POINT('',(6.72928932188135,-0.370710678118655,-33.89)) ;
#122687 = CARTESIAN_POINT('',(6.94309644062712,-0.156903559372885,-34.3761928812542)) ;
#122688 = CARTESIAN_POINT('Origin',(7.,-0.1,-33.89)) ;
#122689 = CARTESIAN_POINT('',(7.,-0.0585786437626909,-34.2314213562373)) ;
#122690 = CARTESIAN_POINT('',(7.,-0.0585786437626909,-34.3485786437627)) ;
#122691 = CARTESIAN_POINT('',(7.,-0.0585786437626909,-33.89)) ;
#122692 = CARTESIAN_POINT('',(7.,0.0585786437626909,-34.3485786437627)) ;
#122693 = CARTESIAN_POINT('',(7.,-0.1,-34.3485786437627)) ;
#122694 = CARTESIAN_POINT('',(7.,0.0585786437626909,-34.2314213562373)) ;
#122695 = CARTESIAN_POINT('',(7.,0.0585786437626909,-33.89)) ;
#122696 = CARTESIAN_POINT('',(7.,-0.1,-34.2314213562373)) ;
#122697 = CARTESIAN_POINT('Origin',(0.6,-0.600000000000001,-33.89)) ;
#122698 = CARTESIAN_POINT('',(6.65857864376269,-0.300000000000001,-33.89)) ;
#122699 = CARTESIAN_POINT('',(6.65857864376269,0.300000000000007,-33.89)) ;
#122700 = CARTESIAN_POINT('',(6.65857864376269,-0.399999999999999,-33.89)) ;
#122701 = CARTESIAN_POINT('',(2.4,0.3,-33.89)) ;
#122702 = CARTESIAN_POINT('',(6.65857864376269,-0.300000000000001,-33.89)) ;
#122703 = CARTESIAN_POINT('Origin',(0.6,-0.600000000000001,-34.69)) ;
#122704 = CARTESIAN_POINT('',(6.65857864376269,0.3,-34.69)) ;
#122705 = CARTESIAN_POINT('',(0.6,0.299999999999999,-34.69)) ;
#122706 = CARTESIAN_POINT('',(6.65857864376269,-0.300000000000001,-34.69)) ;
#122707 = CARTESIAN_POINT('',(6.6585786437627,-0.6,-34.69)) ;
#122708 = CARTESIAN_POINT('',(0.6,-0.3,-34.69)) ;
#122709 = CARTESIAN_POINT('Origin',(0.4,-6.4,-34.39)) ;
#122710 = CARTESIAN_POINT('',(-0.0585786437626895,-6.37071067811866,-34.4192893218813)) ;
#122711 = CARTESIAN_POINT('',(-0.299999999999997,-6.12928932188135,-34.6607106781186)) ;
#122712 = CARTESIAN_POINT('',(0.113807118745769,-6.54309644062712,-34.2469035593729)) ;
#122713 = CARTESIAN_POINT('',(0.299999999999999,-6.12928932188134,-34.6607106781187)) ;
#122714 = CARTESIAN_POINT('',(0.4,-6.12928932188135,-34.6607106781186)) ;
#122715 = CARTESIAN_POINT('',(0.0585786437626844,-6.37071067811866,-34.4192893218813)) ;
#122716 = CARTESIAN_POINT('',(0.152859547920894,-6.27642977396045,-34.5135702260395)) ;
#122717 = CARTESIAN_POINT('',(0.4,-6.37071067811866,-34.4192893218813)) ;
#122718 = CARTESIAN_POINT('Origin',(0.4,-6.1,-33.89)) ;
#122719 = CARTESIAN_POINT('',(0.058578643762689,-6.37071067811866,-34.1607106781187)) ;
#122720 = CARTESIAN_POINT('',(0.300000000000011,-6.12928932188133,-33.9192893218813)) ;
#122721 = CARTESIAN_POINT('',(0.352859547920897,-6.07642977396045,-33.8664297739605)) ;
#122722 = CARTESIAN_POINT('',(-0.300000000000007,-6.12928932188133,-33.9192893218813)) ;
#122723 = CARTESIAN_POINT('',(0.4,-6.12928932188134,-33.9192893218814)) ;
#122724 = CARTESIAN_POINT('',(-0.0585786437626846,-6.37071067811866,-34.1607106781187)) ;
#122725 = CARTESIAN_POINT('',(-0.0861928812542284,-6.34309644062711,-34.1330964406271)) ;
#122726 = CARTESIAN_POINT('',(0.4,-6.37071067811866,-34.1607106781187)) ;
#122727 = CARTESIAN_POINT('Origin',(0.4,-6.4,-30.58)) ;
#122728 = CARTESIAN_POINT('',(-0.0585786437626899,-6.37071067811865,-30.6092893218813)) ;
#122729 = CARTESIAN_POINT('',(-0.299999999999994,-6.12928932188135,-30.8507106781187)) ;
#122730 = CARTESIAN_POINT('',(0.11380711874577,-6.54309644062711,-30.4369035593729)) ;
#122731 = CARTESIAN_POINT('',(0.299999999999999,-6.12928932188135,-30.8507106781187)) ;
#122732 = CARTESIAN_POINT('',(0.4,-6.12928932188134,-30.8507106781187)) ;
#122733 = CARTESIAN_POINT('',(0.058578643762692,-6.37071067811865,-30.6092893218813)) ;
#122734 = CARTESIAN_POINT('',(0.152859547920897,-6.27642977396045,-30.7035702260396)) ;
#122735 = CARTESIAN_POINT('',(0.4,-6.37071067811865,-30.6092893218813)) ;
#122736 = CARTESIAN_POINT('Origin',(0.4,-6.1,-30.08)) ;
#122737 = CARTESIAN_POINT('',(0.0585786437626916,-6.37071067811865,-30.3507106781187)) ;
#122738 = CARTESIAN_POINT('',(0.299999999999992,-6.12928932188135,-30.1092893218814)) ;
#122739 = CARTESIAN_POINT('',(0.352859547920897,-6.07642977396045,-30.0564297739604)) ;
#122740 = CARTESIAN_POINT('',(-0.299999999999994,-6.12928932188135,-30.1092893218814)) ;
#122741 = CARTESIAN_POINT('',(0.4,-6.12928932188135,-30.1092893218813)) ;
#122742 = CARTESIAN_POINT('',(-0.0585786437626909,-6.37071067811865,-30.3507106781187)) ;
#122743 = CARTESIAN_POINT('',(-0.0861928812542305,-6.34309644062712,-30.3230964406271)) ;
#122744 = CARTESIAN_POINT('',(0.4,-6.37071067811865,-30.3507106781187)) ;
#122745 = CARTESIAN_POINT('Origin',(0.4,-6.4,-26.77)) ;
#122746 = CARTESIAN_POINT('',(-0.0585786437626899,-6.37071067811865,-26.7992893218813)) ;
#122747 = CARTESIAN_POINT('',(-0.299999999999994,-6.12928932188135,-27.0407106781187)) ;
#122748 = CARTESIAN_POINT('',(0.11380711874577,-6.54309644062711,-26.6269035593729)) ;
#122749 = CARTESIAN_POINT('',(0.299999999999999,-6.12928932188135,-27.0407106781187)) ;
#122750 = CARTESIAN_POINT('',(0.4,-6.12928932188134,-27.0407106781187)) ;
#122751 = CARTESIAN_POINT('',(0.058578643762692,-6.37071067811865,-26.7992893218813)) ;
#122752 = CARTESIAN_POINT('',(0.152859547920897,-6.27642977396045,-26.8935702260396)) ;
#122753 = CARTESIAN_POINT('',(0.4,-6.37071067811865,-26.7992893218813)) ;
#122754 = CARTESIAN_POINT('Origin',(0.4,-6.1,-26.27)) ;
#122755 = CARTESIAN_POINT('',(0.0585786437626916,-6.37071067811865,-26.5407106781187)) ;
#122756 = CARTESIAN_POINT('',(0.299999999999992,-6.12928932188135,-26.2992893218814)) ;
#122757 = CARTESIAN_POINT('',(0.352859547920897,-6.07642977396045,-26.2464297739604)) ;
#122758 = CARTESIAN_POINT('',(-0.299999999999994,-6.12928932188135,-26.2992893218814)) ;
#122759 = CARTESIAN_POINT('',(0.4,-6.12928932188135,-26.2992893218813)) ;
#122760 = CARTESIAN_POINT('',(-0.0585786437626909,-6.37071067811865,-26.5407106781187)) ;
#122761 = CARTESIAN_POINT('',(-0.0861928812542305,-6.34309644062712,-26.5130964406271)) ;
#122762 = CARTESIAN_POINT('',(0.4,-6.37071067811865,-26.5407106781187)) ;
#122763 = CARTESIAN_POINT('Origin',(0.4,-6.4,-22.96)) ;
#122764 = CARTESIAN_POINT('',(-0.0585786437626899,-6.37071067811865,-22.9892893218813)) ;
#122765 = CARTESIAN_POINT('',(-0.299999999999994,-6.12928932188135,-23.2307106781187)) ;
#122766 = CARTESIAN_POINT('',(0.11380711874577,-6.54309644062711,-22.8169035593729)) ;
#122767 = CARTESIAN_POINT('',(0.299999999999999,-6.12928932188135,-23.2307106781187)) ;
#122768 = CARTESIAN_POINT('',(0.4,-6.12928932188134,-23.2307106781187)) ;
#122769 = CARTESIAN_POINT('',(0.058578643762692,-6.37071067811865,-22.9892893218813)) ;
#122770 = CARTESIAN_POINT('',(0.152859547920897,-6.27642977396045,-23.0835702260395)) ;
#122771 = CARTESIAN_POINT('',(0.4,-6.37071067811865,-22.9892893218813)) ;
#122772 = CARTESIAN_POINT('Origin',(0.4,-6.1,-22.46)) ;
#122773 = CARTESIAN_POINT('',(0.0585786437626916,-6.37071067811865,-22.7307106781187)) ;
#122774 = CARTESIAN_POINT('',(0.299999999999992,-6.12928932188135,-22.4892893218814)) ;
#122775 = CARTESIAN_POINT('',(0.352859547920897,-6.07642977396045,-22.4364297739604)) ;
#122776 = CARTESIAN_POINT('',(-0.299999999999994,-6.12928932188135,-22.4892893218814)) ;
#122777 = CARTESIAN_POINT('',(0.4,-6.12928932188135,-22.4892893218814)) ;
#122778 = CARTESIAN_POINT('',(-0.0585786437626909,-6.37071067811865,-22.7307106781187)) ;
#122779 = CARTESIAN_POINT('',(-0.0861928812542305,-6.34309644062712,-22.7030964406271)) ;
#122780 = CARTESIAN_POINT('',(0.4,-6.37071067811865,-22.7307106781187)) ;
#122781 = CARTESIAN_POINT('Origin',(0.4,-6.4,-19.15)) ;
#122782 = CARTESIAN_POINT('',(-0.0585786437626899,-6.37071067811865,-19.1792893218813)) ;
#122783 = CARTESIAN_POINT('',(-0.299999999999994,-6.12928932188135,-19.4207106781187)) ;
#122784 = CARTESIAN_POINT('',(0.11380711874577,-6.54309644062711,-19.0069035593729)) ;
#122785 = CARTESIAN_POINT('',(0.299999999999999,-6.12928932188135,-19.4207106781187)) ;
#122786 = CARTESIAN_POINT('',(0.4,-6.12928932188134,-19.4207106781187)) ;
#122787 = CARTESIAN_POINT('',(0.058578643762692,-6.37071067811865,-19.1792893218813)) ;
#122788 = CARTESIAN_POINT('',(0.152859547920897,-6.27642977396045,-19.2735702260396)) ;
#122789 = CARTESIAN_POINT('',(0.4,-6.37071067811865,-19.1792893218813)) ;
#122790 = CARTESIAN_POINT('Origin',(0.4,-6.1,-18.65)) ;
#122791 = CARTESIAN_POINT('',(0.0585786437626916,-6.37071067811865,-18.9207106781187)) ;
#122792 = CARTESIAN_POINT('',(0.299999999999992,-6.12928932188135,-18.6792893218814)) ;
#122793 = CARTESIAN_POINT('',(0.352859547920897,-6.07642977396045,-18.6264297739605)) ;
#122794 = CARTESIAN_POINT('',(-0.299999999999994,-6.12928932188135,-18.6792893218814)) ;
#122795 = CARTESIAN_POINT('',(0.4,-6.12928932188135,-18.6792893218813)) ;
#122796 = CARTESIAN_POINT('',(-0.0585786437626909,-6.37071067811865,-18.9207106781187)) ;
#122797 = CARTESIAN_POINT('',(-0.0861928812542305,-6.34309644062712,-18.8930964406271)) ;
#122798 = CARTESIAN_POINT('',(0.4,-6.37071067811865,-18.9207106781187)) ;
#122799 = CARTESIAN_POINT('Origin',(0.4,-6.4,-15.34)) ;
#122800 = CARTESIAN_POINT('',(-0.0585786437626904,-6.37071067811866,-15.3692893218813)) ;
#122801 = CARTESIAN_POINT('',(-0.299999999999999,-6.12928932188134,-15.6107106781187)) ;
#122802 = CARTESIAN_POINT('',(0.11380711874577,-6.54309644062711,-15.1969035593729)) ;
#122803 = CARTESIAN_POINT('',(0.3,-6.12928932188134,-15.6107106781187)) ;
#122804 = CARTESIAN_POINT('',(0.4,-6.12928932188134,-15.6107106781187)) ;
#122805 = CARTESIAN_POINT('',(0.0585786437626911,-6.37071067811866,-15.3692893218813)) ;
#122806 = CARTESIAN_POINT('',(0.152859547920897,-6.27642977396045,-15.4635702260396)) ;
#122807 = CARTESIAN_POINT('',(0.4,-6.37071067811866,-15.3692893218813)) ;
#122808 = CARTESIAN_POINT('Origin',(0.4,-6.1,-14.84)) ;
#122809 = CARTESIAN_POINT('',(0.0585786437626904,-6.37071067811866,-15.1107106781187)) ;
#122810 = CARTESIAN_POINT('',(0.299999999999999,-6.12928932188135,-14.8692893218813)) ;
#122811 = CARTESIAN_POINT('',(0.352859547920896,-6.07642977396045,-14.8164297739604)) ;
#122812 = CARTESIAN_POINT('',(-0.300000000000001,-6.12928932188134,-14.8692893218813)) ;
#122813 = CARTESIAN_POINT('',(0.4,-6.12928932188134,-14.8692893218813)) ;
#122814 = CARTESIAN_POINT('',(-0.0585786437626914,-6.37071067811866,-15.1107106781187)) ;
#122815 = CARTESIAN_POINT('',(-0.0861928812542312,-6.34309644062712,-15.0830964406271)) ;
#122816 = CARTESIAN_POINT('',(0.4,-6.37071067811866,-15.1107106781187)) ;
#122817 = CARTESIAN_POINT('Origin',(0.4,-6.4,-11.53)) ;
#122818 = CARTESIAN_POINT('',(-0.0585786437626916,-6.37071067811866,-11.5592893218813)) ;
#122819 = CARTESIAN_POINT('',(-0.3,-6.12928932188135,-11.8007106781187)) ;
#122820 = CARTESIAN_POINT('',(0.113807118745769,-6.54309644062712,-11.3869035593729)) ;
#122821 = CARTESIAN_POINT('',(0.299999999999998,-6.12928932188135,-11.8007106781187)) ;
#122822 = CARTESIAN_POINT('',(0.4,-6.12928932188134,-11.8007106781187)) ;
#122823 = CARTESIAN_POINT('',(0.0585786437626907,-6.37071067811866,-11.5592893218813)) ;
#122824 = CARTESIAN_POINT('',(0.152859547920896,-6.27642977396045,-11.6535702260396)) ;
#122825 = CARTESIAN_POINT('',(0.4,-6.37071067811866,-11.5592893218813)) ;
#122826 = CARTESIAN_POINT('Origin',(0.4,-6.1,-11.03)) ;
#122827 = CARTESIAN_POINT('',(0.0585786437626913,-6.37071067811866,-11.3007106781187)) ;
#122828 = CARTESIAN_POINT('',(0.300000000000001,-6.12928932188134,-11.0592893218813)) ;
#122829 = CARTESIAN_POINT('',(0.352859547920897,-6.07642977396045,-11.0064297739604)) ;
#122830 = CARTESIAN_POINT('',(-0.300000000000003,-6.12928932188134,-11.0592893218813)) ;
#122831 = CARTESIAN_POINT('',(0.4,-6.12928932188134,-11.0592893218813)) ;
#122832 = CARTESIAN_POINT('',(-0.0585786437626915,-6.37071067811866,-11.3007106781187)) ;
#122833 = CARTESIAN_POINT('',(-0.0861928812542312,-6.34309644062712,-11.2730964406271)) ;
#122834 = CARTESIAN_POINT('',(0.4,-6.37071067811866,-11.3007106781187)) ;
#122835 = CARTESIAN_POINT('Origin',(0.4,-6.4,-7.72)) ;
#122836 = CARTESIAN_POINT('',(-0.0585786437626906,-6.37071067811866,-7.74928932188134)) ;
#122837 = CARTESIAN_POINT('',(-0.299999999999999,-6.12928932188134,-7.99071067811865)) ;
#122838 = CARTESIAN_POINT('',(0.113807118745769,-6.54309644062711,-7.57690355937288)) ;
#122839 = CARTESIAN_POINT('',(0.3,-6.12928932188134,-7.99071067811865)) ;
#122840 = CARTESIAN_POINT('',(0.4,-6.12928932188134,-7.99071067811866)) ;
#122841 = CARTESIAN_POINT('',(0.0585786437626912,-6.37071067811866,-7.74928932188134)) ;
#122842 = CARTESIAN_POINT('',(0.152859547920897,-6.27642977396045,-7.84357022603955)) ;
#122843 = CARTESIAN_POINT('',(0.4,-6.37071067811866,-7.74928932188134)) ;
#122844 = CARTESIAN_POINT('Origin',(0.4,-6.1,-7.22)) ;
#122845 = CARTESIAN_POINT('',(0.0585786437626908,-6.37071067811866,-7.49071067811866)) ;
#122846 = CARTESIAN_POINT('',(0.300000000000002,-6.12928932188134,-7.24928932188134)) ;
#122847 = CARTESIAN_POINT('',(0.352859547920897,-6.07642977396045,-7.19642977396045)) ;
#122848 = CARTESIAN_POINT('',(-0.300000000000001,-6.12928932188134,-7.24928932188134)) ;
#122849 = CARTESIAN_POINT('',(0.4,-6.12928932188134,-7.24928932188134)) ;
#122850 = CARTESIAN_POINT('',(-0.0585786437626907,-6.37071067811866,-7.49071067811866)) ;
#122851 = CARTESIAN_POINT('',(-0.0861928812542307,-6.34309644062712,-7.46309644062712)) ;
#122852 = CARTESIAN_POINT('',(0.4,-6.37071067811866,-7.49071067811866)) ;
#122853 = CARTESIAN_POINT('Origin',(0.4,-6.4,-3.91)) ;
#122854 = CARTESIAN_POINT('',(-0.0585786437626904,-6.37071067811866,-3.93928932188134)) ;
#122855 = CARTESIAN_POINT('',(-0.300000000000001,-6.12928932188134,-4.18071067811866)) ;
#122856 = CARTESIAN_POINT('',(0.11380711874577,-6.54309644062711,-3.76690355937288)) ;
#122857 = CARTESIAN_POINT('',(0.300000000000001,-6.12928932188134,-4.18071067811866)) ;
#122858 = CARTESIAN_POINT('',(0.4,-6.12928932188134,-4.18071067811865)) ;
#122859 = CARTESIAN_POINT('',(0.0585786437626911,-6.37071067811866,-3.93928932188134)) ;
#122860 = CARTESIAN_POINT('',(0.152859547920897,-6.27642977396045,-4.03357022603955)) ;
#122861 = CARTESIAN_POINT('',(0.4,-6.37071067811866,-3.93928932188134)) ;
#122862 = CARTESIAN_POINT('Origin',(0.4,-6.1,-3.41)) ;
#122863 = CARTESIAN_POINT('',(0.0585786437626907,-6.37071067811866,-3.68071067811866)) ;
#122864 = CARTESIAN_POINT('',(0.299999999999999,-6.12928932188135,-3.43928932188135)) ;
#122865 = CARTESIAN_POINT('',(0.352859547920897,-6.07642977396045,-3.38642977396045)) ;
#122866 = CARTESIAN_POINT('',(-0.299999999999999,-6.12928932188135,-3.43928932188135)) ;
#122867 = CARTESIAN_POINT('',(0.4,-6.12928932188134,-3.43928932188135)) ;
#122868 = CARTESIAN_POINT('',(-0.0585786437626909,-6.37071067811866,-3.68071067811866)) ;
#122869 = CARTESIAN_POINT('',(-0.086192881254231,-6.34309644062712,-3.65309644062712)) ;
#122870 = CARTESIAN_POINT('',(0.4,-6.37071067811866,-3.68071067811866)) ;
#122871 = CARTESIAN_POINT('Origin',(6.7,-0.399999999999999,-34.69)) ;
#122872 = CARTESIAN_POINT('',(6.97071067811865,-0.0585786437626952,-34.4192893218813)) ;
#122873 = CARTESIAN_POINT('',(6.72928932188135,-0.300000000000001,-34.6607106781186)) ;
#122874 = CARTESIAN_POINT('',(6.67642977396045,-0.352859547920898,-34.7135702260396)) ;
#122875 = CARTESIAN_POINT('',(6.72928932188134,0.3,-34.6607106781187)) ;
#122876 = CARTESIAN_POINT('',(6.72928932188135,-0.399999999999999,-34.6607106781186)) ;
#122877 = CARTESIAN_POINT('',(6.97071067811865,0.0585786437626901,-34.4192893218813)) ;
#122878 = CARTESIAN_POINT('',(6.94309644062711,0.0861928812542281,-34.4469035593729)) ;
#122879 = CARTESIAN_POINT('',(6.97071067811865,-0.4,-34.4192893218813)) ;
#122880 = CARTESIAN_POINT('Origin',(7.,-0.399999999999999,-34.19)) ;
#122881 = CARTESIAN_POINT('',(6.97071067811866,0.0585786437626919,-34.1607106781187)) ;
#122882 = CARTESIAN_POINT('',(6.72928932188134,0.300000000000006,-33.9192893218814)) ;
#122883 = CARTESIAN_POINT('',(7.14309644062712,-0.113807118745768,-34.3330964406271)) ;
#122884 = CARTESIAN_POINT('',(6.72928932188134,-0.300000000000007,-33.9192893218813)) ;
#122885 = CARTESIAN_POINT('',(6.72928932188134,-0.399999999999999,-33.9192893218814)) ;
#122886 = CARTESIAN_POINT('',(6.97071067811866,-0.058578643762684,-34.1607106781187)) ;
#122887 = CARTESIAN_POINT('',(6.87642977396045,-0.152859547920894,-34.0664297739605)) ;
#122888 = CARTESIAN_POINT('',(6.97071067811866,-0.399999999999999,-34.1607106781187)) ;
#122889 = CARTESIAN_POINT('Origin',(6.7,-0.399999999999999,-30.88)) ;
#122890 = CARTESIAN_POINT('',(6.97071067811866,-0.0585786437626901,-30.6092893218813)) ;
#122891 = CARTESIAN_POINT('',(6.72928932188135,-0.299999999999997,-30.8507106781187)) ;
#122892 = CARTESIAN_POINT('',(6.67642977396045,-0.352859547920897,-30.9035702260396)) ;
#122893 = CARTESIAN_POINT('',(6.72928932188135,0.299999999999998,-30.8507106781187)) ;
#122894 = CARTESIAN_POINT('',(6.72928932188135,-0.399999999999999,-30.8507106781187)) ;
#122895 = CARTESIAN_POINT('',(6.97071067811866,0.0585786437626903,-30.6092893218813)) ;
#122896 = CARTESIAN_POINT('',(6.94309644062712,0.0861928812542301,-30.6369035593729)) ;
#122897 = CARTESIAN_POINT('',(6.97071067811866,-0.4,-30.6092893218813)) ;
#122898 = CARTESIAN_POINT('Origin',(7.,-0.399999999999999,-30.38)) ;
#122899 = CARTESIAN_POINT('',(6.97071067811865,0.058578643762691,-30.3507106781187)) ;
#122900 = CARTESIAN_POINT('',(6.72928932188135,0.299999999999994,-30.1092893218813)) ;
#122901 = CARTESIAN_POINT('',(7.14309644062712,-0.11380711874577,-30.5230964406271)) ;
#122902 = CARTESIAN_POINT('',(6.72928932188135,-0.299999999999999,-30.1092893218813)) ;
#122903 = CARTESIAN_POINT('',(6.72928932188135,-0.399999999999999,-30.1092893218813)) ;
#122904 = CARTESIAN_POINT('',(6.97071067811865,-0.0585786437626907,-30.3507106781187)) ;
#122905 = CARTESIAN_POINT('',(6.87642977396045,-0.152859547920896,-30.2564297739604)) ;
#122906 = CARTESIAN_POINT('',(6.97071067811865,-0.399999999999999,-30.3507106781187)) ;
#122907 = CARTESIAN_POINT('Origin',(6.7,-0.399999999999999,-27.07)) ;
#122908 = CARTESIAN_POINT('',(6.97071067811866,-0.0585786437626901,-26.7992893218813)) ;
#122909 = CARTESIAN_POINT('',(6.72928932188135,-0.299999999999997,-27.0407106781187)) ;
#122910 = CARTESIAN_POINT('',(6.67642977396045,-0.352859547920897,-27.0935702260396)) ;
#122911 = CARTESIAN_POINT('',(6.72928932188135,0.299999999999998,-27.0407106781187)) ;
#122912 = CARTESIAN_POINT('',(6.72928932188135,-0.399999999999999,-27.0407106781187)) ;
#122913 = CARTESIAN_POINT('',(6.97071067811866,0.0585786437626903,-26.7992893218813)) ;
#122914 = CARTESIAN_POINT('',(6.94309644062712,0.0861928812542301,-26.8269035593729)) ;
#122915 = CARTESIAN_POINT('',(6.97071067811866,-0.4,-26.7992893218813)) ;
#122916 = CARTESIAN_POINT('Origin',(7.,-0.399999999999999,-26.57)) ;
#122917 = CARTESIAN_POINT('',(6.97071067811865,0.058578643762691,-26.5407106781187)) ;
#122918 = CARTESIAN_POINT('',(6.72928932188135,0.299999999999994,-26.2992893218813)) ;
#122919 = CARTESIAN_POINT('',(7.14309644062712,-0.11380711874577,-26.7130964406271)) ;
#122920 = CARTESIAN_POINT('',(6.72928932188135,-0.299999999999999,-26.2992893218813)) ;
#122921 = CARTESIAN_POINT('',(6.72928932188135,-0.399999999999999,-26.2992893218813)) ;
#122922 = CARTESIAN_POINT('',(6.97071067811865,-0.0585786437626907,-26.5407106781187)) ;
#122923 = CARTESIAN_POINT('',(6.87642977396045,-0.152859547920896,-26.4464297739605)) ;
#122924 = CARTESIAN_POINT('',(6.97071067811865,-0.399999999999999,-26.5407106781187)) ;
#122925 = CARTESIAN_POINT('Origin',(6.7,-0.399999999999999,-23.26)) ;
#122926 = CARTESIAN_POINT('',(6.97071067811866,-0.0585786437626901,-22.9892893218813)) ;
#122927 = CARTESIAN_POINT('',(6.72928932188135,-0.299999999999997,-23.2307106781187)) ;
#122928 = CARTESIAN_POINT('',(6.67642977396045,-0.352859547920897,-23.2835702260396)) ;
#122929 = CARTESIAN_POINT('',(6.72928932188135,0.299999999999998,-23.2307106781187)) ;
#122930 = CARTESIAN_POINT('',(6.72928932188135,-0.399999999999999,-23.2307106781187)) ;
#122931 = CARTESIAN_POINT('',(6.97071067811866,0.0585786437626903,-22.9892893218813)) ;
#122932 = CARTESIAN_POINT('',(6.94309644062712,0.0861928812542301,-23.0169035593729)) ;
#122933 = CARTESIAN_POINT('',(6.97071067811866,-0.4,-22.9892893218813)) ;
#122934 = CARTESIAN_POINT('Origin',(7.,-0.399999999999999,-22.76)) ;
#122935 = CARTESIAN_POINT('',(6.97071067811865,0.058578643762691,-22.7307106781187)) ;
#122936 = CARTESIAN_POINT('',(6.72928932188135,0.299999999999994,-22.4892893218814)) ;
#122937 = CARTESIAN_POINT('',(7.14309644062712,-0.11380711874577,-22.9030964406271)) ;
#122938 = CARTESIAN_POINT('',(6.72928932188135,-0.299999999999999,-22.4892893218813)) ;
#122939 = CARTESIAN_POINT('',(6.72928932188135,-0.399999999999999,-22.4892893218814)) ;
#122940 = CARTESIAN_POINT('',(6.97071067811865,-0.0585786437626907,-22.7307106781187)) ;
#122941 = CARTESIAN_POINT('',(6.87642977396045,-0.152859547920896,-22.6364297739605)) ;
#122942 = CARTESIAN_POINT('',(6.97071067811865,-0.399999999999999,-22.7307106781187)) ;
#122943 = CARTESIAN_POINT('Origin',(6.7,-0.399999999999999,-19.45)) ;
#122944 = CARTESIAN_POINT('',(6.97071067811866,-0.0585786437626901,-19.1792893218813)) ;
#122945 = CARTESIAN_POINT('',(6.72928932188135,-0.299999999999997,-19.4207106781187)) ;
#122946 = CARTESIAN_POINT('',(6.67642977396045,-0.352859547920897,-19.4735702260396)) ;
#122947 = CARTESIAN_POINT('',(6.72928932188135,0.299999999999998,-19.4207106781187)) ;
#122948 = CARTESIAN_POINT('',(6.72928932188135,-0.399999999999999,-19.4207106781187)) ;
#122949 = CARTESIAN_POINT('',(6.97071067811866,0.0585786437626903,-19.1792893218813)) ;
#122950 = CARTESIAN_POINT('',(6.94309644062712,0.0861928812542301,-19.2069035593729)) ;
#122951 = CARTESIAN_POINT('',(6.97071067811866,-0.4,-19.1792893218813)) ;
#122952 = CARTESIAN_POINT('Origin',(7.,-0.399999999999999,-18.95)) ;
#122953 = CARTESIAN_POINT('',(6.97071067811865,0.058578643762691,-18.9207106781187)) ;
#122954 = CARTESIAN_POINT('',(6.72928932188135,0.299999999999992,-18.6792893218814)) ;
#122955 = CARTESIAN_POINT('',(7.14309644062712,-0.11380711874577,-19.0930964406271)) ;
#122956 = CARTESIAN_POINT('',(6.72928932188135,-0.299999999999999,-18.6792893218813)) ;
#122957 = CARTESIAN_POINT('',(6.72928932188135,-0.399999999999999,-18.6792893218813)) ;
#122958 = CARTESIAN_POINT('',(6.97071067811865,-0.0585786437626907,-18.9207106781187)) ;
#122959 = CARTESIAN_POINT('',(6.87642977396045,-0.152859547920896,-18.8264297739604)) ;
#122960 = CARTESIAN_POINT('',(6.97071067811865,-0.399999999999999,-18.9207106781187)) ;
#122961 = CARTESIAN_POINT('Origin',(6.7,-0.399999999999999,-15.64)) ;
#122962 = CARTESIAN_POINT('',(6.97071067811866,-0.058578643762691,-15.3692893218813)) ;
#122963 = CARTESIAN_POINT('',(6.72928932188135,-0.299999999999999,-15.6107106781187)) ;
#122964 = CARTESIAN_POINT('',(6.67642977396045,-0.352859547920897,-15.6635702260396)) ;
#122965 = CARTESIAN_POINT('',(6.72928932188134,0.300000000000003,-15.6107106781187)) ;
#122966 = CARTESIAN_POINT('',(6.72928932188135,-0.399999999999999,-15.6107106781187)) ;
#122967 = CARTESIAN_POINT('',(6.97071067811866,0.0585786437626913,-15.3692893218813)) ;
#122968 = CARTESIAN_POINT('',(6.94309644062712,0.086192881254231,-15.3969035593729)) ;
#122969 = CARTESIAN_POINT('',(6.97071067811866,-0.4,-15.3692893218813)) ;
#122970 = CARTESIAN_POINT('Origin',(7.,-0.399999999999999,-15.14)) ;
#122971 = CARTESIAN_POINT('',(6.97071067811865,0.0585786437626917,-15.1107106781187)) ;
#122972 = CARTESIAN_POINT('',(6.72928932188135,0.3,-14.8692893218813)) ;
#122973 = CARTESIAN_POINT('',(7.14309644062712,-0.11380711874577,-15.2830964406271)) ;
#122974 = CARTESIAN_POINT('',(6.72928932188135,-0.299999999999999,-14.8692893218813)) ;
#122975 = CARTESIAN_POINT('',(6.72928932188135,-0.399999999999999,-14.8692893218813)) ;
#122976 = CARTESIAN_POINT('',(6.97071067811865,-0.0585786437626915,-15.1107106781187)) ;
#122977 = CARTESIAN_POINT('',(6.87642977396045,-0.152859547920897,-15.0164297739605)) ;
#122978 = CARTESIAN_POINT('',(6.97071067811865,-0.399999999999999,-15.1107106781187)) ;
#122979 = CARTESIAN_POINT('Origin',(6.7,-0.399999999999999,-11.83)) ;
#122980 = CARTESIAN_POINT('',(6.97071067811866,-0.058578643762691,-11.5592893218813)) ;
#122981 = CARTESIAN_POINT('',(6.72928932188134,-0.300000000000002,-11.8007106781187)) ;
#122982 = CARTESIAN_POINT('',(6.67642977396045,-0.352859547920897,-11.8535702260395)) ;
#122983 = CARTESIAN_POINT('',(6.72928932188135,0.300000000000002,-11.8007106781187)) ;
#122984 = CARTESIAN_POINT('',(6.72928932188135,-0.399999999999999,-11.8007106781187)) ;
#122985 = CARTESIAN_POINT('',(6.97071067811866,0.0585786437626919,-11.5592893218813)) ;
#122986 = CARTESIAN_POINT('',(6.94309644062712,0.0861928812542313,-11.5869035593729)) ;
#122987 = CARTESIAN_POINT('',(6.97071067811866,-0.4,-11.5592893218813)) ;
#122988 = CARTESIAN_POINT('Origin',(7.,-0.399999999999999,-11.33)) ;
#122989 = CARTESIAN_POINT('',(6.97071067811865,0.0585786437626923,-11.3007106781187)) ;
#122990 = CARTESIAN_POINT('',(6.72928932188135,0.300000000000001,-11.0592893218813)) ;
#122991 = CARTESIAN_POINT('',(7.14309644062712,-0.113807118745769,-11.4730964406271)) ;
#122992 = CARTESIAN_POINT('',(6.72928932188135,-0.300000000000002,-11.0592893218813)) ;
#122993 = CARTESIAN_POINT('',(6.72928932188134,-0.399999999999999,-11.0592893218813)) ;
#122994 = CARTESIAN_POINT('',(6.97071067811865,-0.0585786437626925,-11.3007106781187)) ;
#122995 = CARTESIAN_POINT('',(6.87642977396045,-0.152859547920897,-11.2064297739604)) ;
#122996 = CARTESIAN_POINT('',(6.97071067811865,-0.399999999999999,-11.3007106781187)) ;
#122997 = CARTESIAN_POINT('Origin',(6.7,-0.399999999999999,-8.02)) ;
#122998 = CARTESIAN_POINT('',(6.97071067811866,-0.0585786437626908,-7.74928932188134)) ;
#122999 = CARTESIAN_POINT('',(6.72928932188134,-0.300000000000002,-7.99071067811866)) ;
#123000 = CARTESIAN_POINT('',(6.67642977396045,-0.352859547920897,-8.04357022603955)) ;
#123001 = CARTESIAN_POINT('',(6.72928932188135,0.300000000000002,-7.99071067811866)) ;
#123002 = CARTESIAN_POINT('',(6.72928932188135,-0.399999999999999,-7.99071067811866)) ;
#123003 = CARTESIAN_POINT('',(6.97071067811866,0.0585786437626916,-7.74928932188134)) ;
#123004 = CARTESIAN_POINT('',(6.94309644062712,0.0861928812542312,-7.77690355937288)) ;
#123005 = CARTESIAN_POINT('',(6.97071067811866,-0.4,-7.74928932188134)) ;
#123006 = CARTESIAN_POINT('Origin',(7.,-0.399999999999999,-7.52)) ;
#123007 = CARTESIAN_POINT('',(6.97071067811866,0.0585786437626905,-7.49071067811866)) ;
#123008 = CARTESIAN_POINT('',(6.72928932188134,0.300000000000002,-7.24928932188134)) ;
#123009 = CARTESIAN_POINT('',(7.14309644062712,-0.11380711874577,-7.66309644062712)) ;
#123010 = CARTESIAN_POINT('',(6.72928932188135,-0.300000000000002,-7.24928932188134)) ;
#123011 = CARTESIAN_POINT('',(6.72928932188135,-0.399999999999999,-7.24928932188134)) ;
#123012 = CARTESIAN_POINT('',(6.97071067811866,-0.058578643762691,-7.49071067811866)) ;
#123013 = CARTESIAN_POINT('',(6.87642977396045,-0.152859547920897,-7.39642977396045)) ;
#123014 = CARTESIAN_POINT('',(6.97071067811866,-0.399999999999999,-7.49071067811866)) ;
#123015 = CARTESIAN_POINT('Origin',(6.7,-0.399999999999999,-4.21)) ;
#123016 = CARTESIAN_POINT('',(6.97071067811866,-0.058578643762691,-3.93928932188135)) ;
#123017 = CARTESIAN_POINT('',(6.72928932188135,-0.300000000000001,-4.18071067811866)) ;
#123018 = CARTESIAN_POINT('',(6.67642977396045,-0.352859547920897,-4.23357022603955)) ;
#123019 = CARTESIAN_POINT('',(6.72928932188135,0.300000000000001,-4.18071067811866)) ;
#123020 = CARTESIAN_POINT('',(6.72928932188135,-0.399999999999999,-4.18071067811866)) ;
#123021 = CARTESIAN_POINT('',(6.97071067811866,0.0585786437626911,-3.93928932188135)) ;
#123022 = CARTESIAN_POINT('',(6.94309644062712,0.0861928812542308,-3.96690355937289)) ;
#123023 = CARTESIAN_POINT('',(6.97071067811866,-0.4,-3.93928932188135)) ;
#123024 = CARTESIAN_POINT('Origin',(7.,-0.399999999999999,-3.71)) ;
#123025 = CARTESIAN_POINT('',(6.97071067811866,0.058578643762691,-3.68071067811866)) ;
#123026 = CARTESIAN_POINT('',(6.72928932188135,0.3,-3.43928932188135)) ;
#123027 = CARTESIAN_POINT('',(7.14309644062712,-0.11380711874577,-3.85309644062712)) ;
#123028 = CARTESIAN_POINT('',(6.72928932188135,-0.3,-3.43928932188135)) ;
#123029 = CARTESIAN_POINT('',(6.72928932188135,-0.399999999999999,-3.43928932188135)) ;
#123030 = CARTESIAN_POINT('',(6.97071067811866,-0.0585786437626913,-3.68071067811866)) ;
#123031 = CARTESIAN_POINT('',(6.87642977396045,-0.152859547920897,-3.58642977396045)) ;
#123032 = CARTESIAN_POINT('',(6.97071067811866,-0.399999999999999,-3.68071067811866)) ;
#123033 = CARTESIAN_POINT('Origin',(-0.113807118745769,-6.47238576250846,
-3.69619288125423)) ;
#123034 = CARTESIAN_POINT('Origin',(0.3,-6.05857864376269,-4.11)) ;
#123035 = CARTESIAN_POINT('Origin',(0.0585786437626911,-6.3,-3.86857864376269)) ;
#123036 = CARTESIAN_POINT('Origin',(0.3,-6.05857864376269,-3.41)) ;
#123037 = CARTESIAN_POINT('Origin',(0.3,-6.05857864376269,-4.11)) ;
#123038 = CARTESIAN_POINT('Origin',(0.3,-6.05857864376269,-3.51)) ;
#123039 = CARTESIAN_POINT('Origin',(0.0585786437626908,-6.3,-3.86857864376269)) ;
#123040 = CARTESIAN_POINT('Origin',(0.0585786437626908,-6.3,-3.86857864376269)) ;
#123041 = CARTESIAN_POINT('Origin',(0.0585786437626908,-6.3,-3.86857864376269)) ;
#123042 = CARTESIAN_POINT('Origin',(0.152859547920897,-6.20571909584179,-3.6571404520791)) ;
#123043 = CARTESIAN_POINT('Origin',(0.3,-6.05857864376269,-3.51)) ;
#123044 = CARTESIAN_POINT('Origin',(0.0585786437626908,-6.3,-3.75142135623731)) ;
#123045 = CARTESIAN_POINT('Origin',(0.0585786437626908,-6.3,-3.41)) ;
#123046 = CARTESIAN_POINT('Origin',(0.0585786437626908,-6.3,-3.75142135623731)) ;
#123047 = CARTESIAN_POINT('Origin',(0.4,-6.3,-3.86857864376269)) ;
#123048 = CARTESIAN_POINT('Origin',(-0.0585786437626904,-6.3,-3.86857864376269)) ;
#123049 = CARTESIAN_POINT('Origin',(0.0585786437626908,-6.3,-3.75142135623731)) ;
#123050 = CARTESIAN_POINT('Origin',(0.0585786437626907,-6.3,-3.75142135623731)) ;
#123051 = CARTESIAN_POINT('Origin',(-0.0585786437626908,-6.3,-3.86857864376269)) ;
#123052 = CARTESIAN_POINT('Origin',(-0.0585786437626908,-6.3,-3.86857864376269)) ;
#123053 = CARTESIAN_POINT('Origin',(-0.0585786437626908,-6.3,-3.86857864376269)) ;
#123054 = CARTESIAN_POINT('Origin',(-0.1,-6.3,-3.75142135623731)) ;
#123055 = CARTESIAN_POINT('Origin',(-0.0585786437626908,-6.3,-3.75142135623731)) ;
#123056 = CARTESIAN_POINT('Origin',(-0.0585786437626908,-6.3,-3.41)) ;
#123057 = CARTESIAN_POINT('Origin',(-0.0585786437626908,-6.3,-3.75142135623731)) ;
#123058 = CARTESIAN_POINT('Origin',(-0.0861928812542299,-6.27238576250846,
-3.89619288125423)) ;
#123059 = CARTESIAN_POINT('Origin',(-0.3,-6.05857864376269,-4.11)) ;
#123060 = CARTESIAN_POINT('Origin',(-0.0585786437626908,-6.3,-3.75142135623731)) ;
#123061 = CARTESIAN_POINT('Origin',(-0.0585786437626909,-6.3,-3.75142135623731)) ;
#123062 = CARTESIAN_POINT('Origin',(-0.3,-6.05857864376269,-3.41)) ;
#123063 = CARTESIAN_POINT('Origin',(-0.3,-6.05857864376269,-4.11)) ;
#123064 = CARTESIAN_POINT('Origin',(-0.3,-6.05857864376269,-3.51)) ;
#123065 = CARTESIAN_POINT('Origin',(-0.352859547920897,-6.00571909584179,
-3.4571404520791)) ;
#123066 = CARTESIAN_POINT('Origin',(-0.3,-6.05857864376269,-3.51)) ;
#123067 = CARTESIAN_POINT('Origin',(7.07238576250846,-0.11380711874577,-3.69619288125423)) ;
#123068 = CARTESIAN_POINT('Origin',(6.65857864376269,0.300000000000001,-4.11)) ;
#123069 = CARTESIAN_POINT('Origin',(6.9,0.0585786437626911,-3.86857864376269)) ;
#123070 = CARTESIAN_POINT('Origin',(6.65857864376269,0.300000000000001,-3.41)) ;
#123071 = CARTESIAN_POINT('Origin',(6.65857864376269,0.300000000000001,-4.11)) ;
#123072 = CARTESIAN_POINT('Origin',(6.65857864376269,0.300000000000001,-3.51)) ;
#123073 = CARTESIAN_POINT('Origin',(6.9,0.0585786437626909,-3.86857864376269)) ;
#123074 = CARTESIAN_POINT('Origin',(6.9,0.0585786437626909,-3.86857864376269)) ;
#123075 = CARTESIAN_POINT('Origin',(6.9,0.0585786437626909,-3.86857864376269)) ;
#123076 = CARTESIAN_POINT('Origin',(6.80571909584179,0.152859547920897,-3.6571404520791)) ;
#123077 = CARTESIAN_POINT('Origin',(6.65857864376269,0.300000000000001,-3.51)) ;
#123078 = CARTESIAN_POINT('Origin',(6.9,0.0585786437626909,-3.75142135623731)) ;
#123079 = CARTESIAN_POINT('Origin',(6.9,0.0585786437626909,-3.41)) ;
#123080 = CARTESIAN_POINT('Origin',(6.9,0.0585786437626909,-3.75142135623731)) ;
#123081 = CARTESIAN_POINT('Origin',(6.9,-0.1,-3.86857864376269)) ;
#123082 = CARTESIAN_POINT('Origin',(6.9,-0.058578643762691,-3.86857864376269)) ;
#123083 = CARTESIAN_POINT('Origin',(6.9,0.0585786437626909,-3.75142135623731)) ;
#123084 = CARTESIAN_POINT('Origin',(6.9,0.058578643762691,-3.75142135623731)) ;
#123085 = CARTESIAN_POINT('Origin',(6.9,-0.0585786437626909,-3.86857864376269)) ;
#123086 = CARTESIAN_POINT('Origin',(6.9,-0.0585786437626909,-3.86857864376269)) ;
#123087 = CARTESIAN_POINT('Origin',(6.9,-0.0585786437626909,-3.86857864376269)) ;
#123088 = CARTESIAN_POINT('Origin',(6.9,-0.399999999999999,-3.75142135623731)) ;
#123089 = CARTESIAN_POINT('Origin',(6.9,-0.0585786437626909,-3.75142135623731)) ;
#123090 = CARTESIAN_POINT('Origin',(6.9,-0.0585786437626909,-3.41)) ;
#123091 = CARTESIAN_POINT('Origin',(6.9,-0.0585786437626909,-3.75142135623731)) ;
#123092 = CARTESIAN_POINT('Origin',(6.87238576250846,-0.0861928812542305,
-3.89619288125423)) ;
#123093 = CARTESIAN_POINT('Origin',(6.65857864376269,-0.3,-4.11)) ;
#123094 = CARTESIAN_POINT('Origin',(6.9,-0.0585786437626909,-3.75142135623731)) ;
#123095 = CARTESIAN_POINT('Origin',(6.9,-0.0585786437626913,-3.75142135623731)) ;
#123096 = CARTESIAN_POINT('Origin',(6.65857864376269,-0.300000000000001,-3.41)) ;
#123097 = CARTESIAN_POINT('Origin',(6.65857864376269,-0.300000000000001,-4.11)) ;
#123098 = CARTESIAN_POINT('Origin',(6.65857864376269,-0.300000000000001,-3.51)) ;
#123099 = CARTESIAN_POINT('Origin',(6.60571909584179,-0.352859547920897,-3.4571404520791)) ;
#123100 = CARTESIAN_POINT('Origin',(6.65857864376269,-0.300000000000001,-3.51)) ;
#123101 = CARTESIAN_POINT('Origin',(-0.11380711874577,-6.47238576250846,-7.50619288125423)) ;
#123102 = CARTESIAN_POINT('Origin',(0.300000000000001,-6.05857864376269,-7.92)) ;
#123103 = CARTESIAN_POINT('Origin',(0.0585786437626912,-6.3,-7.67857864376269)) ;
#123104 = CARTESIAN_POINT('Origin',(0.3,-6.05857864376269,-7.22)) ;
#123105 = CARTESIAN_POINT('Origin',(0.3,-6.05857864376269,-7.92)) ;
#123106 = CARTESIAN_POINT('Origin',(0.3,-6.05857864376269,-7.32)) ;
#123107 = CARTESIAN_POINT('Origin',(0.0585786437626908,-6.3,-7.67857864376269)) ;
#123108 = CARTESIAN_POINT('Origin',(0.0585786437626908,-6.3,-7.67857864376269)) ;
#123109 = CARTESIAN_POINT('Origin',(0.0585786437626908,-6.3,-7.67857864376269)) ;
#123110 = CARTESIAN_POINT('Origin',(0.152859547920898,-6.20571909584179,-7.4671404520791)) ;
#123111 = CARTESIAN_POINT('Origin',(0.300000000000001,-6.05857864376269,-7.32)) ;
#123112 = CARTESIAN_POINT('Origin',(0.0585786437626908,-6.3,-7.56142135623731)) ;
#123113 = CARTESIAN_POINT('Origin',(0.0585786437626908,-6.3,-7.22)) ;
#123114 = CARTESIAN_POINT('Origin',(0.0585786437626908,-6.3,-7.56142135623731)) ;
#123115 = CARTESIAN_POINT('Origin',(0.4,-6.3,-7.67857864376269)) ;
#123116 = CARTESIAN_POINT('Origin',(-0.0585786437626906,-6.3,-7.67857864376269)) ;
#123117 = CARTESIAN_POINT('Origin',(0.0585786437626908,-6.3,-7.56142135623731)) ;
#123118 = CARTESIAN_POINT('Origin',(0.0585786437626908,-6.3,-7.56142135623731)) ;
#123119 = CARTESIAN_POINT('Origin',(-0.0585786437626908,-6.3,-7.67857864376269)) ;
#123120 = CARTESIAN_POINT('Origin',(-0.0585786437626907,-6.3,-7.67857864376269)) ;
#123121 = CARTESIAN_POINT('Origin',(-0.0585786437626908,-6.3,-7.67857864376269)) ;
#123122 = CARTESIAN_POINT('Origin',(-0.1,-6.3,-7.56142135623731)) ;
#123123 = CARTESIAN_POINT('Origin',(-0.0585786437626908,-6.3,-7.56142135623731)) ;
#123124 = CARTESIAN_POINT('Origin',(-0.0585786437626908,-6.3,-7.22)) ;
#123125 = CARTESIAN_POINT('Origin',(-0.0585786437626908,-6.3,-7.56142135623731)) ;
#123126 = CARTESIAN_POINT('Origin',(-0.0861928812542296,-6.27238576250846,
-7.70619288125423)) ;
#123127 = CARTESIAN_POINT('Origin',(-0.3,-6.05857864376269,-7.92)) ;
#123128 = CARTESIAN_POINT('Origin',(-0.0585786437626908,-6.3,-7.56142135623731)) ;
#123129 = CARTESIAN_POINT('Origin',(-0.0585786437626907,-6.3,-7.56142135623731)) ;
#123130 = CARTESIAN_POINT('Origin',(-0.3,-6.05857864376269,-7.22)) ;
#123131 = CARTESIAN_POINT('Origin',(-0.3,-6.05857864376269,-7.92)) ;
#123132 = CARTESIAN_POINT('Origin',(-0.3,-6.05857864376269,-7.32)) ;
#123133 = CARTESIAN_POINT('Origin',(-0.352859547920897,-6.00571909584179,
-7.2671404520791)) ;
#123134 = CARTESIAN_POINT('Origin',(-0.300000000000001,-6.05857864376269,
-7.32)) ;
#123135 = CARTESIAN_POINT('Origin',(7.07238576250846,-0.11380711874577,-7.50619288125423)) ;
#123136 = CARTESIAN_POINT('Origin',(6.65857864376269,0.300000000000002,-7.92)) ;
#123137 = CARTESIAN_POINT('Origin',(6.9,0.0585786437626916,-7.67857864376269)) ;
#123138 = CARTESIAN_POINT('Origin',(6.65857864376269,0.300000000000001,-7.22)) ;
#123139 = CARTESIAN_POINT('Origin',(6.65857864376269,0.300000000000001,-7.92)) ;
#123140 = CARTESIAN_POINT('Origin',(6.65857864376269,0.300000000000001,-7.32)) ;
#123141 = CARTESIAN_POINT('Origin',(6.9,0.0585786437626909,-7.67857864376269)) ;
#123142 = CARTESIAN_POINT('Origin',(6.9,0.0585786437626909,-7.67857864376269)) ;
#123143 = CARTESIAN_POINT('Origin',(6.9,0.0585786437626909,-7.67857864376269)) ;
#123144 = CARTESIAN_POINT('Origin',(6.80571909584179,0.152859547920898,-7.4671404520791)) ;
#123145 = CARTESIAN_POINT('Origin',(6.65857864376269,0.300000000000002,-7.32)) ;
#123146 = CARTESIAN_POINT('Origin',(6.9,0.0585786437626908,-7.56142135623731)) ;
#123147 = CARTESIAN_POINT('Origin',(6.9,0.0585786437626909,-7.22)) ;
#123148 = CARTESIAN_POINT('Origin',(6.9,0.0585786437626909,-7.56142135623731)) ;
#123149 = CARTESIAN_POINT('Origin',(6.9,-0.1,-7.67857864376269)) ;
#123150 = CARTESIAN_POINT('Origin',(6.9,-0.0585786437626908,-7.67857864376269)) ;
#123151 = CARTESIAN_POINT('Origin',(6.9,0.0585786437626909,-7.56142135623731)) ;
#123152 = CARTESIAN_POINT('Origin',(6.9,0.0585786437626905,-7.56142135623731)) ;
#123153 = CARTESIAN_POINT('Origin',(6.9,-0.058578643762691,-7.67857864376269)) ;
#123154 = CARTESIAN_POINT('Origin',(6.9,-0.058578643762691,-7.67857864376269)) ;
#123155 = CARTESIAN_POINT('Origin',(6.9,-0.0585786437626909,-7.67857864376269)) ;
#123156 = CARTESIAN_POINT('Origin',(6.9,-0.399999999999999,-7.56142135623731)) ;
#123157 = CARTESIAN_POINT('Origin',(6.9,-0.0585786437626909,-7.56142135623731)) ;
#123158 = CARTESIAN_POINT('Origin',(6.9,-0.0585786437626909,-7.22)) ;
#123159 = CARTESIAN_POINT('Origin',(6.9,-0.0585786437626909,-7.56142135623731)) ;
#123160 = CARTESIAN_POINT('Origin',(6.87238576250846,-0.0861928812542304,
-7.70619288125423)) ;
#123161 = CARTESIAN_POINT('Origin',(6.65857864376269,-0.300000000000001,-7.92)) ;
#123162 = CARTESIAN_POINT('Origin',(6.9,-0.058578643762691,-7.56142135623731)) ;
#123163 = CARTESIAN_POINT('Origin',(6.9,-0.058578643762691,-7.56142135623731)) ;
#123164 = CARTESIAN_POINT('Origin',(6.65857864376269,-0.300000000000001,-7.22)) ;
#123165 = CARTESIAN_POINT('Origin',(6.65857864376269,-0.300000000000001,-7.92)) ;
#123166 = CARTESIAN_POINT('Origin',(6.65857864376269,-0.300000000000001,-7.32)) ;
#123167 = CARTESIAN_POINT('Origin',(6.60571909584179,-0.352859547920898,-7.2671404520791)) ;
#123168 = CARTESIAN_POINT('Origin',(6.65857864376269,-0.300000000000001,-7.32)) ;
#123169 = CARTESIAN_POINT('Origin',(-0.11380711874577,-6.47238576250846,-11.3161928812542)) ;
#123170 = CARTESIAN_POINT('Origin',(0.299999999999999,-6.05857864376269,-11.73)) ;
#123171 = CARTESIAN_POINT('Origin',(0.0585786437626907,-6.3,-11.4885786437627)) ;
#123172 = CARTESIAN_POINT('Origin',(0.3,-6.05857864376269,-11.03)) ;
#123173 = CARTESIAN_POINT('Origin',(0.3,-6.05857864376269,-11.73)) ;
#123174 = CARTESIAN_POINT('Origin',(0.3,-6.05857864376269,-11.13)) ;
#123175 = CARTESIAN_POINT('Origin',(0.0585786437626908,-6.3,-11.4885786437627)) ;
#123176 = CARTESIAN_POINT('Origin',(0.0585786437626908,-6.3,-11.4885786437627)) ;
#123177 = CARTESIAN_POINT('Origin',(0.0585786437626908,-6.3,-11.4885786437627)) ;
#123178 = CARTESIAN_POINT('Origin',(0.152859547920898,-6.20571909584179,-11.2771404520791)) ;
#123179 = CARTESIAN_POINT('Origin',(0.300000000000003,-6.05857864376269,-11.13)) ;
#123180 = CARTESIAN_POINT('Origin',(0.0585786437626905,-6.3,-11.3714213562373)) ;
#123181 = CARTESIAN_POINT('Origin',(0.0585786437626908,-6.3,-11.03)) ;
#123182 = CARTESIAN_POINT('Origin',(0.0585786437626908,-6.3,-11.3714213562373)) ;
#123183 = CARTESIAN_POINT('Origin',(0.4,-6.3,-11.4885786437627)) ;
#123184 = CARTESIAN_POINT('Origin',(-0.0585786437626916,-6.3,-11.4885786437627)) ;
#123185 = CARTESIAN_POINT('Origin',(0.0585786437626908,-6.3,-11.3714213562373)) ;
#123186 = CARTESIAN_POINT('Origin',(0.0585786437626913,-6.3,-11.3714213562373)) ;
#123187 = CARTESIAN_POINT('Origin',(-0.0585786437626908,-6.3,-11.4885786437627)) ;
#123188 = CARTESIAN_POINT('Origin',(-0.0585786437626908,-6.3,-11.4885786437627)) ;
#123189 = CARTESIAN_POINT('Origin',(-0.0585786437626908,-6.3,-11.4885786437627)) ;
#123190 = CARTESIAN_POINT('Origin',(-0.1,-6.3,-11.3714213562373)) ;
#123191 = CARTESIAN_POINT('Origin',(-0.0585786437626908,-6.3,-11.3714213562373)) ;
#123192 = CARTESIAN_POINT('Origin',(-0.0585786437626908,-6.3,-11.03)) ;
#123193 = CARTESIAN_POINT('Origin',(-0.0585786437626908,-6.3,-11.3714213562373)) ;
#123194 = CARTESIAN_POINT('Origin',(-0.0861928812542293,-6.27238576250846,
-11.5161928812542)) ;
#123195 = CARTESIAN_POINT('Origin',(-0.3,-6.05857864376269,-11.73)) ;
#123196 = CARTESIAN_POINT('Origin',(-0.0585786437626908,-6.3,-11.3714213562373)) ;
#123197 = CARTESIAN_POINT('Origin',(-0.0585786437626915,-6.3,-11.3714213562373)) ;
#123198 = CARTESIAN_POINT('Origin',(-0.3,-6.05857864376269,-11.03)) ;
#123199 = CARTESIAN_POINT('Origin',(-0.3,-6.05857864376269,-11.73)) ;
#123200 = CARTESIAN_POINT('Origin',(-0.3,-6.05857864376269,-11.13)) ;
#123201 = CARTESIAN_POINT('Origin',(-0.352859547920898,-6.00571909584179,
-11.0771404520791)) ;
#123202 = CARTESIAN_POINT('Origin',(-0.300000000000003,-6.05857864376269,
-11.13)) ;
#123203 = CARTESIAN_POINT('Origin',(7.07238576250846,-0.11380711874577,-11.3161928812542)) ;
#123204 = CARTESIAN_POINT('Origin',(6.65857864376269,0.300000000000003,-11.73)) ;
#123205 = CARTESIAN_POINT('Origin',(6.9,0.0585786437626919,-11.4885786437627)) ;
#123206 = CARTESIAN_POINT('Origin',(6.65857864376269,0.300000000000001,-11.03)) ;
#123207 = CARTESIAN_POINT('Origin',(6.65857864376269,0.300000000000001,-11.73)) ;
#123208 = CARTESIAN_POINT('Origin',(6.65857864376269,0.300000000000001,-11.13)) ;
#123209 = CARTESIAN_POINT('Origin',(6.9,0.0585786437626909,-11.4885786437627)) ;
#123210 = CARTESIAN_POINT('Origin',(6.9,0.0585786437626909,-11.4885786437627)) ;
#123211 = CARTESIAN_POINT('Origin',(6.9,0.0585786437626909,-11.4885786437627)) ;
#123212 = CARTESIAN_POINT('Origin',(6.80571909584179,0.152859547920898,-11.2771404520791)) ;
#123213 = CARTESIAN_POINT('Origin',(6.65857864376269,0.300000000000003,-11.13)) ;
#123214 = CARTESIAN_POINT('Origin',(6.9,0.0585786437626911,-11.3714213562373)) ;
#123215 = CARTESIAN_POINT('Origin',(6.9,0.0585786437626909,-11.03)) ;
#123216 = CARTESIAN_POINT('Origin',(6.9,0.0585786437626909,-11.3714213562373)) ;
#123217 = CARTESIAN_POINT('Origin',(6.9,-0.1,-11.4885786437627)) ;
#123218 = CARTESIAN_POINT('Origin',(6.9,-0.058578643762691,-11.4885786437627)) ;
#123219 = CARTESIAN_POINT('Origin',(6.9,0.0585786437626909,-11.3714213562373)) ;
#123220 = CARTESIAN_POINT('Origin',(6.9,0.0585786437626923,-11.3714213562373)) ;
#123221 = CARTESIAN_POINT('Origin',(6.9,-0.058578643762691,-11.4885786437627)) ;
#123222 = CARTESIAN_POINT('Origin',(6.9,-0.0585786437626912,-11.4885786437627)) ;
#123223 = CARTESIAN_POINT('Origin',(6.9,-0.0585786437626909,-11.4885786437627)) ;
#123224 = CARTESIAN_POINT('Origin',(6.9,-0.399999999999999,-11.3714213562373)) ;
#123225 = CARTESIAN_POINT('Origin',(6.9,-0.0585786437626909,-11.3714213562373)) ;
#123226 = CARTESIAN_POINT('Origin',(6.9,-0.0585786437626909,-11.03)) ;
#123227 = CARTESIAN_POINT('Origin',(6.9,-0.0585786437626909,-11.3714213562373)) ;
#123228 = CARTESIAN_POINT('Origin',(6.87238576250846,-0.0861928812542304,
-11.5161928812542)) ;
#123229 = CARTESIAN_POINT('Origin',(6.65857864376269,-0.300000000000002,-11.73)) ;
#123230 = CARTESIAN_POINT('Origin',(6.9,-0.058578643762691,-11.3714213562373)) ;
#123231 = CARTESIAN_POINT('Origin',(6.9,-0.0585786437626925,-11.3714213562373)) ;
#123232 = CARTESIAN_POINT('Origin',(6.65857864376269,-0.300000000000001,-11.03)) ;
#123233 = CARTESIAN_POINT('Origin',(6.65857864376269,-0.300000000000001,-11.73)) ;
#123234 = CARTESIAN_POINT('Origin',(6.65857864376269,-0.300000000000001,-11.13)) ;
#123235 = CARTESIAN_POINT('Origin',(6.60571909584179,-0.352859547920898,-11.0771404520791)) ;
#123236 = CARTESIAN_POINT('Origin',(6.65857864376269,-0.300000000000003,-11.13)) ;
#123237 = CARTESIAN_POINT('Origin',(-0.113807118745769,-6.47238576250846,
-15.1261928812542)) ;
#123238 = CARTESIAN_POINT('Origin',(0.300000000000001,-6.05857864376269,-15.54)) ;
#123239 = CARTESIAN_POINT('Origin',(0.0585786437626911,-6.3,-15.2985786437627)) ;
#123240 = CARTESIAN_POINT('Origin',(0.3,-6.05857864376269,-14.84)) ;
#123241 = CARTESIAN_POINT('Origin',(0.3,-6.05857864376269,-15.54)) ;
#123242 = CARTESIAN_POINT('Origin',(0.3,-6.05857864376269,-14.94)) ;
#123243 = CARTESIAN_POINT('Origin',(0.0585786437626908,-6.3,-15.2985786437627)) ;
#123244 = CARTESIAN_POINT('Origin',(0.0585786437626908,-6.3,-15.2985786437627)) ;
#123245 = CARTESIAN_POINT('Origin',(0.0585786437626908,-6.3,-15.2985786437627)) ;
#123246 = CARTESIAN_POINT('Origin',(0.152859547920898,-6.20571909584179,-15.0871404520791)) ;
#123247 = CARTESIAN_POINT('Origin',(0.300000000000001,-6.05857864376269,-14.94)) ;
#123248 = CARTESIAN_POINT('Origin',(0.0585786437626911,-6.3,-15.1814213562373)) ;
#123249 = CARTESIAN_POINT('Origin',(0.0585786437626908,-6.3,-14.84)) ;
#123250 = CARTESIAN_POINT('Origin',(0.0585786437626908,-6.3,-15.1814213562373)) ;
#123251 = CARTESIAN_POINT('Origin',(0.4,-6.3,-15.2985786437627)) ;
#123252 = CARTESIAN_POINT('Origin',(-0.0585786437626904,-6.3,-15.2985786437627)) ;
#123253 = CARTESIAN_POINT('Origin',(0.0585786437626908,-6.3,-15.1814213562373)) ;
#123254 = CARTESIAN_POINT('Origin',(0.0585786437626904,-6.3,-15.1814213562373)) ;
#123255 = CARTESIAN_POINT('Origin',(-0.0585786437626908,-6.3,-15.2985786437627)) ;
#123256 = CARTESIAN_POINT('Origin',(-0.0585786437626908,-6.3,-15.2985786437627)) ;
#123257 = CARTESIAN_POINT('Origin',(-0.0585786437626908,-6.3,-15.2985786437627)) ;
#123258 = CARTESIAN_POINT('Origin',(-0.1,-6.3,-15.1814213562373)) ;
#123259 = CARTESIAN_POINT('Origin',(-0.0585786437626908,-6.3,-15.1814213562373)) ;
#123260 = CARTESIAN_POINT('Origin',(-0.0585786437626908,-6.3,-14.84)) ;
#123261 = CARTESIAN_POINT('Origin',(-0.0585786437626908,-6.3,-15.1814213562373)) ;
#123262 = CARTESIAN_POINT('Origin',(-0.0861928812542299,-6.27238576250846,
-15.3261928812542)) ;
#123263 = CARTESIAN_POINT('Origin',(-0.300000000000001,-6.05857864376269,
-15.54)) ;
#123264 = CARTESIAN_POINT('Origin',(-0.0585786437626908,-6.3,-15.1814213562373)) ;
#123265 = CARTESIAN_POINT('Origin',(-0.0585786437626914,-6.3,-15.1814213562373)) ;
#123266 = CARTESIAN_POINT('Origin',(-0.3,-6.05857864376269,-14.84)) ;
#123267 = CARTESIAN_POINT('Origin',(-0.3,-6.05857864376269,-15.54)) ;
#123268 = CARTESIAN_POINT('Origin',(-0.3,-6.05857864376269,-14.94)) ;
#123269 = CARTESIAN_POINT('Origin',(-0.352859547920897,-6.00571909584179,
-14.8871404520791)) ;
#123270 = CARTESIAN_POINT('Origin',(-0.3,-6.05857864376269,-14.94)) ;
#123271 = CARTESIAN_POINT('Origin',(7.07238576250846,-0.11380711874577,-15.1261928812542)) ;
#123272 = CARTESIAN_POINT('Origin',(6.65857864376269,0.300000000000003,-15.54)) ;
#123273 = CARTESIAN_POINT('Origin',(6.9,0.0585786437626913,-15.2985786437627)) ;
#123274 = CARTESIAN_POINT('Origin',(6.65857864376269,0.300000000000001,-14.84)) ;
#123275 = CARTESIAN_POINT('Origin',(6.65857864376269,0.300000000000001,-15.54)) ;
#123276 = CARTESIAN_POINT('Origin',(6.65857864376269,0.300000000000001,-14.94)) ;
#123277 = CARTESIAN_POINT('Origin',(6.9,0.0585786437626909,-15.2985786437627)) ;
#123278 = CARTESIAN_POINT('Origin',(6.9,0.0585786437626909,-15.2985786437627)) ;
#123279 = CARTESIAN_POINT('Origin',(6.9,0.0585786437626909,-15.2985786437627)) ;
#123280 = CARTESIAN_POINT('Origin',(6.80571909584179,0.152859547920897,-15.0871404520791)) ;
#123281 = CARTESIAN_POINT('Origin',(6.65857864376269,0.300000000000001,-14.94)) ;
#123282 = CARTESIAN_POINT('Origin',(6.9,0.0585786437626909,-15.1814213562373)) ;
#123283 = CARTESIAN_POINT('Origin',(6.9,0.0585786437626909,-14.84)) ;
#123284 = CARTESIAN_POINT('Origin',(6.9,0.0585786437626909,-15.1814213562373)) ;
#123285 = CARTESIAN_POINT('Origin',(6.9,-0.1,-15.2985786437627)) ;
#123286 = CARTESIAN_POINT('Origin',(6.9,-0.058578643762691,-15.2985786437627)) ;
#123287 = CARTESIAN_POINT('Origin',(6.9,0.0585786437626909,-15.1814213562373)) ;
#123288 = CARTESIAN_POINT('Origin',(6.9,0.0585786437626917,-15.1814213562373)) ;
#123289 = CARTESIAN_POINT('Origin',(6.9,-0.0585786437626909,-15.2985786437627)) ;
#123290 = CARTESIAN_POINT('Origin',(6.9,-0.058578643762691,-15.2985786437627)) ;
#123291 = CARTESIAN_POINT('Origin',(6.9,-0.0585786437626909,-15.2985786437627)) ;
#123292 = CARTESIAN_POINT('Origin',(6.9,-0.399999999999999,-15.1814213562373)) ;
#123293 = CARTESIAN_POINT('Origin',(6.9,-0.0585786437626909,-15.1814213562373)) ;
#123294 = CARTESIAN_POINT('Origin',(6.9,-0.0585786437626909,-14.84)) ;
#123295 = CARTESIAN_POINT('Origin',(6.9,-0.0585786437626909,-15.1814213562373)) ;
#123296 = CARTESIAN_POINT('Origin',(6.87238576250846,-0.0861928812542304,
-15.3261928812542)) ;
#123297 = CARTESIAN_POINT('Origin',(6.65857864376269,-0.300000000000002,-15.54)) ;
#123298 = CARTESIAN_POINT('Origin',(6.9,-0.058578643762691,-15.1814213562373)) ;
#123299 = CARTESIAN_POINT('Origin',(6.9,-0.0585786437626915,-15.1814213562373)) ;
#123300 = CARTESIAN_POINT('Origin',(6.65857864376269,-0.300000000000001,-14.84)) ;
#123301 = CARTESIAN_POINT('Origin',(6.65857864376269,-0.300000000000001,-15.54)) ;
#123302 = CARTESIAN_POINT('Origin',(6.65857864376269,-0.300000000000001,-14.94)) ;
#123303 = CARTESIAN_POINT('Origin',(6.60571909584179,-0.352859547920897,-14.8871404520791)) ;
#123304 = CARTESIAN_POINT('Origin',(6.65857864376269,-0.300000000000001,-14.94)) ;
#123305 = CARTESIAN_POINT('Origin',(-0.113807118745769,-6.47238576250846,
-18.9361928812542)) ;
#123306 = CARTESIAN_POINT('Origin',(0.300000000000001,-6.05857864376269,-19.35)) ;
#123307 = CARTESIAN_POINT('Origin',(0.058578643762692,-6.3,-19.1085786437627)) ;
#123308 = CARTESIAN_POINT('Origin',(0.3,-6.05857864376269,-18.65)) ;
#123309 = CARTESIAN_POINT('Origin',(0.3,-6.05857864376269,-19.35)) ;
#123310 = CARTESIAN_POINT('Origin',(0.3,-6.05857864376269,-18.75)) ;
#123311 = CARTESIAN_POINT('Origin',(0.0585786437626908,-6.3,-19.1085786437627)) ;
#123312 = CARTESIAN_POINT('Origin',(0.0585786437626908,-6.3,-19.1085786437627)) ;
#123313 = CARTESIAN_POINT('Origin',(0.0585786437626908,-6.3,-19.1085786437627)) ;
#123314 = CARTESIAN_POINT('Origin',(0.152859547920896,-6.2057190958418,-18.8971404520791)) ;
#123315 = CARTESIAN_POINT('Origin',(0.299999999999995,-6.0585786437627,-18.75)) ;
#123316 = CARTESIAN_POINT('Origin',(0.0585786437626908,-6.3,-18.9914213562373)) ;
#123317 = CARTESIAN_POINT('Origin',(0.0585786437626908,-6.3,-18.65)) ;
#123318 = CARTESIAN_POINT('Origin',(0.0585786437626908,-6.3,-18.9914213562373)) ;
#123319 = CARTESIAN_POINT('Origin',(0.4,-6.3,-19.1085786437627)) ;
#123320 = CARTESIAN_POINT('Origin',(-0.0585786437626899,-6.3,-19.1085786437627)) ;
#123321 = CARTESIAN_POINT('Origin',(0.0585786437626908,-6.3,-18.9914213562373)) ;
#123322 = CARTESIAN_POINT('Origin',(0.0585786437626916,-6.3,-18.9914213562373)) ;
#123323 = CARTESIAN_POINT('Origin',(-0.0585786437626908,-6.3,-19.1085786437627)) ;
#123324 = CARTESIAN_POINT('Origin',(-0.0585786437626905,-6.3,-19.1085786437627)) ;
#123325 = CARTESIAN_POINT('Origin',(-0.0585786437626908,-6.3,-19.1085786437627)) ;
#123326 = CARTESIAN_POINT('Origin',(-0.1,-6.3,-18.9914213562373)) ;
#123327 = CARTESIAN_POINT('Origin',(-0.0585786437626908,-6.3,-18.9914213562373)) ;
#123328 = CARTESIAN_POINT('Origin',(-0.0585786437626908,-6.3,-18.65)) ;
#123329 = CARTESIAN_POINT('Origin',(-0.0585786437626908,-6.3,-18.9914213562373)) ;
#123330 = CARTESIAN_POINT('Origin',(-0.0861928812542299,-6.27238576250846,
-19.1361928812542)) ;
#123331 = CARTESIAN_POINT('Origin',(-0.299999999999999,-6.05857864376269,
-19.35)) ;
#123332 = CARTESIAN_POINT('Origin',(-0.0585786437626908,-6.3,-18.9914213562373)) ;
#123333 = CARTESIAN_POINT('Origin',(-0.0585786437626909,-6.3,-18.9914213562373)) ;
#123334 = CARTESIAN_POINT('Origin',(-0.3,-6.05857864376269,-18.65)) ;
#123335 = CARTESIAN_POINT('Origin',(-0.3,-6.05857864376269,-19.35)) ;
#123336 = CARTESIAN_POINT('Origin',(-0.3,-6.05857864376269,-18.75)) ;
#123337 = CARTESIAN_POINT('Origin',(-0.352859547920895,-6.00571909584179,
-18.6971404520791)) ;
#123338 = CARTESIAN_POINT('Origin',(-0.299999999999997,-6.05857864376269,
-18.75)) ;
#123339 = CARTESIAN_POINT('Origin',(7.07238576250846,-0.11380711874577,-18.9361928812542)) ;
#123340 = CARTESIAN_POINT('Origin',(6.65857864376269,0.299999999999999,-19.35)) ;
#123341 = CARTESIAN_POINT('Origin',(6.9,0.0585786437626903,-19.1085786437627)) ;
#123342 = CARTESIAN_POINT('Origin',(6.65857864376269,0.300000000000001,-18.65)) ;
#123343 = CARTESIAN_POINT('Origin',(6.65857864376269,0.300000000000001,-19.35)) ;
#123344 = CARTESIAN_POINT('Origin',(6.65857864376269,0.300000000000001,-18.75)) ;
#123345 = CARTESIAN_POINT('Origin',(6.9,0.0585786437626909,-19.1085786437627)) ;
#123346 = CARTESIAN_POINT('Origin',(6.9,0.0585786437626909,-19.1085786437627)) ;
#123347 = CARTESIAN_POINT('Origin',(6.9,0.0585786437626909,-19.1085786437627)) ;
#123348 = CARTESIAN_POINT('Origin',(6.8057190958418,0.152859547920896,-18.8971404520791)) ;
#123349 = CARTESIAN_POINT('Origin',(6.6585786437627,0.299999999999996,-18.75)) ;
#123350 = CARTESIAN_POINT('Origin',(6.9,0.0585786437626908,-18.9914213562373)) ;
#123351 = CARTESIAN_POINT('Origin',(6.9,0.0585786437626909,-18.65)) ;
#123352 = CARTESIAN_POINT('Origin',(6.9,0.0585786437626909,-18.9914213562373)) ;
#123353 = CARTESIAN_POINT('Origin',(6.9,-0.1,-19.1085786437627)) ;
#123354 = CARTESIAN_POINT('Origin',(6.9,-0.0585786437626902,-19.1085786437627)) ;
#123355 = CARTESIAN_POINT('Origin',(6.9,0.0585786437626909,-18.9914213562373)) ;
#123356 = CARTESIAN_POINT('Origin',(6.9,0.058578643762691,-18.9914213562373)) ;
#123357 = CARTESIAN_POINT('Origin',(6.9,-0.0585786437626909,-19.1085786437627)) ;
#123358 = CARTESIAN_POINT('Origin',(6.9,-0.0585786437626907,-19.1085786437627)) ;
#123359 = CARTESIAN_POINT('Origin',(6.9,-0.0585786437626909,-19.1085786437627)) ;
#123360 = CARTESIAN_POINT('Origin',(6.9,-0.399999999999999,-18.9914213562373)) ;
#123361 = CARTESIAN_POINT('Origin',(6.9,-0.0585786437626909,-18.9914213562373)) ;
#123362 = CARTESIAN_POINT('Origin',(6.9,-0.0585786437626909,-18.65)) ;
#123363 = CARTESIAN_POINT('Origin',(6.9,-0.058578643762691,-18.9914213562373)) ;
#123364 = CARTESIAN_POINT('Origin',(6.87238576250846,-0.0861928812542304,
-19.1361928812542)) ;
#123365 = CARTESIAN_POINT('Origin',(6.65857864376269,-0.3,-19.35)) ;
#123366 = CARTESIAN_POINT('Origin',(6.9,-0.0585786437626909,-18.9914213562373)) ;
#123367 = CARTESIAN_POINT('Origin',(6.9,-0.0585786437626907,-18.9914213562373)) ;
#123368 = CARTESIAN_POINT('Origin',(6.65857864376269,-0.300000000000001,-18.65)) ;
#123369 = CARTESIAN_POINT('Origin',(6.65857864376269,-0.300000000000001,-19.35)) ;
#123370 = CARTESIAN_POINT('Origin',(6.65857864376269,-0.300000000000001,-18.75)) ;
#123371 = CARTESIAN_POINT('Origin',(6.6057190958418,-0.352859547920896,-18.6971404520791)) ;
#123372 = CARTESIAN_POINT('Origin',(6.65857864376269,-0.299999999999998,-18.75)) ;
#123373 = CARTESIAN_POINT('Origin',(-0.113807118745769,-6.47238576250846,
-22.7461928812542)) ;
#123374 = CARTESIAN_POINT('Origin',(0.300000000000001,-6.05857864376269,-23.16)) ;
#123375 = CARTESIAN_POINT('Origin',(0.058578643762692,-6.3,-22.9185786437627)) ;
#123376 = CARTESIAN_POINT('Origin',(0.3,-6.05857864376269,-22.46)) ;
#123377 = CARTESIAN_POINT('Origin',(0.3,-6.05857864376269,-23.16)) ;
#123378 = CARTESIAN_POINT('Origin',(0.3,-6.05857864376269,-22.56)) ;
#123379 = CARTESIAN_POINT('Origin',(0.0585786437626908,-6.3,-22.9185786437627)) ;
#123380 = CARTESIAN_POINT('Origin',(0.0585786437626908,-6.3,-22.9185786437627)) ;
#123381 = CARTESIAN_POINT('Origin',(0.0585786437626908,-6.3,-22.9185786437627)) ;
#123382 = CARTESIAN_POINT('Origin',(0.152859547920896,-6.2057190958418,-22.7071404520791)) ;
#123383 = CARTESIAN_POINT('Origin',(0.299999999999995,-6.0585786437627,-22.56)) ;
#123384 = CARTESIAN_POINT('Origin',(0.0585786437626908,-6.3,-22.8014213562373)) ;
#123385 = CARTESIAN_POINT('Origin',(0.0585786437626908,-6.3,-22.46)) ;
#123386 = CARTESIAN_POINT('Origin',(0.0585786437626908,-6.3,-22.8014213562373)) ;
#123387 = CARTESIAN_POINT('Origin',(0.4,-6.3,-22.9185786437627)) ;
#123388 = CARTESIAN_POINT('Origin',(-0.0585786437626899,-6.3,-22.9185786437627)) ;
#123389 = CARTESIAN_POINT('Origin',(0.0585786437626908,-6.3,-22.8014213562373)) ;
#123390 = CARTESIAN_POINT('Origin',(0.0585786437626916,-6.3,-22.8014213562373)) ;
#123391 = CARTESIAN_POINT('Origin',(-0.0585786437626908,-6.3,-22.9185786437627)) ;
#123392 = CARTESIAN_POINT('Origin',(-0.0585786437626905,-6.3,-22.9185786437627)) ;
#123393 = CARTESIAN_POINT('Origin',(-0.0585786437626908,-6.3,-22.9185786437627)) ;
#123394 = CARTESIAN_POINT('Origin',(-0.1,-6.3,-22.8014213562373)) ;
#123395 = CARTESIAN_POINT('Origin',(-0.0585786437626908,-6.3,-22.8014213562373)) ;
#123396 = CARTESIAN_POINT('Origin',(-0.0585786437626908,-6.3,-22.46)) ;
#123397 = CARTESIAN_POINT('Origin',(-0.0585786437626908,-6.3,-22.8014213562373)) ;
#123398 = CARTESIAN_POINT('Origin',(-0.0861928812542299,-6.27238576250846,
-22.9461928812542)) ;
#123399 = CARTESIAN_POINT('Origin',(-0.299999999999999,-6.05857864376269,
-23.16)) ;
#123400 = CARTESIAN_POINT('Origin',(-0.0585786437626908,-6.3,-22.8014213562373)) ;
#123401 = CARTESIAN_POINT('Origin',(-0.0585786437626909,-6.3,-22.8014213562373)) ;
#123402 = CARTESIAN_POINT('Origin',(-0.3,-6.05857864376269,-22.46)) ;
#123403 = CARTESIAN_POINT('Origin',(-0.3,-6.05857864376269,-23.16)) ;
#123404 = CARTESIAN_POINT('Origin',(-0.3,-6.05857864376269,-22.56)) ;
#123405 = CARTESIAN_POINT('Origin',(-0.352859547920895,-6.00571909584179,
-22.5071404520791)) ;
#123406 = CARTESIAN_POINT('Origin',(-0.299999999999997,-6.05857864376269,
-22.56)) ;
#123407 = CARTESIAN_POINT('Origin',(7.07238576250846,-0.11380711874577,-22.7461928812542)) ;
#123408 = CARTESIAN_POINT('Origin',(6.65857864376269,0.299999999999999,-23.16)) ;
#123409 = CARTESIAN_POINT('Origin',(6.9,0.0585786437626903,-22.9185786437627)) ;
#123410 = CARTESIAN_POINT('Origin',(6.65857864376269,0.300000000000001,-22.46)) ;
#123411 = CARTESIAN_POINT('Origin',(6.65857864376269,0.300000000000001,-23.16)) ;
#123412 = CARTESIAN_POINT('Origin',(6.65857864376269,0.300000000000001,-22.56)) ;
#123413 = CARTESIAN_POINT('Origin',(6.9,0.0585786437626909,-22.9185786437627)) ;
#123414 = CARTESIAN_POINT('Origin',(6.9,0.0585786437626909,-22.9185786437627)) ;
#123415 = CARTESIAN_POINT('Origin',(6.9,0.0585786437626909,-22.9185786437627)) ;
#123416 = CARTESIAN_POINT('Origin',(6.8057190958418,0.152859547920896,-22.7071404520791)) ;
#123417 = CARTESIAN_POINT('Origin',(6.6585786437627,0.299999999999996,-22.56)) ;
#123418 = CARTESIAN_POINT('Origin',(6.9,0.0585786437626908,-22.8014213562373)) ;
#123419 = CARTESIAN_POINT('Origin',(6.9,0.0585786437626909,-22.46)) ;
#123420 = CARTESIAN_POINT('Origin',(6.9,0.0585786437626909,-22.8014213562373)) ;
#123421 = CARTESIAN_POINT('Origin',(6.9,-0.1,-22.9185786437627)) ;
#123422 = CARTESIAN_POINT('Origin',(6.9,-0.0585786437626902,-22.9185786437627)) ;
#123423 = CARTESIAN_POINT('Origin',(6.9,0.0585786437626909,-22.8014213562373)) ;
#123424 = CARTESIAN_POINT('Origin',(6.9,0.058578643762691,-22.8014213562373)) ;
#123425 = CARTESIAN_POINT('Origin',(6.9,-0.0585786437626909,-22.9185786437627)) ;
#123426 = CARTESIAN_POINT('Origin',(6.9,-0.0585786437626907,-22.9185786437627)) ;
#123427 = CARTESIAN_POINT('Origin',(6.9,-0.0585786437626909,-22.9185786437627)) ;
#123428 = CARTESIAN_POINT('Origin',(6.9,-0.399999999999999,-22.8014213562373)) ;
#123429 = CARTESIAN_POINT('Origin',(6.9,-0.0585786437626909,-22.8014213562373)) ;
#123430 = CARTESIAN_POINT('Origin',(6.9,-0.0585786437626909,-22.46)) ;
#123431 = CARTESIAN_POINT('Origin',(6.9,-0.058578643762691,-22.8014213562373)) ;
#123432 = CARTESIAN_POINT('Origin',(6.87238576250846,-0.0861928812542304,
-22.9461928812542)) ;
#123433 = CARTESIAN_POINT('Origin',(6.65857864376269,-0.3,-23.16)) ;
#123434 = CARTESIAN_POINT('Origin',(6.9,-0.0585786437626909,-22.8014213562373)) ;
#123435 = CARTESIAN_POINT('Origin',(6.9,-0.0585786437626907,-22.8014213562373)) ;
#123436 = CARTESIAN_POINT('Origin',(6.65857864376269,-0.300000000000001,-22.46)) ;
#123437 = CARTESIAN_POINT('Origin',(6.65857864376269,-0.300000000000001,-23.16)) ;
#123438 = CARTESIAN_POINT('Origin',(6.65857864376269,-0.300000000000001,-22.56)) ;
#123439 = CARTESIAN_POINT('Origin',(6.6057190958418,-0.352859547920896,-22.5071404520791)) ;
#123440 = CARTESIAN_POINT('Origin',(6.65857864376269,-0.299999999999998,-22.56)) ;
#123441 = CARTESIAN_POINT('Origin',(-0.113807118745769,-6.47238576250846,
-26.5561928812542)) ;
#123442 = CARTESIAN_POINT('Origin',(0.300000000000001,-6.05857864376269,-26.97)) ;
#123443 = CARTESIAN_POINT('Origin',(0.058578643762692,-6.3,-26.7285786437627)) ;
#123444 = CARTESIAN_POINT('Origin',(0.3,-6.05857864376269,-26.27)) ;
#123445 = CARTESIAN_POINT('Origin',(0.3,-6.05857864376269,-26.97)) ;
#123446 = CARTESIAN_POINT('Origin',(0.3,-6.05857864376269,-26.37)) ;
#123447 = CARTESIAN_POINT('Origin',(0.0585786437626908,-6.3,-26.7285786437627)) ;
#123448 = CARTESIAN_POINT('Origin',(0.0585786437626908,-6.3,-26.7285786437627)) ;
#123449 = CARTESIAN_POINT('Origin',(0.0585786437626908,-6.3,-26.7285786437627)) ;
#123450 = CARTESIAN_POINT('Origin',(0.152859547920896,-6.2057190958418,-26.5171404520791)) ;
#123451 = CARTESIAN_POINT('Origin',(0.299999999999995,-6.0585786437627,-26.37)) ;
#123452 = CARTESIAN_POINT('Origin',(0.0585786437626908,-6.3,-26.6114213562373)) ;
#123453 = CARTESIAN_POINT('Origin',(0.0585786437626908,-6.3,-26.27)) ;
#123454 = CARTESIAN_POINT('Origin',(0.0585786437626908,-6.3,-26.6114213562373)) ;
#123455 = CARTESIAN_POINT('Origin',(0.4,-6.3,-26.7285786437627)) ;
#123456 = CARTESIAN_POINT('Origin',(-0.0585786437626899,-6.3,-26.7285786437627)) ;
#123457 = CARTESIAN_POINT('Origin',(0.0585786437626908,-6.3,-26.6114213562373)) ;
#123458 = CARTESIAN_POINT('Origin',(0.0585786437626916,-6.3,-26.6114213562373)) ;
#123459 = CARTESIAN_POINT('Origin',(-0.0585786437626908,-6.3,-26.7285786437627)) ;
#123460 = CARTESIAN_POINT('Origin',(-0.0585786437626905,-6.3,-26.7285786437627)) ;
#123461 = CARTESIAN_POINT('Origin',(-0.0585786437626908,-6.3,-26.7285786437627)) ;
#123462 = CARTESIAN_POINT('Origin',(-0.1,-6.3,-26.6114213562373)) ;
#123463 = CARTESIAN_POINT('Origin',(-0.0585786437626908,-6.3,-26.6114213562373)) ;
#123464 = CARTESIAN_POINT('Origin',(-0.0585786437626908,-6.3,-26.27)) ;
#123465 = CARTESIAN_POINT('Origin',(-0.0585786437626908,-6.3,-26.6114213562373)) ;
#123466 = CARTESIAN_POINT('Origin',(-0.0861928812542299,-6.27238576250846,
-26.7561928812542)) ;
#123467 = CARTESIAN_POINT('Origin',(-0.299999999999999,-6.05857864376269,
-26.97)) ;
#123468 = CARTESIAN_POINT('Origin',(-0.0585786437626908,-6.3,-26.6114213562373)) ;
#123469 = CARTESIAN_POINT('Origin',(-0.0585786437626909,-6.3,-26.6114213562373)) ;
#123470 = CARTESIAN_POINT('Origin',(-0.3,-6.05857864376269,-26.27)) ;
#123471 = CARTESIAN_POINT('Origin',(-0.3,-6.05857864376269,-26.97)) ;
#123472 = CARTESIAN_POINT('Origin',(-0.3,-6.05857864376269,-26.37)) ;
#123473 = CARTESIAN_POINT('Origin',(-0.352859547920895,-6.00571909584179,
-26.3171404520791)) ;
#123474 = CARTESIAN_POINT('Origin',(-0.299999999999997,-6.05857864376269,
-26.37)) ;
#123475 = CARTESIAN_POINT('Origin',(7.07238576250846,-0.11380711874577,-26.5561928812542)) ;
#123476 = CARTESIAN_POINT('Origin',(6.65857864376269,0.299999999999999,-26.97)) ;
#123477 = CARTESIAN_POINT('Origin',(6.9,0.0585786437626903,-26.7285786437627)) ;
#123478 = CARTESIAN_POINT('Origin',(6.65857864376269,0.300000000000001,-26.27)) ;
#123479 = CARTESIAN_POINT('Origin',(6.65857864376269,0.300000000000001,-26.97)) ;
#123480 = CARTESIAN_POINT('Origin',(6.65857864376269,0.300000000000001,-26.37)) ;
#123481 = CARTESIAN_POINT('Origin',(6.9,0.0585786437626909,-26.7285786437627)) ;
#123482 = CARTESIAN_POINT('Origin',(6.9,0.0585786437626909,-26.7285786437627)) ;
#123483 = CARTESIAN_POINT('Origin',(6.9,0.0585786437626909,-26.7285786437627)) ;
#123484 = CARTESIAN_POINT('Origin',(6.8057190958418,0.152859547920896,-26.5171404520791)) ;
#123485 = CARTESIAN_POINT('Origin',(6.6585786437627,0.299999999999996,-26.37)) ;
#123486 = CARTESIAN_POINT('Origin',(6.9,0.0585786437626908,-26.6114213562373)) ;
#123487 = CARTESIAN_POINT('Origin',(6.9,0.0585786437626909,-26.27)) ;
#123488 = CARTESIAN_POINT('Origin',(6.9,0.0585786437626909,-26.6114213562373)) ;
#123489 = CARTESIAN_POINT('Origin',(6.9,-0.1,-26.7285786437627)) ;
#123490 = CARTESIAN_POINT('Origin',(6.9,-0.0585786437626902,-26.7285786437627)) ;
#123491 = CARTESIAN_POINT('Origin',(6.9,0.0585786437626909,-26.6114213562373)) ;
#123492 = CARTESIAN_POINT('Origin',(6.9,0.058578643762691,-26.6114213562373)) ;
#123493 = CARTESIAN_POINT('Origin',(6.9,-0.0585786437626909,-26.7285786437627)) ;
#123494 = CARTESIAN_POINT('Origin',(6.9,-0.0585786437626907,-26.7285786437627)) ;
#123495 = CARTESIAN_POINT('Origin',(6.9,-0.0585786437626909,-26.7285786437627)) ;
#123496 = CARTESIAN_POINT('Origin',(6.9,-0.399999999999999,-26.6114213562373)) ;
#123497 = CARTESIAN_POINT('Origin',(6.9,-0.0585786437626909,-26.6114213562373)) ;
#123498 = CARTESIAN_POINT('Origin',(6.9,-0.0585786437626909,-26.27)) ;
#123499 = CARTESIAN_POINT('Origin',(6.9,-0.058578643762691,-26.6114213562373)) ;
#123500 = CARTESIAN_POINT('Origin',(6.87238576250846,-0.0861928812542304,
-26.7561928812542)) ;
#123501 = CARTESIAN_POINT('Origin',(6.65857864376269,-0.3,-26.97)) ;
#123502 = CARTESIAN_POINT('Origin',(6.9,-0.0585786437626909,-26.6114213562373)) ;
#123503 = CARTESIAN_POINT('Origin',(6.9,-0.0585786437626907,-26.6114213562373)) ;
#123504 = CARTESIAN_POINT('Origin',(6.65857864376269,-0.300000000000001,-26.27)) ;
#123505 = CARTESIAN_POINT('Origin',(6.65857864376269,-0.300000000000001,-26.97)) ;
#123506 = CARTESIAN_POINT('Origin',(6.65857864376269,-0.300000000000001,-26.37)) ;
#123507 = CARTESIAN_POINT('Origin',(6.6057190958418,-0.352859547920896,-26.3171404520791)) ;
#123508 = CARTESIAN_POINT('Origin',(6.65857864376269,-0.299999999999998,-26.37)) ;
#123509 = CARTESIAN_POINT('Origin',(-0.113807118745769,-6.47238576250846,
-30.3661928812542)) ;
#123510 = CARTESIAN_POINT('Origin',(0.300000000000001,-6.05857864376269,-30.78)) ;
#123511 = CARTESIAN_POINT('Origin',(0.058578643762692,-6.3,-30.5385786437627)) ;
#123512 = CARTESIAN_POINT('Origin',(0.3,-6.05857864376269,-30.08)) ;
#123513 = CARTESIAN_POINT('Origin',(0.3,-6.05857864376269,-30.78)) ;
#123514 = CARTESIAN_POINT('Origin',(0.3,-6.05857864376269,-30.18)) ;
#123515 = CARTESIAN_POINT('Origin',(0.0585786437626908,-6.3,-30.5385786437627)) ;
#123516 = CARTESIAN_POINT('Origin',(0.0585786437626908,-6.3,-30.5385786437627)) ;
#123517 = CARTESIAN_POINT('Origin',(0.0585786437626908,-6.3,-30.5385786437627)) ;
#123518 = CARTESIAN_POINT('Origin',(0.152859547920896,-6.2057190958418,-30.3271404520791)) ;
#123519 = CARTESIAN_POINT('Origin',(0.299999999999995,-6.0585786437627,-30.18)) ;
#123520 = CARTESIAN_POINT('Origin',(0.0585786437626908,-6.3,-30.4214213562373)) ;
#123521 = CARTESIAN_POINT('Origin',(0.0585786437626908,-6.3,-30.08)) ;
#123522 = CARTESIAN_POINT('Origin',(0.0585786437626908,-6.3,-30.4214213562373)) ;
#123523 = CARTESIAN_POINT('Origin',(0.4,-6.3,-30.5385786437627)) ;
#123524 = CARTESIAN_POINT('Origin',(-0.0585786437626899,-6.3,-30.5385786437627)) ;
#123525 = CARTESIAN_POINT('Origin',(0.0585786437626908,-6.3,-30.4214213562373)) ;
#123526 = CARTESIAN_POINT('Origin',(0.0585786437626916,-6.3,-30.4214213562373)) ;
#123527 = CARTESIAN_POINT('Origin',(-0.0585786437626908,-6.3,-30.5385786437627)) ;
#123528 = CARTESIAN_POINT('Origin',(-0.0585786437626905,-6.3,-30.5385786437627)) ;
#123529 = CARTESIAN_POINT('Origin',(-0.0585786437626908,-6.3,-30.5385786437627)) ;
#123530 = CARTESIAN_POINT('Origin',(-0.1,-6.3,-30.4214213562373)) ;
#123531 = CARTESIAN_POINT('Origin',(-0.0585786437626908,-6.3,-30.4214213562373)) ;
#123532 = CARTESIAN_POINT('Origin',(-0.0585786437626908,-6.3,-30.08)) ;
#123533 = CARTESIAN_POINT('Origin',(-0.0585786437626908,-6.3,-30.4214213562373)) ;
#123534 = CARTESIAN_POINT('Origin',(-0.0861928812542299,-6.27238576250846,
-30.5661928812542)) ;
#123535 = CARTESIAN_POINT('Origin',(-0.299999999999999,-6.05857864376269,
-30.78)) ;
#123536 = CARTESIAN_POINT('Origin',(-0.0585786437626908,-6.3,-30.4214213562373)) ;
#123537 = CARTESIAN_POINT('Origin',(-0.0585786437626909,-6.3,-30.4214213562373)) ;
#123538 = CARTESIAN_POINT('Origin',(-0.3,-6.05857864376269,-30.08)) ;
#123539 = CARTESIAN_POINT('Origin',(-0.3,-6.05857864376269,-30.78)) ;
#123540 = CARTESIAN_POINT('Origin',(-0.3,-6.05857864376269,-30.18)) ;
#123541 = CARTESIAN_POINT('Origin',(-0.352859547920895,-6.00571909584179,
-30.1271404520791)) ;
#123542 = CARTESIAN_POINT('Origin',(-0.299999999999997,-6.05857864376269,
-30.18)) ;
#123543 = CARTESIAN_POINT('Origin',(7.07238576250846,-0.11380711874577,-30.3661928812542)) ;
#123544 = CARTESIAN_POINT('Origin',(6.65857864376269,0.299999999999999,-30.78)) ;
#123545 = CARTESIAN_POINT('Origin',(6.9,0.0585786437626903,-30.5385786437627)) ;
#123546 = CARTESIAN_POINT('Origin',(6.65857864376269,0.300000000000001,-30.08)) ;
#123547 = CARTESIAN_POINT('Origin',(6.65857864376269,0.300000000000001,-30.78)) ;
#123548 = CARTESIAN_POINT('Origin',(6.65857864376269,0.300000000000001,-30.18)) ;
#123549 = CARTESIAN_POINT('Origin',(6.9,0.0585786437626909,-30.5385786437627)) ;
#123550 = CARTESIAN_POINT('Origin',(6.9,0.0585786437626909,-30.5385786437627)) ;
#123551 = CARTESIAN_POINT('Origin',(6.9,0.0585786437626909,-30.5385786437627)) ;
#123552 = CARTESIAN_POINT('Origin',(6.8057190958418,0.152859547920896,-30.3271404520791)) ;
#123553 = CARTESIAN_POINT('Origin',(6.6585786437627,0.299999999999996,-30.18)) ;
#123554 = CARTESIAN_POINT('Origin',(6.9,0.0585786437626908,-30.4214213562373)) ;
#123555 = CARTESIAN_POINT('Origin',(6.9,0.0585786437626909,-30.08)) ;
#123556 = CARTESIAN_POINT('Origin',(6.9,0.0585786437626909,-30.4214213562373)) ;
#123557 = CARTESIAN_POINT('Origin',(6.9,-0.1,-30.5385786437627)) ;
#123558 = CARTESIAN_POINT('Origin',(6.9,-0.0585786437626902,-30.5385786437627)) ;
#123559 = CARTESIAN_POINT('Origin',(6.9,0.0585786437626909,-30.4214213562373)) ;
#123560 = CARTESIAN_POINT('Origin',(6.9,0.058578643762691,-30.4214213562373)) ;
#123561 = CARTESIAN_POINT('Origin',(6.9,-0.0585786437626909,-30.5385786437627)) ;
#123562 = CARTESIAN_POINT('Origin',(6.9,-0.0585786437626907,-30.5385786437627)) ;
#123563 = CARTESIAN_POINT('Origin',(6.9,-0.0585786437626909,-30.5385786437627)) ;
#123564 = CARTESIAN_POINT('Origin',(6.9,-0.399999999999999,-30.4214213562373)) ;
#123565 = CARTESIAN_POINT('Origin',(6.9,-0.0585786437626909,-30.4214213562373)) ;
#123566 = CARTESIAN_POINT('Origin',(6.9,-0.0585786437626909,-30.08)) ;
#123567 = CARTESIAN_POINT('Origin',(6.9,-0.058578643762691,-30.4214213562373)) ;
#123568 = CARTESIAN_POINT('Origin',(6.87238576250846,-0.0861928812542304,
-30.5661928812542)) ;
#123569 = CARTESIAN_POINT('Origin',(6.65857864376269,-0.3,-30.78)) ;
#123570 = CARTESIAN_POINT('Origin',(6.9,-0.0585786437626909,-30.4214213562373)) ;
#123571 = CARTESIAN_POINT('Origin',(6.9,-0.0585786437626907,-30.4214213562373)) ;
#123572 = CARTESIAN_POINT('Origin',(6.65857864376269,-0.300000000000001,-30.08)) ;
#123573 = CARTESIAN_POINT('Origin',(6.65857864376269,-0.300000000000001,-30.78)) ;
#123574 = CARTESIAN_POINT('Origin',(6.65857864376269,-0.300000000000001,-30.18)) ;
#123575 = CARTESIAN_POINT('Origin',(6.6057190958418,-0.352859547920896,-30.1271404520791)) ;
#123576 = CARTESIAN_POINT('Origin',(6.65857864376269,-0.299999999999998,-30.18)) ;
#123577 = CARTESIAN_POINT('Origin',(-0.113807118745771,-6.47238576250846,
-34.1761928812542)) ;
#123578 = CARTESIAN_POINT('Origin',(0.299999999999993,-6.0585786437627,-34.59)) ;
#123579 = CARTESIAN_POINT('Origin',(0.0585786437626844,-6.3,-34.3485786437627)) ;
#123580 = CARTESIAN_POINT('Origin',(0.3,-6.05857864376269,-33.89)) ;
#123581 = CARTESIAN_POINT('Origin',(0.3,-6.05857864376269,-34.59)) ;
#123582 = CARTESIAN_POINT('Origin',(0.3,-6.05857864376269,-33.99)) ;
#123583 = CARTESIAN_POINT('Origin',(0.0585786437626887,-6.3,-34.3485786437627)) ;
#123584 = CARTESIAN_POINT('Origin',(0.0585786437626908,-6.3,-34.3485786437627)) ;
#123585 = CARTESIAN_POINT('Origin',(0.0585786437626908,-6.3,-34.3485786437627)) ;
#123586 = CARTESIAN_POINT('Origin',(0.152859547920899,-6.20571909584179,-34.1371404520791)) ;
#123587 = CARTESIAN_POINT('Origin',(0.300000000000006,-6.05857864376268,-33.99)) ;
#123588 = CARTESIAN_POINT('Origin',(0.0585786437626911,-6.3,-34.2314213562373)) ;
#123589 = CARTESIAN_POINT('Origin',(0.0585786437626908,-6.3,-33.89)) ;
#123590 = CARTESIAN_POINT('Origin',(0.0585786437626908,-6.3,-34.2314213562373)) ;
#123591 = CARTESIAN_POINT('Origin',(0.4,-6.3,-34.3485786437627)) ;
#123592 = CARTESIAN_POINT('Origin',(-0.0585786437626895,-6.3,-34.3485786437627)) ;
#123593 = CARTESIAN_POINT('Origin',(0.0585786437626903,-6.3,-34.2314213562373)) ;
#123594 = CARTESIAN_POINT('Origin',(0.058578643762689,-6.3,-34.2314213562373)) ;
#123595 = CARTESIAN_POINT('Origin',(-0.0585786437626902,-6.3,-34.3485786437627)) ;
#123596 = CARTESIAN_POINT('Origin',(-0.0585786437626905,-6.3,-34.3485786437627)) ;
#123597 = CARTESIAN_POINT('Origin',(-0.0585786437626908,-6.3,-34.3485786437627)) ;
#123598 = CARTESIAN_POINT('Origin',(-0.1,-6.3,-34.2314213562373)) ;
#123599 = CARTESIAN_POINT('Origin',(-0.0585786437626908,-6.3,-34.2314213562373)) ;
#123600 = CARTESIAN_POINT('Origin',(-0.0585786437626908,-6.3,-33.89)) ;
#123601 = CARTESIAN_POINT('Origin',(-0.0585786437626908,-6.3,-34.2314213562373)) ;
#123602 = CARTESIAN_POINT('Origin',(-0.0861928812542287,-6.27238576250846,
-34.3761928812542)) ;
#123603 = CARTESIAN_POINT('Origin',(-0.299999999999994,-6.0585786437627,-34.59)) ;
#123604 = CARTESIAN_POINT('Origin',(-0.0585786437626908,-6.3,-34.2314213562373)) ;
#123605 = CARTESIAN_POINT('Origin',(-0.0585786437626846,-6.3,-34.2314213562373)) ;
#123606 = CARTESIAN_POINT('Origin',(-0.3,-6.05857864376269,-33.89)) ;
#123607 = CARTESIAN_POINT('Origin',(-0.3,-6.05857864376269,-34.59)) ;
#123608 = CARTESIAN_POINT('Origin',(-0.3,-6.05857864376269,-33.99)) ;
#123609 = CARTESIAN_POINT('Origin',(-0.352859547920899,-6.00571909584179,
-33.9371404520791)) ;
#123610 = CARTESIAN_POINT('Origin',(-0.3,-6.05857864376269,-33.99)) ;
#123611 = CARTESIAN_POINT('Origin',(7.07238576250846,-0.113807118745771,-34.1761928812542)) ;
#123612 = CARTESIAN_POINT('Origin',(6.6585786437627,0.299999999999994,-34.59)) ;
#123613 = CARTESIAN_POINT('Origin',(6.9,0.0585786437626901,-34.3485786437627)) ;
#123614 = CARTESIAN_POINT('Origin',(6.65857864376269,0.300000000000001,-33.89)) ;
#123615 = CARTESIAN_POINT('Origin',(6.65857864376269,0.300000000000001,-34.59)) ;
#123616 = CARTESIAN_POINT('Origin',(6.65857864376269,0.300000000000001,-33.99)) ;
#123617 = CARTESIAN_POINT('Origin',(6.9,0.0585786437626906,-34.3485786437627)) ;
#123618 = CARTESIAN_POINT('Origin',(6.9,0.0585786437626909,-34.3485786437627)) ;
#123619 = CARTESIAN_POINT('Origin',(6.9,0.0585786437626909,-34.3485786437627)) ;
#123620 = CARTESIAN_POINT('Origin',(6.80571909584179,0.1528595479209,-34.1371404520791)) ;
#123621 = CARTESIAN_POINT('Origin',(6.65857864376268,0.300000000000007,-33.99)) ;
#123622 = CARTESIAN_POINT('Origin',(6.9,0.0585786437626911,-34.2314213562373)) ;
#123623 = CARTESIAN_POINT('Origin',(6.9,0.0585786437626909,-33.89)) ;
#123624 = CARTESIAN_POINT('Origin',(6.9,0.0585786437626909,-34.2314213562373)) ;
#123625 = CARTESIAN_POINT('Origin',(6.9,-0.1,-34.3485786437627)) ;
#123626 = CARTESIAN_POINT('Origin',(6.9,-0.0585786437626952,-34.3485786437627)) ;
#123627 = CARTESIAN_POINT('Origin',(6.9,0.0585786437626913,-34.2314213562373)) ;
#123628 = CARTESIAN_POINT('Origin',(6.9,0.0585786437626919,-34.2314213562373)) ;
#123629 = CARTESIAN_POINT('Origin',(6.9,-0.0585786437626923,-34.3485786437627)) ;
#123630 = CARTESIAN_POINT('Origin',(6.9,-0.0585786437626907,-34.3485786437627)) ;
#123631 = CARTESIAN_POINT('Origin',(6.9,-0.0585786437626909,-34.3485786437627)) ;
#123632 = CARTESIAN_POINT('Origin',(6.9,-0.399999999999999,-34.2314213562373)) ;
#123633 = CARTESIAN_POINT('Origin',(6.9,-0.0585786437626909,-34.2314213562373)) ;
#123634 = CARTESIAN_POINT('Origin',(6.9,-0.0585786437626909,-33.89)) ;
#123635 = CARTESIAN_POINT('Origin',(6.9,-0.058578643762691,-34.2314213562373)) ;
#123636 = CARTESIAN_POINT('Origin',(6.87238576250846,-0.0861928812542292,
-34.3761928812542)) ;
#123637 = CARTESIAN_POINT('Origin',(6.6585786437627,-0.299999999999995,-34.59)) ;
#123638 = CARTESIAN_POINT('Origin',(6.9,-0.0585786437626886,-34.2314213562373)) ;
#123639 = CARTESIAN_POINT('Origin',(6.9,-0.058578643762684,-34.2314213562373)) ;
#123640 = CARTESIAN_POINT('Origin',(6.65857864376269,-0.300000000000001,-33.89)) ;
#123641 = CARTESIAN_POINT('Origin',(6.65857864376269,-0.300000000000001,-34.59)) ;
#123642 = CARTESIAN_POINT('Origin',(6.65857864376269,-0.300000000000001,-33.99)) ;
#123643 = CARTESIAN_POINT('Origin',(6.60571909584179,-0.3528595479209,-33.9371404520791)) ;
#123644 = CARTESIAN_POINT('Origin',(6.65857864376269,-0.300000000000001,-33.99)) ;
#123645 = CARTESIAN_POINT('Origin',(0.6,-0.6,-4.11)) ;
#123646 = CARTESIAN_POINT('Origin',(0.3,-0.6,-4.11)) ;
#123647 = CARTESIAN_POINT('Origin',(0.3,-6.1,-4.11)) ;
#123648 = CARTESIAN_POINT('Origin',(0.3,-6.05857864376269,-4.11)) ;
#123649 = CARTESIAN_POINT('Origin',(0.3,-6.05857864376269,-4.11)) ;
#123650 = CARTESIAN_POINT('Origin',(0.3,-6.05857864376269,-4.11)) ;
#123651 = CARTESIAN_POINT('Origin',(0.4,-6.05857864376269,-4.11)) ;
#123652 = CARTESIAN_POINT('Origin',(-0.300000000000001,-6.05857864376269,
-4.11)) ;
#123653 = CARTESIAN_POINT('Origin',(-0.3,-6.05857864376269,-4.11)) ;
#123654 = CARTESIAN_POINT('Origin',(-0.3,-6.05857864376269,-4.11)) ;
#123655 = CARTESIAN_POINT('Origin',(-0.3,-0.600000000000001,-4.11)) ;
#123656 = CARTESIAN_POINT('Origin',(-0.3,-0.600000000000001,-4.11)) ;
#123657 = CARTESIAN_POINT('Origin',(0.6,-0.600000000000001,-4.11)) ;
#123658 = CARTESIAN_POINT('Origin',(0.6,-0.600000000000001,-3.51)) ;
#123659 = CARTESIAN_POINT('Origin',(-0.3,-0.600000000000001,-3.51)) ;
#123660 = CARTESIAN_POINT('Origin',(-0.3,-0.600000000000001,-3.51)) ;
#123661 = CARTESIAN_POINT('Origin',(-0.3,-6.05857864376269,-3.51)) ;
#123662 = CARTESIAN_POINT('Origin',(-0.3,-6.05857864376269,-3.51)) ;
#123663 = CARTESIAN_POINT('Origin',(-0.299999999999999,-6.05857864376269,
-3.51)) ;
#123664 = CARTESIAN_POINT('Origin',(0.4,-6.05857864376269,-3.51)) ;
#123665 = CARTESIAN_POINT('Origin',(0.299999999999999,-6.05857864376269,-3.51)) ;
#123666 = CARTESIAN_POINT('Origin',(0.3,-6.05857864376269,-3.51)) ;
#123667 = CARTESIAN_POINT('Origin',(0.3,-6.05857864376269,-3.51)) ;
#123668 = CARTESIAN_POINT('Origin',(0.3,-0.600000000000001,-3.51)) ;
#123669 = CARTESIAN_POINT('Origin',(0.3,-0.6,-3.51)) ;
#123670 = CARTESIAN_POINT('Origin',(0.6,-0.6,-3.51)) ;
#123671 = CARTESIAN_POINT('Origin',(6.7,0.300000000000001,-4.11)) ;
#123672 = CARTESIAN_POINT('Origin',(6.65857864376269,0.300000000000001,-4.11)) ;
#123673 = CARTESIAN_POINT('Origin',(6.65857864376269,0.300000000000001,-4.11)) ;
#123674 = CARTESIAN_POINT('Origin',(6.65857864376269,0.300000000000001,-4.11)) ;
#123675 = CARTESIAN_POINT('Origin',(6.65857864376269,-0.399999999999999,-4.11)) ;
#123676 = CARTESIAN_POINT('Origin',(6.65857864376269,-0.300000000000001,-4.11)) ;
#123677 = CARTESIAN_POINT('Origin',(6.65857864376269,-0.3,-4.11)) ;
#123678 = CARTESIAN_POINT('Origin',(6.65857864376269,-0.300000000000001,-4.11)) ;
#123679 = CARTESIAN_POINT('Origin',(0.6,-0.3,-4.11)) ;
#123680 = CARTESIAN_POINT('Origin',(0.6,0.299999999999999,-3.51)) ;
#123681 = CARTESIAN_POINT('Origin',(6.65857864376269,0.300000000000001,-3.51)) ;
#123682 = CARTESIAN_POINT('Origin',(6.65857864376269,0.300000000000001,-3.51)) ;
#123683 = CARTESIAN_POINT('Origin',(6.65857864376269,0.3,-3.51)) ;
#123684 = CARTESIAN_POINT('Origin',(6.65857864376269,-0.399999999999999,-3.51)) ;
#123685 = CARTESIAN_POINT('Origin',(6.65857864376269,-0.3,-3.51)) ;
#123686 = CARTESIAN_POINT('Origin',(0.6,-0.3,-3.51)) ;
#123687 = CARTESIAN_POINT('Origin',(6.65857864376269,-0.300000000000001,-3.51)) ;
#123688 = CARTESIAN_POINT('Origin',(6.65857864376269,-0.300000000000001,-3.51)) ;
#123689 = CARTESIAN_POINT('Origin',(0.6,-0.6,-7.92)) ;
#123690 = CARTESIAN_POINT('Origin',(0.3,-0.6,-7.92)) ;
#123691 = CARTESIAN_POINT('Origin',(0.3,-6.1,-7.92)) ;
#123692 = CARTESIAN_POINT('Origin',(0.3,-6.05857864376269,-7.92)) ;
#123693 = CARTESIAN_POINT('Origin',(0.3,-6.05857864376269,-7.92)) ;
#123694 = CARTESIAN_POINT('Origin',(0.3,-6.05857864376269,-7.92)) ;
#123695 = CARTESIAN_POINT('Origin',(0.4,-6.05857864376269,-7.92)) ;
#123696 = CARTESIAN_POINT('Origin',(-0.299999999999999,-6.05857864376269,
-7.92)) ;
#123697 = CARTESIAN_POINT('Origin',(-0.3,-6.05857864376269,-7.92)) ;
#123698 = CARTESIAN_POINT('Origin',(-0.3,-6.05857864376269,-7.92)) ;
#123699 = CARTESIAN_POINT('Origin',(-0.3,-0.600000000000001,-7.92)) ;
#123700 = CARTESIAN_POINT('Origin',(-0.3,-0.600000000000001,-7.92)) ;
#123701 = CARTESIAN_POINT('Origin',(0.6,-0.600000000000001,-7.92)) ;
#123702 = CARTESIAN_POINT('Origin',(0.6,-0.600000000000001,-7.32)) ;
#123703 = CARTESIAN_POINT('Origin',(-0.3,-0.600000000000001,-7.32)) ;
#123704 = CARTESIAN_POINT('Origin',(-0.3,-0.600000000000001,-7.32)) ;
#123705 = CARTESIAN_POINT('Origin',(-0.3,-6.05857864376269,-7.32)) ;
#123706 = CARTESIAN_POINT('Origin',(-0.3,-6.05857864376269,-7.32)) ;
#123707 = CARTESIAN_POINT('Origin',(-0.300000000000001,-6.05857864376269,
-7.32)) ;
#123708 = CARTESIAN_POINT('Origin',(0.4,-6.05857864376269,-7.32)) ;
#123709 = CARTESIAN_POINT('Origin',(0.300000000000002,-6.05857864376269,-7.32)) ;
#123710 = CARTESIAN_POINT('Origin',(0.300000000000001,-6.05857864376269,-7.32)) ;
#123711 = CARTESIAN_POINT('Origin',(0.3,-6.05857864376269,-7.32)) ;
#123712 = CARTESIAN_POINT('Origin',(0.3,-0.600000000000001,-7.32)) ;
#123713 = CARTESIAN_POINT('Origin',(0.3,-0.6,-7.32)) ;
#123714 = CARTESIAN_POINT('Origin',(0.6,-0.6,-7.32)) ;
#123715 = CARTESIAN_POINT('Origin',(6.7,0.300000000000001,-7.92)) ;
#123716 = CARTESIAN_POINT('Origin',(6.65857864376269,0.300000000000001,-7.92)) ;
#123717 = CARTESIAN_POINT('Origin',(6.65857864376269,0.300000000000001,-7.92)) ;
#123718 = CARTESIAN_POINT('Origin',(6.65857864376269,0.300000000000002,-7.92)) ;
#123719 = CARTESIAN_POINT('Origin',(6.65857864376269,-0.399999999999999,-7.92)) ;
#123720 = CARTESIAN_POINT('Origin',(6.65857864376269,-0.300000000000002,-7.92)) ;
#123721 = CARTESIAN_POINT('Origin',(6.65857864376269,-0.300000000000001,-7.92)) ;
#123722 = CARTESIAN_POINT('Origin',(6.65857864376269,-0.300000000000001,-7.92)) ;
#123723 = CARTESIAN_POINT('Origin',(0.6,-0.3,-7.92)) ;
#123724 = CARTESIAN_POINT('Origin',(0.6,0.299999999999999,-7.32)) ;
#123725 = CARTESIAN_POINT('Origin',(6.65857864376269,0.300000000000001,-7.32)) ;
#123726 = CARTESIAN_POINT('Origin',(6.65857864376269,0.300000000000001,-7.32)) ;
#123727 = CARTESIAN_POINT('Origin',(6.65857864376269,0.300000000000002,-7.32)) ;
#123728 = CARTESIAN_POINT('Origin',(6.65857864376269,-0.399999999999999,-7.32)) ;
#123729 = CARTESIAN_POINT('Origin',(6.65857864376269,-0.300000000000002,-7.32)) ;
#123730 = CARTESIAN_POINT('Origin',(0.6,-0.3,-7.32)) ;
#123731 = CARTESIAN_POINT('Origin',(6.65857864376269,-0.300000000000001,-7.32)) ;
#123732 = CARTESIAN_POINT('Origin',(6.65857864376269,-0.300000000000001,-7.32)) ;
#123733 = CARTESIAN_POINT('Origin',(0.6,-0.6,-11.73)) ;
#123734 = CARTESIAN_POINT('Origin',(0.3,-0.6,-11.73)) ;
#123735 = CARTESIAN_POINT('Origin',(0.3,-6.1,-11.73)) ;
#123736 = CARTESIAN_POINT('Origin',(0.3,-6.05857864376269,-11.73)) ;
#123737 = CARTESIAN_POINT('Origin',(0.3,-6.05857864376269,-11.73)) ;
#123738 = CARTESIAN_POINT('Origin',(0.299999999999998,-6.05857864376269,-11.73)) ;
#123739 = CARTESIAN_POINT('Origin',(0.4,-6.05857864376269,-11.73)) ;
#123740 = CARTESIAN_POINT('Origin',(-0.299999999999999,-6.05857864376269,
-11.73)) ;
#123741 = CARTESIAN_POINT('Origin',(-0.3,-6.05857864376269,-11.73)) ;
#123742 = CARTESIAN_POINT('Origin',(-0.3,-6.05857864376269,-11.73)) ;
#123743 = CARTESIAN_POINT('Origin',(-0.3,-0.600000000000001,-11.73)) ;
#123744 = CARTESIAN_POINT('Origin',(-0.3,-0.600000000000001,-11.73)) ;
#123745 = CARTESIAN_POINT('Origin',(0.6,-0.600000000000001,-11.73)) ;
#123746 = CARTESIAN_POINT('Origin',(0.6,-0.600000000000001,-11.13)) ;
#123747 = CARTESIAN_POINT('Origin',(-0.3,-0.600000000000001,-11.13)) ;
#123748 = CARTESIAN_POINT('Origin',(-0.3,-0.600000000000001,-11.13)) ;
#123749 = CARTESIAN_POINT('Origin',(-0.3,-6.05857864376269,-11.13)) ;
#123750 = CARTESIAN_POINT('Origin',(-0.3,-6.05857864376269,-11.13)) ;
#123751 = CARTESIAN_POINT('Origin',(-0.300000000000002,-6.05857864376269,
-11.13)) ;
#123752 = CARTESIAN_POINT('Origin',(0.4,-6.05857864376269,-11.13)) ;
#123753 = CARTESIAN_POINT('Origin',(0.300000000000001,-6.05857864376269,-11.13)) ;
#123754 = CARTESIAN_POINT('Origin',(0.300000000000003,-6.05857864376269,-11.13)) ;
#123755 = CARTESIAN_POINT('Origin',(0.3,-6.05857864376269,-11.13)) ;
#123756 = CARTESIAN_POINT('Origin',(0.3,-0.600000000000001,-11.13)) ;
#123757 = CARTESIAN_POINT('Origin',(0.3,-0.6,-11.13)) ;
#123758 = CARTESIAN_POINT('Origin',(0.6,-0.6,-11.13)) ;
#123759 = CARTESIAN_POINT('Origin',(6.7,0.300000000000001,-11.73)) ;
#123760 = CARTESIAN_POINT('Origin',(6.65857864376269,0.300000000000001,-11.73)) ;
#123761 = CARTESIAN_POINT('Origin',(6.65857864376269,0.300000000000001,-11.73)) ;
#123762 = CARTESIAN_POINT('Origin',(6.65857864376269,0.300000000000001,-11.73)) ;
#123763 = CARTESIAN_POINT('Origin',(6.65857864376269,-0.399999999999999,-11.73)) ;
#123764 = CARTESIAN_POINT('Origin',(6.65857864376269,-0.300000000000002,-11.73)) ;
#123765 = CARTESIAN_POINT('Origin',(6.65857864376269,-0.300000000000002,-11.73)) ;
#123766 = CARTESIAN_POINT('Origin',(6.65857864376269,-0.300000000000001,-11.73)) ;
#123767 = CARTESIAN_POINT('Origin',(0.6,-0.3,-11.73)) ;
#123768 = CARTESIAN_POINT('Origin',(0.6,0.299999999999999,-11.13)) ;
#123769 = CARTESIAN_POINT('Origin',(6.65857864376269,0.300000000000001,-11.13)) ;
#123770 = CARTESIAN_POINT('Origin',(6.65857864376269,0.300000000000001,-11.13)) ;
#123771 = CARTESIAN_POINT('Origin',(6.65857864376269,0.300000000000001,-11.13)) ;
#123772 = CARTESIAN_POINT('Origin',(6.65857864376269,-0.399999999999999,-11.13)) ;
#123773 = CARTESIAN_POINT('Origin',(6.65857864376269,-0.300000000000002,-11.13)) ;
#123774 = CARTESIAN_POINT('Origin',(0.6,-0.3,-11.13)) ;
#123775 = CARTESIAN_POINT('Origin',(6.65857864376269,-0.300000000000001,-11.13)) ;
#123776 = CARTESIAN_POINT('Origin',(6.65857864376269,-0.300000000000003,-11.13)) ;
#123777 = CARTESIAN_POINT('Origin',(0.6,-0.6,-15.54)) ;
#123778 = CARTESIAN_POINT('Origin',(0.3,-0.6,-15.54)) ;
#123779 = CARTESIAN_POINT('Origin',(0.3,-6.1,-15.54)) ;
#123780 = CARTESIAN_POINT('Origin',(0.3,-6.05857864376269,-15.54)) ;
#123781 = CARTESIAN_POINT('Origin',(0.3,-6.05857864376269,-15.54)) ;
#123782 = CARTESIAN_POINT('Origin',(0.3,-6.05857864376269,-15.54)) ;
#123783 = CARTESIAN_POINT('Origin',(0.4,-6.05857864376269,-15.54)) ;
#123784 = CARTESIAN_POINT('Origin',(-0.299999999999999,-6.05857864376269,
-15.54)) ;
#123785 = CARTESIAN_POINT('Origin',(-0.300000000000001,-6.05857864376269,
-15.54)) ;
#123786 = CARTESIAN_POINT('Origin',(-0.3,-6.05857864376269,-15.54)) ;
#123787 = CARTESIAN_POINT('Origin',(-0.3,-0.600000000000001,-15.54)) ;
#123788 = CARTESIAN_POINT('Origin',(-0.3,-0.600000000000001,-15.54)) ;
#123789 = CARTESIAN_POINT('Origin',(0.6,-0.600000000000001,-15.54)) ;
#123790 = CARTESIAN_POINT('Origin',(0.6,-0.600000000000001,-14.94)) ;
#123791 = CARTESIAN_POINT('Origin',(-0.3,-0.600000000000001,-14.94)) ;
#123792 = CARTESIAN_POINT('Origin',(-0.3,-0.600000000000001,-14.94)) ;
#123793 = CARTESIAN_POINT('Origin',(-0.3,-6.05857864376269,-14.94)) ;
#123794 = CARTESIAN_POINT('Origin',(-0.3,-6.05857864376269,-14.94)) ;
#123795 = CARTESIAN_POINT('Origin',(-0.3,-6.05857864376269,-14.94)) ;
#123796 = CARTESIAN_POINT('Origin',(0.4,-6.05857864376269,-14.94)) ;
#123797 = CARTESIAN_POINT('Origin',(0.299999999999999,-6.05857864376269,-14.94)) ;
#123798 = CARTESIAN_POINT('Origin',(0.300000000000001,-6.05857864376269,-14.94)) ;
#123799 = CARTESIAN_POINT('Origin',(0.3,-6.05857864376269,-14.94)) ;
#123800 = CARTESIAN_POINT('Origin',(0.3,-0.600000000000001,-14.94)) ;
#123801 = CARTESIAN_POINT('Origin',(0.3,-0.6,-14.94)) ;
#123802 = CARTESIAN_POINT('Origin',(0.6,-0.6,-14.94)) ;
#123803 = CARTESIAN_POINT('Origin',(6.7,0.300000000000001,-15.54)) ;
#123804 = CARTESIAN_POINT('Origin',(6.65857864376269,0.300000000000001,-15.54)) ;
#123805 = CARTESIAN_POINT('Origin',(6.65857864376269,0.300000000000001,-15.54)) ;
#123806 = CARTESIAN_POINT('Origin',(6.65857864376269,0.300000000000003,-15.54)) ;
#123807 = CARTESIAN_POINT('Origin',(6.65857864376269,-0.399999999999999,-15.54)) ;
#123808 = CARTESIAN_POINT('Origin',(6.65857864376269,-0.3,-15.54)) ;
#123809 = CARTESIAN_POINT('Origin',(6.65857864376269,-0.300000000000002,-15.54)) ;
#123810 = CARTESIAN_POINT('Origin',(6.65857864376269,-0.300000000000001,-15.54)) ;
#123811 = CARTESIAN_POINT('Origin',(0.6,-0.3,-15.54)) ;
#123812 = CARTESIAN_POINT('Origin',(0.6,0.299999999999999,-14.94)) ;
#123813 = CARTESIAN_POINT('Origin',(6.65857864376269,0.300000000000001,-14.94)) ;
#123814 = CARTESIAN_POINT('Origin',(6.65857864376269,0.300000000000001,-14.94)) ;
#123815 = CARTESIAN_POINT('Origin',(6.65857864376269,0.3,-14.94)) ;
#123816 = CARTESIAN_POINT('Origin',(6.65857864376269,-0.399999999999999,-14.94)) ;
#123817 = CARTESIAN_POINT('Origin',(6.65857864376269,-0.299999999999999,-14.94)) ;
#123818 = CARTESIAN_POINT('Origin',(0.6,-0.3,-14.94)) ;
#123819 = CARTESIAN_POINT('Origin',(6.65857864376269,-0.300000000000001,-14.94)) ;
#123820 = CARTESIAN_POINT('Origin',(6.65857864376269,-0.300000000000001,-14.94)) ;
#123821 = CARTESIAN_POINT('Origin',(0.6,-0.6,-19.35)) ;
#123822 = CARTESIAN_POINT('Origin',(0.3,-0.6,-19.35)) ;
#123823 = CARTESIAN_POINT('Origin',(0.3,-6.1,-19.35)) ;
#123824 = CARTESIAN_POINT('Origin',(0.3,-6.05857864376269,-19.35)) ;
#123825 = CARTESIAN_POINT('Origin',(0.3,-6.05857864376269,-19.35)) ;
#123826 = CARTESIAN_POINT('Origin',(0.299999999999999,-6.05857864376269,-19.35)) ;
#123827 = CARTESIAN_POINT('Origin',(0.4,-6.05857864376269,-19.35)) ;
#123828 = CARTESIAN_POINT('Origin',(-0.299999999999994,-6.0585786437627,-19.35)) ;
#123829 = CARTESIAN_POINT('Origin',(-0.299999999999999,-6.05857864376269,
-19.35)) ;
#123830 = CARTESIAN_POINT('Origin',(-0.3,-6.05857864376269,-19.35)) ;
#123831 = CARTESIAN_POINT('Origin',(-0.3,-0.600000000000001,-19.35)) ;
#123832 = CARTESIAN_POINT('Origin',(-0.3,-0.600000000000001,-19.35)) ;
#123833 = CARTESIAN_POINT('Origin',(0.6,-0.600000000000001,-19.35)) ;
#123834 = CARTESIAN_POINT('Origin',(0.6,-0.600000000000001,-18.75)) ;
#123835 = CARTESIAN_POINT('Origin',(-0.3,-0.600000000000001,-18.75)) ;
#123836 = CARTESIAN_POINT('Origin',(-0.3,-0.600000000000001,-18.75)) ;
#123837 = CARTESIAN_POINT('Origin',(-0.3,-6.05857864376269,-18.75)) ;
#123838 = CARTESIAN_POINT('Origin',(-0.3,-6.05857864376269,-18.75)) ;
#123839 = CARTESIAN_POINT('Origin',(-0.299999999999994,-6.0585786437627,-18.75)) ;
#123840 = CARTESIAN_POINT('Origin',(0.4,-6.0585786437627,-18.75)) ;
#123841 = CARTESIAN_POINT('Origin',(0.299999999999993,-6.0585786437627,-18.75)) ;
#123842 = CARTESIAN_POINT('Origin',(0.299999999999996,-6.0585786437627,-18.75)) ;
#123843 = CARTESIAN_POINT('Origin',(0.3,-6.05857864376269,-18.75)) ;
#123844 = CARTESIAN_POINT('Origin',(0.3,-0.600000000000001,-18.75)) ;
#123845 = CARTESIAN_POINT('Origin',(0.3,-0.6,-18.75)) ;
#123846 = CARTESIAN_POINT('Origin',(0.6,-0.6,-18.75)) ;
#123847 = CARTESIAN_POINT('Origin',(6.7,0.300000000000001,-19.35)) ;
#123848 = CARTESIAN_POINT('Origin',(6.65857864376269,0.300000000000001,-19.35)) ;
#123849 = CARTESIAN_POINT('Origin',(6.65857864376269,0.300000000000001,-19.35)) ;
#123850 = CARTESIAN_POINT('Origin',(6.65857864376269,0.299999999999997,-19.35)) ;
#123851 = CARTESIAN_POINT('Origin',(6.65857864376269,-0.399999999999999,-19.35)) ;
#123852 = CARTESIAN_POINT('Origin',(6.65857864376269,-0.299999999999997,-19.35)) ;
#123853 = CARTESIAN_POINT('Origin',(6.65857864376269,-0.3,-19.35)) ;
#123854 = CARTESIAN_POINT('Origin',(6.65857864376269,-0.300000000000001,-19.35)) ;
#123855 = CARTESIAN_POINT('Origin',(0.6,-0.3,-19.35)) ;
#123856 = CARTESIAN_POINT('Origin',(0.6,0.299999999999999,-18.75)) ;
#123857 = CARTESIAN_POINT('Origin',(6.65857864376269,0.300000000000001,-18.75)) ;
#123858 = CARTESIAN_POINT('Origin',(6.65857864376269,0.300000000000001,-18.75)) ;
#123859 = CARTESIAN_POINT('Origin',(6.6585786437627,0.299999999999995,-18.75)) ;
#123860 = CARTESIAN_POINT('Origin',(6.6585786437627,-0.399999999999999,-18.75)) ;
#123861 = CARTESIAN_POINT('Origin',(6.6585786437627,-0.299999999999994,-18.75)) ;
#123862 = CARTESIAN_POINT('Origin',(0.6,-0.3,-18.75)) ;
#123863 = CARTESIAN_POINT('Origin',(6.65857864376269,-0.300000000000001,-18.75)) ;
#123864 = CARTESIAN_POINT('Origin',(6.65857864376269,-0.299999999999998,-18.75)) ;
#123865 = CARTESIAN_POINT('Origin',(0.6,-0.6,-23.16)) ;
#123866 = CARTESIAN_POINT('Origin',(0.3,-0.6,-23.16)) ;
#123867 = CARTESIAN_POINT('Origin',(0.3,-6.1,-23.16)) ;
#123868 = CARTESIAN_POINT('Origin',(0.3,-6.05857864376269,-23.16)) ;
#123869 = CARTESIAN_POINT('Origin',(0.3,-6.05857864376269,-23.16)) ;
#123870 = CARTESIAN_POINT('Origin',(0.299999999999999,-6.05857864376269,-23.16)) ;
#123871 = CARTESIAN_POINT('Origin',(0.4,-6.05857864376269,-23.16)) ;
#123872 = CARTESIAN_POINT('Origin',(-0.299999999999994,-6.0585786437627,-23.16)) ;
#123873 = CARTESIAN_POINT('Origin',(-0.299999999999999,-6.05857864376269,
-23.16)) ;
#123874 = CARTESIAN_POINT('Origin',(-0.3,-6.05857864376269,-23.16)) ;
#123875 = CARTESIAN_POINT('Origin',(-0.3,-0.600000000000001,-23.16)) ;
#123876 = CARTESIAN_POINT('Origin',(-0.3,-0.600000000000001,-23.16)) ;
#123877 = CARTESIAN_POINT('Origin',(0.6,-0.600000000000001,-23.16)) ;
#123878 = CARTESIAN_POINT('Origin',(0.6,-0.600000000000001,-22.56)) ;
#123879 = CARTESIAN_POINT('Origin',(-0.3,-0.600000000000001,-22.56)) ;
#123880 = CARTESIAN_POINT('Origin',(-0.3,-0.600000000000001,-22.56)) ;
#123881 = CARTESIAN_POINT('Origin',(-0.3,-6.05857864376269,-22.56)) ;
#123882 = CARTESIAN_POINT('Origin',(-0.3,-6.05857864376269,-22.56)) ;
#123883 = CARTESIAN_POINT('Origin',(-0.299999999999994,-6.0585786437627,-22.56)) ;
#123884 = CARTESIAN_POINT('Origin',(0.4,-6.0585786437627,-22.56)) ;
#123885 = CARTESIAN_POINT('Origin',(0.299999999999993,-6.0585786437627,-22.56)) ;
#123886 = CARTESIAN_POINT('Origin',(0.299999999999996,-6.0585786437627,-22.56)) ;
#123887 = CARTESIAN_POINT('Origin',(0.3,-6.05857864376269,-22.56)) ;
#123888 = CARTESIAN_POINT('Origin',(0.3,-0.600000000000001,-22.56)) ;
#123889 = CARTESIAN_POINT('Origin',(0.3,-0.6,-22.56)) ;
#123890 = CARTESIAN_POINT('Origin',(0.6,-0.6,-22.56)) ;
#123891 = CARTESIAN_POINT('Origin',(6.7,0.300000000000001,-23.16)) ;
#123892 = CARTESIAN_POINT('Origin',(6.65857864376269,0.300000000000001,-23.16)) ;
#123893 = CARTESIAN_POINT('Origin',(6.65857864376269,0.300000000000001,-23.16)) ;
#123894 = CARTESIAN_POINT('Origin',(6.65857864376269,0.299999999999997,-23.16)) ;
#123895 = CARTESIAN_POINT('Origin',(6.65857864376269,-0.399999999999999,-23.16)) ;
#123896 = CARTESIAN_POINT('Origin',(6.65857864376269,-0.299999999999997,-23.16)) ;
#123897 = CARTESIAN_POINT('Origin',(6.65857864376269,-0.3,-23.16)) ;
#123898 = CARTESIAN_POINT('Origin',(6.65857864376269,-0.300000000000001,-23.16)) ;
#123899 = CARTESIAN_POINT('Origin',(0.6,-0.3,-23.16)) ;
#123900 = CARTESIAN_POINT('Origin',(0.6,0.299999999999999,-22.56)) ;
#123901 = CARTESIAN_POINT('Origin',(6.65857864376269,0.300000000000001,-22.56)) ;
#123902 = CARTESIAN_POINT('Origin',(6.65857864376269,0.300000000000001,-22.56)) ;
#123903 = CARTESIAN_POINT('Origin',(6.6585786437627,0.299999999999995,-22.56)) ;
#123904 = CARTESIAN_POINT('Origin',(6.6585786437627,-0.399999999999999,-22.56)) ;
#123905 = CARTESIAN_POINT('Origin',(6.6585786437627,-0.299999999999994,-22.56)) ;
#123906 = CARTESIAN_POINT('Origin',(0.6,-0.3,-22.56)) ;
#123907 = CARTESIAN_POINT('Origin',(6.65857864376269,-0.300000000000001,-22.56)) ;
#123908 = CARTESIAN_POINT('Origin',(6.65857864376269,-0.299999999999998,-22.56)) ;
#123909 = CARTESIAN_POINT('Origin',(0.6,-0.6,-26.97)) ;
#123910 = CARTESIAN_POINT('Origin',(0.3,-0.6,-26.97)) ;
#123911 = CARTESIAN_POINT('Origin',(0.3,-6.1,-26.97)) ;
#123912 = CARTESIAN_POINT('Origin',(0.3,-6.05857864376269,-26.97)) ;
#123913 = CARTESIAN_POINT('Origin',(0.3,-6.05857864376269,-26.97)) ;
#123914 = CARTESIAN_POINT('Origin',(0.299999999999999,-6.05857864376269,-26.97)) ;
#123915 = CARTESIAN_POINT('Origin',(0.4,-6.05857864376269,-26.97)) ;
#123916 = CARTESIAN_POINT('Origin',(-0.299999999999994,-6.0585786437627,-26.97)) ;
#123917 = CARTESIAN_POINT('Origin',(-0.299999999999999,-6.05857864376269,
-26.97)) ;
#123918 = CARTESIAN_POINT('Origin',(-0.3,-6.05857864376269,-26.97)) ;
#123919 = CARTESIAN_POINT('Origin',(-0.3,-0.600000000000001,-26.97)) ;
#123920 = CARTESIAN_POINT('Origin',(-0.3,-0.600000000000001,-26.97)) ;
#123921 = CARTESIAN_POINT('Origin',(0.6,-0.600000000000001,-26.97)) ;
#123922 = CARTESIAN_POINT('Origin',(0.6,-0.600000000000001,-26.37)) ;
#123923 = CARTESIAN_POINT('Origin',(-0.3,-0.600000000000001,-26.37)) ;
#123924 = CARTESIAN_POINT('Origin',(-0.3,-0.600000000000001,-26.37)) ;
#123925 = CARTESIAN_POINT('Origin',(-0.3,-6.05857864376269,-26.37)) ;
#123926 = CARTESIAN_POINT('Origin',(-0.3,-6.05857864376269,-26.37)) ;
#123927 = CARTESIAN_POINT('Origin',(-0.299999999999994,-6.0585786437627,-26.37)) ;
#123928 = CARTESIAN_POINT('Origin',(0.4,-6.0585786437627,-26.37)) ;
#123929 = CARTESIAN_POINT('Origin',(0.299999999999993,-6.0585786437627,-26.37)) ;
#123930 = CARTESIAN_POINT('Origin',(0.299999999999996,-6.0585786437627,-26.37)) ;
#123931 = CARTESIAN_POINT('Origin',(0.3,-6.05857864376269,-26.37)) ;
#123932 = CARTESIAN_POINT('Origin',(0.3,-0.600000000000001,-26.37)) ;
#123933 = CARTESIAN_POINT('Origin',(0.3,-0.6,-26.37)) ;
#123934 = CARTESIAN_POINT('Origin',(0.6,-0.6,-26.37)) ;
#123935 = CARTESIAN_POINT('Origin',(6.7,0.300000000000001,-26.97)) ;
#123936 = CARTESIAN_POINT('Origin',(6.65857864376269,0.300000000000001,-26.97)) ;
#123937 = CARTESIAN_POINT('Origin',(6.65857864376269,0.300000000000001,-26.97)) ;
#123938 = CARTESIAN_POINT('Origin',(6.65857864376269,0.299999999999997,-26.97)) ;
#123939 = CARTESIAN_POINT('Origin',(6.65857864376269,-0.399999999999999,-26.97)) ;
#123940 = CARTESIAN_POINT('Origin',(6.65857864376269,-0.299999999999997,-26.97)) ;
#123941 = CARTESIAN_POINT('Origin',(6.65857864376269,-0.3,-26.97)) ;
#123942 = CARTESIAN_POINT('Origin',(6.65857864376269,-0.300000000000001,-26.97)) ;
#123943 = CARTESIAN_POINT('Origin',(0.6,-0.3,-26.97)) ;
#123944 = CARTESIAN_POINT('Origin',(0.6,0.299999999999999,-26.37)) ;
#123945 = CARTESIAN_POINT('Origin',(6.65857864376269,0.300000000000001,-26.37)) ;
#123946 = CARTESIAN_POINT('Origin',(6.65857864376269,0.300000000000001,-26.37)) ;
#123947 = CARTESIAN_POINT('Origin',(6.6585786437627,0.299999999999995,-26.37)) ;
#123948 = CARTESIAN_POINT('Origin',(6.6585786437627,-0.399999999999999,-26.37)) ;
#123949 = CARTESIAN_POINT('Origin',(6.6585786437627,-0.299999999999994,-26.37)) ;
#123950 = CARTESIAN_POINT('Origin',(0.6,-0.3,-26.37)) ;
#123951 = CARTESIAN_POINT('Origin',(6.65857864376269,-0.300000000000001,-26.37)) ;
#123952 = CARTESIAN_POINT('Origin',(6.65857864376269,-0.299999999999998,-26.37)) ;
#123953 = CARTESIAN_POINT('Origin',(0.6,-0.6,-30.78)) ;
#123954 = CARTESIAN_POINT('Origin',(0.3,-0.6,-30.78)) ;
#123955 = CARTESIAN_POINT('Origin',(0.3,-6.1,-30.78)) ;
#123956 = CARTESIAN_POINT('Origin',(0.3,-6.05857864376269,-30.78)) ;
#123957 = CARTESIAN_POINT('Origin',(0.3,-6.05857864376269,-30.78)) ;
#123958 = CARTESIAN_POINT('Origin',(0.299999999999999,-6.05857864376269,-30.78)) ;
#123959 = CARTESIAN_POINT('Origin',(0.4,-6.05857864376269,-30.78)) ;
#123960 = CARTESIAN_POINT('Origin',(-0.299999999999994,-6.0585786437627,-30.78)) ;
#123961 = CARTESIAN_POINT('Origin',(-0.299999999999999,-6.05857864376269,
-30.78)) ;
#123962 = CARTESIAN_POINT('Origin',(-0.3,-6.05857864376269,-30.78)) ;
#123963 = CARTESIAN_POINT('Origin',(-0.3,-0.600000000000001,-30.78)) ;
#123964 = CARTESIAN_POINT('Origin',(-0.3,-0.600000000000001,-30.78)) ;
#123965 = CARTESIAN_POINT('Origin',(0.6,-0.600000000000001,-30.78)) ;
#123966 = CARTESIAN_POINT('Origin',(0.6,-0.600000000000001,-30.18)) ;
#123967 = CARTESIAN_POINT('Origin',(-0.3,-0.600000000000001,-30.18)) ;
#123968 = CARTESIAN_POINT('Origin',(-0.3,-0.600000000000001,-30.18)) ;
#123969 = CARTESIAN_POINT('Origin',(-0.3,-6.05857864376269,-30.18)) ;
#123970 = CARTESIAN_POINT('Origin',(-0.3,-6.05857864376269,-30.18)) ;
#123971 = CARTESIAN_POINT('Origin',(-0.299999999999994,-6.0585786437627,-30.18)) ;
#123972 = CARTESIAN_POINT('Origin',(0.4,-6.0585786437627,-30.18)) ;
#123973 = CARTESIAN_POINT('Origin',(0.299999999999993,-6.0585786437627,-30.18)) ;
#123974 = CARTESIAN_POINT('Origin',(0.299999999999996,-6.0585786437627,-30.18)) ;
#123975 = CARTESIAN_POINT('Origin',(0.3,-6.05857864376269,-30.18)) ;
#123976 = CARTESIAN_POINT('Origin',(0.3,-0.600000000000001,-30.18)) ;
#123977 = CARTESIAN_POINT('Origin',(0.3,-0.6,-30.18)) ;
#123978 = CARTESIAN_POINT('Origin',(0.6,-0.6,-30.18)) ;
#123979 = CARTESIAN_POINT('Origin',(6.7,0.300000000000001,-30.78)) ;
#123980 = CARTESIAN_POINT('Origin',(6.65857864376269,0.300000000000001,-30.78)) ;
#123981 = CARTESIAN_POINT('Origin',(6.65857864376269,0.300000000000001,-30.78)) ;
#123982 = CARTESIAN_POINT('Origin',(6.65857864376269,0.299999999999997,-30.78)) ;
#123983 = CARTESIAN_POINT('Origin',(6.65857864376269,-0.399999999999999,-30.78)) ;
#123984 = CARTESIAN_POINT('Origin',(6.65857864376269,-0.299999999999997,-30.78)) ;
#123985 = CARTESIAN_POINT('Origin',(6.65857864376269,-0.3,-30.78)) ;
#123986 = CARTESIAN_POINT('Origin',(6.65857864376269,-0.300000000000001,-30.78)) ;
#123987 = CARTESIAN_POINT('Origin',(0.6,-0.3,-30.78)) ;
#123988 = CARTESIAN_POINT('Origin',(0.6,0.299999999999999,-30.18)) ;
#123989 = CARTESIAN_POINT('Origin',(6.65857864376269,0.300000000000001,-30.18)) ;
#123990 = CARTESIAN_POINT('Origin',(6.65857864376269,0.300000000000001,-30.18)) ;
#123991 = CARTESIAN_POINT('Origin',(6.6585786437627,0.299999999999995,-30.18)) ;
#123992 = CARTESIAN_POINT('Origin',(6.6585786437627,-0.399999999999999,-30.18)) ;
#123993 = CARTESIAN_POINT('Origin',(6.6585786437627,-0.299999999999994,-30.18)) ;
#123994 = CARTESIAN_POINT('Origin',(0.6,-0.3,-30.18)) ;
#123995 = CARTESIAN_POINT('Origin',(6.65857864376269,-0.300000000000001,-30.18)) ;
#123996 = CARTESIAN_POINT('Origin',(6.65857864376269,-0.299999999999998,-30.18)) ;
#123997 = CARTESIAN_POINT('Origin',(0.6,-0.6,-34.59)) ;
#123998 = CARTESIAN_POINT('Origin',(0.3,-0.6,-34.59)) ;
#123999 = CARTESIAN_POINT('Origin',(0.3,-6.1,-34.59)) ;
#124000 = CARTESIAN_POINT('Origin',(0.3,-6.05857864376269,-34.59)) ;
#124001 = CARTESIAN_POINT('Origin',(0.3,-6.05857864376269,-34.59)) ;
#124002 = CARTESIAN_POINT('Origin',(0.3,-6.05857864376269,-34.59)) ;
#124003 = CARTESIAN_POINT('Origin',(0.4,-6.05857864376269,-34.59)) ;
#124004 = CARTESIAN_POINT('Origin',(-0.299999999999998,-6.05857864376269,
-34.59)) ;
#124005 = CARTESIAN_POINT('Origin',(-0.299999999999994,-6.0585786437627,-34.59)) ;
#124006 = CARTESIAN_POINT('Origin',(-0.3,-6.05857864376269,-34.59)) ;
#124007 = CARTESIAN_POINT('Origin',(-0.3,-0.600000000000001,-34.59)) ;
#124008 = CARTESIAN_POINT('Origin',(-0.3,-0.600000000000001,-34.59)) ;
#124009 = CARTESIAN_POINT('Origin',(0.6,-0.600000000000001,-34.59)) ;
#124010 = CARTESIAN_POINT('Origin',(0.6,-0.600000000000001,-33.99)) ;
#124011 = CARTESIAN_POINT('Origin',(-0.3,-0.600000000000001,-33.99)) ;
#124012 = CARTESIAN_POINT('Origin',(-0.3,-0.600000000000001,-33.99)) ;
#124013 = CARTESIAN_POINT('Origin',(-0.3,-6.05857864376269,-33.99)) ;
#124014 = CARTESIAN_POINT('Origin',(-0.3,-6.05857864376269,-33.99)) ;
#124015 = CARTESIAN_POINT('Origin',(-0.300000000000007,-6.05857864376268,
-33.99)) ;
#124016 = CARTESIAN_POINT('Origin',(0.4,-6.05857864376269,-33.99)) ;
#124017 = CARTESIAN_POINT('Origin',(0.30000000000001,-6.05857864376268,-33.99)) ;
#124018 = CARTESIAN_POINT('Origin',(0.300000000000006,-6.05857864376268,-33.99)) ;
#124019 = CARTESIAN_POINT('Origin',(0.3,-6.05857864376269,-33.99)) ;
#124020 = CARTESIAN_POINT('Origin',(0.3,-0.600000000000001,-33.99)) ;
#124021 = CARTESIAN_POINT('Origin',(0.3,-0.6,-33.99)) ;
#124022 = CARTESIAN_POINT('Origin',(0.6,-0.6,-33.99)) ;
#124023 = CARTESIAN_POINT('Origin',(6.7,0.300000000000001,-34.59)) ;
#124024 = CARTESIAN_POINT('Origin',(6.65857864376269,0.300000000000001,-34.59)) ;
#124025 = CARTESIAN_POINT('Origin',(6.65857864376269,0.300000000000001,-34.59)) ;
#124026 = CARTESIAN_POINT('Origin',(6.65857864376269,0.300000000000001,-34.59)) ;
#124027 = CARTESIAN_POINT('Origin',(6.6585786437627,-0.399999999999999,-34.59)) ;
#124028 = CARTESIAN_POINT('Origin',(6.65857864376269,-0.300000000000002,-34.59)) ;
#124029 = CARTESIAN_POINT('Origin',(6.6585786437627,-0.299999999999996,-34.59)) ;
#124030 = CARTESIAN_POINT('Origin',(6.65857864376269,-0.300000000000001,-34.59)) ;
#124031 = CARTESIAN_POINT('Origin',(0.6,-0.3,-34.59)) ;
#124032 = CARTESIAN_POINT('Origin',(0.6,0.299999999999999,-33.99)) ;
#124033 = CARTESIAN_POINT('Origin',(6.65857864376269,0.300000000000001,-33.99)) ;
#124034 = CARTESIAN_POINT('Origin',(6.65857864376269,0.300000000000001,-33.99)) ;
#124035 = CARTESIAN_POINT('Origin',(6.65857864376269,0.300000000000005,-33.99)) ;
#124036 = CARTESIAN_POINT('Origin',(6.65857864376269,-0.399999999999999,-33.99)) ;
#124037 = CARTESIAN_POINT('Origin',(6.65857864376268,-0.300000000000006,-33.99)) ;
#124038 = CARTESIAN_POINT('Origin',(0.6,-0.3,-33.99)) ;
#124039 = CARTESIAN_POINT('Origin',(6.65857864376269,-0.300000000000001,-33.99)) ;
#124040 = CARTESIAN_POINT('Origin',(6.65857864376269,-0.300000000000001,-33.99)) ;
#124041 = CARTESIAN_POINT('',(0.,0.,0.)) ;
#124042 = CARTESIAN_POINT('Origin',(1.38777878078145E-16,-6.28125000068279,
-2.77555756156289E-16)) ;
#124043 = CARTESIAN_POINT('',(-1.2293670625,-1.09375000068279,-5.21005851079475E-15)) ;
#124044 = CARTESIAN_POINT('',(-1.2293670625,-0.968750000682796,-2.98084374001462E-14)) ;
#124045 = CARTESIAN_POINT('',(-1.2293670625,-6.28125000068279,-7.05665556119359E-16)) ;
#124046 = CARTESIAN_POINT('',(1.16918410523995,-0.819406422395167,-0.379936708431992)) ;
#124047 = CARTESIAN_POINT('Ctrl Pts',(-1.2293670625,-1.09375000068279,-9.67975699595058E-15)) ;
#124048 = CARTESIAN_POINT('Ctrl Pts',(-1.2293670625,-1.0846749481888,0.154589977307616)) ;
#124049 = CARTESIAN_POINT('Ctrl Pts',(-1.20021118839201,-1.07468536503738,
0.307925475665665)) ;
#124050 = CARTESIAN_POINT('Ctrl Pts',(-1.08420684294538,-1.05352652382332,
0.601382937533272)) ;
#124051 = CARTESIAN_POINT('Ctrl Pts',(-0.996398213495616,-1.0425417450548,
0.737808020725081)) ;
#124052 = CARTESIAN_POINT('Ctrl Pts',(-0.776616964406496,-1.02171673600945,
0.96566315863742)) ;
#124053 = CARTESIAN_POINT('Ctrl Pts',(-0.648097680210764,-1.01268166410948,
1.05621820882725)) ;
#124054 = CARTESIAN_POINT('Ctrl Pts',(-0.357410832361479,-0.992977293684764,
1.18752407058778)) ;
#124055 = CARTESIAN_POINT('Ctrl Pts',(-0.196880508044035,-0.982095655942453,
1.22440775145394)) ;
#124056 = CARTESIAN_POINT('Ctrl Pts',(0.124915731705902,-0.960282518003032,
1.23327661515053)) ;
#124057 = CARTESIAN_POINT('Ctrl Pts',(0.283075541788596,-0.949561566892828,
1.20683758809188)) ;
#124058 = CARTESIAN_POINT('Ctrl Pts',(0.579861378775666,-0.929443773081141,
1.09549036257894)) ;
#124059 = CARTESIAN_POINT('Ctrl Pts',(0.715754183345007,-0.920563114801157,
1.01194688536211)) ;
#124060 = CARTESIAN_POINT('Ctrl Pts',(0.952247755389101,-0.899781359138197,
0.794477416094161)) ;
#124061 = CARTESIAN_POINT('Ctrl Pts',(1.0491659407666,-0.888673772908759,
0.661219760303515)) ;
#124062 = CARTESIAN_POINT('Ctrl Pts',(1.18274942698846,-0.867066164473483,
0.370267045631756)) ;
#124063 = CARTESIAN_POINT('Ctrl Pts',(1.22033776635663,-0.856754477438507,
0.21631311942058)) ;
#124064 = CARTESIAN_POINT('Ctrl Pts',(1.23512911303773,-0.838310078143878,
-0.0893402358594326)) ;
#124065 = CARTESIAN_POINT('Ctrl Pts',(1.21524070660064,-0.829287562268207,
-0.238206138425924)) ;
#124066 = CARTESIAN_POINT('Ctrl Pts',(1.16918410523995,-0.819406422395166,
-0.379936708431992)) ;
#124067 = CARTESIAN_POINT('',(1.16918849388564,-0.694407135956962,-0.379923189325734)) ;
#124068 = CARTESIAN_POINT('',(1.16918410523995,-0.819406422395166,-0.37993670843199)) ;
#124069 = CARTESIAN_POINT('Ctrl Pts',(1.16918850806102,-0.694407367007051,
-0.379923159307147)) ;
#124070 = CARTESIAN_POINT('Ctrl Pts',(1.21645797241154,-0.704549055321802,
-0.234454495060375)) ;
#124071 = CARTESIAN_POINT('Ctrl Pts',(1.23615258137902,-0.713735817175049,
-0.0814970379028584)) ;
#124072 = CARTESIAN_POINT('Ctrl Pts',(1.21821185875717,-0.732517494081259,
0.228083416806234)) ;
#124073 = CARTESIAN_POINT('Ctrl Pts',(1.17909262427295,-0.742867933316568,
0.381813608918001)) ;
#124074 = CARTESIAN_POINT('Ctrl Pts',(1.0425035983168,-0.764515665918384,
0.671714573931943)) ;
#124075 = CARTESIAN_POINT('Ctrl Pts',(0.944144533195031,-0.775622301867799,
0.804124149765071)) ;
#124076 = CARTESIAN_POINT('Ctrl Pts',(0.705528340879558,-0.796326994915782,
1.01905539207879)) ;
#124077 = CARTESIAN_POINT('Ctrl Pts',(0.569079951032635,-0.805174598185578,
1.10108618075603)) ;
#124078 = CARTESIAN_POINT('Ctrl Pts',(0.271386894021466,-0.825353888413578,
1.20953938890892)) ;
#124079 = CARTESIAN_POINT('Ctrl Pts',(0.112823651501299,-0.836102186417004,
1.23446116299375)) ;
#124080 = CARTESIAN_POINT('Ctrl Pts',(-0.209011673067325,-0.857917973742702,
1.22239412378343)) ;
#124081 = CARTESIAN_POINT('Ctrl Pts',(-0.369160526837812,-0.868773753290811,
1.18392323231963)) ;
#124082 = CARTESIAN_POINT('Ctrl Pts',(-0.658474392523389,-0.888385055352298,
1.04977191270669)) ;
#124083 = CARTESIAN_POINT('Ctrl Pts',(-0.786055421205409,-0.897487203807662,
0.957987835975483)) ;
#124084 = CARTESIAN_POINT('Ctrl Pts',(-1.00367155178044,-0.918368881220496,
0.727917342783409)) ;
#124085 = CARTESIAN_POINT('Ctrl Pts',(-1.09020270986942,-0.929369371550939,
0.590487070832282)) ;
#124086 = CARTESIAN_POINT('Ctrl Pts',(-1.2017840793143,-0.950226809738017,
0.299610285508617)) ;
#124087 = CARTESIAN_POINT('Ctrl Pts',(-1.22936706250001,-0.959922721618476,
0.150369253637278)) ;
#124088 = CARTESIAN_POINT('Ctrl Pts',(-1.2293670625,-0.968750000682796,-5.94663207564849E-14)) ;
#124089 = CARTESIAN_POINT('Origin',(1.38777878078145E-16,-6.28125000068279,
-2.77555756156289E-16)) ;
#124090 = CARTESIAN_POINT('',(-1.2293670625,-1.59375000068279,2.42108516417716E-14)) ;
#124091 = CARTESIAN_POINT('',(-1.2293670625,-1.46875000068279,4.41765678087653E-15)) ;
#124092 = CARTESIAN_POINT('',(-1.2293670625,-6.28125000068279,-7.05665556119359E-16)) ;
#124093 = CARTESIAN_POINT('Ctrl Pts',(-1.2293670625,-1.59375000068279,4.91273688396627E-14)) ;
#124094 = CARTESIAN_POINT('Ctrl Pts',(-1.2293670625,-1.5929636944515,0.0133944197603256)) ;
#124095 = CARTESIAN_POINT('Ctrl Pts',(-1.22914815761871,-1.59216952410361,
0.0267964168859271)) ;
#124096 = CARTESIAN_POINT('Ctrl Pts',(-1.22337688007584,-1.58161879139812,
0.203191982006123)) ;
#124097 = CARTESIAN_POINT('Ctrl Pts',(-1.18566753703356,-1.57093214183561,
0.36346338702498)) ;
#124098 = CARTESIAN_POINT('Ctrl Pts',(-1.05128310495245,-1.54914312506858,
0.657043895518347)) ;
#124099 = CARTESIAN_POINT('Ctrl Pts',(-0.957014484116075,-1.53825707637603,
0.788057472633634)) ;
#124100 = CARTESIAN_POINT('Ctrl Pts',(-0.726080978284878,-1.51773530910495,
1.00430824684218)) ;
#124101 = CARTESIAN_POINT('Ctrl Pts',(-0.592534031366209,-1.50891525112215,
1.08845244229616)) ;
#124102 = CARTESIAN_POINT('Ctrl Pts',(-0.293706456717641,-1.4886590569821,
1.20501927343027)) ;
#124103 = CARTESIAN_POINT('Ctrl Pts',(-0.130245411804608,-1.47757875870646,
1.23343243303519)) ;
#124104 = CARTESIAN_POINT('Ctrl Pts',(0.191877553061588,-1.45574347352245,
1.22453704189747)) ;
#124105 = CARTESIAN_POINT('Ctrl Pts',(0.347535237170195,-1.44519213041965,
1.18976666575577)) ;
#124106 = CARTESIAN_POINT('Ctrl Pts',(0.639126244266634,-1.42542647105511,
1.06231616683244)) ;
#124107 = CARTESIAN_POINT('Ctrl Pts',(0.771929174362773,-1.41620378837636,
0.970120107315155)) ;
#124108 = CARTESIAN_POINT('Ctrl Pts',(0.996185419970736,-1.39500206676428,
0.738431458301724)) ;
#124109 = CARTESIAN_POINT('Ctrl Pts',(1.08483303727253,-1.38391015640713,
0.600665820172445)) ;
#124110 = CARTESIAN_POINT('Ctrl Pts',(1.20134026294244,-1.36255891131156,
0.304221171309325)) ;
#124111 = CARTESIAN_POINT('Ctrl Pts',(1.23021641354854,-1.35254167696737,
0.149272401123027)) ;
#124112 = CARTESIAN_POINT('Ctrl Pts',(1.22844108996505,-1.33374566651196,
-0.169885317488781)) ;
#124113 = CARTESIAN_POINT('Ctrl Pts',(1.19510722167321,-1.32315253950266,
-0.33108978383975)) ;
#124114 = CARTESIAN_POINT('Ctrl Pts',(1.06861176256678,-1.30140166463955,
-0.628575260556984)) ;
#124115 = CARTESIAN_POINT('Ctrl Pts',(0.977633222956603,-1.29046118528742,
-0.76241557199597)) ;
#124116 = CARTESIAN_POINT('Ctrl Pts',(0.752425302092438,-1.26978135739856,
-0.984664515160361)) ;
#124117 = CARTESIAN_POINT('Ctrl Pts',(0.621501524548423,-1.26087882883529,
-1.0721180183845)) ;
#124118 = CARTESIAN_POINT('Ctrl Pts',(0.325900396799594,-1.24084134120136,
-1.19677560672971)) ;
#124119 = CARTESIAN_POINT('Ctrl Pts',(0.162802692597181,-1.22978567217883,
-1.22961794504459)) ;
#124120 = CARTESIAN_POINT('Ctrl Pts',(-0.160283283818217,-1.2078851087188,
-1.22912292604001)) ;
#124121 = CARTESIAN_POINT('Ctrl Pts',(-0.317178287315828,-1.19724989322978,
-1.19826854858965)) ;
#124122 = CARTESIAN_POINT('Ctrl Pts',(-0.611257629180353,-1.17731556070243,
-1.07843535840023)) ;
#124123 = CARTESIAN_POINT('Ctrl Pts',(-0.745523661530749,-1.16828825891483,
-0.990383019442521)) ;
#124124 = CARTESIAN_POINT('Ctrl Pts',(-0.975660261061792,-1.14728319141039,
-0.7654393203204)) ;
#124125 = CARTESIAN_POINT('Ctrl Pts',(-1.06827259754044,-1.13617936197068,
-0.62975967695568)) ;
#124126 = CARTESIAN_POINT('Ctrl Pts',(-1.19291445872554,-1.11470249565326,
-0.335871653611875)) ;
#124127 = CARTESIAN_POINT('Ctrl Pts',(-1.22596595845213,-1.10451088909497,
-0.181343905866327)) ;
#124128 = CARTESIAN_POINT('Ctrl Pts',(-1.22928414193443,-1.09472088788474,
-0.0164908103436252)) ;
#124129 = CARTESIAN_POINT('Ctrl Pts',(-1.2293670625,-1.09423394389032,-0.00824378366076975)) ;
#124130 = CARTESIAN_POINT('Ctrl Pts',(-1.2293670625,-1.09375000068279,-9.71445146547014E-15)) ;
#124131 = CARTESIAN_POINT('Ctrl Pts',(-1.2293670625,-0.968750000682796,-5.89112092441731E-14)) ;
#124132 = CARTESIAN_POINT('Ctrl Pts',(-1.2293670625,-0.969561252441858,-0.0138193570899708)) ;
#124133 = CARTESIAN_POINT('Ctrl Pts',(-1.2291340479447,-0.970380907670849,
-0.0276473329945444)) ;
#124134 = CARTESIAN_POINT('Ctrl Pts',(-1.22337520926784,-0.980590330322463,
-0.198235996140464)) ;
#124135 = CARTESIAN_POINT('Ctrl Pts',(-1.18813428765872,-0.990840862008632,
-0.352503447128259)) ;
#124136 = CARTESIAN_POINT('Ctrl Pts',(-1.0591708524137,-1.01238302768322,
-0.645008757588703)) ;
#124137 = CARTESIAN_POINT('Ctrl Pts',(-0.964473899961518,-1.02348989465029,
-0.779536590453002)) ;
#124138 = CARTESIAN_POINT('Ctrl Pts',(-0.731256601296687,-1.04438813821597,
-1.00088194299678)) ;
#124139 = CARTESIAN_POINT('Ctrl Pts',(-0.596208734201048,-1.05333565845826,
-1.08675312767868)) ;
#124140 = CARTESIAN_POINT('Ctrl Pts',(-0.300819820295893,-1.0733587610582,
-1.20250729295855)) ;
#124141 = CARTESIAN_POINT('Ctrl Pts',(-0.143301720801929,-1.08403621345754,
-1.23124582846075)) ;
#124142 = CARTESIAN_POINT('Ctrl Pts',(0.178373476902107,-1.10584114649424,
-1.22724221806317)) ;
#124143 = CARTESIAN_POINT('Ctrl Pts',(0.339453479583223,-1.1167600444916,
-1.19278259194041)) ;
#124144 = CARTESIAN_POINT('Ctrl Pts',(0.632211559049604,-1.13660481450894,
-1.06582143468517)) ;
#124145 = CARTESIAN_POINT('Ctrl Pts',(0.7621669073982,-1.14555401570759,-0.97712690087377)) ;
#124146 = CARTESIAN_POINT('Ctrl Pts',(0.98521007958537,-1.16629229695877,
-0.752632409264716)) ;
#124147 = CARTESIAN_POINT('Ctrl Pts',(1.07492981302683,-1.17725129431447,
-0.617749878782074)) ;
#124148 = CARTESIAN_POINT('Ctrl Pts',(1.19848488575403,-1.19899347881046,
-0.318714806209338)) ;
#124149 = CARTESIAN_POINT('Ctrl Pts',(1.23011615353584,-1.20949855073417,
-0.157162351188974)) ;
#124150 = CARTESIAN_POINT('Ctrl Pts',(1.22862156582599,-1.22829404501319,
0.162148657491748)) ;
#124151 = CARTESIAN_POINT('Ctrl Pts',(1.19805319996093,-1.23841662568408,
0.316934214189202)) ;
#124152 = CARTESIAN_POINT('Ctrl Pts',(1.07832719948975,-1.25981447009513,
0.612314303705971)) ;
#124153 = CARTESIAN_POINT('Ctrl Pts',(0.988094145778355,-1.27091209897793,
0.749262002550019)) ;
#124154 = CARTESIAN_POINT('Ctrl Pts',(0.761482650580558,-1.29203619338474,
0.978268498434431)) ;
#124155 = CARTESIAN_POINT('Ctrl Pts',(0.628097914878412,-1.30117403252555,
1.06880791258277)) ;
#124156 = CARTESIAN_POINT('Ctrl Pts',(0.335512092244417,-1.32100712601724,
1.19323354512822)) ;
#124157 = CARTESIAN_POINT('Ctrl Pts',(0.179351679657468,-1.33159254685088,
1.22645458408494)) ;
#124158 = CARTESIAN_POINT('Ctrl Pts',(-0.143179062758288,-1.35345547346396,
1.23202141102484)) ;
#124159 = CARTESIAN_POINT('Ctrl Pts',(-0.306509769412905,-1.36452693668793,
1.20185074800083)) ;
#124160 = CARTESIAN_POINT('Ctrl Pts',(-0.604066552363513,-1.38469698950258,
1.08206937457938)) ;
#124161 = CARTESIAN_POINT('Ctrl Pts',(-0.736568263154353,-1.39354235236009,
0.9966154167158)) ;
#124162 = CARTESIAN_POINT('Ctrl Pts',(-0.965244170093328,-1.41412704291671,
0.777989343568323)) ;
#124163 = CARTESIAN_POINT('Ctrl Pts',(-1.05822258321062,-1.42503550116704,
0.645849126608738)) ;
#124164 = CARTESIAN_POINT('Ctrl Pts',(-1.18950334941557,-1.44681140540772,
0.350700082554891)) ;
#124165 = CARTESIAN_POINT('Ctrl Pts',(-1.22548651319292,-1.45746205873105,
0.190045249358232)) ;
#124166 = CARTESIAN_POINT('Ctrl Pts',(-1.22926817372685,-1.46768945647037,
0.0180088632755795)) ;
#124167 = CARTESIAN_POINT('Ctrl Pts',(-1.2293670625,-1.46822151063544,0.00900262169078512)) ;
#124168 = CARTESIAN_POINT('Ctrl Pts',(-1.2293670625,-1.46875000068279,9.54097911787242E-15)) ;
#124169 = CARTESIAN_POINT('Origin',(1.38777878078145E-16,-6.28125000068279,
-2.77555756156289E-16)) ;
#124170 = CARTESIAN_POINT('',(-1.2293670625,-2.09375000068277,1.96156642580576E-13)) ;
#124171 = CARTESIAN_POINT('',(-1.2293670625,-1.96875000068277,1.76519572832522E-13)) ;
#124172 = CARTESIAN_POINT('',(-1.2293670625,-6.28125000068279,-7.05665556119359E-16)) ;
#124173 = CARTESIAN_POINT('Ctrl Pts',(-1.2293670625,-2.09375000068277,3.93018950717272E-13)) ;
#124174 = CARTESIAN_POINT('Ctrl Pts',(-1.2293670625,-2.09165438781884,0.0356979472348365)) ;
#124175 = CARTESIAN_POINT('Ctrl Pts',(-1.22781227856084,-2.08950396001902,
0.0714319905826287)) ;
#124176 = CARTESIAN_POINT('Ctrl Pts',(-1.21048122524801,-2.0772828419258,
0.269607879191005)) ;
#124177 = CARTESIAN_POINT('Ctrl Pts',(-1.16407025798557,-2.06643292732197,
0.427636555381604)) ;
#124178 = CARTESIAN_POINT('Ctrl Pts',(-1.01421336879494,-2.04461684769803,
0.712745041802709)) ;
#124179 = CARTESIAN_POINT('Ctrl Pts',(-0.913596365833781,-2.03386263496667,
0.837847604645138)) ;
#124180 = CARTESIAN_POINT('Ctrl Pts',(-0.671280967314773,-2.01366982229743,
1.04192342679273)) ;
#124181 = CARTESIAN_POINT('Ctrl Pts',(-0.532242729905873,-2.00482837156033,
1.11934866326663)) ;
#124182 = CARTESIAN_POINT('Ctrl Pts',(-0.227050909601382,-1.98414077347199,
1.21921468555743)) ;
#124183 = CARTESIAN_POINT('Ctrl Pts',(-0.0632066373057889,-1.97303449791407,
1.23856003380864)) ;
#124184 = CARTESIAN_POINT('Ctrl Pts',(0.256275879686575,-1.95137819696474,
1.21258984202624)) ;
#124185 = CARTESIAN_POINT('Ctrl Pts',(0.409093928059733,-1.94101934015713,
1.16992076791325)) ;
#124186 = CARTESIAN_POINT('Ctrl Pts',(0.695384673063911,-1.92161296202043,
1.02678847829774)) ;
#124187 = CARTESIAN_POINT('Ctrl Pts',(0.825134773353636,-1.91179643974479,
0.925760910432755)) ;
#124188 = CARTESIAN_POINT('Ctrl Pts',(1.03673917815347,-1.89020351767688,
0.680103770640548)) ;
#124189 = CARTESIAN_POINT('Ctrl Pts',(1.11694520626755,-1.87916265408012,
0.53833394036141)) ;
#124190 = CARTESIAN_POINT('Ctrl Pts',(1.21629298572484,-1.85811584366874,
0.2371682066349)) ;
#124191 = CARTESIAN_POINT('Ctrl Pts',(1.23651862738949,-1.84876701661882,
0.0813339504507454)) ;
#124192 = CARTESIAN_POINT('Ctrl Pts',(1.21729932128853,-1.82943313601169,
-0.236914888266518)) ;
#124193 = CARTESIAN_POINT('Ctrl Pts',(1.17516767052112,-1.81865968229379,
-0.396111747637677)) ;
#124194 = CARTESIAN_POINT('Ctrl Pts',(1.03288359615056,-1.79684870117668,
-0.685505549659799)) ;
#124195 = CARTESIAN_POINT('Ctrl Pts',(0.935356034691252,-1.78602568611029,
-0.81356382330911)) ;
#124196 = CARTESIAN_POINT('Ctrl Pts',(0.698641389678176,-1.76566863202775,
-1.02367103037446)) ;
#124197 = CARTESIAN_POINT('Ctrl Pts',(0.562350489766241,-1.75686924288746,
-1.10442891361411)) ;
#124198 = CARTESIAN_POINT('Ctrl Pts',(0.260280297711559,-1.73639324611448,
-1.21261626569671)) ;
#124199 = CARTESIAN_POINT('Ctrl Pts',(0.0965657576394018,-1.72529576452781,
-1.23646516205919)) ;
#124200 = CARTESIAN_POINT('Ctrl Pts',(-0.224340566425014,-1.70354295002045,
-1.21895446149861)) ;
#124201 = CARTESIAN_POINT('Ctrl Pts',(-0.378620423336193,-1.69308500370419,
-1.18018834916704)) ;
#124202 = CARTESIAN_POINT('Ctrl Pts',(-0.667579897397263,-1.67349772427702,
-1.04486279772397)) ;
#124203 = CARTESIAN_POINT('Ctrl Pts',(-0.798859430521799,-1.66400913970839,
-0.948283314454632)) ;
#124204 = CARTESIAN_POINT('Ctrl Pts',(-1.01685635677711,-1.64260846532705,
-0.709591762953443)) ;
#124205 = CARTESIAN_POINT('Ctrl Pts',(-1.10131027098922,-1.63153764939205,
-0.569764224464767)) ;
#124206 = CARTESIAN_POINT('Ctrl Pts',(-1.20468360637947,-1.61123179889717,
-0.283544609526032)) ;
#124207 = CARTESIAN_POINT('Ctrl Pts',(-1.2293670625,-1.60210052180872,-0.142247868232065)) ;
#124208 = CARTESIAN_POINT('Ctrl Pts',(-1.2293670625,-1.59375000068279,4.88498130835069E-14)) ;
#124209 = CARTESIAN_POINT('Ctrl Pts',(-1.2293670625,-1.46875000068279,9.22872889219661E-15)) ;
#124210 = CARTESIAN_POINT('Ctrl Pts',(-1.2293670625,-1.47736724240036,-0.146791349411587)) ;
#124211 = CARTESIAN_POINT('Ctrl Pts',(-1.20307951446642,-1.48681290739968,
-0.292517443166858)) ;
#124212 = CARTESIAN_POINT('Ctrl Pts',(-1.09493092752208,-1.50747090916634,
-0.58197882480792)) ;
#124213 = CARTESIAN_POINT('Ctrl Pts',(-1.00882144120501,-1.51855107489725,
-0.721009788420243)) ;
#124214 = CARTESIAN_POINT('Ctrl Pts',(-0.788347960357798,-1.53987430492733,
-0.956952266163614)) ;
#124215 = CARTESIAN_POINT('Ctrl Pts',(-0.656469261544164,-1.54925086493719,
-1.05180073591998)) ;
#124216 = CARTESIAN_POINT('Ctrl Pts',(-0.366470758871749,-1.56890857549942,
-1.18403844371561)) ;
#124217 = CARTESIAN_POINT('Ctrl Pts',(-0.211638887418654,-1.57940394042988,
-1.22124454314158)) ;
#124218 = CARTESIAN_POINT('Ctrl Pts',(0.109771023084182,-1.60119089082539,
-1.23538629411922)) ;
#124219 = CARTESIAN_POINT('Ctrl Pts',(0.273400911000042,-1.61228263421834,
-1.20974993006314)) ;
#124220 = CARTESIAN_POINT('Ctrl Pts',(0.574211105371675,-1.63267322134425,
-1.09827509239713)) ;
#124221 = CARTESIAN_POINT('Ctrl Pts',(0.709422123302591,-1.64147300103867,
-1.01619317767247)) ;
#124222 = CARTESIAN_POINT('Ctrl Pts',(0.943886318187304,-1.66189478869789,
-0.803683961406093)) ;
#124223 = CARTESIAN_POINT('Ctrl Pts',(1.04015319533478,-1.67274330845377,
-0.674463368898782)) ;
#124224 = CARTESIAN_POINT('Ctrl Pts',(1.17937093493386,-1.69454773917046,
-0.383410801185453)) ;
#124225 = CARTESIAN_POINT('Ctrl Pts',(1.21978105472352,-1.70528833345974,
-0.223779762982546)) ;
#124226 = CARTESIAN_POINT('Ctrl Pts',(1.23557210196305,-1.72451804821813,
0.0946739573331135)) ;
#124227 = CARTESIAN_POINT('Ctrl Pts',(1.21365982179292,-1.73397712347788,
0.250319514127987)) ;
#124228 = CARTESIAN_POINT('Ctrl Pts',(1.11097892959094,-1.75508450037914,
0.550592600830559)) ;
#124229 = CARTESIAN_POINT('Ctrl Pts',(1.0291181553708,-1.76613804226454,0.691623032698593)) ;
#124230 = CARTESIAN_POINT('Ctrl Pts',(0.815016630588374,-1.78765717379843,
0.934581466649517)) ;
#124231 = CARTESIAN_POINT('Ctrl Pts',(0.684671650277794,-1.79733915025667,
1.03387490725552)) ;
#124232 = CARTESIAN_POINT('Ctrl Pts',(0.397340687297885,-1.81681604015015,
1.1739852240539)) ;
#124233 = CARTESIAN_POINT('Ctrl Pts',(0.243945652517922,-1.82721400830378,
1.21515064916355)) ;
#124234 = CARTESIAN_POINT('Ctrl Pts',(-0.0761134399203039,-1.84890939274191,
1.23785648021424)) ;
#124235 = CARTESIAN_POINT('Ctrl Pts',(-0.239921769047805,-1.86001323187211,
1.21677070536761)) ;
#124236 = CARTESIAN_POINT('Ctrl Pts',(-0.543915824845551,-1.88061963882401,
1.11368192566813)) ;
#124237 = CARTESIAN_POINT('Ctrl Pts',(-0.681888322082539,-1.88943761756165,
1.03496849326193)) ;
#124238 = CARTESIAN_POINT('Ctrl Pts',(-0.92205026961941,-1.90969407799152,
0.828565160848998)) ;
#124239 = CARTESIAN_POINT('Ctrl Pts',(-1.02148790594684,-1.9204756400724,
0.702315804868243)) ;
#124240 = CARTESIAN_POINT('Ctrl Pts',(-1.16844390552385,-1.94229166039066,
0.415533499296891)) ;
#124241 = CARTESIAN_POINT('Ctrl Pts',(-1.21321088382915,-1.95311308808705,
0.257040928989308)) ;
#124242 = CARTESIAN_POINT('Ctrl Pts',(-1.22815948864037,-1.96501358188157,
0.0629512428882878)) ;
#124243 = CARTESIAN_POINT('Ctrl Pts',(-1.2293670625,-1.96690316013386,0.031460207942469)) ;
#124244 = CARTESIAN_POINT('Ctrl Pts',(-1.2293670625,-1.96875000068277,3.53744811221163E-13)) ;
#124245 = CARTESIAN_POINT('Origin',(1.38777878078145E-16,-6.28125000068279,
-2.77555756156289E-16)) ;
#124246 = CARTESIAN_POINT('',(-1.2293670625,-2.59375000068278,7.81954462141675E-14)) ;
#124247 = CARTESIAN_POINT('',(-1.2293670625,-2.46875000068278,1.17469585710279E-13)) ;
#124248 = CARTESIAN_POINT('',(-1.2293670625,-6.28125000068279,-7.05665556119359E-16)) ;
#124249 = CARTESIAN_POINT('Ctrl Pts',(-1.2293670625,-2.59375000068278,1.57096557984454E-13)) ;
#124250 = CARTESIAN_POINT('Ctrl Pts',(-1.2293670625,-2.59041798638127,0.0567595631653337)) ;
#124251 = CARTESIAN_POINT('Ctrl Pts',(-1.22543686828171,-2.58695022597981,
0.113562409472403)) ;
#124252 = CARTESIAN_POINT('Ctrl Pts',(-1.19480516907715,-2.57303397011835,
0.332935176876669)) ;
#124253 = CARTESIAN_POINT('Ctrl Pts',(-1.1395877039601,-2.56196442677115,
0.489620709083913)) ;
#124254 = CARTESIAN_POINT('Ctrl Pts',(-0.974041076411476,-2.5400962334137,
0.76655845795135)) ;
#124255 = CARTESIAN_POINT('Ctrl Pts',(-0.867410782333212,-2.52950410624931,
0.885428181176129)) ;
#124256 = CARTESIAN_POINT('Ctrl Pts',(-0.613787858855096,-2.50965757318927,
1.0770768627525)) ;
#124257 = CARTESIAN_POINT('Ctrl Pts',(-0.46891377075706,-2.50053558267458,
1.14758762858906)) ;
#124258 = CARTESIAN_POINT('Ctrl Pts',(-0.157513148493988,-2.47942711747584,
1.23001001946445)) ;
#124259 = CARTESIAN_POINT('Ctrl Pts',(0.006218152925851,-2.46832849971186,
1.24003667142442)) ;
#124260 = CARTESIAN_POINT('Ctrl Pts',(0.322046623598325,-2.4469198903343,
1.19669326815554)) ;
#124261 = CARTESIAN_POINT('Ctrl Pts',(0.471515827620829,-2.43678803681242,
1.14607411866743)) ;
#124262 = CARTESIAN_POINT('Ctrl Pts',(0.749151391346744,-2.4179683549754,
0.988261200208687)) ;
#124263 = CARTESIAN_POINT('Ctrl Pts',(0.873466868907703,-2.40749203866311,
0.880341666361781)) ;
#124264 = CARTESIAN_POINT('Ctrl Pts',(1.07120344959392,-2.38575349716913,
0.624197364495544)) ;
#124265 = CARTESIAN_POINT('Ctrl Pts',(1.14345926894784,-2.3747909469172,0.479171516312729)) ;
#124266 = CARTESIAN_POINT('Ctrl Pts',(1.22695710483627,-2.35404111192044,
0.173913673680809)) ;
#124267 = CARTESIAN_POINT('Ctrl Pts',(1.23910029772179,-2.34508162647748,
0.0170642397129778)) ;
#124268 = CARTESIAN_POINT('Ctrl Pts',(1.20331046761246,-2.32525541988233,
-0.30000418356211)) ;
#124269 = CARTESIAN_POINT('Ctrl Pts',(1.15292816679629,-2.31434132547231,
-0.456833287205966)) ;
#124270 = CARTESIAN_POINT('Ctrl Pts',(0.996107159246821,-2.29253501246639,
-0.737754667491894)) ;
#124271 = CARTESIAN_POINT('Ctrl Pts',(0.892680168271379,-2.28185165155821,
-0.860027949842806)) ;
#124272 = CARTESIAN_POINT('Ctrl Pts',(0.645153465138463,-2.26181589338037,
-1.0584196619051)) ;
#124273 = CARTESIAN_POINT('Ctrl Pts',(0.503476137496918,-2.25287841201838,
-1.13269166401237)) ;
#124274 = CARTESIAN_POINT('Ctrl Pts',(0.195404224196466,-2.23199558521684,
-1.2246286865075)) ;
#124275 = CARTESIAN_POINT('Ctrl Pts',(0.0315475709482201,-2.22088847040912,
-1.23971560736718)) ;
#124276 = CARTESIAN_POINT('Ctrl Pts',(-0.286383953719449,-2.19933730434125,
-1.20578422735289)) ;
#124277 = CARTESIAN_POINT('Ctrl Pts',(-0.437726039859254,-2.18907849645844,
-1.15946100120441)) ;
#124278 = CARTESIAN_POINT('Ctrl Pts',(-0.721421918168738,-2.16984801281072,
-1.00890347709829)) ;
#124279 = CARTESIAN_POINT('Ctrl Pts',(-0.849691297930594,-2.15966018389652,
-0.903548341897603)) ;
#124280 = CARTESIAN_POINT('Ctrl Pts',(-1.05503584224954,-2.13788960898763,
-0.651250823162222)) ;
#124281 = CARTESIAN_POINT('Ctrl Pts',(-1.13112248596896,-2.12688577801174,
-0.507733501436846)) ;
#124282 = CARTESIAN_POINT('Ctrl Pts',(-1.21192352861261,-2.10835460046965,
-0.238712628313484)) ;
#124283 = CARTESIAN_POINT('Ctrl Pts',(-1.2293670625,-2.10077062207742,-0.119593545360066)) ;
#124284 = CARTESIAN_POINT('Ctrl Pts',(-1.2293670625,-2.09375000068277,3.92845478369708E-13)) ;
#124285 = CARTESIAN_POINT('Ctrl Pts',(-1.2293670625,-1.96875000068277,3.53744811221163E-13)) ;
#124286 = CARTESIAN_POINT('Ctrl Pts',(-1.2293670625,-1.97602011811598,-0.123843612999709)) ;
#124287 = CARTESIAN_POINT('Ctrl Pts',(-1.21066132790823,-1.98389183184118,
-0.247135423133918)) ;
#124288 = CARTESIAN_POINT('Ctrl Pts',(-1.12578541802853,-2.00275804813483,
-0.519510924931424)) ;
#124289 = CARTESIAN_POINT('Ctrl Pts',(-1.04811519801998,-2.01377702882892,
-0.66237203799655)) ;
#124290 = CARTESIAN_POINT('Ctrl Pts',(-0.840356495119533,-2.03548032780585,
-0.912129722381499)) ;
#124291 = CARTESIAN_POINT('Ctrl Pts',(-0.711517533433462,-2.0455193870648,
-1.0158192466044)) ;
#124292 = CARTESIAN_POINT('Ctrl Pts',(-0.426823083637583,-2.06481755943875,
-1.16353821348196)) ;
#124293 = CARTESIAN_POINT('Ctrl Pts',(-0.274907102661338,-2.07511526910376,
-1.20847145320079)) ;
#124294 = CARTESIAN_POINT('Ctrl Pts',(0.0436397000272458,-2.09670814213611,
-1.23936975273838)) ;
#124295 = CARTESIAN_POINT('Ctrl Pts',(0.207504304544632,-2.10781579592505,
-1.22265811063854)) ;
#124296 = CARTESIAN_POINT('Ctrl Pts',(0.514485845843513,-2.12862471125114,
-1.1276881894575)) ;
#124297 = CARTESIAN_POINT('Ctrl Pts',(0.65515090648707,-2.13751912062421,
-1.05221248572423)) ;
#124298 = CARTESIAN_POINT('Ctrl Pts',(0.900698625889017,-2.15761502660094,
-0.851653612593324)) ;
#124299 = CARTESIAN_POINT('Ctrl Pts',(1.00306605051807,-2.16832607035337,
-0.72829702287968)) ;
#124300 = CARTESIAN_POINT('Ctrl Pts',(1.15725220582521,-2.19013775064452,
-0.445762980333208)) ;
#124301 = CARTESIAN_POINT('Ctrl Pts',(1.20612781607305,-2.20102827364389,
-0.288465518264877)) ;
#124302 = CARTESIAN_POINT('Ctrl Pts',(1.23887181053964,-2.22076540786069,
0.0288441058375796)) ;
#124303 = CARTESIAN_POINT('Ctrl Pts',(1.22525026400788,-2.22977878149898,
0.185494142032774)) ;
#124304 = CARTESIAN_POINT('Ctrl Pts',(1.13887075927967,-2.25058368608936,
0.490026341418299)) ;
#124305 = CARTESIAN_POINT('Ctrl Pts',(1.06516063862746,-2.26156267277276,
0.634492536550117)) ;
#124306 = CARTESIAN_POINT('Ctrl Pts',(0.86483519491506,-2.28328258411032,
0.888824800207864)) ;
#124307 = CARTESIAN_POINT('Ctrl Pts',(0.739459526525195,-2.29362532344838,
0.995539248251014)) ;
#124308 = CARTESIAN_POINT('Ctrl Pts',(0.460128937266179,-2.31255990353838,
1.15071369555177)) ;
#124309 = CARTESIAN_POINT('Ctrl Pts',(0.310012498096698,-2.32273563025639,
1.1998871679237)) ;
#124310 = CARTESIAN_POINT('Ctrl Pts',(-0.00655816362446758,-2.34419454946894,
1.24005672079214)) ;
#124311 = CARTESIAN_POINT('Ctrl Pts',(-0.170348886917707,-2.35529719517782,
1.22832051933773)) ;
#124312 = CARTESIAN_POINT('Ctrl Pts',(-0.480636390556873,-2.37633020700859,
1.14267145379631)) ;
#124313 = CARTESIAN_POINT('Ctrl Pts',(-0.624422912529161,-2.38538137805601,
1.07088728044485)) ;
#124314 = CARTESIAN_POINT('Ctrl Pts',(-0.875997192095689,-2.40529216881394,
0.876961208950336)) ;
#124315 = CARTESIAN_POINT('Ctrl Pts',(-0.981561473325557,-2.41591595614751,
0.756936704295497)) ;
#124316 = CARTESIAN_POINT('Ctrl Pts',(-1.14450005928456,-2.43780819134319,
0.478083658583261)) ;
#124317 = CARTESIAN_POINT('Ctrl Pts',(-1.19817685059442,-2.44886780965977,
0.32067768696166)) ;
#124318 = CARTESIAN_POINT('Ctrl Pts',(-1.2260031200219,-2.46246809002492,
0.105067723177115)) ;
#124319 = CARTESIAN_POINT('Ctrl Pts',(-1.2293670625,-2.46566738973036,0.0525110744537505)) ;
#124320 = CARTESIAN_POINT('Ctrl Pts',(-1.2293670625,-2.46875000068278,2.35644836976677E-13)) ;
#124321 = CARTESIAN_POINT('Origin',(1.38777878078145E-16,-6.28125000068279,
-2.77555756156289E-16)) ;
#124322 = CARTESIAN_POINT('',(-1.2293670625,-3.09375000068279,-4.22221717098752E-16)) ;
#124323 = CARTESIAN_POINT('',(-1.2293670625,-2.96875000068279,-4.74263421378056E-16)) ;
#124324 = CARTESIAN_POINT('',(-1.2293670625,-6.28125000068279,-7.05665556119359E-16)) ;
#124325 = CARTESIAN_POINT('Ctrl Pts',(-1.2293670625,-3.09375000068279,-1.38777878078145E-16)) ;
#124326 = CARTESIAN_POINT('Ctrl Pts',(-1.2293670625,-3.08907858841676,0.0795756847333051)) ;
#124327 = CARTESIAN_POINT('Ctrl Pts',(-1.22164306954691,-3.08414664976013,
0.15912988543831)) ;
#124328 = CARTESIAN_POINT('Ctrl Pts',(-1.17458248654693,-3.06852479441537,
0.398071653875583)) ;
#124329 = CARTESIAN_POINT('Ctrl Pts',(-1.11125235594702,-3.05742160331921,
0.550646512753655)) ;
#124330 = CARTESIAN_POINT('Ctrl Pts',(-0.932081198075618,-3.03571849836161,
0.816905918913092)) ;
#124331 = CARTESIAN_POINT('Ctrl Pts',(-0.819942382837346,-3.02531265364806,
0.92942204711778)) ;
#124332 = CARTESIAN_POINT('Ctrl Pts',(-0.555366920714295,-3.00582142925331,
1.10869473312039)) ;
#124333 = CARTESIAN_POINT('Ctrl Pts',(-0.404448494324175,-2.99616576788673,
1.17221119465974)) ;
#124334 = CARTESIAN_POINT('Ctrl Pts',(-0.0872134952455146,-2.97466181619515,
1.23686382378819)) ;
#124335 = CARTESIAN_POINT('Ctrl Pts',(0.075888549641947,-2.96360585293686,
1.23761013237613)) ;
#124336 = CARTESIAN_POINT('Ctrl Pts',(0.387454086296202,-2.94248620892396,
1.17707813246554)) ;
#124337 = CARTESIAN_POINT('Ctrl Pts',(0.533342525856703,-2.93300347345133,
1.11854812003175)) ;
#124338 = CARTESIAN_POINT('Ctrl Pts',(0.801619005635154,-2.91379501973696,
0.946229105745676)) ;
#124339 = CARTESIAN_POINT('Ctrl Pts',(0.91990801488037,-2.9030612584997,0.831677863708403)) ;
#124340 = CARTESIAN_POINT('Ctrl Pts',(1.102959175131,-2.88125847403389,0.565960576449154)) ;
#124341 = CARTESIAN_POINT('Ctrl Pts',(1.16706618916963,-2.87040491535142,
0.418086642171035)) ;
#124342 = CARTESIAN_POINT('Ctrl Pts',(1.23452333449516,-2.84997005106801,
0.108933105695769)) ;
#124343 = CARTESIAN_POINT('Ctrl Pts',(1.23834432366122,-2.84116898791691,
-0.0491495692642937)) ;
#124344 = CARTESIAN_POINT('Ctrl Pts',(1.18518353494756,-2.82079580679762,
-0.365506362451576)) ;
#124345 = CARTESIAN_POINT('Ctrl Pts',(1.1258936245669,-2.80970538121382,-0.520196388040076)) ;
#124346 = CARTESIAN_POINT('Ctrl Pts',(0.953484360932666,-2.78791180440425,
-0.791900928345222)) ;
#124347 = CARTESIAN_POINT('Ctrl Pts',(0.844066384664019,-2.77740899183833,
-0.907639743180857)) ;
#124348 = CARTESIAN_POINT('Ctrl Pts',(0.58498249902388,-2.75773710547782,
-1.09316049841969)) ;
#124349 = CARTESIAN_POINT('Ctrl Pts',(0.437143185563796,-2.74838199580304,
-1.16022547474248)) ;
#124350 = CARTESIAN_POINT('Ctrl Pts',(0.122806801786795,-2.7270745283695,
-1.23389875445401)) ;
#124351 = CARTESIAN_POINT('Ctrl Pts',(-0.0406776909787178,-2.71599264066807,
-1.2393264481315)) ;
#124352 = CARTESIAN_POINT('Ctrl Pts',(-0.354503158377584,-2.69471980598674,
-1.18744927179352)) ;
#124353 = CARTESIAN_POINT('Ctrl Pts',(-0.502179089971365,-2.68490265480334,
-1.13290771502913)) ;
#124354 = CARTESIAN_POINT('Ctrl Pts',(-0.775238664101213,-2.6659645740121,
-0.967955918775394)) ;
#124355 = CARTESIAN_POINT('Ctrl Pts',(-0.89661686844318,-2.65532131305562,
-0.856729861320318)) ;
#124356 = CARTESIAN_POINT('Ctrl Pts',(-1.08716606259604,-2.63354835571964,
-0.59584965946805)) ;
#124357 = CARTESIAN_POINT('Ctrl Pts',(-1.15543913531375,-2.62263553183912,
-0.449371440771829)) ;
#124358 = CARTESIAN_POINT('Ctrl Pts',(-1.21744939388122,-2.60574934374318,
-0.197523456591343)) ;
#124359 = CARTESIAN_POINT('Ctrl Pts',(-1.2293670625,-2.59955296821977,-0.0988512871362581)) ;
#124360 = CARTESIAN_POINT('Ctrl Pts',(-1.2293670625,-2.59375000068278,1.57096557984454E-13)) ;
#124361 = CARTESIAN_POINT('Ctrl Pts',(-1.2293670625,-2.46875000068278,2.36529545949438E-13)) ;
#124362 = CARTESIAN_POINT('Ctrl Pts',(-1.2293670625,-2.47479559615011,-0.102984359233321)) ;
#124363 = CARTESIAN_POINT('Ctrl Pts',(-1.21643218951429,-2.48126625543479,
-0.205741562296177)) ;
#124364 = CARTESIAN_POINT('Ctrl Pts',(-1.15082544508,-2.49848123688728,-0.461113980896463)) ;
#124365 = CARTESIAN_POINT('Ctrl Pts',(-1.08098469341727,-2.50941445151738,
-0.607034448192572)) ;
#124366 = CARTESIAN_POINT('Ctrl Pts',(-0.887634325931833,-2.53117173733727,
-0.866030433706927)) ;
#124367 = CARTESIAN_POINT('Ctrl Pts',(-0.765113431653198,-2.54177862439221,
-0.975977143603221)) ;
#124368 = CARTESIAN_POINT('Ctrl Pts',(-0.490262894597181,-2.56061314703315,
-1.13813085425707)) ;
#124369 = CARTESIAN_POINT('Ctrl Pts',(-0.341894108069714,-2.57057451750811,
-1.19115887646372)) ;
#124370 = CARTESIAN_POINT('Ctrl Pts',(-0.0272233677377015,-2.59190464948757,
-1.23971771974343)) ;
#124371 = CARTESIAN_POINT('Ctrl Pts',(0.136372501981445,-2.60299408693804,
-1.23249648183158)) ;
#124372 = CARTESIAN_POINT('Ctrl Pts',(0.449574226570522,-2.62422464086445,
-1.15539865499199)) ;
#124373 = CARTESIAN_POINT('Ctrl Pts',(0.596250201571124,-2.63348147569385,
-1.08698585341061)) ;
#124374 = CARTESIAN_POINT('Ctrl Pts',(0.85321269201525,-2.6532217913139,-0.899074644355462)) ;
#124375 = CARTESIAN_POINT('Ctrl Pts',(0.961557236992823,-2.66376014660443,
-0.782110627233372)) ;
#124376 = CARTESIAN_POINT('Ctrl Pts',(1.1313164616044,-2.68558452870488,-0.508351330077954)) ;
#124377 = CARTESIAN_POINT('Ctrl Pts',(1.18903054470321,-2.69666780846138,
-0.352873226563285)) ;
#124378 = CARTESIAN_POINT('Ctrl Pts',(1.23877047881811,-2.71695593887551,
-0.0359902076201987)) ;
#124379 = CARTESIAN_POINT('Ctrl Pts',(1.23329130610041,-2.72576903638811,
0.121832196860172)) ;
#124380 = CARTESIAN_POINT('Ctrl Pts',(1.1626648881041,-2.74626724801714,0.430235050214568)) ;
#124381 = CARTESIAN_POINT('Ctrl Pts',(1.0969419384568,-2.7571446637695,0.577582419508308)) ;
#124382 = CARTESIAN_POINT('Ctrl Pts',(0.910973195462585,-2.77893790350951,
0.841452648906544)) ;
#124383 = CARTESIAN_POINT('Ctrl Pts',(0.791476950211163,-2.78963761801788,
0.954726920172135)) ;
#124384 = CARTESIAN_POINT('Ctrl Pts',(0.521340775364793,-2.80874201746369,
1.12419971515682)) ;
#124385 = CARTESIAN_POINT('Ctrl Pts',(0.374767996714821,-2.81834614259553,
1.18118791847062)) ;
#124386 = CARTESIAN_POINT('Ctrl Pts',(0.062323631990983,-2.83952535846024,
1.23839012382985)) ;
#124387 = CARTESIAN_POINT('Ctrl Pts',(-0.100941337485042,-2.85059236565282,
1.23584244565613)) ;
#124388 = CARTESIAN_POINT('Ctrl Pts',(-0.417071868631584,-2.87202145036841,
1.1677040626515)) ;
#124389 = CARTESIAN_POINT('Ctrl Pts',(-0.566798102144141,-2.88155394679947,
1.10281637829345)) ;
#124390 = CARTESIAN_POINT('Ctrl Pts',(-0.829267848896132,-2.90111505220184,
0.921137561263793)) ;
#124391 = CARTESIAN_POINT('Ctrl Pts',(-0.940373407989954,-2.91155892088745,
0.807377158822231)) ;
#124392 = CARTESIAN_POINT('Ctrl Pts',(-1.11696887428682,-2.93329854470353,
0.539008591937846)) ;
#124393 = CARTESIAN_POINT('Ctrl Pts',(-1.17875668419664,-2.94439782077258,
0.385609964753008)) ;
#124394 = CARTESIAN_POINT('Ctrl Pts',(-1.2224733540385,-2.95969010605744,
0.150351684495328)) ;
#124395 = CARTESIAN_POINT('Ctrl Pts',(-1.2293670625,-2.96433685050023,0.0751762909392223)) ;
#124396 = CARTESIAN_POINT('Ctrl Pts',(-1.2293670625,-2.96875000068279,-2.42861286636753E-16)) ;
#124397 = CARTESIAN_POINT('Origin',(1.38777878078145E-16,-6.28125000068279,
-2.77555756156289E-16)) ;
#124398 = CARTESIAN_POINT('',(-1.2293670625,-3.59375000068281,-1.33093873159813E-13)) ;
#124399 = CARTESIAN_POINT('',(-1.2293670625,-3.4687500006828,-6.19008217057184E-14)) ;
#124400 = CARTESIAN_POINT('',(-1.2293670625,-6.28125000068279,-7.05665556119359E-16)) ;
#124401 = CARTESIAN_POINT('Ctrl Pts',(-1.2293670625,-3.59375000068281,-2.6477084413834E-13)) ;
#124402 = CARTESIAN_POINT('Ctrl Pts',(-1.22936706250002,-3.58760601015228,
0.104660480732079)) ;
#124403 = CARTESIAN_POINT('Ctrl Pts',(-1.21600778734524,-3.58102380425275,
0.209072808136304)) ;
#124404 = CARTESIAN_POINT('Ctrl Pts',(-1.14892130661534,-3.56367559742544,
0.465860342851234)) ;
#124405 = CARTESIAN_POINT('Ctrl Pts',(-1.07844627114001,-3.55273443320507,
0.611550024384985)) ;
#124406 = CARTESIAN_POINT('Ctrl Pts',(-0.883965747763156,-3.53098418698764,
0.869773597210837)) ;
#124407 = CARTESIAN_POINT('Ctrl Pts',(-0.760985628392447,-3.52039238066184,
0.979198279041553)) ;
#124408 = CARTESIAN_POINT('Ctrl Pts',(-0.485411672162505,-3.50160004833661,
1.14021562787906)) ;
#124409 = CARTESIAN_POINT('Ctrl Pts',(-0.336759268855858,-3.49157741591188,
1.19262899043324)) ;
#124410 = CARTESIAN_POINT('Ctrl Pts',(-0.0217473940391149,-3.47022415994073,
1.23983515216573)) ;
#124411 = CARTESIAN_POINT('Ctrl Pts',(0.141888301312603,-3.45913202288751,
1.231883176924)) ;
#124412 = CARTESIAN_POINT('Ctrl Pts',(0.454623961896689,-3.43793306137013,
1.15339476994935)) ;
#124413 = CARTESIAN_POINT('Ctrl Pts',(0.60082851666236,-3.42871357231804,
1.08443438350177)) ;
#124414 = CARTESIAN_POINT('Ctrl Pts',(0.856923708288166,-3.40894549540734,
0.895549536489281)) ;
#124415 = CARTESIAN_POINT('Ctrl Pts',(0.964825898786098,-3.39839291846952,
0.778087865678279)) ;
#124416 = CARTESIAN_POINT('Ctrl Pts',(1.13349582868348,-3.37655660776514,
0.503496464814202)) ;
#124417 = CARTESIAN_POINT('Ctrl Pts',(1.19056336220522,-3.36547660348108,
0.34770087212176)) ;
#124418 = CARTESIAN_POINT('Ctrl Pts',(1.23890533877188,-3.34522346818345,
0.0306068701632447)) ;
#124419 = CARTESIAN_POINT('Ctrl Pts',(1.2327486931859,-3.33640267430905,-0.127111222554901)) ;
#124420 = CARTESIAN_POINT('Ctrl Pts',(1.16082336244135,-3.31587865740719,
-0.435203731035599)) ;
#124421 = CARTESIAN_POINT('Ctrl Pts',(1.09443883629321,-3.30499179111457,
-0.582330125223285)) ;
#124422 = CARTESIAN_POINT('Ctrl Pts',(0.910768604013118,-3.28360944903533,
-0.840527919120294)) ;
#124423 = CARTESIAN_POINT('Ctrl Pts',(0.796088100862452,-3.2733038140609,
-0.94986956932987)) ;
#124424 = CARTESIAN_POINT('Ctrl Pts',(0.52621714509681,-3.25399174662172,
-1.1230330318379)) ;
#124425 = CARTESIAN_POINT('Ctrl Pts',(0.372237511017996,-3.243982328383,-1.18303829228058)) ;
#124426 = CARTESIAN_POINT('Ctrl Pts',(0.0522678883627475,-3.2222930087041,
-1.23877414166441)) ;
#124427 = CARTESIAN_POINT('Ctrl Pts',(-0.110332419279826,-3.21127105598534,
-1.23495833974307)) ;
#124428 = CARTESIAN_POINT('Ctrl Pts',(-0.419620068981708,-3.19030581981244,
-1.16598981359416)) ;
#124429 = CARTESIAN_POINT('Ctrl Pts',(-0.563793406330703,-3.18108853879862,
-1.10350877964673)) ;
#124430 = CARTESIAN_POINT('Ctrl Pts',(-0.827245262968623,-3.1616164357492,
-0.923913104369628)) ;
#124431 = CARTESIAN_POINT('Ctrl Pts',(-0.942369880473406,-3.15080100137205,
-0.806143629847639)) ;
#124432 = CARTESIAN_POINT('Ctrl Pts',(-1.11784570469313,-3.12898528792528,
-0.535832480147024)) ;
#124433 = CARTESIAN_POINT('Ctrl Pts',(-1.17778645929249,-3.11819824637287,
-0.386686248209585)) ;
#124434 = CARTESIAN_POINT('Ctrl Pts',(-1.22211804529408,-3.10304610177953,
-0.154170231946575)) ;
#124435 = CARTESIAN_POINT('Ctrl Pts',(-1.2293670625,-3.09827547011273,-0.0770896054808835)) ;
#124436 = CARTESIAN_POINT('Ctrl Pts',(-1.2293670625,-3.09375000068279,-1.38777878078145E-16)) ;
#124437 = CARTESIAN_POINT('Ctrl Pts',(-1.2293670625,-2.96875000068279,-2.42861286636753E-16)) ;
#124438 = CARTESIAN_POINT('Ctrl Pts',(-1.2293670625,-2.9735185044223,-0.0812296000898806)) ;
#124439 = CARTESIAN_POINT('Ctrl Pts',(-1.22131876533305,-2.97855794949859,
-0.16242789356958)) ;
#124440 = CARTESIAN_POINT('Ctrl Pts',(-1.17378991834763,-2.99403993871629,
-0.398716744783189)) ;
#124441 = CARTESIAN_POINT('Ctrl Pts',(-1.11225471253075,-3.00485328327833,
-0.54739048138406)) ;
#124442 = CARTESIAN_POINT('Ctrl Pts',(-0.933870791753979,-3.02666602419055,
-0.81597200478877)) ;
#124443 = CARTESIAN_POINT('Ctrl Pts',(-0.817526375905969,-3.03745123578314,
-0.932522395069542)) ;
#124444 = CARTESIAN_POINT('Ctrl Pts',(-0.552222673387235,-3.05682321399114,
-1.10934331903335)) ;
#124445 = CARTESIAN_POINT('Ctrl Pts',(-0.407401061733189,-3.06613409204707,
-1.17031584431765)) ;
#124446 = CARTESIAN_POINT('Ctrl Pts',(-0.0972396532885814,-3.08715855644462,
-1.23608004546991)) ;
#124447 = CARTESIAN_POINT('Ctrl Pts',(0.0655662515812561,-3.09819444568632,
-1.23816371320781)) ;
#124448 = CARTESIAN_POINT('Ctrl Pts',(0.384508316336356,-3.11981411177874,
-1.17902676959833)) ;
#124449 = CARTESIAN_POINT('Ctrl Pts',(0.537318554711961,-3.12968216870808,
-1.11768136289317)) ;
#124450 = CARTESIAN_POINT('Ctrl Pts',(0.805184905728154,-3.14906263877633,
-0.942195329204265)) ;
#124451 = CARTESIAN_POINT('Ctrl Pts',(0.918912938143374,-3.15940697617733,
-0.831644489027856)) ;
#124452 = CARTESIAN_POINT('Ctrl Pts',(1.1020653917792,-3.18104846412195,-0.568733306817234)) ;
#124453 = CARTESIAN_POINT('Ctrl Pts',(1.16778794606958,-3.19215532625225,
-0.417477179767121)) ;
#124454 = CARTESIAN_POINT('Ctrl Pts',(1.23513416838476,-3.21287233027657,
-0.10345346149256)) ;
#124455 = CARTESIAN_POINT('Ctrl Pts',(1.23820309414711,-3.22172462798742,
0.0557731004087756)) ;
#124456 = CARTESIAN_POINT('Ctrl Pts',(1.18290380469142,-3.24220806707491,
0.372773431072468)) ;
#124457 = CARTESIAN_POINT('Ctrl Pts',(1.12270956248791,-3.25330205090422,
0.527001953763053)) ;
#124458 = CARTESIAN_POINT('Ctrl Pts',(0.948782669306098,-3.2750768270657,
0.797510028537988)) ;
#124459 = CARTESIAN_POINT('Ctrl Pts',(0.838751730640217,-3.2855586719991,
0.912537773932019)) ;
#124460 = CARTESIAN_POINT('Ctrl Pts',(0.57844541351642,-3.30519078524983,
1.09667523862282)) ;
#124461 = CARTESIAN_POINT('Ctrl Pts',(0.429929124653981,-3.31460701471273,
1.16295792032336)) ;
#124462 = CARTESIAN_POINT('Ctrl Pts',(0.114942506030843,-3.33595855867868,
1.23464275025172)) ;
#124463 = CARTESIAN_POINT('Ctrl Pts',(-0.0484687036745916,-3.34703547884692,
1.23903305836949)) ;
#124464 = CARTESIAN_POINT('Ctrl Pts',(-0.361800080875293,-3.36827482134806,
1.18523743760659)) ;
#124465 = CARTESIAN_POINT('Ctrl Pts',(-0.509077341519926,-3.37801258291071,
1.12981703328546)) ;
#124466 = CARTESIAN_POINT('Ctrl Pts',(-0.781090789954048,-3.39701056694208,
0.963240827763799)) ;
#124467 = CARTESIAN_POINT('Ctrl Pts',(-0.901797856044311,-3.40767444388521,
0.851276103172143)) ;
#124468 = CARTESIAN_POINT('Ctrl Pts',(-1.0907089679849,-3.42945540836165,
0.589313755601145)) ;
#124469 = CARTESIAN_POINT('Ctrl Pts',(-1.15806817539359,-3.4403558606355,
0.442518662013712)) ;
#124470 = CARTESIAN_POINT('Ctrl Pts',(-1.21802169125973,-3.45705071436777,
0.192742523089721)) ;
#124471 = CARTESIAN_POINT('Ctrl Pts',(-1.22936706250001,-3.46308811210588,
0.0964480621133391)) ;
#124472 = CARTESIAN_POINT('Ctrl Pts',(-1.2293670625,-3.4687500006828,-1.23095977855318E-13)) ;
#124473 = CARTESIAN_POINT('Origin',(1.38777878078145E-16,-6.28125000068279,
-2.77555756156289E-16)) ;
#124474 = CARTESIAN_POINT('',(-1.2293670625,-4.09375000068281,-1.69945164818064E-13)) ;
#124475 = CARTESIAN_POINT('',(-1.2293670625,-3.96875000068281,-1.99426391777733E-13)) ;
#124476 = CARTESIAN_POINT('',(-1.2293670625,-6.28125000068279,-7.05665556119359E-16)) ;
#124477 = CARTESIAN_POINT('Ctrl Pts',(-1.2293670625,-4.09375000068281,-3.38930272736349E-13)) ;
#124478 = CARTESIAN_POINT('Ctrl Pts',(-1.22936706250003,-4.08638052380908,
0.125536162289958)) ;
#124479 = CARTESIAN_POINT('Ctrl Pts',(-1.21014633715312,-4.07839389712964,
0.250488139698543)) ;
#124480 = CARTESIAN_POINT('Ctrl Pts',(-1.12362683665224,-4.05939449681373,
0.524183451846886)) ;
#124481 = CARTESIAN_POINT('Ctrl Pts',(-1.0453277057579,-4.04836981458519,
0.666778586456919)) ;
#124482 = CARTESIAN_POINT('Ctrl Pts',(-0.836612973503375,-4.02669358615773,
0.915523170792202)) ;
#124483 = CARTESIAN_POINT('Ctrl Pts',(-0.707547991574335,-4.01671153668759,
1.01855193211573)) ;
#124484 = CARTESIAN_POINT('Ctrl Pts',(-0.422457351582659,-3.99738650833981,
1.16513818239883)) ;
#124485 = CARTESIAN_POINT('Ctrl Pts',(-0.270315676817875,-3.98707349989521,
1.20951433049297)) ;
#124486 = CARTESIAN_POINT('Ctrl Pts',(0.0484689556015864,-3.96546450544165,
1.23919865340816)) ;
#124487 = CARTESIAN_POINT('Ctrl Pts',(0.212332360409137,-3.95435693297571,
1.22183753073967)) ;
#124488 = CARTESIAN_POINT('Ctrl Pts',(0.518875100939212,-3.93357776200495,
1.12565795121915)) ;
#124489 = CARTESIAN_POINT('Ctrl Pts',(0.659137378893126,-3.92469835485736,
1.0497013584745)) ;
#124490 = CARTESIAN_POINT('Ctrl Pts',(0.903890852904691,-3.90457848394732,
0.848275694268292)) ;
#124491 = CARTESIAN_POINT('Ctrl Pts',(1.00583041356504,-3.89385659734632,
0.724487373483557)) ;
#124492 = CARTESIAN_POINT('Ctrl Pts',(1.15895567003433,-3.87204333499161,
0.441313870872362)) ;
#124493 = CARTESIAN_POINT('Ctrl Pts',(1.20722606073727,-3.86116254905237,
0.283832852155816)) ;
#124494 = CARTESIAN_POINT('Ctrl Pts',(1.23874930343796,-3.84146129761652,
-0.0335703241386011)) ;
#124495 = CARTESIAN_POINT('Ctrl Pts',(1.2245344497137,-3.8324241078749,-0.190142053275185)) ;
#124496 = CARTESIAN_POINT('Ctrl Pts',(1.13699604646107,-3.81159718918911,
-0.494380163809215)) ;
#124497 = CARTESIAN_POINT('Ctrl Pts',(1.06270206926562,-3.8006118661332,-0.638617206841338)) ;
#124498 = CARTESIAN_POINT('Ctrl Pts',(0.861339561302336,-3.7789000006111,
-0.892213663848438)) ;
#124499 = CARTESIAN_POINT('Ctrl Pts',(0.73554048225724,-3.76860902331144,
-0.998440434382698)) ;
#124500 = CARTESIAN_POINT('Ctrl Pts',(0.455535097815912,-3.74962870185291,
-1.15254829981474)) ;
#124501 = CARTESIAN_POINT('Ctrl Pts',(0.305162198330013,-3.73943559082904,
-1.20113795706868)) ;
#124502 = CARTESIAN_POINT('Ctrl Pts',(-0.0116982000569486,-3.71795703165468,
-1.24002767785997)) ;
#124503 = CARTESIAN_POINT('Ctrl Pts',(-0.17550792565351,-3.70685309786405,
-1.22760302835133)) ;
#124504 = CARTESIAN_POINT('Ctrl Pts',(-0.485343860960918,-3.68585069584499,
-1.14065819846299)) ;
#124505 = CARTESIAN_POINT('Ctrl Pts',(-0.628694615511167,-3.67682560507665,
-1.06836209807631)) ;
#124506 = CARTESIAN_POINT('Ctrl Pts',(-0.879440832705246,-3.65688903408383,
-0.873518788308913)) ;
#124507 = CARTESIAN_POINT('Ctrl Pts',(-0.984571189267261,-3.64625273681576,
-0.753030655278479)) ;
#124508 = CARTESIAN_POINT('Ctrl Pts',(-1.14645061853887,-3.62435139506056,
-0.473410978480525)) ;
#124509 = CARTESIAN_POINT('Ctrl Pts',(-1.19950278771445,-3.6132961104085,
-0.315718203385222)) ;
#124510 = CARTESIAN_POINT('Ctrl Pts',(-1.22621928597872,-3.59982319482307,
-0.101637122233833)) ;
#124511 = CARTESIAN_POINT('Ctrl Pts',(-1.22936706249999,-3.59673190874796,
-0.0507956400729371)) ;
#124512 = CARTESIAN_POINT('Ctrl Pts',(-1.2293670625,-3.59375000068281,-2.65482080763506E-13)) ;
#124513 = CARTESIAN_POINT('Ctrl Pts',(-1.2293670625,-3.4687500006828,-1.23095977855318E-13)) ;
#124514 = CARTESIAN_POINT('Ctrl Pts',(-1.22936706249999,-3.47222775039935,
-0.0592421090809118)) ;
#124515 = CARTESIAN_POINT('Ctrl Pts',(-1.2250856159725,-3.47585300320359,
-0.118524981385997)) ;
#124516 = CARTESIAN_POINT('Ctrl Pts',(-1.19277723758023,-3.48995421553719,
-0.340080378925659)) ;
#124517 = CARTESIAN_POINT('Ctrl Pts',(-1.13666371204228,-3.50102902580151,
-0.496338290285139)) ;
#124518 = CARTESIAN_POINT('Ctrl Pts',(-0.969603180734232,-3.52288219124833,
-0.772145991817219)) ;
#124519 = CARTESIAN_POINT('Ctrl Pts',(-0.862355731305695,-3.5334553732651,
-0.890336677038728)) ;
#124520 = CARTESIAN_POINT('Ctrl Pts',(-0.6075371086556,-3.55326408644235,
-1.08065077443381)) ;
#124521 = CARTESIAN_POINT('Ctrl Pts',(-0.462022010915018,-3.56243158048319,
-1.15041362155065)) ;
#124522 = CARTESIAN_POINT('Ctrl Pts',(-0.149974532350621,-3.5835838931978,
-1.23093887072348)) ;
#124523 = CARTESIAN_POINT('Ctrl Pts',(0.0137138229336498,-3.59467959983398,
-1.23996367402928)) ;
#124524 = CARTESIAN_POINT('Ctrl Pts',(0.329092262799837,-3.61605770362185,
-1.19476309977395)) ;
#124525 = CARTESIAN_POINT('Ctrl Pts',(0.478175266376449,-3.62616337833069,
-1.14329942778789)) ;
#124526 = CARTESIAN_POINT('Ctrl Pts',(0.754804709660387,-3.6449148597313,
-0.98394691504196)) ;
#124527 = CARTESIAN_POINT('Ctrl Pts',(0.878493111818562,-3.65547281413675,
-0.875325006304689)) ;
#124528 = CARTESIAN_POINT('Ctrl Pts',(1.07470347427421,-3.67722138650442,
-0.618128669913968)) ;
#124529 = CARTESIAN_POINT('Ctrl Pts',(1.14610401386665,-3.68817383765985,
-0.472781059897794)) ;
#124530 = CARTESIAN_POINT('Ctrl Pts',(1.22791026291866,-3.70889112795589,
-0.167100965425369)) ;
#124531 = CARTESIAN_POINT('Ctrl Pts',(1.23918350911488,-3.71782254272044,
-0.0101313563127505)) ;
#124532 = CARTESIAN_POINT('Ctrl Pts',(1.20159883077571,-3.73770092954693,
0.306789680728972)) ;
#124533 = CARTESIAN_POINT('Ctrl Pts',(1.15033099587973,-3.74862842966255,
0.463335881996003)) ;
#124534 = CARTESIAN_POINT('Ctrl Pts',(0.991965571920356,-3.77043063170934,
0.743295564467743)) ;
#124535 = CARTESIAN_POINT('Ctrl Pts',(0.887919578162098,-3.78109726087565,
0.864926446702843)) ;
#124536 = CARTESIAN_POINT('Ctrl Pts',(0.639228485315649,-3.80109733796104,
1.06203808456671)) ;
#124537 = CARTESIAN_POINT('Ctrl Pts',(0.496949753192357,-3.81006398395441,
1.13559806310939)) ;
#124538 = CARTESIAN_POINT('Ctrl Pts',(0.188238382595696,-3.83099015672611,
1.22573793466198)) ;
#124539 = CARTESIAN_POINT('Ctrl Pts',(0.0243937945375404,-3.84209645368818,
1.23986468914897)) ;
#124540 = CARTESIAN_POINT('Ctrl Pts',(-0.293160443086161,-3.86362204514294,
1.20414337576111)) ;
#124541 = CARTESIAN_POINT('Ctrl Pts',(-0.444157114198976,-3.87385743887512,
1.15700113913959)) ;
#124542 = CARTESIAN_POINT('Ctrl Pts',(-0.72725774007465,-3.89304757300398,
1.00476258948857)) ;
#124543 = CARTESIAN_POINT('Ctrl Pts',(-0.855187517823339,-3.90332747876962,
0.898414466008073)) ;
#124544 = CARTESIAN_POINT('Ctrl Pts',(-1.05908987483039,-3.92513750554639,
0.644612252868314)) ;
#124545 = CARTESIAN_POINT('Ctrl Pts',(-1.13423370611862,-3.93613178141959,
0.500713365577207)) ;
#124546 = CARTESIAN_POINT('Ctrl Pts',(-1.2126517599951,-3.95446371636377,
0.233710693139845)) ;
#124547 = CARTESIAN_POINT('Ctrl Pts',(-1.22936706250004,-3.96187746419692,
0.117070976735388)) ;
#124548 = CARTESIAN_POINT('Ctrl Pts',(-1.2293670625,-3.96875000068281,-3.97772093041482E-13)) ;
#124549 = CARTESIAN_POINT('Origin',(1.38777878078145E-16,-6.28125000068279,
-2.77555756156289E-16)) ;
#124550 = CARTESIAN_POINT('',(-1.2293670625,-4.59375000068279,-2.88487871326898E-15)) ;
#124551 = CARTESIAN_POINT('',(-1.2293670625,-4.46875000068279,-4.21931813261631E-14)) ;
#124552 = CARTESIAN_POINT('',(-1.2293670625,-6.28125000068279,-7.05665556119359E-16)) ;
#124553 = CARTESIAN_POINT('Ctrl Pts',(-1.2293670625,-4.59375000068279,-5.51642065360625E-15)) ;
#124554 = CARTESIAN_POINT('Ctrl Pts',(-1.2293670625,-4.58502896270038,0.148559478272167)) ;
#124555 = CARTESIAN_POINT('Ctrl Pts',(-1.20244149704241,-4.57546057872006,
0.29600768244092)) ;
#124556 = CARTESIAN_POINT('Ctrl Pts',(-1.09241263142596,-4.55466592437684,
0.586711307991789)) ;
#124557 = CARTESIAN_POINT('Ctrl Pts',(-1.00566097257559,-4.54358248897905,
0.725427210618369)) ;
#124558 = CARTESIAN_POINT('Ctrl Pts',(-0.784228883049274,-4.52228968246801,
0.960297982609938)) ;
#124559 = CARTESIAN_POINT('Ctrl Pts',(-0.652117065633409,-4.51295412039647,
1.05447525637748)) ;
#124560 = CARTESIAN_POINT('Ctrl Pts',(-0.361715619769164,-4.4932690961048,
1.18550797902303)) ;
#124561 = CARTESIAN_POINT('Ctrl Pts',(-0.20667242902016,-4.48275940677778,
1.22210291679461)) ;
#124562 = CARTESIAN_POINT('Ctrl Pts',(0.114924739347508,-4.46095976300325,
1.23492670753276)) ;
#124563 = CARTESIAN_POINT('Ctrl Pts',(0.278516439940176,-4.44987060815935,
1.20859199982724)) ;
#124564 = CARTESIAN_POINT('Ctrl Pts',(0.578830914555416,-4.42951362367414,
1.09583492247798)) ;
#124565 = CARTESIAN_POINT('Ctrl Pts',(0.713621918901493,-4.42071100408087,
1.01323505807178)) ;
#124566 = CARTESIAN_POINT('Ctrl Pts',(0.947202221169259,-4.40026400633689,
0.799786082210475)) ;
#124567 = CARTESIAN_POINT('Ctrl Pts',(1.04297114101472,-4.38940580677613,
0.670113102222645)) ;
#124568 = CARTESIAN_POINT('Ctrl Pts',(1.18098138091927,-4.36760464824602,
0.378419124657103)) ;
#124569 = CARTESIAN_POINT('Ctrl Pts',(1.22071531321839,-4.35687728656373,
0.218623101719924)) ;
#124570 = CARTESIAN_POINT('Ctrl Pts',(1.23516206743971,-4.33768862691041,
-0.0999073888403545)) ;
#124571 = CARTESIAN_POINT('Ctrl Pts',(1.212586789702,-4.32818351361548,-0.255480936687184)) ;
#124572 = CARTESIAN_POINT('Ctrl Pts',(1.10859373622348,-4.30705247791321,
-0.555399465164944)) ;
#124573 = CARTESIAN_POINT('Ctrl Pts',(1.02608340058017,-4.29599431067272,
-0.696133663689217)) ;
#124574 = CARTESIAN_POINT('Ctrl Pts',(0.811004123444689,-4.27450452743128,
-0.93802765534849)) ;
#124575 = CARTESIAN_POINT('Ctrl Pts',(0.68042538038046,-4.264873015331,-1.03664089660206)) ;
#124576 = CARTESIAN_POINT('Ctrl Pts',(0.392686325852142,-4.24536846272385,
-1.17555839978656)) ;
#124577 = CARTESIAN_POINT('Ctrl Pts',(0.239067393119562,-4.23495531752239,
-1.21612778762906)) ;
#124578 = CARTESIAN_POINT('Ctrl Pts',(-0.0812104726257985,-4.21324510341337,
-1.23754148401705)) ;
#124579 = CARTESIAN_POINT('Ctrl Pts',(-0.244999659907664,-4.20214256182388,
-1.21576769693668)) ;
#124580 = CARTESIAN_POINT('Ctrl Pts',(-0.548516914349574,-4.18156847511833,
-1.11140752058824)) ;
#124581 = CARTESIAN_POINT('Ctrl Pts',(-0.686070105373153,-4.17275723050083,
-1.03218467955117)) ;
#124582 = CARTESIAN_POINT('Ctrl Pts',(-0.925376763970217,-4.15247569306073,
-0.824860368756792)) ;
#124583 = CARTESIAN_POINT('Ctrl Pts',(-1.02434314788367,-4.14168358188332,
-0.698159235325802)) ;
#124584 = CARTESIAN_POINT('Ctrl Pts',(-1.17014351158204,-4.11986824510788,
-0.410721366954031)) ;
#124585 = CARTESIAN_POINT('Ctrl Pts',(-1.21425721494069,-4.10905844566451,
-0.25204971093212)) ;
#124586 = CARTESIAN_POINT('Ctrl Pts',(-1.22828505133293,-4.0972847201261,
-0.0595878667026296)) ;
#124587 = CARTESIAN_POINT('Ctrl Pts',(-1.22936706249999,-4.09549818489378,
-0.0297796357305136)) ;
#124588 = CARTESIAN_POINT('Ctrl Pts',(-1.2293670625,-4.09375000068281,-3.3918466408001E-13)) ;
#124589 = CARTESIAN_POINT('Ctrl Pts',(-1.2293670625,-3.96875000068281,-3.98147117999346E-13)) ;
#124590 = CARTESIAN_POINT('Ctrl Pts',(-1.22936706249999,-3.97099398318985,
-0.0382253661975134)) ;
#124591 = CARTESIAN_POINT('Ctrl Pts',(-1.22758434631669,-3.9733006693718,
-0.0764896133558483)) ;
#124592 = CARTESIAN_POINT('Ctrl Pts',(-1.20879117961218,-3.98571363210003,
-0.277089348885761)) ;
#124593 = CARTESIAN_POINT('Ctrl Pts',(-1.16140207282899,-3.99657996572339,
-0.434832987550155)) ;
#124594 = CARTESIAN_POINT('Ctrl Pts',(-1.00982419566573,-4.01839494669545,
-0.718929145995987)) ;
#124595 = CARTESIAN_POINT('Ctrl Pts',(-0.908509961324784,-4.02913233953647,
-0.843342641846237)) ;
#124596 = CARTESIAN_POINT('Ctrl Pts',(-0.664912394162676,-4.04928690955548,
-1.04602675496179)) ;
#124597 = CARTESIAN_POINT('Ctrl Pts',(-0.525232762040495,-4.05814680439437,
-1.12268103208231)) ;
#124598 = CARTESIAN_POINT('Ctrl Pts',(-0.219329781308588,-4.07888260888969,
-1.22061340271302)) ;
#124599 = CARTESIAN_POINT('Ctrl Pts',(-0.0554725601817823,-4.08998976219138,
-1.23891705515827)) ;
#124600 = CARTESIAN_POINT('Ctrl Pts',(0.263648966044517,-4.1116215931799,
-1.21099598897818)) ;
#124601 = CARTESIAN_POINT('Ctrl Pts',(0.416114393967901,-4.12195654741327,
-1.16742976198749)) ;
#124602 = CARTESIAN_POINT('Ctrl Pts',(0.701777012591598,-4.14132034765226,
-1.0224853899473)) ;
#124603 = CARTESIAN_POINT('Ctrl Pts',(0.831168411807016,-4.15122215030892,
-0.920410477317314)) ;
#124604 = CARTESIAN_POINT('Ctrl Pts',(1.04126155347177,-4.1728589190223,-0.673133898854699)) ;
#124605 = CARTESIAN_POINT('Ctrl Pts',(1.12046919701639,-4.18389151887796,
-0.530928420580006)) ;
#124606 = CARTESIAN_POINT('Ctrl Pts',(1.21781227475221,-4.20490157974945,
-0.229231285843895)) ;
#124607 = CARTESIAN_POINT('Ctrl Pts',(1.23702161082716,-4.214188766796,-0.0732794835073471)) ;
#124608 = CARTESIAN_POINT('Ctrl Pts',(1.21573099869258,-4.23358520739107,
0.244839171091622)) ;
#124609 = CARTESIAN_POINT('Ctrl Pts',(1.172561374576,-4.2443778941776,0.403764384087774)) ;
#124610 = CARTESIAN_POINT('Ctrl Pts',(1.02843398404133,-4.26619158332599,
0.692140077282357)) ;
#124611 = CARTESIAN_POINT('Ctrl Pts',(0.930151239543393,-4.27699862077546,
0.819490173332727)) ;
#124612 = CARTESIAN_POINT('Ctrl Pts',(0.692079448142443,-4.29731625571283,
1.02814234181259)) ;
#124613 = CARTESIAN_POINT('Ctrl Pts',(0.555129934481888,-4.30612020785312,
1.10809793093287)) ;
#124614 = CARTESIAN_POINT('Ctrl Pts',(0.252301527439119,-4.32664760065277,
1.21428676574491)) ;
#124615 = CARTESIAN_POINT('Ctrl Pts',(0.0885448104424789,-4.33774794122583,
1.23705126113019)) ;
#124616 = CARTESIAN_POINT('Ctrl Pts',(-0.232038974862563,-4.35947889226316,
1.21749986572218)) ;
#124617 = CARTESIAN_POINT('Ctrl Pts',(-0.38597614135646,-4.36991360911797,
1.17779036275969)) ;
#124618 = CARTESIAN_POINT('Ctrl Pts',(-0.674299787885864,-4.3894577886206,
1.0405887745593)) ;
#124619 = CARTESIAN_POINT('Ctrl Pts',(-0.805213866067154,-4.39901932993295,
0.942949798707443)) ;
#124620 = CARTESIAN_POINT('Ctrl Pts',(-1.02169191086748,-4.4204666797767,
0.702586222304148)) ;
#124621 = CARTESIAN_POINT('Ctrl Pts',(-1.10513306619431,-4.43153112845838,
0.562282430875642)) ;
#124622 = CARTESIAN_POINT('Ctrl Pts',(-1.20563624208665,-4.45162168231164,
0.278073222839467)) ;
#124623 = CARTESIAN_POINT('Ctrl Pts',(-1.22936706250001,-4.46056203071758,
0.139478872651708)) ;
#124624 = CARTESIAN_POINT('Ctrl Pts',(-1.2293670625,-4.4687500006828,-8.41687830543947E-14)) ;
#124625 = CARTESIAN_POINT('Origin',(1.38777878078145E-16,-6.28125000068279,
-2.77555756156289E-16)) ;
#124626 = CARTESIAN_POINT('',(-1.2293670625,-5.09375000068279,4.13369617262378E-14)) ;
#124627 = CARTESIAN_POINT('',(-1.2293670625,-4.96875000068279,8.00274656689887E-16)) ;
#124628 = CARTESIAN_POINT('',(-1.2293670625,-6.28125000068279,-7.05665556119359E-16)) ;
#124629 = CARTESIAN_POINT('Ctrl Pts',(-1.2293670625,-5.09375000068279,8.3379589008595E-14)) ;
#124630 = CARTESIAN_POINT('Ctrl Pts',(-1.2293670625,-5.09284878208426,0.0153519070867942)) ;
#124631 = CARTESIAN_POINT('Ctrl Pts',(-1.22907950061357,-5.09193720633504,
0.0307142202611759)) ;
#124632 = CARTESIAN_POINT('Ctrl Pts',(-1.22262209133582,-5.08161187395681,
0.202874040436789)) ;
#124633 = CARTESIAN_POINT('Ctrl Pts',(-1.18677932781036,-5.07134546323376,
0.357064511027953)) ;
#124634 = CARTESIAN_POINT('Ctrl Pts',(-1.05663006087162,-5.04978606774068,
0.649178684474244)) ;
#124635 = CARTESIAN_POINT('Ctrl Pts',(-0.961362253967709,-5.03867876569656,
0.78338434573489)) ;
#124636 = CARTESIAN_POINT('Ctrl Pts',(-0.727302402490689,-5.01781019475081,
1.00373778868626)) ;
#124637 = CARTESIAN_POINT('Ctrl Pts',(-0.592038632639754,-5.00888167024263,
1.0890111704998)) ;
#124638 = CARTESIAN_POINT('Ctrl Pts',(-0.296290879588158,-4.98883424353062,
1.20363887658012)) ;
#124639 = CARTESIAN_POINT('Ctrl Pts',(-0.138605626097923,-4.97814546050423,
1.23179093614033)) ;
#124640 = CARTESIAN_POINT('Ctrl Pts',(0.183107568848696,-4.95633795180321,
1.22654437988664)) ;
#124641 = CARTESIAN_POINT('Ctrl Pts',(0.344050664648374,-4.9454283341153,
1.19146438075983)) ;
#124642 = CARTESIAN_POINT('Ctrl Pts',(0.636281586836292,-4.92561929774868,
1.06339132794893)) ;
#124643 = CARTESIAN_POINT('Ctrl Pts',(0.765869002702726,-4.91665000809934,
0.97422244440075)) ;
#124644 = CARTESIAN_POINT('Ctrl Pts',(0.988082378871063,-4.8958895101667,
0.748870417339189)) ;
#124645 = CARTESIAN_POINT('Ctrl Pts',(1.07731754330718,-4.88492371284935,
0.613592286118149)) ;
#124646 = CARTESIAN_POINT('Ctrl Pts',(1.19972527392039,-4.8631886143498,0.3140155024508)) ;
#124647 = CARTESIAN_POINT('Ctrl Pts',(1.23072524817926,-4.85273861333006,
0.152333359387764)) ;
#124648 = CARTESIAN_POINT('Ctrl Pts',(1.22797339605001,-4.83389663328735,
-0.167043634183287)) ;
#124649 = CARTESIAN_POINT('Ctrl Pts',(1.19677229142187,-4.82375624256793,
-0.321767266211094)) ;
#124650 = CARTESIAN_POINT('Ctrl Pts',(1.07579219170482,-4.80233776217868,
-0.616774827025522)) ;
#124651 = CARTESIAN_POINT('Ctrl Pts',(0.984951348674464,-4.7912382756839,
-0.75340326223757)) ;
#124652 = CARTESIAN_POINT('Ctrl Pts',(0.757438346836806,-4.77014429628392,
-0.981376275633077)) ;
#124653 = CARTESIAN_POINT('Ctrl Pts',(0.623829483135525,-4.76103663080903,
-1.07128051838844)) ;
#124654 = CARTESIAN_POINT('Ctrl Pts',(0.330862225988127,-4.74117768156569,
-1.19453918189261)) ;
#124655 = CARTESIAN_POINT('Ctrl Pts',(0.174511857316672,-4.73057938445271,
-1.22716045151316)) ;
#124656 = CARTESIAN_POINT('Ctrl Pts',(-0.148167291193781,-4.70870639804956,
-1.23144051771096)) ;
#124657 = CARTESIAN_POINT('Ctrl Pts',(-0.311442806770412,-4.69763867598367,
-1.20059131312558)) ;
#124658 = CARTESIAN_POINT('Ctrl Pts',(-0.608505635138163,-4.67750210615645,
-1.07957038658589)) ;
#124659 = CARTESIAN_POINT('Ctrl Pts',(-0.740605368455963,-4.66864436882701,
-0.993609634978932)) ;
#124660 = CARTESIAN_POINT('Ctrl Pts',(-0.96840469503832,-4.64803545715341,
-0.774064870652292)) ;
#124661 = CARTESIAN_POINT('Ctrl Pts',(-1.06087962465526,-4.63711863061326,
-0.641491416807209)) ;
#124662 = CARTESIAN_POINT('Ctrl Pts',(-1.19095276777593,-4.61534849633566,
-0.345743440309638)) ;
#124663 = CARTESIAN_POINT('Ctrl Pts',(-1.22626597007615,-4.60471213040813,
-0.184945184885094)) ;
#124664 = CARTESIAN_POINT('Ctrl Pts',(-1.22930203210093,-4.59460948656494,
-0.0146034612325995)) ;
#124665 = CARTESIAN_POINT('Ctrl Pts',(-1.2293670625,-4.59417857029751,-0.00730051611917697)) ;
#124666 = CARTESIAN_POINT('Ctrl Pts',(-1.2293670625,-4.59375000068279,-5.06409187041859E-15)) ;
#124667 = CARTESIAN_POINT('Ctrl Pts',(-1.2293670625,-4.46875000068279,-8.36806970962069E-14)) ;
#124668 = CARTESIAN_POINT('Ctrl Pts',(-1.2293670625,-4.46969418767222,-0.0160838568556484)) ;
#124669 = CARTESIAN_POINT('Ctrl Pts',(-1.22905142635401,-4.47064969040176,
-0.032178240313783)) ;
#124670 = CARTESIAN_POINT('Ctrl Pts',(-1.22201498643679,-4.48139941711593,
-0.211233148868625)) ;
#124671 = CARTESIAN_POINT('Ctrl Pts',(-1.18325041985583,-4.4921074897812,
-0.371260254487391)) ;
#124672 = CARTESIAN_POINT('Ctrl Pts',(-1.04697425945045,-4.51390327251257,
-0.663863828685305)) ;
#124673 = CARTESIAN_POINT('Ctrl Pts',(-0.951921929457506,-4.52477501772297,
-0.794181276872157)) ;
#124674 = CARTESIAN_POINT('Ctrl Pts',(-0.719608812587659,-4.54525794704699,
-1.00897394300623)) ;
#124675 = CARTESIAN_POINT('Ctrl Pts',(-0.585415954352627,-4.55406725307158,
-1.09231439546215)) ;
#124676 = CARTESIAN_POINT('Ctrl Pts',(-0.285812911339319,-4.57437601276808,
-1.2069010047664)) ;
#124677 = CARTESIAN_POINT('Ctrl Pts',(-0.122280738326348,-4.58546113250172,
-1.23423319108302)) ;
#124678 = CARTESIAN_POINT('Ctrl Pts',(0.199574657571679,-4.6072782803737,
-1.22329361058302)) ;
#124679 = CARTESIAN_POINT('Ctrl Pts',(0.354915451505969,-4.61780814289895,
-1.18757326266864)) ;
#124680 = CARTESIAN_POINT('Ctrl Pts',(0.645889580423866,-4.63753198683143,
-1.05826043376743)) ;
#124681 = CARTESIAN_POINT('Ctrl Pts',(0.77833354374751,-4.64681167308246,
-0.965037010195778)) ;
#124682 = CARTESIAN_POINT('Ctrl Pts',(1.00112632899522,-4.66806086570081,
-0.731694781884955)) ;
#124683 = CARTESIAN_POINT('Ctrl Pts',(1.08879073817631,-4.67914860187923,
-0.593432593788058)) ;
#124684 = CARTESIAN_POINT('Ctrl Pts',(1.20327793618126,-4.70046498019187,
-0.296415623447903)) ;
#124685 = CARTESIAN_POINT('Ctrl Pts',(1.23113924151489,-4.71039075322585,
-0.141373349843462)) ;
#124686 = CARTESIAN_POINT('Ctrl Pts',(1.2273366077552,-4.72925026045624,0.177695543471893)) ;
#124687 = CARTESIAN_POINT('Ctrl Pts',(1.1929760443945,-4.73986600719604,0.338692565429254)) ;
#124688 = CARTESIAN_POINT('Ctrl Pts',(1.06462297287925,-4.76162728401739,
0.635282742420915)) ;
#124689 = CARTESIAN_POINT('Ctrl Pts',(0.972866586397243,-4.77255569380347,
0.768468363411924)) ;
#124690 = CARTESIAN_POINT('Ctrl Pts',(0.746314148313346,-4.79319885597278,
0.989316462975599)) ;
#124691 = CARTESIAN_POINT('Ctrl Pts',(0.614782536371606,-4.80207662289861,
1.07599647139047)) ;
#124692 = CARTESIAN_POINT('Ctrl Pts',(0.318422776110228,-4.82216553486134,
1.19877238766902)) ;
#124693 = CARTESIAN_POINT('Ctrl Pts',(0.155230107174869,-4.83322764112137,
1.23058301764731)) ;
#124694 = CARTESIAN_POINT('Ctrl Pts',(-0.167650703191224,-4.85511429728609,
1.22812774481372)) ;
#124695 = CARTESIAN_POINT('Ctrl Pts',(-0.324266271721261,-4.86573057111969,
1.19635781101463)) ;
#124696 = CARTESIAN_POINT('Ctrl Pts',(-0.6177715031012,-4.88562598724701,
1.07475189497485)) ;
#124697 = CARTESIAN_POINT('Ctrl Pts',(-0.751697555684333,-4.89469335132708,
0.985743499654557)) ;
#124698 = CARTESIAN_POINT('Ctrl Pts',(-0.980480609085495,-4.91574452589831,
0.759232914422474)) ;
#124699 = CARTESIAN_POINT('Ctrl Pts',(-1.07217853127028,-4.92684631372623,
0.623060111779056)) ;
#124700 = CARTESIAN_POINT('Ctrl Pts',(-1.1949290402703,-4.94829337115356,
0.328587898550516)) ;
#124701 = CARTESIAN_POINT('Ctrl Pts',(-1.22702424319334,-4.95845867067516,
0.173956162690442)) ;
#124702 = CARTESIAN_POINT('Ctrl Pts',(-1.22932590429998,-4.96806660773399,
0.0116175694612323)) ;
#124703 = CARTESIAN_POINT('Ctrl Pts',(-1.2293670625,-4.96840905022387,0.00580795799728944)) ;
#124704 = CARTESIAN_POINT('Ctrl Pts',(-1.2293670625,-4.96875000068279,2.30621486949913E-15)) ;
#124705 = CARTESIAN_POINT('Origin',(1.38777878078145E-16,-6.28125000068279,
-2.77555756156289E-16)) ;
#124706 = CARTESIAN_POINT('',(-1.2293670625,-5.59375000068276,2.30508168050804E-13)) ;
#124707 = CARTESIAN_POINT('',(-1.2293670625,-5.46875000068277,1.7277409858811E-13)) ;
#124708 = CARTESIAN_POINT('',(-1.2293670625,-6.28125000068279,-7.05665556119359E-16)) ;
#124709 = CARTESIAN_POINT('Ctrl Pts',(-1.2293670625,-5.59375000068276,4.61722001657727E-13)) ;
#124710 = CARTESIAN_POINT('Ctrl Pts',(-1.2293670625,-5.59164548201965,0.0358496540482043)) ;
#124711 = CARTESIAN_POINT('Ctrl Pts',(-1.22779903349981,-5.5894855426238,
0.071738076682763)) ;
#124712 = CARTESIAN_POINT('Ctrl Pts',(-1.21085554071052,-5.57758691020917,
0.264644305792692)) ;
#124713 = CARTESIAN_POINT('Ctrl Pts',(-1.16696861853625,-5.56712153675488,
0.417579731695604)) ;
#124714 = CARTESIAN_POINT('Ctrl Pts',(-1.02105739078779,-5.54536183800115,
0.704005820693454)) ;
#124715 = CARTESIAN_POINT('Ctrl Pts',(-0.918250213710935,-5.53426538160571,
0.833673873163033)) ;
#124716 = CARTESIAN_POINT('Ctrl Pts',(-0.673086072626478,-5.51380607448702,
1.04064460195925)) ;
#124717 = CARTESIAN_POINT('Ctrl Pts',(-0.534883633508067,-5.50500738668682,
1.1179832669468)) ;
#124718 = CARTESIAN_POINT('Ctrl Pts',(-0.234380415239824,-5.48463760810762,
1.21731386882016)) ;
#124719 = CARTESIAN_POINT('Ctrl Pts',(-0.0746398841095792,-5.47380950693786,
1.2374189512917)) ;
#124720 = CARTESIAN_POINT('Ctrl Pts',(0.247108611652305,-5.45199960535135,
1.2152613505116)) ;
#124721 = CARTESIAN_POINT('Ctrl Pts',(0.405949532666192,-5.44123248475606,
1.17181512506259)) ;
#124722 = CARTESIAN_POINT('Ctrl Pts',(0.69087078452292,-5.42191893847767,
1.02873323211164)) ;
#124723 = CARTESIAN_POINT('Ctrl Pts',(0.815517005212891,-5.41254933387899,
0.933033347134467)) ;
#124724 = CARTESIAN_POINT('Ctrl Pts',(1.02618449411922,-5.39149063919752,
0.695935633721784)) ;
#124725 = CARTESIAN_POINT('Ctrl Pts',(1.10857205809211,-5.38044719452686,
0.555381346171666)) ;
#124726 = CARTESIAN_POINT('Ctrl Pts',(1.21481446902847,-5.35886860071852,
0.249137507169526)) ;
#124727 = CARTESIAN_POINT('Ctrl Pts',(1.23707969576023,-5.34907907533427,
0.0863258158992063)) ;
#124728 = CARTESIAN_POINT('Ctrl Pts',(1.21727824541617,-5.32965889532013,
-0.233056998398954)) ;
#124729 = CARTESIAN_POINT('Ctrl Pts',(1.17751154204835,-5.31929233582844,
-0.386687976452286)) ;
#124730 = CARTESIAN_POINT('Ctrl Pts',(1.03965314901271,-5.29762824188659,
-0.676134781082961)) ;
#124731 = CARTESIAN_POINT('Ctrl Pts',(0.940686524261572,-5.28652234596215,
-0.808180976163961)) ;
#124732 = CARTESIAN_POINT('Ctrl Pts',(0.701175784845335,-5.265850506202,-1.0220361085325)) ;
#124733 = CARTESIAN_POINT('Ctrl Pts',(0.564491191556748,-5.25701435155461,
-1.10342827247686)) ;
#124734 = CARTESIAN_POINT('Ctrl Pts',(0.266415312056727,-5.23680911149027,
-1.2106525210943)) ;
#124735 = CARTESIAN_POINT('Ctrl Pts',(0.107685092815524,-5.2260494948765,
-1.23492835474597)) ;
#124736 = CARTESIAN_POINT('Ctrl Pts',(-0.214157127434278,-5.2042332401232,
-1.22150263084659)) ;
#124737 = CARTESIAN_POINT('Ctrl Pts',(-0.374139095164007,-5.19338877303862,
-1.18235894157638)) ;
#124738 = CARTESIAN_POINT('Ctrl Pts',(-0.662866899682181,-5.17381719746088,
-1.04700112806878)) ;
#124739 = CARTESIAN_POINT('Ctrl Pts',(-0.790050604030013,-5.16468398806342,
-0.954693314448044)) ;
#124740 = CARTESIAN_POINT('Ctrl Pts',(-1.00674170146085,-5.14377831804275,
-0.72368004841069)) ;
#124741 = CARTESIAN_POINT('Ctrl Pts',(-1.09272499297458,-5.13277145411584,
-0.58582489381677)) ;
#124742 = CARTESIAN_POINT('Ctrl Pts',(-1.2024388735119,-5.1120432358759,-0.296071124635525)) ;
#124743 = CARTESIAN_POINT('Ctrl Pts',(-1.2293670625,-5.10247198077965,-0.148575526824205)) ;
#124744 = CARTESIAN_POINT('Ctrl Pts',(-1.2293670625,-5.09375000068278,8.31973379078477E-14)) ;
#124745 = CARTESIAN_POINT('Ctrl Pts',(-1.2293670625,-4.96875000068279,2.28983498828939E-15)) ;
#124746 = CARTESIAN_POINT('Ctrl Pts',(-1.2293670625,-4.9779692030022,-0.157045513322919)) ;
#124747 = CARTESIAN_POINT('Ctrl Pts',(-1.19927615342303,-4.98813037442379,
-0.312764108202359)) ;
#124748 = CARTESIAN_POINT('Ctrl Pts',(-1.08066375780161,-5.00946453554043,
-0.607702317713977)) ;
#124749 = CARTESIAN_POINT('Ctrl Pts',(-0.992116119573704,-5.02043967283196,
-0.743536495191188)) ;
#124750 = CARTESIAN_POINT('Ctrl Pts',(-0.771076879831951,-5.04123142702765,
-0.970098848476667)) ;
#124751 = CARTESIAN_POINT('Ctrl Pts',(-0.642007014364489,-5.05023119644413,
-1.05993767817084)) ;
#124752 = CARTESIAN_POINT('Ctrl Pts',(-0.35052171785429,-5.06998969015752,
-1.18957625383883)) ;
#124753 = CARTESIAN_POINT('Ctrl Pts',(-0.189775773925879,-5.08088594379565,
-1.22552972972925)) ;
#124754 = CARTESIAN_POINT('Ctrl Pts',(0.131982747362557,-5.10269652496808,
-1.23252888345983)) ;
#124755 = CARTESIAN_POINT('Ctrl Pts',(0.289899945947995,-5.11340103052236,
-1.20520492820835)) ;
#124756 = CARTESIAN_POINT('Ctrl Pts',(0.586151376763805,-5.13348259931309,
-1.09216483808053)) ;
#124757 = CARTESIAN_POINT('Ctrl Pts',(0.721719503405525,-5.14238657510161,
-1.00773069578433)) ;
#124758 = CARTESIAN_POINT('Ctrl Pts',(0.956960869932357,-5.16321320460779,
-0.788773856918631)) ;
#124759 = CARTESIAN_POINT('Ctrl Pts',(1.05302964360807,-5.17432082613859,
-0.65502519170843)) ;
#124760 = CARTESIAN_POINT('Ctrl Pts',(1.18484451629919,-5.19590391876801,
-0.363468984722966)) ;
#124761 = CARTESIAN_POINT('Ctrl Pts',(1.22153340201252,-5.20619242080942,
-0.209390706018484)) ;
#124762 = CARTESIAN_POINT('Ctrl Pts',(1.23524705774866,-5.22547449563549,
0.11115433015815)) ;
#124763 = CARTESIAN_POINT('Ctrl Pts',(1.20945802580139,-5.2355482796211,0.274657637770185)) ;
#124764 = CARTESIAN_POINT('Ctrl Pts',(1.0962294828551,-5.25726770184908,0.579266988739864)) ;
#124765 = CARTESIAN_POINT('Ctrl Pts',(1.0110180947514,-5.2682831804208,0.717714549087699)) ;
#124766 = CARTESIAN_POINT('Ctrl Pts',(0.79562688147457,-5.28922234415717,
0.950048855965618)) ;
#124767 = CARTESIAN_POINT('Ctrl Pts',(0.668997995129403,-5.29840159772973,
1.04309131886271)) ;
#124768 = CARTESIAN_POINT('Ctrl Pts',(0.381093133546937,-5.3179173896607,
1.18013529979385)) ;
#124769 = CARTESIAN_POINT('Ctrl Pts',(0.221349534550088,-5.32874569878751,
1.2202190139566)) ;
#124770 = CARTESIAN_POINT('Ctrl Pts',(-0.100492620884541,-5.35056194914727,
1.23554610633831)) ;
#124771 = CARTESIAN_POINT('Ctrl Pts',(-0.259452092351532,-5.36133710575128,
1.2121755814012)) ;
#124772 = CARTESIAN_POINT('Ctrl Pts',(-0.55806114307902,-5.38157848712523,
1.10667077730846)) ;
#124773 = CARTESIAN_POINT('Ctrl Pts',(-0.695076546443144,-5.39040120294259,
1.02616841726249)) ;
#124774 = CARTESIAN_POINT('Ctrl Pts',(-0.935832077499682,-5.41102695405935,
0.813817067734723)) ;
#124775 = CARTESIAN_POINT('Ctrl Pts',(-1.03564439017971,-5.42213148123599,
0.682282446891744)) ;
#124776 = CARTESIAN_POINT('Ctrl Pts',(-1.17527171908201,-5.4438177929767,
0.393478466327615)) ;
#124777 = CARTESIAN_POINT('Ctrl Pts',(-1.21594161068744,-5.45420657140173,
0.239990453388942)) ;
#124778 = CARTESIAN_POINT('Ctrl Pts',(-1.22843447299397,-5.46547080560192,
0.0553213775535472)) ;
#124779 = CARTESIAN_POINT('Ctrl Pts',(-1.2293670625,-5.46712701393339,0.0276469458359286)) ;
#124780 = CARTESIAN_POINT('Ctrl Pts',(-1.2293670625,-5.46875000068277,3.46253862732339E-13)) ;
#124781 = CARTESIAN_POINT('Origin',(0.,-6.,0.)) ;
#124782 = CARTESIAN_POINT('',(-5.11233613721112E-18,-5.375,-1.5)) ;
#124783 = CARTESIAN_POINT('',(2.44084776499009E-15,-5.43750000136559,-1.5)) ;
#124784 = CARTESIAN_POINT('',(-1.83697019872103E-16,-6.,-1.5)) ;
#124785 = CARTESIAN_POINT('',(1.5,-5.5,2.18789702550307E-15)) ;
#124786 = CARTESIAN_POINT('Ctrl Pts',(2.6028203465122E-16,-5.375,-1.5)) ;
#124787 = CARTESIAN_POINT('Ctrl Pts',(0.00627939642630949,-5.37534885535701,
-1.5)) ;
#124788 = CARTESIAN_POINT('Ctrl Pts',(0.0125606239867182,-5.37569781244372,
-1.49996056922169)) ;
#124789 = CARTESIAN_POINT('Ctrl Pts',(0.211760718905342,-5.38676448438364,
-1.49745797770769)) ;
#124790 = CARTESIAN_POINT('Ctrl Pts',(0.402432473209262,-5.39735735962274,
-1.45783659499529)) ;
#124791 = CARTESIAN_POINT('Ctrl Pts',(0.759763626140605,-5.41720909034115,
-1.30790067891821)) ;
#124792 = CARTESIAN_POINT('Ctrl Pts',(0.922783335544204,-5.42630494071755,
-1.19846684672405)) ;
#124793 = CARTESIAN_POINT('Ctrl Pts',(1.20053817819605,-5.44737703217331,
-0.920853483620446)) ;
#124794 = CARTESIAN_POINT('Ctrl Pts',(1.31154581317371,-5.45846953542253,
-0.754390421027587)) ;
#124795 = CARTESIAN_POINT('Ctrl Pts',(1.46163692622999,-5.48017399618236,
-0.3899268201106)) ;
#124796 = CARTESIAN_POINT('Ctrl Pts',(1.49999999999998,-5.4905763386166,-0.195867123712562)) ;
#124797 = CARTESIAN_POINT('Ctrl Pts',(1.5,-5.49999999999999,-1.21361254379337E-13)) ;
#124798 = CARTESIAN_POINT('',(1.0702882195569,-5.5,-1.05094392194718)) ;
#124799 = CARTESIAN_POINT('Origin',(0.,-5.5,0.)) ;
#124800 = CARTESIAN_POINT('Ctrl Pts',(1.07028821955797,-5.50000000000008,
-1.05094392194609)) ;
#124801 = CARTESIAN_POINT('Ctrl Pts',(0.951434023208664,-5.49087486355005,
-1.17198581917894)) ;
#124802 = CARTESIAN_POINT('Ctrl Pts',(0.812952038001049,-5.48266400347676,
-1.27195507031725)) ;
#124803 = CARTESIAN_POINT('Ctrl Pts',(0.488455764700654,-5.46463643273785,
-1.43116046170094)) ;
#124804 = CARTESIAN_POINT('Ctrl Pts',(0.301613723641133,-5.45425631934565,
-1.48182926271782)) ;
#124805 = CARTESIAN_POINT('Ctrl Pts',(0.0735608407828244,-5.44158671474241,
-1.49864874723003)) ;
#124806 = CARTESIAN_POINT('Ctrl Pts',(0.0367597598691759,-5.43954221024721,
-1.5)) ;
#124807 = CARTESIAN_POINT('Ctrl Pts',(5.8009255759016E-15,-5.43750000136559,
-1.5)) ;
#124808 = CARTESIAN_POINT('Origin',(0.,-6.,0.)) ;
#124809 = CARTESIAN_POINT('',(-5.60223848449789E-16,-4.875,-1.5)) ;
#124810 = CARTESIAN_POINT('',(2.73575075590614E-15,-4.93750000136559,-1.5)) ;
#124811 = CARTESIAN_POINT('',(-1.83697019872103E-16,-6.,-1.5)) ;
#124812 = CARTESIAN_POINT('Ctrl Pts',(-2.90044460754259E-15,-4.875,-1.5)) ;
#124813 = CARTESIAN_POINT('Ctrl Pts',(0.0349268394965454,-4.87694037997203,
-1.5)) ;
#124814 = CARTESIAN_POINT('Ctrl Pts',(0.0698921259947087,-4.8788828958886,
-1.4987801389553)) ;
#124815 = CARTESIAN_POINT('Ctrl Pts',(0.296235001513499,-4.89145750008409,
-1.48292265504425)) ;
#124816 = CARTESIAN_POINT('Ctrl Pts',(0.483325472522242,-4.90185141514013,
-1.43291016146182)) ;
#124817 = CARTESIAN_POINT('Ctrl Pts',(0.833833573082252,-4.92132408739346,
-1.26247976005801)) ;
#124818 = CARTESIAN_POINT('Ctrl Pts',(0.992890450701865,-4.93098682628875,
-1.14163204431774)) ;
#124819 = CARTESIAN_POINT('Ctrl Pts',(1.25436042977266,-4.9524833708566,-0.845794518574959)) ;
#124820 = CARTESIAN_POINT('Ctrl Pts',(1.35445596581748,-4.96353065663441,
-0.673971180220349)) ;
#124821 = CARTESIAN_POINT('Ctrl Pts',(1.48027440059481,-4.98463133952581,
-0.308043029300386)) ;
#124822 = CARTESIAN_POINT('Ctrl Pts',(1.50734151292801,-4.99410432545235,
-0.118300669872091)) ;
#124823 = CARTESIAN_POINT('Ctrl Pts',(1.48883164120595,-5.01330273861437,
0.270044174962478)) ;
#124824 = CARTESIAN_POINT('Ctrl Pts',(1.43996163357746,-5.02402998059384,
0.464790600505272)) ;
#124825 = CARTESIAN_POINT('Ctrl Pts',(1.27095866584812,-5.0458190474935,0.820093942629593)) ;
#124826 = CARTESIAN_POINT('Ctrl Pts',(1.15391895956398,-5.05666462066784,
0.977942042002604)) ;
#124827 = CARTESIAN_POINT('Ctrl Pts',(0.868676473684781,-5.07708618396317,
1.23771143836587)) ;
#124828 = CARTESIAN_POINT('Ctrl Pts',(0.704105023314977,-5.08588305426029,
1.33819376579349)) ;
#124829 = CARTESIAN_POINT('Ctrl Pts',(0.337688250459132,-5.10623954164117,
1.47512215716681)) ;
#124830 = CARTESIAN_POINT('Ctrl Pts',(0.138187517703181,-5.11732291568316,
1.506953454537)) ;
#124831 = CARTESIAN_POINT('Ctrl Pts',(-0.253896032125235,-5.13910533511807,
1.49082395737517)) ;
#124832 = CARTESIAN_POINT('Ctrl Pts',(-0.442856428360514,-5.14960313490892,
1.44599994376874)) ;
#124833 = CARTESIAN_POINT('Ctrl Pts',(-0.796837488041822,-5.16926874933566,
1.28588072861318)) ;
#124834 = CARTESIAN_POINT('Ctrl Pts',(-0.957898920644956,-5.17860925758179,
1.17084651260735)) ;
#124835 = CARTESIAN_POINT('Ctrl Pts',(-1.22769099510352,-5.19989497128947,
0.884195788016511)) ;
#124836 = CARTESIAN_POINT('Ctrl Pts',(-1.33334132709955,-5.21097013125647,
0.715000158456778)) ;
#124837 = CARTESIAN_POINT('Ctrl Pts',(-1.47043879159951,-5.23223468081537,
0.352178053658129)) ;
#124838 = CARTESIAN_POINT('Ctrl Pts',(-1.50319554783772,-5.24206769335176,
0.163024947227471)) ;
#124839 = CARTESIAN_POINT('Ctrl Pts',(-1.4961573087957,-5.26097674263809,
-0.225928732608051)) ;
#124840 = CARTESIAN_POINT('Ctrl Pts',(-1.45307315827811,-5.27160694938967,
-0.421998784973272)) ;
#124841 = CARTESIAN_POINT('Ctrl Pts',(-1.2944520114607,-5.29336372026264,
-0.782624813886513)) ;
#124842 = CARTESIAN_POINT('Ctrl Pts',(-1.1817196818813,-5.304272525567,-0.944274033501697)) ;
#124843 = CARTESIAN_POINT('Ctrl Pts',(-0.904044499744878,-5.32486772741253,
-1.21202142421113)) ;
#124844 = CARTESIAN_POINT('Ctrl Pts',(-0.743003475249922,-5.33372202915279,
-1.31690283208648)) ;
#124845 = CARTESIAN_POINT('Ctrl Pts',(-0.386661677317576,-5.35351879570459,
-1.46228259539781)) ;
#124846 = CARTESIAN_POINT('Ctrl Pts',(-0.194206592983103,-5.36421074483427,
-1.5)) ;
#124847 = CARTESIAN_POINT('Ctrl Pts',(3.46944695195361E-16,-5.375,-1.5)) ;
#124848 = CARTESIAN_POINT('Ctrl Pts',(5.62050406216485E-15,-5.43750000136559,
-1.5)) ;
#124849 = CARTESIAN_POINT('Ctrl Pts',(-0.161994290474594,-5.42850031856145,
-1.5)) ;
#124850 = CARTESIAN_POINT('Ctrl Pts',(-0.323186117287328,-5.41954521707184,
-1.47375554236172)) ;
#124851 = CARTESIAN_POINT('Ctrl Pts',(-0.659347051983786,-5.4008696095887,
-1.36094099963937)) ;
#124852 = CARTESIAN_POINT('Ctrl Pts',(-0.828000153264918,-5.39204971142785,
-1.26543038225483)) ;
#124853 = CARTESIAN_POINT('Ctrl Pts',(-1.12165392398143,-5.37182789626481,
-1.01466893042269)) ;
#124854 = CARTESIAN_POINT('Ctrl Pts',(-1.24336974114535,-5.36106353363079,
-0.861208514308281)) ;
#124855 = CARTESIAN_POINT('Ctrl Pts',(-1.42378561965319,-5.33926125406271,
-0.512219799137908)) ;
#124856 = CARTESIAN_POINT('Ctrl Pts',(-1.47908425176341,-5.32843676932294,
-0.319163788852183)) ;
#124857 = CARTESIAN_POINT('Ctrl Pts',(-1.51042735663741,-5.30892123156154,
0.0683630963888204)) ;
#124858 = CARTESIAN_POINT('Ctrl Pts',(-1.48965804817001,-5.2997591131944,
0.258843459079508)) ;
#124859 = CARTESIAN_POINT('Ctrl Pts',(-1.37625164813583,-5.2788448851852,
0.628062309648105)) ;
#124860 = CARTESIAN_POINT('Ctrl Pts',(-1.28234235921275,-5.26784005660849,
0.802574823090399)) ;
#124861 = CARTESIAN_POINT('Ctrl Pts',(-1.0302400818302,-5.24612128021888,
1.10843979560054)) ;
#124862 = CARTESIAN_POINT('Ctrl Pts',(-0.873405472831508,-5.23602252763399,
1.23578325781099)) ;
#124863 = CARTESIAN_POINT('Ctrl Pts',(-0.526771579872414,-5.21676508913627,
1.41743721034463)) ;
#124864 = CARTESIAN_POINT('Ctrl Pts',(-0.341867333422598,-5.20649263100017,
1.47299730884172)) ;
#124865 = CARTESIAN_POINT('Ctrl Pts',(0.0462100909223037,-5.18493277409212,
1.51240764724932)) ;
#124866 = CARTESIAN_POINT('Ctrl Pts',(0.246014476734837,-5.17383253043587,
1.49298285093653)) ;
#124867 = CARTESIAN_POINT('Ctrl Pts',(0.621002890592565,-5.15299984077711,
1.37900479354308)) ;
#124868 = CARTESIAN_POINT('Ctrl Pts',(0.793171709133358,-5.14408867506976,
1.28770123413088)) ;
#124869 = CARTESIAN_POINT('Ctrl Pts',(1.09381042503216,-5.12403797775275,
1.04452915992086)) ;
#124870 = CARTESIAN_POINT('Ctrl Pts',(1.21930985636277,-5.11334977285415,
0.894836123269743)) ;
#124871 = CARTESIAN_POINT('Ctrl Pts',(1.40907773114056,-5.0915550033271,0.551402878935084)) ;
#124872 = CARTESIAN_POINT('Ctrl Pts',(1.46969977226217,-5.08065861913372,
0.359925938194671)) ;
#124873 = CARTESIAN_POINT('Ctrl Pts',(1.51176058718588,-5.06088381495732,
-0.0268018255058508)) ;
#124874 = CARTESIAN_POINT('Ctrl Pts',(1.49620870472285,-5.05190795725008,
-0.217962597419856)) ;
#124875 = CARTESIAN_POINT('Ctrl Pts',(1.39300652386959,-5.03115159167009,
-0.589791747703553)) ;
#124876 = CARTESIAN_POINT('Ctrl Pts',(1.30423149612885,-5.02019081729288,
-0.76635287887949)) ;
#124877 = CARTESIAN_POINT('Ctrl Pts',(1.06197871256978,-4.9984749914188,-1.07784313398654)) ;
#124878 = CARTESIAN_POINT('Ctrl Pts',(0.909936830813567,-4.98805204752189,
-1.20892691786967)) ;
#124879 = CARTESIAN_POINT('Ctrl Pts',(0.57067768749066,-4.96920431733728,
-1.40025758894091)) ;
#124880 = CARTESIAN_POINT('Ctrl Pts',(0.388176202716192,-4.95906534596093,
-1.46139985085397)) ;
#124881 = CARTESIAN_POINT('Ctrl Pts',(0.132995506608445,-4.94488864062161,
-1.49558275095357)) ;
#124882 = CARTESIAN_POINT('Ctrl Pts',(0.0664632989529273,-4.94119240686297,
-1.5)) ;
#124883 = CARTESIAN_POINT('Ctrl Pts',(6.54463398306847E-15,-4.93750000136559,
-1.5)) ;
#124884 = CARTESIAN_POINT('Origin',(0.,-6.,0.)) ;
#124885 = CARTESIAN_POINT('',(-2.58117669796277E-15,-4.375,-1.5)) ;
#124886 = CARTESIAN_POINT('',(-1.94691842705875E-15,-4.43750000136559,-1.5)) ;
#124887 = CARTESIAN_POINT('',(-1.83697019872103E-16,-6.,-1.5)) ;
#124888 = CARTESIAN_POINT('Ctrl Pts',(-2.90044460754259E-15,-4.375,-1.5)) ;
#124889 = CARTESIAN_POINT('Ctrl Pts',(0.0646412971543186,-4.37859118317524,
-1.5)) ;
#124890 = CARTESIAN_POINT('Ctrl Pts',(0.129351575045616,-4.38218619861364,
-1.49582161897791)) ;
#124891 = CARTESIAN_POINT('Ctrl Pts',(0.382903534036573,-4.39627241855758,
-1.46279893074578)) ;
#124892 = CARTESIAN_POINT('Ctrl Pts',(0.565688061329142,-4.40642711451828,
-1.40228980244635)) ;
#124893 = CARTESIAN_POINT('Ctrl Pts',(0.9056869803183,-4.42531594335101,-1.21211601328188)) ;
#124894 = CARTESIAN_POINT('Ctrl Pts',(1.0581933129685,-4.43569097384046,-1.08156079863571)) ;
#124895 = CARTESIAN_POINT('Ctrl Pts',(1.30158022961293,-4.45740012168722,
-0.770864135762298)) ;
#124896 = CARTESIAN_POINT('Ctrl Pts',(1.39099228872664,-4.46836678784929,
-0.594548336372274)) ;
#124897 = CARTESIAN_POINT('Ctrl Pts',(1.49545643839563,-4.4891428936166,-0.223037492035378)) ;
#124898 = CARTESIAN_POINT('Ctrl Pts',(1.51165586675903,-4.49813833108958,
-0.0319645438657472)) ;
#124899 = CARTESIAN_POINT('Ctrl Pts',(1.47092876716576,-4.51788115719622,
0.354868589041279)) ;
#124900 = CARTESIAN_POINT('Ctrl Pts',(1.41096661834321,-4.52876906002735,
0.546550236973955)) ;
#124901 = CARTESIAN_POINT('Ctrl Pts',(1.22235311022667,-4.55056568182347,
0.890688453901026)) ;
#124902 = CARTESIAN_POINT('Ctrl Pts',(1.09731829876053,-4.56126377194236,
1.04085519940139)) ;
#124903 = CARTESIAN_POINT('Ctrl Pts',(0.797546755734701,-4.58133598597994,
1.28497515274195)) ;
#124904 = CARTESIAN_POINT('Ctrl Pts',(0.625821141799246,-4.59023215878893,
1.37680518623772)) ;
#124905 = CARTESIAN_POINT('Ctrl Pts',(0.251311008607692,-4.61103827729958,
1.4921099010432)) ;
#124906 = CARTESIAN_POINT('Ctrl Pts',(0.0515039259646006,-4.62213867077975,
1.5122458642563)) ;
#124907 = CARTESIAN_POINT('Ctrl Pts',(-0.336840442440354,-4.64371335791335,
1.47416320532842)) ;
#124908 = CARTESIAN_POINT('Ctrl Pts',(-0.521994293529454,-4.65399968297386,
1.41921195969608)) ;
#124909 = CARTESIAN_POINT('Ctrl Pts',(-0.86906205182113,-4.67328122510117,
1.23880073999231)) ;
#124910 = CARTESIAN_POINT('Ctrl Pts',(-1.0261453300444,-4.68332733239396,
1.11218525198224)) ;
#124911 = CARTESIAN_POINT('Ctrl Pts',(-1.27930114605304,-4.70502190906147,
0.807431522059718)) ;
#124912 = CARTESIAN_POINT('Ctrl Pts',(-1.37390227146845,-4.71603206906703,
0.633207628934896)) ;
#124913 = CARTESIAN_POINT('Ctrl Pts',(-1.48868992421953,-4.7369673532902,
0.264348599805235)) ;
#124914 = CARTESIAN_POINT('Ctrl Pts',(-1.51016244923422,-4.74615954009191,
0.0739551674221457)) ;
#124915 = CARTESIAN_POINT('Ctrl Pts',(-1.4802584543877,-4.76563987235946,
-0.313670855932048)) ;
#124916 = CARTESIAN_POINT('Ctrl Pts',(-1.42567798733999,-4.77645405423592,
-0.506927358017484)) ;
#124917 = CARTESIAN_POINT('Ctrl Pts',(-1.24653064568719,-4.79825605774633,
-0.856642725531518)) ;
#124918 = CARTESIAN_POINT('Ctrl Pts',(-1.12533143605636,-4.80903007223487,
-1.01060201517332)) ;
#124919 = CARTESIAN_POINT('Ctrl Pts',(-0.832618460366114,-4.82927455266081,
-1.26237772390985)) ;
#124920 = CARTESIAN_POINT('Ctrl Pts',(-0.664429502277172,-4.8380872498735,
-1.3584494122206)) ;
#124921 = CARTESIAN_POINT('Ctrl Pts',(-0.327003075299122,-4.85683316248339,
-1.47312623171267)) ;
#124922 = CARTESIAN_POINT('Ctrl Pts',(-0.163924989693454,-4.86589305612814,
-1.5)) ;
#124923 = CARTESIAN_POINT('Ctrl Pts',(-3.46944695195361E-15,-4.875,-1.5)) ;
#124924 = CARTESIAN_POINT('Ctrl Pts',(6.69603261727048E-15,-4.93750000136559,
-1.5)) ;
#124925 = CARTESIAN_POINT('Ctrl Pts',(-0.130815870223861,-4.93023245301982,
-1.5)) ;
#124926 = CARTESIAN_POINT('Ctrl Pts',(-0.261364789692205,-4.92297973527157,
-1.48288628464552)) ;
#124927 = CARTESIAN_POINT('Ctrl Pts',(-0.576211118206899,-4.90548827257631,
-1.39851230341137)) ;
#124928 = CARTESIAN_POINT('Ctrl Pts',(-0.752521316565833,-4.89639089959295,
-1.31208255717432)) ;
#124929 = CARTESIAN_POINT('Ctrl Pts',(-1.06108752372491,-4.87654051230214,
-1.07765078788927)) ;
#124930 = CARTESIAN_POINT('Ctrl Pts',(-1.19076365958232,-4.86594830373867,
-0.932364419078407)) ;
#124931 = CARTESIAN_POINT('Ctrl Pts',(-1.39186582163854,-4.84408722415966,
-0.594096800006323)) ;
#124932 = CARTESIAN_POINT('Ctrl Pts',(-1.45876423175756,-4.83302620311843,
-0.402821609972903)) ;
#124933 = CARTESIAN_POINT('Ctrl Pts',(-1.51197026583597,-4.81290441323619,
-0.0153165790875582)) ;
#124934 = CARTESIAN_POINT('Ctrl Pts',(-1.50170161487065,-4.80405079988388,
0.176595782800065)) ;
#124935 = CARTESIAN_POINT('Ctrl Pts',(-1.40874187252435,-4.78345686103223,
0.550962431560849)) ;
#124936 = CARTESIAN_POINT('Ctrl Pts',(-1.32515569478117,-4.77254848933251,
0.729430177481386)) ;
#124937 = CARTESIAN_POINT('Ctrl Pts',(-1.09222653520524,-4.75079140970906,
1.04716087248384)) ;
#124938 = CARTESIAN_POINT('Ctrl Pts',(-0.943996237490369,-4.74016045303707,
1.18254035526347)) ;
#124939 = CARTESIAN_POINT('Ctrl Pts',(-0.610717416559541,-4.72124925036386,
1.38318370463077)) ;
#124940 = CARTESIAN_POINT('Ctrl Pts',(-0.430545184352667,-4.71141917827407,
1.44943066767392)) ;
#124941 = CARTESIAN_POINT('Ctrl Pts',(-0.0478048447914621,-4.69015582607623,
1.51219616926508)) ;
#124942 = CARTESIAN_POINT('Ctrl Pts',(0.151544985468626,-4.67908083550622,
1.50534371639794)) ;
#124943 = CARTESIAN_POINT('Ctrl Pts',(0.534716566927561,-4.65779352542517,
1.41510953087164)) ;
#124944 = CARTESIAN_POINT('Ctrl Pts',(0.714899541237845,-4.64845088828263,
1.3331776759439)) ;
#124945 = CARTESIAN_POINT('Ctrl Pts',(1.03061126520019,-4.62878669835578,
1.10674141224403)) ;
#124946 = CARTESIAN_POINT('Ctrl Pts',(1.16393729767628,-4.61828964652437,
0.965540107763861)) ;
#124947 = CARTESIAN_POINT('Ctrl Pts',(1.37401459251156,-4.59650789075635,
0.634102998468438)) ;
#124948 = CARTESIAN_POINT('Ctrl Pts',(1.4462381198111,-4.58542438206486,0.445434869239173)) ;
#124949 = CARTESIAN_POINT('Ctrl Pts',(1.5109498623578,-4.56506613345469,0.0596579598670437)) ;
#124950 = CARTESIAN_POINT('Ctrl Pts',(1.50625743322842,-4.55626941762015,
-0.133112982053908)) ;
#124951 = CARTESIAN_POINT('Ctrl Pts',(1.42399202102172,-4.5358491728675,-0.510043841146295)) ;
#124952 = CARTESIAN_POINT('Ctrl Pts',(1.34585236191532,-4.52500410689068,
-0.690340351326157)) ;
#124953 = CARTESIAN_POINT('Ctrl Pts',(1.12272623748609,-4.5032148709766,-1.01439918725928)) ;
#124954 = CARTESIAN_POINT('Ctrl Pts',(0.978536665193565,-4.49248693785947,
-1.15412720151065)) ;
#124955 = CARTESIAN_POINT('Ctrl Pts',(0.651522387758622,-4.47328637770086,
-1.36440156914687)) ;
#124956 = CARTESIAN_POINT('Ctrl Pts',(0.473684284235579,-4.46381579493424,
-1.43587098432322)) ;
#124957 = CARTESIAN_POINT('Ctrl Pts',(0.192349898494841,-4.44818610683753,
-1.49075118620303)) ;
#124958 = CARTESIAN_POINT('Ctrl Pts',(0.0961708540385476,-4.44284282658996,
-1.5)) ;
#124959 = CARTESIAN_POINT('Ctrl Pts',(-3.27231699153423E-15,-4.43750000136559,
-1.5)) ;
#124960 = CARTESIAN_POINT('Origin',(0.,-6.,0.)) ;
#124961 = CARTESIAN_POINT('',(1.4076030946114E-15,-3.875,-1.5)) ;
#124962 = CARTESIAN_POINT('',(-1.51432176023703E-15,-3.93750000136559,-1.5)) ;
#124963 = CARTESIAN_POINT('',(-1.83697019872103E-16,-6.,-1.5)) ;
#124964 = CARTESIAN_POINT('Ctrl Pts',(2.60282034651221E-16,-3.875,-1.5)) ;
#124965 = CARTESIAN_POINT('Ctrl Pts',(0.0942423192034461,-3.88023568440019,
-1.5)) ;
#124966 = CARTESIAN_POINT('Ctrl Pts',(0.188500951634548,-3.8854722750908,
-1.4911184271582)) ;
#124967 = CARTESIAN_POINT('Ctrl Pts',(0.46816646802523,-3.90100924822362,
-1.43768292334024)) ;
#124968 = CARTESIAN_POINT('Ctrl Pts',(0.646300575696504,-3.91052180730236,
-1.36688571863216)) ;
#124969 = CARTESIAN_POINT('Ctrl Pts',(0.974128090628617,-3.92968536543257,
-1.15784994660216)) ;
#124970 = CARTESIAN_POINT('Ctrl Pts',(1.11884638083205,-3.94040132656015,
-1.01867602090901)) ;
#124971 = CARTESIAN_POINT('Ctrl Pts',(1.34324687246104,-3.96218750156777,
-0.695416560967739)) ;
#124972 = CARTESIAN_POINT('Ctrl Pts',(1.42209117090439,-3.97304122919988,
-0.5153468453742)) ;
#124973 = CARTESIAN_POINT('Ctrl Pts',(1.50573756977115,-3.99348413465912,
-0.138742305359965)) ;
#124974 = CARTESIAN_POINT('Ctrl Pts',(1.51115389055952,-4.00228408629164,
0.0539135437891495)) ;
#124975 = CARTESIAN_POINT('Ctrl Pts',(1.44793534887079,-4.02261199480333,
0.439921945973768)) ;
#124976 = CARTESIAN_POINT('Ctrl Pts',(1.3763982541349,-4.03369311341226,0.628936710295236)) ;
#124977 = CARTESIAN_POINT('Ctrl Pts',(1.16747431042337,-4.05548614561118,
0.961274083387404)) ;
#124978 = CARTESIAN_POINT('Ctrl Pts',(1.03461530485744,-4.0659959981852,1.10301108441868)) ;
#124979 = CARTESIAN_POINT('Ctrl Pts',(0.719830412477448,-4.08568464584996,
1.33049079911853)) ;
#124980 = CARTESIAN_POINT('Ctrl Pts',(0.540157294751756,-4.09499126140268,
1.41301220964346)) ;
#124981 = CARTESIAN_POINT('Ctrl Pts',(0.157480541459988,-4.11625108103,1.50474454179345)) ;
#124982 = CARTESIAN_POINT('Ctrl Pts',(-0.041920265696383,-4.1273289036498,
1.51238076232928)) ;
#124983 = CARTESIAN_POINT('Ctrl Pts',(-0.425030160643521,-4.14861278670241,
1.4510648450455)) ;
#124984 = CARTESIAN_POINT('Ctrl Pts',(-0.605504207978813,-4.15849392757573,
1.3854806133664)) ;
#124985 = CARTESIAN_POINT('Ctrl Pts',(-0.939569016813357,-4.17736812341821,
1.18606022685966)) ;
#124986 = CARTESIAN_POINT('Ctrl Pts',(-1.08830077291439,-4.18798613601125,
1.05123929884302)) ;
#124987 = CARTESIAN_POINT('Ctrl Pts',(-1.3224570684676,-4.20973777009996,
0.734330274441642)) ;
#124988 = CARTESIAN_POINT('Ctrl Pts',(-1.40672934906018,-4.2206535178302,
0.556105342270486)) ;
#124989 = CARTESIAN_POINT('Ctrl Pts',(-1.50103999144478,-4.2412691022799,
0.182068740703184)) ;
#124990 = CARTESIAN_POINT('Ctrl Pts',(-1.51200845611127,-4.25013507314821,
-0.00974052803380514)) ;
#124991 = CARTESIAN_POINT('Ctrl Pts',(-1.46024638357755,-4.27022676020464,
-0.397453555020732)) ;
#124992 = CARTESIAN_POINT('Ctrl Pts',(-1.39402190482696,-4.28128429938543,
-0.589045470400813)) ;
#124993 = CARTESIAN_POINT('Ctrl Pts',(-1.19406008533681,-4.30315410409528,
-0.928152814999461)) ;
#124994 = CARTESIAN_POINT('Ctrl Pts',(-1.06485019338996,-4.31375768718844,
-1.07394478501753)) ;
#124995 = CARTESIAN_POINT('Ctrl Pts',(-0.757181391102665,-4.3336310782375,
-1.3093727953836)) ;
#124996 = CARTESIAN_POINT('Ctrl Pts',(-0.581348167225834,-4.34270287959856,
-1.39636008114215)) ;
#124997 = CARTESIAN_POINT('Ctrl Pts',(-0.265154173659441,-4.36026921257447,
-1.48238373539969)) ;
#124998 = CARTESIAN_POINT('Ctrl Pts',(-0.132722487609192,-4.36762652846615,
-1.5)) ;
#124999 = CARTESIAN_POINT('Ctrl Pts',(-3.01841884819964E-15,-4.375,-1.5)) ;
#125000 = CARTESIAN_POINT('Ctrl Pts',(-3.97251675998689E-15,-4.43750000136559,
-1.5)) ;
#125001 = CARTESIAN_POINT('Ctrl Pts',(-0.0998335372168724,-4.43195369374243,
-1.5)) ;
#125002 = CARTESIAN_POINT('Ctrl Pts',(-0.199658248269081,-4.42640787646175,
-1.49003323466658)) ;
#125003 = CARTESIAN_POINT('Ctrl Pts',(-0.49191789941691,-4.41017122917576,
-1.43079611298183)) ;
#125004 = CARTESIAN_POINT('Ctrl Pts',(-0.676133757207218,-4.40050582845571,
-1.35350736953389)) ;
#125005 = CARTESIAN_POINT('Ctrl Pts',(-0.999037892355418,-4.38103459961541,
-1.13523426723781)) ;
#125006 = CARTESIAN_POINT('Ctrl Pts',(-1.1359209996514,-4.37064148043957,
-0.998246840542587)) ;
#125007 = CARTESIAN_POINT('Ctrl Pts',(-1.35483349461492,-4.34895721561397,
-0.673937047606172)) ;
#125008 = CARTESIAN_POINT('Ctrl Pts',(-1.43233728352691,-4.33786052119468,
-0.488043418634293)) ;
#125009 = CARTESIAN_POINT('Ctrl Pts',(-1.50864480205144,-4.31727026199915,
-0.104139084183682)) ;
#125010 = CARTESIAN_POINT('Ctrl Pts',(-1.50958033404375,-4.30845717980767,
0.0895596765701229)) ;
#125011 = CARTESIAN_POINT('Ctrl Pts',(-1.43797083262724,-4.28821401126395,
0.468962268737551)) ;
#125012 = CARTESIAN_POINT('Ctrl Pts',(-1.36527778751035,-4.27744055255317,
0.650915053894818)) ;
#125013 = CARTESIAN_POINT('Ctrl Pts',(-1.15206224529449,-4.25563852472727,
0.980961642031033)) ;
#125014 = CARTESIAN_POINT('Ctrl Pts',(-1.0120182649773,-4.24482374142398,
1.12488826214615)) ;
#125015 = CARTESIAN_POINT('Ctrl Pts',(-0.691322923457565,-4.22534136580834,
1.34466829341293)) ;
#125016 = CARTESIAN_POINT('Ctrl Pts',(-0.515717164638227,-4.2161509549566,
1.42130708291937)) ;
#125017 = CARTESIAN_POINT('Ctrl Pts',(-0.138904002513243,-4.1952168903941,
1.5064074405763)) ;
#125018 = CARTESIAN_POINT('Ctrl Pts',(0.0592733838908032,-4.18420703559388,
1.511635564)) ;
#125019 = CARTESIAN_POINT('Ctrl Pts',(0.449801105031135,-4.16251105108608,
1.44485818892842)) ;
#125020 = CARTESIAN_POINT('Ctrl Pts',(0.638024314217126,-4.1524619170851,
1.37216141104746)) ;
#125021 = CARTESIAN_POINT('Ctrl Pts',(0.967848797712361,-4.13318177246089,
1.16185538458189)) ;
#125022 = CARTESIAN_POINT('Ctrl Pts',(1.10803832240908,-4.12289624965393,
1.02901326739432)) ;
#125023 = CARTESIAN_POINT('Ctrl Pts',(1.3352501696126,-4.10132241697745,0.711790396824513)) ;
#125024 = CARTESIAN_POINT('Ctrl Pts',(1.41775118270551,-4.09022202847339,
0.528705136468632)) ;
#125025 = CARTESIAN_POINT('Ctrl Pts',(1.50523004438318,-4.06941436417902,
0.146731899870329)) ;
#125026 = CARTESIAN_POINT('Ctrl Pts',(1.51160504407379,-4.06051734841374,
-0.0479088430764911)) ;
#125027 = CARTESIAN_POINT('Ctrl Pts',(1.4501496273714,-4.04044638316897,-0.429594720430866)) ;
#125028 = CARTESIAN_POINT('Ctrl Pts',(1.38265615327964,-4.02974886441085,
-0.612971097043189)) ;
#125029 = CARTESIAN_POINT('Ctrl Pts',(1.17899944361955,-4.00795234313619,
-0.948422028210402)) ;
#125030 = CARTESIAN_POINT('Ctrl Pts',(1.04300877637827,-3.99706394374256,
-1.09621891142586)) ;
#125031 = CARTESIAN_POINT('Ctrl Pts',(0.728409026090832,-3.97731925686015,
-1.3249702712289)) ;
#125032 = CARTESIAN_POINT('Ctrl Pts',(0.554849708907109,-3.96832498519377,
-1.40651277173017)) ;
#125033 = CARTESIAN_POINT('Ctrl Pts',(0.249253928268807,-3.95134744182497,
-1.4844418180471)) ;
#125034 = CARTESIAN_POINT('Ctrl Pts',(0.124729698084853,-3.94442942903697,
-1.5)) ;
#125035 = CARTESIAN_POINT('Ctrl Pts',(-3.40005801291454E-15,-3.93750000136559,
-1.5)) ;
#125036 = CARTESIAN_POINT('Origin',(0.,-6.,0.)) ;
#125037 = CARTESIAN_POINT('',(3.08703225979145E-15,-3.37499999999999,-1.5)) ;
#125038 = CARTESIAN_POINT('',(-1.32350217787958E-15,-3.43750000136559,-1.5)) ;
#125039 = CARTESIAN_POINT('',(-1.83697019872103E-16,-6.,-1.5)) ;
#125040 = CARTESIAN_POINT('Ctrl Pts',(1.20736753927986E-14,-3.37499999999999,
-1.5)) ;
#125041 = CARTESIAN_POINT('Ctrl Pts',(0.123025767620368,-3.38183476486779,
-1.5)) ;
#125042 = CARTESIAN_POINT('Ctrl Pts',(0.245864401420877,-3.38865913341226,
-1.48486403806509)) ;
#125043 = CARTESIAN_POINT('Ctrl Pts',(0.550039486660369,-3.4055577492589,
-1.40839677588521)) ;
#125044 = CARTESIAN_POINT('Ctrl Pts',(0.723848898809359,-3.41457268167444,
-1.32746242112634)) ;
#125045 = CARTESIAN_POINT('Ctrl Pts',(1.03920974331056,-3.43428512761029,
-1.0998205947628)) ;
#125046 = CARTESIAN_POINT('Ctrl Pts',(1.17570902074221,-3.44516487040949,
-0.952497281714251)) ;
#125047 = CARTESIAN_POINT('Ctrl Pts',(1.38055843843326,-3.46696300706962,
-0.61770138569343)) ;
#125048 = CARTESIAN_POINT('Ctrl Pts',(1.44869790488294,-3.47767035854733,
-0.434493603703968)) ;
#125049 = CARTESIAN_POINT('Ctrl Pts',(1.5114145116643,-3.49776290479369,-0.053087322086436)) ;
#125050 = CARTESIAN_POINT('Ctrl Pts',(1.50571947322053,-3.50664582679239,
0.141433055356179)) ;
#125051 = CARTESIAN_POINT('Ctrl Pts',(1.41963444045046,-3.5274267144909,0.523654478355581)) ;
#125052 = CARTESIAN_POINT('Ctrl Pts',(1.33775190161653,-3.53852712433378,
0.707097258510357)) ;
#125053 = CARTESIAN_POINT('Ctrl Pts',(1.11156381318303,-3.56011561436665,
1.02521584391335)) ;
#125054 = CARTESIAN_POINT('Ctrl Pts',(0.971780230466467,-3.57041495677473,
1.15857956682781)) ;
#125055 = CARTESIAN_POINT('Ctrl Pts',(0.642818743148598,-3.58971922767343,
1.3698852995673)) ;
#125056 = CARTESIAN_POINT('Ctrl Pts',(0.455102019190075,-3.59971655448944,
1.44316189862217)) ;
#125057 = CARTESIAN_POINT('Ctrl Pts',(0.0650132634678198,-3.62138815202956,
1.51140914512229)) ;
#125058 = CARTESIAN_POINT('Ctrl Pts',(-0.133257745415366,-3.63240320807863,
1.50692689389207)) ;
#125059 = CARTESIAN_POINT('Ctrl Pts',(-0.510449552502788,-3.65335830847237,
1.42320674145113)) ;
#125060 = CARTESIAN_POINT('Ctrl Pts',(-0.686332998975074,-3.66257994297825,
1.34722090227418)) ;
#125061 = CARTESIAN_POINT('Ctrl Pts',(-1.0078327000363,-3.68202700523824,
1.12863924251933)) ;
#125062 = CARTESIAN_POINT('Ctrl Pts',(-1.14840782613823,-3.69283133527332,
0.985236546665589)) ;
#125063 = CARTESIAN_POINT('Ctrl Pts',(-1.36288531483847,-3.71463279978794,
0.655930251877055)) ;
#125064 = CARTESIAN_POINT('Ctrl Pts',(-1.43626868098597,-3.72541578717667,
0.474177973900462)) ;
#125065 = CARTESIAN_POINT('Ctrl Pts',(-1.50922719478472,-3.74568156538545,
0.0950843013314755)) ;
#125066 = CARTESIAN_POINT('Ctrl Pts',(-1.50900853204741,-3.75448856214089,
-0.0984940905742062)) ;
#125067 = CARTESIAN_POINT('Ctrl Pts',(-1.4341764099549,-3.77504963836379,
-0.482643688856358)) ;
#125068 = CARTESIAN_POINT('Ctrl Pts',(-1.3573393155221,-3.78614518417671,
-0.66889836072996)) ;
#125069 = CARTESIAN_POINT('Ctrl Pts',(-1.13953871385644,-3.80784282577407,
-0.994128136541216)) ;
#125070 = CARTESIAN_POINT('Ctrl Pts',(-1.00310120634842,-3.81824961031078,
-1.13165685958585)) ;
#125071 = CARTESIAN_POINT('Ctrl Pts',(-0.681111648821587,-3.83774569029164,
-1.35097451477486)) ;
#125072 = CARTESIAN_POINT('Ctrl Pts',(-0.497416098316471,-3.84736577231575,
-1.42886065532683)) ;
#125073 = CARTESIAN_POINT('Ctrl Pts',(-0.203658757535048,-3.86368562458138,
-1.48962877654428)) ;
#125074 = CARTESIAN_POINT('Ctrl Pts',(-0.101838903337983,-3.86934228314789,
-1.5)) ;
#125075 = CARTESIAN_POINT('Ctrl Pts',(-6.93889390390723E-17,-3.875,-1.5)) ;
#125076 = CARTESIAN_POINT('Ctrl Pts',(-3.27231699153424E-15,-3.93750000136559,
-1.5)) ;
#125077 = CARTESIAN_POINT('Ctrl Pts',(-0.070231194483588,-3.93359826833872,
-1.5)) ;
#125078 = CARTESIAN_POINT('Ctrl Pts',(-0.140527531456689,-3.92969291628466,
-1.49506770113817)) ;
#125079 = CARTESIAN_POINT('Ctrl Pts',(-0.407265219101565,-3.91487415585995,
-1.45728574992466)) ;
#125080 = CARTESIAN_POINT('Ctrl Pts',(-0.596595698355777,-3.9044963629537,
-1.3905277518438)) ;
#125081 = CARTESIAN_POINT('Ctrl Pts',(-0.931327375415623,-3.88560991898453,
-1.19123780935363)) ;
#125082 = CARTESIAN_POINT('Ctrl Pts',(-1.07514580432589,-3.87545613444443,
-1.06322896944864)) ;
#125083 = CARTESIAN_POINT('Ctrl Pts',(-1.31157428121161,-3.85402811525593,
-0.754357998942086)) ;
#125084 = CARTESIAN_POINT('Ctrl Pts',(-1.39967070126838,-3.8429343023808,
-0.574639920183848)) ;
#125085 = CARTESIAN_POINT('Ctrl Pts',(-1.4999169296833,-3.82188614237405,
-0.195039316694249)) ;
#125086 = CARTESIAN_POINT('Ctrl Pts',(-1.5125422847797,-3.81281288352773,
0.000738157874615904)) ;
#125087 = CARTESIAN_POINT('Ctrl Pts',(-1.46256638272007,-3.79294082983558,
0.384917437113829)) ;
#125088 = CARTESIAN_POINT('Ctrl Pts',(-1.40095083835048,-3.78233790561831,
0.569721327423226)) ;
#125089 = CARTESIAN_POINT('Ctrl Pts',(-1.2073316710414,-3.76046860146178,
0.912480200160393)) ;
#125090 = CARTESIAN_POINT('Ctrl Pts',(-1.07455600022974,-3.749410855499,1.06565306477226)) ;
#125091 = CARTESIAN_POINT('Ctrl Pts',(-0.764720191675931,-3.72931741291523,
1.30440363874785)) ;
#125092 = CARTESIAN_POINT('Ctrl Pts',(-0.593139462781269,-3.72045219374233,
1.39084758505053)) ;
#125093 = CARTESIAN_POINT('Ctrl Pts',(-0.222081613845145,-3.69983786880143,
1.49626828321634)) ;
#125094 = CARTESIAN_POINT('Ctrl Pts',(-0.0256058221544604,-3.68892254704084,
1.51244053751281)) ;
#125095 = CARTESIAN_POINT('Ctrl Pts',(0.365929456853119,-3.66717058709597,
1.46819562366311)) ;
#125096 = CARTESIAN_POINT('Ctrl Pts',(0.557067337200572,-3.65655181596556,
1.40684216814683)) ;
#125097 = CARTESIAN_POINT('Ctrl Pts',(0.896841729089794,-3.6376754608606,
1.21731903993412)) ;
#125098 = CARTESIAN_POINT('Ctrl Pts',(1.04390101088138,-3.62779733095075,
1.09385063513606)) ;
#125099 = CARTESIAN_POINT('Ctrl Pts',(1.28861960359674,-3.60651464312407,
0.792786620866651)) ;
#125100 = CARTESIAN_POINT('Ctrl Pts',(1.38174500714516,-3.5954369811341,0.61630771692526)) ;
#125101 = CARTESIAN_POINT('Ctrl Pts',(1.4937309636147,-3.5741755542344,0.239052379458141)) ;
#125102 = CARTESIAN_POINT('Ctrl Pts',(1.51214651100827,-3.56486686984892,
0.0421816462151671)) ;
#125103 = CARTESIAN_POINT('Ctrl Pts',(1.47261553235169,-3.545179647906,-0.344186356596442)) ;
#125104 = CARTESIAN_POINT('Ctrl Pts',(1.41633790577741,-3.53467053911417,
-0.530122178180987)) ;
#125105 = CARTESIAN_POINT('Ctrl Pts',(1.23306641992855,-3.51287815733459,
-0.877256486013357)) ;
#125106 = CARTESIAN_POINT('Ctrl Pts',(1.10518091116016,-3.50179689482562,
-1.03374146923098)) ;
#125107 = CARTESIAN_POINT('Ctrl Pts',(0.802552349766301,-3.48146721179632,
-1.28156331474823)) ;
#125108 = CARTESIAN_POINT('Ctrl Pts',(0.633014668514489,-3.47266748294973,
-1.37324051716546)) ;
#125109 = CARTESIAN_POINT('Ctrl Pts',(0.304714521415647,-3.45442858588868,
-1.47668899033705)) ;
#125110 = CARTESIAN_POINT('Ctrl Pts',(0.152673453390108,-3.44598185988726,
-1.5)) ;
#125111 = CARTESIAN_POINT('Ctrl Pts',(4.5102810375397E-16,-3.43750000136559,
-1.5)) ;
#125112 = CARTESIAN_POINT('Origin',(0.,-6.,0.)) ;
#125113 = CARTESIAN_POINT('',(-3.50058014023048E-15,-2.875,-1.5)) ;
#125114 = CARTESIAN_POINT('',(-7.16348961287702E-16,-2.93750000136559,-1.5)) ;
#125115 = CARTESIAN_POINT('',(-1.83697019872103E-16,-6.,-1.5)) ;
#125116 = CARTESIAN_POINT('Ctrl Pts',(-1.3912482277334E-14,-2.875,-1.5)) ;
#125117 = CARTESIAN_POINT('Ctrl Pts',(0.14927646169187,-2.88329313676066,
-1.5)) ;
#125118 = CARTESIAN_POINT('Ctrl Pts',(0.298008422113359,-2.89155602345074,
-1.47771475584672)) ;
#125119 = CARTESIAN_POINT('Ctrl Pts',(0.625668423501798,-2.90975935686121,
-1.37687521093521)) ;
#125120 = CARTESIAN_POINT('Ctrl Pts',(0.797408078633453,-2.91865598955823,
-1.28506187278717)) ;
#125121 = CARTESIAN_POINT('Ctrl Pts',(1.09720715239368,-2.93872752168036,
-1.04097198767013)) ;
#125122 = CARTESIAN_POINT('Ctrl Pts',(1.2222567372371,-2.94942529983834,-0.890820255568953)) ;
#125123 = CARTESIAN_POINT('Ctrl Pts',(1.41090692411199,-2.97122186685069,
-0.546704353792156)) ;
#125124 = CARTESIAN_POINT('Ctrl Pts',(1.47089002802769,-2.98211004090072,
-0.35502916710887)) ;
#125125 = CARTESIAN_POINT('Ctrl Pts',(1.51165945654184,-3.00185388317589,
0.0318006478503855)) ;
#125126 = CARTESIAN_POINT('Ctrl Pts',(1.49548058650827,-3.01084868359775,
0.222876369642636)) ;
#125127 = CARTESIAN_POINT('Ctrl Pts',(1.39105652263104,-3.03162416325971,
0.594397344166714)) ;
#125128 = CARTESIAN_POINT('Ctrl Pts',(1.3016646900582,-3.04259064418931,0.770720971371029)) ;
#125129 = CARTESIAN_POINT('Ctrl Pts',(1.0583137636934,-3.06430000807502,1.08144290352728)) ;
#125130 = CARTESIAN_POINT('Ctrl Pts',(0.905822158922318,-3.07467654672654,
1.21201493367489)) ;
#125131 = CARTESIAN_POINT('Ctrl Pts',(0.565846680809043,-3.09356407328839,
1.40222551737039)) ;
#125132 = CARTESIAN_POINT('Ctrl Pts',(0.383071111602179,-3.10371827157766,
1.46275477782419)) ;
#125133 = CARTESIAN_POINT('Ctrl Pts',(-0.0026417638336251,-3.12514676465742,
1.5130356496647)) ;
#125134 = CARTESIAN_POINT('Ctrl Pts',(-0.202331067414456,-3.13624061485636,
1.49945057545605)) ;
#125135 = CARTESIAN_POINT('Ctrl Pts',(-0.581185047696406,-3.15728805820535,
1.39642875645191)) ;
#125136 = CARTESIAN_POINT('Ctrl Pts',(-0.757033408993981,-3.16636065503082,
1.30945917866451)) ;
#125137 = CARTESIAN_POINT('Ctrl Pts',(-1.06473075224911,-3.18623331576859,
1.07406282566911)) ;
#125138 = CARTESIAN_POINT('Ctrl Pts',(-1.19395549893989,-3.19683653909601,
0.928286909631763)) ;
#125139 = CARTESIAN_POINT('Ctrl Pts',(-1.39395362952719,-3.21870607056373,
0.589206208486066)) ;
#125140 = CARTESIAN_POINT('Ctrl Pts',(-1.46019955879773,-3.22976372273207,
0.397624329167115)) ;
#125141 = CARTESIAN_POINT('Ctrl Pts',(-1.51250754431013,-3.25005028037023,
0.00617617620382795)) ;
#125142 = CARTESIAN_POINT('Ctrl Pts',(-1.50060837449239,-3.25909881964487,
-0.189466660143033)) ;
#125143 = CARTESIAN_POINT('Ctrl Pts',(-1.40184088383919,-3.28011957356614,
-0.569351388487747)) ;
#125144 = CARTESIAN_POINT('Ctrl Pts',(-1.31438594418839,-3.29121473591674,
-0.749467874451868)) ;
#125145 = CARTESIAN_POINT('Ctrl Pts',(-1.07900985504578,-3.31266070438634,
-1.05931951010697)) ;
#125146 = CARTESIAN_POINT('Ctrl Pts',(-0.935603378011179,-3.32283021821386,
-1.18789311763799)) ;
#125147 = CARTESIAN_POINT('Ctrl Pts',(-0.60151270711808,-3.34175786763303,
-1.38840958440627)) ;
#125148 = CARTESIAN_POINT('Ctrl Pts',(-0.41241160302782,-3.35208824427622,
-1.45583849950391)) ;
#125149 = CARTESIAN_POINT('Ctrl Pts',(-0.144049011394607,-3.36699727714473,
-1.49481720919358)) ;
#125150 = CARTESIAN_POINT('Ctrl Pts',(-0.0719924648342288,-3.37100041862031,
-1.5)) ;
#125151 = CARTESIAN_POINT('Ctrl Pts',(1.32192589950948E-14,-3.37499999999999,
-1.5)) ;
#125152 = CARTESIAN_POINT('Ctrl Pts',(0.,-3.43750000136559,-1.5)) ;
#125153 = CARTESIAN_POINT('Ctrl Pts',(-0.0414351247760593,-3.43519804998914,
-1.5)) ;
#125154 = CARTESIAN_POINT('Ctrl Pts',(-0.0829168287552058,-3.43289351087919,
-1.49828316721394)) ;
#125155 = CARTESIAN_POINT('Ctrl Pts',(-0.322446416719623,-3.41958631154783,
-1.47835938700884)) ;
#125156 = CARTESIAN_POINT('Ctrl Pts',(-0.515346390198614,-3.40886964635455,
-1.4226595609534)) ;
#125157 = CARTESIAN_POINT('Ctrl Pts',(-0.860329408803675,-3.38970392309872,
-1.24334782196046)) ;
#125158 = CARTESIAN_POINT('Ctrl Pts',(-1.01073400139118,-3.38019385287707,
-1.12451242613287)) ;
#125159 = CARTESIAN_POINT('Ctrl Pts',(-1.26379037511403,-3.35907435841513,
-0.831654142362913)) ;
#125160 = CARTESIAN_POINT('Ctrl Pts',(-1.36198013234628,-3.34802340642958,
-0.658654301400892)) ;
#125161 = CARTESIAN_POINT('Ctrl Pts',(-1.48607548799382,-3.32655030240577,
-0.283990702403635)) ;
#125162 = CARTESIAN_POINT('Ctrl Pts',(-1.51051733580799,-3.31692760115312,
-0.0859537467911005)) ;
#125163 = CARTESIAN_POINT('Ctrl Pts',(-1.4816571571331,-3.29743297384205,
0.302572041010721)) ;
#125164 = CARTESIAN_POINT('Ctrl Pts',(-1.43081303000291,-3.28702698592376,
0.489501567854581)) ;
#125165 = CARTESIAN_POINT('Ctrl Pts',(-1.25813524563156,-3.26533011978006,
0.840766896875701)) ;
#125166 = CARTESIAN_POINT('Ctrl Pts',(-1.13529030741348,-3.25423450246132,
1.00046041397559)) ;
#125167 = CARTESIAN_POINT('Ctrl Pts',(-0.840078635521338,-3.23367171450641,
1.25740939753883)) ;
#125168 = CARTESIAN_POINT('Ctrl Pts',(-0.672559065071132,-3.22486439386955,
1.35442781593296)) ;
#125169 = CARTESIAN_POINT('Ctrl Pts',(-0.30779887117551,-3.20459993865312,
1.48086824581934)) ;
#125170 = CARTESIAN_POINT('Ctrl Pts',(-0.113715081646265,-3.1938175059015,
1.50823346071337)) ;
#125171 = CARTESIAN_POINT('Ctrl Pts',(0.278712025227951,-3.17201599996404,
1.48722939991194)) ;
#125172 = CARTESIAN_POINT('Ctrl Pts',(0.473201068701714,-3.16121105310438,
1.43723140636941)) ;
#125173 = CARTESIAN_POINT('Ctrl Pts',(0.82328548612006,-3.14176191880336,
1.26817124058548)) ;
#125174 = CARTESIAN_POINT('Ctrl Pts',(0.977057863522894,-3.13254214748269,
1.15387788568608)) ;
#125175 = CARTESIAN_POINT('Ctrl Pts',(1.23821659195876,-3.11158827889642,
0.869139967771304)) ;
#125176 = CARTESIAN_POINT('Ctrl Pts',(1.34126903660841,-3.10057352373717,
0.699699937605282)) ;
#125177 = CARTESIAN_POINT('Ctrl Pts',(1.47729709806211,-3.07890049196363,
0.327770269273075)) ;
#125178 = CARTESIAN_POINT('Ctrl Pts',(1.50774033687445,-3.06890015468157,
0.128555803056094)) ;
#125179 = CARTESIAN_POINT('Ctrl Pts',(1.48930107103342,-3.04959729792276,
-0.262000625496734)) ;
#125180 = CARTESIAN_POINT('Ctrl Pts',(1.44373492322925,-3.03929876374884,
-0.449744010988673)) ;
#125181 = CARTESIAN_POINT('Ctrl Pts',(1.28305772881047,-3.0179308183088,-0.80110139540444)) ;
#125182 = CARTESIAN_POINT('Ctrl Pts',(1.16819602396499,-3.00705194575476,
-0.96089907910427)) ;
#125183 = CARTESIAN_POINT('Ctrl Pts',(0.886799510020267,-2.98654140483531,
-1.22473831358787)) ;
#125184 = CARTESIAN_POINT('Ctrl Pts',(0.724038965074748,-2.97772438831419,
-1.32746429229688)) ;
#125185 = CARTESIAN_POINT('Ctrl Pts',(0.372142347920373,-2.95817457625006,
-1.46509728046957)) ;
#125186 = CARTESIAN_POINT('Ctrl Pts',(0.186817297896326,-2.94787874013761,
-1.5)) ;
#125187 = CARTESIAN_POINT('Ctrl Pts',(-4.16333634234434E-16,-2.93750000136559,
-1.5)) ;
#125188 = CARTESIAN_POINT('Origin',(0.,-6.,0.)) ;
#125189 = CARTESIAN_POINT('',(1.05306898420864E-15,-2.37499999999999,-1.5)) ;
#125190 = CARTESIAN_POINT('',(-2.24595708969792E-17,-2.43750000136559,-1.5)) ;
#125191 = CARTESIAN_POINT('',(-1.83697019872103E-16,-6.,-1.5)) ;
#125192 = CARTESIAN_POINT('Ctrl Pts',(1.83880688453542E-15,-2.37499999999999,
-1.5)) ;
#125193 = CARTESIAN_POINT('Ctrl Pts',(0.179045843136507,-2.38494699128535,
-1.5)) ;
#125194 = CARTESIAN_POINT('Ctrl Pts',(0.356844193855229,-2.3948246774364,
-1.46794016277328)) ;
#125195 = CARTESIAN_POINT('Ctrl Pts',(0.703943741687518,-2.4141079856493,
-1.33827904569682)) ;
#125196 = CARTESIAN_POINT('Ctrl Pts',(0.868529861133173,-2.42290477109696,
-1.23781478711461)) ;
#125197 = CARTESIAN_POINT('Ctrl Pts',(1.15380320041922,-2.44332561450054,
-0.978078166643146)) ;
#125198 = CARTESIAN_POINT('Ctrl Pts',(1.27086028245954,-2.45417091080648,
-0.820245853769252)) ;
#125199 = CARTESIAN_POINT('Ctrl Pts',(1.43990537762083,-2.47596007012258,
-0.464964913089586)) ;
#125200 = CARTESIAN_POINT('Ctrl Pts',(1.48879898154894,-2.48668768952965,
-0.270224266191242)) ;
#125201 = CARTESIAN_POINT('Ctrl Pts',(1.50735577308132,-2.50588727499066,
0.118117855255059)) ;
#125202 = CARTESIAN_POINT('Ctrl Pts',(1.48031180593145,-2.51535894825184,
0.307862760530866)) ;
#125203 = CARTESIAN_POINT('Ctrl Pts',(1.3545391434805,-2.53645895512261,0.673803287290782)) ;
#125204 = CARTESIAN_POINT('Ctrl Pts',(1.25446628635798,-2.5475061069721,0.845636935679458)) ;
#125205 = CARTESIAN_POINT('Ctrl Pts',(0.99303044534197,-2.56900349033031,
1.14151160496747)) ;
#125206 = CARTESIAN_POINT('Ctrl Pts',(0.833981721521096,-2.57866768213772,
1.26238308549651)) ;
#125207 = CARTESIAN_POINT('Ctrl Pts',(0.483487806892448,-2.59813956628375,
1.43285511112529)) ;
#125208 = CARTESIAN_POINT('Ctrl Pts',(0.296405157239994,-2.60853304682,1.4828883767912)) ;
#125209 = CARTESIAN_POINT('Ctrl Pts',(-0.0939180130779636,-2.63021766739322,
1.51027982196163)) ;
#125210 = CARTESIAN_POINT('Ctrl Pts',(-0.29365800396888,-2.64131433355382,
1.48443330920183)) ;
#125211 = CARTESIAN_POINT('Ctrl Pts',(-0.664268866896788,-2.66190382593871,
1.35852851474607)) ;
#125212 = CARTESIAN_POINT('Ctrl Pts',(-0.832472488380221,-2.67071673287117,
1.26247457376114)) ;
#125213 = CARTESIAN_POINT('Ctrl Pts',(-1.12521525458455,-2.69096049698547,
1.01073095284365)) ;
#125214 = CARTESIAN_POINT('Ctrl Pts',(-1.24643084741289,-2.70173420805323,
0.856787428527987)) ;
#125215 = CARTESIAN_POINT('Ctrl Pts',(-1.42561838823675,-2.72353622496772,
0.50709499141758)) ;
#125216 = CARTESIAN_POINT('Ctrl Pts',(-1.48022159937158,-2.73435073531192,
0.313844793563222)) ;
#125217 = CARTESIAN_POINT('Ctrl Pts',(-1.51017114759058,-2.75383218337074,
-0.0737781208251271)) ;
#125218 = CARTESIAN_POINT('Ctrl Pts',(-1.48872089276062,-2.76302339992767,
-0.264174288743228)) ;
#125219 = CARTESIAN_POINT('Ctrl Pts',(-1.37397700269541,-2.78395801818002,
-0.633044742327755)) ;
#125220 = CARTESIAN_POINT('Ctrl Pts',(-1.27939778464178,-2.7949680115897,
-0.807277821043497)) ;
#125221 = CARTESIAN_POINT('Ctrl Pts',(-1.02627530537409,-2.8166633570728,
-1.11206677747424)) ;
#125222 = CARTESIAN_POINT('Ctrl Pts',(-0.869199899582457,-2.82671111668986,
-1.23870531056205)) ;
#125223 = CARTESIAN_POINT('Ctrl Pts',(-0.522145877061563,-2.8459918957188,
-1.41915592803456)) ;
#125224 = CARTESIAN_POINT('Ctrl Pts',(-0.336999910677903,-2.85627778274012,
-1.4741264970106)) ;
#125225 = CARTESIAN_POINT('Ctrl Pts',(-0.0977631271775219,-2.8695687151568,
-1.49761350529533)) ;
#125226 = CARTESIAN_POINT('Ctrl Pts',(-0.048852405561043,-2.87228597746883,
-1.5)) ;
#125227 = CARTESIAN_POINT('Ctrl Pts',(-1.2605732511172E-14,-2.875,-1.5)) ;
#125228 = CARTESIAN_POINT('Ctrl Pts',(0.,-2.93750000136559,-1.5)) ;
#125229 = CARTESIAN_POINT('Ctrl Pts',(-0.0132523212698805,-2.93676376129504,
-1.5)) ;
#125230 = CARTESIAN_POINT('Ctrl Pts',(-0.026512151688511,-2.93602710404956,
-1.49982437670836)) ;
#125231 = CARTESIAN_POINT('Ctrl Pts',(-0.232382246772646,-2.92458987654489,
-1.49436332168044)) ;
#125232 = CARTESIAN_POINT('Ctrl Pts',(-0.42223498468532,-2.91404250221641,
-1.45219084965621)) ;
#125233 = CARTESIAN_POINT('Ctrl Pts',(-0.77793923996282,-2.89428115470099,
-1.29727969127008)) ;
#125234 = CARTESIAN_POINT('Ctrl Pts',(-0.94000408053958,-2.8850748885874,
-1.18512690941558)) ;
#125235 = CARTESIAN_POINT('Ctrl Pts',(-1.21389970388962,-2.8638978065848,
-0.903103237471781)) ;
#125236 = CARTESIAN_POINT('Ctrl Pts',(-1.32230634146135,-2.85281253025025,
-0.735288696927187)) ;
#125237 = CARTESIAN_POINT('Ctrl Pts',(-1.46505521612337,-2.83146796669241,
-0.374066375569203)) ;
#125238 = CARTESIAN_POINT('Ctrl Pts',(-1.50065473529158,-2.82142771299859,
-0.185180990127344)) ;
#125239 = CARTESIAN_POINT('Ctrl Pts',(-1.4992977711023,-2.80266394994054,
0.204033057725338)) ;
#125240 = CARTESIAN_POINT('Ctrl Pts',(-1.45908938348214,-2.79208526701016,
0.400692530060151)) ;
#125241 = CARTESIAN_POINT('Ctrl Pts',(-1.305666754252,-2.77035162712593,0.763839155929079)) ;
#125242 = CARTESIAN_POINT('Ctrl Pts',(-1.19510987201921,-2.75941481549434,
0.927326471235875)) ;
#125243 = CARTESIAN_POINT('Ctrl Pts',(-0.921200286387028,-2.73873538151063,
1.19899866221631)) ;
#125244 = CARTESIAN_POINT('Ctrl Pts',(-0.76186745976206,-2.72982597135238,
1.30604686821552)) ;
#125245 = CARTESIAN_POINT('Ctrl Pts',(-0.401830477127252,-2.70982391676155,
1.45907902690513)) ;
#125246 = CARTESIAN_POINT('Ctrl Pts',(-0.202995714400276,-2.6987775410545,
1.49971794259337)) ;
#125247 = CARTESIAN_POINT('Ctrl Pts',(0.191096578722603,-2.67688352476989,
1.50026836417804)) ;
#125248 = CARTESIAN_POINT('Ctrl Pts',(0.382553545209961,-2.6662470266317,
1.46321266530721)) ;
#125249 = CARTESIAN_POINT('Ctrl Pts',(0.741491518165052,-2.6463060281342,
1.31824794173905)) ;
#125250 = CARTESIAN_POINT('Ctrl Pts',(0.905463088608233,-2.63730316853214,
1.21149858735916)) ;
#125251 = CARTESIAN_POINT('Ctrl Pts',(1.18701578749506,-2.61633707960545,
0.938281138768189)) ;
#125252 = CARTESIAN_POINT('Ctrl Pts',(1.30059020178559,-2.60523969723543,
0.773198596281036)) ;
#125253 = CARTESIAN_POINT('Ctrl Pts',(1.45396456412132,-2.58375897476809,
0.415280893301883)) ;
#125254 = CARTESIAN_POINT('Ctrl Pts',(1.49498684495197,-2.57355865072957,
0.226955364321571)) ;
#125255 = CARTESIAN_POINT('Ctrl Pts',(1.50433565895458,-2.55454999214157,
-0.162734644895059)) ;
#125256 = CARTESIAN_POINT('Ctrl Pts',(1.46956061091959,-2.54431087635249,
-0.360479674535448)) ;
#125257 = CARTESIAN_POINT('Ctrl Pts',(1.32589085798636,-2.52262288504127,
-0.728308338386614)) ;
#125258 = CARTESIAN_POINT('Ctrl Pts',(1.21947671138053,-2.51163959036419,
-0.895153595180616)) ;
#125259 = CARTESIAN_POINT('Ctrl Pts',(0.952647844145463,-2.49080569364162,
-1.17412428857262)) ;
#125260 = CARTESIAN_POINT('Ctrl Pts',(0.79644403135156,-2.48174689199624,
-1.28521198093932)) ;
#125261 = CARTESIAN_POINT('Ctrl Pts',(0.442771250326625,-2.46209840416152,
-1.44689800637849)) ;
#125262 = CARTESIAN_POINT('Ctrl Pts',(0.247250914219815,-2.45123616326669,
-1.49278504712828)) ;
#125263 = CARTESIAN_POINT('Ctrl Pts',(0.0323322730512658,-2.43929623875733,
-1.49973882485724)) ;
#125264 = CARTESIAN_POINT('Ctrl Pts',(0.0161609579953818,-2.43839783236533,
-1.5)) ;
#125265 = CARTESIAN_POINT('Ctrl Pts',(0.,-2.43750000136559,-1.5)) ;
#125266 = CARTESIAN_POINT('Origin',(0.,-6.,0.)) ;
#125267 = CARTESIAN_POINT('',(-1.23676600408074E-15,-1.87499999999999,-1.5)) ;
#125268 = CARTESIAN_POINT('',(2.06788221765507E-15,-1.93750000136559,-1.5)) ;
#125269 = CARTESIAN_POINT('',(-1.83697019872103E-16,-6.,-1.5)) ;
#125270 = CARTESIAN_POINT('Ctrl Pts',(2.60282034651221E-16,-1.87499999999999,
-1.5)) ;
#125271 = CARTESIAN_POINT('Ctrl Pts',(0.00943735868268793,-1.87552429770459,
-1.5)) ;
#125272 = CARTESIAN_POINT('Ctrl Pts',(0.0188785514875759,-1.87604880841598,
-1.49991093644605)) ;
#125273 = CARTESIAN_POINT('Ctrl Pts',(0.22714652682835,-1.88761925149046,
-1.49597781079793)) ;
#125274 = CARTESIAN_POINT('Ctrl Pts',(0.4232774234807,-1.89851541241559,-1.45272168687975)) ;
#125275 = CARTESIAN_POINT('Ctrl Pts',(0.779208648772136,-1.91828936937623,
-1.29575149131839)) ;
#125276 = CARTESIAN_POINT('Ctrl Pts',(0.93697217883324,-1.92726573334301,
-1.18668907950213)) ;
#125277 = CARTESIAN_POINT('Ctrl Pts',(1.20736056247296,-1.94802262290301,
-0.911374037682096)) ;
#125278 = CARTESIAN_POINT('Ctrl Pts',(1.31586542221273,-1.95898355504511,
-0.746200651240154)) ;
#125279 = CARTESIAN_POINT('Ctrl Pts',(1.4644642889903,-1.98069920720196,-0.380642892713603)) ;
#125280 = CARTESIAN_POINT('Ctrl Pts',(1.50194695578602,-1.99112086962977,
-0.183425183692144)) ;
#125281 = CARTESIAN_POINT('Ctrl Pts',(1.49797825778615,-2.00996969178462,
0.206048899069629)) ;
#125282 = CARTESIAN_POINT('Ctrl Pts',(1.45965998564815,-2.02010908144715,
0.394669090974854)) ;
#125283 = CARTESIAN_POINT('Ctrl Pts',(1.31163447008062,-2.04152055546697,
0.754235650122164)) ;
#125284 = CARTESIAN_POINT('Ctrl Pts',(1.20064793304481,-2.0526130092772,0.920709866047377)) ;
#125285 = CARTESIAN_POINT('Ctrl Pts',(0.92292434835193,-2.07368596213456,
1.19835917983805)) ;
#125286 = CARTESIAN_POINT('Ctrl Pts',(0.759912420907417,-2.08278264328292,
1.30781507008685)) ;
#125287 = CARTESIAN_POINT('Ctrl Pts',(0.40259446922281,-2.10263364059874,
1.4577915896283)) ;
#125288 = CARTESIAN_POINT('Ctrl Pts',(0.211929265373631,-2.11322615192369,
1.49743386092166)) ;
#125289 = CARTESIAN_POINT('Ctrl Pts',(-0.181574388459856,-2.13508746602555,
1.50242238157228)) ;
#125290 = CARTESIAN_POINT('Ctrl Pts',(-0.380671142079628,-2.1461483967822,
1.46470086422455)) ;
#125291 = CARTESIAN_POINT('Ctrl Pts',(-0.742849037099933,-2.16626939094999,
1.31699025508058)) ;
#125292 = CARTESIAN_POINT('Ctrl Pts',(-0.903904054165086,-2.17512331637634,
1.21212648927073)) ;
#125293 = CARTESIAN_POINT('Ctrl Pts',(-1.18160979654635,-2.19571782871237,
0.944411073712693)) ;
#125294 = CARTESIAN_POINT('Ctrl Pts',(-1.29435969760203,-2.20662639734714,
0.782776918078987)) ;
#125295 = CARTESIAN_POINT('Ctrl Pts',(-1.45302295344634,-2.2283833369147,
0.422171694572619)) ;
#125296 = CARTESIAN_POINT('Ctrl Pts',(-1.49613045578213,-2.23901395315421,
0.226106613339065)) ;
#125297 = CARTESIAN_POINT('Ctrl Pts',(-1.50321487640017,-2.25792417813516,
-0.162844839904798)) ;
#125298 = CARTESIAN_POINT('Ctrl Pts',(-1.47048115626658,-2.26775558478375,
-0.352000187186925)) ;
#125299 = CARTESIAN_POINT('Ctrl Pts',(-1.33342945165836,-2.2890194806551,
-0.714835124830947)) ;
#125300 = CARTESIAN_POINT('Ctrl Pts',(-1.22780151418331,-2.30009454820616,
-0.884041763044062)) ;
#125301 = CARTESIAN_POINT('Ctrl Pts',(-0.958042844808662,-2.32138113354333,
-1.17072989054784)) ;
#125302 = CARTESIAN_POINT('Ctrl Pts',(-0.796989535015222,-2.33072280361027,
-1.2857875225238)) ;
#125303 = CARTESIAN_POINT('Ctrl Pts',(-0.443022474300268,-2.35038764031665,
-1.44594879262274)) ;
#125304 = CARTESIAN_POINT('Ctrl Pts',(-0.254069427816286,-2.36088503178798,
-1.49079413572083)) ;
#125305 = CARTESIAN_POINT('Ctrl Pts',(-0.0412129187210752,-2.37271039340438,
-1.49957571771944)) ;
#125306 = CARTESIAN_POINT('Ctrl Pts',(-0.0205982039601356,-2.37385565533554,
-1.5)) ;
#125307 = CARTESIAN_POINT('Ctrl Pts',(2.6028203465122E-16,-2.37499999999999,
-1.5)) ;
#125308 = CARTESIAN_POINT('Ctrl Pts',(-1.07552855510562E-15,-2.43750000136559,
-1.5)) ;
#125309 = CARTESIAN_POINT('Ctrl Pts',(-0.177332442740351,-2.42764819899113,
-1.5)) ;
#125310 = CARTESIAN_POINT('Ctrl Pts',(-0.353417850306997,-2.41786567634853,
-1.46855134717232)) ;
#125311 = CARTESIAN_POINT('Ctrl Pts',(-0.700665072932742,-2.39857416398043,
-1.34020877878796)) ;
#125312 = CARTESIAN_POINT('Ctrl Pts',(-0.866743242519118,-2.38971601567301,
-1.23929375986335)) ;
#125313 = CARTESIAN_POINT('Ctrl Pts',(-1.15650631385966,-2.36898820306878,
-0.975769052379438)) ;
#125314 = CARTESIAN_POINT('Ctrl Pts',(-1.27564803794744,-2.35788815355817,
-0.813845362226324)) ;
#125315 = CARTESIAN_POINT('Ctrl Pts',(-1.44058755834756,-2.33627150333408,
-0.459779600998612)) ;
#125316 = CARTESIAN_POINT('Ctrl Pts',(-1.4874822923766,-2.32594524830586,
-0.272227107984242)) ;
#125317 = CARTESIAN_POINT('Ctrl Pts',(-1.5085508736479,-2.30659366029616,
0.117824144626538)) ;
#125318 = CARTESIAN_POINT('Ctrl Pts',(-1.47963309169109,-2.29669516685316,
0.316738476574083)) ;
#125319 = CARTESIAN_POINT('Ctrl Pts',(-1.34662537643692,-2.27507190351172,
0.689377525161628)) ;
#125320 = CARTESIAN_POINT('Ctrl Pts',(-1.24479148771335,-2.26404706697388,
0.859730626438732)) ;
#125321 = CARTESIAN_POINT('Ctrl Pts',(-0.985673414919529,-2.24305083706711,
1.14652718095046)) ;
#125322 = CARTESIAN_POINT('Ctrl Pts',(-0.832760732880199,-2.2337644865256,
1.26196855215552)) ;
#125323 = CARTESIAN_POINT('Ctrl Pts',(-0.483964356688177,-2.21438691007049,
1.43364193376676)) ;
#125324 = CARTESIAN_POINT('Ctrl Pts',(-0.289863219534461,-2.20360351356195,
1.48509519379718)) ;
#125325 = CARTESIAN_POINT('Ctrl Pts',(0.102527341581848,-2.18180403794437,
1.50905337356658)) ;
#125326 = CARTESIAN_POINT('Ctrl Pts',(0.296950144442835,-2.17100277111876,
1.48309999427456)) ;
#125327 = CARTESIAN_POINT('Ctrl Pts',(0.662529120150319,-2.1506928280239,
1.35932974810785)) ;
#125328 = CARTESIAN_POINT('Ctrl Pts',(0.83056065201908,-2.14189443954733,
1.26368142146705)) ;
#125329 = CARTESIAN_POINT('Ctrl Pts',(1.12768045373333,-2.12139066244948,
1.00906061480182)) ;
#125330 = CARTESIAN_POINT('Ctrl Pts',(1.25182239011894,-2.11029780742779,
0.850173333209126)) ;
#125331 = CARTESIAN_POINT('Ctrl Pts',(1.42721924685902,-2.08857483450314,
0.499935242099737)) ;
#125332 = CARTESIAN_POINT('Ctrl Pts',(1.47945500711303,-2.07814170737608,
0.313245097152927)) ;
#125333 = CARTESIAN_POINT('Ctrl Pts',(1.511052979967,-2.05859730310795,-0.0747346190667385)) ;
#125334 = CARTESIAN_POINT('Ctrl Pts',(1.48816846050364,-2.04906221844655,
-0.272468130568953)) ;
#125335 = CARTESIAN_POINT('Ctrl Pts',(1.36719082913346,-2.02764278422735,
-0.647816242575988)) ;
#125336 = CARTESIAN_POINT('Ctrl Pts',(1.2702926922646,-2.01658398592398,-0.821724883555877)) ;
#125337 = CARTESIAN_POINT('Ctrl Pts',(1.01937149866044,-1.99542199406449,
-1.11669920596306)) ;
#125338 = CARTESIAN_POINT('Ctrl Pts',(0.869834738526956,-1.98582415350598,
-1.23672475538724)) ;
#125339 = CARTESIAN_POINT('Ctrl Pts',(0.526189893171804,-1.96673277320847,
-1.4186835775582)) ;
#125340 = CARTESIAN_POINT('Ctrl Pts',(0.333729565204767,-1.95604053276585,
-1.47585193693545)) ;
#125341 = CARTESIAN_POINT('Ctrl Pts',(0.0905495303401054,-1.94253053082893,
-1.49795258490765)) ;
#125342 = CARTESIAN_POINT('Ctrl Pts',(0.0452488974255713,-1.94001382900035,
-1.5)) ;
#125343 = CARTESIAN_POINT('Ctrl Pts',(0.,-1.93750000136559,-1.5)) ;
#125344 = CARTESIAN_POINT('Origin',(0.,-6.,0.)) ;
#125345 = CARTESIAN_POINT('',(-1.83697019872103E-16,-0.1,-1.5)) ;
#125346 = CARTESIAN_POINT('Origin',(0.,-0.1,0.)) ;
#125347 = CARTESIAN_POINT('',(1.27966723825811E-15,-0.93750000136559,-1.5)) ;
#125348 = CARTESIAN_POINT('',(-1.83697019872103E-16,-6.,-1.5)) ;
#125349 = CARTESIAN_POINT('',(1.48723526368499,-0.552750382528326,-0.19527229821924)) ;
#125350 = CARTESIAN_POINT('Ctrl Pts',(0.,-0.93750000136559,-1.5)) ;
#125351 = CARTESIAN_POINT('Ctrl Pts',(-0.0924142321550466,-0.932365877356976,
-1.5)) ;
#125352 = CARTESIAN_POINT('Ctrl Pts',(-0.184851853456529,-0.927230453951329,
-1.49145967026687)) ;
#125353 = CARTESIAN_POINT('Ctrl Pts',(-0.462932371399564,-0.911781536287827,
-1.43938052160168)) ;
#125354 = CARTESIAN_POINT('Ctrl Pts',(-0.641347933989665,-0.902228062825542,
-1.36921973430852)) ;
#125355 = CARTESIAN_POINT('Ctrl Pts',(-0.969943538414926,-0.883099606137119,
-1.16135698872124)) ;
#125356 = CARTESIAN_POINT('Ctrl Pts',(-1.11516010244463,-0.872395120488618,
-1.02270925490941)) ;
#125357 = CARTESIAN_POINT('Ctrl Pts',(-1.3407638224346,-0.850612138321202,
-0.700210841123837)) ;
#125358 = CARTESIAN_POINT('Ctrl Pts',(-1.42027434193999,-0.839750349397203,
-0.52035821763424)) ;
#125359 = CARTESIAN_POINT('Ctrl Pts',(-1.50522706343029,-0.819286071047164,
-0.144063656145068)) ;
#125360 = CARTESIAN_POINT('Ctrl Pts',(-1.51132705318559,-0.810481931552609,
0.0484844705972081)) ;
#125361 = CARTESIAN_POINT('Ctrl Pts',(-1.44951895516163,-0.790182777922516,
0.434709533820591)) ;
#125362 = CARTESIAN_POINT('Ctrl Pts',(-1.37863155578292,-0.779104061815861,
0.624049464859449)) ;
#125363 = CARTESIAN_POINT('Ctrl Pts',(-1.17080022717307,-0.75730064673869,
0.957233463646603)) ;
#125364 = CARTESIAN_POINT('Ctrl Pts',(-1.03838420938941,-0.746778825997023,
1.09947497748658)) ;
#125365 = CARTESIAN_POINT('Ctrl Pts',(-0.724474918368461,-0.727067156923346,
1.32793871186564)) ;
#125366 = CARTESIAN_POINT('Ctrl Pts',(-0.545281412466567,-0.717793413169278,
1.41101535151924)) ;
#125367 = CARTESIAN_POINT('Ctrl Pts',(-0.163073280254602,-0.696559628046391,
1.50415834013272)) ;
#125368 = CARTESIAN_POINT('Ctrl Pts',(0.0363728332714122,-0.685479288406057,
1.51253380685678)) ;
#125369 = CARTESIAN_POINT('Ctrl Pts',(0.419829625717041,-0.664176133270189,
1.45258543441048)) ;
#125370 = CARTESIAN_POINT('Ctrl Pts',(0.600589014989293,-0.654245791110056,
1.38762525630755)) ;
#125371 = CARTESIAN_POINT('Ctrl Pts',(0.935392040807353,-0.635406495702389,
1.18935647149059)) ;
#125372 = CARTESIAN_POINT('Ctrl Pts',(1.08459357960647,-0.62480079948512,
1.05506276370435)) ;
#125373 = CARTESIAN_POINT('Ctrl Pts',(1.31990170521924,-0.603054571176904,
0.738931105735517)) ;
#125374 = CARTESIAN_POINT('Ctrl Pts',(1.40481888017356,-0.592132013847489,
0.56093696863664)) ;
#125375 = CARTESIAN_POINT('Ctrl Pts',(1.50056674105296,-0.571460167677666,
0.186560767661118)) ;
#125376 = CARTESIAN_POINT('Ctrl Pts',(1.51210623124261,-0.562554840242503,
-0.00584973121425299)) ;
#125377 = CARTESIAN_POINT('Ctrl Pts',(1.48723526368499,-0.552750382528326,
-0.19527229821924)) ;
#125378 = CARTESIAN_POINT('',(0.903681962956226,-0.694267812214528,-1.19722968131749)) ;
#125379 = CARTESIAN_POINT('Origin',(0.,-1.40417355919753,0.)) ;
#125380 = CARTESIAN_POINT('',(0.903681962086507,-0.819267341061323,-1.19722968197397)) ;
#125381 = CARTESIAN_POINT('',(0.903681962956226,-0.694267812214528,-1.19722968131749)) ;
#125382 = CARTESIAN_POINT('',(1.42658067231545,-0.975658586206326,-0.463538116421942)) ;
#125383 = CARTESIAN_POINT('Origin',(0.,-0.109621223236985,0.)) ;
#125384 = CARTESIAN_POINT('',(-9.18485099360515E-17,-1.37499999999999,-1.5)) ;
#125385 = CARTESIAN_POINT('Ctrl Pts',(1.42658067231545,-0.975658586206326,
-0.463538116421941)) ;
#125386 = CARTESIAN_POINT('Ctrl Pts',(1.4608676911025,-0.981687904878683,
-0.35801670064177)) ;
#125387 = CARTESIAN_POINT('Ctrl Pts',(1.4833430518337,-0.987556547803326,
-0.249015403606839)) ;
#125388 = CARTESIAN_POINT('Ctrl Pts',(1.50354576305376,-0.998598705815113,
-0.0311724999487236)) ;
#125389 = CARTESIAN_POINT('Ctrl Pts',(1.50190176982991,-1.00364732798507,
0.0769062759071393)) ;
#125390 = CARTESIAN_POINT('Ctrl Pts',(1.46503210262907,-1.01903086279124,
0.375360330235355)) ;
#125391 = CARTESIAN_POINT('Ctrl Pts',(1.40467081292517,-1.02961241555355,
0.560444167463701)) ;
#125392 = CARTESIAN_POINT('Ctrl Pts',(1.21347769961073,-1.05146516319492,
0.90425960242237)) ;
#125393 = CARTESIAN_POINT('Ctrl Pts',(1.08184553656645,-1.06252928019626,
1.0582250911012)) ;
#125394 = CARTESIAN_POINT('Ctrl Pts',(0.773696965752526,-1.08267888640319,
1.29911713122624)) ;
#125395 = CARTESIAN_POINT('Ctrl Pts',(0.602602377832728,-1.09152209012042,
1.3867903141585)) ;
#125396 = CARTESIAN_POINT('Ctrl Pts',(0.232273153510163,-1.11209593591611,
1.4947030359203)) ;
#125397 = CARTESIAN_POINT('Ctrl Pts',(0.0360475909930078,-1.12299735605596,
1.51221063712791)) ;
#125398 = CARTESIAN_POINT('Ctrl Pts',(-0.355665576846667,-1.14475919871371,
1.4707170273039)) ;
#125399 = CARTESIAN_POINT('Ctrl Pts',(-0.547235950104445,-1.15540199722803,
1.41069664698689)) ;
#125400 = CARTESIAN_POINT('Ctrl Pts',(-0.888252485248476,-1.17434736029159,
1.22358660666486)) ;
#125401 = CARTESIAN_POINT('Ctrl Pts',(-1.0361018207849,-1.18413130376333,
1.10122340347657)) ;
#125402 = CARTESIAN_POINT('Ctrl Pts',(-1.28281560741993,-1.20537561709001,
0.802108913958369)) ;
#125403 = CARTESIAN_POINT('Ctrl Pts',(-1.37715772840634,-1.2164478442942,
0.626445442058699)) ;
#125404 = CARTESIAN_POINT('Ctrl Pts',(-1.49202537596067,-1.23776042435012,
0.249790651328553)) ;
#125405 = CARTESIAN_POINT('Ctrl Pts',(-1.51186968215624,-1.24713737546132,
0.0526455695399674)) ;
#125406 = CARTESIAN_POINT('Ctrl Pts',(-1.47488723137769,-1.26677894559483,
-0.334244971487723)) ;
#125407 = CARTESIAN_POINT('Ctrl Pts',(-1.41990947355275,-1.2772640810985,
-0.520432997207323)) ;
#125408 = CARTESIAN_POINT('Ctrl Pts',(-1.23916679121819,-1.29903518512036,
-0.868585060540103)) ;
#125409 = CARTESIAN_POINT('Ctrl Pts',(-1.11248140632144,-1.31012075688599,
-1.02585250181586)) ;
#125410 = CARTESIAN_POINT('Ctrl Pts',(-0.811619236320399,-1.33050687516637,
-1.27586715854565)) ;
#125411 = CARTESIAN_POINT('Ctrl Pts',(-0.642569451667573,-1.33930169712959,
-1.36882027675838)) ;
#125412 = CARTESIAN_POINT('Ctrl Pts',(-0.311549635183878,-1.35769168693423,
-1.47562252873181)) ;
#125413 = CARTESIAN_POINT('Ctrl Pts',(-0.156126656755279,-1.36632629684692,
-1.5)) ;
#125414 = CARTESIAN_POINT('Ctrl Pts',(5.89805981832114E-16,-1.37499999999999,
-1.5)) ;
#125415 = CARTESIAN_POINT('',(-2.10412774206915E-15,-1.43750000136559,-1.5)) ;
#125416 = CARTESIAN_POINT('',(-1.83697019872103E-16,-6.,-1.5)) ;
#125417 = CARTESIAN_POINT('Ctrl Pts',(-1.45716771982052E-15,-1.43750000136559,
-1.5)) ;
#125418 = CARTESIAN_POINT('Ctrl Pts',(-0.12139289337904,-1.43075595173342,
-1.5)) ;
#125419 = CARTESIAN_POINT('Ctrl Pts',(-0.242615485235266,-1.42402136329696,
-1.48526320021271)) ;
#125420 = CARTESIAN_POINT('Ctrl Pts',(-0.54542560532699,-1.40719857884742,
-1.41018650153551)) ;
#125421 = CARTESIAN_POINT('Ctrl Pts',(-0.719475265230306,-1.39816291148787,
-1.32983398614367)) ;
#125422 = CARTESIAN_POINT('Ctrl Pts',(-1.03556294373952,-1.37848139126207,
-1.1032545764031)) ;
#125423 = CARTESIAN_POINT('Ctrl Pts',(-1.17254730770333,-1.36761005677763,
-0.956386091734899)) ;
#125424 = CARTESIAN_POINT('Ctrl Pts',(-1.37853603313159,-1.34581062140582,
-0.622220982127438)) ;
#125425 = CARTESIAN_POINT('Ctrl Pts',(-1.44729330200646,-1.33509397144994,
-0.439176623295063)) ;
#125426 = CARTESIAN_POINT('Ctrl Pts',(-1.51121609450788,-1.31498083622332,
-0.0580387994088512)) ;
#125427 = CARTESIAN_POINT('Ctrl Pts',(-1.50617017426866,-1.30611041853233,
0.136367337051198)) ;
#125428 = CARTESIAN_POINT('Ctrl Pts',(-1.42141652159494,-1.28535520160221,
0.518823875806305)) ;
#125429 = CARTESIAN_POINT('Ctrl Pts',(-1.34012610682817,-1.27425489967523,
0.702606275960677)) ;
#125430 = CARTESIAN_POINT('Ctrl Pts',(-1.11491907204454,-1.25265264228599,
1.02157742208114)) ;
#125431 = CARTESIAN_POINT('Ctrl Pts',(-0.97552501409157,-1.24234020400036,
1.15543822992624)) ;
#125432 = CARTESIAN_POINT('Ctrl Pts',(-0.647387975472766,-1.22301296441911,
1.36769735344609)) ;
#125433 = CARTESIAN_POINT('Ctrl Pts',(-0.460153323374986,-1.21306407488642,
1.44152590664843)) ;
#125434 = CARTESIAN_POINT('Ctrl Pts',(-0.0704853868697509,-1.19141585619168,
1.51117296929148)) ;
#125435 = CARTESIAN_POINT('Ctrl Pts',(0.127872336502056,-1.18039598267102,
1.50740248439617)) ;
#125436 = CARTESIAN_POINT('Ctrl Pts',(0.505423896210884,-1.15942089602053,
1.42499909293535)) ;
#125437 = CARTESIAN_POINT('Ctrl Pts',(0.681572805914866,-1.1501684229538,
1.34963476410479)) ;
#125438 = CARTESIAN_POINT('Ctrl Pts',(1.0038364982207,-1.13075505293512,1.13219447498585)) ;
#125439 = CARTESIAN_POINT('Ctrl Pts',(1.14491523340415,-1.11996081308417,
0.989292258509651)) ;
#125440 = CARTESIAN_POINT('Ctrl Pts',(1.3605913200847,-1.09816016784024,0.660695002809255)) ;
#125441 = CARTESIAN_POINT('Ctrl Pts',(1.43463121008879,-1.08736823961763,
0.479135937315464)) ;
#125442 = CARTESIAN_POINT('Ctrl Pts',(1.50887308707389,-1.06708098933289,
0.100336926109472)) ;
#125443 = CARTESIAN_POINT('Ctrl Pts',(1.50933516496826,-1.05827872850654,
-0.0931271687809125)) ;
#125444 = CARTESIAN_POINT('Ctrl Pts',(1.43590454263757,-1.03774545194468,
-0.477508118223692)) ;
#125445 = CARTESIAN_POINT('Ctrl Pts',(1.35970219382423,-1.02665114013334,
-0.664103612410434)) ;
#125446 = CARTESIAN_POINT('Ctrl Pts',(1.14296119693593,-1.00494105320597,
-0.990203822651857)) ;
#125447 = CARTESIAN_POINT('Ctrl Pts',(1.00694889425996,-0.994521405798722,
-1.12824538756443)) ;
#125448 = CARTESIAN_POINT('Ctrl Pts',(0.685828290440808,-0.975001799998438,
-1.34855370838484)) ;
#125449 = CARTESIAN_POINT('Ctrl Pts',(0.502625072513882,-0.965423616505241,
-1.4270054983915)) ;
#125450 = CARTESIAN_POINT('Ctrl Pts',(0.207451669629485,-0.949025094122774,
-1.4892377999239)) ;
#125451 = CARTESIAN_POINT('Ctrl Pts',(0.103740571639932,-0.943263366456697,
-1.5)) ;
#125452 = CARTESIAN_POINT('Ctrl Pts',(-3.81639164714898E-16,-0.93750000136559,
-1.5)) ;
#125453 = CARTESIAN_POINT('Origin',(0.,-6.,0.)) ;
#125454 = CARTESIAN_POINT('Ctrl Pts',(2.60282034651221E-16,-1.37499999999999,
-1.5)) ;
#125455 = CARTESIAN_POINT('Ctrl Pts',(0.0378880627307306,-1.37710489237392,
-1.5)) ;
#125456 = CARTESIAN_POINT('Ctrl Pts',(0.0758175659488453,-1.37921208699716,
-1.49856452262518)) ;
#125457 = CARTESIAN_POINT('Ctrl Pts',(0.31193570823378,-1.39232976156855,
-1.48061396356261)) ;
#125458 = CARTESIAN_POINT('Ctrl Pts',(0.505234227970466,-1.40306856822058,
-1.42628306779644)) ;
#125459 = CARTESIAN_POINT('Ctrl Pts',(0.851455565955026,-1.4223030869975,
-1.24943605696842)) ;
#125460 = CARTESIAN_POINT('Ctrl Pts',(1.002668770544,-1.43173619321328,-1.13170226086917)) ;
#125461 = CARTESIAN_POINT('Ctrl Pts',(1.25769711838986,-1.45281601037343,
-0.840807174121323)) ;
#125462 = CARTESIAN_POINT('Ctrl Pts',(1.35707620689297,-1.46385909327745,
-0.66865754967684)) ;
#125463 = CARTESIAN_POINT('Ctrl Pts',(1.48406103596784,-1.48538141381695,
-0.29463924287184)) ;
#125464 = CARTESIAN_POINT('Ctrl Pts',(1.50995001557063,-1.49508944413126,
-0.0963193429286017)) ;
#125465 = CARTESIAN_POINT('Ctrl Pts',(1.48362149567478,-1.51453781872515,
0.292706754077122)) ;
#125466 = CARTESIAN_POINT('Ctrl Pts',(1.43406250307638,-1.5249183011972,0.479848132943688)) ;
#125467 = CARTESIAN_POINT('Ctrl Pts',(1.26389924289045,-1.54659005786061,
0.832043332432613)) ;
#125468 = CARTESIAN_POINT('Ctrl Pts',(1.14225570304284,-1.55768766952758,
0.992471928954704)) ;
#125469 = CARTESIAN_POINT('Ctrl Pts',(0.84881104050339,-1.5783045798591,1.25156600831668)) ;
#125470 = CARTESIAN_POINT('Ctrl Pts',(0.681763120312136,-1.58712427109378,
1.34985039084804)) ;
#125471 = CARTESIAN_POINT('Ctrl Pts',(0.317759579117409,-1.60734669004904,
1.47874613221529)) ;
#125472 = CARTESIAN_POINT('Ctrl Pts',(0.123996398982104,-1.61811131116766,
1.50740639143056)) ;
#125473 = CARTESIAN_POINT('Ctrl Pts',(-0.268444572010862,-1.63991358733394,
1.48911788802839)) ;
#125474 = CARTESIAN_POINT('Ctrl Pts',(-0.463280400432789,-1.65073780002404,
1.44046068521351)) ;
#125475 = CARTESIAN_POINT('Ctrl Pts',(-0.814543246749689,-1.67025240259721,
1.2738066884214)) ;
#125476 = CARTESIAN_POINT('Ctrl Pts',(-0.969108063961199,-1.67941530512131,
1.16056473101709)) ;
#125477 = CARTESIAN_POINT('Ctrl Pts',(-1.23213115359432,-1.70033009362367,
0.877715466832144)) ;
#125478 = CARTESIAN_POINT('Ctrl Pts',(-1.33629297016389,-1.71133506582633,
0.709119267777291)) ;
#125479 = CARTESIAN_POINT('Ctrl Pts',(-1.47508909334509,-1.73305320093322,
0.337850285448988)) ;
#125480 = CARTESIAN_POINT('Ctrl Pts',(-1.5069343887875,-1.74315054142095,
0.138359751926198)) ;
#125481 = CARTESIAN_POINT('Ctrl Pts',(-1.49090003004465,-1.76240862090636,
-0.252654472236755)) ;
#125482 = CARTESIAN_POINT('Ctrl Pts',(-1.44654705011602,-1.77268144862352,
-0.440563981857862)) ;
#125483 = CARTESIAN_POINT('Ctrl Pts',(-1.28660460880766,-1.79424170245274,
-0.796342630989032)) ;
#125484 = CARTESIAN_POINT('Ctrl Pts',(-1.16986364904193,-1.8053419518461,
-0.959656557554787)) ;
#125485 = CARTESIAN_POINT('Ctrl Pts',(-0.883637371833339,-1.8261739373672,
-1.22738842750026)) ;
#125486 = CARTESIAN_POINT('Ctrl Pts',(-0.718475544917168,-1.83508469194905,
-1.33082202979742)) ;
#125487 = CARTESIAN_POINT('Ctrl Pts',(-0.366370874060449,-1.8546460625522,
-1.46617447464151)) ;
#125488 = CARTESIAN_POINT('Ctrl Pts',(-0.183913488692333,-1.86478258396153,
-1.5)) ;
#125489 = CARTESIAN_POINT('Ctrl Pts',(3.81639164714898E-16,-1.87499999999999,
-1.5)) ;
#125490 = CARTESIAN_POINT('Ctrl Pts',(-5.20417042793042E-16,-1.93750000136559,
-1.5)) ;
#125491 = CARTESIAN_POINT('Ctrl Pts',(-0.148963326007169,-1.92922426103186,
-1.5)) ;
#125492 = CARTESIAN_POINT('Ctrl Pts',(-0.297365951084213,-1.9209796707498,
-1.4778082396457)) ;
#125493 = CARTESIAN_POINT('Ctrl Pts',(-0.622721506224344,-1.9029043621309,
-1.37791446022743)) ;
#125494 = CARTESIAN_POINT('Ctrl Pts',(-0.792785345987669,-1.89409462925514,
-1.28760192268381)) ;
#125495 = CARTESIAN_POINT('Ctrl Pts',(-1.09729928647212,-1.87382581947286,
-1.04213382797214)) ;
#125496 = CARTESIAN_POINT('Ctrl Pts',(-1.22646524414687,-1.86274978204871,
-0.886496713623897)) ;
#125497 = CARTESIAN_POINT('Ctrl Pts',(-1.4124393734564,-1.8409357283315,-0.540472334956)) ;
#125498 = CARTESIAN_POINT('Ctrl Pts',(-1.4701082237838,-1.83040144918074,
-0.354816580693619)) ;
#125499 = CARTESIAN_POINT('Ctrl Pts',(-1.51236437049839,-1.81066565131077,
0.0309876772900098)) ;
#125500 = CARTESIAN_POINT('Ctrl Pts',(-1.49546953995707,-1.80142527481105,
0.227568206543377)) ;
#125501 = CARTESIAN_POINT('Ctrl Pts',(-1.38655761046561,-1.78021894123352,
0.605453241115908)) ;
#125502 = CARTESIAN_POINT('Ctrl Pts',(-1.29473792765022,-1.76913611908959,
0.782793255060013)) ;
#125503 = CARTESIAN_POINT('Ctrl Pts',(-1.05215553348107,-1.74781282097243,
1.08593467317216)) ;
#125504 = CARTESIAN_POINT('Ctrl Pts',(-0.905935169714077,-1.73782973301637,
1.21058411696564)) ;
#125505 = CARTESIAN_POINT('Ctrl Pts',(-0.567487526947019,-1.71902708619598,
1.40267001389958)) ;
#125506 = CARTESIAN_POINT('Ctrl Pts',(-0.376819826414949,-1.70843443616642,
1.46543693014733)) ;
#125507 = CARTESIAN_POINT('Ctrl Pts',(0.0145050608199446,-1.68669416465337,
1.51260589749027)) ;
#125508 = CARTESIAN_POINT('Ctrl Pts',(0.211237065013851,-1.67576460886482,
1.49785589403808)) ;
#125509 = CARTESIAN_POINT('Ctrl Pts',(0.583064477857225,-1.65510753037352,
1.39508568987848)) ;
#125510 = CARTESIAN_POINT('Ctrl Pts',(0.755163912351607,-1.64621452491384,
1.30994238169818)) ;
#125511 = CARTESIAN_POINT('Ctrl Pts',(1.06678098124075,-1.62618094467741,
1.07346443438125)) ;
#125512 = CARTESIAN_POINT('Ctrl Pts',(1.20076273752401,-1.61513050794521,
0.921139823045825)) ;
#125513 = CARTESIAN_POINT('Ctrl Pts',(1.39694502659761,-1.59324470839863,
0.57951791910547)) ;
#125514 = CARTESIAN_POINT('Ctrl Pts',(1.45988754717958,-1.58261962593753,
0.395019608420067)) ;
#125515 = CARTESIAN_POINT('Ctrl Pts',(1.51245624265528,-1.56270225690715,
0.0113954175393681)) ;
#125516 = CARTESIAN_POINT('Ctrl Pts',(1.50125258566012,-1.55367636326687,
-0.184119054602967)) ;
#125517 = CARTESIAN_POINT('Ctrl Pts',(1.40390259390527,-1.53268199224902,
-0.564273817968124)) ;
#125518 = CARTESIAN_POINT('Ctrl Pts',(1.3170642170248,-1.52158568063126,-0.744770163683011)) ;
#125519 = CARTESIAN_POINT('Ctrl Pts',(1.08270069078918,-1.50012276598368,
-1.05555862250021)) ;
#125520 = CARTESIAN_POINT('Ctrl Pts',(0.939691176779303,-1.48993828925679,
-1.18467241476354)) ;
#125521 = CARTESIAN_POINT('Ctrl Pts',(0.606219181844705,-1.47097134753674,
-1.38636274940083)) ;
#125522 = CARTESIAN_POINT('Ctrl Pts',(0.417340103520255,-1.46068556267227,
-1.45443413180486)) ;
#125523 = CARTESIAN_POINT('Ctrl Pts',(0.147424479608115,-1.4456902502327,
-1.49457125502935)) ;
#125524 = CARTESIAN_POINT('Ctrl Pts',(0.0736808700220528,-1.44159338303348,
-1.5)) ;
#125525 = CARTESIAN_POINT('Ctrl Pts',(0.,-1.43750000136559,-1.5)) ;
#125526 = CARTESIAN_POINT('Origin',(1.38777878078145E-16,-6.28125000068279,
-2.77555756156289E-16)) ;
#125527 = CARTESIAN_POINT('',(0.981274813826767,-5.7706329375,0.740569452589779)) ;
#125528 = CARTESIAN_POINT('Ctrl Pts',(-1.2293670625,-5.46875000068277,3.46250805804971E-13)) ;
#125529 = CARTESIAN_POINT('Ctrl Pts',(-1.2293670625,-5.47663542588566,-0.134325140705998)) ;
#125530 = CARTESIAN_POINT('Ctrl Pts',(-1.20735998606848,-5.48522354848241,
-0.26791466575826)) ;
#125531 = CARTESIAN_POINT('Ctrl Pts',(-1.11207474840861,-5.5049165150107,
-0.548363706932059)) ;
#125532 = CARTESIAN_POINT('Ctrl Pts',(-1.03052046597732,-5.51596717534778,
-0.689522005866121)) ;
#125533 = CARTESIAN_POINT('Ctrl Pts',(-0.821238183951841,-5.53706027020258,
-0.928005462370774)) ;
#125534 = CARTESIAN_POINT('Ctrl Pts',(-0.697163736115499,-5.54649236723724,
-1.02448119159251)) ;
#125535 = CARTESIAN_POINT('Ctrl Pts',(-0.41311506452483,-5.56574676517468,
-1.16930744315786)) ;
#125536 = CARTESIAN_POINT('Ctrl Pts',(-0.254549227404192,-5.57649523905455,
-1.21372372448782)) ;
#125537 = CARTESIAN_POINT('Ctrl Pts',(0.06714482586041,-5.59830145022596,
-1.23786045820561)) ;
#125538 = CARTESIAN_POINT('Ctrl Pts',(0.227099237787686,-5.60914404942507,
-1.21870540434508)) ;
#125539 = CARTESIAN_POINT('Ctrl Pts',(0.528144905817568,-5.62955059826449,
-1.12116368850811)) ;
#125540 = CARTESIAN_POINT('Ctrl Pts',(0.666691868415718,-5.6383493957678,
-1.04473225017952)) ;
#125541 = CARTESIAN_POINT('Ctrl Pts',(0.913115375964076,-5.65876020209116,
-0.83931480906913)) ;
#125542 = CARTESIAN_POINT('Ctrl Pts',(1.0167778391346,-5.66985341368972,-0.710195830104623)) ;
#125543 = CARTESIAN_POINT('Ctrl Pts',(1.1644893331077,-5.69163252737805,-0.424478399462458)) ;
#125544 = CARTESIAN_POINT('Ctrl Pts',(1.2093003899459,-5.70211916585118,-0.271714281660297)) ;
#125545 = CARTESIAN_POINT('Ctrl Pts',(1.23789882222414,-5.72101542683666,
0.0336648365788081)) ;
#125546 = CARTESIAN_POINT('Ctrl Pts',(1.22473007440643,-5.72966378679881,
0.183234920590739)) ;
#125547 = CARTESIAN_POINT('Ctrl Pts',(1.14387771782609,-5.74961362474896,
0.476392493957535)) ;
#125548 = CARTESIAN_POINT('Ctrl Pts',(1.07470989404902,-5.76019836853254,
0.616765411484169)) ;
#125549 = CARTESIAN_POINT('Ctrl Pts',(0.981274813826767,-5.7706329375,0.740569452589778)) ;
#125550 = CARTESIAN_POINT('',(0.753945082394938,-5.77063293749981,-0.971035626067536)) ;
#125551 = CARTESIAN_POINT('Origin',(-1.72639680329212E-13,-5.77063293749983,
-4.62130334000221E-14)) ;
#125552 = CARTESIAN_POINT('Ctrl Pts',(0.753945082396521,-5.77063293749993,
-0.971035626066305)) ;
#125553 = CARTESIAN_POINT('Ctrl Pts',(0.634608850354497,-5.76114897999618,
-1.06369233492909)) ;
#125554 = CARTESIAN_POINT('Ctrl Pts',(0.499255840074009,-5.75259233679917,
-1.13354224868022)) ;
#125555 = CARTESIAN_POINT('Ctrl Pts',(0.20144221606974,-5.73240487387017,
-1.22325085756158)) ;
#125556 = CARTESIAN_POINT('Ctrl Pts',(0.0407802794899434,-5.72151431471711,
-1.23905218162873)) ;
#125557 = CARTESIAN_POINT('Ctrl Pts',(-0.28062497204338,-5.69972768013244,
-1.20795774713924)) ;
#125558 = CARTESIAN_POINT('Ctrl Pts',(-0.438175539990935,-5.68904802684083,
-1.16014631737484)) ;
#125559 = CARTESIAN_POINT('Ctrl Pts',(-0.71912711227131,-5.67000356751088,
-1.00920294138272)) ;
#125560 = CARTESIAN_POINT('Ctrl Pts',(-0.841199147635058,-5.66032534014921,
-0.909976073797117)) ;
#125561 = CARTESIAN_POINT('Ctrl Pts',(-1.04554886849715,-5.63911215798865,
-0.666599161392545)) ;
#125562 = CARTESIAN_POINT('Ctrl Pts',(-1.12411864786825,-5.62803939565067,
-0.523341259854422)) ;
#125563 = CARTESIAN_POINT('Ctrl Pts',(-1.21032348273614,-5.60903436230084,
-0.249368318883973)) ;
#125564 = CARTESIAN_POINT('Ctrl Pts',(-1.2293670625,-5.60108550690606,-0.124957485518691)) ;
#125565 = CARTESIAN_POINT('Ctrl Pts',(-1.2293670625,-5.59375000068276,4.61644611426948E-13)) ;
#125566 = CARTESIAN_POINT('Origin',(0.,18.,0.)) ;
#125567 = CARTESIAN_POINT('',(-1.53080849893419E-16,17.65,-1.25)) ;
#125568 = CARTESIAN_POINT('Origin',(0.,17.65,0.)) ;
#125569 = CARTESIAN_POINT('',(-1.95943487863577E-16,18.,-1.6)) ;
#125570 = CARTESIAN_POINT('',(-1.95943487863577E-16,18.,-1.6)) ;
#125571 = CARTESIAN_POINT('Origin',(0.,18.,0.)) ;
#125572 = CARTESIAN_POINT('Origin',(0.,18.,0.)) ;
#125573 = CARTESIAN_POINT('',(-1.53080849893419E-16,12.5,-1.25)) ;
#125574 = CARTESIAN_POINT('Origin',(0.,12.5,0.)) ;
#125575 = CARTESIAN_POINT('',(-1.53080849893419E-16,18.,-1.25)) ;
#125576 = CARTESIAN_POINT('Origin',(0.,12.5,0.)) ;
#125577 = CARTESIAN_POINT('',(-1.53107198751854E-15,11.7489242262155,0.)) ;
#125578 = CARTESIAN_POINT('',(-1.53080849893419E-16,12.5,-1.25)) ;
#125579 = CARTESIAN_POINT('Origin',(0.,-0.1,0.)) ;
#125580 = CARTESIAN_POINT('',(-1.95943487863577E-16,0.,-1.6)) ;
#125581 = CARTESIAN_POINT('Origin',(0.,0.,0.)) ;
#125582 = CARTESIAN_POINT('Origin',(-1.95943487863577E-16,-0.1,-1.6)) ;
#125583 = CARTESIAN_POINT('Origin',(0.,-6.,0.)) ;
#125584 = CARTESIAN_POINT('',(2.17906421430282E-8,-5.7377404754049,-1.26225952459509)) ;
#125585 = CARTESIAN_POINT('Ctrl Pts',(2.1866717776764E-8,-5.73774047449605,
-1.26225952550394)) ;
#125586 = CARTESIAN_POINT('Ctrl Pts',(-0.0951280656409561,-5.73375893783556,
-1.26624106381238)) ;
#125587 = CARTESIAN_POINT('Ctrl Pts',(-0.190610416698374,-5.72980069988564,
-1.2594456998284)) ;
#125588 = CARTESIAN_POINT('Ctrl Pts',(-0.450648170228269,-5.71911673850938,
-1.21081193891058)) ;
#125589 = CARTESIAN_POINT('Ctrl Pts',(-0.607374360928914,-5.71318902882096,
-1.14689385528148)) ;
#125590 = CARTESIAN_POINT('Ctrl Pts',(-0.895203825302845,-5.70041758644624,
-0.958275366297781)) ;
#125591 = CARTESIAN_POINT('Ctrl Pts',(-1.02125376648178,-5.69341610589362,
-0.833639491410614)) ;
#125592 = CARTESIAN_POINT('Ctrl Pts',(-1.21006754341351,-5.67981112061703,
-0.552467316470427)) ;
#125593 = CARTESIAN_POINT('Ctrl Pts',(-1.27501499197834,-5.67333137756034,
-0.401226892638821)) ;
#125594 = CARTESIAN_POINT('Ctrl Pts',(-1.35641798423161,-5.65939991142765,
-0.0370296772463542)) ;
#125595 = CARTESIAN_POINT('Ctrl Pts',(-1.34606239437347,-5.65347934071539,
0.146692754942947)) ;
#125596 = CARTESIAN_POINT('Ctrl Pts',(-1.28962811685841,-5.6415391541019,
0.462693260701388)) ;
#125597 = CARTESIAN_POINT('Ctrl Pts',(-1.22414853729526,-5.63459768074411,
0.630545962613037)) ;
#125598 = CARTESIAN_POINT('Ctrl Pts',(-1.03122244096974,-5.62082886886645,
0.933420099928659)) ;
#125599 = CARTESIAN_POINT('Ctrl Pts',(-0.904931516807769,-5.61413834418237,
1.06504118805754)) ;
#125600 = CARTESIAN_POINT('Ctrl Pts',(-0.683806844472658,-5.60503521401725,
1.21910575872353)) ;
#125601 = CARTESIAN_POINT('Ctrl Pts',(-0.60562741341424,-5.60212911291405,
1.26296031260107)) ;
#125602 = CARTESIAN_POINT('Ctrl Pts',(-0.362982426443556,-5.59284767566245,
1.3710135518573)) ;
#125603 = CARTESIAN_POINT('Ctrl Pts',(-0.189062330338105,-5.58628148087862,
1.41216222698045)) ;
#125604 = CARTESIAN_POINT('Ctrl Pts',(0.175704914409963,-5.57270889856158,
1.42883650540158)) ;
#125605 = CARTESIAN_POINT('Ctrl Pts',(0.363337370015593,-5.5658338966939,
1.40004302390087)) ;
#125606 = CARTESIAN_POINT('Ctrl Pts',(0.734812991615101,-5.55239504200623,
1.26436112246092)) ;
#125607 = CARTESIAN_POINT('Ctrl Pts',(0.895294849174838,-5.54655524435109,
1.15743901284809)) ;
#125608 = CARTESIAN_POINT('Ctrl Pts',(1.15932714106493,-5.5341022447373,0.916548243459604)) ;
#125609 = CARTESIAN_POINT('Ctrl Pts',(1.27259612584018,-5.52731204223573,
0.764558468756784)) ;
#125610 = CARTESIAN_POINT('Ctrl Pts',(1.39737099473228,-5.51712872405058,
0.506053099003585)) ;
#125611 = CARTESIAN_POINT('Ctrl Pts',(1.43135642621274,-5.51366992565339,
0.412585048988348)) ;
#125612 = CARTESIAN_POINT('Ctrl Pts',(1.47795810128641,-5.50725550608955,
0.22838679311422)) ;
#125613 = CARTESIAN_POINT('Ctrl Pts',(1.49619812498846,-5.50380187501517,
0.124642988468019)) ;
#125614 = CARTESIAN_POINT('Ctrl Pts',(1.50000000000133,-5.49999999999866,
-4.37310951340031E-11)) ;
#125615 = CARTESIAN_POINT('',(-1.22464679914735E-16,-6.,-0.999999999999998)) ;
#125616 = CARTESIAN_POINT('',(-1.22464679914735E-16,-6.,-0.999999999999998)) ;
#125617 = CARTESIAN_POINT('Origin',(0.,-6.,0.)) ;
#125618 = CARTESIAN_POINT('Ctrl Pts',(0.753945082395014,-5.77063293749988,
-0.971035626067628)) ;
#125619 = CARTESIAN_POINT('Ctrl Pts',(0.660062751113685,-5.76575199098791,
-1.05010851979854)) ;
#125620 = CARTESIAN_POINT('Ctrl Pts',(0.56562744963666,-5.76186505079845,
-1.10530231965888)) ;
#125621 = CARTESIAN_POINT('Ctrl Pts',(0.388796024291164,-5.75421567817824,
-1.18795136393926)) ;
#125622 = CARTESIAN_POINT('Ctrl Pts',(0.291380801751046,-5.75004165425893,
-1.21979558247614)) ;
#125623 = CARTESIAN_POINT('Ctrl Pts',(0.12800248544407,-5.7431151491797,-1.25200515595124)) ;
#125624 = CARTESIAN_POINT('Ctrl Pts',(0.0640816264084869,-5.74042257674819,
-1.25957742214169)) ;
#125625 = CARTESIAN_POINT('Ctrl Pts',(2.18667176318559E-8,-5.73774047449605,
-1.26225952550394)) ;
#125626 = CARTESIAN_POINT('Ctrl Pts',(0.981274813826771,-5.77063293749999,
0.740569452589782)) ;
#125627 = CARTESIAN_POINT('Ctrl Pts',(1.05284908434852,-5.75501478209421,
0.671658180365851)) ;
#125628 = CARTESIAN_POINT('Ctrl Pts',(1.11588152236375,-5.7395221143503,0.594367419289388)) ;
#125629 = CARTESIAN_POINT('Ctrl Pts',(1.225548935604,-5.70837632247707,0.420996666920777)) ;
#125630 = CARTESIAN_POINT('Ctrl Pts',(1.27045943674123,-5.69289700324141,
0.324733598497716)) ;
#125631 = CARTESIAN_POINT('Ctrl Pts',(1.36480677937284,-5.64992724118353,
0.0294077284638439)) ;
#125632 = CARTESIAN_POINT('Ctrl Pts',(1.36961990956584,-5.62856530733333,
-0.152118142611198)) ;
#125633 = CARTESIAN_POINT('Ctrl Pts',(1.34936797478974,-5.59217850615072,
-0.423529198806479)) ;
#125634 = CARTESIAN_POINT('Ctrl Pts',(1.3200119253903,-5.57359136443191,-0.557140339533079)) ;
#125635 = CARTESIAN_POINT('Ctrl Pts',(1.22318730692142,-5.53625530800328,
-0.815863444886249)) ;
#125636 = CARTESIAN_POINT('Ctrl Pts',(1.15514201583412,-5.5177094022426,-0.939251833099467)) ;
#125637 = CARTESIAN_POINT('Ctrl Pts',(1.07028821955689,-5.5,-1.05094392194718)) ;
#125638 = CARTESIAN_POINT('Origin',(0.,18.,0.)) ;
#125639 = CARTESIAN_POINT('',(1.40590516189806,17.7519237886467,2.06490082896921)) ;
#125640 = CARTESIAN_POINT('',(1.40590516189806,0.248076211353313,2.06490082896921)) ;
#125641 = CARTESIAN_POINT('',(1.40590516189806,18.,2.06490082896921)) ;
#125642 = CARTESIAN_POINT('',(1.08530399323385,17.7519237886467,2.25)) ;
#125643 = CARTESIAN_POINT('Origin',(0.,17.7519237886467,0.)) ;
#125644 = CARTESIAN_POINT('',(1.08530399323385,0.248076211353313,2.25)) ;
#125645 = CARTESIAN_POINT('',(1.08530399323385,18.,2.25)) ;
#125646 = CARTESIAN_POINT('Origin',(0.,0.248076211353313,0.)) ;
#125647 = CARTESIAN_POINT('Origin',(0.,18.,0.)) ;
#125648 = CARTESIAN_POINT('',(2.49120915513191,0.248076211353313,0.185099171030792)) ;
#125649 = CARTESIAN_POINT('',(2.49120915513191,17.7519237886467,0.185099171030793)) ;
#125650 = CARTESIAN_POINT('',(2.49120915513191,18.,0.185099171030792)) ;
#125651 = CARTESIAN_POINT('',(2.49120915513191,0.248076211353313,-0.185099171030794)) ;
#125652 = CARTESIAN_POINT('Origin',(0.,0.248076211353313,0.)) ;
#125653 = CARTESIAN_POINT('',(2.49120915513191,17.7519237886467,-0.185099171030793)) ;
#125654 = CARTESIAN_POINT('',(2.49120915513191,18.,-0.185099171030794)) ;
#125655 = CARTESIAN_POINT('Origin',(0.,17.7519237886467,0.)) ;
#125656 = CARTESIAN_POINT('Origin',(0.,18.,0.)) ;
#125657 = CARTESIAN_POINT('',(-1.08530399323399,17.7519237886467,2.25)) ;
#125658 = CARTESIAN_POINT('',(-1.08530399323385,0.248076211353313,2.25)) ;
#125659 = CARTESIAN_POINT('',(-1.08530399323385,18.,2.25)) ;
#125660 = CARTESIAN_POINT('',(-1.40590516189806,17.7519237886467,2.06490082896921)) ;
#125661 = CARTESIAN_POINT('Origin',(0.,17.7519237886467,0.)) ;
#125662 = CARTESIAN_POINT('',(-1.40590516189806,0.248076211353313,2.06490082896921)) ;
#125663 = CARTESIAN_POINT('',(-1.40590516189806,18.,2.06490082896921)) ;
#125664 = CARTESIAN_POINT('Origin',(0.,0.248076211353313,0.)) ;
#125665 = CARTESIAN_POINT('Origin',(0.,18.,0.)) ;
#125666 = CARTESIAN_POINT('',(-2.49120915513191,17.7519237886467,0.185099171030792)) ;
#125667 = CARTESIAN_POINT('',(-2.49120915513191,0.248076211353313,0.18509917103079)) ;
#125668 = CARTESIAN_POINT('',(-2.49120915513191,18.,0.18509917103079)) ;
#125669 = CARTESIAN_POINT('',(-2.49120915513191,17.7519237886467,-0.185099171030793)) ;
#125670 = CARTESIAN_POINT('Origin',(0.,17.7519237886467,0.)) ;
#125671 = CARTESIAN_POINT('',(-2.49120915513191,0.248076211353313,-0.185099171030793)) ;
#125672 = CARTESIAN_POINT('',(-2.49120915513191,18.,-0.185099171030793)) ;
#125673 = CARTESIAN_POINT('Origin',(0.,0.248076211353313,0.)) ;
#125674 = CARTESIAN_POINT('Origin',(0.,18.,0.)) ;
#125675 = CARTESIAN_POINT('',(-1.40590516189806,17.7519237886467,-2.06490082896921)) ;
#125676 = CARTESIAN_POINT('',(-1.40590516189806,0.248076211353313,-2.06490082896921)) ;
#125677 = CARTESIAN_POINT('',(-1.40590516189806,18.,-2.06490082896921)) ;
#125678 = CARTESIAN_POINT('',(-1.08530399323385,17.7519237886467,-2.25)) ;
#125679 = CARTESIAN_POINT('Origin',(0.,17.7519237886467,0.)) ;
#125680 = CARTESIAN_POINT('',(-1.08530399323385,0.248076211353313,-2.25)) ;
#125681 = CARTESIAN_POINT('',(-1.08530399323385,18.,-2.25)) ;
#125682 = CARTESIAN_POINT('Origin',(0.,0.248076211353313,0.)) ;
#125683 = CARTESIAN_POINT('Origin',(0.,18.,0.)) ;
#125684 = CARTESIAN_POINT('',(1.08530399323385,17.7519237886467,-2.25)) ;
#125685 = CARTESIAN_POINT('',(1.08530399323385,0.248076211353313,-2.25)) ;
#125686 = CARTESIAN_POINT('',(1.08530399323385,18.,-2.25)) ;
#125687 = CARTESIAN_POINT('',(1.40590516189806,17.7519237886467,-2.06490082896921)) ;
#125688 = CARTESIAN_POINT('Origin',(0.,17.7519237886467,0.)) ;
#125689 = CARTESIAN_POINT('',(1.40590516189806,0.248076211353313,-2.06490082896921)) ;
#125690 = CARTESIAN_POINT('',(1.40590516189806,18.,-2.06490082896921)) ;
#125691 = CARTESIAN_POINT('Origin',(0.,0.248076211353313,0.)) ;
#125692 = CARTESIAN_POINT('Origin',(0.,0.248076211353313,0.)) ;
#125693 = CARTESIAN_POINT('',(1.94855715851499,-5.70547202639737E-15,1.125)) ;
#125694 = CARTESIAN_POINT('Ctrl Pts',(2.49120915513191,0.248076211353315,
0.185099171030797)) ;
#125695 = CARTESIAN_POINT('Ctrl Pts',(2.20570698889652,-2.99760216648792E-15,
0.679603428621479)) ;
#125696 = CARTESIAN_POINT('Ctrl Pts',(1.94855715851498,-5.10230155997917E-16,
1.12500000000001)) ;
#125697 = CARTESIAN_POINT('',(1.94855715851499,-6.07033558534708E-15,-1.125)) ;
#125698 = CARTESIAN_POINT('Origin',(0.,0.,0.)) ;
#125699 = CARTESIAN_POINT('Ctrl Pts',(1.948557158515,2.89130421732174E-15,
-1.12499999999999)) ;
#125700 = CARTESIAN_POINT('Ctrl Pts',(2.20570698889652,5.89805981832114E-15,
-0.67960342862147)) ;
#125701 = CARTESIAN_POINT('Ctrl Pts',(2.49120915513191,0.248076211353317,
-0.1850991710308)) ;
#125702 = CARTESIAN_POINT('Origin',(0.,0.248076211353313,0.)) ;
#125703 = CARTESIAN_POINT('',(-1.18674972404001E-21,-3.4888067610237E-15,
2.25)) ;
#125704 = CARTESIAN_POINT('Origin',(0.,0.,0.)) ;
#125705 = CARTESIAN_POINT('Ctrl Pts',(1.94855715851498,-5.10230155997917E-16,
1.12500000000001)) ;
#125706 = CARTESIAN_POINT('Ctrl Pts',(1.69140732813346,2.25514051876985E-15,
1.57039657137853)) ;
#125707 = CARTESIAN_POINT('Ctrl Pts',(1.40590516189807,0.248076211353312,
2.0649008289692)) ;
#125708 = CARTESIAN_POINT('Ctrl Pts',(1.08530399323385,0.248076211353317,
2.25)) ;
#125709 = CARTESIAN_POINT('Ctrl Pts',(0.514299660763062,3.80251385934116E-15,
2.25)) ;
#125710 = CARTESIAN_POINT('Ctrl Pts',(8.16368249596716E-15,2.04092062399181E-15,
2.25)) ;
#125711 = CARTESIAN_POINT('Origin',(0.,0.248076211353313,0.)) ;
#125712 = CARTESIAN_POINT('',(-1.94855715851499,-6.18872890638757E-15,1.125)) ;
#125713 = CARTESIAN_POINT('Origin',(0.,0.,0.)) ;
#125714 = CARTESIAN_POINT('Ctrl Pts',(8.16368249596716E-15,2.04092062399181E-15,
2.25)) ;
#125715 = CARTESIAN_POINT('Ctrl Pts',(-0.514299660763059,1.38777878078145E-16,
2.25)) ;
#125716 = CARTESIAN_POINT('Ctrl Pts',(-1.08530399323386,0.248076211353322,
2.25)) ;
#125717 = CARTESIAN_POINT('Ctrl Pts',(-1.40590516189806,0.248076211353319,
2.06490082896921)) ;
#125718 = CARTESIAN_POINT('Ctrl Pts',(-1.69140732813346,-1.83186799063151E-15,
1.57039657137853)) ;
#125719 = CARTESIAN_POINT('Ctrl Pts',(-1.94855715851499,-5.10230155997935E-16,
1.12499999999999)) ;
#125720 = CARTESIAN_POINT('Origin',(0.,0.248076211353313,0.)) ;
#125721 = CARTESIAN_POINT('',(-1.94855715851499,-6.09408526551492E-15,-1.125)) ;
#125722 = CARTESIAN_POINT('Origin',(0.,0.,0.)) ;
#125723 = CARTESIAN_POINT('Ctrl Pts',(-1.94855715851499,-5.10230155997935E-16,
1.12499999999999)) ;
#125724 = CARTESIAN_POINT('Ctrl Pts',(-2.20570698889652,6.24500451351651E-16,
0.67960342862147)) ;
#125725 = CARTESIAN_POINT('Ctrl Pts',(-2.49120915513191,0.248076211353317,
0.185099171030793)) ;
#125726 = CARTESIAN_POINT('Ctrl Pts',(-2.49120915513191,0.248076211353319,
-0.185099171030792)) ;
#125727 = CARTESIAN_POINT('Ctrl Pts',(-2.20570698889652,-1.38777878078145E-16,
-0.679603428621472)) ;
#125728 = CARTESIAN_POINT('Ctrl Pts',(-1.94855715851499,-6.8030687466392E-16,
-1.125)) ;
#125729 = CARTESIAN_POINT('Origin',(0.,0.248076211353313,0.)) ;
#125730 = CARTESIAN_POINT('',(-3.75579836458312E-16,-3.69604056788555E-15,
-2.25)) ;
#125731 = CARTESIAN_POINT('Origin',(0.,0.,0.)) ;
#125732 = CARTESIAN_POINT('Ctrl Pts',(-1.94855715851499,-6.8030687466392E-16,
-1.125)) ;
#125733 = CARTESIAN_POINT('Ctrl Pts',(-1.69140732813346,-1.42247325030098E-15,
-1.57039657137852)) ;
#125734 = CARTESIAN_POINT('Ctrl Pts',(-1.40590516189807,0.248076211353311,
-2.0649008289692)) ;
#125735 = CARTESIAN_POINT('Ctrl Pts',(-1.08530399323385,0.248076211353314,
-2.25)) ;
#125736 = CARTESIAN_POINT('Ctrl Pts',(-0.514299660763063,-1.08246744900953E-15,
-2.25)) ;
#125737 = CARTESIAN_POINT('Ctrl Pts',(-7.99360577730116E-15,-2.21099734265776E-15,
-2.25)) ;
#125738 = CARTESIAN_POINT('Origin',(0.,0.248076211353313,0.)) ;
#125739 = CARTESIAN_POINT('Origin',(0.,0.,0.)) ;
#125740 = CARTESIAN_POINT('Ctrl Pts',(-7.99360577730116E-15,-2.21099734265776E-15,
-2.25)) ;
#125741 = CARTESIAN_POINT('Ctrl Pts',(0.514299660763054,-3.43475248243408E-15,
-2.25)) ;
#125742 = CARTESIAN_POINT('Ctrl Pts',(1.08530399323385,0.248076211353315,
-2.25)) ;
#125743 = CARTESIAN_POINT('Ctrl Pts',(1.40590516189807,0.248076211353319,
-2.06490082896921)) ;
#125744 = CARTESIAN_POINT('Ctrl Pts',(1.69140732813347,-4.44089209850067E-16,
-1.57039657137852)) ;
#125745 = CARTESIAN_POINT('Ctrl Pts',(1.948557158515,2.89130421732174E-15,
-1.12499999999999)) ;
#125746 = CARTESIAN_POINT('Origin',(0.,18.,0.)) ;
#125747 = CARTESIAN_POINT('',(1.94855715851499,18.,1.125)) ;
#125748 = CARTESIAN_POINT('Ctrl Pts',(1.40590516189807,17.7519237886467,2.0649008289692)) ;
#125749 = CARTESIAN_POINT('Ctrl Pts',(1.69140732813345,18.,1.57039657137854)) ;
#125750 = CARTESIAN_POINT('Ctrl Pts',(1.94855715851497,18.,1.12500000000003)) ;
#125751 = CARTESIAN_POINT('',(0.,18.,2.25)) ;
#125752 = CARTESIAN_POINT('Origin',(0.,18.,0.)) ;
#125753 = CARTESIAN_POINT('Ctrl Pts',(-2.72122749865572E-14,18.,2.25)) ;
#125754 = CARTESIAN_POINT('Ctrl Pts',(0.514299660763043,18.,2.25)) ;
#125755 = CARTESIAN_POINT('Ctrl Pts',(1.08530399323385,17.7519237886467,2.25)) ;
#125756 = CARTESIAN_POINT('Origin',(0.,18.,0.)) ;
#125757 = CARTESIAN_POINT('',(1.94855715851499,18.,-1.125)) ;
#125758 = CARTESIAN_POINT('Origin',(0.,18.,0.)) ;
#125759 = CARTESIAN_POINT('Ctrl Pts',(1.94855715851497,18.,1.12500000000003)) ;
#125760 = CARTESIAN_POINT('Ctrl Pts',(2.20570698889652,18.,0.679603428621478)) ;
#125761 = CARTESIAN_POINT('Ctrl Pts',(2.49120915513193,17.7519237886467,0.18509917103077)) ;
#125762 = CARTESIAN_POINT('Ctrl Pts',(2.49120915513191,17.7519237886467,-0.185099171030805)) ;
#125763 = CARTESIAN_POINT('Ctrl Pts',(2.20570698889653,18.,-0.679603428621451)) ;
#125764 = CARTESIAN_POINT('Ctrl Pts',(1.94855715851502,18.,-1.12499999999995)) ;
#125765 = CARTESIAN_POINT('Origin',(0.,18.,0.)) ;
#125766 = CARTESIAN_POINT('Ctrl Pts',(-1.08530399323398,17.7519237886466,
2.25)) ;
#125767 = CARTESIAN_POINT('Ctrl Pts',(-0.514299660763131,18.,2.25)) ;
#125768 = CARTESIAN_POINT('Ctrl Pts',(-2.72122749865572E-14,18.,2.25)) ;
#125769 = CARTESIAN_POINT('',(-1.94855715851499,18.,1.125)) ;
#125770 = CARTESIAN_POINT('Origin',(0.,18.,0.)) ;
#125771 = CARTESIAN_POINT('Ctrl Pts',(-1.94855715851499,18.,1.125)) ;
#125772 = CARTESIAN_POINT('Ctrl Pts',(-1.69140732813345,18.,1.57039657137854)) ;
#125773 = CARTESIAN_POINT('Ctrl Pts',(-1.40590516189804,17.7519237886467,
2.06490082896925)) ;
#125774 = CARTESIAN_POINT('Origin',(0.,18.,0.)) ;
#125775 = CARTESIAN_POINT('Ctrl Pts',(-2.4912091551319,17.7519237886467,0.185099171030818)) ;
#125776 = CARTESIAN_POINT('Ctrl Pts',(-2.20570698889652,18.,0.67960342862148)) ;
#125777 = CARTESIAN_POINT('Ctrl Pts',(-1.94855715851499,18.,1.125)) ;
#125778 = CARTESIAN_POINT('',(-1.94855715851499,18.,-1.125)) ;
#125779 = CARTESIAN_POINT('Origin',(0.,18.,0.)) ;
#125780 = CARTESIAN_POINT('Ctrl Pts',(-1.94855715851499,18.,-1.125)) ;
#125781 = CARTESIAN_POINT('Ctrl Pts',(-2.20570698889652,18.,-0.679603428621479)) ;
#125782 = CARTESIAN_POINT('Ctrl Pts',(-2.49120915513191,17.7519237886467,
-0.185099171030809)) ;
#125783 = CARTESIAN_POINT('Origin',(0.,18.,0.)) ;
#125784 = CARTESIAN_POINT('Ctrl Pts',(-1.40590516189808,17.7519237886467,
-2.06490082896919)) ;
#125785 = CARTESIAN_POINT('Ctrl Pts',(-1.69140732813347,18.,-1.57039657137852)) ;
#125786 = CARTESIAN_POINT('Ctrl Pts',(-1.94855715851499,18.,-1.125)) ;
#125787 = CARTESIAN_POINT('',(-3.7557864968429E-16,18.,-2.25)) ;
#125788 = CARTESIAN_POINT('Origin',(0.,18.,0.)) ;
#125789 = CARTESIAN_POINT('Ctrl Pts',(-3.40153437331965E-14,18.,-2.25)) ;
#125790 = CARTESIAN_POINT('Ctrl Pts',(-0.514299660763108,18.,-2.25)) ;
#125791 = CARTESIAN_POINT('Ctrl Pts',(-1.08530399323392,17.7519237886466,
-2.25)) ;
#125792 = CARTESIAN_POINT('Origin',(0.,18.,0.)) ;
#125793 = CARTESIAN_POINT('Ctrl Pts',(1.08530399323384,17.7519237886467,-2.25)) ;
#125794 = CARTESIAN_POINT('Ctrl Pts',(0.514299660763037,18.,-2.25)) ;
#125795 = CARTESIAN_POINT('Ctrl Pts',(-3.40153437331965E-14,18.,-2.25)) ;
#125796 = CARTESIAN_POINT('Origin',(0.,18.,0.)) ;
#125797 = CARTESIAN_POINT('Ctrl Pts',(1.94855715851502,18.,-1.12499999999995)) ;
#125798 = CARTESIAN_POINT('Ctrl Pts',(1.69140732813348,18.,-1.5703965713785)) ;
#125799 = CARTESIAN_POINT('Ctrl Pts',(1.40590516189807,17.7519237886467,-2.0649008289692)) ;
#125800 = CARTESIAN_POINT('Origin',(0.,18.,0.)) ;
#125801 = CARTESIAN_POINT('Origin',(0.,0.,0.)) ;
#125802 = CARTESIAN_POINT('Origin',(0.,-6.,0.)) ;
#125803 = CARTESIAN_POINT('Origin',(2.59807621135332,-6.,-4.08638347560999E-16)) ;
#125804 = CARTESIAN_POINT('Origin',(1.29903810567666,-6.,-2.25)) ;
#125805 = CARTESIAN_POINT('Origin',(-1.29903810567666,-6.,-2.25)) ;
#125806 = CARTESIAN_POINT('Origin',(-2.59807621135332,-6.,-4.47194905911973E-16)) ;
#125807 = CARTESIAN_POINT('Origin',(-1.29903810567666,-6.,2.25)) ;
#125808 = CARTESIAN_POINT('Origin',(1.29903810567666,-6.,2.25)) ;
#125809 = CARTESIAN_POINT('Ctrl Pts',(1.2293670625,-6.34375000068279,0.)) ;
#125810 = CARTESIAN_POINT('Ctrl Pts',(1.2293670625,-6.30208333401613,-0.709775404467235)) ;
#125811 = CARTESIAN_POINT('Ctrl Pts',(0.61468353125,-6.26041666734946,-1.06466310670085)) ;
#125812 = CARTESIAN_POINT('Ctrl Pts',(8.69224177194317E-17,-6.21875000068279,
-1.41955080893447)) ;
#125813 = CARTESIAN_POINT('Ctrl Pts',(-0.61468353125,-6.17708333401613,-1.06466310670085)) ;
#125814 = CARTESIAN_POINT('Ctrl Pts',(-1.2293670625,-6.13541666734946,-0.709775404467235)) ;
#125815 = CARTESIAN_POINT('Ctrl Pts',(-1.2293670625,-6.09375000068279,-1.50554043806781E-16)) ;
#125816 = CARTESIAN_POINT('Ctrl Pts',(-1.2293670625,-6.05208333401613,0.709775404467234)) ;
#125817 = CARTESIAN_POINT('Ctrl Pts',(-0.614683531250001,-6.01041666734946,
1.06466310670085)) ;
#125818 = CARTESIAN_POINT('Ctrl Pts',(-2.60767253158295E-16,-5.96875000068279,
1.41955080893447)) ;
#125819 = CARTESIAN_POINT('Ctrl Pts',(0.614683531249999,-5.92708333401613,
1.06466310670085)) ;
#125820 = CARTESIAN_POINT('Ctrl Pts',(1.2293670625,-5.88541666734946,0.709775404467235)) ;
#125821 = CARTESIAN_POINT('Ctrl Pts',(1.2293670625,-5.84375000068279,0.)) ;
#125822 = CARTESIAN_POINT('Ctrl Pts',(1.2293670625,-5.80208333401613,-0.709775404467235)) ;
#125823 = CARTESIAN_POINT('Ctrl Pts',(0.61468353125,-5.76041666734946,-1.06466310670085)) ;
#125824 = CARTESIAN_POINT('Ctrl Pts',(8.69224177194317E-17,-5.71875000068279,
-1.41955080893447)) ;
#125825 = CARTESIAN_POINT('Ctrl Pts',(-0.61468353125,-5.67708333401613,-1.06466310670085)) ;
#125826 = CARTESIAN_POINT('Ctrl Pts',(-1.2293670625,-5.63541666734946,-0.709775404467235)) ;
#125827 = CARTESIAN_POINT('Ctrl Pts',(-1.2293670625,-5.59375000068279,-1.50554043806781E-16)) ;
#125828 = CARTESIAN_POINT('Ctrl Pts',(-1.2293670625,-5.55208333401613,0.709775404467234)) ;
#125829 = CARTESIAN_POINT('Ctrl Pts',(-0.614683531250001,-5.51041666734946,
1.06466310670085)) ;
#125830 = CARTESIAN_POINT('Ctrl Pts',(-2.60767253158295E-16,-5.46875000068279,
1.41955080893447)) ;
#125831 = CARTESIAN_POINT('Ctrl Pts',(0.614683531249999,-5.42708333401613,
1.06466310670085)) ;
#125832 = CARTESIAN_POINT('Ctrl Pts',(1.2293670625,-5.38541666734946,0.709775404467235)) ;
#125833 = CARTESIAN_POINT('Ctrl Pts',(1.2293670625,-5.34375000068279,0.)) ;
#125834 = CARTESIAN_POINT('Ctrl Pts',(1.2293670625,-5.30208333401613,-0.709775404467235)) ;
#125835 = CARTESIAN_POINT('Ctrl Pts',(0.61468353125,-5.26041666734946,-1.06466310670085)) ;
#125836 = CARTESIAN_POINT('Ctrl Pts',(8.69224177194317E-17,-5.21875000068279,
-1.41955080893447)) ;
#125837 = CARTESIAN_POINT('Ctrl Pts',(-0.61468353125,-5.17708333401613,-1.06466310670085)) ;
#125838 = CARTESIAN_POINT('Ctrl Pts',(-1.2293670625,-5.13541666734946,-0.709775404467235)) ;
#125839 = CARTESIAN_POINT('Ctrl Pts',(-1.2293670625,-5.09375000068279,-1.50554043806781E-16)) ;
#125840 = CARTESIAN_POINT('Ctrl Pts',(-1.2293670625,-5.05208333401613,0.709775404467234)) ;
#125841 = CARTESIAN_POINT('Ctrl Pts',(-0.614683531250001,-5.01041666734946,
1.06466310670085)) ;
#125842 = CARTESIAN_POINT('Ctrl Pts',(-2.60767253158295E-16,-4.96875000068279,
1.41955080893447)) ;
#125843 = CARTESIAN_POINT('Ctrl Pts',(0.614683531249999,-4.92708333401613,
1.06466310670085)) ;
#125844 = CARTESIAN_POINT('Ctrl Pts',(1.2293670625,-4.88541666734946,0.709775404467235)) ;
#125845 = CARTESIAN_POINT('Ctrl Pts',(1.2293670625,-4.84375000068279,0.)) ;
#125846 = CARTESIAN_POINT('Ctrl Pts',(1.2293670625,-4.80208333401612,-0.709775404467235)) ;
#125847 = CARTESIAN_POINT('Ctrl Pts',(0.61468353125,-4.76041666734946,-1.06466310670085)) ;
#125848 = CARTESIAN_POINT('Ctrl Pts',(8.69224177194317E-17,-4.71875000068279,
-1.41955080893447)) ;
#125849 = CARTESIAN_POINT('Ctrl Pts',(-0.61468353125,-4.67708333401613,-1.06466310670085)) ;
#125850 = CARTESIAN_POINT('Ctrl Pts',(-1.2293670625,-4.63541666734946,-0.709775404467235)) ;
#125851 = CARTESIAN_POINT('Ctrl Pts',(-1.2293670625,-4.59375000068279,-1.50554043806781E-16)) ;
#125852 = CARTESIAN_POINT('Ctrl Pts',(-1.2293670625,-4.55208333401613,0.709775404467234)) ;
#125853 = CARTESIAN_POINT('Ctrl Pts',(-0.614683531250001,-4.51041666734946,
1.06466310670085)) ;
#125854 = CARTESIAN_POINT('Ctrl Pts',(-2.60767253158295E-16,-4.46875000068279,
1.41955080893447)) ;
#125855 = CARTESIAN_POINT('Ctrl Pts',(0.614683531249999,-4.42708333401613,
1.06466310670085)) ;
#125856 = CARTESIAN_POINT('Ctrl Pts',(1.2293670625,-4.38541666734946,0.709775404467235)) ;
#125857 = CARTESIAN_POINT('Ctrl Pts',(1.2293670625,-4.34375000068279,0.)) ;
#125858 = CARTESIAN_POINT('Ctrl Pts',(1.2293670625,-4.30208333401613,-0.709775404467235)) ;
#125859 = CARTESIAN_POINT('Ctrl Pts',(0.61468353125,-4.26041666734946,-1.06466310670085)) ;
#125860 = CARTESIAN_POINT('Ctrl Pts',(8.69224177194317E-17,-4.21875000068279,
-1.41955080893447)) ;
#125861 = CARTESIAN_POINT('Ctrl Pts',(-0.61468353125,-4.17708333401613,-1.06466310670085)) ;
#125862 = CARTESIAN_POINT('Ctrl Pts',(-1.2293670625,-4.13541666734946,-0.709775404467235)) ;
#125863 = CARTESIAN_POINT('Ctrl Pts',(-1.2293670625,-4.09375000068279,-1.50554043806781E-16)) ;
#125864 = CARTESIAN_POINT('Ctrl Pts',(-1.2293670625,-4.05208333401613,0.709775404467234)) ;
#125865 = CARTESIAN_POINT('Ctrl Pts',(-0.614683531250001,-4.01041666734946,
1.06466310670085)) ;
#125866 = CARTESIAN_POINT('Ctrl Pts',(-2.60767253158295E-16,-3.96875000068279,
1.41955080893447)) ;
#125867 = CARTESIAN_POINT('Ctrl Pts',(0.614683531249999,-3.92708333401613,
1.06466310670085)) ;
#125868 = CARTESIAN_POINT('Ctrl Pts',(1.2293670625,-3.88541666734946,0.709775404467235)) ;
#125869 = CARTESIAN_POINT('Ctrl Pts',(1.2293670625,-3.84375000068279,0.)) ;
#125870 = CARTESIAN_POINT('Ctrl Pts',(1.2293670625,-3.80208333401613,-0.709775404467235)) ;
#125871 = CARTESIAN_POINT('Ctrl Pts',(0.61468353125,-3.76041666734946,-1.06466310670085)) ;
#125872 = CARTESIAN_POINT('Ctrl Pts',(8.69224177194317E-17,-3.71875000068279,
-1.41955080893447)) ;
#125873 = CARTESIAN_POINT('Ctrl Pts',(-0.61468353125,-3.67708333401613,-1.06466310670085)) ;
#125874 = CARTESIAN_POINT('Ctrl Pts',(-1.2293670625,-3.63541666734946,-0.709775404467235)) ;
#125875 = CARTESIAN_POINT('Ctrl Pts',(-1.2293670625,-3.59375000068279,-1.50554043806781E-16)) ;
#125876 = CARTESIAN_POINT('Ctrl Pts',(-1.2293670625,-3.55208333401613,0.709775404467234)) ;
#125877 = CARTESIAN_POINT('Ctrl Pts',(-0.614683531250001,-3.51041666734946,
1.06466310670085)) ;
#125878 = CARTESIAN_POINT('Ctrl Pts',(-2.60767253158295E-16,-3.46875000068279,
1.41955080893447)) ;
#125879 = CARTESIAN_POINT('Ctrl Pts',(0.614683531249999,-3.42708333401613,
1.06466310670085)) ;
#125880 = CARTESIAN_POINT('Ctrl Pts',(1.2293670625,-3.38541666734946,0.709775404467235)) ;
#125881 = CARTESIAN_POINT('Ctrl Pts',(1.2293670625,-3.34375000068279,0.)) ;
#125882 = CARTESIAN_POINT('Ctrl Pts',(1.2293670625,-3.30208333401613,-0.709775404467235)) ;
#125883 = CARTESIAN_POINT('Ctrl Pts',(0.61468353125,-3.26041666734946,-1.06466310670085)) ;
#125884 = CARTESIAN_POINT('Ctrl Pts',(8.69224177194317E-17,-3.21875000068279,
-1.41955080893447)) ;
#125885 = CARTESIAN_POINT('Ctrl Pts',(-0.61468353125,-3.17708333401613,-1.06466310670085)) ;
#125886 = CARTESIAN_POINT('Ctrl Pts',(-1.2293670625,-3.13541666734946,-0.709775404467235)) ;
#125887 = CARTESIAN_POINT('Ctrl Pts',(-1.2293670625,-3.09375000068279,-1.50554043806781E-16)) ;
#125888 = CARTESIAN_POINT('Ctrl Pts',(-1.2293670625,-3.05208333401613,0.709775404467234)) ;
#125889 = CARTESIAN_POINT('Ctrl Pts',(-0.614683531250001,-3.01041666734946,
1.06466310670085)) ;
#125890 = CARTESIAN_POINT('Ctrl Pts',(-2.60767253158295E-16,-2.96875000068279,
1.41955080893447)) ;
#125891 = CARTESIAN_POINT('Ctrl Pts',(0.614683531249999,-2.92708333401613,
1.06466310670085)) ;
#125892 = CARTESIAN_POINT('Ctrl Pts',(1.2293670625,-2.88541666734946,0.709775404467235)) ;
#125893 = CARTESIAN_POINT('Ctrl Pts',(1.2293670625,-2.84375000068279,0.)) ;
#125894 = CARTESIAN_POINT('Ctrl Pts',(1.2293670625,-2.80208333401613,-0.709775404467235)) ;
#125895 = CARTESIAN_POINT('Ctrl Pts',(0.61468353125,-2.76041666734946,-1.06466310670085)) ;
#125896 = CARTESIAN_POINT('Ctrl Pts',(8.69224177194317E-17,-2.71875000068279,
-1.41955080893447)) ;
#125897 = CARTESIAN_POINT('Ctrl Pts',(-0.61468353125,-2.67708333401613,-1.06466310670085)) ;
#125898 = CARTESIAN_POINT('Ctrl Pts',(-1.2293670625,-2.63541666734946,-0.709775404467235)) ;
#125899 = CARTESIAN_POINT('Ctrl Pts',(-1.2293670625,-2.59375000068279,-1.50554043806781E-16)) ;
#125900 = CARTESIAN_POINT('Ctrl Pts',(-1.2293670625,-2.55208333401612,0.709775404467234)) ;
#125901 = CARTESIAN_POINT('Ctrl Pts',(-0.614683531250001,-2.51041666734946,
1.06466310670085)) ;
#125902 = CARTESIAN_POINT('Ctrl Pts',(-2.60767253158295E-16,-2.46875000068279,
1.41955080893447)) ;
#125903 = CARTESIAN_POINT('Ctrl Pts',(0.614683531249999,-2.42708333401613,
1.06466310670085)) ;
#125904 = CARTESIAN_POINT('Ctrl Pts',(1.2293670625,-2.38541666734946,0.709775404467235)) ;
#125905 = CARTESIAN_POINT('Ctrl Pts',(1.2293670625,-2.34375000068279,0.)) ;
#125906 = CARTESIAN_POINT('Ctrl Pts',(1.2293670625,-2.30208333401613,-0.709775404467235)) ;
#125907 = CARTESIAN_POINT('Ctrl Pts',(0.61468353125,-2.26041666734946,-1.06466310670085)) ;
#125908 = CARTESIAN_POINT('Ctrl Pts',(8.69224177194317E-17,-2.21875000068279,
-1.41955080893447)) ;
#125909 = CARTESIAN_POINT('Ctrl Pts',(-0.61468353125,-2.17708333401613,-1.06466310670085)) ;
#125910 = CARTESIAN_POINT('Ctrl Pts',(-1.2293670625,-2.13541666734946,-0.709775404467235)) ;
#125911 = CARTESIAN_POINT('Ctrl Pts',(-1.2293670625,-2.09375000068279,-1.50554043806781E-16)) ;
#125912 = CARTESIAN_POINT('Ctrl Pts',(-1.2293670625,-2.05208333401613,0.709775404467234)) ;
#125913 = CARTESIAN_POINT('Ctrl Pts',(-0.614683531250001,-2.01041666734946,
1.06466310670085)) ;
#125914 = CARTESIAN_POINT('Ctrl Pts',(-2.60767253158295E-16,-1.96875000068279,
1.41955080893447)) ;
#125915 = CARTESIAN_POINT('Ctrl Pts',(0.614683531249999,-1.92708333401613,
1.06466310670085)) ;
#125916 = CARTESIAN_POINT('Ctrl Pts',(1.2293670625,-1.88541666734946,0.709775404467235)) ;
#125917 = CARTESIAN_POINT('Ctrl Pts',(1.2293670625,-1.84375000068279,0.)) ;
#125918 = CARTESIAN_POINT('Ctrl Pts',(1.2293670625,-1.80208333401612,-0.709775404467235)) ;
#125919 = CARTESIAN_POINT('Ctrl Pts',(0.61468353125,-1.76041666734946,-1.06466310670085)) ;
#125920 = CARTESIAN_POINT('Ctrl Pts',(8.69224177194317E-17,-1.71875000068279,
-1.41955080893447)) ;
#125921 = CARTESIAN_POINT('Ctrl Pts',(-0.61468353125,-1.67708333401613,-1.06466310670085)) ;
#125922 = CARTESIAN_POINT('Ctrl Pts',(-1.2293670625,-1.63541666734946,-0.709775404467235)) ;
#125923 = CARTESIAN_POINT('Ctrl Pts',(-1.2293670625,-1.59375000068279,-1.50554043806781E-16)) ;
#125924 = CARTESIAN_POINT('Ctrl Pts',(-1.2293670625,-1.55208333401613,0.709775404467234)) ;
#125925 = CARTESIAN_POINT('Ctrl Pts',(-0.614683531250001,-1.51041666734946,
1.06466310670085)) ;
#125926 = CARTESIAN_POINT('Ctrl Pts',(-2.60767253158295E-16,-1.46875000068279,
1.41955080893447)) ;
#125927 = CARTESIAN_POINT('Ctrl Pts',(0.614683531249999,-1.42708333401613,
1.06466310670085)) ;
#125928 = CARTESIAN_POINT('Ctrl Pts',(1.2293670625,-1.38541666734946,0.709775404467235)) ;
#125929 = CARTESIAN_POINT('Ctrl Pts',(1.2293670625,-1.34375000068279,0.)) ;
#125930 = CARTESIAN_POINT('Ctrl Pts',(1.2293670625,-1.30208333401613,-0.709775404467235)) ;
#125931 = CARTESIAN_POINT('Ctrl Pts',(0.61468353125,-1.26041666734946,-1.06466310670085)) ;
#125932 = CARTESIAN_POINT('Ctrl Pts',(8.69224177194317E-17,-1.21875000068279,
-1.41955080893447)) ;
#125933 = CARTESIAN_POINT('Ctrl Pts',(-0.61468353125,-1.17708333401613,-1.06466310670085)) ;
#125934 = CARTESIAN_POINT('Ctrl Pts',(-1.2293670625,-1.13541666734946,-0.709775404467235)) ;
#125935 = CARTESIAN_POINT('Ctrl Pts',(-1.2293670625,-1.09375000068279,-1.50554043806781E-16)) ;
#125936 = CARTESIAN_POINT('Ctrl Pts',(-1.2293670625,-1.05208333401613,0.709775404467234)) ;
#125937 = CARTESIAN_POINT('Ctrl Pts',(-0.614683531250001,-1.01041666734946,
1.06466310670085)) ;
#125938 = CARTESIAN_POINT('Ctrl Pts',(-2.60767253158295E-16,-0.968750000682792,
1.41955080893447)) ;
#125939 = CARTESIAN_POINT('Ctrl Pts',(0.614683531249999,-0.927083334016125,
1.06466310670085)) ;
#125940 = CARTESIAN_POINT('Ctrl Pts',(1.2293670625,-0.885416667349459,0.709775404467235)) ;
#125941 = CARTESIAN_POINT('Ctrl Pts',(1.2293670625,-0.843750000682792,0.)) ;
#125942 = CARTESIAN_POINT('Ctrl Pts',(1.2293670625,-0.832318278700032,-0.1947349222577)) ;
#125943 = CARTESIAN_POINT('Ctrl Pts',(1.16918410523995,-0.819406422395166,
-0.37993670843199)) ;
#125944 = CARTESIAN_POINT('Ctrl Pts',(1.50001654048127,-6.50000954965131,
0.)) ;
#125945 = CARTESIAN_POINT('Ctrl Pts',(1.50001654048127,-6.45834288298464,
-0.866034953435751)) ;
#125946 = CARTESIAN_POINT('Ctrl Pts',(0.750008270240635,-6.41667621631797,
-1.29905243015363)) ;
#125947 = CARTESIAN_POINT('Ctrl Pts',(1.06058693367482E-16,-6.37500954965132,
-1.73206990687151)) ;
#125948 = CARTESIAN_POINT('Ctrl Pts',(-0.750008270240634,-6.33334288298464,
-1.29905243015363)) ;
#125949 = CARTESIAN_POINT('Ctrl Pts',(-1.50001654048127,-6.29167621631797,
-0.866034953435752)) ;
#125950 = CARTESIAN_POINT('Ctrl Pts',(-1.50001654048127,-6.25000954965131,
-1.83699045496847E-16)) ;
#125951 = CARTESIAN_POINT('Ctrl Pts',(-1.50001654048127,-6.20834288298464,
0.866034953435751)) ;
#125952 = CARTESIAN_POINT('Ctrl Pts',(-0.750008270240635,-6.16667621631797,
1.29905243015363)) ;
#125953 = CARTESIAN_POINT('Ctrl Pts',(-3.18176080102445E-16,-6.1250095496513,
1.73206990687151)) ;
#125954 = CARTESIAN_POINT('Ctrl Pts',(0.750008270240633,-6.08334288298464,
1.29905243015363)) ;
#125955 = CARTESIAN_POINT('Ctrl Pts',(1.50001654048127,-6.04167621631797,
0.866034953435752)) ;
#125956 = CARTESIAN_POINT('Ctrl Pts',(1.50001654048127,-6.00000954965131,
0.)) ;
#125957 = CARTESIAN_POINT('Ctrl Pts',(1.50001654048127,-5.95834288298464,
-0.866034953435751)) ;
#125958 = CARTESIAN_POINT('Ctrl Pts',(0.750008270240635,-5.91667621631797,
-1.29905243015363)) ;
#125959 = CARTESIAN_POINT('Ctrl Pts',(1.06058693367482E-16,-5.87500954965131,
-1.73206990687151)) ;
#125960 = CARTESIAN_POINT('Ctrl Pts',(-0.750008270240634,-5.83334288298464,
-1.29905243015363)) ;
#125961 = CARTESIAN_POINT('Ctrl Pts',(-1.50001654048127,-5.79167621631797,
-0.866034953435752)) ;
#125962 = CARTESIAN_POINT('Ctrl Pts',(-1.50001654048127,-5.75000954965131,
-1.83699045496847E-16)) ;
#125963 = CARTESIAN_POINT('Ctrl Pts',(-1.50001654048127,-5.70834288298464,
0.866034953435751)) ;
#125964 = CARTESIAN_POINT('Ctrl Pts',(-0.750008270240635,-5.66667621631797,
1.29905243015363)) ;
#125965 = CARTESIAN_POINT('Ctrl Pts',(-3.18176080102445E-16,-5.62500954965131,
1.73206990687151)) ;
#125966 = CARTESIAN_POINT('Ctrl Pts',(0.750008270240633,-5.58334288298464,
1.29905243015363)) ;
#125967 = CARTESIAN_POINT('Ctrl Pts',(1.50001654048127,-5.54167621631797,
0.866034953435752)) ;
#125968 = CARTESIAN_POINT('Ctrl Pts',(1.50001654048127,-5.50000954965131,
0.)) ;
#125969 = CARTESIAN_POINT('Ctrl Pts',(1.50001654048127,-5.45834288298464,
-0.866034953435751)) ;
#125970 = CARTESIAN_POINT('Ctrl Pts',(0.750008270240635,-5.41667621631797,
-1.29905243015363)) ;
#125971 = CARTESIAN_POINT('Ctrl Pts',(1.06058693367482E-16,-5.37500954965131,
-1.73206990687151)) ;
#125972 = CARTESIAN_POINT('Ctrl Pts',(-0.750008270240634,-5.33334288298464,
-1.29905243015363)) ;
#125973 = CARTESIAN_POINT('Ctrl Pts',(-1.50001654048127,-5.29167621631797,
-0.866034953435752)) ;
#125974 = CARTESIAN_POINT('Ctrl Pts',(-1.50001654048127,-5.25000954965131,
-1.83699045496847E-16)) ;
#125975 = CARTESIAN_POINT('Ctrl Pts',(-1.50001654048127,-5.20834288298464,
0.866034953435751)) ;
#125976 = CARTESIAN_POINT('Ctrl Pts',(-0.750008270240635,-5.16667621631797,
1.29905243015363)) ;
#125977 = CARTESIAN_POINT('Ctrl Pts',(-3.18176080102445E-16,-5.12500954965131,
1.73206990687151)) ;
#125978 = CARTESIAN_POINT('Ctrl Pts',(0.750008270240633,-5.08334288298464,
1.29905243015363)) ;
#125979 = CARTESIAN_POINT('Ctrl Pts',(1.50001654048127,-5.04167621631797,
0.866034953435752)) ;
#125980 = CARTESIAN_POINT('Ctrl Pts',(1.50001654048127,-5.00000954965131,
0.)) ;
#125981 = CARTESIAN_POINT('Ctrl Pts',(1.50001654048127,-4.95834288298464,
-0.866034953435751)) ;
#125982 = CARTESIAN_POINT('Ctrl Pts',(0.750008270240635,-4.91667621631797,
-1.29905243015363)) ;
#125983 = CARTESIAN_POINT('Ctrl Pts',(1.06058693367482E-16,-4.87500954965131,
-1.73206990687151)) ;
#125984 = CARTESIAN_POINT('Ctrl Pts',(-0.750008270240634,-4.83334288298464,
-1.29905243015363)) ;
#125985 = CARTESIAN_POINT('Ctrl Pts',(-1.50001654048127,-4.79167621631797,
-0.866034953435752)) ;
#125986 = CARTESIAN_POINT('Ctrl Pts',(-1.50001654048127,-4.75000954965131,
-1.83699045496847E-16)) ;
#125987 = CARTESIAN_POINT('Ctrl Pts',(-1.50001654048127,-4.70834288298464,
0.866034953435751)) ;
#125988 = CARTESIAN_POINT('Ctrl Pts',(-0.750008270240635,-4.66667621631797,
1.29905243015363)) ;
#125989 = CARTESIAN_POINT('Ctrl Pts',(-3.18176080102445E-16,-4.62500954965131,
1.73206990687151)) ;
#125990 = CARTESIAN_POINT('Ctrl Pts',(0.750008270240633,-4.58334288298464,
1.29905243015363)) ;
#125991 = CARTESIAN_POINT('Ctrl Pts',(1.50001654048127,-4.54167621631797,
0.866034953435752)) ;
#125992 = CARTESIAN_POINT('Ctrl Pts',(1.50001654048127,-4.50000954965131,
0.)) ;
#125993 = CARTESIAN_POINT('Ctrl Pts',(1.50001654048127,-4.45834288298464,
-0.866034953435751)) ;
#125994 = CARTESIAN_POINT('Ctrl Pts',(0.750008270240635,-4.41667621631797,
-1.29905243015363)) ;
#125995 = CARTESIAN_POINT('Ctrl Pts',(1.06058693367482E-16,-4.37500954965131,
-1.73206990687151)) ;
#125996 = CARTESIAN_POINT('Ctrl Pts',(-0.750008270240634,-4.33334288298464,
-1.29905243015363)) ;
#125997 = CARTESIAN_POINT('Ctrl Pts',(-1.50001654048127,-4.29167621631797,
-0.866034953435752)) ;
#125998 = CARTESIAN_POINT('Ctrl Pts',(-1.50001654048127,-4.2500095496513,
-1.83699045496847E-16)) ;
#125999 = CARTESIAN_POINT('Ctrl Pts',(-1.50001654048127,-4.20834288298464,
0.866034953435751)) ;
#126000 = CARTESIAN_POINT('Ctrl Pts',(-0.750008270240635,-4.16667621631797,
1.29905243015363)) ;
#126001 = CARTESIAN_POINT('Ctrl Pts',(-3.18176080102445E-16,-4.12500954965131,
1.73206990687151)) ;
#126002 = CARTESIAN_POINT('Ctrl Pts',(0.750008270240633,-4.08334288298464,
1.29905243015363)) ;
#126003 = CARTESIAN_POINT('Ctrl Pts',(1.50001654048127,-4.04167621631797,
0.866034953435752)) ;
#126004 = CARTESIAN_POINT('Ctrl Pts',(1.50001654048127,-4.0000095496513,0.)) ;
#126005 = CARTESIAN_POINT('Ctrl Pts',(1.50001654048127,-3.95834288298464,
-0.866034953435751)) ;
#126006 = CARTESIAN_POINT('Ctrl Pts',(0.750008270240635,-3.91667621631797,
-1.29905243015363)) ;
#126007 = CARTESIAN_POINT('Ctrl Pts',(1.06058693367482E-16,-3.87500954965131,
-1.73206990687151)) ;
#126008 = CARTESIAN_POINT('Ctrl Pts',(-0.750008270240634,-3.83334288298464,
-1.29905243015363)) ;
#126009 = CARTESIAN_POINT('Ctrl Pts',(-1.50001654048127,-3.79167621631797,
-0.866034953435752)) ;
#126010 = CARTESIAN_POINT('Ctrl Pts',(-1.50001654048127,-3.7500095496513,
-1.83699045496847E-16)) ;
#126011 = CARTESIAN_POINT('Ctrl Pts',(-1.50001654048127,-3.70834288298464,
0.866034953435751)) ;
#126012 = CARTESIAN_POINT('Ctrl Pts',(-0.750008270240635,-3.66667621631797,
1.29905243015363)) ;
#126013 = CARTESIAN_POINT('Ctrl Pts',(-3.18176080102445E-16,-3.62500954965131,
1.73206990687151)) ;
#126014 = CARTESIAN_POINT('Ctrl Pts',(0.750008270240633,-3.58334288298464,
1.29905243015363)) ;
#126015 = CARTESIAN_POINT('Ctrl Pts',(1.50001654048127,-3.54167621631797,
0.866034953435752)) ;
#126016 = CARTESIAN_POINT('Ctrl Pts',(1.50001654048127,-3.50000954965131,
0.)) ;
#126017 = CARTESIAN_POINT('Ctrl Pts',(1.50001654048127,-3.45834288298464,
-0.866034953435751)) ;
#126018 = CARTESIAN_POINT('Ctrl Pts',(0.750008270240635,-3.41667621631797,
-1.29905243015363)) ;
#126019 = CARTESIAN_POINT('Ctrl Pts',(1.06058693367482E-16,-3.3750095496513,
-1.73206990687151)) ;
#126020 = CARTESIAN_POINT('Ctrl Pts',(-0.750008270240634,-3.33334288298464,
-1.29905243015363)) ;
#126021 = CARTESIAN_POINT('Ctrl Pts',(-1.50001654048127,-3.29167621631797,
-0.866034953435752)) ;
#126022 = CARTESIAN_POINT('Ctrl Pts',(-1.50001654048127,-3.2500095496513,
-1.83699045496847E-16)) ;
#126023 = CARTESIAN_POINT('Ctrl Pts',(-1.50001654048127,-3.20834288298464,
0.866034953435751)) ;
#126024 = CARTESIAN_POINT('Ctrl Pts',(-0.750008270240635,-3.16667621631797,
1.29905243015363)) ;
#126025 = CARTESIAN_POINT('Ctrl Pts',(-3.18176080102445E-16,-3.12500954965131,
1.73206990687151)) ;
#126026 = CARTESIAN_POINT('Ctrl Pts',(0.750008270240633,-3.08334288298464,
1.29905243015363)) ;
#126027 = CARTESIAN_POINT('Ctrl Pts',(1.50001654048127,-3.04167621631797,
0.866034953435752)) ;
#126028 = CARTESIAN_POINT('Ctrl Pts',(1.50001654048127,-3.0000095496513,0.)) ;
#126029 = CARTESIAN_POINT('Ctrl Pts',(1.50001654048127,-2.95834288298464,
-0.866034953435751)) ;
#126030 = CARTESIAN_POINT('Ctrl Pts',(0.750008270240635,-2.91667621631797,
-1.29905243015363)) ;
#126031 = CARTESIAN_POINT('Ctrl Pts',(1.06058693367482E-16,-2.87500954965131,
-1.73206990687151)) ;
#126032 = CARTESIAN_POINT('Ctrl Pts',(-0.750008270240634,-2.83334288298464,
-1.29905243015363)) ;
#126033 = CARTESIAN_POINT('Ctrl Pts',(-1.50001654048127,-2.79167621631797,
-0.866034953435752)) ;
#126034 = CARTESIAN_POINT('Ctrl Pts',(-1.50001654048127,-2.75000954965131,
-1.83699045496847E-16)) ;
#126035 = CARTESIAN_POINT('Ctrl Pts',(-1.50001654048127,-2.70834288298464,
0.866034953435751)) ;
#126036 = CARTESIAN_POINT('Ctrl Pts',(-0.750008270240635,-2.66667621631797,
1.29905243015363)) ;
#126037 = CARTESIAN_POINT('Ctrl Pts',(-3.18176080102445E-16,-2.6250095496513,
1.73206990687151)) ;
#126038 = CARTESIAN_POINT('Ctrl Pts',(0.750008270240633,-2.58334288298464,
1.29905243015363)) ;
#126039 = CARTESIAN_POINT('Ctrl Pts',(1.50001654048127,-2.54167621631797,
0.866034953435752)) ;
#126040 = CARTESIAN_POINT('Ctrl Pts',(1.50001654048127,-2.5000095496513,0.)) ;
#126041 = CARTESIAN_POINT('Ctrl Pts',(1.50001654048127,-2.45834288298464,
-0.866034953435751)) ;
#126042 = CARTESIAN_POINT('Ctrl Pts',(0.750008270240635,-2.41667621631797,
-1.29905243015363)) ;
#126043 = CARTESIAN_POINT('Ctrl Pts',(1.06058693367482E-16,-2.3750095496513,
-1.73206990687151)) ;
#126044 = CARTESIAN_POINT('Ctrl Pts',(-0.750008270240634,-2.33334288298464,
-1.29905243015363)) ;
#126045 = CARTESIAN_POINT('Ctrl Pts',(-1.50001654048127,-2.29167621631797,
-0.866034953435752)) ;
#126046 = CARTESIAN_POINT('Ctrl Pts',(-1.50001654048127,-2.25000954965131,
-1.83699045496847E-16)) ;
#126047 = CARTESIAN_POINT('Ctrl Pts',(-1.50001654048127,-2.20834288298464,
0.866034953435751)) ;
#126048 = CARTESIAN_POINT('Ctrl Pts',(-0.750008270240635,-2.16667621631797,
1.29905243015363)) ;
#126049 = CARTESIAN_POINT('Ctrl Pts',(-3.18176080102445E-16,-2.12500954965131,
1.73206990687151)) ;
#126050 = CARTESIAN_POINT('Ctrl Pts',(0.750008270240633,-2.08334288298464,
1.29905243015363)) ;
#126051 = CARTESIAN_POINT('Ctrl Pts',(1.50001654048127,-2.04167621631797,
0.866034953435752)) ;
#126052 = CARTESIAN_POINT('Ctrl Pts',(1.50001654048127,-2.00000954965131,
0.)) ;
#126053 = CARTESIAN_POINT('Ctrl Pts',(1.50001654048127,-1.95834288298464,
-0.866034953435751)) ;
#126054 = CARTESIAN_POINT('Ctrl Pts',(0.750008270240635,-1.91667621631797,
-1.29905243015363)) ;
#126055 = CARTESIAN_POINT('Ctrl Pts',(1.06058693367482E-16,-1.8750095496513,
-1.73206990687151)) ;
#126056 = CARTESIAN_POINT('Ctrl Pts',(-0.750008270240634,-1.83334288298464,
-1.29905243015363)) ;
#126057 = CARTESIAN_POINT('Ctrl Pts',(-1.50001654048127,-1.79167621631797,
-0.866034953435752)) ;
#126058 = CARTESIAN_POINT('Ctrl Pts',(-1.50001654048127,-1.75000954965131,
-1.83699045496847E-16)) ;
#126059 = CARTESIAN_POINT('Ctrl Pts',(-1.50001654048127,-1.70834288298464,
0.866034953435751)) ;
#126060 = CARTESIAN_POINT('Ctrl Pts',(-0.750008270240635,-1.66667621631797,
1.29905243015363)) ;
#126061 = CARTESIAN_POINT('Ctrl Pts',(-3.18176080102445E-16,-1.6250095496513,
1.73206990687151)) ;
#126062 = CARTESIAN_POINT('Ctrl Pts',(0.750008270240633,-1.58334288298464,
1.29905243015363)) ;
#126063 = CARTESIAN_POINT('Ctrl Pts',(1.50001654048127,-1.54167621631797,
0.866034953435752)) ;
#126064 = CARTESIAN_POINT('Ctrl Pts',(1.50001654048127,-1.5000095496513,0.)) ;
#126065 = CARTESIAN_POINT('Ctrl Pts',(1.50001654048127,-1.45834288298464,
-0.866034953435751)) ;
#126066 = CARTESIAN_POINT('Ctrl Pts',(0.750008270240635,-1.41667621631797,
-1.29905243015363)) ;
#126067 = CARTESIAN_POINT('Ctrl Pts',(1.06058693367482E-16,-1.3750095496513,
-1.73206990687151)) ;
#126068 = CARTESIAN_POINT('Ctrl Pts',(-0.750008270240634,-1.33334288298464,
-1.29905243015363)) ;
#126069 = CARTESIAN_POINT('Ctrl Pts',(-1.50001654048127,-1.29167621631797,
-0.866034953435752)) ;
#126070 = CARTESIAN_POINT('Ctrl Pts',(-1.50001654048127,-1.25000954965131,
-1.83699045496847E-16)) ;
#126071 = CARTESIAN_POINT('Ctrl Pts',(-1.50001654048127,-1.20834288298464,
0.866034953435751)) ;
#126072 = CARTESIAN_POINT('Ctrl Pts',(-0.750008270240635,-1.16667621631797,
1.29905243015363)) ;
#126073 = CARTESIAN_POINT('Ctrl Pts',(-3.18176080102445E-16,-1.12500954965131,
1.73206990687151)) ;
#126074 = CARTESIAN_POINT('Ctrl Pts',(0.750008270240633,-1.08334288298464,
1.29905243015363)) ;
#126075 = CARTESIAN_POINT('Ctrl Pts',(1.50001654048127,-1.04167621631797,
0.866034953435752)) ;
#126076 = CARTESIAN_POINT('Ctrl Pts',(1.50001654048127,-1.00000954965131,
0.)) ;
#126077 = CARTESIAN_POINT('Ctrl Pts',(1.50001654048127,-0.988577827668548,
-0.237606499560732)) ;
#126078 = CARTESIAN_POINT('Ctrl Pts',(1.42658409373784,-0.975665971363682,
-0.46358110963624)) ;
#126079 = CARTESIAN_POINT('',(1.42658067231545,-0.975658586206325,-0.463538116421941)) ;
#126080 = CARTESIAN_POINT('Ctrl Pts',(1.5,-6.06250000136559,0.)) ;
#126081 = CARTESIAN_POINT('Ctrl Pts',(1.5,-6.02083333469892,-0.866025403784439)) ;
#126082 = CARTESIAN_POINT('Ctrl Pts',(0.75,-5.97916666803226,-1.29903810567666)) ;
#126083 = CARTESIAN_POINT('Ctrl Pts',(1.06057523872491E-16,-5.93750000136559,
-1.73205080756888)) ;
#126084 = CARTESIAN_POINT('Ctrl Pts',(-0.75,-5.89583333469892,-1.29903810567666)) ;
#126085 = CARTESIAN_POINT('Ctrl Pts',(-1.5,-5.85416666803226,-0.866025403784439)) ;
#126086 = CARTESIAN_POINT('Ctrl Pts',(-1.5,-5.81250000136559,-1.83697019872103E-16)) ;
#126087 = CARTESIAN_POINT('Ctrl Pts',(-1.5,-5.77083333469892,0.866025403784438)) ;
#126088 = CARTESIAN_POINT('Ctrl Pts',(-0.750000000000001,-5.72916666803226,
1.29903810567666)) ;
#126089 = CARTESIAN_POINT('Ctrl Pts',(-3.18172571617472E-16,-5.68750000136559,
1.73205080756888)) ;
#126090 = CARTESIAN_POINT('Ctrl Pts',(0.749999999999999,-5.64583333469892,
1.29903810567666)) ;
#126091 = CARTESIAN_POINT('Ctrl Pts',(1.5,-5.60416666803226,0.86602540378444)) ;
#126092 = CARTESIAN_POINT('Ctrl Pts',(1.5,-5.56250000136559,0.)) ;
#126093 = CARTESIAN_POINT('Ctrl Pts',(1.5,-5.52083333469892,-0.866025403784439)) ;
#126094 = CARTESIAN_POINT('Ctrl Pts',(0.75,-5.47916666803226,-1.29903810567666)) ;
#126095 = CARTESIAN_POINT('Ctrl Pts',(1.06057523872491E-16,-5.43750000136559,
-1.73205080756888)) ;
#126096 = CARTESIAN_POINT('Ctrl Pts',(-0.75,-5.39583333469892,-1.29903810567666)) ;
#126097 = CARTESIAN_POINT('Ctrl Pts',(-1.5,-5.35416666803226,-0.866025403784439)) ;
#126098 = CARTESIAN_POINT('Ctrl Pts',(-1.5,-5.31250000136559,-1.83697019872103E-16)) ;
#126099 = CARTESIAN_POINT('Ctrl Pts',(-1.5,-5.27083333469892,0.866025403784438)) ;
#126100 = CARTESIAN_POINT('Ctrl Pts',(-0.750000000000001,-5.22916666803225,
1.29903810567666)) ;
#126101 = CARTESIAN_POINT('Ctrl Pts',(-3.18172571617472E-16,-5.18750000136559,
1.73205080756888)) ;
#126102 = CARTESIAN_POINT('Ctrl Pts',(0.749999999999999,-5.14583333469892,
1.29903810567666)) ;
#126103 = CARTESIAN_POINT('Ctrl Pts',(1.5,-5.10416666803225,0.86602540378444)) ;
#126104 = CARTESIAN_POINT('Ctrl Pts',(1.5,-5.06250000136559,0.)) ;
#126105 = CARTESIAN_POINT('Ctrl Pts',(1.5,-5.02083333469892,-0.866025403784439)) ;
#126106 = CARTESIAN_POINT('Ctrl Pts',(0.75,-4.97916666803225,-1.29903810567666)) ;
#126107 = CARTESIAN_POINT('Ctrl Pts',(1.06057523872491E-16,-4.93750000136559,
-1.73205080756888)) ;
#126108 = CARTESIAN_POINT('Ctrl Pts',(-0.75,-4.89583333469892,-1.29903810567666)) ;
#126109 = CARTESIAN_POINT('Ctrl Pts',(-1.5,-4.85416666803226,-0.866025403784439)) ;
#126110 = CARTESIAN_POINT('Ctrl Pts',(-1.5,-4.81250000136559,-1.83697019872103E-16)) ;
#126111 = CARTESIAN_POINT('Ctrl Pts',(-1.5,-4.77083333469892,0.866025403784438)) ;
#126112 = CARTESIAN_POINT('Ctrl Pts',(-0.750000000000001,-4.72916666803226,
1.29903810567666)) ;
#126113 = CARTESIAN_POINT('Ctrl Pts',(-3.18172571617472E-16,-4.68750000136559,
1.73205080756888)) ;
#126114 = CARTESIAN_POINT('Ctrl Pts',(0.749999999999999,-4.64583333469892,
1.29903810567666)) ;
#126115 = CARTESIAN_POINT('Ctrl Pts',(1.5,-4.60416666803225,0.86602540378444)) ;
#126116 = CARTESIAN_POINT('Ctrl Pts',(1.5,-4.56250000136559,0.)) ;
#126117 = CARTESIAN_POINT('Ctrl Pts',(1.5,-4.52083333469892,-0.866025403784439)) ;
#126118 = CARTESIAN_POINT('Ctrl Pts',(0.75,-4.47916666803226,-1.29903810567666)) ;
#126119 = CARTESIAN_POINT('Ctrl Pts',(1.06057523872491E-16,-4.43750000136559,
-1.73205080756888)) ;
#126120 = CARTESIAN_POINT('Ctrl Pts',(-0.75,-4.39583333469892,-1.29903810567666)) ;
#126121 = CARTESIAN_POINT('Ctrl Pts',(-1.5,-4.35416666803225,-0.866025403784439)) ;
#126122 = CARTESIAN_POINT('Ctrl Pts',(-1.5,-4.31250000136559,-1.83697019872103E-16)) ;
#126123 = CARTESIAN_POINT('Ctrl Pts',(-1.5,-4.27083333469892,0.866025403784438)) ;
#126124 = CARTESIAN_POINT('Ctrl Pts',(-0.750000000000001,-4.22916666803225,
1.29903810567666)) ;
#126125 = CARTESIAN_POINT('Ctrl Pts',(-3.18172571617472E-16,-4.18750000136559,
1.73205080756888)) ;
#126126 = CARTESIAN_POINT('Ctrl Pts',(0.749999999999999,-4.14583333469892,
1.29903810567666)) ;
#126127 = CARTESIAN_POINT('Ctrl Pts',(1.5,-4.10416666803226,0.86602540378444)) ;
#126128 = CARTESIAN_POINT('Ctrl Pts',(1.5,-4.06250000136559,0.)) ;
#126129 = CARTESIAN_POINT('Ctrl Pts',(1.5,-4.02083333469892,-0.866025403784439)) ;
#126130 = CARTESIAN_POINT('Ctrl Pts',(0.75,-3.97916666803226,-1.29903810567666)) ;
#126131 = CARTESIAN_POINT('Ctrl Pts',(1.06057523872491E-16,-3.93750000136559,
-1.73205080756888)) ;
#126132 = CARTESIAN_POINT('Ctrl Pts',(-0.75,-3.89583333469892,-1.29903810567666)) ;
#126133 = CARTESIAN_POINT('Ctrl Pts',(-1.5,-3.85416666803226,-0.866025403784439)) ;
#126134 = CARTESIAN_POINT('Ctrl Pts',(-1.5,-3.81250000136559,-1.83697019872103E-16)) ;
#126135 = CARTESIAN_POINT('Ctrl Pts',(-1.5,-3.77083333469892,0.866025403784438)) ;
#126136 = CARTESIAN_POINT('Ctrl Pts',(-0.750000000000001,-3.72916666803226,
1.29903810567666)) ;
#126137 = CARTESIAN_POINT('Ctrl Pts',(-3.18172571617472E-16,-3.68750000136559,
1.73205080756888)) ;
#126138 = CARTESIAN_POINT('Ctrl Pts',(0.749999999999999,-3.64583333469892,
1.29903810567666)) ;
#126139 = CARTESIAN_POINT('Ctrl Pts',(1.5,-3.60416666803226,0.86602540378444)) ;
#126140 = CARTESIAN_POINT('Ctrl Pts',(1.5,-3.56250000136559,0.)) ;
#126141 = CARTESIAN_POINT('Ctrl Pts',(1.5,-3.52083333469892,-0.866025403784439)) ;
#126142 = CARTESIAN_POINT('Ctrl Pts',(0.75,-3.47916666803226,-1.29903810567666)) ;
#126143 = CARTESIAN_POINT('Ctrl Pts',(1.06057523872491E-16,-3.43750000136559,
-1.73205080756888)) ;
#126144 = CARTESIAN_POINT('Ctrl Pts',(-0.75,-3.39583333469892,-1.29903810567666)) ;
#126145 = CARTESIAN_POINT('Ctrl Pts',(-1.5,-3.35416666803225,-0.866025403784439)) ;
#126146 = CARTESIAN_POINT('Ctrl Pts',(-1.5,-3.31250000136559,-1.83697019872103E-16)) ;
#126147 = CARTESIAN_POINT('Ctrl Pts',(-1.5,-3.27083333469892,0.866025403784438)) ;
#126148 = CARTESIAN_POINT('Ctrl Pts',(-0.750000000000001,-3.22916666803226,
1.29903810567666)) ;
#126149 = CARTESIAN_POINT('Ctrl Pts',(-3.18172571617472E-16,-3.18750000136559,
1.73205080756888)) ;
#126150 = CARTESIAN_POINT('Ctrl Pts',(0.749999999999999,-3.14583333469892,
1.29903810567666)) ;
#126151 = CARTESIAN_POINT('Ctrl Pts',(1.5,-3.10416666803226,0.86602540378444)) ;
#126152 = CARTESIAN_POINT('Ctrl Pts',(1.5,-3.06250000136559,0.)) ;
#126153 = CARTESIAN_POINT('Ctrl Pts',(1.5,-3.02083333469892,-0.866025403784439)) ;
#126154 = CARTESIAN_POINT('Ctrl Pts',(0.75,-2.97916666803226,-1.29903810567666)) ;
#126155 = CARTESIAN_POINT('Ctrl Pts',(1.06057523872491E-16,-2.93750000136559,
-1.73205080756888)) ;
#126156 = CARTESIAN_POINT('Ctrl Pts',(-0.75,-2.89583333469892,-1.29903810567666)) ;
#126157 = CARTESIAN_POINT('Ctrl Pts',(-1.5,-2.85416666803226,-0.866025403784439)) ;
#126158 = CARTESIAN_POINT('Ctrl Pts',(-1.5,-2.81250000136559,-1.83697019872103E-16)) ;
#126159 = CARTESIAN_POINT('Ctrl Pts',(-1.5,-2.77083333469892,0.866025403784438)) ;
#126160 = CARTESIAN_POINT('Ctrl Pts',(-0.750000000000001,-2.72916666803226,
1.29903810567666)) ;
#126161 = CARTESIAN_POINT('Ctrl Pts',(-3.18172571617472E-16,-2.68750000136559,
1.73205080756888)) ;
#126162 = CARTESIAN_POINT('Ctrl Pts',(0.749999999999999,-2.64583333469892,
1.29903810567666)) ;
#126163 = CARTESIAN_POINT('Ctrl Pts',(1.5,-2.60416666803226,0.86602540378444)) ;
#126164 = CARTESIAN_POINT('Ctrl Pts',(1.5,-2.56250000136559,0.)) ;
#126165 = CARTESIAN_POINT('Ctrl Pts',(1.5,-2.52083333469892,-0.866025403784439)) ;
#126166 = CARTESIAN_POINT('Ctrl Pts',(0.75,-2.47916666803226,-1.29903810567666)) ;
#126167 = CARTESIAN_POINT('Ctrl Pts',(1.06057523872491E-16,-2.43750000136559,
-1.73205080756888)) ;
#126168 = CARTESIAN_POINT('Ctrl Pts',(-0.75,-2.39583333469892,-1.29903810567666)) ;
#126169 = CARTESIAN_POINT('Ctrl Pts',(-1.5,-2.35416666803226,-0.866025403784439)) ;
#126170 = CARTESIAN_POINT('Ctrl Pts',(-1.5,-2.31250000136559,-1.83697019872103E-16)) ;
#126171 = CARTESIAN_POINT('Ctrl Pts',(-1.5,-2.27083333469892,0.866025403784438)) ;
#126172 = CARTESIAN_POINT('Ctrl Pts',(-0.750000000000001,-2.22916666803226,
1.29903810567666)) ;
#126173 = CARTESIAN_POINT('Ctrl Pts',(-3.18172571617472E-16,-2.18750000136559,
1.73205080756888)) ;
#126174 = CARTESIAN_POINT('Ctrl Pts',(0.749999999999999,-2.14583333469892,
1.29903810567666)) ;
#126175 = CARTESIAN_POINT('Ctrl Pts',(1.5,-2.10416666803226,0.86602540378444)) ;
#126176 = CARTESIAN_POINT('Ctrl Pts',(1.5,-2.06250000136559,0.)) ;
#126177 = CARTESIAN_POINT('Ctrl Pts',(1.5,-2.02083333469892,-0.866025403784439)) ;
#126178 = CARTESIAN_POINT('Ctrl Pts',(0.75,-1.97916666803226,-1.29903810567666)) ;
#126179 = CARTESIAN_POINT('Ctrl Pts',(1.06057523872491E-16,-1.93750000136559,
-1.73205080756888)) ;
#126180 = CARTESIAN_POINT('Ctrl Pts',(-0.75,-1.89583333469892,-1.29903810567666)) ;
#126181 = CARTESIAN_POINT('Ctrl Pts',(-1.5,-1.85416666803226,-0.866025403784439)) ;
#126182 = CARTESIAN_POINT('Ctrl Pts',(-1.5,-1.81250000136559,-1.83697019872103E-16)) ;
#126183 = CARTESIAN_POINT('Ctrl Pts',(-1.5,-1.77083333469892,0.866025403784438)) ;
#126184 = CARTESIAN_POINT('Ctrl Pts',(-0.750000000000001,-1.72916666803226,
1.29903810567666)) ;
#126185 = CARTESIAN_POINT('Ctrl Pts',(-3.18172571617472E-16,-1.68750000136559,
1.73205080756888)) ;
#126186 = CARTESIAN_POINT('Ctrl Pts',(0.749999999999999,-1.64583333469892,
1.29903810567666)) ;
#126187 = CARTESIAN_POINT('Ctrl Pts',(1.5,-1.60416666803226,0.86602540378444)) ;
#126188 = CARTESIAN_POINT('Ctrl Pts',(1.5,-1.56250000136559,0.)) ;
#126189 = CARTESIAN_POINT('Ctrl Pts',(1.5,-1.52083333469892,-0.866025403784439)) ;
#126190 = CARTESIAN_POINT('Ctrl Pts',(0.75,-1.47916666803226,-1.29903810567666)) ;
#126191 = CARTESIAN_POINT('Ctrl Pts',(1.06057523872491E-16,-1.43750000136559,
-1.73205080756888)) ;
#126192 = CARTESIAN_POINT('Ctrl Pts',(-0.75,-1.39583333469892,-1.29903810567666)) ;
#126193 = CARTESIAN_POINT('Ctrl Pts',(-1.5,-1.35416666803225,-0.866025403784439)) ;
#126194 = CARTESIAN_POINT('Ctrl Pts',(-1.5,-1.31250000136559,-1.83697019872103E-16)) ;
#126195 = CARTESIAN_POINT('Ctrl Pts',(-1.5,-1.27083333469892,0.866025403784438)) ;
#126196 = CARTESIAN_POINT('Ctrl Pts',(-0.750000000000001,-1.22916666803226,
1.29903810567666)) ;
#126197 = CARTESIAN_POINT('Ctrl Pts',(-3.18172571617472E-16,-1.18750000136559,
1.73205080756888)) ;
#126198 = CARTESIAN_POINT('Ctrl Pts',(0.749999999999999,-1.14583333469892,
1.29903810567666)) ;
#126199 = CARTESIAN_POINT('Ctrl Pts',(1.5,-1.10416666803226,0.86602540378444)) ;
#126200 = CARTESIAN_POINT('Ctrl Pts',(1.5,-1.06250000136559,0.)) ;
#126201 = CARTESIAN_POINT('Ctrl Pts',(1.5,-1.02083333469892,-0.866025403784439)) ;
#126202 = CARTESIAN_POINT('Ctrl Pts',(0.75,-0.979166668032255,-1.29903810567666)) ;
#126203 = CARTESIAN_POINT('Ctrl Pts',(1.06057523872491E-16,-0.937500001365588,
-1.73205080756888)) ;
#126204 = CARTESIAN_POINT('Ctrl Pts',(-0.75,-0.895833334698922,-1.29903810567666)) ;
#126205 = CARTESIAN_POINT('Ctrl Pts',(-1.5,-0.854166668032255,-0.866025403784439)) ;
#126206 = CARTESIAN_POINT('Ctrl Pts',(-1.5,-0.812500001365589,-1.83697019872103E-16)) ;
#126207 = CARTESIAN_POINT('Ctrl Pts',(-1.5,-0.770833334698922,0.866025403784438)) ;
#126208 = CARTESIAN_POINT('Ctrl Pts',(-0.750000000000001,-0.729166668032255,
1.29903810567666)) ;
#126209 = CARTESIAN_POINT('Ctrl Pts',(-3.18172571617472E-16,-0.687500001365589,
1.73205080756888)) ;
#126210 = CARTESIAN_POINT('Ctrl Pts',(0.749999999999999,-0.645833334698922,
1.29903810567666)) ;
#126211 = CARTESIAN_POINT('Ctrl Pts',(1.5,-0.604166668032255,0.86602540378444)) ;
#126212 = CARTESIAN_POINT('Ctrl Pts',(1.5,-0.562500001365589,0.)) ;
#126213 = CARTESIAN_POINT('Ctrl Pts',(1.5,-0.551068708039016,-0.237594970054175)) ;
#126214 = CARTESIAN_POINT('Ctrl Pts',(1.42657373504468,-0.538157367689847,
-0.463559465959517)) ;
#126215 = CARTESIAN_POINT('Ctrl Pts',(1.2293670625,-6.21875000068279,0.)) ;
#126216 = CARTESIAN_POINT('Ctrl Pts',(1.2293670625,-6.17708333401612,-0.709775404467235)) ;
#126217 = CARTESIAN_POINT('Ctrl Pts',(0.61468353125,-6.13541666734946,-1.06466310670085)) ;
#126218 = CARTESIAN_POINT('Ctrl Pts',(8.69224177194317E-17,-6.09375000068279,
-1.41955080893447)) ;
#126219 = CARTESIAN_POINT('Ctrl Pts',(-0.61468353125,-6.05208333401613,-1.06466310670085)) ;
#126220 = CARTESIAN_POINT('Ctrl Pts',(-1.2293670625,-6.01041666734946,-0.709775404467235)) ;
#126221 = CARTESIAN_POINT('Ctrl Pts',(-1.2293670625,-5.96875000068279,-1.50554043806781E-16)) ;
#126222 = CARTESIAN_POINT('Ctrl Pts',(-1.2293670625,-5.92708333401613,0.709775404467234)) ;
#126223 = CARTESIAN_POINT('Ctrl Pts',(-0.614683531250001,-5.88541666734946,
1.06466310670085)) ;
#126224 = CARTESIAN_POINT('Ctrl Pts',(-2.60767253158295E-16,-5.84375000068279,
1.41955080893447)) ;
#126225 = CARTESIAN_POINT('Ctrl Pts',(0.614683531249999,-5.80208333401612,
1.06466310670085)) ;
#126226 = CARTESIAN_POINT('Ctrl Pts',(1.2293670625,-5.76041666734946,0.709775404467235)) ;
#126227 = CARTESIAN_POINT('Ctrl Pts',(1.2293670625,-5.71875000068279,0.)) ;
#126228 = CARTESIAN_POINT('Ctrl Pts',(1.2293670625,-5.67708333401613,-0.709775404467235)) ;
#126229 = CARTESIAN_POINT('Ctrl Pts',(0.61468353125,-5.63541666734946,-1.06466310670085)) ;
#126230 = CARTESIAN_POINT('Ctrl Pts',(8.69224177194317E-17,-5.59375000068279,
-1.41955080893447)) ;
#126231 = CARTESIAN_POINT('Ctrl Pts',(-0.61468353125,-5.55208333401612,-1.06466310670085)) ;
#126232 = CARTESIAN_POINT('Ctrl Pts',(-1.2293670625,-5.51041666734946,-0.709775404467235)) ;
#126233 = CARTESIAN_POINT('Ctrl Pts',(-1.2293670625,-5.46875000068279,-1.50554043806781E-16)) ;
#126234 = CARTESIAN_POINT('Ctrl Pts',(-1.2293670625,-5.42708333401612,0.709775404467234)) ;
#126235 = CARTESIAN_POINT('Ctrl Pts',(-0.614683531250001,-5.38541666734946,
1.06466310670085)) ;
#126236 = CARTESIAN_POINT('Ctrl Pts',(-2.60767253158295E-16,-5.34375000068279,
1.41955080893447)) ;
#126237 = CARTESIAN_POINT('Ctrl Pts',(0.614683531249999,-5.30208333401613,
1.06466310670085)) ;
#126238 = CARTESIAN_POINT('Ctrl Pts',(1.2293670625,-5.26041666734946,0.709775404467235)) ;
#126239 = CARTESIAN_POINT('Ctrl Pts',(1.2293670625,-5.21875000068279,0.)) ;
#126240 = CARTESIAN_POINT('Ctrl Pts',(1.2293670625,-5.17708333401613,-0.709775404467235)) ;
#126241 = CARTESIAN_POINT('Ctrl Pts',(0.61468353125,-5.13541666734946,-1.06466310670085)) ;
#126242 = CARTESIAN_POINT('Ctrl Pts',(8.69224177194317E-17,-5.09375000068279,
-1.41955080893447)) ;
#126243 = CARTESIAN_POINT('Ctrl Pts',(-0.61468353125,-5.05208333401613,-1.06466310670085)) ;
#126244 = CARTESIAN_POINT('Ctrl Pts',(-1.2293670625,-5.01041666734946,-0.709775404467235)) ;
#126245 = CARTESIAN_POINT('Ctrl Pts',(-1.2293670625,-4.96875000068279,-1.50554043806781E-16)) ;
#126246 = CARTESIAN_POINT('Ctrl Pts',(-1.2293670625,-4.92708333401613,0.709775404467234)) ;
#126247 = CARTESIAN_POINT('Ctrl Pts',(-0.614683531250001,-4.88541666734946,
1.06466310670085)) ;
#126248 = CARTESIAN_POINT('Ctrl Pts',(-2.60767253158295E-16,-4.84375000068279,
1.41955080893447)) ;
#126249 = CARTESIAN_POINT('Ctrl Pts',(0.614683531249999,-4.80208333401612,
1.06466310670085)) ;
#126250 = CARTESIAN_POINT('Ctrl Pts',(1.2293670625,-4.76041666734946,0.709775404467235)) ;
#126251 = CARTESIAN_POINT('Ctrl Pts',(1.2293670625,-4.71875000068279,0.)) ;
#126252 = CARTESIAN_POINT('Ctrl Pts',(1.2293670625,-4.67708333401612,-0.709775404467235)) ;
#126253 = CARTESIAN_POINT('Ctrl Pts',(0.61468353125,-4.63541666734946,-1.06466310670085)) ;
#126254 = CARTESIAN_POINT('Ctrl Pts',(8.69224177194317E-17,-4.59375000068279,
-1.41955080893447)) ;
#126255 = CARTESIAN_POINT('Ctrl Pts',(-0.61468353125,-4.55208333401613,-1.06466310670085)) ;
#126256 = CARTESIAN_POINT('Ctrl Pts',(-1.2293670625,-4.51041666734946,-0.709775404467235)) ;
#126257 = CARTESIAN_POINT('Ctrl Pts',(-1.2293670625,-4.46875000068279,-1.50554043806781E-16)) ;
#126258 = CARTESIAN_POINT('Ctrl Pts',(-1.2293670625,-4.42708333401613,0.709775404467234)) ;
#126259 = CARTESIAN_POINT('Ctrl Pts',(-0.614683531250001,-4.38541666734946,
1.06466310670085)) ;
#126260 = CARTESIAN_POINT('Ctrl Pts',(-2.60767253158295E-16,-4.34375000068279,
1.41955080893447)) ;
#126261 = CARTESIAN_POINT('Ctrl Pts',(0.614683531249999,-4.30208333401613,
1.06466310670085)) ;
#126262 = CARTESIAN_POINT('Ctrl Pts',(1.2293670625,-4.26041666734946,0.709775404467235)) ;
#126263 = CARTESIAN_POINT('Ctrl Pts',(1.2293670625,-4.21875000068279,0.)) ;
#126264 = CARTESIAN_POINT('Ctrl Pts',(1.2293670625,-4.17708333401613,-0.709775404467235)) ;
#126265 = CARTESIAN_POINT('Ctrl Pts',(0.61468353125,-4.13541666734946,-1.06466310670085)) ;
#126266 = CARTESIAN_POINT('Ctrl Pts',(8.69224177194317E-17,-4.09375000068279,
-1.41955080893447)) ;
#126267 = CARTESIAN_POINT('Ctrl Pts',(-0.61468353125,-4.05208333401613,-1.06466310670085)) ;
#126268 = CARTESIAN_POINT('Ctrl Pts',(-1.2293670625,-4.01041666734946,-0.709775404467235)) ;
#126269 = CARTESIAN_POINT('Ctrl Pts',(-1.2293670625,-3.96875000068279,-1.50554043806781E-16)) ;
#126270 = CARTESIAN_POINT('Ctrl Pts',(-1.2293670625,-3.92708333401613,0.709775404467234)) ;
#126271 = CARTESIAN_POINT('Ctrl Pts',(-0.614683531250001,-3.88541666734946,
1.06466310670085)) ;
#126272 = CARTESIAN_POINT('Ctrl Pts',(-2.60767253158295E-16,-3.84375000068279,
1.41955080893447)) ;
#126273 = CARTESIAN_POINT('Ctrl Pts',(0.614683531249999,-3.80208333401613,
1.06466310670085)) ;
#126274 = CARTESIAN_POINT('Ctrl Pts',(1.2293670625,-3.76041666734946,0.709775404467235)) ;
#126275 = CARTESIAN_POINT('Ctrl Pts',(1.2293670625,-3.71875000068279,0.)) ;
#126276 = CARTESIAN_POINT('Ctrl Pts',(1.2293670625,-3.67708333401613,-0.709775404467235)) ;
#126277 = CARTESIAN_POINT('Ctrl Pts',(0.61468353125,-3.63541666734946,-1.06466310670085)) ;
#126278 = CARTESIAN_POINT('Ctrl Pts',(8.69224177194317E-17,-3.59375000068279,
-1.41955080893447)) ;
#126279 = CARTESIAN_POINT('Ctrl Pts',(-0.61468353125,-3.55208333401613,-1.06466310670085)) ;
#126280 = CARTESIAN_POINT('Ctrl Pts',(-1.2293670625,-3.51041666734946,-0.709775404467235)) ;
#126281 = CARTESIAN_POINT('Ctrl Pts',(-1.2293670625,-3.46875000068279,-1.50554043806781E-16)) ;
#126282 = CARTESIAN_POINT('Ctrl Pts',(-1.2293670625,-3.42708333401613,0.709775404467234)) ;
#126283 = CARTESIAN_POINT('Ctrl Pts',(-0.614683531250001,-3.38541666734946,
1.06466310670085)) ;
#126284 = CARTESIAN_POINT('Ctrl Pts',(-2.60767253158295E-16,-3.34375000068279,
1.41955080893447)) ;
#126285 = CARTESIAN_POINT('Ctrl Pts',(0.614683531249999,-3.30208333401613,
1.06466310670085)) ;
#126286 = CARTESIAN_POINT('Ctrl Pts',(1.2293670625,-3.26041666734946,0.709775404467235)) ;
#126287 = CARTESIAN_POINT('Ctrl Pts',(1.2293670625,-3.21875000068279,0.)) ;
#126288 = CARTESIAN_POINT('Ctrl Pts',(1.2293670625,-3.17708333401613,-0.709775404467235)) ;
#126289 = CARTESIAN_POINT('Ctrl Pts',(0.61468353125,-3.13541666734946,-1.06466310670085)) ;
#126290 = CARTESIAN_POINT('Ctrl Pts',(8.69224177194317E-17,-3.09375000068279,
-1.41955080893447)) ;
#126291 = CARTESIAN_POINT('Ctrl Pts',(-0.61468353125,-3.05208333401613,-1.06466310670085)) ;
#126292 = CARTESIAN_POINT('Ctrl Pts',(-1.2293670625,-3.01041666734946,-0.709775404467235)) ;
#126293 = CARTESIAN_POINT('Ctrl Pts',(-1.2293670625,-2.96875000068279,-1.50554043806781E-16)) ;
#126294 = CARTESIAN_POINT('Ctrl Pts',(-1.2293670625,-2.92708333401613,0.709775404467234)) ;
#126295 = CARTESIAN_POINT('Ctrl Pts',(-0.614683531250001,-2.88541666734946,
1.06466310670085)) ;
#126296 = CARTESIAN_POINT('Ctrl Pts',(-2.60767253158295E-16,-2.84375000068279,
1.41955080893447)) ;
#126297 = CARTESIAN_POINT('Ctrl Pts',(0.614683531249999,-2.80208333401613,
1.06466310670085)) ;
#126298 = CARTESIAN_POINT('Ctrl Pts',(1.2293670625,-2.76041666734946,0.709775404467235)) ;
#126299 = CARTESIAN_POINT('Ctrl Pts',(1.2293670625,-2.71875000068279,0.)) ;
#126300 = CARTESIAN_POINT('Ctrl Pts',(1.2293670625,-2.67708333401613,-0.709775404467235)) ;
#126301 = CARTESIAN_POINT('Ctrl Pts',(0.61468353125,-2.63541666734946,-1.06466310670085)) ;
#126302 = CARTESIAN_POINT('Ctrl Pts',(8.69224177194317E-17,-2.59375000068279,
-1.41955080893447)) ;
#126303 = CARTESIAN_POINT('Ctrl Pts',(-0.61468353125,-2.55208333401613,-1.06466310670085)) ;
#126304 = CARTESIAN_POINT('Ctrl Pts',(-1.2293670625,-2.51041666734946,-0.709775404467235)) ;
#126305 = CARTESIAN_POINT('Ctrl Pts',(-1.2293670625,-2.46875000068279,-1.50554043806781E-16)) ;
#126306 = CARTESIAN_POINT('Ctrl Pts',(-1.2293670625,-2.42708333401613,0.709775404467234)) ;
#126307 = CARTESIAN_POINT('Ctrl Pts',(-0.614683531250001,-2.38541666734946,
1.06466310670085)) ;
#126308 = CARTESIAN_POINT('Ctrl Pts',(-2.60767253158295E-16,-2.34375000068279,
1.41955080893447)) ;
#126309 = CARTESIAN_POINT('Ctrl Pts',(0.614683531249999,-2.30208333401613,
1.06466310670085)) ;
#126310 = CARTESIAN_POINT('Ctrl Pts',(1.2293670625,-2.26041666734946,0.709775404467235)) ;
#126311 = CARTESIAN_POINT('Ctrl Pts',(1.2293670625,-2.21875000068279,0.)) ;
#126312 = CARTESIAN_POINT('Ctrl Pts',(1.2293670625,-2.17708333401613,-0.709775404467235)) ;
#126313 = CARTESIAN_POINT('Ctrl Pts',(0.61468353125,-2.13541666734946,-1.06466310670085)) ;
#126314 = CARTESIAN_POINT('Ctrl Pts',(8.69224177194317E-17,-2.09375000068279,
-1.41955080893447)) ;
#126315 = CARTESIAN_POINT('Ctrl Pts',(-0.61468353125,-2.05208333401613,-1.06466310670085)) ;
#126316 = CARTESIAN_POINT('Ctrl Pts',(-1.2293670625,-2.01041666734946,-0.709775404467235)) ;
#126317 = CARTESIAN_POINT('Ctrl Pts',(-1.2293670625,-1.96875000068279,-1.50554043806781E-16)) ;
#126318 = CARTESIAN_POINT('Ctrl Pts',(-1.2293670625,-1.92708333401613,0.709775404467234)) ;
#126319 = CARTESIAN_POINT('Ctrl Pts',(-0.614683531250001,-1.88541666734946,
1.06466310670085)) ;
#126320 = CARTESIAN_POINT('Ctrl Pts',(-2.60767253158295E-16,-1.84375000068279,
1.41955080893447)) ;
#126321 = CARTESIAN_POINT('Ctrl Pts',(0.614683531249999,-1.80208333401613,
1.06466310670085)) ;
#126322 = CARTESIAN_POINT('Ctrl Pts',(1.2293670625,-1.76041666734946,0.709775404467235)) ;
#126323 = CARTESIAN_POINT('Ctrl Pts',(1.2293670625,-1.71875000068279,0.)) ;
#126324 = CARTESIAN_POINT('Ctrl Pts',(1.2293670625,-1.67708333401613,-0.709775404467235)) ;
#126325 = CARTESIAN_POINT('Ctrl Pts',(0.61468353125,-1.63541666734946,-1.06466310670085)) ;
#126326 = CARTESIAN_POINT('Ctrl Pts',(8.69224177194317E-17,-1.59375000068279,
-1.41955080893447)) ;
#126327 = CARTESIAN_POINT('Ctrl Pts',(-0.61468353125,-1.55208333401613,-1.06466310670085)) ;
#126328 = CARTESIAN_POINT('Ctrl Pts',(-1.2293670625,-1.51041666734946,-0.709775404467235)) ;
#126329 = CARTESIAN_POINT('Ctrl Pts',(-1.2293670625,-1.46875000068279,-1.50554043806781E-16)) ;
#126330 = CARTESIAN_POINT('Ctrl Pts',(-1.2293670625,-1.42708333401613,0.709775404467234)) ;
#126331 = CARTESIAN_POINT('Ctrl Pts',(-0.614683531250001,-1.38541666734946,
1.06466310670085)) ;
#126332 = CARTESIAN_POINT('Ctrl Pts',(-2.60767253158295E-16,-1.34375000068279,
1.41955080893447)) ;
#126333 = CARTESIAN_POINT('Ctrl Pts',(0.614683531249999,-1.30208333401613,
1.06466310670085)) ;
#126334 = CARTESIAN_POINT('Ctrl Pts',(1.2293670625,-1.26041666734946,0.709775404467235)) ;
#126335 = CARTESIAN_POINT('Ctrl Pts',(1.2293670625,-1.21875000068279,0.)) ;
#126336 = CARTESIAN_POINT('Ctrl Pts',(1.2293670625,-1.17708333401613,-0.709775404467235)) ;
#126337 = CARTESIAN_POINT('Ctrl Pts',(0.61468353125,-1.13541666734946,-1.06466310670085)) ;
#126338 = CARTESIAN_POINT('Ctrl Pts',(8.69224177194317E-17,-1.09375000068279,
-1.41955080893447)) ;
#126339 = CARTESIAN_POINT('Ctrl Pts',(-0.61468353125,-1.05208333401613,-1.06466310670085)) ;
#126340 = CARTESIAN_POINT('Ctrl Pts',(-1.2293670625,-1.01041666734946,-0.709775404467235)) ;
#126341 = CARTESIAN_POINT('Ctrl Pts',(-1.2293670625,-0.968750000682792,-1.50554043806781E-16)) ;
#126342 = CARTESIAN_POINT('Ctrl Pts',(-1.2293670625,-0.927083334016125,0.709775404467234)) ;
#126343 = CARTESIAN_POINT('Ctrl Pts',(-0.614683531250001,-0.885416667349459,
1.06466310670085)) ;
#126344 = CARTESIAN_POINT('Ctrl Pts',(-2.60767253158295E-16,-0.843750000682792,
1.41955080893447)) ;
#126345 = CARTESIAN_POINT('Ctrl Pts',(0.614683531249999,-0.802083334016125,
1.06466310670085)) ;
#126346 = CARTESIAN_POINT('Ctrl Pts',(1.2293670625,-0.760416667349459,0.709775404467235)) ;
#126347 = CARTESIAN_POINT('Ctrl Pts',(1.2293670625,-0.718750000682792,0.)) ;
#126348 = CARTESIAN_POINT('Ctrl Pts',(1.2293670625,-0.707318707356219,-0.194727620266851)) ;
#126349 = CARTESIAN_POINT('Ctrl Pts',(1.16918850806102,-0.694407367007051,
-0.379923159307147)) ;
#126350 = CARTESIAN_POINT('',(1.25324553728064,-0.694450928507311,-0.12117112409355)) ;
#126351 = CARTESIAN_POINT('Origin',(0.0710244857294275,1.34904687806339,0.12019472536195)) ;
#126352 = CARTESIAN_POINT('Ctrl Pts',(1.48723526368499,-0.552750382528326,
-0.19527229821924)) ;
#126353 = CARTESIAN_POINT('Ctrl Pts',(1.46320852678865,-0.567307775622241,
-0.187623192231587)) ;
#126354 = CARTESIAN_POINT('Ctrl Pts',(1.43917883085798,-0.581865143924219,
-0.179983325197973)) ;
#126355 = CARTESIAN_POINT('Ctrl Pts',(1.41514564580341,-0.596422476608758,
-0.17235438796974)) ;
#126356 = CARTESIAN_POINT('Ctrl Pts',(1.39111246013927,-0.610979809662529,
-0.164725450548007)) ;
#126357 = CARTESIAN_POINT('Ctrl Pts',(1.36707578381675,-0.62553710951487,
-0.157107434118075)) ;
#126358 = CARTESIAN_POINT('Ctrl Pts',(1.34303495730321,-0.640094360830228,
-0.149502452876954)) ;
#126359 = CARTESIAN_POINT('Ctrl Pts',(1.31311211923601,-0.658213300025925,
-0.140036779055212)) ;
#126360 = CARTESIAN_POINT('Ctrl Pts',(1.28318286116683,-0.676332170829035,
-0.130591232118516)) ;
#126361 = CARTESIAN_POINT('Ctrl Pts',(1.25324553728064,-0.694450928507311,
-0.12117112409355)) ;
#126362 = CARTESIAN_POINT('Origin',(0.963125678325566,-0.975415808634025,
-1.89018765487928)) ;
#126363 = CARTESIAN_POINT('',(0.705741417818,-0.819163651371321,-1.80654836425755)) ;
#126364 = CARTESIAN_POINT('Origin',(0.70574766896911,-0.694164125798689,-1.8065291234134)) ;
#126365 = CARTESIAN_POINT('',(0.70574766896911,-0.694164125798689,-1.8065291234134)) ;
#126366 = CARTESIAN_POINT('Origin',(0.963147555709039,-0.537916056909366,
-1.89012031114991)) ;
#126367 = CARTESIAN_POINT('',(0.,0.,0.)) ;
#126368 = CARTESIAN_POINT('Origin',(-998.069344648895,0.,0.)) ;
#126369 = CARTESIAN_POINT('',(1.93065535110549,-2.07039899118859E-17,0.)) ;
#126370 = CARTESIAN_POINT('',(1.75000000000779,-6.80903620330553E-17,-0.55600000000311)) ;
#126371 = CARTESIAN_POINT('',(-998.069344648895,-3.76907529259025E-13,-3077.68353717531)) ;
#126372 = CARTESIAN_POINT('',(1.75,-0.175779377683682,-0.527482331818932)) ;
#126373 = CARTESIAN_POINT('Origin',(1.75,0.,0.)) ;
#126374 = CARTESIAN_POINT('',(1.75,-0.369999999999998,-0.415013252800438)) ;
#126375 = CARTESIAN_POINT('Origin',(1.75,0.,0.)) ;
#126376 = CARTESIAN_POINT('',(1.75,-0.415013252800437,-0.370000000000001)) ;
#126377 = CARTESIAN_POINT('Origin',(1.75,0.,0.)) ;
#126378 = CARTESIAN_POINT('',(1.75,-0.527482331818932,-0.175779377683682)) ;
#126379 = CARTESIAN_POINT('Origin',(1.75,0.,0.)) ;
#126380 = CARTESIAN_POINT('',(1.75,-0.527482331818932,0.175779377683681)) ;
#126381 = CARTESIAN_POINT('Origin',(1.75,0.,0.)) ;
#126382 = CARTESIAN_POINT('',(1.75,-0.415013252800437,0.37)) ;
#126383 = CARTESIAN_POINT('Origin',(1.75,0.,0.)) ;
#126384 = CARTESIAN_POINT('',(1.75,-0.370000000000001,0.415013252800437)) ;
#126385 = CARTESIAN_POINT('Origin',(1.75,0.,0.)) ;
#126386 = CARTESIAN_POINT('',(1.75,-0.175779377683684,0.527482331818931)) ;
#126387 = CARTESIAN_POINT('Origin',(1.75,0.,0.)) ;
#126388 = CARTESIAN_POINT('',(1.75,0.175779377683681,0.527482331818932)) ;
#126389 = CARTESIAN_POINT('Origin',(1.75,0.,0.)) ;
#126390 = CARTESIAN_POINT('',(1.75,0.369999999999999,0.415013252800439)) ;
#126391 = CARTESIAN_POINT('Origin',(1.75,0.,0.)) ;
#126392 = CARTESIAN_POINT('',(1.75,0.415013252800437,0.37)) ;
#126393 = CARTESIAN_POINT('Origin',(1.75,0.,0.)) ;
#126394 = CARTESIAN_POINT('',(1.75,0.527482331818932,0.175779377683681)) ;
#126395 = CARTESIAN_POINT('Origin',(1.75,0.,0.)) ;
#126396 = CARTESIAN_POINT('',(1.75,0.527482331818932,-0.175779377683681)) ;
#126397 = CARTESIAN_POINT('Origin',(1.75,0.,0.)) ;
#126398 = CARTESIAN_POINT('',(1.75,0.415013252800437,-0.370000000000001)) ;
#126399 = CARTESIAN_POINT('Origin',(1.75,0.,0.)) ;
#126400 = CARTESIAN_POINT('',(1.75,0.370000000000001,-0.415013252800437)) ;
#126401 = CARTESIAN_POINT('Origin',(1.75,0.,0.)) ;
#126402 = CARTESIAN_POINT('',(1.75,0.175779377683685,-0.527482331818931)) ;
#126403 = CARTESIAN_POINT('Origin',(1.75,0.,0.)) ;
#126404 = CARTESIAN_POINT('Origin',(1.75,0.,0.)) ;
#126405 = CARTESIAN_POINT('Origin',(1.75,0.,0.)) ;
#126406 = CARTESIAN_POINT('Origin',(2.66965268827524,7.90481402181727E-13,
0.0689604923272864)) ;
#126407 = CARTESIAN_POINT('Origin',(2.5,0.,0.)) ;
#126408 = CARTESIAN_POINT('',(2.4,-1.95943487863577E-16,-1.6)) ;
#126409 = CARTESIAN_POINT('Origin',(2.4,0.,0.)) ;
#126410 = CARTESIAN_POINT('',(2.5,-1.83697019872103E-16,-1.5)) ;
#126411 = CARTESIAN_POINT('Origin',(2.5,-1.95943487863577E-16,-1.6)) ;
#126412 = CARTESIAN_POINT('Origin',(2.5,0.,0.)) ;
#126413 = CARTESIAN_POINT('Origin',(1.00350153259131,0.,0.)) ;
#126414 = CARTESIAN_POINT('',(0.775371598933733,-3.27521818376618E-16,-2.67441860465116)) ;
#126415 = CARTESIAN_POINT('Origin',(0.775371598933733,0.,0.)) ;
#126416 = CARTESIAN_POINT('',(1.00350153259131,-3.42901103761259E-16,-2.8)) ;
#126417 = CARTESIAN_POINT('Origin',(1.00350153259131,-3.0983564018428E-16,
-2.53)) ;
#126418 = CARTESIAN_POINT('Origin',(1.00350153259131,0.,0.)) ;
#126419 = CARTESIAN_POINT('Origin',(-25.4,0.,0.)) ;
#126420 = CARTESIAN_POINT('',(2.4,-3.42901103761259E-16,-2.8)) ;
#126421 = CARTESIAN_POINT('',(-25.4,-3.42901103761259E-16,-2.8)) ;
#126422 = CARTESIAN_POINT('Origin',(2.4,0.,0.)) ;
#126423 = CARTESIAN_POINT('Origin',(-25.4,0.,0.)) ;
#126424 = CARTESIAN_POINT('',(6.40000000000001,-1.83697019872103E-16,-1.5)) ;
#126425 = CARTESIAN_POINT('',(-25.4,-1.83697019872103E-16,-1.5)) ;
#126426 = CARTESIAN_POINT('Origin',(6.4,0.,0.)) ;
#126427 = CARTESIAN_POINT('Origin',(5.,-7.47034547479885E-16,0.)) ;
#126428 = CARTESIAN_POINT('',(0.18786973422864,1.30633162146802,-0.37)) ;
#126429 = CARTESIAN_POINT('',(0.18786973422864,1.30633162146802,0.37)) ;
#126430 = CARTESIAN_POINT('Origin',(4.56358262530798,-0.875317983305919,0.)) ;
#126431 = CARTESIAN_POINT('',(0.0457951200896417,0.56476013304091,0.37)) ;
#126432 = CARTESIAN_POINT('Origin',(5.,-8.04072685956911E-16,0.37)) ;
#126433 = CARTESIAN_POINT('',(0.0457951200896434,0.369999999999998,0.564760133040918)) ;
#126434 = CARTESIAN_POINT('Origin',(0.0457951200896417,-7.47034547479885E-16,
0.)) ;
#126435 = CARTESIAN_POINT('',(0.187869734228641,0.369999999999995,1.30633162146802)) ;
#126436 = CARTESIAN_POINT('Origin',(5.,0.37,1.29184809537196E-15)) ;
#126437 = CARTESIAN_POINT('',(0.187869734228641,-0.370000000000004,1.30633162146802)) ;
#126438 = CARTESIAN_POINT('Origin',(4.56358262530798,2.30912185678654E-15,
-0.875317983305919)) ;
#126439 = CARTESIAN_POINT('',(0.045795120089643,-0.370000000000002,0.564760133040916)) ;
#126440 = CARTESIAN_POINT('Origin',(5.,-0.37,-1.34888623384898E-15)) ;
#126441 = CARTESIAN_POINT('',(0.0457951200896417,-0.564760133040912,0.37)) ;
#126442 = CARTESIAN_POINT('Origin',(0.0457951200896417,-7.47034547479885E-16,
0.)) ;
#126443 = CARTESIAN_POINT('',(0.18786973422864,-1.30633162146802,0.369999999999999)) ;
#126444 = CARTESIAN_POINT('Origin',(5.,-8.04072685956911E-16,0.37)) ;
#126445 = CARTESIAN_POINT('',(0.18786973422864,-1.30633162146802,-0.37)) ;
#126446 = CARTESIAN_POINT('Origin',(4.56358262530798,0.875317983305919,0.)) ;
#126447 = CARTESIAN_POINT('',(0.0457951200896417,-0.564760133040916,-0.37)) ;
#126448 = CARTESIAN_POINT('Origin',(5.,-7.47034547479885E-16,-0.37)) ;
#126449 = CARTESIAN_POINT('',(0.0457951200896434,-0.369999999999998,-0.564760133040918)) ;
#126450 = CARTESIAN_POINT('Origin',(0.0457951200896417,-7.47034547479885E-16,
0.)) ;
#126451 = CARTESIAN_POINT('',(0.18786973422864,-0.369999999999995,-1.30633162146802)) ;
#126452 = CARTESIAN_POINT('Origin',(5.,-0.37,-1.34888623384898E-15)) ;
#126453 = CARTESIAN_POINT('',(0.18786973422864,0.370000000000004,-1.30633162146802)) ;
#126454 = CARTESIAN_POINT('Origin',(4.56358262530798,-3.80319095174631E-15,
0.875317983305919)) ;
#126455 = CARTESIAN_POINT('',(0.0457951200896425,0.370000000000002,-0.564760133040916)) ;
#126456 = CARTESIAN_POINT('Origin',(5.,0.37,1.29184809537196E-15)) ;
#126457 = CARTESIAN_POINT('',(0.0457951200896417,0.564760133040915,-0.37)) ;
#126458 = CARTESIAN_POINT('Origin',(0.0457951200896417,-7.47034547479885E-16,
0.)) ;
#126459 = CARTESIAN_POINT('Origin',(5.,-7.47034547479885E-16,-0.37)) ;
#126460 = CARTESIAN_POINT('Origin',(1.75,0.527482331818931,-0.37)) ;
#126461 = CARTESIAN_POINT('Ctrl Pts',(0.0457951200892473,0.564760133040949,
-0.37)) ;
#126462 = CARTESIAN_POINT('Ctrl Pts',(1.02813143236002,0.48263940638371,-0.37)) ;
#126463 = CARTESIAN_POINT('Ctrl Pts',(1.75000000000145,0.415013252800303,
-0.37)) ;
#126464 = CARTESIAN_POINT('',(1.75,0.527482331818932,-0.37)) ;
#126465 = CARTESIAN_POINT('',(1.75,-0.527482331818931,-0.37)) ;
#126466 = CARTESIAN_POINT('',(0.,1.4,-0.37)) ;
#126467 = CARTESIAN_POINT('Origin',(1.75,0.527482331818931,-0.37)) ;
#126468 = CARTESIAN_POINT('',(1.75,-0.527482331818931,-0.37)) ;
#126469 = CARTESIAN_POINT('',(1.75,-0.527482331818931,-0.37)) ;
#126470 = CARTESIAN_POINT('Ctrl Pts',(1.75000000000145,-0.415013252800302,
-0.37)) ;
#126471 = CARTESIAN_POINT('Ctrl Pts',(1.02813143236002,-0.48263940638371,
-0.37)) ;
#126472 = CARTESIAN_POINT('Ctrl Pts',(0.0457951200892475,-0.564760133040949,
-0.37)) ;
#126473 = CARTESIAN_POINT('',(0.,-1.4,-0.37)) ;
#126474 = CARTESIAN_POINT('Origin',(1.75,-0.527482331818931,0.37)) ;
#126475 = CARTESIAN_POINT('',(1.75,0.527482331818932,0.37)) ;
#126476 = CARTESIAN_POINT('',(1.75,0.527482331818931,0.37)) ;
#126477 = CARTESIAN_POINT('Ctrl Pts',(1.75000000000145,0.415013252800303,
0.37)) ;
#126478 = CARTESIAN_POINT('Ctrl Pts',(1.02813143236001,0.482639406383711,
0.37)) ;
#126479 = CARTESIAN_POINT('Ctrl Pts',(0.0457951200892475,0.564760133040949,
0.37)) ;
#126480 = CARTESIAN_POINT('',(0.,1.4,0.37)) ;
#126481 = CARTESIAN_POINT('Origin',(1.75,-0.527482331818931,0.37)) ;
#126482 = CARTESIAN_POINT('Ctrl Pts',(0.0457951200892472,-0.56476013304095,
0.37)) ;
#126483 = CARTESIAN_POINT('Ctrl Pts',(1.02813143236001,-0.482639406383711,
0.37)) ;
#126484 = CARTESIAN_POINT('Ctrl Pts',(1.75000000000145,-0.415013252800303,
0.37)) ;
#126485 = CARTESIAN_POINT('',(1.75,-0.527482331818931,0.37)) ;
#126486 = CARTESIAN_POINT('',(1.75,0.527482331818931,0.37)) ;
#126487 = CARTESIAN_POINT('',(0.,-1.4,0.369999999999999)) ;
#126488 = CARTESIAN_POINT('Origin',(1.75,0.527482331818931,0.37)) ;
#126489 = CARTESIAN_POINT('Origin',(2.6696526882827,0.0689604923235791,0.)) ;
#126490 = CARTESIAN_POINT('',(1.75,0.527482331818931,0.37)) ;
#126491 = CARTESIAN_POINT('',(1.75,0.527482331818931,0.37)) ;
#126492 = CARTESIAN_POINT('Origin',(0.,-1.4,-0.37)) ;
#126493 = CARTESIAN_POINT('Origin',(2.66965268828244,-0.0689604923237097,
2.08166817117217E-16)) ;
#126494 = CARTESIAN_POINT('',(1.75,-0.527482331818931,-0.37)) ;
#126495 = CARTESIAN_POINT('',(1.75,-0.527482331818931,-0.37)) ;
#126496 = CARTESIAN_POINT('Origin',(1.75,0.527482331818931,-0.37)) ;
#126497 = CARTESIAN_POINT('',(1.75,-0.370000000000002,0.52748233181893)) ;
#126498 = CARTESIAN_POINT('',(1.75,-0.370000000000002,0.52748233181893)) ;
#126499 = CARTESIAN_POINT('',(1.75,-0.370000000000002,0.52748233181893)) ;
#126500 = CARTESIAN_POINT('Origin',(1.75,0.527482331818931,-0.37)) ;
#126501 = CARTESIAN_POINT('Origin',(1.75,0.527482331818931,-0.37)) ;
#126502 = CARTESIAN_POINT('Origin',(1.75,0.527482331818931,-0.37)) ;
#126503 = CARTESIAN_POINT('',(1.75,-0.369999999999998,-0.527482331818932)) ;
#126504 = CARTESIAN_POINT('',(1.75,-0.370000000000002,0.52748233181893)) ;
#126505 = CARTESIAN_POINT('',(1.75,0.370000000000002,-0.52748233181893)) ;
#126506 = CARTESIAN_POINT('Origin',(1.75,0.527482331818931,-0.37)) ;
#126507 = CARTESIAN_POINT('',(1.75,0.370000000000002,-0.52748233181893)) ;
#126508 = CARTESIAN_POINT('',(1.75,0.370000000000002,-0.52748233181893)) ;
#126509 = CARTESIAN_POINT('',(1.75,0.370000000000002,-0.52748233181893)) ;
#126510 = CARTESIAN_POINT('Origin',(1.75,0.527482331818931,-0.37)) ;
#126511 = CARTESIAN_POINT('Origin',(1.75,0.527482331818931,-0.37)) ;
#126512 = CARTESIAN_POINT('Origin',(1.75,0.369999999999998,0.527482331818933)) ;
#126513 = CARTESIAN_POINT('Ctrl Pts',(0.0457951200892495,0.369999999999998,
0.564760133040951)) ;
#126514 = CARTESIAN_POINT('Ctrl Pts',(1.02813143235992,0.369999999999998,
0.48263940638372)) ;
#126515 = CARTESIAN_POINT('Ctrl Pts',(1.75000000000145,0.369999999999999,
0.415013252800303)) ;
#126516 = CARTESIAN_POINT('',(1.75,0.369999999999998,0.527482331818933)) ;
#126517 = CARTESIAN_POINT('',(1.75,0.370000000000002,-0.52748233181893)) ;
#126518 = CARTESIAN_POINT('',(0.,0.369999999999995,1.4)) ;
#126519 = CARTESIAN_POINT('Origin',(1.75,-0.369999999999998,-0.527482331818932)) ;
#126520 = CARTESIAN_POINT('Ctrl Pts',(1.75000000000145,-0.370000000000001,
0.4150132528003)) ;
#126521 = CARTESIAN_POINT('Ctrl Pts',(1.02813143235991,-0.370000000000002,
0.482639406383718)) ;
#126522 = CARTESIAN_POINT('Ctrl Pts',(0.0457951200892481,-0.370000000000002,
0.564760133040949)) ;
#126523 = CARTESIAN_POINT('',(0.,-0.370000000000005,1.4)) ;
#126524 = CARTESIAN_POINT('Origin',(1.75,-0.370000000000002,0.52748233181893)) ;
#126525 = CARTESIAN_POINT('',(1.75,-0.370000000000002,0.52748233181893)) ;
#126526 = CARTESIAN_POINT('Origin',(0.,0.370000000000005,-1.4)) ;
#126527 = CARTESIAN_POINT('Origin',(2.6696526882837,2.04697370165263E-15,
-0.0689604923230734)) ;
#126528 = CARTESIAN_POINT('',(0.,0.370000000000005,-1.4)) ;
#126529 = CARTESIAN_POINT('',(0.,-0.369999999999995,-1.4)) ;
#126530 = CARTESIAN_POINT('Origin',(1.75,0.369999999999998,0.527482331818933)) ;
#126531 = CARTESIAN_POINT('Ctrl Pts',(1.75000000000145,0.370000000000001,
-0.415013252800299)) ;
#126532 = CARTESIAN_POINT('Ctrl Pts',(1.02813143235982,0.370000000000002,
-0.482639406383727)) ;
#126533 = CARTESIAN_POINT('Ctrl Pts',(0.0457951200892477,0.370000000000002,
-0.56476013304095)) ;
#126534 = CARTESIAN_POINT('Origin',(1.75,-0.369999999999998,-0.527482331818932)) ;
#126535 = CARTESIAN_POINT('Ctrl Pts',(0.0457951200892493,-0.369999999999998,
-0.564760133040952)) ;
#126536 = CARTESIAN_POINT('Ctrl Pts',(1.0281314323599,-0.369999999999998,
-0.482639406383722)) ;
#126537 = CARTESIAN_POINT('Ctrl Pts',(1.75000000000145,-0.369999999999998,
-0.415013252800303)) ;
#126538 = CARTESIAN_POINT('Origin',(2.4,1.5,0.)) ;
#126539 = CARTESIAN_POINT('Origin',(6.4,1.5,0.)) ;
#126540 = CARTESIAN_POINT('Origin',(1.75,0.527482331818931,-0.37)) ;
#126541 = CARTESIAN_POINT('Origin',(1.75,0.,0.)) ;
#126542 = CARTESIAN_POINT('Origin',(1.75,0.,0.)) ;
#126543 = CARTESIAN_POINT('Origin',(1.75,0.,0.)) ;
#126544 = CARTESIAN_POINT('Origin',(1.75,0.,0.)) ;
#126545 = CARTESIAN_POINT('Origin',(1.75,0.,0.)) ;
#126546 = CARTESIAN_POINT('Origin',(1.75,0.,0.)) ;
#126547 = CARTESIAN_POINT('Origin',(1.75,0.,0.)) ;
#126548 = CARTESIAN_POINT('',(43.,0.,34.25)) ;
#126549 = CARTESIAN_POINT('',(2.60208521396521E-14,19.75,1.38777878078145E-14)) ;
#126550 = CARTESIAN_POINT('',(45.5,6.35,30.21)) ;
#126551 = CARTESIAN_POINT('',(51.8530000000001,10.,-36.77)) ;
#126552 = CARTESIAN_POINT('',(47.5,9.35,4.75)) ;
#126553 = CARTESIAN_POINT('',(43.,22.15,-34.25)) ;
#126554 = CARTESIAN_POINT('',(43.,0.,-34.25)) ;
#126555 = CARTESIAN_POINT('',(43.,22.15,34.25)) ;
#126556 = UNCERTAINTY_MEASURE_WITH_UNIT(LENGTH_MEASURE(0.01),#126572,
'DISTANCE_ACCURACY_VALUE',
'Maximum model space distance between geometric entities at asserted c
onnectivities') ;
#126557 = UNCERTAINTY_MEASURE_WITH_UNIT(LENGTH_MEASURE(0.01),#126572,
'DISTANCE_ACCURACY_VALUE',
'Maximum model space distance between geometric entities at asserted c
onnectivities') ;
#126558 = UNCERTAINTY_MEASURE_WITH_UNIT(LENGTH_MEASURE(0.01),#126572,
'DISTANCE_ACCURACY_VALUE',
'Maximum model space distance between geometric entities at asserted c
onnectivities') ;
#126559 = UNCERTAINTY_MEASURE_WITH_UNIT(LENGTH_MEASURE(0.01),#126572,
'DISTANCE_ACCURACY_VALUE',
'Maximum model space distance between geometric entities at asserted c
onnectivities') ;
#126560 = UNCERTAINTY_MEASURE_WITH_UNIT(LENGTH_MEASURE(0.01),#126572,
'DISTANCE_ACCURACY_VALUE',
'Maximum model space distance between geometric entities at asserted c
onnectivities') ;
#126561 = UNCERTAINTY_MEASURE_WITH_UNIT(LENGTH_MEASURE(0.01),#126572,
'DISTANCE_ACCURACY_VALUE',
'Maximum model space distance between geometric entities at asserted c
onnectivities') ;
#126562 = UNCERTAINTY_MEASURE_WITH_UNIT(LENGTH_MEASURE(0.01),#126572,
'DISTANCE_ACCURACY_VALUE',
'Maximum model space distance between geometric entities at asserted c
onnectivities') ;
#126563 = UNCERTAINTY_MEASURE_WITH_UNIT(LENGTH_MEASURE(0.01),#126572,
'DISTANCE_ACCURACY_VALUE',
'Maximum model space distance between geometric entities at asserted c
onnectivities') ;
#126564 = (
GEOMETRIC_REPRESENTATION_CONTEXT(3)
GLOBAL_UNCERTAINTY_ASSIGNED_CONTEXT((#126556))
GLOBAL_UNIT_ASSIGNED_CONTEXT((#126572,#126574,#126575))
REPRESENTATION_CONTEXT('','3D')
) ;
#126565 = (
GEOMETRIC_REPRESENTATION_CONTEXT(3)
GLOBAL_UNCERTAINTY_ASSIGNED_CONTEXT((#126557))
GLOBAL_UNIT_ASSIGNED_CONTEXT((#126572,#126574,#126575))
REPRESENTATION_CONTEXT('','3D')
) ;
#126566 = (
GEOMETRIC_REPRESENTATION_CONTEXT(3)
GLOBAL_UNCERTAINTY_ASSIGNED_CONTEXT((#126558))
GLOBAL_UNIT_ASSIGNED_CONTEXT((#126572,#126574,#126575))
REPRESENTATION_CONTEXT('','3D')
) ;
#126567 = (
GEOMETRIC_REPRESENTATION_CONTEXT(3)
GLOBAL_UNCERTAINTY_ASSIGNED_CONTEXT((#126559))
GLOBAL_UNIT_ASSIGNED_CONTEXT((#126572,#126574,#126575))
REPRESENTATION_CONTEXT('','3D')
) ;
#126568 = (
GEOMETRIC_REPRESENTATION_CONTEXT(3)
GLOBAL_UNCERTAINTY_ASSIGNED_CONTEXT((#126560))
GLOBAL_UNIT_ASSIGNED_CONTEXT((#126572,#126574,#126575))
REPRESENTATION_CONTEXT('','3D')
) ;
#126569 = (
GEOMETRIC_REPRESENTATION_CONTEXT(3)
GLOBAL_UNCERTAINTY_ASSIGNED_CONTEXT((#126561))
GLOBAL_UNIT_ASSIGNED_CONTEXT((#126572,#126574,#126575))
REPRESENTATION_CONTEXT('','3D')
) ;
#126570 = (
GEOMETRIC_REPRESENTATION_CONTEXT(3)
GLOBAL_UNCERTAINTY_ASSIGNED_CONTEXT((#126562))
GLOBAL_UNIT_ASSIGNED_CONTEXT((#126572,#126574,#126575))
REPRESENTATION_CONTEXT('','3D')
) ;
#126571 = (
GEOMETRIC_REPRESENTATION_CONTEXT(3)
GLOBAL_UNCERTAINTY_ASSIGNED_CONTEXT((#126563))
GLOBAL_UNIT_ASSIGNED_CONTEXT((#126572,#126574,#126575))
REPRESENTATION_CONTEXT('','3D')
) ;
#126572 = (
LENGTH_UNIT()
NAMED_UNIT(*)
SI_UNIT(.MILLI.,.METRE.)
) ;
#126573 = (
LENGTH_UNIT()
NAMED_UNIT(*)
SI_UNIT($,.METRE.)
) ;
#126574 = (
NAMED_UNIT(*)
PLANE_ANGLE_UNIT()
SI_UNIT($,.RADIAN.)
) ;
#126575 = (
NAMED_UNIT(*)
SI_UNIT($,.STERADIAN.)
SOLID_ANGLE_UNIT()
) ;
#126576 = SHAPE_DEFINITION_REPRESENTATION(#126583,#126598) ;
#126577 = SHAPE_DEFINITION_REPRESENTATION(#126584,#126599) ;
#126578 = SHAPE_DEFINITION_REPRESENTATION(#126585,#126600) ;
#126579 = SHAPE_DEFINITION_REPRESENTATION(#126586,#126601) ;
#126580 = SHAPE_DEFINITION_REPRESENTATION(#126587,#126602) ;
#126581 = SHAPE_DEFINITION_REPRESENTATION(#126588,#126603) ;
#126582 = SHAPE_DEFINITION_REPRESENTATION(#126589,#126604) ;
#126583 = PRODUCT_DEFINITION_SHAPE('',$,#126606) ;
#126584 = PRODUCT_DEFINITION_SHAPE('',$,#126607) ;
#126585 = PRODUCT_DEFINITION_SHAPE('',$,#126608) ;
#126586 = PRODUCT_DEFINITION_SHAPE('',$,#126609) ;
#126587 = PRODUCT_DEFINITION_SHAPE('',$,#126610) ;
#126588 = PRODUCT_DEFINITION_SHAPE('',$,#126611) ;
#126589 = PRODUCT_DEFINITION_SHAPE('',$,#126612) ;
#126590 = PRODUCT_DEFINITION_SHAPE($,$,#35) ;
#126591 = PRODUCT_DEFINITION_SHAPE($,$,#36) ;
#126592 = PRODUCT_DEFINITION_SHAPE($,$,#37) ;
#126593 = PRODUCT_DEFINITION_SHAPE($,$,#38) ;
#126594 = PRODUCT_DEFINITION_SHAPE($,$,#39) ;
#126595 = PRODUCT_DEFINITION_SHAPE($,$,#40) ;
#126596 = PRODUCT_DEFINITION_SHAPE($,$,#41) ;
#126597 = PRODUCT_DEFINITION_SHAPE($,$,#42) ;
#126598 = SHAPE_REPRESENTATION('',(#67763,#76844,#76845,#76846,#76847,#76848,
#76849,#76850,#76851),#126564) ;
#126599 = SHAPE_REPRESENTATION('',(#67764),#126565) ;
#126600 = SHAPE_REPRESENTATION('',(#68778),#126566) ;
#126601 = SHAPE_REPRESENTATION('',(#71829),#126567) ;
#126602 = SHAPE_REPRESENTATION('',(#71866),#126568) ;
#126603 = SHAPE_REPRESENTATION('',(#76669),#126569) ;
#126604 = SHAPE_REPRESENTATION('',(#76762),#126570) ;
#126605 = PRODUCT_DEFINITION_CONTEXT('part definition',#126628,'design') ;
#126606 = PRODUCT_DEFINITION('MAS-642','MAS-642',#126613,
#126605) ;
#126607 = PRODUCT_DEFINITION('Enclosure_Cover','Enclosure_Cover',#126614,#126605) ;
#126608 = PRODUCT_DEFINITION('Header_200mil_N5','Header_200mil_N5',#126615,
#126605) ;
#126609 = PRODUCT_DEFINITION('LED_Green','LED_Green',#126616,#126605) ;
#126610 = PRODUCT_DEFINITION('Header_3.81mm_N10','Header_3.81mm_N10',#126617,
#126605) ;
#126611 = PRODUCT_DEFINITION('Standoff_M3x18','Standoff_M3x18',#126618,#126605) ;
#126612 = PRODUCT_DEFINITION('Screw_ISO7045_M3x4','Screw_ISO7045_M3x4',#126619,
#126605) ;
#126613 = PRODUCT_DEFINITION_FORMATION('',$,#126630) ;
#126614 = PRODUCT_DEFINITION_FORMATION('',$,#126631) ;
#126615 = PRODUCT_DEFINITION_FORMATION('',$,#126632) ;
#126616 = PRODUCT_DEFINITION_FORMATION('',$,#126633) ;
#126617 = PRODUCT_DEFINITION_FORMATION('',$,#126634) ;
#126618 = PRODUCT_DEFINITION_FORMATION('',$,#126635) ;
#126619 = PRODUCT_DEFINITION_FORMATION('',$,#126636) ;
#126620 = PRODUCT_RELATED_PRODUCT_CATEGORY('MAS-642','MAS-642',(#126630)) ;
#126621 = PRODUCT_RELATED_PRODUCT_CATEGORY('Enclosure_Cover',
'Enclosure_Cover',(#126631)) ;
#126622 = PRODUCT_RELATED_PRODUCT_CATEGORY('Header_200mil_N5',
'Header_200mil_N5',(#126632)) ;
#126623 = PRODUCT_RELATED_PRODUCT_CATEGORY('LED_Green','LED_Green',(#126633)) ;
#126624 = PRODUCT_RELATED_PRODUCT_CATEGORY('Header_3.81mm_N10',
'Header_3.81mm_N10',(#126634)) ;
#126625 = PRODUCT_RELATED_PRODUCT_CATEGORY('Standoff_M3x18',
'Standoff_M3x18',(#126635)) ;
#126626 = PRODUCT_RELATED_PRODUCT_CATEGORY('Screw_ISO7045_M3x4',
'Screw_ISO7045_M3x4',(#126636)) ;
#126627 = APPLICATION_PROTOCOL_DEFINITION('international standard',
'automotive_design',2009,#126628) ;
#126628 = APPLICATION_CONTEXT(
'Core Data for Automotive Mechanical Design Process') ;
#126629 = PRODUCT_CONTEXT('part definition',#126628,'mechanical') ;
#126630 = PRODUCT('MAS-642','MAS-642',$,(#126629)) ;
#126631 = PRODUCT('Enclosure_Cover','Enclosure_Cover',$,(#126629)) ;
#126632 = PRODUCT('Header_200mil_N5','Header_200mil_N5',$,(#126629)) ;
#126633 = PRODUCT('LED_Green','LED_Green',$,(#126629)) ;
#126634 = PRODUCT('Header_3.81mm_N10','Header_3.81mm_N10',$,(#126629)) ;
#126635 = PRODUCT('Standoff_M3x18','Standoff_M3x18',$,(#126629)) ;
#126636 = PRODUCT('Screw_ISO7045_M3x4','Screw_ISO7045_M3x4',$,(#126629)) ;
#126637 = PRESENTATION_STYLE_ASSIGNMENT((#126646)) ;
#126638 = PRESENTATION_STYLE_ASSIGNMENT((#126647)) ;
#126639 = PRESENTATION_STYLE_ASSIGNMENT((#126648)) ;
#126640 = PRESENTATION_STYLE_ASSIGNMENT((#126649)) ;
#126641 = PRESENTATION_STYLE_ASSIGNMENT((#126650)) ;
#126642 = PRESENTATION_STYLE_ASSIGNMENT((#126651)) ;
#126643 = PRESENTATION_STYLE_ASSIGNMENT((#126652)) ;
#126644 = PRESENTATION_STYLE_ASSIGNMENT((#126653)) ;
#126645 = PRESENTATION_STYLE_ASSIGNMENT((#126654)) ;
#126646 = SURFACE_STYLE_USAGE(.BOTH.,#126655) ;
#126647 = SURFACE_STYLE_USAGE(.BOTH.,#126656) ;
#126648 = SURFACE_STYLE_USAGE(.BOTH.,#126657) ;
#126649 = SURFACE_STYLE_USAGE(.BOTH.,#126658) ;
#126650 = SURFACE_STYLE_USAGE(.BOTH.,#126659) ;
#126651 = SURFACE_STYLE_USAGE(.BOTH.,#126660) ;
#126652 = SURFACE_STYLE_USAGE(.BOTH.,#126661) ;
#126653 = SURFACE_STYLE_USAGE(.BOTH.,#126662) ;
#126654 = SURFACE_STYLE_USAGE(.BOTH.,#126663) ;
#126655 = SURFACE_SIDE_STYLE('',(#126664)) ;
#126656 = SURFACE_SIDE_STYLE('',(#126665)) ;
#126657 = SURFACE_SIDE_STYLE('',(#126666)) ;
#126658 = SURFACE_SIDE_STYLE('',(#126667)) ;
#126659 = SURFACE_SIDE_STYLE('',(#126668)) ;
#126660 = SURFACE_SIDE_STYLE('',(#126669)) ;
#126661 = SURFACE_SIDE_STYLE('',(#126670)) ;
#126662 = SURFACE_SIDE_STYLE('',(#126671)) ;
#126663 = SURFACE_SIDE_STYLE('',(#126672)) ;
#126664 = SURFACE_STYLE_FILL_AREA(#126673) ;
#126665 = SURFACE_STYLE_FILL_AREA(#126674) ;
#126666 = SURFACE_STYLE_FILL_AREA(#126675) ;
#126667 = SURFACE_STYLE_FILL_AREA(#126676) ;
#126668 = SURFACE_STYLE_FILL_AREA(#126677) ;
#126669 = SURFACE_STYLE_FILL_AREA(#126678) ;
#126670 = SURFACE_STYLE_FILL_AREA(#126679) ;
#126671 = SURFACE_STYLE_FILL_AREA(#126680) ;
#126672 = SURFACE_STYLE_FILL_AREA(#126681) ;
#126673 = FILL_AREA_STYLE('Steel - Satin',(#126682)) ;
#126674 = FILL_AREA_STYLE('Opaque(228,233,237)',(#126683)) ;
#126675 = FILL_AREA_STYLE('Opaque(202,209,238)',(#126684)) ;
#126676 = FILL_AREA_STYLE('Opaque(128,255,128)',(#126685)) ;
#126677 = FILL_AREA_STYLE('Opaque(204,207,204)',(#126686)) ;
#126678 = FILL_AREA_STYLE('Opaque(128,128,128)',(#126687)) ;
#126679 = FILL_AREA_STYLE('Opaque(0,255,0)',(#126688)) ;
#126680 = FILL_AREA_STYLE('Opaque(165,132,0)',(#126689)) ;
#126681 = FILL_AREA_STYLE('Opaque(198,193,188)',(#126690)) ;
#126682 = FILL_AREA_STYLE_COLOUR('Steel - Satin',#126691) ;
#126683 = FILL_AREA_STYLE_COLOUR('Opaque(228,233,237)',#126692) ;
#126684 = FILL_AREA_STYLE_COLOUR('Opaque(202,209,238)',#126693) ;
#126685 = FILL_AREA_STYLE_COLOUR('Opaque(128,255,128)',#126694) ;
#126686 = FILL_AREA_STYLE_COLOUR('Opaque(204,207,204)',#126695) ;
#126687 = FILL_AREA_STYLE_COLOUR('Opaque(128,128,128)',#126696) ;
#126688 = FILL_AREA_STYLE_COLOUR('Opaque(0,255,0)',#126697) ;
#126689 = FILL_AREA_STYLE_COLOUR('Opaque(165,132,0)',#126698) ;
#126690 = FILL_AREA_STYLE_COLOUR('Opaque(198,193,188)',#126699) ;
#126691 = COLOUR_RGB('Steel - Satin', 0.09019608, 0.27058824, 0.51372549) ;
#126692 = COLOUR_RGB('Opaque(228,233,237)', 0.09019608, 0.27058824, 0.51372549) ;
#126693 = COLOUR_RGB('Opaque(202,209,238)', 0.66274510, 0.83137255, 0.94901961) ;
#126694 = COLOUR_RGB('Opaque(128,255,128)', 0.66274510, 0.83137255, 0.94901961) ;
#126695 = COLOUR_RGB('Opaque(204,207,204)', 0.40784314, 0.44705882, 0.49803922) ;
#126696 = COLOUR_RGB('Opaque(128,128,128)', 0.09019608, 0.27058824, 0.51372549) ;
#126697 = COLOUR_RGB('Opaque(0,255,0)', 0.08235294, 0.09019608, 0.10196078) ;
#126698 = COLOUR_RGB('Opaque(165,132,0)', 0.31764706, 0.68627451, 0.89019608) ;
#126699 = COLOUR_RGB('Opaque(198,193,188)', 0.40784314, 0.44705882, 0.49803922) ;
ENDSEC;
END-ISO-10303-21;
